#121526 = CARTESIAN_POINT('Ctrl Pts',(-22.0627069665889,12.7436129687706,
131.427847524928)) ;
#121527 = CARTESIAN_POINT('Ctrl Pts',(-22.1228015587848,12.9681022843807,
131.570102893173)) ;
#121528 = CARTESIAN_POINT('Ctrl Pts',(-22.1614820013196,13.2239471753799,
131.650012500945)) ;
#121529 = CARTESIAN_POINT('Ctrl Pts',(-22.1772375533801,13.4941633310118,
131.662924277638)) ;
#121530 = CARTESIAN_POINT('Ctrl Pts',(-22.1695983588983,13.7589186956337,
131.607544732681)) ;
#121531 = CARTESIAN_POINT('Ctrl Pts',(-22.1398896393099,13.9998349614895,
131.487676911223)) ;
#121532 = CARTESIAN_POINT('Ctrl Pts',(-22.0908619235723,14.1997646891006,
131.311332678912)) ;
#121533 = CARTESIAN_POINT('Ctrl Pts',(-22.0266945737524,14.344263749604,131.090721536142)) ;
#121534 = CARTESIAN_POINT('Ctrl Pts',(-21.952680793742,14.4224928496146,130.841310291008)) ;
#121535 = CARTESIAN_POINT('Ctrl Pts',(-21.8754606570184,14.4291711030004,
130.58274926124)) ;
#121536 = CARTESIAN_POINT('Ctrl Pts',(-21.8001571446588,14.3636108427049,
130.329504565342)) ;
#121537 = CARTESIAN_POINT('Ctrl Pts',(-21.7338905583542,14.2305640728087,
130.102800547914)) ;
#121538 = CARTESIAN_POINT('Ctrl Pts',(-21.6819125731549,14.0406274763076,
129.917954418755)) ;
#121539 = CARTESIAN_POINT('Ctrl Pts',(-21.6482766927022,13.8058698761943,
129.786568126659)) ;
#121540 = CARTESIAN_POINT('Ctrl Pts',(-21.6364270305114,13.5427807142404,
129.718722262125)) ;
#121541 = CARTESIAN_POINT('Ctrl Pts',(-21.6479525293074,13.2720604281958,
129.719284180321)) ;
#121542 = CARTESIAN_POINT('Ctrl Pts',(-21.6827354707971,13.0118428173477,
129.787740591491)) ;
#121543 = CARTESIAN_POINT('Ctrl Pts',(-21.7387645363647,12.7818787427455,
129.918382531202)) ;
#121544 = CARTESIAN_POINT('Ctrl Pts',(-21.8131751278323,12.5968716108038,
130.102584387991)) ;
#121545 = CARTESIAN_POINT('Ctrl Pts',(-21.9012978983489,12.4712516936664,
130.326815834056)) ;
#121546 = CARTESIAN_POINT('Ctrl Pts',(-21.9970924731431,12.4142247915804,
130.573571167119)) ;
#121547 = CARTESIAN_POINT('Ctrl Pts',(-22.0946249674174,12.4291610555867,
130.825434404428)) ;
#121548 = CARTESIAN_POINT('Ctrl Pts',(-22.1880538379132,12.5152749819563,
131.065210306025)) ;
#121549 = CARTESIAN_POINT('Ctrl Pts',(-22.2712353524733,12.6672522728085,
131.274961582696)) ;
#121550 = CARTESIAN_POINT('Ctrl Pts',(-22.3381448037188,12.8714563958125,
131.437501065827)) ;
#121551 = CARTESIAN_POINT('Ctrl Pts',(-22.3859106141911,13.1164156857726,
131.543882892038)) ;
#121552 = CARTESIAN_POINT('Ctrl Pts',(-22.4112282957359,13.3833143982509,
131.584711419103)) ;
#121553 = CARTESIAN_POINT('Ctrl Pts',(-22.4130217695324,13.6536761836367,
131.55673452737)) ;
#121554 = CARTESIAN_POINT('Ctrl Pts',(-22.3920167236971,13.9063303712051,
131.462322269529)) ;
#121555 = CARTESIAN_POINT('Ctrl Pts',(-22.3501194078207,14.1256565234766,
131.306665041968)) ;
#121556 = CARTESIAN_POINT('Ctrl Pts',(-22.2918172565239,14.2929703987116,
131.103406435929)) ;
#121557 = CARTESIAN_POINT('Ctrl Pts',(-22.2209556831958,14.3994043098715,
130.863140859753)) ;
#121558 = CARTESIAN_POINT('Ctrl Pts',(-22.1443006583547,14.4351253202518,
130.60615685561)) ;
#121559 = CARTESIAN_POINT('Ctrl Pts',(-22.0676126713909,14.3988243976867,
130.349047099311)) ;
#121560 = CARTESIAN_POINT('Ctrl Pts',(-21.9970015558164,14.2923293350233,
130.109611142122)) ;
#121561 = CARTESIAN_POINT('Ctrl Pts',(-21.9386211582789,14.1241731198379,
129.906023714666)) ;
#121562 = CARTESIAN_POINT('Ctrl Pts',(-21.8969564647824,13.9051613921294,
129.751139774253)) ;
#121563 = CARTESIAN_POINT('Ctrl Pts',(-21.8760425466096,13.6518311296983,
129.656921029517)) ;
#121564 = CARTESIAN_POINT('Ctrl Pts',(-21.8779576296647,13.382470855745,129.629430197668)) ;
#121565 = CARTESIAN_POINT('Ctrl Pts',(-21.903356370173,13.1154253093326,129.670468190117)) ;
#121566 = CARTESIAN_POINT('Ctrl Pts',(-21.9511796972224,12.870532627165,129.777021512631)) ;
#121567 = CARTESIAN_POINT('Ctrl Pts',(-22.018597334857,12.6655370623813,129.940858603322)) ;
#121568 = CARTESIAN_POINT('Ctrl Pts',(-22.1016149733205,12.5146112144562,
130.150247300748)) ;
#121569 = CARTESIAN_POINT('Ctrl Pts',(-22.1950646404757,12.4289101805898,
130.390085189532)) ;
#121570 = CARTESIAN_POINT('Ctrl Pts',(-22.2924700780955,12.414189675376,130.641628079446)) ;
#121571 = CARTESIAN_POINT('Ctrl Pts',(-22.3890144251563,12.4724108843215,
130.890294126128)) ;
#121572 = CARTESIAN_POINT('Ctrl Pts',(-22.4763336587939,12.5978142660017,
131.112435610646)) ;
#121573 = CARTESIAN_POINT('Ctrl Pts',(-22.5506291996143,12.7826552616513,
131.296338429027)) ;
#121574 = CARTESIAN_POINT('Ctrl Pts',(-22.6066949619686,13.0133815728599,
131.427008840756)) ;
#121575 = CARTESIAN_POINT('Ctrl Pts',(-22.6413737989187,13.2742169731993,
131.495103126571)) ;
#121576 = CARTESIAN_POINT('Ctrl Pts',(-22.652675011079,13.5450315924184,131.494998262817)) ;
#121577 = CARTESIAN_POINT('Ctrl Pts',(-22.6407386602464,13.8067212996898,
131.427059832861)) ;
#121578 = CARTESIAN_POINT('Ctrl Pts',(-22.6071088701475,14.041251387199,131.295715732246)) ;
#121579 = CARTESIAN_POINT('Ctrl Pts',(-22.5548293120912,14.2318697837458,
131.109842788739)) ;
#121580 = CARTESIAN_POINT('Ctrl Pts',(-22.4882219597125,14.3645253457052,
130.882041140552)) ;
#121581 = CARTESIAN_POINT('Ctrl Pts',(-22.4135301561278,14.4291513856489,
130.630867987503)) ;
#121582 = CARTESIAN_POINT('Ctrl Pts',(-22.3359383497484,14.4223448074479,
130.371059800614)) ;
#121583 = CARTESIAN_POINT('Ctrl Pts',(-22.2619633520101,14.3433927947591,
130.121750920733)) ;
#121584 = CARTESIAN_POINT('Ctrl Pts',(-22.1981313809753,14.1993296986607,
129.902268927259)) ;
#121585 = CARTESIAN_POINT('Ctrl Pts',(-22.1490456223981,13.9988089965648,
129.725677746774)) ;
#121586 = CARTESIAN_POINT('Ctrl Pts',(-22.1194205531409,13.7578101300497,
129.60606621788)) ;
#121587 = CARTESIAN_POINT('Ctrl Pts',(-22.1119250099299,13.4916490682303,
129.550940820402)) ;
#121588 = CARTESIAN_POINT('Ctrl Pts',(-22.1278069450151,13.2223242995655,
129.564332881806)) ;
#121589 = CARTESIAN_POINT('Ctrl Pts',(-22.166820729976,12.9657468504133,129.645089069852)) ;
#121590 = CARTESIAN_POINT('Ctrl Pts',(-22.2266899368361,12.7429296521264,
129.78689267835)) ;
#121591 = CARTESIAN_POINT('Ctrl Pts',(-22.3038746479134,12.5685157086448,
129.979270003299)) ;
#121592 = CARTESIAN_POINT('Ctrl Pts',(-22.3941718104836,12.4549912632195,
130.209772948028)) ;
#121593 = CARTESIAN_POINT('Ctrl Pts',(-22.4904254232344,12.4115665136302,
130.457995293597)) ;
#121594 = CARTESIAN_POINT('Ctrl Pts',(-22.5877870812419,12.4399153720153,
130.709299834689)) ;
#121595 = CARTESIAN_POINT('Ctrl Pts',(-22.6798460130406,12.5392662733084,
130.945012346427)) ;
#121596 = CARTESIAN_POINT('Ctrl Pts',(-22.7601047464817,12.7015765304021,
131.146380117816)) ;
#121597 = CARTESIAN_POINT('Ctrl Pts',(-22.8238896240796,12.9151235302472,
131.299658737214)) ;
#121598 = CARTESIAN_POINT('Ctrl Pts',(-22.8675764779866,13.1655123638567,
131.394148657853)) ;
#121599 = CARTESIAN_POINT('Ctrl Pts',(-22.8885227240857,13.4357073085102,
131.42204915288)) ;
#121600 = CARTESIAN_POINT('Ctrl Pts',(-22.8858619215617,13.7027427406616,
131.381268339562)) ;
#121601 = CARTESIAN_POINT('Ctrl Pts',(-22.8607916607201,13.9504288317899,
131.274952297113)) ;
#121602 = CARTESIAN_POINT('Ctrl Pts',(-22.815558311505,14.1608971109305,131.109650229729)) ;
#121603 = CARTESIAN_POINT('Ctrl Pts',(-22.7543026730754,14.3182076735822,
130.897587615978)) ;
#121604 = CARTESIAN_POINT('Ctrl Pts',(-22.6820714114506,14.4114239786406,
130.653451460202)) ;
#121605 = CARTESIAN_POINT('Ctrl Pts',(-22.6049103118654,14.4338711414245,
130.394968464032)) ;
#121606 = CARTESIAN_POINT('Ctrl Pts',(-22.5287473843446,14.3839736196214,
130.139317443058)) ;
#121607 = CARTESIAN_POINT('Ctrl Pts',(-22.459971667544,14.2649033535115,129.905232477421)) ;
#121608 = CARTESIAN_POINT('Ctrl Pts',(-22.4044402450173,14.0862372824977,
129.709967380025)) ;
#121609 = CARTESIAN_POINT('Ctrl Pts',(-22.3664456626379,13.8593709017047,
129.565802970245)) ;
#121610 = CARTESIAN_POINT('Ctrl Pts',(-22.3497272642463,13.6016401376878,
129.483857102706)) ;
#121611 = CARTESIAN_POINT('Ctrl Pts',(-22.3560994962859,13.3309240386314,
129.469335731797)) ;
#121612 = CARTESIAN_POINT('Ctrl Pts',(-22.3858506421703,13.0670232558749,
129.523137281469)) ;
#121613 = CARTESIAN_POINT('Ctrl Pts',(-22.4375345414781,12.828626100883,129.641014989765)) ;
#121614 = CARTESIAN_POINT('Ctrl Pts',(-22.5083363812964,12.6324568485675,
129.814684706642)) ;
#121615 = CARTESIAN_POINT('Ctrl Pts',(-22.5937839707588,12.4932133187338,
130.031160714492)) ;
#121616 = CARTESIAN_POINT('Ctrl Pts',(-22.6881953246157,12.4206918000049,
130.273922071333)) ;
#121617 = CARTESIAN_POINT('Ctrl Pts',(-22.7861951971573,12.4196226873693,
130.527040965204)) ;
#121618 = CARTESIAN_POINT('Ctrl Pts',(-22.8812583930361,12.491015534073,130.77152639582)) ;
#121619 = CARTESIAN_POINT('Ctrl Pts',(-22.9666341838661,12.6283740411058,
130.987922473245)) ;
#121620 = CARTESIAN_POINT('Ctrl Pts',(-23.0380241779246,12.8237070115403,
131.163235063303)) ;
#121621 = CARTESIAN_POINT('Ctrl Pts',(-23.0901672903314,13.061674988434,131.282420600478)) ;
#121622 = CARTESIAN_POINT('Ctrl Pts',(-23.1203227852946,13.32403831549,131.33754630017)) ;
#121623 = CARTESIAN_POINT('Ctrl Pts',(-23.1273409911795,13.5952494532198,
131.324861458868)) ;
#121624 = CARTESIAN_POINT('Ctrl Pts',(-23.1110257455182,13.8544595639362,
131.243964214945)) ;
#121625 = CARTESIAN_POINT('Ctrl Pts',(-23.0735006754812,14.0816540138682,
131.101239043931)) ;
#121626 = CARTESIAN_POINT('Ctrl Pts',(-23.0184218320253,14.2612880227879,
130.907347850486)) ;
#121627 = CARTESIAN_POINT('Ctrl Pts',(-22.9500143562106,14.3817634541805,
130.674390989242)) ;
#121628 = CARTESIAN_POINT('Ctrl Pts',(-22.8738736556778,14.4336477376616,
130.418767505991)) ;
#121629 = CARTESIAN_POINT('Ctrl Pts',(-22.7962947688756,14.4124733819028,
130.158897256619)) ;
#121630 = CARTESIAN_POINT('Ctrl Pts',(-22.7244222517359,14.3214777204803,
129.916058077239)) ;
#121631 = CARTESIAN_POINT('Ctrl Pts',(-22.6625658163423,14.1652192318908,
129.702115717874)) ;
#121632 = CARTESIAN_POINT('Ctrl Pts',(-22.616956336506,13.955565015999,129.535701263914)) ;
#121633 = CARTESIAN_POINT('Ctrl Pts',(-22.5914008763533,13.709559951643,129.428089151197)) ;
#121634 = CARTESIAN_POINT('Ctrl Pts',(-22.5882016234741,13.4405995053874,
129.385467312093)) ;
#121635 = CARTESIAN_POINT('Ctrl Pts',(-22.6086689737768,13.1715077449996,
129.412122430663)) ;
#121636 = CARTESIAN_POINT('Ctrl Pts',(-22.6515386816599,12.9214880577471,
129.504375180884)) ;
#121637 = CARTESIAN_POINT('Ctrl Pts',(-22.7152706299767,12.7055052948916,
129.657291190798)) ;
#121638 = CARTESIAN_POINT('Ctrl Pts',(-22.7950426841781,12.5425196624815,
129.857326438602)) ;
#121639 = CARTESIAN_POINT('Ctrl Pts',(-22.8865698066011,12.4416160232308,
130.091588674576)) ;
#121640 = CARTESIAN_POINT('Ctrl Pts',(-22.984492058789,12.4112449643292,130.344321485387)) ;
#121641 = CARTESIAN_POINT('Ctrl Pts',(-23.0811185429017,12.4537097251659,
130.593526328685)) ;
#121642 = CARTESIAN_POINT('Ctrl Pts',(-23.1710261323751,12.5652232898652,
130.823102119305)) ;
#121643 = CARTESIAN_POINT('Ctrl Pts',(-23.2485247769713,12.7379440423451,
131.01643444413)) ;
#121644 = CARTESIAN_POINT('Ctrl Pts',(-23.3089752450533,12.9603974854775,
131.159852173904)) ;
#121645 = CARTESIAN_POINT('Ctrl Pts',(-23.348408153789,13.2156635264027,131.241930685278)) ;
#121646 = CARTESIAN_POINT('Ctrl Pts',(-23.3649083403446,13.4857934304202,
131.257011973087)) ;
#121647 = CARTESIAN_POINT('Ctrl Pts',(-23.357909971757,13.7522947042676,131.203342265099)) ;
#121648 = CARTESIAN_POINT('Ctrl Pts',(-23.328617454617,13.9943545056691,131.084632132187)) ;
#121649 = CARTESIAN_POINT('Ctrl Pts',(-23.2803059324415,14.1947046686213,
130.910538675676)) ;
#121650 = CARTESIAN_POINT('Ctrl Pts',(-23.2162094085204,14.341452975733,130.689990853063)) ;
#121651 = CARTESIAN_POINT('Ctrl Pts',(-23.142748044954,14.4211243225131,130.442364505768)) ;
#121652 = CARTESIAN_POINT('Ctrl Pts',(-23.0653904655543,14.4300014254347,
130.183330074937)) ;
#121653 = CARTESIAN_POINT('Ctrl Pts',(-22.9900701305937,14.3664765373256,
129.930097446145)) ;
#121654 = CARTESIAN_POINT('Ctrl Pts',(-22.923513785988,14.2356051810154,129.702583954865)) ;
#121655 = CARTESIAN_POINT('Ctrl Pts',(-22.8708357577981,14.0463420011333,
129.515552886833)) ;
#121656 = CARTESIAN_POINT('Ctrl Pts',(-22.8367444403438,13.8127311118514,
129.382871206129)) ;
#121657 = CARTESIAN_POINT('Ctrl Pts',(-22.8242308008636,13.5514860506215,
129.313245492721)) ;
#121658 = CARTESIAN_POINT('Ctrl Pts',(-22.8350769331615,13.2797430818136,
129.311697539403)) ;
#121659 = CARTESIAN_POINT('Ctrl Pts',(-22.869098225033,13.0196140734991,129.378020218601)) ;
#121660 = CARTESIAN_POINT('Ctrl Pts',(-22.9247143370731,12.7876901355889,
129.507337456949)) ;
#121661 = CARTESIAN_POINT('Ctrl Pts',(-22.9985974383203,12.6015317076786,
129.69004468155)) ;
#121662 = CARTESIAN_POINT('Ctrl Pts',(-23.086121475707,12.474259722316,129.912620832564)) ;
#121663 = CARTESIAN_POINT('Ctrl Pts',(-23.1818805907226,12.41484596922,130.159228255654)) ;
#121664 = CARTESIAN_POINT('Ctrl Pts',(-23.2797131219869,12.4277168198839,
130.411880974866)) ;
#121665 = CARTESIAN_POINT('Ctrl Pts',(-23.3732545642975,12.511951186466,130.652010946363)) ;
#121666 = CARTESIAN_POINT('Ctrl Pts',(-23.4565110007243,12.6612551341691,
130.862127850995)) ;
#121667 = CARTESIAN_POINT('Ctrl Pts',(-23.5244261393507,12.8654798246469,
131.027369978243)) ;
#121668 = CARTESIAN_POINT('Ctrl Pts',(-23.5725829742774,13.1088716253824,
131.135002247458)) ;
#121669 = CARTESIAN_POINT('Ctrl Pts',(-23.5986019731753,13.3752799217244,
131.177886352702)) ;
#121670 = CARTESIAN_POINT('Ctrl Pts',(-23.6011015071733,13.6458120251598,
131.151980086065)) ;
#121671 = CARTESIAN_POINT('Ctrl Pts',(-23.5806843251492,13.8994658312756,
131.059242348324)) ;
#121672 = CARTESIAN_POINT('Ctrl Pts',(-23.5395648399883,14.1192749080617,
130.905996408547)) ;
#121673 = CARTESIAN_POINT('Ctrl Pts',(-23.4813848765133,14.2891803120814,
130.702911334462)) ;
#121674 = CARTESIAN_POINT('Ctrl Pts',(-23.4111139306529,14.3970324954729,
130.464529997136)) ;
#121675 = CARTESIAN_POINT('Ctrl Pts',(-23.3344012694939,14.4351164738745,
130.207301293697)) ;
#121676 = CARTESIAN_POINT('Ctrl Pts',(-23.2576890516809,14.4010787693592,
129.950158636102)) ;
#121677 = CARTESIAN_POINT('Ctrl Pts',(-23.1864140310954,14.2958209261601,
129.708587842653)) ;
#121678 = CARTESIAN_POINT('Ctrl Pts',(-23.1278795559311,14.1296521769512,
129.504668064509)) ;
#121679 = CARTESIAN_POINT('Ctrl Pts',(-23.0856754302554,13.9121761365587,
129.348238913807)) ;
#121680 = CARTESIAN_POINT('Ctrl Pts',(-23.0641329052405,13.6594303450515,
129.252162708667)) ;
#121681 = CARTESIAN_POINT('Ctrl Pts',(-23.0653052820305,13.3906473022496,
129.222550978665)) ;
#121682 = CARTESIAN_POINT('Ctrl Pts',(-23.090283304595,13.1215485534994,129.26213901249)) ;
#121683 = CARTESIAN_POINT('Ctrl Pts',(-23.1372175806603,12.8774994745799,
129.366325807078)) ;
#121684 = CARTESIAN_POINT('Ctrl Pts',(-23.204393997006,12.6702279287505,129.52931153654)) ;
#121685 = CARTESIAN_POINT('Ctrl Pts',(-23.2867150726529,12.5183910310168,
129.736808163785)) ;
#121686 = CARTESIAN_POINT('Ctrl Pts',(-23.3799501396602,12.4302683036152,
129.976005708702)) ;
#121687 = CARTESIAN_POINT('Ctrl Pts',(-23.4780194336623,12.4138255898749,
130.229248949606)) ;
#121688 = CARTESIAN_POINT('Ctrl Pts',(-23.5734967171244,12.4692849906945,
130.475218068993)) ;
#121689 = CARTESIAN_POINT('Ctrl Pts',(-23.6617647155434,12.593086865603,130.699920489542)) ;
#121690 = CARTESIAN_POINT('Ctrl Pts',(-23.7366528628754,12.7771359957172,
130.88546921267)) ;
#121691 = CARTESIAN_POINT('Ctrl Pts',(-23.7930824889268,13.0059650352549,
131.017318083727)) ;
#121692 = CARTESIAN_POINT('Ctrl Pts',(-23.8284573242334,13.2661472489738,
131.087445926367)) ;
#121693 = CARTESIAN_POINT('Ctrl Pts',(-23.8404774545327,13.5369907136561,
131.089436183749)) ;
#121694 = CARTESIAN_POINT('Ctrl Pts',(-23.829155718935,13.7997449792612,131.023219419023)) ;
#121695 = CARTESIAN_POINT('Ctrl Pts',(-23.7961622175003,14.0350784316614,
130.893776777003)) ;
#121696 = CARTESIAN_POINT('Ctrl Pts',(-23.7440972612148,14.2276701569779,
130.708399650426)) ;
#121697 = CARTESIAN_POINT('Ctrl Pts',(-23.6784579579534,14.3610391391533,
130.483737931397)) ;
#121698 = CARTESIAN_POINT('Ctrl Pts',(-23.6033254135512,14.4285213682471,
130.230995383092)) ;
#121699 = CARTESIAN_POINT('Ctrl Pts',(-23.5258829163053,14.4233691347863,
129.971694462302)) ;
#121700 = CARTESIAN_POINT('Ctrl Pts',(-23.4519103008065,14.3469900200021,
129.722496786167)) ;
#121701 = CARTESIAN_POINT('Ctrl Pts',(-23.3872758527117,14.2034039230656,
129.50041476823)) ;
#121702 = CARTESIAN_POINT('Ctrl Pts',(-23.3380843805541,14.0056847317555,
129.323768358841)) ;
#121703 = CARTESIAN_POINT('Ctrl Pts',(-23.3077174301833,13.7644934618712,
129.201819431847)) ;
#121704 = CARTESIAN_POINT('Ctrl Pts',(-23.2995656105439,13.5002463021735,
129.144972753961)) ;
#121705 = CARTESIAN_POINT('Ctrl Pts',(-23.31497764899,13.2284057614088,129.156686870194)) ;
#121706 = CARTESIAN_POINT('Ctrl Pts',(-23.3529809802264,12.9739037003026,
129.234851116751)) ;
#121707 = CARTESIAN_POINT('Ctrl Pts',(-23.4125409802653,12.7484703827135,
129.375556014686)) ;
#121708 = CARTESIAN_POINT('Ctrl Pts',(-23.489066219191,12.5731123065293,129.566119181298)) ;
#121709 = CARTESIAN_POINT('Ctrl Pts',(-23.5791220316779,12.4573590720307,
129.795883585505)) ;
#121710 = CARTESIAN_POINT('Ctrl Pts',(-23.6753629969101,12.4118025437708,
130.044038138499)) ;
#121711 = CARTESIAN_POINT('Ctrl Pts',(-23.7728143173082,12.4381298316287,
130.295594078623)) ;
#121712 = CARTESIAN_POINT('Ctrl Pts',(-23.8649582071419,12.5352056674708,
130.53162152315)) ;
#121713 = CARTESIAN_POINT('Ctrl Pts',(-23.9458556331746,12.6963006126537,
130.734754487128)) ;
#121714 = CARTESIAN_POINT('Ctrl Pts',(-24.0101297169403,12.9082756109017,
130.889506306032)) ;
#121715 = CARTESIAN_POINT('Ctrl Pts',(-24.0545841543703,13.1596325292673,
130.986017902497)) ;
#121716 = CARTESIAN_POINT('Ctrl Pts',(-24.0759302955051,13.4259468803236,
131.015538335644)) ;
#121717 = CARTESIAN_POINT('Ctrl Pts',(-24.0740919955481,13.6953761001562,
130.976901663814)) ;
#121718 = CARTESIAN_POINT('Ctrl Pts',(-24.0495884975813,13.943717027651,130.872263472699)) ;
#121719 = CARTESIAN_POINT('Ctrl Pts',(-24.0048388868655,14.1557110892649,
130.7083358927)) ;
#121720 = CARTESIAN_POINT('Ctrl Pts',(-23.9440791244033,14.3144000289701,
130.497783976676)) ;
#121721 = CARTESIAN_POINT('Ctrl Pts',(-23.8721181136908,14.4096307928531,
130.254444307952)) ;
#121722 = CARTESIAN_POINT('Ctrl Pts',(-23.7949917478579,14.4343455409311,
129.996055887983)) ;
#121723 = CARTESIAN_POINT('Ctrl Pts',(-23.7183945611364,14.3860725213322,
129.738990412357)) ;
#121724 = CARTESIAN_POINT('Ctrl Pts',(-23.6497155209254,14.269509697164,129.505378523881)) ;
#121725 = CARTESIAN_POINT('Ctrl Pts',(-23.5935085503092,14.0917907400684,
129.308007286199)) ;
#121726 = CARTESIAN_POINT('Ctrl Pts',(-23.5550865672651,13.8666926815631,
129.162696838379)) ;
#121727 = CARTESIAN_POINT('Ctrl Pts',(-23.5376687883105,13.6093228235484,
129.078662798644)) ;
#121728 = CARTESIAN_POINT('Ctrl Pts',(-23.5433650492229,13.3388431242067,
129.062185597359)) ;
#121729 = CARTESIAN_POINT('Ctrl Pts',(-23.5724839615649,13.0740473551912,
129.114088332955)) ;
#121730 = CARTESIAN_POINT('Ctrl Pts',(-23.6237334254588,12.834394570963,129.230640971734)) ;
#121731 = CARTESIAN_POINT('Ctrl Pts',(-23.6936925175192,12.6378258855697,
129.402017995682)) ;
#121732 = CARTESIAN_POINT('Ctrl Pts',(-23.7787793504876,12.4964629704439,
129.617422649139)) ;
#121733 = CARTESIAN_POINT('Ctrl Pts',(-23.8732647499766,12.4217253903026,
129.860312611565)) ;
#121734 = CARTESIAN_POINT('Ctrl Pts',(-23.9711567729886,12.4187226329277,
130.113148873488)) ;
#121735 = CARTESIAN_POINT('Ctrl Pts',(-24.0660810815152,12.4875916931866,
130.357347207621)) ;
#121736 = CARTESIAN_POINT('Ctrl Pts',(-24.1521509829385,12.6235712974209,
130.575641050135)) ;
#121737 = CARTESIAN_POINT('Ctrl Pts',(-24.2237599658154,12.8167008380917,
130.751719197744)) ;
#121738 = CARTESIAN_POINT('Ctrl Pts',(-24.2766320275245,13.053470182096,130.873029282451)) ;
#121739 = CARTESIAN_POINT('Ctrl Pts',(-24.3076017852851,13.3166530721009,
130.930371105452)) ;
#121740 = CARTESIAN_POINT('Ctrl Pts',(-24.3152190181606,13.5871782516177,
130.919526468752)) ;
#121741 = CARTESIAN_POINT('Ctrl Pts',(-24.2997261236397,13.8461111103248,
130.841158630787)) ;
#121742 = CARTESIAN_POINT('Ctrl Pts',(-24.2627363075861,14.0754123777246,
130.699882780774)) ;
#121743 = CARTESIAN_POINT('Ctrl Pts',(-24.2079729206968,14.2569965796042,
130.506838743706)) ;
#121744 = CARTESIAN_POINT('Ctrl Pts',(-24.1398686531416,14.3792169528627,
130.274773785101)) ;
#121745 = CARTESIAN_POINT('Ctrl Pts',(-24.0640873934345,14.4330645797171,
130.020296166721)) ;
#121746 = CARTESIAN_POINT('Ctrl Pts',(-23.9864701853882,14.4142942026361,
129.760321344143)) ;
#121747 = CARTESIAN_POINT('Ctrl Pts',(-23.9140656407132,14.3249818434921,
129.515797144389)) ;
#121748 = CARTESIAN_POINT('Ctrl Pts',(-23.8518321133868,14.1700409218133,
129.300722456645)) ;
#121749 = CARTESIAN_POINT('Ctrl Pts',(-23.8059089034799,13.9629928676694,
129.133578126005)) ;
#121750 = CARTESIAN_POINT('Ctrl Pts',(-23.7795827562579,13.7164972263621,
129.023526816175)) ;
#121751 = CARTESIAN_POINT('Ctrl Pts',(-23.7757564515604,13.4493823729498,
128.97926513916)) ;
#121752 = CARTESIAN_POINT('Ctrl Pts',(-23.7954419194189,13.1794660077169,
129.00356919432)) ;
#121753 = CARTESIAN_POINT('Ctrl Pts',(-23.8379907278059,12.9274139547086,
129.094708724123)) ;
#121754 = CARTESIAN_POINT('Ctrl Pts',(-23.9008430840631,12.7115777217288,
129.24525361468)) ;
#121755 = CARTESIAN_POINT('Ctrl Pts',(-23.9801928783826,12.5463884356972,
129.444024662867)) ;
#121756 = CARTESIAN_POINT('Ctrl Pts',(-24.0722443681962,12.443178693002,129.679554649046)) ;
#121757 = CARTESIAN_POINT('Ctrl Pts',(-24.1690180676137,12.4112124572602,
129.92930163527)) ;
#121758 = CARTESIAN_POINT('Ctrl Pts',(-24.2661327749485,12.4513454619086,
130.179802073149)) ;
#121759 = CARTESIAN_POINT('Ctrl Pts',(-24.3562959525543,12.5610016946322,
130.410134143463)) ;
#121760 = CARTESIAN_POINT('Ctrl Pts',(-24.4343250881083,12.732231543376,130.604978977865)) ;
#121761 = CARTESIAN_POINT('Ctrl Pts',(-24.4953391322898,12.9536822141676,
130.750023050811)) ;
#121762 = CARTESIAN_POINT('Ctrl Pts',(-24.5353305531141,13.2077095887355,
130.833800831059)) ;
#121763 = CARTESIAN_POINT('Ctrl Pts',(-24.5525587376172,13.4778390375596,
130.850989350465)) ;
#121764 = CARTESIAN_POINT('Ctrl Pts',(-24.5462019536801,13.7447250723396,
130.799190280117)) ;
#121765 = CARTESIAN_POINT('Ctrl Pts',(-24.5176953064597,13.9871379837623,
130.682880665988)) ;
#121766 = CARTESIAN_POINT('Ctrl Pts',(-24.4695538860457,14.1900737145365,
130.509067328973)) ;
#121767 = CARTESIAN_POINT('Ctrl Pts',(-24.4064340261719,14.3373318040479,
130.291685786572)) ;
#121768 = CARTESIAN_POINT('Ctrl Pts',(-24.3327321271544,14.419933546752,130.04313050484)) ;
#121769 = CARTESIAN_POINT('Ctrl Pts',(-24.2554111115595,14.4307823852778,
129.784218809138)) ;
#121770 = CARTESIAN_POINT('Ctrl Pts',(-24.1797499325286,14.3690285004678,
129.529899580821)) ;
#121771 = CARTESIAN_POINT('Ctrl Pts',(-24.1131557614582,14.2404409367686,
129.302414068984)) ;
#121772 = CARTESIAN_POINT('Ctrl Pts',(-24.0599615774343,14.0528075419849,
129.113868915362)) ;
#121773 = CARTESIAN_POINT('Ctrl Pts',(-24.0252316135323,13.8202654365076,
128.979314882882)) ;
#121774 = CARTESIAN_POINT('Ctrl Pts',(-24.0120333005036,13.5584443869878,
128.907549138537)) ;
#121775 = CARTESIAN_POINT('Ctrl Pts',(-24.0222813639588,13.2871049531719,
128.904304542644)) ;
#121776 = CARTESIAN_POINT('Ctrl Pts',(-24.0555382378822,13.0271135604128,
128.96848416764)) ;
#121777 = CARTESIAN_POINT('Ctrl Pts',(-24.1106071061266,12.7938647144907,
129.096170233129)) ;
#121778 = CARTESIAN_POINT('Ctrl Pts',(-24.1839223129408,12.6063347659711,
129.277257696409)) ;
#121779 = CARTESIAN_POINT('Ctrl Pts',(-24.2712622814274,12.4770287601625,
129.499241059545)) ;
#121780 = CARTESIAN_POINT('Ctrl Pts',(-24.366585154662,12.4155889088205,129.744672790457)) ;
#121781 = CARTESIAN_POINT('Ctrl Pts',(-24.4648941553705,12.4264045930434,
129.998562059193)) ;
#121782 = CARTESIAN_POINT('Ctrl Pts',(-24.5583069638422,12.5084013028489,
130.238438570714)) ;
#121783 = CARTESIAN_POINT('Ctrl Pts',(-24.6421105256963,12.6562046151244,
130.450082237767)) ;
#121784 = CARTESIAN_POINT('Ctrl Pts',(-24.7103360959245,12.8582528702238,
130.616348720843)) ;
#121785 = CARTESIAN_POINT('Ctrl Pts',(-24.7594534193122,13.10224809555,130.726572672664)) ;
#121786 = CARTESIAN_POINT('Ctrl Pts',(-24.7859819902892,13.3685511856617,
130.770923579385)) ;
#121787 = CARTESIAN_POINT('Ctrl Pts',(-24.7891497215362,13.6374690862059,
130.747188210183)) ;
#121788 = CARTESIAN_POINT('Ctrl Pts',(-24.7693680180505,13.8926337693761,
130.656209398717)) ;
#121789 = CARTESIAN_POINT('Ctrl Pts',(-24.728815676264,14.1134974060216,130.50464468711)) ;
#121790 = CARTESIAN_POINT('Ctrl Pts',(-24.670909042521,14.2854804589728,130.302270913447)) ;
#121791 = CARTESIAN_POINT('Ctrl Pts',(-24.60088451724,14.394916969494,130.064614299334)) ;
#121792 = CARTESIAN_POINT('Ctrl Pts',(-24.5245965657273,14.435095047054,129.808769177446)) ;
#121793 = CARTESIAN_POINT('Ctrl Pts',(-24.4473637068243,14.4027523560096,
129.549904857935)) ;
#121794 = CARTESIAN_POINT('Ctrl Pts',(-24.3764277230312,14.3004224301193,
129.309619108113)) ;
#121795 = CARTESIAN_POINT('Ctrl Pts',(-24.3169230241164,14.1345848207203,
129.102566773987)) ;
#121796 = CARTESIAN_POINT('Ctrl Pts',(-24.2744113644466,13.9188292654447,
128.945352262584)) ;
#121797 = CARTESIAN_POINT('Ctrl Pts',(-24.2522045947965,13.6668968226668,
128.847333371272)) ;
#121798 = CARTESIAN_POINT('Ctrl Pts',(-24.2527678420555,13.3982258049414,
128.815930108952)) ;
#121799 = CARTESIAN_POINT('Ctrl Pts',(-24.276897987138,13.1299459818543,128.853191114343)) ;
#121800 = CARTESIAN_POINT('Ctrl Pts',(-24.3234245762368,12.8837060048702,
128.956014438392)) ;
#121801 = CARTESIAN_POINT('Ctrl Pts',(-24.3900144260355,12.6755091037675,
129.117341319656)) ;
#121802 = CARTESIAN_POINT('Ctrl Pts',(-24.4721077500629,12.5215778341602,
129.324106647647)) ;
#121803 = CARTESIAN_POINT('Ctrl Pts',(-24.565308269843,12.4317802078497,129.563149664211)) ;
#121804 = CARTESIAN_POINT('Ctrl Pts',(-24.6624846240227,12.4131805145463,
129.814074666226)) ;
#121805 = CARTESIAN_POINT('Ctrl Pts',(-24.7588780185162,12.4668842843224,
130.062448733751)) ;
#121806 = CARTESIAN_POINT('Ctrl Pts',(-24.8470359043657,12.5884450791791,
130.286983079046)) ;
#121807 = CARTESIAN_POINT('Ctrl Pts',(-24.9226051504243,12.7713421564293,
130.474427343393)) ;
#121808 = CARTESIAN_POINT('Ctrl Pts',(-24.9795413821956,12.9988618767288,
130.607794145805)) ;
#121809 = CARTESIAN_POINT('Ctrl Pts',(-25.0156442703355,13.259491403766,130.679917395231)) ;
#121810 = CARTESIAN_POINT('Ctrl Pts',(-25.0282091631295,13.5289134128762,
130.683668585279)) ;
#121811 = CARTESIAN_POINT('Ctrl Pts',(-25.0176337181152,13.792044854945,130.619653232571)) ;
#121812 = CARTESIAN_POINT('Ctrl Pts',(-24.9852005413018,14.0286824176204,
130.491809147473)) ;
#121813 = CARTESIAN_POINT('Ctrl Pts',(-24.9337121650507,14.2226477736602,
130.308157090339)) ;
#121814 = CARTESIAN_POINT('Ctrl Pts',(-24.8682137054445,14.3581280459106,
130.083808960179)) ;
#121815 = CARTESIAN_POINT('Ctrl Pts',(-24.7936202112881,14.4275172368953,
129.832803504155)) ;
#121816 = CARTESIAN_POINT('Ctrl Pts',(-24.7155627562385,14.4244373227483,
129.57144348336)) ;
#121817 = CARTESIAN_POINT('Ctrl Pts',(-24.6418264545641,14.3501367823951,
129.323115479504)) ;
#121818 = CARTESIAN_POINT('Ctrl Pts',(-24.5769236801836,14.2089997399679,
129.100323776134)) ;
#121819 = CARTESIAN_POINT('Ctrl Pts',(-24.5270385018368,14.0121250451069,
128.921539786194)) ;
#121820 = CARTESIAN_POINT('Ctrl Pts',(-24.4960631962097,13.7718246711113,
128.797806971439)) ;
#121821 = CARTESIAN_POINT('Ctrl Pts',(-24.4872948571739,13.5078186231509,
128.739133036855)) ;
#121822 = CARTESIAN_POINT('Ctrl Pts',(-24.5018717870073,13.2372789127591,
128.748585611505)) ;
#121823 = CARTESIAN_POINT('Ctrl Pts',(-24.5394131760315,12.980432676453,128.82518927761)) ;
#121824 = CARTESIAN_POINT('Ctrl Pts',(-24.5984747883142,12.7540238473754,
128.964448209837)) ;
#121825 = CARTESIAN_POINT('Ctrl Pts',(-24.6744370598604,12.5774627214212,
129.153422120935)) ;
#121826 = CARTESIAN_POINT('Ctrl Pts',(-24.7639922634429,12.4598742845048,
129.381793089141)) ;
#121827 = CARTESIAN_POINT('Ctrl Pts',(-24.8605500897258,12.4120040771025,
129.630724349691)) ;
#121828 = CARTESIAN_POINT('Ctrl Pts',(-24.958005807099,12.4365719363613,129.882309681314)) ;
#121829 = CARTESIAN_POINT('Ctrl Pts',(-25.050014463376,12.5311793730478,130.118080286586)) ;
#121830 = CARTESIAN_POINT('Ctrl Pts',(-25.1316226244339,12.6910252991536,
130.323175898126)) ;
#121831 = CARTESIAN_POINT('Ctrl Pts',(-25.1962471146522,12.9015546057863,
130.478998345646)) ;
#121832 = CARTESIAN_POINT('Ctrl Pts',(-25.241234670559,13.1503193802668,130.577277708208)) ;
#121833 = CARTESIAN_POINT('Ctrl Pts',(-25.2634976452827,13.4198238149612,
130.609042385242)) ;
#121834 = CARTESIAN_POINT('Ctrl Pts',(-25.2622779519396,13.6867201832379,
130.572566966855)) ;
#121835 = CARTESIAN_POINT('Ctrl Pts',(-25.2383200577923,13.9376559863072,
130.469290386923)) ;
#121836 = CARTESIAN_POINT('Ctrl Pts',(-25.1941474736539,14.1502428615257,
130.307142874577)) ;
#121837 = CARTESIAN_POINT('Ctrl Pts',(-25.1337264695222,14.3108380697217,
130.097535620536)) ;
#121838 = CARTESIAN_POINT('Ctrl Pts',(-25.0620137026065,14.4079445348436,
129.854934695128)) ;
#121839 = CARTESIAN_POINT('Ctrl Pts',(-24.9848714963236,14.4345276706247,
129.596461986952)) ;
#121840 = CARTESIAN_POINT('Ctrl Pts',(-24.9086676865302,14.3888298731307,
129.340776078196)) ;
#121841 = CARTESIAN_POINT('Ctrl Pts',(-24.8393136852622,14.273828468375,129.105021772797)) ;
#121842 = CARTESIAN_POINT('Ctrl Pts',(-24.7827347158713,14.0978368302853,
128.906604072011)) ;
#121843 = CARTESIAN_POINT('Ctrl Pts',(-24.7436676855994,13.8735407233332,
128.759347918809)) ;
#121844 = CARTESIAN_POINT('Ctrl Pts',(-24.7256369859318,13.6168750178338,
128.673534453122)) ;
#121845 = CARTESIAN_POINT('Ctrl Pts',(-24.7306702277621,13.346506361492,128.655118284453)) ;
#121846 = CARTESIAN_POINT('Ctrl Pts',(-24.7590932103143,13.0815407666398,
128.705024346918)) ;
#121847 = CARTESIAN_POINT('Ctrl Pts',(-24.8097282840083,12.8409646602013,
128.819785475391)) ;
#121848 = CARTESIAN_POINT('Ctrl Pts',(-24.8791063732593,12.6428639918128,
128.989483254521)) ;
#121849 = CARTESIAN_POINT('Ctrl Pts',(-24.9645394688412,12.4989646430065,
129.205645392299)) ;
#121850 = CARTESIAN_POINT('Ctrl Pts',(-25.0579878899541,12.4231076853541,
129.445814572811)) ;
#121851 = CARTESIAN_POINT('Ctrl Pts',(-25.1562511213808,12.4177381591252,
129.699599598718)) ;
#121852 = CARTESIAN_POINT('Ctrl Pts',(-25.2512788586479,12.4847095466627,
129.944123699546)) ;
#121853 = CARTESIAN_POINT('Ctrl Pts',(-25.3377821946392,12.6190668251906,
130.163642451019)) ;
#121854 = CARTESIAN_POINT('Ctrl Pts',(-25.4097944339434,12.8107471895688,
130.340916677767)) ;
#121855 = CARTESIAN_POINT('Ctrl Pts',(-25.4631706931729,13.0461049078406,
130.463753164619)) ;
#121856 = CARTESIAN_POINT('Ctrl Pts',(-25.4948238815669,13.3089104890012,
130.523073615046)) ;
#121857 = CARTESIAN_POINT('Ctrl Pts',(-25.5031265241636,13.5795918474296,
130.514220263891)) ;
#121858 = CARTESIAN_POINT('Ctrl Pts',(-25.4881933952742,13.8398549511919,
130.437390626082)) ;
#121859 = CARTESIAN_POINT('Ctrl Pts',(-25.4517218808051,14.0698649783882,
130.297660885074)) ;
#121860 = CARTESIAN_POINT('Ctrl Pts',(-25.3975893597401,14.2524396498396,
130.106562738251)) ;
#121861 = CARTESIAN_POINT('Ctrl Pts',(-25.329628163741,14.3767943288433,129.874835912649)) ;
#121862 = CARTESIAN_POINT('Ctrl Pts',(-25.2541712601105,14.4324209617662,
129.621391122632)) ;
#121863 = CARTESIAN_POINT('Ctrl Pts',(-25.1765759645738,14.4159981078524,
129.361510885237)) ;
#121864 = CARTESIAN_POINT('Ctrl Pts',(-25.1037149073964,14.3283155075796,
129.115542900356)) ;
#121865 = CARTESIAN_POINT('Ctrl Pts',(-25.0413114335729,14.1755658927935,
128.900081780878)) ;
#121866 = CARTESIAN_POINT('Ctrl Pts',(-24.9947967152274,13.9699067943466,
128.731193187408)) ;
#121867 = CARTESIAN_POINT('Ctrl Pts',(-24.9678237957013,13.7239839863066,
128.619211007753)) ;
#121868 = CARTESIAN_POINT('Ctrl Pts',(-24.9632948194165,13.4571372735282,
128.57289064357)) ;
#121869 = CARTESIAN_POINT('Ctrl Pts',(-24.9824896393098,13.1860385080971,
128.595632297208)) ;
#121870 = CARTESIAN_POINT('Ctrl Pts',(-25.0240453693991,12.9351633372793,
128.684136780175)) ;
#121871 = CARTESIAN_POINT('Ctrl Pts',(-25.0868468687025,12.7162804283108,
128.834258486375)) ;
#121872 = CARTESIAN_POINT('Ctrl Pts',(-25.1654757864791,12.5504602978257,
129.03108391557)) ;
#121873 = CARTESIAN_POINT('Ctrl Pts',(-25.257301839938,12.4451571789981,129.265930804602)) ;
#121874 = CARTESIAN_POINT('Ctrl Pts',(-25.3538628354389,12.4110818133835,
129.515105703089)) ;
#121875 = CARTESIAN_POINT('Ctrl Pts',(-25.4513699463354,12.4493848627309,
129.766644069087)) ;
#121876 = CARTESIAN_POINT('Ctrl Pts',(-25.5413331144309,12.5564279149636,
129.996576060182)) ;
#121877 = CARTESIAN_POINT('Ctrl Pts',(-25.62031355426,12.7270948796437,130.19397859587)) ;
#121878 = CARTESIAN_POINT('Ctrl Pts',(-25.6816176160566,12.9467013560163,
130.339987705186)) ;
#121879 = CARTESIAN_POINT('Ctrl Pts',(-25.7223434773691,13.2005745815833,
130.425833032778)) ;
#121880 = CARTESIAN_POINT('Ctrl Pts',(-25.7401264335062,13.4697556430519,
130.444737141503)) ;
#121881 = CARTESIAN_POINT('Ctrl Pts',(-25.7345998226882,13.736255276326,130.395473264133)) ;
#121882 = CARTESIAN_POINT('Ctrl Pts',(-25.7064542497978,13.9814042376555,
130.279958796847)) ;
#121883 = CARTESIAN_POINT('Ctrl Pts',(-25.6591900336752,14.1841667225104,
130.108970524327)) ;
#121884 = CARTESIAN_POINT('Ctrl Pts',(-25.5960522185544,14.3343212234818,
129.891306413167)) ;
#121885 = CARTESIAN_POINT('Ctrl Pts',(-25.5227733731923,14.4184551255459,
129.644101823257)) ;
#121886 = CARTESIAN_POINT('Ctrl Pts',(-25.4454407026881,14.4314519910157,
129.385130431416)) ;
#121887 = CARTESIAN_POINT('Ctrl Pts',(-25.3699325639496,14.3721434966701,
129.13139873682)) ;
#121888 = CARTESIAN_POINT('Ctrl Pts',(-25.3027559014807,14.245373795937,128.90211376727)) ;
#121889 = CARTESIAN_POINT('Ctrl Pts',(-25.2488792802276,14.0581566175582,
128.711411678173)) ;
#121890 = CARTESIAN_POINT('Ctrl Pts',(-25.2137932802583,13.8276967157625,
128.575975328907)) ;
#121891 = CARTESIAN_POINT('Ctrl Pts',(-25.199880050692,13.5670202701056,128.502182318622)) ;
#121892 = CARTESIAN_POINT('Ctrl Pts',(-25.2093925008277,13.2953785672156,
128.496751191105)) ;
#121893 = CARTESIAN_POINT('Ctrl Pts',(-25.242028626857,13.0342213948757,128.559046958988)) ;
#121894 = CARTESIAN_POINT('Ctrl Pts',(-25.2967851107302,12.799235193231,128.685702810719)) ;
#121895 = CARTESIAN_POINT('Ctrl Pts',(-25.3692327223565,12.6113832489784,
128.864447663773)) ;
#121896 = CARTESIAN_POINT('Ctrl Pts',(-25.4562878134917,12.4798503572911,
129.085564966862)) ;
#121897 = CARTESIAN_POINT('Ctrl Pts',(-25.5516448147479,12.4163978542697,
129.33103303498)) ;
#121898 = CARTESIAN_POINT('Ctrl Pts',(-25.6496515407606,12.4249215089451,
129.584153609053)) ;
#121899 = CARTESIAN_POINT('Ctrl Pts',(-25.7437456969646,12.505375632336,129.82584674247)) ;
#121900 = CARTESIAN_POINT('Ctrl Pts',(-25.8274940922264,12.6507859579669,
130.037493290738)) ;
#121901 = CARTESIAN_POINT('Ctrl Pts',(-25.8964204891319,12.8517471604921,
130.205732105265)) ;
#121902 = CARTESIAN_POINT('Ctrl Pts',(-25.9460652372226,13.0945615121704,
130.317535454147)) ;
#121903 = CARTESIAN_POINT('Ctrl Pts',(-25.9733381607594,13.3602126938648,
130.364087679988)) ;
#121904 = CARTESIAN_POINT('Ctrl Pts',(-25.9771342123268,13.6310672418703,
130.341965603779)) ;
#121905 = CARTESIAN_POINT('Ctrl Pts',(-25.9580426264907,13.8852754196112,
130.253211878795)) ;
#121906 = CARTESIAN_POINT('Ctrl Pts',(-25.9180734791188,14.1076160961634,
130.103323578132)) ;
#121907 = CARTESIAN_POINT('Ctrl Pts',(-25.8607234852378,14.2808806775566,
129.902643243913)) ;
#121908 = CARTESIAN_POINT('Ctrl Pts',(-25.7910301799006,14.3926567140697,
129.665957266958)) ;
#121909 = CARTESIAN_POINT('Ctrl Pts',(-25.7142471691777,14.4348969487797,
129.408406813689)) ;
#121910 = CARTESIAN_POINT('Ctrl Pts',(-25.6376724285755,14.4049966938089,
129.151792715386)) ;
#121911 = CARTESIAN_POINT('Ctrl Pts',(-25.5658305442248,14.3037928879971,
128.908552136202)) ;
#121912 = CARTESIAN_POINT('Ctrl Pts',(-25.506358907673,14.1405203886364,128.701827306642)) ;
#121913 = CARTESIAN_POINT('Ctrl Pts',(-25.4631682807316,13.9258191090176,
128.542562680316)) ;
#121914 = CARTESIAN_POINT('Ctrl Pts',(-25.4403035221641,13.6747404934951,
128.442635874831)) ;
#121915 = CARTESIAN_POINT('Ctrl Pts',(-25.4402682048589,13.4052256661744,
128.409346773511)) ;
#121916 = CARTESIAN_POINT('Ctrl Pts',(-25.4635287824975,13.138469239792,128.444304954167)) ;
#121917 = CARTESIAN_POINT('Ctrl Pts',(-25.5097037479834,12.8897551396211,
128.545882952362)) ;
#121918 = CARTESIAN_POINT('Ctrl Pts',(-25.5754518262798,12.6813707794316,
128.704929877967)) ;
#121919 = CARTESIAN_POINT('Ctrl Pts',(-25.6572496262362,12.5252896254052,
128.910771575894)) ;
#121920 = CARTESIAN_POINT('Ctrl Pts',(-25.7500041562407,12.4335761990142,
129.148588024565)) ;
#121921 = CARTESIAN_POINT('Ctrl Pts',(-25.8474528188583,12.4126069682806,
129.400196063375)) ;
#121922 = CARTESIAN_POINT('Ctrl Pts',(-25.9442289971032,12.4645413943428,
129.649602932719)) ;
#121923 = CARTESIAN_POINT('Ctrl Pts',(-26.0326523326431,12.5845283028617,
129.87490638314)) ;
#121924 = CARTESIAN_POINT('Ctrl Pts',(-26.1084253037707,12.7652451622035,
130.063060396479)) ;
#121925 = CARTESIAN_POINT('Ctrl Pts',(-26.1660218667408,12.9922348070079,
130.198275358319)) ;
#121926 = CARTESIAN_POINT('Ctrl Pts',(-26.2025467695787,13.2501819432392,
130.271891359002)) ;
#121927 = CARTESIAN_POINT('Ctrl Pts',(-26.2160056211235,13.5208713939763,
130.278085368767)) ;
#121928 = CARTESIAN_POINT('Ctrl Pts',(-26.206009335873,13.7852949674506,130.21566252207)) ;
#121929 = CARTESIAN_POINT('Ctrl Pts',(-26.1740705858152,14.0230294711121,
130.089232482416)) ;
#121930 = CARTESIAN_POINT('Ctrl Pts',(-26.1231731249939,14.217815504055,129.907395112279)) ;
#121931 = CARTESIAN_POINT('Ctrl Pts',(-26.0580185278002,14.355293096106,129.684044299522)) ;
#121932 = CARTESIAN_POINT('Ctrl Pts',(-25.983262509313,14.4265292690715,129.43242362093)) ;
#121933 = CARTESIAN_POINT('Ctrl Pts',(-25.9060966194187,14.4257522115435,
129.174057322067)) ;
#121934 = CARTESIAN_POINT('Ctrl Pts',(-25.8315111612316,14.353191154613,128.922957605569)) ;
#121935 = CARTESIAN_POINT('Ctrl Pts',(-25.7664287352936,14.2139748477186,
128.699722439815)) ;
#121936 = CARTESIAN_POINT('Ctrl Pts',(-25.7159572141074,14.0181342342469,
128.519151627063)) ;
#121937 = CARTESIAN_POINT('Ctrl Pts',(-25.6844901245746,13.7796844257176,
128.394105513431)) ;
#121938 = CARTESIAN_POINT('Ctrl Pts',(-25.6750002228921,13.515523516605,128.333239510458)) ;
#121939 = CARTESIAN_POINT('Ctrl Pts',(-25.6888958759568,13.2452125858444,
128.340744783975)) ;
#121940 = CARTESIAN_POINT('Ctrl Pts',(-25.7257689266178,12.9877057714763,
128.415394038105)) ;
#121941 = CARTESIAN_POINT('Ctrl Pts',(-25.7841890846381,12.760206013501,128.55280276842)) ;
#121942 = CARTESIAN_POINT('Ctrl Pts',(-25.8598555926733,12.5817512352831,
128.740846836256)) ;
#121943 = CARTESIAN_POINT('Ctrl Pts',(-25.9488208517265,12.4625557335165,
128.967601700787)) ;
#121944 = CARTESIAN_POINT('Ctrl Pts',(-26.0453904919063,12.4124303702056,
129.216512455731)) ;
#121945 = CARTESIAN_POINT('Ctrl Pts',(-26.1427552661478,12.4345388206878,
129.467894999594)) ;
#121946 = CARTESIAN_POINT('Ctrl Pts',(-26.2357965592368,12.5283216628162,
129.706376449232)) ;
#121947 = CARTESIAN_POINT('Ctrl Pts',(-26.3169003500636,12.6848122547612,
129.910366034385)) ;
#121948 = CARTESIAN_POINT('Ctrl Pts',(-26.3826387576274,12.8954783028643,
130.069177959724)) ;
#121949 = CARTESIAN_POINT('Ctrl Pts',(-26.4280095043964,13.143031226721,130.168655675774)) ;
#121950 = CARTESIAN_POINT('Ctrl Pts',(-26.450935350615,13.4109716015929,130.202504343147)) ;
#121951 = CARTESIAN_POINT('Ctrl Pts',(-26.4504475400349,13.6794256952143,
130.168012298584)) ;
#121952 = CARTESIAN_POINT('Ctrl Pts',(-26.4270028495607,13.9314101071075,
130.066190753789)) ;
#121953 = CARTESIAN_POINT('Ctrl Pts',(-26.3834997753375,14.1445006476294,
129.906112198424)) ;
#121954 = CARTESIAN_POINT('Ctrl Pts',(-26.3235981297211,14.3067536446236,
129.698061730427)) ;
#121955 = CARTESIAN_POINT('Ctrl Pts',(-26.2520620230828,14.4060487060152,
129.455937008284)) ;
#121956 = CARTESIAN_POINT('Ctrl Pts',(-26.174928116071,14.4348548850669,129.197464917097)) ;
#121957 = CARTESIAN_POINT('Ctrl Pts',(-26.0984041323465,14.3909041577753,
128.94074554739)) ;
#121958 = CARTESIAN_POINT('Ctrl Pts',(-26.0290760972212,14.2783347271922,
128.705219923887)) ;
#121959 = CARTESIAN_POINT('Ctrl Pts',(-25.9717745366847,14.1031935059032,
128.504534965738)) ;
#121960 = CARTESIAN_POINT('Ctrl Pts',(-25.9322636718303,13.880010412854,128.356003427703)) ;
#121961 = CARTESIAN_POINT('Ctrl Pts',(-25.9136478323287,13.6249526911944,
128.268597684632)) ;
#121962 = CARTESIAN_POINT('Ctrl Pts',(-25.9179653984303,13.354798949211,128.248097370987)) ;
#121963 = CARTESIAN_POINT('Ctrl Pts',(-25.9455877308256,13.0897726213642,
128.295720076923)) ;
#121964 = CARTESIAN_POINT('Ctrl Pts',(-25.9958936161693,12.8467548703801,
128.409323070075)) ;
#121965 = CARTESIAN_POINT('Ctrl Pts',(-26.0647784470602,12.6478123647641,
128.57762440491)) ;
#121966 = CARTESIAN_POINT('Ctrl Pts',(-26.1492052203305,12.5027971632239,
128.791074301569)) ;
#121967 = CARTESIAN_POINT('Ctrl Pts',(-26.2432329578599,12.4240443471672,
129.032655898126)) ;
#121968 = CARTESIAN_POINT('Ctrl Pts',(-26.3415402813396,12.4170503727496,
129.286553901924)) ;
#121969 = CARTESIAN_POINT('Ctrl Pts',(-26.4363638435478,12.4817914292567,
129.530606090837)) ;
#121970 = CARTESIAN_POINT('Ctrl Pts',(-26.5232308323837,12.6142901362916,
129.751179335933)) ;
#121971 = CARTESIAN_POINT('Ctrl Pts',(-26.59563989411,12.8042104652996,129.929654314528)) ;
#121972 = CARTESIAN_POINT('Ctrl Pts',(-26.6497502115733,13.0388187683455,
130.054583398585)) ;
#121973 = CARTESIAN_POINT('Ctrl Pts',(-26.6820960427729,13.3023286417973,
130.115780574569)) ;
#121974 = CARTESIAN_POINT('Ctrl Pts',(-26.6909894034587,13.571341528554,130.108864472769)) ;
#121975 = CARTESIAN_POINT('Ctrl Pts',(-26.6767021676116,13.8329963549421,
130.0338176991)) ;
#121976 = CARTESIAN_POINT('Ctrl Pts',(-26.6408767843664,14.0635777479953,
129.896055870966)) ;
#121977 = CARTESIAN_POINT('Ctrl Pts',(-26.5871216615792,14.2479537659708,
129.706003217297)) ;
#121978 = CARTESIAN_POINT('Ctrl Pts',(-26.5197195012801,14.3739504814687,
129.476021464279)) ;
#121979 = CARTESIAN_POINT('Ctrl Pts',(-26.4437789239592,14.4320428256961,
129.220888386353)) ;
#121980 = CARTESIAN_POINT('Ctrl Pts',(-26.3663527850407,14.417227489115,128.961592061449)) ;
#121981 = CARTESIAN_POINT('Ctrl Pts',(-26.2935448158709,14.3318166696858,
128.715892691924)) ;
#121982 = CARTESIAN_POINT('Ctrl Pts',(-26.23079022742,14.1811817924182,128.499448823311)) ;
#121983 = CARTESIAN_POINT('Ctrl Pts',(-26.183588181247,13.9759967234678,128.328412475923)) ;
#121984 = CARTESIAN_POINT('Ctrl Pts',(-26.1560379678286,13.7313492030733,
128.214805352919)) ;
#121985 = CARTESIAN_POINT('Ctrl Pts',(-26.1509807959761,13.4634560829624,
128.166765320148)) ;
#121986 = CARTESIAN_POINT('Ctrl Pts',(-26.1691472957076,13.1958849143636,
128.186976695918)) ;
#121987 = CARTESIAN_POINT('Ctrl Pts',(-26.2104817509094,12.9412336892527,
128.274433943599)) ;
#121988 = CARTESIAN_POINT('Ctrl Pts',(-26.2721716135339,12.7230235102752,
128.421620019773)) ;
#121989 = CARTESIAN_POINT('Ctrl Pts',(-26.3510948457971,12.5539648148601,
128.618984638309)) ;
#121990 = CARTESIAN_POINT('Ctrl Pts',(-26.4416854984019,12.4477725883293,
128.850585921141)) ;
#121991 = CARTESIAN_POINT('Ctrl Pts',(-26.5388603867134,12.4110238127138,
129.101295822546)) ;
#121992 = CARTESIAN_POINT('Ctrl Pts',(-26.6359779446456,12.4468710240649,
129.351877582573)) ;
#121993 = CARTESIAN_POINT('Ctrl Pts',(-26.7271512360903,12.5531554013667,
129.584988732517)) ;
#121994 = CARTESIAN_POINT('Ctrl Pts',(-26.8058876475167,12.7211113727201,
129.781943258164)) ;
#121995 = CARTESIAN_POINT('Ctrl Pts',(-26.867958160108,12.9400020484962,129.930089354973)) ;
#121996 = CARTESIAN_POINT('Ctrl Pts',(-26.9091588040755,13.1921120918715,
130.017459671564)) ;
#121997 = CARTESIAN_POINT('Ctrl Pts',(-26.9277711979778,13.4620045892925,
130.038672040359)) ;
#121998 = CARTESIAN_POINT('Ctrl Pts',(-26.9228008675889,13.7292706883455,
129.990975910418)) ;
#121999 = CARTESIAN_POINT('Ctrl Pts',(-26.8955075945293,13.9738126531135,
129.878168064945)) ;
#122000 = CARTESIAN_POINT('Ctrl Pts',(-26.8485030327011,14.179494761427,129.707716653188)) ;
#122001 = CARTESIAN_POINT('Ctrl Pts',(-26.7855978873256,14.3311259562621,
129.490701648116)) ;
#122002 = CARTESIAN_POINT('Ctrl Pts',(-26.7129553496451,14.4169205750236,
129.24554392929)) ;
#122003 = CARTESIAN_POINT('Ctrl Pts',(-26.6352142982145,14.4320030262707,
128.98518159896)) ;
#122004 = CARTESIAN_POINT('Ctrl Pts',(-26.5599753455434,14.3751243416082,
128.732432725729)) ;
#122005 = CARTESIAN_POINT('Ctrl Pts',(-26.491906908084,14.2488767663409,128.500232903427)) ;
#122006 = CARTESIAN_POINT('Ctrl Pts',(-26.4381398546264,14.0648018016439,
128.310179587544)) ;
#122007 = CARTESIAN_POINT('Ctrl Pts',(-26.4022035176628,13.8343787612975,
128.17207828747)) ;
#122008 = CARTESIAN_POINT('Ctrl Pts',(-26.3877376570125,13.57360703546,128.096606127826)) ;
#122009 = CARTESIAN_POINT('Ctrl Pts',(-26.3966428099618,13.3025524242793,
128.089467724452)) ;
#122010 = CARTESIAN_POINT('Ctrl Pts',(-26.4285388264674,13.0417944958654,
128.149713107354)) ;
#122011 = CARTESIAN_POINT('Ctrl Pts',(-26.4824445567047,12.8063139825281,
128.273986576365)) ;
#122012 = CARTESIAN_POINT('Ctrl Pts',(-26.5547260838546,12.6158856325691,
128.452084531992)) ;
#122013 = CARTESIAN_POINT('Ctrl Pts',(-26.6416219728868,12.4825396581066,
128.672687777498)) ;
#122014 = CARTESIAN_POINT('Ctrl Pts',(-26.7365473365606,12.4173081126312,
128.916989601117)) ;
#122015 = CARTESIAN_POINT('Ctrl Pts',(-26.8344661154599,12.4236050164849,
129.169887633563)) ;
#122016 = CARTESIAN_POINT('Ctrl Pts',(-26.9287291207569,12.5018026361359,
129.4120930787)) ;
#122017 = CARTESIAN_POINT('Ctrl Pts',(-27.0131217845774,12.6458566369947,
129.625516102499)) ;
#122018 = CARTESIAN_POINT('Ctrl Pts',(-27.0824647965145,12.8453791511498,
129.794993955093)) ;
#122019 = CARTESIAN_POINT('Ctrl Pts',(-27.1326350432609,13.0865653368531,
129.908416385334)) ;
#122020 = CARTESIAN_POINT('Ctrl Pts',(-27.1606365627051,13.3521428238873,
129.957049192237)) ;
#122021 = CARTESIAN_POINT('Ctrl Pts',(-27.1651689294827,13.6222557770976,
129.93719049098)) ;
#122022 = CARTESIAN_POINT('Ctrl Pts',(-27.1467153752729,13.878388340665,129.850152045609)) ;
#122023 = CARTESIAN_POINT('Ctrl Pts',(-27.1071678329421,14.1022120909712,
129.701435023225)) ;
#122024 = CARTESIAN_POINT('Ctrl Pts',(-27.0504028748614,14.2765229673721,
129.502557758353)) ;
#122025 = CARTESIAN_POINT('Ctrl Pts',(-26.9810910649829,14.3902287028563,
129.267020257534)) ;
#122026 = CARTESIAN_POINT('Ctrl Pts',(-26.9043059277822,14.4347769425123,
129.009416197046)) ;
#122027 = CARTESIAN_POINT('Ctrl Pts',(-26.8275120953152,14.406672259026,128.752091523846)) ;
#122028 = CARTESIAN_POINT('Ctrl Pts',(-26.7558435515678,14.3082119103095,
128.509567117461)) ;
#122029 = CARTESIAN_POINT('Ctrl Pts',(-26.6956342816198,14.146035786889,128.300525349841)) ;
#122030 = CARTESIAN_POINT('Ctrl Pts',(-26.6519469354556,13.9328084599434,
128.139848548639)) ;
#122031 = CARTESIAN_POINT('Ctrl Pts',(-26.6284335363191,13.6817741285683,
128.037926381176)) ;
#122032 = CARTESIAN_POINT('Ctrl Pts',(-26.627674518559,13.4140262407359,128.002715819442)) ;
#122033 = CARTESIAN_POINT('Ctrl Pts',(-26.6504162861654,13.1453688481844,
128.035950834501)) ;
#122034 = CARTESIAN_POINT('Ctrl Pts',(-26.6955480888432,12.8977836730895,
128.134762681728)) ;
#122035 = CARTESIAN_POINT('Ctrl Pts',(-26.7612516854397,12.6861562581584,
128.293396651609)) ;
#122036 = CARTESIAN_POINT('Ctrl Pts',(-26.8425418015955,12.5289208542769,
128.497830773323)) ;
#122037 = CARTESIAN_POINT('Ctrl Pts',(-26.9351615000927,12.43515491016,128.735214369181)) ;
#122038 = CARTESIAN_POINT('Ctrl Pts',(-27.0323345672073,12.4122393521451,
128.986094141453)) ;
#122039 = CARTESIAN_POINT('Ctrl Pts',(-27.1292337281549,12.461921394401,129.235865336576)) ;
#122040 = CARTESIAN_POINT('Ctrl Pts',(-27.2181630496938,12.5803996881322,
129.462565138042)) ;
#122041 = CARTESIAN_POINT('Ctrl Pts',(-27.2941848507928,12.7591299511845,
129.651530481398)) ;
#122042 = CARTESIAN_POINT('Ctrl Pts',(-27.3524160962972,12.9850687744513,
129.788575819063)) ;
#122043 = CARTESIAN_POINT('Ctrl Pts',(-27.3895887844412,13.2423777832249,
129.864086182952)) ;
#122044 = CARTESIAN_POINT('Ctrl Pts',(-27.4037202433593,13.5129449874981,
129.872246514025)) ;
#122045 = CARTESIAN_POINT('Ctrl Pts',(-27.3944549137884,13.7774321466873,
129.812018614547)) ;
#122046 = CARTESIAN_POINT('Ctrl Pts',(-27.3630500859143,14.0166134840393,
129.687079327019)) ;
#122047 = CARTESIAN_POINT('Ctrl Pts',(-27.3129661381804,14.2120831170415,
129.507790243548)) ;
#122048 = CARTESIAN_POINT('Ctrl Pts',(-27.2477111859512,14.3524989582878,
129.283900035096)) ;
#122049 = CARTESIAN_POINT('Ctrl Pts',(-27.1733683419627,14.4253825851082,
129.033603144489)) ;
#122050 = CARTESIAN_POINT('Ctrl Pts',(-27.0960794174057,14.4267682802424,
128.774817103346)) ;
#122051 = CARTESIAN_POINT('Ctrl Pts',(-27.0214960019201,14.3564919766321,
128.523812290043)) ;
#122052 = CARTESIAN_POINT('Ctrl Pts',(-26.9558285638099,14.2186718710266,
128.298750545118)) ;
#122053 = CARTESIAN_POINT('Ctrl Pts',(-26.9049226632705,14.024316702861,128.116933923083)) ;
#122054 = CARTESIAN_POINT('Ctrl Pts',(-26.8728650693728,13.7866135128635,
127.990131547778)) ;
#122055 = CARTESIAN_POINT('Ctrl Pts',(-26.8627445051173,13.5238036073327,
127.927533017912)) ;
#122056 = CARTESIAN_POINT('Ctrl Pts',(-26.8759282572692,13.2527085149488,
127.932875171152)) ;
#122057 = CARTESIAN_POINT('Ctrl Pts',(-26.9124124688024,12.9936529878453,
128.006256802744)) ;
#122058 = CARTESIAN_POINT('Ctrl Pts',(-26.9700245887179,12.7662441294868,
128.141471141094)) ;
#122059 = CARTESIAN_POINT('Ctrl Pts',(-27.0453501773252,12.5858801023732,
128.328462165356)) ;
#122060 = CARTESIAN_POINT('Ctrl Pts',(-27.1340923349453,12.4648530530782,
128.554546945788)) ;
#122061 = CARTESIAN_POINT('Ctrl Pts',(-27.2306903180176,12.4128201852834,
128.803491256227)) ;
#122062 = CARTESIAN_POINT('Ctrl Pts',(-27.3277245909402,12.4330274205639,
129.054033267904)) ;
#122063 = CARTESIAN_POINT('Ctrl Pts',(-27.420587314234,12.5240123419654,129.292155039348)) ;
#122064 = CARTESIAN_POINT('Ctrl Pts',(-27.5026088157967,12.6795221471728,
129.4986303408)) ;
#122065 = CARTESIAN_POINT('Ctrl Pts',(-27.56880507535,12.8889214300487,129.658790927613)) ;
#122066 = CARTESIAN_POINT('Ctrl Pts',(-27.614815972317,13.1354947204779,129.760149867447)) ;
#122067 = CARTESIAN_POINT('Ctrl Pts',(-27.6384438856448,13.4042911484909,
129.795909071005)) ;
#122068 = CARTESIAN_POINT('Ctrl Pts',(-27.638531524892,13.6719452324486,129.763222402758)) ;
#122069 = CARTESIAN_POINT('Ctrl Pts',(-27.6158224189632,13.9242175313922,
129.663622850511)) ;
#122070 = CARTESIAN_POINT('Ctrl Pts',(-27.572798679322,14.1390288718251,129.504884677249)) ;
#122071 = CARTESIAN_POINT('Ctrl Pts',(-27.513252891317,14.3030286134432,129.297851793418)) ;
#122072 = CARTESIAN_POINT('Ctrl Pts',(-27.4419265027612,14.404195333154,129.056326335695)) ;
#122073 = CARTESIAN_POINT('Ctrl Pts',(-27.3651061813518,14.4349854783543,
128.79887103993)) ;
#122074 = CARTESIAN_POINT('Ctrl Pts',(-27.2884597326731,14.3934046860553,
128.541796190572)) ;
#122075 = CARTESIAN_POINT('Ctrl Pts',(-27.2186122844583,14.2822103029933,
128.304629732468)) ;
#122076 = CARTESIAN_POINT('Ctrl Pts',(-27.1612236221931,14.1097942178576,
128.103897060506)) ;
#122077 = CARTESIAN_POINT('Ctrl Pts',(-27.1209695384075,13.8877666791924,
127.953145883014)) ;
#122078 = CARTESIAN_POINT('Ctrl Pts',(-27.1016395309341,13.6324083997063,
127.863526650496)) ;
#122079 = CARTESIAN_POINT('Ctrl Pts',(-27.1052954562786,13.3624184985193,
127.841099006874)) ;
#122080 = CARTESIAN_POINT('Ctrl Pts',(-27.1323671349213,13.0965814202268,
127.887054838906)) ;
#122081 = CARTESIAN_POINT('Ctrl Pts',(-27.1817582727546,12.8540735599423,
127.99818617381)) ;
#122082 = CARTESIAN_POINT('Ctrl Pts',(-27.2501946458088,12.6529923851621,
128.165102805726)) ;
#122083 = CARTESIAN_POINT('Ctrl Pts',(-27.3347670251361,12.5055873938463,
128.378795585395)) ;
#122084 = CARTESIAN_POINT('Ctrl Pts',(-27.4281737202757,12.4255318492028,
128.618720146286)) ;
#122085 = CARTESIAN_POINT('Ctrl Pts',(-27.5260110615558,12.41606276029,128.871394756553)) ;
#122086 = CARTESIAN_POINT('Ctrl Pts',(-27.6214751824357,12.478829942444,129.117158137395)) ;
#122087 = CARTESIAN_POINT('Ctrl Pts',(-27.7087309583013,12.6096603386007,
129.338843492308)) ;
#122088 = CARTESIAN_POINT('Ctrl Pts',(-27.7817420501725,12.7985462969973,
129.519009420162)) ;
#122089 = CARTESIAN_POINT('Ctrl Pts',(-27.8362342975662,13.0317087125592,
129.645126399872)) ;
#122090 = CARTESIAN_POINT('Ctrl Pts',(-27.8691744514199,13.2930836864475,
129.708250616972)) ;
#122091 = CARTESIAN_POINT('Ctrl Pts',(-27.8788768367921,13.5641925745626,
129.70344323476)) ;
#122092 = CARTESIAN_POINT('Ctrl Pts',(-27.8651790612343,13.8256807565213,
129.630204378494)) ;
#122093 = CARTESIAN_POINT('Ctrl Pts',(-27.8301586837401,14.0565823950309,
129.494921896745)) ;
#122094 = CARTESIAN_POINT('Ctrl Pts',(-27.7767369569256,14.2434411721512,
129.305720870279)) ;
#122095 = CARTESIAN_POINT('Ctrl Pts',(-27.7093477667888,14.3714533932326,
129.075650866819)) ;
#122096 = CARTESIAN_POINT('Ctrl Pts',(-27.6341917569376,14.4311593781317,
128.823088377139)) ;
#122097 = CARTESIAN_POINT('Ctrl Pts',(-27.5565394264049,14.4188767221607,
128.563046725448)) ;
#122098 = CARTESIAN_POINT('Ctrl Pts',(-27.4833555543512,14.3353893492018,
128.316188475308)) ;
#122099 = CARTESIAN_POINT('Ctrl Pts',(-27.4200615928807,14.1858865785186,
128.098061220149)) ;
#122100 = CARTESIAN_POINT('Ctrl Pts',(-27.3725451189786,13.982932266947,127.926249851755)) ;
#122101 = CARTESIAN_POINT('Ctrl Pts',(-27.3443171583994,13.7386001468469,
127.81057521293)) ;
#122102 = CARTESIAN_POINT('Ctrl Pts',(-27.3385532435846,13.472491032427,127.760647208021)) ;
#122103 = CARTESIAN_POINT('Ctrl Pts',(-27.3561183196159,13.2027754330182,
127.778859895872)) ;
#122104 = CARTESIAN_POINT('Ctrl Pts',(-27.3969178375316,12.947572926699,127.864767200057)) ;
#122105 = CARTESIAN_POINT('Ctrl Pts',(-27.4579595443552,12.7286906750514,
128.010126305813)) ;
#122106 = CARTESIAN_POINT('Ctrl Pts',(-27.536242792453,12.5582194191414,128.205697792925)) ;
#122107 = CARTESIAN_POINT('Ctrl Pts',(-27.6270550381186,12.4495814743775,
128.437768406524)) ;
#122108 = CARTESIAN_POINT('Ctrl Pts',(-27.7239408227956,12.4111325032394,
128.687708168369)) ;
#122109 = CARTESIAN_POINT('Ctrl Pts',(-27.8209192941087,12.4448573223553,
128.937954006686)) ;
#122110 = CARTESIAN_POINT('Ctrl Pts',(-27.912140970553,12.5485736252265,129.171305648138)) ;
#122111 = CARTESIAN_POINT('Ctrl Pts',(-27.9918422589982,12.7160675406203,
129.370845077553)) ;
#122112 = CARTESIAN_POINT('Ctrl Pts',(-28.0541095191813,12.9327061663297,
129.519736214929)) ;
#122113 = CARTESIAN_POINT('Ctrl Pts',(-28.0961114867268,13.1846668461228,
129.609355795154)) ;
#122114 = CARTESIAN_POINT('Ctrl Pts',(-28.1153430533785,13.4544224662781,
129.632372704712)) ;
#122115 = CARTESIAN_POINT('Ctrl Pts',(-28.1110671408469,13.7215757501031,
129.586762859001)) ;
#122116 = CARTESIAN_POINT('Ctrl Pts',(-28.0843498664941,13.9674106040572,
129.475585032641)) ;
#122117 = CARTESIAN_POINT('Ctrl Pts',(-28.037929043125,14.1739595566239,129.306902469622)) ;
#122118 = CARTESIAN_POINT('Ctrl Pts',(-27.9756458993413,14.3272529144105,
129.091797948064)) ;
#122119 = CARTESIAN_POINT('Ctrl Pts',(-27.902736501693,14.4155298054197,128.845637413294)) ;
#122120 = CARTESIAN_POINT('Ctrl Pts',(-27.8255218107392,14.4326688880929,
128.587029784971)) ;
#122121 = CARTESIAN_POINT('Ctrl Pts',(-27.7496698410169,14.3775210612736,
128.332273988261)) ;
#122122 = CARTESIAN_POINT('Ctrl Pts',(-27.6817779587366,14.2540409039206,
128.10083691294)) ;
#122123 = CARTESIAN_POINT('Ctrl Pts',(-27.6272334434837,14.0709647731437,
127.908361698852)) ;
#122124 = CARTESIAN_POINT('Ctrl Pts',(-27.590771642816,13.8416199051522,127.768737814126)) ;
#122125 = CARTESIAN_POINT('Ctrl Pts',(-27.575654232938,13.5823884703292,127.691471326001)) ;
#122126 = CARTESIAN_POINT('Ctrl Pts',(-27.5837290890939,13.3112803473401,
127.681899023074)) ;
#122127 = CARTESIAN_POINT('Ctrl Pts',(-27.6151958140633,13.0483997002377,
127.740682725908)) ;
#122128 = CARTESIAN_POINT('Ctrl Pts',(-27.6682760357924,12.8130297532618,
127.862704973521)) ;
#122129 = CARTESIAN_POINT('Ctrl Pts',(-27.7402747174842,12.6204060162552,
128.039867549227)) ;
#122130 = CARTESIAN_POINT('Ctrl Pts',(-27.8268049555487,12.4854478919258,
128.259425965447)) ;
#122131 = CARTESIAN_POINT('Ctrl Pts',(-27.9215833060717,12.4181326606572,
128.503289393107)) ;
#122132 = CARTESIAN_POINT('Ctrl Pts',(-28.0197801582564,12.4224942646145,
128.756911867378)) ;
#122133 = CARTESIAN_POINT('Ctrl Pts',(-28.1141333474196,12.4989653492952,
128.99940414225)) ;
#122134 = CARTESIAN_POINT('Ctrl Pts',(-28.1985201718138,12.6405920086238,
129.212953820927)) ;
#122135 = CARTESIAN_POINT('Ctrl Pts',(-28.26860111647,12.8391594148647,129.384491828424)) ;
#122136 = CARTESIAN_POINT('Ctrl Pts',(-28.3194453499789,13.0802460396382,
129.499785089664)) ;
#122137 = CARTESIAN_POINT('Ctrl Pts',(-28.3479518760318,13.3449462912613,
129.549955580643)) ;
#122138 = CARTESIAN_POINT('Ctrl Pts',(-28.3531447899655,13.614299734848,129.532134045205)) ;
#122139 = CARTESIAN_POINT('Ctrl Pts',(-28.3353747732206,13.8710421702277,
129.447102522243)) ;
#122140 = CARTESIAN_POINT('Ctrl Pts',(-28.29643056891,14.0962488627573,129.300139789109)) ;
#122141 = CARTESIAN_POINT('Ctrl Pts',(-28.239735048489,14.272991429521,129.10127534637)) ;
#122142 = CARTESIAN_POINT('Ctrl Pts',(-28.171042991182,14.3876795568682,128.867727126792)) ;
#122143 = CARTESIAN_POINT('Ctrl Pts',(-28.0945098708047,14.4346057862448,
128.610910309842)) ;
#122144 = CARTESIAN_POINT('Ctrl Pts',(-28.0172199102355,14.4082599424993,
128.351948838014)) ;
#122145 = CARTESIAN_POINT('Ctrl Pts',(-27.945755360923,14.3122705822436,128.110224199333)) ;
#122146 = CARTESIAN_POINT('Ctrl Pts',(-27.8848607524878,14.1514361820495,
127.89905904971)) ;
#122147 = CARTESIAN_POINT('Ctrl Pts',(-27.8406503955374,13.9387188784373,
127.736773571724)) ;
#122148 = CARTESIAN_POINT('Ctrl Pts',(-27.8166293155747,13.6904434149952,
127.63362073482)) ;
#122149 = CARTESIAN_POINT('Ctrl Pts',(-27.8151767965197,13.4208420632377,
127.596115768567)) ;
#122150 = CARTESIAN_POINT('Ctrl Pts',(-27.8371800049029,13.1534853920285,
127.627393021463)) ;
#122151 = CARTESIAN_POINT('Ctrl Pts',(-27.8817255227419,12.9044050276542,
127.724409631791)) ;
#122152 = CARTESIAN_POINT('Ctrl Pts',(-27.9469701066089,12.691347593862,127.881682377476)) ;
#122153 = CARTESIAN_POINT('Ctrl Pts',(-28.027963628144,12.5324268950077,128.085219224786)) ;
#122154 = CARTESIAN_POINT('Ctrl Pts',(-28.1200287328796,12.4369854895294,
128.321097685028)) ;
#122155 = CARTESIAN_POINT('Ctrl Pts',(-28.2173464985682,12.4119049764517,
128.572326876044)) ;
#122156 = CARTESIAN_POINT('Ctrl Pts',(-28.3140197030252,12.4592885985088,
128.821560747272)) ;
#122157 = CARTESIAN_POINT('Ctrl Pts',(-28.4033508529203,12.575733706437,129.049405146958)) ;
#122158 = CARTESIAN_POINT('Ctrl Pts',(-28.4798796992957,12.7527803278304,
129.239845940824)) ;
#122159 = CARTESIAN_POINT('Ctrl Pts',(-28.5389784527639,12.9786618836061,
129.379263313413)) ;
#122160 = CARTESIAN_POINT('Ctrl Pts',(-28.5767125295995,13.2359089048801,
129.456355493055)) ;
#122161 = CARTESIAN_POINT('Ctrl Pts',(-28.5914322564073,13.5051027063819,
129.466392895388)) ;
#122162 = CARTESIAN_POINT('Ctrl Pts',(-28.5827452242765,13.771120969237,129.407710773932)) ;
#122163 = CARTESIAN_POINT('Ctrl Pts',(-28.5520458960196,14.0100004351276,
129.285003580461)) ;
#122164 = CARTESIAN_POINT('Ctrl Pts',(-28.5023750590468,14.2073725024461,
129.106849407342)) ;
#122165 = CARTESIAN_POINT('Ctrl Pts',(-28.4375690543573,14.3492226720416,
128.884331903099)) ;
#122166 = CARTESIAN_POINT('Ctrl Pts',(-28.3635165159496,14.4242520037555,
128.634920057826)) ;
#122167 = CARTESIAN_POINT('Ctrl Pts',(-28.2858996813637,14.4277364435235,
128.375036176081)) ;
#122168 = CARTESIAN_POINT('Ctrl Pts',(-28.2112539541308,14.3592419699784,
128.123884396452)) ;
#122169 = CARTESIAN_POINT('Ctrl Pts',(-28.1455253888997,14.2240686259208,
127.898803886575)) ;
#122170 = CARTESIAN_POINT('Ctrl Pts',(-28.0939162702605,14.0305584607837,
127.714807716224)) ;
#122171 = CARTESIAN_POINT('Ctrl Pts',(-28.061332463252,13.7945205251559,127.586559380918)) ;
#122172 = CARTESIAN_POINT('Ctrl Pts',(-28.0504816310014,13.5313066856814,
127.521709190659)) ;
#122173 = CARTESIAN_POINT('Ctrl Pts',(-28.0630246250275,13.2605191131678,
127.525225826364)) ;
#122174 = CARTESIAN_POINT('Ctrl Pts',(-28.0986987267832,13.0015410285169,
127.596334676114)) ;
#122175 = CARTESIAN_POINT('Ctrl Pts',(-28.1557429004217,12.7725523248786,
127.729845571357)) ;
#122176 = CARTESIAN_POINT('Ctrl Pts',(-28.2308151450779,12.5901313640957,
127.916009506223)) ;
#122177 = CARTESIAN_POINT('Ctrl Pts',(-28.3192039621127,12.4675131143056,
128.141087303876)) ;
#122178 = CARTESIAN_POINT('Ctrl Pts',(-28.4152292054608,12.4133289099041,
128.388505252399)) ;
#122179 = CARTESIAN_POINT('Ctrl Pts',(-28.51300012079,12.4315113584402,128.64096395705)) ;
#122180 = CARTESIAN_POINT('Ctrl Pts',(-28.6057703554483,12.5204618944922,
128.878923702572)) ;
#122181 = CARTESIAN_POINT('Ctrl Pts',(-28.6881745533434,12.6740885855686,
129.086523806388)) ;
#122182 = CARTESIAN_POINT('Ctrl Pts',(-28.7549081392456,12.8820605871686,
129.248262102328)) ;
#122183 = CARTESIAN_POINT('Ctrl Pts',(-28.8015673967949,13.1280849227168,
129.351472289244)) ;
#122184 = CARTESIAN_POINT('Ctrl Pts',(-28.8258432151059,13.3954305595711,
129.389263233344)) ;
#122185 = CARTESIAN_POINT('Ctrl Pts',(-28.8266274541713,13.664772130159,129.358428105594)) ;
#122186 = CARTESIAN_POINT('Ctrl Pts',(-28.8046464651445,13.916650368435,129.261114435001)) ;
#122187 = CARTESIAN_POINT('Ctrl Pts',(-28.7621302419893,14.1333087809813,
129.103782522449)) ;
#122188 = CARTESIAN_POINT('Ctrl Pts',(-28.7030824646286,14.2989356818664,
128.898242342101)) ;
#122189 = CARTESIAN_POINT('Ctrl Pts',(-28.6315878673714,14.4025578141661,
128.656030107433)) ;
#122190 = CARTESIAN_POINT('Ctrl Pts',(-28.5551034289532,14.4350103980761,
128.399673764832)) ;
#122191 = CARTESIAN_POINT('Ctrl Pts',(-28.4784248234603,14.3956728073431,
128.142535589966)) ;
#122192 = CARTESIAN_POINT('Ctrl Pts',(-28.4082689021954,14.2862787528374,
127.904446866476)) ;
#122193 = CARTESIAN_POINT('Ctrl Pts',(-28.3504831872354,14.1158603426533,
127.702603041365)) ;
#122194 = CARTESIAN_POINT('Ctrl Pts',(-28.3094811784105,13.8934485150928,
127.549446047251)) ;
#122195 = CARTESIAN_POINT('Ctrl Pts',(-28.2896953739857,13.6404741079279,
127.458725935806)) ;
#122196 = CARTESIAN_POINT('Ctrl Pts',(-28.2926725255243,13.3695006911583,
127.434168724953)) ;
#122197 = CARTESIAN_POINT('Ctrl Pts',(-28.3190303266563,13.1044456788723,
127.478181906027)) ;
#122198 = CARTESIAN_POINT('Ctrl Pts',(-28.3677161485524,12.8607039818763,
127.587239387159)) ;
#122199 = CARTESIAN_POINT('Ctrl Pts',(-28.436248601719,12.6571154322834,127.754197746226)) ;
#122200 = CARTESIAN_POINT('Ctrl Pts',(-28.519396273585,12.509808022699,127.964148826798)) ;
#122201 = CARTESIAN_POINT('Ctrl Pts',(-28.6131255277483,12.4266891378063,
128.204805011976)) ;
#122202 = CARTESIAN_POINT('Ctrl Pts',(-28.7112079392635,12.4154229833254,
128.458110282106)) ;
#122203 = CARTESIAN_POINT('Ctrl Pts',(-28.8064841551431,12.4759771003581,
128.703440260766)) ;
#122204 = CARTESIAN_POINT('Ctrl Pts',(-28.894082157132,12.6048252979973,128.92612571075)) ;
#122205 = CARTESIAN_POINT('Ctrl Pts',(-28.9676084232411,12.792164644416,129.10779157021)) ;
#122206 = CARTESIAN_POINT('Ctrl Pts',(-29.0227856027514,13.0247863190839,
129.235835629259)) ;
#122207 = CARTESIAN_POINT('Ctrl Pts',(-29.0563556978844,13.2853106439738,
129.300842762572)) ;
#122208 = CARTESIAN_POINT('Ctrl Pts',(-29.066673658485,13.5574332084958,129.297702546237)) ;
#122209 = CARTESIAN_POINT('Ctrl Pts',(-29.0537954995477,13.8171022396022,
129.22717000876)) ;
#122210 = CARTESIAN_POINT('Ctrl Pts',(-29.0191433426595,14.051173953077,129.092681320874)) ;
#122211 = CARTESIAN_POINT('Ctrl Pts',(-28.9661997934839,14.2388282531697,
128.904948271921)) ;
#122212 = CARTESIAN_POINT('Ctrl Pts',(-28.8993924137718,14.3685839592775,
128.676682134356)) ;
#122213 = CARTESIAN_POINT('Ctrl Pts',(-28.8238015023144,14.4305511556418,
128.422593404806)) ;
#122214 = CARTESIAN_POINT('Ctrl Pts',(-28.7466935435304,14.4203097239978,
128.164395594464)) ;
#122215 = CARTESIAN_POINT('Ctrl Pts',(-28.6729565347358,14.3384207836783,
127.915751318186)) ;
#122216 = CARTESIAN_POINT('Ctrl Pts',(-28.6096196405582,14.1915731436481,
127.697694520971)) ;
#122217 = CARTESIAN_POINT('Ctrl Pts',(-28.5612220772461,13.9880714714153,
127.523004005157)) ;
#122218 = CARTESIAN_POINT('Ctrl Pts',(-28.5327231257182,13.7471725052838,
127.406897590129)) ;
#122219 = CARTESIAN_POINT('Ctrl Pts',(-28.5261588350729,13.4800206037099,
127.354436040776)) ;
#122220 = CARTESIAN_POINT('Ctrl Pts',(-28.5430314034632,13.2110030429649,
127.370738064937)) ;
#122221 = CARTESIAN_POINT('Ctrl Pts',(-28.5831526985241,12.9547748927777,
127.454630608314)) ;
#122222 = CARTESIAN_POINT('Ctrl Pts',(-28.6436998125845,12.7344342247069,
127.598514032658)) ;
#122223 = CARTESIAN_POINT('Ctrl Pts',(-28.7215842030367,12.5623453660856,
127.792909823269)) ;
#122224 = CARTESIAN_POINT('Ctrl Pts',(-28.8119292432189,12.4518692088092,
128.023682354771)) ;
#122225 = CARTESIAN_POINT('Ctrl Pts',(-28.9089970305816,12.4112334911996,
128.274053197857)) ;
#122226 = CARTESIAN_POINT('Ctrl Pts',(-29.0059571272688,12.442749147776,128.524289458661)) ;
#122227 = CARTESIAN_POINT('Ctrl Pts',(-29.0979629404732,12.5456206773071,
128.759711132298)) ;
#122228 = CARTESIAN_POINT('Ctrl Pts',(-29.1770171698936,12.7091960236905,
128.957812071618)) ;
#122229 = CARTESIAN_POINT('Ctrl Pts',(-29.2404374453014,12.9259029773537,
129.109812864898)) ;
#122230 = CARTESIAN_POINT('Ctrl Pts',(-29.2829880269622,13.1770736237047,
129.201057279156)) ;
#122231 = CARTESIAN_POINT('Ctrl Pts',(-29.3029145413432,13.4468768400015,
129.226065673819)) ;
#122232 = CARTESIAN_POINT('Ctrl Pts',(-29.2992993295531,13.7138795897728,
129.182448022358)) ;
#122233 = CARTESIAN_POINT('Ctrl Pts',(-29.273233977091,13.9605431985016,129.073181644377)) ;
#122234 = CARTESIAN_POINT('Ctrl Pts',(-29.2273578624926,14.1686235654109,
128.906083428739)) ;
#122235 = CARTESIAN_POINT('Ctrl Pts',(-29.1651531009933,14.324111284162,128.691062013158)) ;
#122236 = CARTESIAN_POINT('Ctrl Pts',(-29.0928693974923,14.4138215880485,
128.446919954995)) ;
#122237 = CARTESIAN_POINT('Ctrl Pts',(-29.0154061666861,14.4331945050443,
128.187453589773)) ;
#122238 = CARTESIAN_POINT('Ctrl Pts',(-28.9396480617869,14.3801614626116,
127.933074508633)) ;
#122239 = CARTESIAN_POINT('Ctrl Pts',(-28.871348616006,14.2584942565519,127.70040173552)) ;
#122240 = CARTESIAN_POINT('Ctrl Pts',(-28.816378809689,14.0770491380578,127.506702993462)) ;
#122241 = CARTESIAN_POINT('Ctrl Pts',(-28.7792697685908,13.8484874642558,
127.365136455592)) ;
#122242 = CARTESIAN_POINT('Ctrl Pts',(-28.7635626541173,13.5893549989453,
127.286091315825)) ;
#122243 = CARTESIAN_POINT('Ctrl Pts',(-28.7709351586529,13.319692173746,127.274636454019)) ;
#122244 = CARTESIAN_POINT('Ctrl Pts',(-28.8016628955735,13.0561133199218,
127.331243888594)) ;
#122245 = CARTESIAN_POINT('Ctrl Pts',(-28.8542955948744,12.8190740737043,
127.451871104289)) ;
#122246 = CARTESIAN_POINT('Ctrl Pts',(-28.9257721083705,12.6252975626819,
127.627540714235)) ;
#122247 = CARTESIAN_POINT('Ctrl Pts',(-29.0116152850741,12.4887796662223,
127.845210673493)) ;
#122248 = CARTESIAN_POINT('Ctrl Pts',(-29.1065799591714,12.4190606373648,
128.089488486785)) ;
#122249 = CARTESIAN_POINT('Ctrl Pts',(-29.2044154397174,12.4213023433048,
128.342181133046)) ;
#122250 = CARTESIAN_POINT('Ctrl Pts',(-29.2990096465751,12.4953372710628,
128.585372578871)) ;
#122251 = CARTESIAN_POINT('Ctrl Pts',(-29.3841743519178,12.6358733450884,
128.801032099907)) ;
#122252 = CARTESIAN_POINT('Ctrl Pts',(-29.4545133975427,12.8325870207608,
128.973414377414)) ;
#122253 = CARTESIAN_POINT('Ctrl Pts',(-29.5058639057111,13.0715963225307,
129.090313702067)) ;
#122254 = CARTESIAN_POINT('Ctrl Pts',(-29.5352417115144,13.336692941588,129.142915133705)) ;
#122255 = CARTESIAN_POINT('Ctrl Pts',(-29.5411110857573,13.6067854476423,
129.126995341538)) ;
#122256 = CARTESIAN_POINT('Ctrl Pts',(-29.5239546110153,13.8640947363139,
129.043762287714)) ;
#122257 = CARTESIAN_POINT('Ctrl Pts',(-29.4857056732189,14.089839779911,128.898926454628)) ;
#122258 = CARTESIAN_POINT('Ctrl Pts',(-29.4295331965174,14.2683601910573,
128.701597333411)) ;
#122259 = CARTESIAN_POINT('Ctrl Pts',(-29.360862541889,14.385487730189,128.467980808694)) ;
#122260 = CARTESIAN_POINT('Ctrl Pts',(-29.2843675405681,14.4341894586694,
128.211244603888)) ;
#122261 = CARTESIAN_POINT('Ctrl Pts',(-29.2074361909077,14.4102459791679,
127.953517340241)) ;
#122262 = CARTESIAN_POINT('Ctrl Pts',(-29.1353314148325,14.3157190447574,
127.709734613321)) ;
#122263 = CARTESIAN_POINT('Ctrl Pts',(-29.0743992312775,14.1574302898824,
127.498651642287)) ;
#122264 = CARTESIAN_POINT('Ctrl Pts',(-29.0294533466867,13.9458829058386,
127.334150515467)) ;
#122265 = CARTESIAN_POINT('Ctrl Pts',(-29.0047556089691,13.6969896283466,
127.228845194687)) ;
#122266 = CARTESIAN_POINT('Ctrl Pts',(-29.002697162624,13.4292803806108,127.189768555857)) ;
#122267 = CARTESIAN_POINT('Ctrl Pts',(-29.0238997906195,13.1613091083809,
127.21867643542)) ;
#122268 = CARTESIAN_POINT('Ctrl Pts',(-29.0683112780447,12.9096301895175,
127.315037442774)) ;
#122269 = CARTESIAN_POINT('Ctrl Pts',(-29.1323454225498,12.6977069155964,
127.469143576858)) ;
#122270 = CARTESIAN_POINT('Ctrl Pts',(-29.2131615019566,12.536159176258,127.672031435155)) ;
#122271 = CARTESIAN_POINT('Ctrl Pts',(-29.3049808389405,12.4388403103588,
127.907201582671)) ;
#122272 = CARTESIAN_POINT('Ctrl Pts',(-29.4023352939487,12.4115721830993,
128.158500758783)) ;
#122273 = CARTESIAN_POINT('Ctrl Pts',(-29.4991788664738,12.457029419961,128.408212309088)) ;
#122274 = CARTESIAN_POINT('Ctrl Pts',(-29.5886148768168,12.5713337690677,
128.636430741871)) ;
#122275 = CARTESIAN_POINT('Ctrl Pts',(-29.6656598966229,12.7468028835324,
128.8283599722)) ;
#122276 = CARTESIAN_POINT('Ctrl Pts',(-29.72530058467,12.9715573467482,128.969356878356)) ;
#122277 = CARTESIAN_POINT('Ctrl Pts',(-29.7636615833883,13.2272671930713,
129.048385247754)) ;
#122278 = CARTESIAN_POINT('Ctrl Pts',(-29.7791134079089,13.4980619502807,
129.060344507591)) ;
#122279 = CARTESIAN_POINT('Ctrl Pts',(-29.7712053180438,13.7620975253013,
129.004251069011)) ;
#122280 = CARTESIAN_POINT('Ctrl Pts',(-29.7410277162991,14.0037249771829,
128.882841708814)) ;
#122281 = CARTESIAN_POINT('Ctrl Pts',(-29.6918330478677,14.202400093294,128.706094471898)) ;
#122282 = CARTESIAN_POINT('Ctrl Pts',(-29.6272000762833,14.3463073278919,
128.483991538536)) ;
#122283 = CARTESIAN_POINT('Ctrl Pts',(-29.5536316150379,14.4229407274136,
128.23613229049)) ;
#122284 = CARTESIAN_POINT('Ctrl Pts',(-29.4760239469434,14.4287087096985,
127.976268927856)) ;
#122285 = CARTESIAN_POINT('Ctrl Pts',(-29.4011723177642,14.3623691322231,
127.724508956974)) ;
#122286 = CARTESIAN_POINT('Ctrl Pts',(-29.3348404453428,14.2283779056864,
127.497526108696)) ;
#122287 = CARTESIAN_POINT('Ctrl Pts',(-29.2828965479532,14.0364255545022,
127.312602435389)) ;
#122288 = CARTESIAN_POINT('Ctrl Pts',(-29.2497959119098,13.8020943881553,
127.182934318226)) ;
#122289 = CARTESIAN_POINT('Ctrl Pts',(-29.2382576660052,13.5391612776222,
127.116043482078)) ;
#122290 = CARTESIAN_POINT('Ctrl Pts',(-29.2500815258749,13.268618582974,127.117498545445)) ;
#122291 = CARTESIAN_POINT('Ctrl Pts',(-29.2851644533423,13.0086418344895,
127.186825345389)) ;
#122292 = CARTESIAN_POINT('Ctrl Pts',(-29.3414272233796,12.7791079862287,
127.318152239982)) ;
#122293 = CARTESIAN_POINT('Ctrl Pts',(-29.4163793099061,12.5942976841109,
127.503809818284)) ;
#122294 = CARTESIAN_POINT('Ctrl Pts',(-29.5041535385455,12.4702970290912,
127.727214554869)) ;
#122295 = CARTESIAN_POINT('Ctrl Pts',(-29.6002280837878,12.4139049816003,
127.974704992316)) ;
#122296 = CARTESIAN_POINT('Ctrl Pts',(-29.6977091902929,12.4297924440583,
128.226434592627)) ;
#122297 = CARTESIAN_POINT('Ctrl Pts',(-29.7913157701915,12.5172147656158,
128.466623365714)) ;
#122298 = CARTESIAN_POINT('Ctrl Pts',(-29.874057974889,12.6696686051205,128.675189083843)) ;
#122299 = CARTESIAN_POINT('Ctrl Pts',(-29.9408743154327,12.8748936311913,
128.83738804483)) ;
#122300 = CARTESIAN_POINT('Ctrl Pts',(-29.9883376423857,13.1206629569548,
128.942849658263)) ;
#122301 = CARTESIAN_POINT('Ctrl Pts',(-30.0132537062615,13.3874987151297,
128.982535373887)) ;
#122302 = CARTESIAN_POINT('Ctrl Pts',(-30.0147150469051,13.6577700593923,
128.953591097854)) ;
#122303 = CARTESIAN_POINT('Ctrl Pts',(-29.9932705416419,13.9102263629719,
128.857849398636)) ;
#122304 = CARTESIAN_POINT('Ctrl Pts',(-29.9515223359549,14.127342135122,128.702904343381)) ;
#122305 = CARTESIAN_POINT('Ctrl Pts',(-29.8925096530416,14.2954362012379,
128.49726452035)) ;
#122306 = CARTESIAN_POINT('Ctrl Pts',(-29.8219114303992,14.400199046936,128.257970798247)) ;
#122307 = CARTESIAN_POINT('Ctrl Pts',(-29.7447976913517,14.4351706373417,
127.999457902045)) ;
#122308 = CARTESIAN_POINT('Ctrl Pts',(-29.6684583326803,14.3977719560938,
127.743498139774)) ;
#122309 = CARTESIAN_POINT('Ctrl Pts',(-29.5978717537841,14.2904204320916,
127.504095055123)) ;
#122310 = CARTESIAN_POINT('Ctrl Pts',(-29.5395109023276,14.1205426182846,
127.300429244723)) ;
#122311 = CARTESIAN_POINT('Ctrl Pts',(-29.4983530336309,13.9015880180689,
127.147150529684)) ;
#122312 = CARTESIAN_POINT('Ctrl Pts',(-29.4777158030966,13.6483197429669,
127.053786309688)) ;
#122313 = CARTESIAN_POINT('Ctrl Pts',(-29.4800308791957,13.3774459783215,
127.027292014993)) ;
#122314 = CARTESIAN_POINT('Ctrl Pts',(-29.5057826138513,13.1115163789139,
127.069470833923)) ;
#122315 = CARTESIAN_POINT('Ctrl Pts',(-29.553761607172,12.867627711837,127.176556695985)) ;
#122316 = CARTESIAN_POINT('Ctrl Pts',(-29.6214344601104,12.6630941323673,
127.341122773102)) ;
#122317 = CARTESIAN_POINT('Ctrl Pts',(-29.7047886913497,12.5128296370691,
127.551436680502)) ;
#122318 = CARTESIAN_POINT('Ctrl Pts',(-29.7983168331104,12.4280522080275,
127.791517147946)) ;
#122319 = CARTESIAN_POINT('Ctrl Pts',(-29.896197969887,12.4147676790035,128.044288782186)) ;
#122320 = CARTESIAN_POINT('Ctrl Pts',(-29.9916432988877,12.4732052495888,
128.290111005686)) ;
#122321 = CARTESIAN_POINT('Ctrl Pts',(-30.0798394969363,12.6008830846757,
128.514423176177)) ;
#122322 = CARTESIAN_POINT('Ctrl Pts',(-30.153418094144,12.7859101152191,128.69640859045)) ;
#122323 = CARTESIAN_POINT('Ctrl Pts',(-30.2092050348681,13.0171550939707,
128.826255988633)) ;
#122324 = CARTESIAN_POINT('Ctrl Pts',(-30.2434739775271,13.2774025189781,
128.893266135644)) ;
#122325 = CARTESIAN_POINT('Ctrl Pts',(-30.2545103544402,13.5492093049786,
128.892265384779)) ;
#122326 = CARTESIAN_POINT('Ctrl Pts',(-30.2422243054412,13.8101283643081,
128.823364688969)) ;
#122327 = CARTESIAN_POINT('Ctrl Pts',(-30.2083754507383,14.0442617204232,
128.691385046736)) ;
#122328 = CARTESIAN_POINT('Ctrl Pts',(-30.1554956679367,14.2348997538622,
128.503575628584)) ;
#122329 = CARTESIAN_POINT('Ctrl Pts',(-30.0893154304115,14.3654883224984,
128.277320876037)) ;
#122330 = CARTESIAN_POINT('Ctrl Pts',(-30.0140893274458,14.4297229265612,
128.02437201421)) ;
#122331 = CARTESIAN_POINT('Ctrl Pts',(-29.9366945426251,14.421668005349,127.765225227294)) ;
#122332 = CARTESIAN_POINT('Ctrl Pts',(-29.8627322861493,14.3417420843685,
127.515916221253)) ;
#122333 = CARTESIAN_POINT('Ctrl Pts',(-29.7990172516701,14.1964291100303,
127.296728535392)) ;
#122334 = CARTESIAN_POINT('Ctrl Pts',(-29.7503115001684,13.9955518397601,
127.121315751128)) ;
#122335 = CARTESIAN_POINT('Ctrl Pts',(-29.7209679395557,13.7541464168563,
127.002530885163)) ;
#122336 = CARTESIAN_POINT('Ctrl Pts',(-29.7138270012993,13.4873870374965,
126.948394752065)) ;
#122337 = CARTESIAN_POINT('Ctrl Pts',(-29.7300210673021,13.2187118678006,
126.962770014111)) ;
#122338 = CARTESIAN_POINT('Ctrl Pts',(-29.7693618809783,12.9622340205071,
127.04445153456)) ;
#122339 = CARTESIAN_POINT('Ctrl Pts',(-29.8296161918263,12.7396654906289,
127.187330698386)) ;
#122340 = CARTESIAN_POINT('Ctrl Pts',(-29.9070992084671,12.5663130117826,
127.380570436631)) ;
#122341 = CARTESIAN_POINT('Ctrl Pts',(-29.9967702563037,12.4542929765583,
127.609512573754)) ;
#122342 = CARTESIAN_POINT('Ctrl Pts',(-30.0940660663216,12.4113060992836,
127.860434811166)) ;
#122343 = CARTESIAN_POINT('Ctrl Pts',(-30.1909321832857,12.4409729765678,
128.110447724348)) ;
#122344 = CARTESIAN_POINT('Ctrl Pts',(-30.2827250654669,12.5408195809103,
128.345442109958)) ;
#122345 = CARTESIAN_POINT('Ctrl Pts',(-30.3631110575611,12.7045177174677,
128.54705780663)) ;
#122346 = CARTESIAN_POINT('Ctrl Pts',(-30.4266778642014,12.919412680773,128.69962285843)) ;
#122347 = CARTESIAN_POINT('Ctrl Pts',(-30.4698068753402,13.1689179430447,
128.792656682487)) ;
#122348 = CARTESIAN_POINT('Ctrl Pts',(-30.4904930950395,13.4397285825566,
128.819731723829)) ;
#122349 = CARTESIAN_POINT('Ctrl Pts',(-30.4874907257796,13.7064270622518,
128.777980012696)) ;
#122350 = CARTESIAN_POINT('Ctrl Pts',(-30.4620654317262,13.9538863073551,
128.670590863252)) ;
#122351 = CARTESIAN_POINT('Ctrl Pts',(-30.4167476705665,14.163192773507,128.505145630859)) ;
#122352 = CARTESIAN_POINT('Ctrl Pts',(-30.3548906755859,14.3205261321744,
128.291114365887)) ;
#122353 = CARTESIAN_POINT('Ctrl Pts',(-30.2829346299508,14.4121066537417,
128.047974510391)) ;
#122354 = CARTESIAN_POINT('Ctrl Pts',(-30.2054667933554,14.433704272446,127.788469415393)) ;
#122355 = CARTESIAN_POINT('Ctrl Pts',(-30.1294973360627,14.3826278008681,
127.533437022415)) ;
#122356 = CARTESIAN_POINT('Ctrl Pts',(-30.0609394463252,14.2628852203127,
127.300029416679)) ;
#122357 = CARTESIAN_POINT('Ctrl Pts',(-30.0055020233255,14.0829261229302,
127.104952049683)) ;
#122358 = CARTESIAN_POINT('Ctrl Pts',(-29.9678519682289,13.8556921301219,
126.961834528388)) ;
#122359 = CARTESIAN_POINT('Ctrl Pts',(-29.9515006435671,13.5972598207812,
126.880912604436)) ;
#122360 = CARTESIAN_POINT('Ctrl Pts',(-29.9581093878637,13.3277678231801,
126.867244122754)) ;
#122361 = CARTESIAN_POINT('Ctrl Pts',(-29.9885236753733,13.061810881333,126.92268198126)) ;
#122362 = CARTESIAN_POINT('Ctrl Pts',(-30.0401392420675,12.8260388711121,
127.040646354392)) ;
#122363 = CARTESIAN_POINT('Ctrl Pts',(-30.1113480471282,12.6298695868286,
127.215398293609)) ;
#122364 = CARTESIAN_POINT('Ctrl Pts',(-30.1968274118044,12.491768708706,127.432029083831)) ;
#122365 = CARTESIAN_POINT('Ctrl Pts',(-30.2917304339287,12.4199839155212,
127.676085528742)) ;
#122366 = CARTESIAN_POINT('Ctrl Pts',(-30.3895172732968,12.4203084391601,
127.928654142182)) ;
#122367 = CARTESIAN_POINT('Ctrl Pts',(-30.4841396004474,12.492208510643,128.171981243385)) ;
#122368 = CARTESIAN_POINT('Ctrl Pts',(-30.5697024940823,12.630997013847,128.388786123922)) ;
#122369 = CARTESIAN_POINT('Ctrl Pts',(-30.6405627396724,12.8263312491105,
128.562679987083)) ;
#122370 = CARTESIAN_POINT('Ctrl Pts',(-30.6926223743772,13.0651229525308,
128.681553834385)) ;
#122371 = CARTESIAN_POINT('Ctrl Pts',(-30.7225260149649,13.3295669294852,
128.735723381487)) ;
#122372 = CARTESIAN_POINT('Ctrl Pts',(-30.7290589510896,13.5989125314577,
128.72184499335)) ;
#122373 = CARTESIAN_POINT('Ctrl Pts',(-30.7124997713408,13.8574711990645,
128.640276978673)) ;
#122374 = CARTESIAN_POINT('Ctrl Pts',(-30.6748800157575,14.08370800358,128.497364451285)) ;
#122375 = CARTESIAN_POINT('Ctrl Pts',(-30.6192581352089,14.2638192585231,
128.301674339225)) ;
#122376 = CARTESIAN_POINT('Ctrl Pts',(-30.5506481335535,14.3831696043844,
128.068124805853)) ;
#122377 = CARTESIAN_POINT('Ctrl Pts',(-30.4745251971265,14.4337176712718,
127.812585526878)) ;
#122378 = CARTESIAN_POINT('Ctrl Pts',(-30.3974954804431,14.4120588565301,
127.554554597263)) ;
#122379 = CARTESIAN_POINT('Ctrl Pts',(-30.3250685590978,14.3193772826324,
127.309789317507)) ;
#122380 = CARTESIAN_POINT('Ctrl Pts',(-30.2637016994033,14.1628170776178,
127.097430559327)) ;
#122381 = CARTESIAN_POINT('Ctrl Pts',(-30.2181498014506,13.9515916120412,
126.931029962997)) ;
#122382 = CARTESIAN_POINT('Ctrl Pts',(-30.1929956511177,13.7055233139094,
126.824657543455)) ;
#122383 = CARTESIAN_POINT('Ctrl Pts',(-30.1902289107925,13.4359481903885,
126.783236403317)) ;
#122384 = CARTESIAN_POINT('Ctrl Pts',(-30.2107593001267,13.1690262561277,
126.810343623313)) ;
#122385 = CARTESIAN_POINT('Ctrl Pts',(-30.2545482372846,12.9162728254293,
126.904850728262)) ;
#122386 = CARTESIAN_POINT('Ctrl Pts',(-30.3178913728212,12.7036779683092,
127.057027568581)) ;
#122387 = CARTESIAN_POINT('Ctrl Pts',(-30.3981222067462,12.5403117617381,
127.258247374178)) ;
#122388 = CARTESIAN_POINT('Ctrl Pts',(-30.4903111236193,12.4404489557871,
127.494277250787)) ;
#122389 = CARTESIAN_POINT('Ctrl Pts',(-30.5871336885702,12.4114485631191,
127.744183561599)) ;
#122390 = CARTESIAN_POINT('Ctrl Pts',(-30.6840345143622,12.4544846447878,
127.994082811986)) ;
#122391 = CARTESIAN_POINT('Ctrl Pts',(-30.7741275020112,12.5672617831098,
128.224093354097)) ;
#122392 = CARTESIAN_POINT('Ctrl Pts',(-30.8516515642429,12.741774518216,128.417359705438)) ;
#122393 = CARTESIAN_POINT('Ctrl Pts',(-30.9114063327502,12.9633751206612,
128.558968956766)) ;
#122394 = CARTESIAN_POINT('Ctrl Pts',(-30.9507706166524,13.2203112306522,
128.64066766554)) ;
#122395 = CARTESIAN_POINT('Ctrl Pts',(-30.9667741641491,13.4905144393576,
128.654304855092)) ;
#122396 = CARTESIAN_POINT('Ctrl Pts',(-30.9595000465809,13.7550217254887,
128.60004785508)) ;
#122397 = CARTESIAN_POINT('Ctrl Pts',(-30.9300640821417,13.9967496932403,
128.480932627841)) ;
#122398 = CARTESIAN_POINT('Ctrl Pts',(-30.88124976571,14.1974243252069,128.305200960729)) ;
#122399 = CARTESIAN_POINT('Ctrl Pts',(-30.8173009837137,14.3425140414095,
128.0852559147)) ;
#122400 = CARTESIAN_POINT('Ctrl Pts',(-30.7437385247045,14.4218016114581,
127.837311335821)) ;
#122401 = CARTESIAN_POINT('Ctrl Pts',(-30.6657606026371,14.4294553389326,
127.576204351649)) ;
#122402 = CARTESIAN_POINT('Ctrl Pts',(-30.5911196828898,14.3652617891387,
127.325217316403)) ;
#122403 = CARTESIAN_POINT('Ctrl Pts',(-30.5245394207173,14.2335996006041,
127.097570146183)) ;
#122404 = CARTESIAN_POINT('Ctrl Pts',(-30.4720096954179,14.0430657817291,
126.910897477969)) ;
#122405 = CARTESIAN_POINT('Ctrl Pts',(-30.4382095748234,13.8093137336756,
126.779115500136)) ;
#122406 = CARTESIAN_POINT('Ctrl Pts',(-30.4260630552414,13.5459138184761,
126.710330077877)) ;
#122407 = CARTESIAN_POINT('Ctrl Pts',(-30.4371827081375,13.2769102523372,
126.709919831468)) ;
#122408 = CARTESIAN_POINT('Ctrl Pts',(-30.4715571173939,13.0160045287208,
126.777143004842)) ;
#122409 = CARTESIAN_POINT('Ctrl Pts',(-30.5273885697427,12.7850160477838,
126.907146547319)) ;
#122410 = CARTESIAN_POINT('Ctrl Pts',(-30.6015916024625,12.5991695463159,
127.09073027164)) ;
#122411 = CARTESIAN_POINT('Ctrl Pts',(-30.689509572293,12.4727066402134,127.314381139998)) ;
#122412 = CARTESIAN_POINT('Ctrl Pts',(-30.78498211656,12.414634000185,127.56027701158)) ;
#122413 = CARTESIAN_POINT('Ctrl Pts',(-30.8827162241977,12.4282724908794,
127.812670727123)) ;
#122414 = CARTESIAN_POINT('Ctrl Pts',(-30.9764215447378,12.5136822539145,
128.053186598358)) ;
#122415 = CARTESIAN_POINT('Ctrl Pts',(-31.0595380623793,12.6640314349918,
128.262872652563)) ;
#122416 = CARTESIAN_POINT('Ctrl Pts',(-31.1272621654378,12.8694014847424,
128.427501230652)) ;
#122417 = CARTESIAN_POINT('Ctrl Pts',(-31.1749753148501,13.11284739186,128.533901712675)) ;
#122418 = CARTESIAN_POINT('Ctrl Pts',(-31.2006444289191,13.3794714169119,
128.575760031987)) ;
#122419 = CARTESIAN_POINT('Ctrl Pts',(-31.2027867558287,13.649387589438,128.548872446442)) ;
#122420 = CARTESIAN_POINT('Ctrl Pts',(-31.182112101246,13.9027716993511,128.455382730857)) ;
#122421 = CARTESIAN_POINT('Ctrl Pts',(-31.1405097423725,14.1226004021729,
128.300604633976)) ;
#122422 = CARTESIAN_POINT('Ctrl Pts',(-31.0824924132861,14.2907614939367,
128.098200056456)) ;
#122423 = CARTESIAN_POINT('Ctrl Pts',(-31.0115394554541,14.3985142695992,
127.857562086865)) ;
#122424 = CARTESIAN_POINT('Ctrl Pts',(-30.9350167672811,14.4350393249369,
127.60100492444)) ;
#122425 = CARTESIAN_POINT('Ctrl Pts',(-30.8584423775873,14.4000355942845,
127.344298627008)) ;
#122426 = CARTESIAN_POINT('Ctrl Pts',(-30.7873589741607,14.294019259171,127.103326699404)) ;
#122427 = CARTESIAN_POINT('Ctrl Pts',(-30.7288526610613,14.1264036787102,
126.899375100568)) ;
#122428 = CARTESIAN_POINT('Ctrl Pts',(-30.687031834005,13.908713601209,126.744138494649)) ;
#122429 = CARTESIAN_POINT('Ctrl Pts',(-30.665740603527,13.6545233253026,126.648660834423)) ;
#122430 = CARTESIAN_POINT('Ctrl Pts',(-30.6674256184851,13.385850090519,126.620576704158)) ;
#122431 = CARTESIAN_POINT('Ctrl Pts',(-30.6924732658782,13.1190055030057,
126.660631420444)) ;
#122432 = CARTESIAN_POINT('Ctrl Pts',(-30.739931250503,12.8738785083339,126.766149985998)) ;
#122433 = CARTESIAN_POINT('Ctrl Pts',(-30.8072994517156,12.6676053408392,
126.929745605886)) ;
#122434 = CARTESIAN_POINT('Ctrl Pts',(-30.8902244330813,12.5160770794409,
127.138850466977)) ;
#122435 = CARTESIAN_POINT('Ctrl Pts',(-30.9830990181765,12.429744459131,127.377173832304)) ;
#122436 = CARTESIAN_POINT('Ctrl Pts',(-31.0808346305105,12.4139325867349,
127.629558482749)) ;
#122437 = CARTESIAN_POINT('Ctrl Pts',(-31.1769815706491,12.470818666654,127.877230342766)) ;
#122438 = CARTESIAN_POINT('Ctrl Pts',(-31.2647445655939,12.5954481980338,
128.100568864441)) ;
#122439 = CARTESIAN_POINT('Ctrl Pts',(-31.3392856003309,12.7795463836638,
128.285188591065)) ;
#122440 = CARTESIAN_POINT('Ctrl Pts',(-31.3957801377511,13.0105019678005,
128.417005984796)) ;
#122441 = CARTESIAN_POINT('Ctrl Pts',(-31.4306543783806,13.2704660588973,
128.485753447239)) ;
#122442 = CARTESIAN_POINT('Ctrl Pts',(-31.442287999366,13.5415026123175,128.48658603552)) ;
#122443 = CARTESIAN_POINT('Ctrl Pts',(-31.4307033779827,13.8030871080867,
128.419727155045)) ;
#122444 = CARTESIAN_POINT('Ctrl Pts',(-31.3971754129151,14.0389748553007,
128.288544481416)) ;
#122445 = CARTESIAN_POINT('Ctrl Pts',(-31.3454184265653,14.2290324993106,
128.104404269474)) ;
#122446 = CARTESIAN_POINT('Ctrl Pts',(-31.2790627226709,14.3629001779689,
127.877345831259)) ;
#122447 = CARTESIAN_POINT('Ctrl Pts',(-31.2041424100767,14.428830285179,127.625371610393)) ;
#122448 = CARTESIAN_POINT('Ctrl Pts',(-31.1265767826112,14.4228365042112,
127.365651786092)) ;
#122449 = CARTESIAN_POINT('Ctrl Pts',(-31.052679859191,14.3452101955046,127.116656966355)) ;
#122450 = CARTESIAN_POINT('Ctrl Pts',(-30.9884269255255,14.2014202619827,
126.895813741383)) ;
#122451 = CARTESIAN_POINT('Ctrl Pts',(-30.9392882282485,14.0021641250436,
126.719179096165)) ;
#122452 = CARTESIAN_POINT('Ctrl Pts',(-30.9093211350562,13.7617530552763,
126.598570707612)) ;
#122453 = CARTESIAN_POINT('Ctrl Pts',(-30.9014747573705,13.4956079562807,
126.542397455449)) ;
#122454 = CARTESIAN_POINT('Ctrl Pts',(-30.9170318360537,13.2262845260177,
126.55484606842)) ;
#122455 = CARTESIAN_POINT('Ctrl Pts',(-30.9555778404963,12.9698876491267,
126.634313026387)) ;
#122456 = CARTESIAN_POINT('Ctrl Pts',(-31.0153287793161,12.7457363777613,
126.77566667277)) ;
#122457 = CARTESIAN_POINT('Ctrl Pts',(-31.0921782746939,12.5708017324576,
126.967118677833)) ;
#122458 = CARTESIAN_POINT('Ctrl Pts',(-31.1824180985943,12.4561497047602,
127.197416346179)) ;
#122459 = CARTESIAN_POINT('Ctrl Pts',(-31.278554206561,12.4116404870753,127.445319108056)) ;
#122460 = CARTESIAN_POINT('Ctrl Pts',(-31.3762681488149,12.4391729366694,
127.697540638099)) ;
#122461 = CARTESIAN_POINT('Ctrl Pts',(-31.4680268263453,12.53717976609,127.932527251887)) ;
#122462 = CARTESIAN_POINT('Ctrl Pts',(-31.5485854179887,12.6985743476714,
128.13474547452)) ;
#122463 = CARTESIAN_POINT('Ctrl Pts',(-31.6127577477514,12.9117741339943,
128.289108577839)) ;
#122464 = CARTESIAN_POINT('Ctrl Pts',(-31.6567710961282,13.1624013119324,
128.384477088599)) ;
#122465 = CARTESIAN_POINT('Ctrl Pts',(-31.6779406587271,13.4305279124855,
128.413268749148)) ;
#122466 = CARTESIAN_POINT('Ctrl Pts',(-31.6757209320686,13.6988963529668,
128.373634329705)) ;
#122467 = CARTESIAN_POINT('Ctrl Pts',(-31.6508856851263,13.9472005440968,
128.267972545371)) ;
#122468 = CARTESIAN_POINT('Ctrl Pts',(-31.6060004910728,14.1580510718868,
128.103736864114)) ;
#122469 = CARTESIAN_POINT('Ctrl Pts',(-31.5448207362963,14.3165352463583,
127.891828892358)) ;
#122470 = CARTESIAN_POINT('Ctrl Pts',(-31.4727358243366,14.4105996736352,
127.648139770064)) ;
#122471 = CARTESIAN_POINT('Ctrl Pts',(-31.3955355088999,14.4340684642594,
127.389513002923)) ;
#122472 = CARTESIAN_POINT('Ctrl Pts',(-31.3193139953007,14.3850543763753,
127.133688710295)) ;
#122473 = CARTESIAN_POINT('Ctrl Pts',(-31.2504690412177,14.2669952008499,
126.899435868025)) ;
#122474 = CARTESIAN_POINT('Ctrl Pts',(-31.1947324047151,14.0891153904615,
126.703574539752)) ;
#122475 = CARTESIAN_POINT('Ctrl Pts',(-31.1564387248963,13.862922820575,126.558547490818)) ;
#122476 = CARTESIAN_POINT('Ctrl Pts',(-31.1394099641997,13.6044942948714,
126.47557023365)) ;
#122477 = CARTESIAN_POINT('Ctrl Pts',(-31.1454472203925,13.3352194719608,
126.460244590561)) ;
#122478 = CARTESIAN_POINT('Ctrl Pts',(-31.1748811284131,13.0705828677346,
126.513054618359)) ;
#122479 = CARTESIAN_POINT('Ctrl Pts',(-31.2262659374063,12.8316691546943,
126.630062656991)) ;
#122480 = CARTESIAN_POINT('Ctrl Pts',(-31.2971356400406,12.6342705619082,
126.803808781442)) ;
#122481 = CARTESIAN_POINT('Ctrl Pts',(-31.3819483703303,12.4949547618174,
127.018616528483)) ;
#122482 = CARTESIAN_POINT('Ctrl Pts',(-31.4766833238412,12.4210676007864,
127.262174213226)) ;
#122483 = CARTESIAN_POINT('Ctrl Pts',(-31.5743436337679,12.4192534953992,
127.514414718138)) ;
#122484 = CARTESIAN_POINT('Ctrl Pts',(-31.6693177267353,12.4890551433301,
127.758717643024)) ;
#122485 = CARTESIAN_POINT('Ctrl Pts',(-31.7555447049053,12.6269266116115,
127.977315822043)) ;
#122486 = CARTESIAN_POINT('Ctrl Pts',(-31.8264211692197,12.8196496525906,
128.15146867102)) ;
#122487 = CARTESIAN_POINT('Ctrl Pts',(-31.8792655119042,13.0580837190484,
128.272530897348)) ;
#122488 = CARTESIAN_POINT('Ctrl Pts',(-31.9097495081077,13.3214663424209,
128.328476209486)) ;
#122489 = CARTESIAN_POINT('Ctrl Pts',(-31.9169670179251,13.5912988654113,
128.316540654689)) ;
#122490 = CARTESIAN_POINT('Ctrl Pts',(-31.9011691067475,13.8497220068298,
128.237308488014)) ;
#122491 = CARTESIAN_POINT('Ctrl Pts',(-31.8637971767436,14.0789423187272,
128.0948445745)) ;
#122492 = CARTESIAN_POINT('Ctrl Pts',(-31.8086550954363,14.259760152893,127.900645843771)) ;
#122493 = CARTESIAN_POINT('Ctrl Pts',(-31.7405929166887,14.3805241864287,
127.668810176457)) ;
#122494 = CARTESIAN_POINT('Ctrl Pts',(-31.6647024826629,14.4333051091104,
127.413993047517)) ;
#122495 = CARTESIAN_POINT('Ctrl Pts',(-31.5873081578645,14.4135763051709,
127.154757112012)) ;
#122496 = CARTESIAN_POINT('Ctrl Pts',(-31.5147598783728,14.3230159686918,
126.909698801431)) ;
#122497 = CARTESIAN_POINT('Ctrl Pts',(-31.4527958504163,14.1669880508,126.695418871326)) ;
#122498 = CARTESIAN_POINT('Ctrl Pts',(-31.4072827436831,13.960185490464,126.529605369715)) ;
#122499 = CARTESIAN_POINT('Ctrl Pts',(-31.381143378296,13.7121979598798,126.419953822516)) ;
#122500 = CARTESIAN_POINT('Ctrl Pts',(-31.3777158961212,13.445325428157,126.376915063972)) ;
#122501 = CARTESIAN_POINT('Ctrl Pts',(-31.397745527697,13.1756579311624,126.402235763468)) ;
#122502 = CARTESIAN_POINT('Ctrl Pts',(-31.4404084183114,12.9248371147139,
126.493828264377)) ;
#122503 = CARTESIAN_POINT('Ctrl Pts',(-31.5036578664833,12.7087904234027,
126.645429976648)) ;
#122504 = CARTESIAN_POINT('Ctrl Pts',(-31.5834548863671,12.5441839986788,
126.845425287598)) ;
#122505 = CARTESIAN_POINT('Ctrl Pts',(-31.6753525848934,12.4422953627895,
127.08061008035)) ;
#122506 = CARTESIAN_POINT('Ctrl Pts',(-31.7723120116357,12.4112745918663,
127.330847845115)) ;
#122507 = CARTESIAN_POINT('Ctrl Pts',(-31.8691208728923,12.4523611263307,
127.580540139706)) ;
#122508 = CARTESIAN_POINT('Ctrl Pts',(-31.9592601337174,12.5627156351226,
127.810782853242)) ;
#122509 = CARTESIAN_POINT('Ctrl Pts',(-32.0375124865879,12.7362032520556,
128.006054251628)) ;
#122510 = CARTESIAN_POINT('Ctrl Pts',(-32.0976971478895,12.9562237292826,
128.148985066523)) ;
#122511 = CARTESIAN_POINT('Ctrl Pts',(-32.13773953768,13.2127632851082,128.232621281861)) ;
#122512 = CARTESIAN_POINT('Ctrl Pts',(-32.1543946447233,13.4814740425718,
128.248327464853)) ;
#122513 = CARTESIAN_POINT('Ctrl Pts',(-32.1478604320586,13.7476021325284,
128.196087364076)) ;
#122514 = CARTESIAN_POINT('Ctrl Pts',(-32.1188973813439,13.9907503270219,
128.078278588462)) ;
#122515 = CARTESIAN_POINT('Ctrl Pts',(-32.0707073756381,14.1921269255571,
127.904467261036)) ;
#122516 = CARTESIAN_POINT('Ctrl Pts',(-32.0072133952261,14.3392030791961,
127.685872025095)) ;
#122517 = CARTESIAN_POINT('Ctrl Pts',(-31.9332416636767,14.4207500388282,
127.436469066278)) ;
#122518 = CARTESIAN_POINT('Ctrl Pts',(-31.8560118722166,14.4302362494743,
127.177863683382)) ;
#122519 = CARTESIAN_POINT('Ctrl Pts',(-31.7807999346763,14.3680282355215,
126.925031033499)) ;
#122520 = CARTESIAN_POINT('Ctrl Pts',(-31.7138116605628,14.2375542878188,
126.69612628114)) ;
#122521 = CARTESIAN_POINT('Ctrl Pts',(-31.6609816023683,14.0487158820881,
126.50864330256)) ;
#122522 = CARTESIAN_POINT('Ctrl Pts',(-31.6267397291478,13.8167882878437,
126.375682453872)) ;
#122523 = CARTESIAN_POINT('Ctrl Pts',(-31.6138694456944,13.5548283790035,
126.304885636777)) ;
#122524 = CARTESIAN_POINT('Ctrl Pts',(-31.6242959406042,13.2844749263172,
126.302288767915)) ;
#122525 = CARTESIAN_POINT('Ctrl Pts',(-31.6581468262068,13.0226682928204,
126.367933605866)) ;
#122526 = CARTESIAN_POINT('Ctrl Pts',(-31.7132570926775,12.7913019037466,
126.495925056773)) ;
#122527 = CARTESIAN_POINT('Ctrl Pts',(-31.7868846932829,12.6040506886806,
126.677862167633)) ;
#122528 = CARTESIAN_POINT('Ctrl Pts',(-31.8744032872355,12.4756113608574,
126.900365413074)) ;
#122529 = CARTESIAN_POINT('Ctrl Pts',(-31.9700299165858,12.4152434806169,
127.14660580532)) ;
#122530 = CARTESIAN_POINT('Ctrl Pts',(-32.067726874144,12.4269403893897,127.398912991664)) ;
#122531 = CARTESIAN_POINT('Ctrl Pts',(-32.1614230211097,12.5099953392157,
127.639486026072)) ;
#122532 = CARTESIAN_POINT('Ctrl Pts',(-32.2450419055353,12.6587329493789,
127.850591786388)) ;
#122533 = CARTESIAN_POINT('Ctrl Pts',(-32.3131064085061,12.8618952615055,
128.016327167337)) ;
#122534 = CARTESIAN_POINT('Ctrl Pts',(-32.3617247556363,13.105407033224,128.125223389019)) ;
#122535 = CARTESIAN_POINT('Ctrl Pts',(-32.3880370855062,13.372198744835,128.168900378835)) ;
#122536 = CARTESIAN_POINT('Ctrl Pts',(-32.3908241094825,13.6415134475053,
128.143990115677)) ;
#122537 = CARTESIAN_POINT('Ctrl Pts',(-32.3708584046227,13.8954057522976,
128.052605580229)) ;
#122538 = CARTESIAN_POINT('Ctrl Pts',(-32.3297866697098,14.1169004817223,
127.899329717684)) ;
#122539 = CARTESIAN_POINT('Ctrl Pts',(-32.2720357073091,14.2868623314226,
127.697634443906)) ;
#122540 = CARTESIAN_POINT('Ctrl Pts',(-32.2018019882442,14.3960130363954,
127.45930091582)) ;
#122541 = CARTESIAN_POINT('Ctrl Pts',(-32.1250722199058,14.4351149221843,
127.202000748098)) ;
#122542 = CARTESIAN_POINT('Ctrl Pts',(-32.0482999804116,14.4019052033915,
126.944665606573)) ;
#122543 = CARTESIAN_POINT('Ctrl Pts',(-31.9771926809482,14.2983009205314,
126.70374147036)) ;
#122544 = CARTESIAN_POINT('Ctrl Pts',(-31.9180230665024,14.1317969233753,
126.497728005608)) ;
#122545 = CARTESIAN_POINT('Ctrl Pts',(-31.8757597160519,13.9153433735369,
126.341222269938)) ;
#122546 = CARTESIAN_POINT('Ctrl Pts',(-31.8538948818607,13.6633971657659,
126.244251306656)) ;
#122547 = CARTESIAN_POINT('Ctrl Pts',(-31.8547561893373,13.3943409356125,
126.213683501552)) ;
#122548 = CARTESIAN_POINT('Ctrl Pts',(-31.879305119298,13.125759479102,126.252108551624)) ;
#122549 = CARTESIAN_POINT('Ctrl Pts',(-31.9260462665466,12.8806964502858,
126.355648570145)) ;
#122550 = CARTESIAN_POINT('Ctrl Pts',(-31.992649963062,12.6734733504626,126.517098736783)) ;
#122551 = CARTESIAN_POINT('Ctrl Pts',(-32.0753331596735,12.5195857964099,
126.725421864695)) ;
#122552 = CARTESIAN_POINT('Ctrl Pts',(-32.1684606176005,12.431093262312,126.964324569044)) ;
#122553 = CARTESIAN_POINT('Ctrl Pts',(-32.2656426943434,12.4134132732782,
127.215267971027)) ;
#122554 = CARTESIAN_POINT('Ctrl Pts',(-32.3620515668434,12.4681188865971,
127.463663966544)) ;
#122555 = CARTESIAN_POINT('Ctrl Pts',(-32.4501306508827,12.5909169952097,
127.687925854587)) ;
#122556 = CARTESIAN_POINT('Ctrl Pts',(-32.5251176857849,12.7734489728906,
127.873850465839)) ;
#122557 = CARTESIAN_POINT('Ctrl Pts',(-32.5821383880763,13.0028155052197,
128.007264413582)) ;
#122558 = CARTESIAN_POINT('Ctrl Pts',(-32.6177275928939,13.2626813874081,
128.078031538423)) ;
#122559 = CARTESIAN_POINT('Ctrl Pts',(-32.6300773966959,13.5323092973528,
128.081128075608)) ;
#122560 = CARTESIAN_POINT('Ctrl Pts',(-32.6191171645962,13.7963544405994,
128.015846971038)) ;
#122561 = CARTESIAN_POINT('Ctrl Pts',(-32.5862481873824,14.0324258924939,
127.886706170116)) ;
#122562 = CARTESIAN_POINT('Ctrl Pts',(-32.5349051847159,14.2243212394665,
127.703714987948)) ;
#122563 = CARTESIAN_POINT('Ctrl Pts',(-32.4690664082192,14.3597397385498,
127.478255566514)) ;
#122564 = CARTESIAN_POINT('Ctrl Pts',(-32.3940630824478,14.4280132276383,
127.225921237608)) ;
#122565 = CARTESIAN_POINT('Ctrl Pts',(-32.3165287082417,14.4240026774031,
126.966315839368)) ;
#122566 = CARTESIAN_POINT('Ctrl Pts',(-32.2423883005505,14.3482148360276,
126.716578494938)) ;
#122567 = CARTESIAN_POINT('Ctrl Pts',(-32.1779893014855,14.2066838492508,
126.49541837889)) ;
#122568 = CARTESIAN_POINT('Ctrl Pts',(-32.1281752856826,14.0084843901798,
126.316727480174)) ;
#122569 = CARTESIAN_POINT('Ctrl Pts',(-32.0975903701439,13.7679162492584,
126.194182548856)) ;
#122570 = CARTESIAN_POINT('Ctrl Pts',(-32.0891787939898,13.5034892563332,
126.13652430323)) ;
#122571 = CARTESIAN_POINT('Ctrl Pts',(-32.1040626123099,13.2335993396584,
126.146949017154)) ;
#122572 = CARTESIAN_POINT('Ctrl Pts',(-32.1420329442231,12.9764075734903,
126.224715938811)) ;
#122573 = CARTESIAN_POINT('Ctrl Pts',(-32.2013713025453,12.7508791959946,
126.364815084693)) ;
#122574 = CARTESIAN_POINT('Ctrl Pts',(-32.2775403681359,12.5752390295055,
126.554404335388)) ;
#122575 = CARTESIAN_POINT('Ctrl Pts',(-32.3669984352675,12.4588914827239,
126.782580215258)) ;
#122576 = CARTESIAN_POINT('Ctrl Pts',(-32.4635757710145,12.4118138337187,
127.031576925067)) ;
#122577 = CARTESIAN_POINT('Ctrl Pts',(-32.5613228642034,12.4374481802068,
127.283905827195)) ;
#122578 = CARTESIAN_POINT('Ctrl Pts',(-32.6533055517079,12.5333386761198,
127.519560385033)) ;
#122579 = CARTESIAN_POINT('Ctrl Pts',(-32.7345801972341,12.6939673682458,
127.72372104471)) ;
#122580 = CARTESIAN_POINT('Ctrl Pts',(-32.7989235968999,12.905003236762,127.878741838257)) ;
#122581 = CARTESIAN_POINT('Ctrl Pts',(-32.8436689907595,13.1551454221065,
127.976196286225)) ;
#122582 = CARTESIAN_POINT('Ctrl Pts',(-32.8581698291871,13.3338159430811,
127.996517118284)) ;
#122583 = CARTESIAN_POINT('Ctrl Pts',(-32.8615556099148,13.423122164697,127.995387104394)) ;
#122584 = CARTESIAN_POINT('Ctrl Pts',(-11.4238141454945,13.1551399285885,
133.176569308009)) ;
#122585 = CARTESIAN_POINT('Ctrl Pts',(-11.4245530443044,13.1489709760559,
133.177996857566)) ;
#122586 = CARTESIAN_POINT('Ctrl Pts',(-11.4366069089063,13.0505875198745,
133.201526775898)) ;
#122587 = CARTESIAN_POINT('Ctrl Pts',(-11.4693539332526,12.8648901900081,
133.274214160344)) ;
#122588 = CARTESIAN_POINT('Ctrl Pts',(-11.5380924228032,12.637899642759,133.441994108163)) ;
#122589 = CARTESIAN_POINT('Ctrl Pts',(-11.6243468898402,12.4661938429578,
133.66085914641)) ;
#122590 = CARTESIAN_POINT('Ctrl Pts',(-11.723176143549,12.3629468652583,133.9162908092)) ;
#122591 = CARTESIAN_POINT('Ctrl Pts',(-11.8266263732223,12.3360866593215,
134.185565771878)) ;
#122592 = CARTESIAN_POINT('Ctrl Pts',(-11.9299575986037,12.3868468010151,
134.454196270192)) ;
#122593 = CARTESIAN_POINT('Ctrl Pts',(-12.0251860635232,12.5118616654237,
134.699290577349)) ;
#122594 = CARTESIAN_POINT('Ctrl Pts',(-12.1067707542268,12.7022377085439,
134.904476363702)) ;
#122595 = CARTESIAN_POINT('Ctrl Pts',(-12.1693898147792,12.9442212424904,
135.054278991416)) ;
#122596 = CARTESIAN_POINT('Ctrl Pts',(-12.2093211316432,13.2203923683254,
135.137814270087)) ;
#122597 = CARTESIAN_POINT('Ctrl Pts',(-12.2245264343576,13.5109002567873,
135.149142252338)) ;
#122598 = CARTESIAN_POINT('Ctrl Pts',(-12.2144214456397,13.7967279051741,
135.086333358288)) ;
#122599 = CARTESIAN_POINT('Ctrl Pts',(-12.1808130028206,14.053163616969,134.955192972495)) ;
#122600 = CARTESIAN_POINT('Ctrl Pts',(-12.1265747443939,14.2659162320927,
134.763620195857)) ;
#122601 = CARTESIAN_POINT('Ctrl Pts',(-12.0563659530723,14.4182156131257,
134.525407960618)) ;
#122602 = CARTESIAN_POINT('Ctrl Pts',(-11.9757170636332,14.4993926376335,
134.256600011119)) ;
#122603 = CARTESIAN_POINT('Ctrl Pts',(-11.8915786962281,14.5030673759949,
133.977690925007)) ;
#122604 = CARTESIAN_POINT('Ctrl Pts',(-11.8106152149464,14.4296657361334,
133.708106117249)) ;
#122605 = CARTESIAN_POINT('Ctrl Pts',(-11.7391300458456,14.2842404294125,
133.466176489072)) ;
#122606 = CARTESIAN_POINT('Ctrl Pts',(-11.6829581874867,14.0768884033213,
133.268933114529)) ;
#122607 = CARTESIAN_POINT('Ctrl Pts',(-11.646996920623,13.8219373708246,133.130656743182)) ;
#122608 = CARTESIAN_POINT('Ctrl Pts',(-11.6346497120723,13.5404395793698,
133.061608552357)) ;
#122609 = CARTESIAN_POINT('Ctrl Pts',(-11.6472238284623,13.2491901831122,
133.065198744336)) ;
#122610 = CARTESIAN_POINT('Ctrl Pts',(-11.6849339883728,12.969918720115,133.142151589187)) ;
#122611 = CARTESIAN_POINT('Ctrl Pts',(-11.7452470370939,12.7245501655325,
133.285329855241)) ;
#122612 = CARTESIAN_POINT('Ctrl Pts',(-11.8252651009664,12.5279693790049,
133.485884901424)) ;
#122613 = CARTESIAN_POINT('Ctrl Pts',(-11.9193252668049,12.3961376577074,
133.727590480155)) ;
#122614 = CARTESIAN_POINT('Ctrl Pts',(-12.0221825717366,12.3376103607184,
133.994834780915)) ;
#122615 = CARTESIAN_POINT('Ctrl Pts',(-12.1260592524752,12.3569098768634,
134.265282641821)) ;
#122616 = CARTESIAN_POINT('Ctrl Pts',(-12.2255494729972,12.4527690637887,
134.522706406723)) ;
#122617 = CARTESIAN_POINT('Ctrl Pts',(-12.3132365332066,12.6179594101214,
134.745773282964)) ;
#122618 = CARTESIAN_POINT('Ctrl Pts',(-12.3840649431859,12.8405880896203,
134.919582179066)) ;
#122619 = CARTESIAN_POINT('Ctrl Pts',(-12.4337419164154,13.1065246819692,
135.03142287103)) ;
#122620 = CARTESIAN_POINT('Ctrl Pts',(-12.4589118501879,13.3925179969382,
135.071991071504)) ;
#122621 = CARTESIAN_POINT('Ctrl Pts',(-12.4591401291713,13.6819916806813,
135.039543536461)) ;
#122622 = CARTESIAN_POINT('Ctrl Pts',(-12.4346814882847,13.953724245336,134.934877287873)) ;
#122623 = CARTESIAN_POINT('Ctrl Pts',(-12.388273358954,14.1863734270825,134.7662188792)) ;
#122624 = CARTESIAN_POINT('Ctrl Pts',(-12.3240143345099,14.3643807952629,
134.54544367418)) ;
#122625 = CARTESIAN_POINT('Ctrl Pts',(-12.2470026289218,14.4754559836596,
134.287355923251)) ;
#122626 = CARTESIAN_POINT('Ctrl Pts',(-12.1633433065906,14.5110246745496,
134.009759570375)) ;
#122627 = CARTESIAN_POINT('Ctrl Pts',(-12.0803955015974,14.468706357864,133.73440535818)) ;
#122628 = CARTESIAN_POINT('Ctrl Pts',(-12.0040990392821,14.3514018733064,
133.478353554825)) ;
#122629 = CARTESIAN_POINT('Ctrl Pts',(-11.9410368381369,14.1671964526519,
133.260957267519)) ;
#122630 = CARTESIAN_POINT('Ctrl Pts',(-11.8965833260819,13.9308607646815,
133.098080106287)) ;
#122631 = CARTESIAN_POINT('Ctrl Pts',(-11.8742320407181,13.6570089391064,
132.999605731374)) ;
#122632 = CARTESIAN_POINT('Ctrl Pts',(-11.8766523771408,13.3664658768335,
132.973516684588)) ;
#122633 = CARTESIAN_POINT('Ctrl Pts',(-11.9042552122956,13.0805680543038,
133.021054045171)) ;
#122634 = CARTESIAN_POINT('Ctrl Pts',(-11.9557279014714,12.8190538509803,
133.138321033065)) ;
#122635 = CARTESIAN_POINT('Ctrl Pts',(-12.0286271711589,12.599933753752,133.318014227644)) ;
#122636 = CARTESIAN_POINT('Ctrl Pts',(-12.1172930726756,12.4413956885076,
133.544067361959)) ;
#122637 = CARTESIAN_POINT('Ctrl Pts',(-12.2173395667587,12.3520377966892,
133.803159801022)) ;
#122638 = CARTESIAN_POINT('Ctrl Pts',(-12.3217048099071,12.3397344016033,
134.074918582379)) ;
#122639 = CARTESIAN_POINT('Ctrl Pts',(-12.4237285580169,12.4049383820741,
134.339842915822)) ;
#122640 = CARTESIAN_POINT('Ctrl Pts',(-12.5168448241173,12.5429636135127,
134.57875667178)) ;
#122641 = CARTESIAN_POINT('Ctrl Pts',(-12.5952694191645,12.744355559365,134.774694138797)) ;
#122642 = CARTESIAN_POINT('Ctrl Pts',(-12.6538589035849,12.99435234836,134.912710643206)) ;
#122643 = CARTESIAN_POINT('Ctrl Pts',(-12.6891834098298,13.2741649900779,
134.982863751975)) ;
#122644 = CARTESIAN_POINT('Ctrl Pts',(-12.6996678027026,13.5657204845938,
134.980326914716)) ;
#122645 = CARTESIAN_POINT('Ctrl Pts',(-12.6849427514785,13.8474317542271,
134.904091993754)) ;
#122646 = CARTESIAN_POINT('Ctrl Pts',(-12.6471924840568,14.0971651338937,
134.760804466809)) ;
#122647 = CARTESIAN_POINT('Ctrl Pts',(-12.5893357951143,14.300212406185,134.558553497018)) ;
#122648 = CARTESIAN_POINT('Ctrl Pts',(-12.5166162325577,14.439451037695,134.312982315221)) ;
#122649 = CARTESIAN_POINT('Ctrl Pts',(-12.4353628774632,14.5058688377535,
134.042653457514)) ;
#122650 = CARTESIAN_POINT('Ctrl Pts',(-12.35110971528,14.4952594512815,133.763340940985)) ;
#122651 = CARTESIAN_POINT('Ctrl Pts',(-12.2710628646113,14.4071576201155,
133.496266914171)) ;
#122652 = CARTESIAN_POINT('Ctrl Pts',(-12.2021338287001,14.2488069359853,
133.261802498077)) ;
#122653 = CARTESIAN_POINT('Ctrl Pts',(-12.1497382582167,14.0323324822322,
133.075749850883)) ;
#122654 = CARTESIAN_POINT('Ctrl Pts',(-12.1179861315855,13.7715184536488,
132.949872907299)) ;
#122655 = CARTESIAN_POINT('Ctrl Pts',(-12.1101419823041,13.4849967549257,
132.893761615134)) ;
#122656 = CARTESIAN_POINT('Ctrl Pts',(-12.1277484366407,13.1936953531143,
132.911952789586)) ;
#122657 = CARTESIAN_POINT('Ctrl Pts',(-12.1695498192332,12.9217410379526,
133.001184961085)) ;
#122658 = CARTESIAN_POINT('Ctrl Pts',(-12.2341785842338,12.6826992816898,
133.156739191655)) ;
#122659 = CARTESIAN_POINT('Ctrl Pts',(-12.3173687753878,12.4976839055064,
133.366582282212)) ;
#122660 = CARTESIAN_POINT('Ctrl Pts',(-12.4131346667197,12.37947113767,133.613382407111)) ;
#122661 = CARTESIAN_POINT('Ctrl Pts',(-12.5169846737337,12.3351744205894,
133.883477168164)) ;
#122662 = CARTESIAN_POINT('Ctrl Pts',(-12.620799301784,12.3695012767601,134.153620745015)) ;
#122663 = CARTESIAN_POINT('Ctrl Pts',(-12.718006444483,12.4786183713965,134.404573343174)) ;
#122664 = CARTESIAN_POINT('Ctrl Pts',(-12.8030921061426,12.6556201650726,
134.619996403116)) ;
#122665 = CARTESIAN_POINT('Ctrl Pts',(-12.8703633587299,12.8885376927875,
134.783284046582)) ;
#122666 = CARTESIAN_POINT('Ctrl Pts',(-12.9153284854686,13.1578672301346,
134.881649635031)) ;
#122667 = CARTESIAN_POINT('Ctrl Pts',(-12.9360932774699,13.4488181207259,
134.909004136217)) ;
#122668 = CARTESIAN_POINT('Ctrl Pts',(-12.9313786707726,13.7357351510131,
134.862180593803)) ;
#122669 = CARTESIAN_POINT('Ctrl Pts',(-12.902794866539,14.0000244491373,134.745686603675)) ;
#122670 = CARTESIAN_POINT('Ctrl Pts',(-12.8524484285654,14.2248064092014,
134.565353916144)) ;
#122671 = CARTESIAN_POINT('Ctrl Pts',(-12.7854240568806,14.3907221874245,
134.336542174488)) ;
#122672 = CARTESIAN_POINT('Ctrl Pts',(-12.706579030057,14.4880878252355,134.073042339653)) ;
#122673 = CARTESIAN_POINT('Ctrl Pts',(-12.6227960155401,14.5090844466389,
133.795223033695)) ;
#122674 = CARTESIAN_POINT('Ctrl Pts',(-12.539998525129,14.4517330875411,133.520035240251)) ;
#122675 = CARTESIAN_POINT('Ctrl Pts',(-12.4662105878813,14.3213872706393,
133.271495742536)) ;
#122676 = CARTESIAN_POINT('Ctrl Pts',(-12.4062689631647,14.1266125068475,
133.063268319006)) ;
#122677 = CARTESIAN_POINT('Ctrl Pts',(-12.3655117240341,13.8801112237431,
132.910943391806)) ;
#122678 = CARTESIAN_POINT('Ctrl Pts',(-12.3479181290299,13.6025838419119,
132.826510049742)) ;
#122679 = CARTESIAN_POINT('Ctrl Pts',(-12.3550115270232,13.3122087049322,
132.814182204973)) ;
#122680 = CARTESIAN_POINT('Ctrl Pts',(-12.3873488064402,13.0284663697123,
132.875444965799)) ;
#122681 = CARTESIAN_POINT('Ctrl Pts',(-12.4430942234961,12.7739763347418,
133.005207312266)) ;
#122682 = CARTESIAN_POINT('Ctrl Pts',(-12.5191788386626,12.5655227594086,
133.194325737859)) ;
#122683 = CARTESIAN_POINT('Ctrl Pts',(-12.6106767313811,12.4188417655465,
133.428523192485)) ;
#122684 = CARTESIAN_POINT('Ctrl Pts',(-12.7117766054599,12.343819791052,133.690792434329)) ;
#122685 = CARTESIAN_POINT('Ctrl Pts',(-12.816567838712,12.3461750188478,133.963682834605)) ;
#122686 = CARTESIAN_POINT('Ctrl Pts',(-12.9172505658003,12.4256200301873,
134.224741101302)) ;
#122687 = CARTESIAN_POINT('Ctrl Pts',(-13.0081288677706,12.5766361181176,
134.457068472408)) ;
#122688 = CARTESIAN_POINT('Ctrl Pts',(-13.0830551204936,12.7882866055861,
134.642823016933)) ;
#122689 = CARTESIAN_POINT('Ctrl Pts',(-13.1374659893816,13.0452021106171,
134.768666892341)) ;
#122690 = CARTESIAN_POINT('Ctrl Pts',(-13.1682549286523,13.3293878961544,
134.82547934159)) ;
#122691 = CARTESIAN_POINT('Ctrl Pts',(-13.173880051194,13.6204037391964,134.808769964606)) ;
#122692 = CARTESIAN_POINT('Ctrl Pts',(-13.1546580785961,13.8971497414612,
134.719488338554)) ;
#122693 = CARTESIAN_POINT('Ctrl Pts',(-13.1127775878744,14.1397539982186,
134.564047361394)) ;
#122694 = CARTESIAN_POINT('Ctrl Pts',(-13.0518026076723,14.3313465280224,
134.352767547066)) ;
#122695 = CARTESIAN_POINT('Ctrl Pts',(-12.9771687196265,14.4574458886048,
134.101695813006)) ;
#122696 = CARTESIAN_POINT('Ctrl Pts',(-12.8945575156937,14.509972396165,133.827242524673)) ;
#122697 = CARTESIAN_POINT('Ctrl Pts',(-12.810549262933,14.4843439557881,133.54862424111)) ;
#122698 = CARTESIAN_POINT('Ctrl Pts',(-12.7323948337942,14.3827749210334,
133.287220875815)) ;
#122699 = CARTESIAN_POINT('Ctrl Pts',(-12.6660452885251,14.2124739765949,
133.060271073219)) ;
#122700 = CARTESIAN_POINT('Ctrl Pts',(-12.617078134981,13.9855789270548,132.88409986354)) ;
#122701 = CARTESIAN_POINT('Ctrl Pts',(-12.5897214243873,13.7185805831256,
132.771079224658)) ;
#122702 = CARTESIAN_POINT('Ctrl Pts',(-12.5866426015232,13.4303185672317,
132.728965795836)) ;
#122703 = CARTESIAN_POINT('Ctrl Pts',(-12.6087424481062,13.1417758390937,
132.760436389614)) ;
#122704 = CARTESIAN_POINT('Ctrl Pts',(-12.6553781410414,12.8725286087569,
132.863473470132)) ;
#122705 = CARTESIAN_POINT('Ctrl Pts',(-12.7236698746677,12.6435096250976,
133.029870355786)) ;
#122706 = CARTESIAN_POINT('Ctrl Pts',(-12.8095900819889,12.470154617103,133.24774107517)) ;
#122707 = CARTESIAN_POINT('Ctrl Pts',(-12.9076323750732,12.3650501816311,
133.501043473753)) ;
#122708 = CARTESIAN_POINT('Ctrl Pts',(-13.0118238480069,12.3357586673989,
133.77222183819)) ;
#122709 = CARTESIAN_POINT('Ctrl Pts',(-13.1147537603917,12.3843195645159,
134.039849230825)) ;
#122710 = CARTESIAN_POINT('Ctrl Pts',(-13.2104578166392,12.5073667033233,
134.286277155853)) ;
#122711 = CARTESIAN_POINT('Ctrl Pts',(-13.2923817417662,12.695820098274,134.492504363806)) ;
#122712 = CARTESIAN_POINT('Ctrl Pts',(-13.3556189438732,12.9363650189031,
134.644124622663)) ;
#122713 = CARTESIAN_POINT('Ctrl Pts',(-13.3962896174136,13.2120463476192,
134.729791046471)) ;
#122714 = CARTESIAN_POINT('Ctrl Pts',(-13.4122210373586,13.5022482408363,
134.743260767323)) ;
#122715 = CARTESIAN_POINT('Ctrl Pts',(-13.4028633875802,13.788401757224,134.682652163882)) ;
#122716 = CARTESIAN_POINT('Ctrl Pts',(-13.3699700950396,14.0459452112238,
134.553608753382)) ;
#122717 = CARTESIAN_POINT('Ctrl Pts',(-13.3160081710471,14.261068186074,134.362699423646)) ;
#122718 = CARTESIAN_POINT('Ctrl Pts',(-13.2464308886998,14.4145624952327,
134.126463196777)) ;
#122719 = CARTESIAN_POINT('Ctrl Pts',(-13.1660070259215,14.4980852442795,
133.858308768603)) ;
#122720 = CARTESIAN_POINT('Ctrl Pts',(-13.0818602097117,14.5041312509629,
133.579371099685)) ;
#122721 = CARTESIAN_POINT('Ctrl Pts',(-13.0005482976357,14.4326961548768,
133.308694344568)) ;
#122722 = CARTESIAN_POINT('Ctrl Pts',(-12.9287700664934,14.2894246996344,
133.065951377945)) ;
#122723 = CARTESIAN_POINT('Ctrl Pts',(-12.8719513781794,14.0826506129639,
132.86668732997)) ;
#122724 = CARTESIAN_POINT('Ctrl Pts',(-12.8356455811312,13.8312289814619,
132.727716504135)) ;
#122725 = CARTESIAN_POINT('Ctrl Pts',(-12.8223908350727,13.5479803719868,
132.655735280563)) ;
#122726 = CARTESIAN_POINT('Ctrl Pts',(-12.8343672045851,13.257297898438,132.657650391912)) ;
#122727 = CARTESIAN_POINT('Ctrl Pts',(-12.8711497724761,12.9781390141801,
132.731997740918)) ;
#122728 = CARTESIAN_POINT('Ctrl Pts',(-12.9313756283262,12.7298469956755,
132.874665515828)) ;
#122729 = CARTESIAN_POINT('Ctrl Pts',(-13.0103407400145,12.5331717504731,
133.072398199913)) ;
#122730 = CARTESIAN_POINT('Ctrl Pts',(-13.104520422701,12.3987049958051,133.314282750599)) ;
#122731 = CARTESIAN_POINT('Ctrl Pts',(-13.206651695878,12.3381977038027,133.579601997238)) ;
#122732 = CARTESIAN_POINT('Ctrl Pts',(-13.3114979804847,12.3556286047268,
133.852577072708)) ;
#122733 = CARTESIAN_POINT('Ctrl Pts',(-13.410155841517,12.4484986932729,134.107929156)) ;
#122734 = CARTESIAN_POINT('Ctrl Pts',(-13.4988137139682,12.6124652381156,
134.333636594698)) ;
#122735 = CARTESIAN_POINT('Ctrl Pts',(-13.5699367109128,12.833019455732,134.508418387899)) ;
#122736 = CARTESIAN_POINT('Ctrl Pts',(-13.6204000704498,13.0981217097557,
134.622522835896)) ;
#122737 = CARTESIAN_POINT('Ctrl Pts',(-13.6463216515392,13.3840424084956,
134.665255919507)) ;
#122738 = CARTESIAN_POINT('Ctrl Pts',(-13.6472573616294,13.673804350161,134.63486456253)) ;
#122739 = CARTESIAN_POINT('Ctrl Pts',(-13.6235693400262,13.9458856599705,
134.532515817835)) ;
#122740 = CARTESIAN_POINT('Ctrl Pts',(-13.5776193745675,14.1805609779054,
134.365096818976)) ;
#122741 = CARTESIAN_POINT('Ctrl Pts',(-13.513877843915,14.3602096691543,134.145871518623)) ;
#122742 = CARTESIAN_POINT('Ctrl Pts',(-13.4366571499825,14.47371465445,133.886974753033)) ;
#122743 = CARTESIAN_POINT('Ctrl Pts',(-13.3536493203175,14.5109817362897,
133.611512807046)) ;
#122744 = CARTESIAN_POINT('Ctrl Pts',(-13.270489833554,14.4710234549687,133.335494570733)) ;
#122745 = CARTESIAN_POINT('Ctrl Pts',(-13.1939950003663,14.3558611737084,
133.078903250233)) ;
#122746 = CARTESIAN_POINT('Ctrl Pts',(-13.1304641501164,14.173605953239,132.860148687561)) ;
#122747 = CARTESIAN_POINT('Ctrl Pts',(-13.0853217322533,13.9381264570577,
132.695195172933)) ;
#122748 = CARTESIAN_POINT('Ctrl Pts',(-13.0623501902045,13.6651920565378,
132.594928970547)) ;
#122749 = CARTESIAN_POINT('Ctrl Pts',(-13.0639502382484,13.3755914390975,
132.566529475268)) ;
#122750 = CARTESIAN_POINT('Ctrl Pts',(-13.0910376757839,13.0874856739398,
132.612349617676)) ;
#122751 = CARTESIAN_POINT('Ctrl Pts',(-13.1416877816723,12.8264336867777,
132.72738070205)) ;
#122752 = CARTESIAN_POINT('Ctrl Pts',(-13.2137845958373,12.6060973636301,
132.904801873855)) ;
#122753 = CARTESIAN_POINT('Ctrl Pts',(-13.3022604878942,12.4450312815742,
133.130209138199)) ;
#122754 = CARTESIAN_POINT('Ctrl Pts',(-13.4023564676707,12.3534665915943,
133.389360301153)) ;
#122755 = CARTESIAN_POINT('Ctrl Pts',(-13.5063840325338,12.3390030026154,
133.660229603222)) ;
#122756 = CARTESIAN_POINT('Ctrl Pts',(-13.6088026539799,12.4020393022516,
133.926234642771)) ;
#122757 = CARTESIAN_POINT('Ctrl Pts',(-13.7023554945417,12.5385712255671,
134.166373386109)) ;
#122758 = CARTESIAN_POINT('Ctrl Pts',(-13.7808725717634,12.7373374755761,
134.362748710196)) ;
#122759 = CARTESIAN_POINT('Ctrl Pts',(-13.8402040940885,12.9861208763485,
134.502915815351)) ;
#122760 = CARTESIAN_POINT('Ctrl Pts',(-13.876327184752,13.2660912868939,134.575313990181)) ;
#122761 = CARTESIAN_POINT('Ctrl Pts',(-13.8874746844965,13.5573229974737,
134.57474671631)) ;
#122762 = CARTESIAN_POINT('Ctrl Pts',(-13.8735918642489,13.8386954173301,
134.501090795817)) ;
#122763 = CARTESIAN_POINT('Ctrl Pts',(-13.8363610091342,14.0906009261112,
134.359190696365)) ;
#122764 = CARTESIAN_POINT('Ctrl Pts',(-13.7792326201737,14.2945041038628,
134.159193115425)) ;
#122765 = CARTESIAN_POINT('Ctrl Pts',(-13.7069314087024,14.4361574942565,
133.914839142184)) ;
#122766 = CARTESIAN_POINT('Ctrl Pts',(-13.6254421725762,14.5051117773277,
133.643658661375)) ;
#122767 = CARTESIAN_POINT('Ctrl Pts',(-13.5413998090464,14.4965825882903,
133.36505223233)) ;
#122768 = CARTESIAN_POINT('Ctrl Pts',(-13.4614100970346,14.4113394048867,
133.098272224482)) ;
#122769 = CARTESIAN_POINT('Ctrl Pts',(-13.3917824494901,14.2546478359796,
132.861652683335)) ;
#122770 = CARTESIAN_POINT('Ctrl Pts',(-13.3387306382198,14.0391437504434,
132.673608609)) ;
#122771 = CARTESIAN_POINT('Ctrl Pts',(-13.3063690219606,13.7793415261531,
132.545957337206)) ;
#122772 = CARTESIAN_POINT('Ctrl Pts',(-13.2978117868869,13.4941094654563,
132.487858778329)) ;
#122773 = CARTESIAN_POINT('Ctrl Pts',(-13.3145790512622,13.2026873964626,
132.503605828306)) ;
#122774 = CARTESIAN_POINT('Ctrl Pts',(-13.3558347243656,12.9288332689777,
132.591113022334)) ;
#122775 = CARTESIAN_POINT('Ctrl Pts',(-13.42001442131,12.6885083227908,132.745324620566)) ;
#122776 = CARTESIAN_POINT('Ctrl Pts',(-13.502239679633,12.5026390523848,132.95253565952)) ;
#122777 = CARTESIAN_POINT('Ctrl Pts',(-13.5982356435554,12.3816810142256,
133.199819473708)) ;
#122778 = CARTESIAN_POINT('Ctrl Pts',(-13.7013793589073,12.3354826601101,
133.4680451402)) ;
#122779 = CARTESIAN_POINT('Ctrl Pts',(-13.80552054206,12.3671988695935,133.739067392066)) ;
#122780 = CARTESIAN_POINT('Ctrl Pts',(-13.9034200313392,12.4748749590594,
133.991897701478)) ;
#122781 = CARTESIAN_POINT('Ctrl Pts',(-13.9886532302031,12.6498955161038,
134.207834562929)) ;
#122782 = CARTESIAN_POINT('Ctrl Pts',(-14.0562984562977,12.8801431271714,
134.372370038988)) ;
#122783 = CARTESIAN_POINT('Ctrl Pts',(-14.1022223995616,13.1504415256103,
134.473311483202)) ;
#122784 = CARTESIAN_POINT('Ctrl Pts',(-14.123569864062,13.4387392039499,134.502646409052)) ;
#122785 = CARTESIAN_POINT('Ctrl Pts',(-14.1196852055216,13.7280473627643,
134.458016194927)) ;
#122786 = CARTESIAN_POINT('Ctrl Pts',(-14.0916226131084,13.9932362270437,
134.343028102369)) ;
#122787 = CARTESIAN_POINT('Ctrl Pts',(-14.0420866562791,14.2186784013421,
134.165196371218)) ;
#122788 = CARTESIAN_POINT('Ctrl Pts',(-13.9751431455741,14.3872014595801,
133.936454641031)) ;
#122789 = CARTESIAN_POINT('Ctrl Pts',(-13.8968885105808,14.4862165376707,
133.674833892658)) ;
#122790 = CARTESIAN_POINT('Ctrl Pts',(-13.8128617180063,14.5095010534955,
133.396175956052)) ;
#122791 = CARTESIAN_POINT('Ctrl Pts',(-13.7304497643329,14.4548476370639,
133.12233385827)) ;
#122792 = CARTESIAN_POINT('Ctrl Pts',(-13.6557838577664,14.3259645840264,
132.871005987492)) ;
#122793 = CARTESIAN_POINT('Ctrl Pts',(-13.5953724007658,14.132023950122,132.661341229371)) ;
#122794 = CARTESIAN_POINT('Ctrl Pts',(-13.5543327518314,13.8890686102105,
132.508494471355)) ;
#122795 = CARTESIAN_POINT('Ctrl Pts',(-13.5358381663009,13.6109286818878,
132.421258113055)) ;
#122796 = CARTESIAN_POINT('Ctrl Pts',(-13.542226996446,13.3205779167508,132.406873150315)) ;
#122797 = CARTESIAN_POINT('Ctrl Pts',(-13.5739794264152,13.0356408417454,
132.466340476707)) ;
#122798 = CARTESIAN_POINT('Ctrl Pts',(-13.6288864921363,12.7811566928917,
132.593791195391)) ;
#122799 = CARTESIAN_POINT('Ctrl Pts',(-13.7044062779157,12.5709849974497,
132.78125363208)) ;
#122800 = CARTESIAN_POINT('Ctrl Pts',(-13.7955344981284,12.4221765780121,
133.014364402187)) ;
#122801 = CARTESIAN_POINT('Ctrl Pts',(-13.8968781749281,12.3447406523641,
133.277205956951)) ;
#122802 = CARTESIAN_POINT('Ctrl Pts',(-14.0015137983245,12.3451621896592,
133.549692248237)) ;
#122803 = CARTESIAN_POINT('Ctrl Pts',(-14.1021214510041,12.4221618578868,
133.810621215989)) ;
#122804 = CARTESIAN_POINT('Ctrl Pts',(-14.1934712046152,12.5713294888185,
134.04429329116)) ;
#122805 = CARTESIAN_POINT('Ctrl Pts',(-14.2688631560375,12.781135912573,134.231447471873)) ;
#122806 = CARTESIAN_POINT('Ctrl Pts',(-14.3239990336241,13.0373855963871,
134.359354214164)) ;
#122807 = CARTESIAN_POINT('Ctrl Pts',(-14.3554632461864,13.3202249658799,
134.418237999123)) ;
#122808 = CARTESIAN_POINT('Ctrl Pts',(-14.3618511494396,13.6126651184226,
134.403601562198)) ;
#122809 = CARTESIAN_POINT('Ctrl Pts',(-14.3433707383352,13.8891096825995,
134.316608545591)) ;
#122810 = CARTESIAN_POINT('Ctrl Pts',(-14.3020343167185,14.1334577296797,
134.162685402609)) ;
#122811 = CARTESIAN_POINT('Ctrl Pts',(-14.2417808956239,14.3262011562841,
133.95363095538)) ;
#122812 = CARTESIAN_POINT('Ctrl Pts',(-14.1670021264005,14.4552702569289,
133.701921829577)) ;
#122813 = CARTESIAN_POINT('Ctrl Pts',(-14.0844340238259,14.5094659908496,
133.427572654941)) ;
#122814 = CARTESIAN_POINT('Ctrl Pts',(-14.0009203738356,14.4862792648155,
133.150618168943)) ;
#122815 = CARTESIAN_POINT('Ctrl Pts',(-13.9222696214615,14.3867194046613,
132.887667382131)) ;
#122816 = CARTESIAN_POINT('Ctrl Pts',(-13.8555447933731,14.2183273088974,
132.659645946051)) ;
#122817 = CARTESIAN_POINT('Ctrl Pts',(-13.8058821838959,13.992244078071,132.481355163551)) ;
#122818 = CARTESIAN_POINT('Ctrl Pts',(-13.7779670985824,13.7260908725509,
132.366711198007)) ;
#122819 = CARTESIAN_POINT('Ctrl Pts',(-13.7741339235042,13.4392990631296,
132.322525920907)) ;
#122820 = CARTESIAN_POINT('Ctrl Pts',(-13.7956345554261,13.1491383959326,
132.352086669861)) ;
#122821 = CARTESIAN_POINT('Ctrl Pts',(-13.8414238224562,12.8801381500525,
132.452791421209)) ;
#122822 = CARTESIAN_POINT('Ctrl Pts',(-13.9094358836924,12.64883120769,132.618229163413)) ;
#122823 = CARTESIAN_POINT('Ctrl Pts',(-13.9945003827061,12.4746173054018,
132.833772527183)) ;
#122824 = CARTESIAN_POINT('Ctrl Pts',(-14.092526137208,12.3669410554066,133.086930422302)) ;
#122825 = CARTESIAN_POINT('Ctrl Pts',(-14.1966145933381,12.3355244461353,
133.35782177204)) ;
#122826 = CARTESIAN_POINT('Ctrl Pts',(-14.2996113408853,12.3818824720289,
133.625656611254)) ;
#122827 = CARTESIAN_POINT('Ctrl Pts',(-14.3954499004576,12.5024424639559,
133.872548813345)) ;
#122828 = CARTESIAN_POINT('Ctrl Pts',(-14.4782507258047,12.6900860834509,
134.081174564054)) ;
#122829 = CARTESIAN_POINT('Ctrl Pts',(-14.5418899408693,12.9290694340201,
134.234032679536)) ;
#122830 = CARTESIAN_POINT('Ctrl Pts',(-14.5832089306858,13.2033803581446,
134.32166291928)) ;
#122831 = CARTESIAN_POINT('Ctrl Pts',(-14.5998913013211,13.4938855393019,
134.33727238423)) ;
#122832 = CARTESIAN_POINT('Ctrl Pts',(-14.5913281946562,13.7798209622441,
134.27907156831)) ;
#122833 = CARTESIAN_POINT('Ctrl Pts',(-14.5588933837246,14.0398148496058,
134.151181115851)) ;
#122834 = CARTESIAN_POINT('Ctrl Pts',(-14.5055772883064,14.2555982023478,
133.962265861814)) ;
#122835 = CARTESIAN_POINT('Ctrl Pts',(-14.4363858406778,14.4112165805385,
133.727140752466)) ;
#122836 = CARTESIAN_POINT('Ctrl Pts',(-14.3558616395475,14.4969136071728,
133.458576254405)) ;
#122837 = CARTESIAN_POINT('Ctrl Pts',(-14.2721531493714,14.5049696606859,
133.18108471151)) ;
#122838 = CARTESIAN_POINT('Ctrl Pts',(-14.1907040785466,14.4360248987559,
132.910029619532)) ;
#122839 = CARTESIAN_POINT('Ctrl Pts',(-14.1184830111954,14.2945753095186,
132.665954434727)) ;
#122840 = CARTESIAN_POINT('Ctrl Pts',(-14.0611734388472,14.0897547152948,
132.465297187422)) ;
#122841 = CARTESIAN_POINT('Ctrl Pts',(-14.0241626277862,13.8386999371902,
132.324168957696)) ;
#122842 = CARTESIAN_POINT('Ctrl Pts',(-14.0101940089266,13.557404245294,132.250264713925)) ;
#122843 = CARTESIAN_POINT('Ctrl Pts',(-14.0215298956694,13.2644127915957,
132.250046158682)) ;
#122844 = CARTESIAN_POINT('Ctrl Pts',(-14.0575338067527,12.9862193835362,
132.322298184115)) ;
#122845 = CARTESIAN_POINT('Ctrl Pts',(-14.11688454634,12.7371110279746,132.462483680312)) ;
#122846 = CARTESIAN_POINT('Ctrl Pts',(-14.1955901076799,12.5380202146654,
132.659347067288)) ;
#122847 = CARTESIAN_POINT('Ctrl Pts',(-14.28946201566,12.4015272035531,132.900325805036)) ;
#122848 = CARTESIAN_POINT('Ctrl Pts',(-14.3915176998432,12.3389469979449,
133.165397994997)) ;
#122849 = CARTESIAN_POINT('Ctrl Pts',(-14.495856941834,12.3537865285607,133.437069895814)) ;
#122850 = CARTESIAN_POINT('Ctrl Pts',(-14.5953958091729,12.4449099781865,
133.694784504948)) ;
#122851 = CARTESIAN_POINT('Ctrl Pts',(-14.6843904512869,12.6072328334928,
133.921485691051)) ;
#122852 = CARTESIAN_POINT('Ctrl Pts',(-14.7559156143078,12.8259752277409,
134.097497642623)) ;
#122853 = CARTESIAN_POINT('Ctrl Pts',(-14.8069969604636,13.0894865992637,
134.213476347008)) ;
#122854 = CARTESIAN_POINT('Ctrl Pts',(-14.8337697603498,13.3763086885043,
134.258547210058)) ;
#122855 = CARTESIAN_POINT('Ctrl Pts',(-14.8353123618202,13.6661024734113,
134.229945019376)) ;
#122856 = CARTESIAN_POINT('Ctrl Pts',(-14.8124440803992,13.9378774690874,
134.130130172042)) ;
#122857 = CARTESIAN_POINT('Ctrl Pts',(-14.7669543359677,14.1747933111433,
133.963938244878)) ;
#122858 = CARTESIAN_POINT('Ctrl Pts',(-14.7037362321117,14.3556679919274,
133.746303038478)) ;
#122859 = CARTESIAN_POINT('Ctrl Pts',(-14.6272249106364,14.4711053285872,
133.489636572354)) ;
#122860 = CARTESIAN_POINT('Ctrl Pts',(-14.5437193293295,14.5111709794694,
133.21248187099)) ;
#122861 = CARTESIAN_POINT('Ctrl Pts',(-14.4603753611253,14.4729025358904,
132.935881904141)) ;
#122862 = CARTESIAN_POINT('Ctrl Pts',(-14.3839774531889,14.3605014207988,
132.679746155635)) ;
#122863 = CARTESIAN_POINT('Ctrl Pts',(-14.3196308997706,14.1789799465746,
132.458418098484)) ;
#122864 = CARTESIAN_POINT('Ctrl Pts',(-14.2741191671532,13.9453130634453,
132.292485354684)) ;
#122865 = CARTESIAN_POINT('Ctrl Pts',(-14.2504732824165,13.6736132719233,
132.190294327821)) ;
#122866 = CARTESIAN_POINT('Ctrl Pts',(-14.2513173292015,13.3843416076431,
132.159699879319)) ;
#122867 = CARTESIAN_POINT('Ctrl Pts',(-14.2776743807249,13.0956424209517,
132.20336504898)) ;
#122868 = CARTESIAN_POINT('Ctrl Pts',(-14.3276746731947,12.8335786861196,
132.31649173796)) ;
#122869 = CARTESIAN_POINT('Ctrl Pts',(-14.3992226458396,12.611652190356,132.492301020647)) ;
#122870 = CARTESIAN_POINT('Ctrl Pts',(-14.4874521229701,12.4486057551385,
132.716936908001)) ;
#122871 = CARTESIAN_POINT('Ctrl Pts',(-14.5869437822239,12.3551665725231,
132.974446240664)) ;
#122872 = CARTESIAN_POINT('Ctrl Pts',(-14.6912604023576,12.338311146402,133.246052457304)) ;
#122873 = CARTESIAN_POINT('Ctrl Pts',(-14.7936701073007,12.39913191908,133.512086338097)) ;
#122874 = CARTESIAN_POINT('Ctrl Pts',(-14.8875591251362,12.5336134533254,
133.753205453511)) ;
#122875 = CARTESIAN_POINT('Ctrl Pts',(-14.9666002083636,12.7304748931974,
133.951130887302)) ;
#122876 = CARTESIAN_POINT('Ctrl Pts',(-15.0268934696713,12.9801495362985,
134.093853087901)) ;
#122877 = CARTESIAN_POINT('Ctrl Pts',(-15.0633119226926,13.2569932871313,
134.1674226943)) ;
#122878 = CARTESIAN_POINT('Ctrl Pts',(-15.0753247260425,13.5493203158773,
134.169247540756)) ;
#122879 = CARTESIAN_POINT('Ctrl Pts',(-15.0620951374536,13.8310611217576,
134.097523512761)) ;
#122880 = CARTESIAN_POINT('Ctrl Pts',(-15.0254414043506,14.0843639820839,
133.957268069224)) ;
#122881 = CARTESIAN_POINT('Ctrl Pts',(-14.9688116918277,14.2896245798539,
133.758745314845)) ;
#122882 = CARTESIAN_POINT('Ctrl Pts',(-14.8969851728588,14.433006390985,133.515831551673)) ;
#122883 = CARTESIAN_POINT('Ctrl Pts',(-14.8156323832822,14.5042107644556,
133.245031813908)) ;
#122884 = CARTESIAN_POINT('Ctrl Pts',(-14.7315386625411,14.4979449677576,
132.96626438036)) ;
#122885 = CARTESIAN_POINT('Ctrl Pts',(-14.6511153589677,14.4144600975177,
132.698120714996)) ;
#122886 = CARTESIAN_POINT('Ctrl Pts',(-14.5812309184614,14.259520873967,132.46078302777)) ;
#122887 = CARTESIAN_POINT('Ctrl Pts',(-14.5278024226519,14.0462147796788,
132.271741524007)) ;
#122888 = CARTESIAN_POINT('Ctrl Pts',(-14.4947222340059,13.7868051984224,
132.141911296577)) ;
#122889 = CARTESIAN_POINT('Ctrl Pts',(-14.4855193570548,13.5027355977882,
132.082011946942)) ;
#122890 = CARTESIAN_POINT('Ctrl Pts',(-14.5014599681923,13.2114163358095,
132.095374697993)) ;
#122891 = CARTESIAN_POINT('Ctrl Pts',(-14.5421822561904,12.9359342039492,
132.181213543049)) ;
#122892 = CARTESIAN_POINT('Ctrl Pts',(-14.6055653322678,12.6951561372944,
132.33320802425)) ;
#122893 = CARTESIAN_POINT('Ctrl Pts',(-14.6873122286846,12.5073060889563,
132.539005348311)) ;
#122894 = CARTESIAN_POINT('Ctrl Pts',(-14.7831217899283,12.3841592537523,
132.785703089486)) ;
#122895 = CARTESIAN_POINT('Ctrl Pts',(-14.8861739591066,12.3356200242118,
133.053655565713)) ;
#122896 = CARTESIAN_POINT('Ctrl Pts',(-14.9907676880009,12.3655842342963,
133.325869841831)) ;
#122897 = CARTESIAN_POINT('Ctrl Pts',(-15.0881721710896,12.4702048662911,
133.57752343002)) ;
#122898 = CARTESIAN_POINT('Ctrl Pts',(-15.1745656232195,12.6448837990351,
133.796562666015)) ;
#122899 = CARTESIAN_POINT('Ctrl Pts',(-15.2423252658601,12.8725084203653,
133.96163895876)) ;
#122900 = CARTESIAN_POINT('Ctrl Pts',(-15.2891967482421,13.1434988264021,
134.065150989214)) ;
#122901 = CARTESIAN_POINT('Ctrl Pts',(-15.3110173033622,13.4301737730148,
134.096029449475)) ;
#122902 = CARTESIAN_POINT('Ctrl Pts',(-15.3080372177454,13.718779591721,134.054168270157)) ;
#122903 = CARTESIAN_POINT('Ctrl Pts',(-15.2804060867555,13.9870154535706,
133.940172267824)) ;
#122904 = CARTESIAN_POINT('Ctrl Pts',(-15.2316377774267,14.2124398495338,
133.764769336654)) ;
#122905 = CARTESIAN_POINT('Ctrl Pts',(-15.165220452902,14.3830654639858,133.537573308493)) ;
#122906 = CARTESIAN_POINT('Ctrl Pts',(-15.086831973333,14.4846609671348,133.275405165143)) ;
#122907 = CARTESIAN_POINT('Ctrl Pts',(-15.0028388335443,14.5097913596576,
132.99683728162)) ;
#122908 = CARTESIAN_POINT('Ctrl Pts',(-14.9206500675865,14.4576092834796,
132.723792129969)) ;
#122909 = CARTESIAN_POINT('Ctrl Pts',(-14.8454721612017,14.3304830753539,
132.470882970049)) ;
#122910 = CARTESIAN_POINT('Ctrl Pts',(-14.7847088609425,14.1386182913456,
132.260264003398)) ;
#122911 = CARTESIAN_POINT('Ctrl Pts',(-14.743001227268,13.8965845637284,132.105417644869)) ;
#122912 = CARTESIAN_POINT('Ctrl Pts',(-14.7238223056134,13.6198364139058,
132.016265937607)) ;
#122913 = CARTESIAN_POINT('Ctrl Pts',(-14.7294887108316,13.3288843077371,
131.999686789623)) ;
#122914 = CARTESIAN_POINT('Ctrl Pts',(-14.7603420714365,13.0447398144614,
132.056683740009)) ;
#122915 = CARTESIAN_POINT('Ctrl Pts',(-14.8146479427189,12.7881834818384,
132.182276189974)) ;
#122916 = CARTESIAN_POINT('Ctrl Pts',(-14.8900730017905,12.5755908845443,
132.369299666731)) ;
#122917 = CARTESIAN_POINT('Ctrl Pts',(-14.9804283663031,12.4257573634701,
132.600310180538)) ;
#122918 = CARTESIAN_POINT('Ctrl Pts',(-15.081355257857,12.3460112100503,132.861995469573)) ;
#122919 = CARTESIAN_POINT('Ctrl Pts',(-15.1861080584628,12.3439532777376,
133.134786433152)) ;
#122920 = CARTESIAN_POINT('Ctrl Pts',(-15.2871434627303,12.4188219737117,
133.396894492333)) ;
#122921 = CARTESIAN_POINT('Ctrl Pts',(-15.3791342092762,12.5668342389243,
133.632321418082)) ;
#122922 = CARTESIAN_POINT('Ctrl Pts',(-15.4545799026391,12.7739567012615,
133.819824457066)) ;
#122923 = CARTESIAN_POINT('Ctrl Pts',(-15.5105014700374,13.0292277214245,
133.949992547475)) ;
#122924 = CARTESIAN_POINT('Ctrl Pts',(-15.54268567825,13.3121169680532,134.010916269422)) ;
#122925 = CARTESIAN_POINT('Ctrl Pts',(-15.5498365649966,13.603671342882,133.998623037179)) ;
#122926 = CARTESIAN_POINT('Ctrl Pts',(-15.531946047433,13.8822011658837,133.913179480728)) ;
#122927 = CARTESIAN_POINT('Ctrl Pts',(-15.491392435008,14.1265341471654,133.76170716662)) ;
#122928 = CARTESIAN_POINT('Ctrl Pts',(-15.431540081892,14.3215277974717,133.553749376831)) ;
#122929 = CARTESIAN_POINT('Ctrl Pts',(-15.3571603450366,14.4523872873454,
133.303244580285)) ;
#122930 = CARTESIAN_POINT('Ctrl Pts',(-15.2748106437101,14.509081275177,133.029560282638)) ;
#122931 = CARTESIAN_POINT('Ctrl Pts',(-15.1906905864766,14.4877530377578,
132.750612125616)) ;
#122932 = CARTESIAN_POINT('Ctrl Pts',(-15.1123084559039,14.3906972119634,
132.488655125181)) ;
#122933 = CARTESIAN_POINT('Ctrl Pts',(-15.0450774786089,14.2242126836462,
132.259127840119)) ;
#122934 = CARTESIAN_POINT('Ctrl Pts',(-14.9949477568096,14.0000453573048,
132.079539850124)) ;
#122935 = CARTESIAN_POINT('Ctrl Pts',(-14.9662169923433,13.7349940893193,
131.962516118515)) ;
#122936 = CARTESIAN_POINT('Ctrl Pts',(-14.9617452970706,13.4462937932098,
131.916206457482)) ;
#122937 = CARTESIAN_POINT('Ctrl Pts',(-14.9822951077096,13.1586523998495,
131.943317162503)) ;
#122938 = CARTESIAN_POINT('Ctrl Pts',(-15.0277849352445,12.8863235955885,
132.042839199694)) ;
#122939 = CARTESIAN_POINT('Ctrl Pts',(-15.0948411666316,12.6553854618845,
132.205713830206)) ;
#122940 = CARTESIAN_POINT('Ctrl Pts',(-15.1795278177596,12.4787538622729,
132.420093453233)) ;
#122941 = CARTESIAN_POINT('Ctrl Pts',(-15.2776667934257,12.3688114819393,
132.673464609376)) ;
#122942 = CARTESIAN_POINT('Ctrl Pts',(-15.3812344932646,12.3354319131045,
132.942973836331)) ;
#122943 = CARTESIAN_POINT('Ctrl Pts',(-15.4844363162764,12.3792576345139,
133.211386539826)) ;
#122944 = CARTESIAN_POINT('Ctrl Pts',(-15.5811089769105,12.4988399158766,
133.460512436159)) ;
#122945 = CARTESIAN_POINT('Ctrl Pts',(-15.6637127965401,12.6835118837374,
133.668813420161)) ;
#122946 = CARTESIAN_POINT('Ctrl Pts',(-15.728149203225,12.9214924452222,133.823933063528)) ;
#122947 = CARTESIAN_POINT('Ctrl Pts',(-15.7701936666408,13.1954917190088,
133.913637309434)) ;
#122948 = CARTESIAN_POINT('Ctrl Pts',(-15.7875791085066,13.4865486647074,
133.931220140978)) ;
#122949 = CARTESIAN_POINT('Ctrl Pts',(-15.7796291542385,13.7724716992733,
133.874855409992)) ;
#122950 = CARTESIAN_POINT('Ctrl Pts',(-15.7479919520967,14.0322260172615,
133.749447091464)) ;
#122951 = CARTESIAN_POINT('Ctrl Pts',(-15.695387454676,14.249618629869,133.56264873374)) ;
#122952 = CARTESIAN_POINT('Ctrl Pts',(-15.6261515803863,14.4079187286369,
133.327193888207)) ;
#122953 = CARTESIAN_POINT('Ctrl Pts',(-15.5465490261103,14.4951289707047,
133.061613614476)) ;
#122954 = CARTESIAN_POINT('Ctrl Pts',(-15.4624323059552,14.5060206612055,
132.782752303538)) ;
#122955 = CARTESIAN_POINT('Ctrl Pts',(-15.3805684268842,14.4388851270518,
132.51038836699)) ;
#122956 = CARTESIAN_POINT('Ctrl Pts',(-15.3079732071055,14.2990478381217,
132.265189265335)) ;
#122957 = CARTESIAN_POINT('Ctrl Pts',(-15.2503508442927,14.0962769263581,
132.063706906888)) ;
#122958 = CARTESIAN_POINT('Ctrl Pts',(-15.2126467032428,13.8463550292072,
131.920546038618)) ;
#122959 = CARTESIAN_POINT('Ctrl Pts',(-15.1980783490908,13.5643760642883,
131.844749375842)) ;
#122960 = CARTESIAN_POINT('Ctrl Pts',(-15.208492795854,13.2747378724678,131.842228274416)) ;
#122961 = CARTESIAN_POINT('Ctrl Pts',(-15.2439809385834,12.9934295019574,
131.912682502554)) ;
#122962 = CARTESIAN_POINT('Ctrl Pts',(-15.3026382333439,12.7438066422354,
132.050923610819)) ;
#122963 = CARTESIAN_POINT('Ctrl Pts',(-15.3810068220172,12.542694227186,132.246728650902)) ;
#122964 = CARTESIAN_POINT('Ctrl Pts',(-15.4741969738666,12.4046935574579,
132.485839130881)) ;
#122965 = CARTESIAN_POINT('Ctrl Pts',(-15.5763327366627,12.3396331607935,
132.751061057437)) ;
#122966 = CARTESIAN_POINT('Ctrl Pts',(-15.680579517544,12.3522551180279,133.022505742555)) ;
#122967 = CARTESIAN_POINT('Ctrl Pts',(-15.7803492810426,12.4411586824075,
133.280892840196)) ;
#122968 = CARTESIAN_POINT('Ctrl Pts',(-15.8697167426766,12.6013770610415,
133.508706785249)) ;
#122969 = CARTESIAN_POINT('Ctrl Pts',(-15.9419214668062,12.819071741669,133.686638072034)) ;
#122970 = CARTESIAN_POINT('Ctrl Pts',(-15.9935297236979,13.0807347129293,
133.804263305628)) ;
#122971 = CARTESIAN_POINT('Ctrl Pts',(-16.0211044801934,13.3675409458687,
133.851621859569)) ;
#122972 = CARTESIAN_POINT('Ctrl Pts',(-16.0234843448819,13.6570979950049,
133.825528484065)) ;
#122973 = CARTESIAN_POINT('Ctrl Pts',(-16.000995765069,13.9319894333905,133.726516831796)) ;
#122974 = CARTESIAN_POINT('Ctrl Pts',(-15.9565643522182,14.1676085516927,
133.563784888754)) ;
#122975 = CARTESIAN_POINT('Ctrl Pts',(-15.8933708369746,14.3519029701599,
133.345953408387)) ;
#122976 = CARTESIAN_POINT('Ctrl Pts',(-15.8172885156954,14.4687263887883,
133.09063231366)) ;
#122977 = CARTESIAN_POINT('Ctrl Pts',(-15.7341653709837,14.5110206737837,
132.814693127497)) ;
#122978 = CARTESIAN_POINT('Ctrl Pts',(-15.6507620381886,14.475483911121,132.537948900306)) ;
#122979 = CARTESIAN_POINT('Ctrl Pts',(-15.5735490936641,14.3641243915887,
132.279183520569)) ;
#122980 = CARTESIAN_POINT('Ctrl Pts',(-15.5093304300685,14.185998118253,132.058533710743)) ;
#122981 = CARTESIAN_POINT('Ctrl Pts',(-15.462903310711,13.9527739610766,131.889757868276)) ;
#122982 = CARTESIAN_POINT('Ctrl Pts',(-15.4385984833737,13.6818171752754,
131.785645579049)) ;
#122983 = CARTESIAN_POINT('Ctrl Pts',(-15.4387626916475,13.392345635537,131.753011052265)) ;
#122984 = CARTESIAN_POINT('Ctrl Pts',(-15.464243148025,13.1044624962765,131.794260353384)) ;
#122985 = CARTESIAN_POINT('Ctrl Pts',(-15.5138238528878,12.8400819723837,
131.905988502202)) ;
#122986 = CARTESIAN_POINT('Ctrl Pts',(-15.5846558690521,12.6174282729713,
132.079803115879)) ;
#122987 = CARTESIAN_POINT('Ctrl Pts',(-15.6725999837267,12.452181454216,132.303549807549)) ;
#122988 = CARTESIAN_POINT('Ctrl Pts',(-15.7718997242251,12.3567834927398,
132.560491848969)) ;
#122989 = CARTESIAN_POINT('Ctrl Pts',(-15.875884107787,12.3377092342152,132.831217635272)) ;
#122990 = CARTESIAN_POINT('Ctrl Pts',(-15.9785433015848,12.396207648245,133.097951008103)) ;
#122991 = CARTESIAN_POINT('Ctrl Pts',(-16.0729880468236,12.5290433262916,
133.340617185065)) ;
#122992 = CARTESIAN_POINT('Ctrl Pts',(-16.1524039006371,12.7244086521529,
133.539649727989)) ;
#122993 = CARTESIAN_POINT('Ctrl Pts',(-16.2129909856311,12.970950220754,133.683466380543)) ;
#122994 = CARTESIAN_POINT('Ctrl Pts',(-16.2505098060545,13.24944047257,133.759968218975)) ;
#122995 = CARTESIAN_POINT('Ctrl Pts',(-16.263091069111,13.5418969111079,133.763438478373)) ;
#122996 = CARTESIAN_POINT('Ctrl Pts',(-16.250600258302,13.8230885860474,133.693996985821)) ;
#122997 = CARTESIAN_POINT('Ctrl Pts',(-16.2145955295992,14.0775912623992,
133.555629667295)) ;
#122998 = CARTESIAN_POINT('Ctrl Pts',(-16.1585655383278,14.2842120208938,
133.358900373682)) ;
#122999 = CARTESIAN_POINT('Ctrl Pts',(-16.0870153349153,14.4299776255762,
133.11674202411)) ;
#123000 = CARTESIAN_POINT('Ctrl Pts',(-16.0054619777215,14.5033310573158,
132.845209708425)) ;
#123001 = CARTESIAN_POINT('Ctrl Pts',(-15.9218838426601,14.4992417521952,
132.568160042897)) ;
#123002 = CARTESIAN_POINT('Ctrl Pts',(-15.8410076302058,14.4177938992537,
132.298589352133)) ;
#123003 = CARTESIAN_POINT('Ctrl Pts',(-15.7708993179965,14.2650804914184,
132.060678070363)) ;
#123004 = CARTESIAN_POINT('Ctrl Pts',(-15.7168610518159,14.0529680000281,
131.86979828044)) ;
#123005 = CARTESIAN_POINT('Ctrl Pts',(-15.6831746324261,13.7955268691578,
131.738309075754)) ;
#123006 = CARTESIAN_POINT('Ctrl Pts',(-15.6731981033107,13.5095707979293,
131.675874334833)) ;
#123007 = CARTESIAN_POINT('Ctrl Pts',(-15.6885514732525,13.2189035142274,
131.687611361385)) ;
#123008 = CARTESIAN_POINT('Ctrl Pts',(-15.7284480149979,12.9437119836813,
131.771151515632)) ;
#123009 = CARTESIAN_POINT('Ctrl Pts',(-15.7910818229785,12.7018112503585,
131.921000136973)) ;
#123010 = CARTESIAN_POINT('Ctrl Pts',(-15.8727068944032,12.5115374305282,
132.126301688539)) ;
#123011 = CARTESIAN_POINT('Ctrl Pts',(-15.9680538025931,12.3865362301687,
132.371709386679)) ;
#123012 = CARTESIAN_POINT('Ctrl Pts',(-16.0715247163839,12.3360647675439,
132.640708439766)) ;
#123013 = CARTESIAN_POINT('Ctrl Pts',(-16.174745238061,12.3630945112241,132.909384991678)) ;
#123014 = CARTESIAN_POINT('Ctrl Pts',(-16.2735878679855,12.466576968382,133.164838729843)) ;
#123015 = CARTESIAN_POINT('Ctrl Pts',(-16.3596505741579,12.6378737412179,
133.38322435223)) ;
#123016 = CARTESIAN_POINT('Ctrl Pts',(-16.4286413429061,12.8661806777279,
133.551573412885)) ;
#123017 = CARTESIAN_POINT('Ctrl Pts',(-16.4756920792434,13.133327748888,133.655983965445)) ;
#123018 = CARTESIAN_POINT('Ctrl Pts',(-16.4985958888438,13.4221934769942,
133.689725454439)) ;
#123019 = CARTESIAN_POINT('Ctrl Pts',(-16.4962280317727,13.7107571262916,
133.649695546072)) ;
#123020 = CARTESIAN_POINT('Ctrl Pts',(-16.4693138102463,13.9798563789946,
133.537799466451)) ;
#123021 = CARTESIAN_POINT('Ctrl Pts',(-16.420975161463,14.2070905645433,133.363583331429)) ;
#123022 = CARTESIAN_POINT('Ctrl Pts',(-16.3550739984878,14.3790287585347,
133.137956843767)) ;
#123023 = CARTESIAN_POINT('Ctrl Pts',(-16.2771937418169,14.4826462603949,
132.877370348531)) ;
#123024 = CARTESIAN_POINT('Ctrl Pts',(-16.1929644857992,14.5101765741511,
132.597990225894)) ;
#123025 = CARTESIAN_POINT('Ctrl Pts',(-16.1108016882086,14.4602520915312,
132.325086668321)) ;
#123026 = CARTESIAN_POINT('Ctrl Pts',(-16.0352286482908,14.3349862853441,
132.070979800291)) ;
#123027 = CARTESIAN_POINT('Ctrl Pts',(-15.9742472099228,14.1459035788167,
131.859889211481)) ;
#123028 = CARTESIAN_POINT('Ctrl Pts',(-15.9316559559395,13.9042673527481,
131.702317007935)) ;
#123029 = CARTESIAN_POINT('Ctrl Pts',(-15.9118084366381,13.6274932797063,
131.611137097283)) ;
#123030 = CARTESIAN_POINT('Ctrl Pts',(-15.9167751273571,13.3375399739688,
131.592610463019)) ;
#123031 = CARTESIAN_POINT('Ctrl Pts',(-15.9467825641615,13.0529654851711,
131.647157462469)) ;
#123032 = CARTESIAN_POINT('Ctrl Pts',(-16.0009860132793,12.7935418575334,
131.77218792311)) ;
#123033 = CARTESIAN_POINT('Ctrl Pts',(-16.0752207882529,12.5815360245405,
131.956050381901)) ;
#123034 = CARTESIAN_POINT('Ctrl Pts',(-16.165618131101,12.4287257654979,132.187006003975)) ;
#123035 = CARTESIAN_POINT('Ctrl Pts',(-16.2665986908856,12.3470719681604,
132.448782400074)) ;
#123036 = CARTESIAN_POINT('Ctrl Pts',(-16.371126927041,12.3430683476044,132.720984392827)) ;
#123037 = CARTESIAN_POINT('Ctrl Pts',(-16.4719895721837,12.4155936903918,
132.982699381913)) ;
#123038 = CARTESIAN_POINT('Ctrl Pts',(-16.5641213124433,12.5608877107137,
133.218641097177)) ;
#123039 = CARTESIAN_POINT('Ctrl Pts',(-16.64051349192,12.76729595803,133.408747345421)) ;
#123040 = CARTESIAN_POINT('Ctrl Pts',(-16.6970812746958,13.021989825902,133.540754215802)) ;
#123041 = CARTESIAN_POINT('Ctrl Pts',(-16.7298559652697,13.303543839919,133.603497574117)) ;
#123042 = CARTESIAN_POINT('Ctrl Pts',(-16.7377714864704,13.5948424473805,
133.593472415343)) ;
#123043 = CARTESIAN_POINT('Ctrl Pts',(-16.7206605383398,13.8739531403396,
133.510325245329)) ;
#123044 = CARTESIAN_POINT('Ctrl Pts',(-16.6806111118358,14.1203175585331,
133.360220188526)) ;
#123045 = CARTESIAN_POINT('Ctrl Pts',(-16.6212526466619,14.3167169570115,
133.15372717127)) ;
#123046 = CARTESIAN_POINT('Ctrl Pts',(-16.5474137428711,14.4494067343281,
132.904886251952)) ;
#123047 = CARTESIAN_POINT('Ctrl Pts',(-16.4651040331395,14.5084702765568,
132.631270940826)) ;
#123048 = CARTESIAN_POINT('Ctrl Pts',(-16.381207376955,14.4897007225782,132.353087802305)) ;
#123049 = CARTESIAN_POINT('Ctrl Pts',(-16.3022005550565,14.3946105615284,
132.089157332748)) ;
#123050 = CARTESIAN_POINT('Ctrl Pts',(-16.2344715297939,14.2294634797175,
131.858114788284)) ;
#123051 = CARTESIAN_POINT('Ctrl Pts',(-16.1839485347065,14.0073333338193,
131.677471929649)) ;
#123052 = CARTESIAN_POINT('Ctrl Pts',(-16.1545348340837,13.743582797636,131.558487337903)) ;
#123053 = CARTESIAN_POINT('Ctrl Pts',(-16.1492756367797,13.4548247152231,
131.509829227)) ;
#123054 = CARTESIAN_POINT('Ctrl Pts',(-16.1692158859155,13.1663898310179,
131.53509076053)) ;
#123055 = CARTESIAN_POINT('Ctrl Pts',(-16.2137083792206,12.8948251828515,
131.63190140386)) ;
#123056 = CARTESIAN_POINT('Ctrl Pts',(-16.2803486569312,12.661361440579,131.79342760969)) ;
#123057 = CARTESIAN_POINT('Ctrl Pts',(-16.3648242376105,12.4827884895572,
132.007122021634)) ;
#123058 = CARTESIAN_POINT('Ctrl Pts',(-16.4621290434118,12.3713199015498,
132.258240175335)) ;
#123059 = CARTESIAN_POINT('Ctrl Pts',(-16.5656958305595,12.3351536533699,
132.527714564387)) ;
#123060 = CARTESIAN_POINT('Ctrl Pts',(-16.6694929915143,12.3771106009455,
132.79770710281)) ;
#123061 = CARTESIAN_POINT('Ctrl Pts',(-16.7657977656074,12.4937460494275,
133.04598965838)) ;
#123062 = CARTESIAN_POINT('Ctrl Pts',(-16.8492058389657,12.6767291591256,
133.256549538761)) ;
#123063 = CARTESIAN_POINT('Ctrl Pts',(-16.9145312067199,12.9147363341255,
133.414096808471)) ;
#123064 = CARTESIAN_POINT('Ctrl Pts',(-16.9570460781137,13.1870897744472,
133.505289820544)) ;
#123065 = CARTESIAN_POINT('Ctrl Pts',(-16.9751986910918,13.4771403047647,
133.525201879438)) ;
#123066 = CARTESIAN_POINT('Ctrl Pts',(-16.968053826777,13.7642377896945,133.47111354397)) ;
#123067 = CARTESIAN_POINT('Ctrl Pts',(-16.9368413071542,14.0261140993903,
133.34678648386)) ;
#123068 = CARTESIAN_POINT('Ctrl Pts',(-16.8850225105273,14.2437566933168,
133.16245913461)) ;
#123069 = CARTESIAN_POINT('Ctrl Pts',(-16.8161456299396,14.4043005148666,
132.928011967567)) ;
#123070 = CARTESIAN_POINT('Ctrl Pts',(-16.7367529131212,14.4936452056158,
132.66304467086)) ;
#123071 = CARTESIAN_POINT('Ctrl Pts',(-16.6526808835843,14.5067755080675,
132.384315913876)) ;
#123072 = CARTESIAN_POINT('Ctrl Pts',(-16.5707753130581,14.4421250993153,
132.111889673594)) ;
#123073 = CARTESIAN_POINT('Ctrl Pts',(-16.4976974816868,14.3039890578845,
131.865211800435)) ;
#123074 = CARTESIAN_POINT('Ctrl Pts',(-16.4397839505893,14.1040920585568,
131.663050653327)) ;
#123075 = CARTESIAN_POINT('Ctrl Pts',(-16.4011325865525,13.8535850410252,
131.516876468062)) ;
#123076 = CARTESIAN_POINT('Ctrl Pts',(-16.385954724659,13.573095030684,131.439416068659)) ;
#123077 = CARTESIAN_POINT('Ctrl Pts',(-16.395634910027,13.2829859633842,131.434689671062)) ;
#123078 = CARTESIAN_POINT('Ctrl Pts',(-16.4303004889498,13.0017735288795,
131.502829909788)) ;
#123079 = CARTESIAN_POINT('Ctrl Pts',(-16.4885081607421,12.7500889121872,
131.639639946355)) ;
#123080 = CARTESIAN_POINT('Ctrl Pts',(-16.5663528174175,12.5475576765503,
131.833937570297)) ;
#123081 = CARTESIAN_POINT('Ctrl Pts',(-16.6592929614882,12.4075651763914,
132.072286468684)) ;
#123082 = CARTESIAN_POINT('Ctrl Pts',(-16.7609250951473,12.3405227195362,
132.336146966397)) ;
#123083 = CARTESIAN_POINT('Ctrl Pts',(-16.8654707864991,12.3506976033877,
132.608381377182)) ;
#123084 = CARTESIAN_POINT('Ctrl Pts',(-16.9658202329978,12.4381775614935,
132.868330160183)) ;
#123085 = CARTESIAN_POINT('Ctrl Pts',(-17.0551055310643,12.5958828969702,
133.096070183763)) ;
#123086 = CARTESIAN_POINT('Ctrl Pts',(-17.1279925803926,12.8123888981795,
133.275937593456)) ;
#123087 = CARTESIAN_POINT('Ctrl Pts',(-17.1802441869066,13.0732935402693,
133.395423875302)) ;
#123088 = CARTESIAN_POINT('Ctrl Pts',(-17.2084980990116,13.3601445566741,
133.444717176536)) ;
#123089 = CARTESIAN_POINT('Ctrl Pts',(-17.2115018031446,13.6487325565986,
133.420571161755)) ;
#123090 = CARTESIAN_POINT('Ctrl Pts',(-17.1899377747894,13.9231969676619,
133.324422291905)) ;
#123091 = CARTESIAN_POINT('Ctrl Pts',(-17.1459076362519,14.161664923211,133.162667592942)) ;
#123092 = CARTESIAN_POINT('Ctrl Pts',(-17.0831501699344,14.3474885312589,
132.946120430805)) ;
#123093 = CARTESIAN_POINT('Ctrl Pts',(-17.0074107794741,14.4664584642889,
132.691814732617)) ;
#123094 = CARTESIAN_POINT('Ctrl Pts',(-16.9240118897558,14.5109046596075,
132.414920572147)) ;
#123095 = CARTESIAN_POINT('Ctrl Pts',(-16.8409250151227,14.4775384051983,
132.139258966291)) ;
#123096 = CARTESIAN_POINT('Ctrl Pts',(-16.7633048308355,14.3681997153804,
131.879250841701)) ;
#123097 = CARTESIAN_POINT('Ctrl Pts',(-16.698669890579,14.1916180826176,131.657376441869)) ;
#123098 = CARTESIAN_POINT('Ctrl Pts',(-16.6517651552372,13.9603525000671,
131.487287164895)) ;
#123099 = CARTESIAN_POINT('Ctrl Pts',(-16.6267138914172,13.6895220896488,
131.380907935397)) ;
#123100 = CARTESIAN_POINT('Ctrl Pts',(-16.6262261903022,13.4007319535163,
131.346419955467)) ;
#123101 = CARTESIAN_POINT('Ctrl Pts',(-16.6508307815869,13.1132078069033,
131.385200211347)) ;
#123102 = CARTESIAN_POINT('Ctrl Pts',(-16.7000127575053,12.846606824237,131.495596242918)) ;
#123103 = CARTESIAN_POINT('Ctrl Pts',(-16.7699340004991,12.623698437481,131.6669249854)) ;
#123104 = CARTESIAN_POINT('Ctrl Pts',(-16.8575811531176,12.4561011636242,
131.889737975163)) ;
#123105 = CARTESIAN_POINT('Ctrl Pts',(-16.9565025908863,12.3585967931485,
132.145620482729)) ;
#123106 = CARTESIAN_POINT('Ctrl Pts',(-17.0607608295923,12.3371246783343,
132.417041652335)) ;
#123107 = CARTESIAN_POINT('Ctrl Pts',(-17.1634369259646,12.3935413864574,
132.683861422773)) ;
#123108 = CARTESIAN_POINT('Ctrl Pts',(-17.2579099625892,12.5236724613545,
132.926727411168)) ;
#123109 = CARTESIAN_POINT('Ctrl Pts',(-17.3381899050013,12.7179305396398,
133.128155534346)) ;
#123110 = CARTESIAN_POINT('Ctrl Pts',(-17.3995267077133,12.9643002141067,
133.27404690597)) ;
#123111 = CARTESIAN_POINT('Ctrl Pts',(-17.4374881845313,13.2410163015689,
133.351981082144)) ;
#123112 = CARTESIAN_POINT('Ctrl Pts',(-17.4508755384222,13.5320328266363,
133.357960508206)) ;
#123113 = CARTESIAN_POINT('Ctrl Pts',(-17.4391231761998,13.8151978209727,
133.29051487951)) ;
#123114 = CARTESIAN_POINT('Ctrl Pts',(-17.4037054751815,14.0709652782984,
133.153839129592)) ;
#123115 = CARTESIAN_POINT('Ctrl Pts',(-17.3480561457166,14.2795163173677,
132.958154017432)) ;
#123116 = CARTESIAN_POINT('Ctrl Pts',(-17.2769868362532,14.4266234403896,
132.717472688248)) ;
#123117 = CARTESIAN_POINT('Ctrl Pts',(-17.1961177738273,14.5021445242865,
132.448130239206)) ;
#123118 = CARTESIAN_POINT('Ctrl Pts',(-17.1118876681302,14.5004798974739,
132.16892134338)) ;
#123119 = CARTESIAN_POINT('Ctrl Pts',(-17.0310427991464,14.4210757518903,
131.899528163471)) ;
#123120 = CARTESIAN_POINT('Ctrl Pts',(-16.9607834264823,14.2711636067417,
131.661303307297)) ;
#123121 = CARTESIAN_POINT('Ctrl Pts',(-16.9059182551002,14.0600318658462,
131.467885599582)) ;
#123122 = CARTESIAN_POINT('Ctrl Pts',(-16.8715689169995,13.8025044724255,
131.334333695269)) ;
#123123 = CARTESIAN_POINT('Ctrl Pts',(-16.8609448001921,13.5194348559979,
131.270285840575)) ;
#123124 = CARTESIAN_POINT('Ctrl Pts',(-16.8754425519544,13.2279296915562,
131.279438819765)) ;
#123125 = CARTESIAN_POINT('Ctrl Pts',(-16.9146883120641,12.9514278673655,
131.361017100262)) ;
#123126 = CARTESIAN_POINT('Ctrl Pts',(-16.9769612891766,12.7076269304905,
131.509703903638)) ;
#123127 = CARTESIAN_POINT('Ctrl Pts',(-17.0577658489045,12.5164543303433,
131.712752029851)) ;
#123128 = CARTESIAN_POINT('Ctrl Pts',(-17.1530301116951,12.3891143614251,
131.957830660672)) ;
#123129 = CARTESIAN_POINT('Ctrl Pts',(-17.255826018226,12.3364756135891,132.22503445106)) ;
#123130 = CARTESIAN_POINT('Ctrl Pts',(-17.3598675535299,12.3612642379946,
132.495867624495)) ;
#123131 = CARTESIAN_POINT('Ctrl Pts',(-17.4588984356061,12.4629839046161,
132.751884061504)) ;
#123132 = CARTESIAN_POINT('Ctrl Pts',(-17.5451750061563,12.6321971909499,
132.97096084242)) ;
#123133 = CARTESIAN_POINT('Ctrl Pts',(-17.6146347409835,12.8584558944589,
133.140756526335)) ;
#123134 = CARTESIAN_POINT('Ctrl Pts',(-17.6625907018637,13.126164869302,133.247632658704)) ;
#123135 = CARTESIAN_POINT('Ctrl Pts',(-17.686067276807,13.4141234527586,133.283124808462)) ;
#123136 = CARTESIAN_POINT('Ctrl Pts',(-17.6844047923767,13.7023852281616,
133.24521446728)) ;
#123137 = CARTESIAN_POINT('Ctrl Pts',(-17.6584006494406,13.9714211958417,
133.136118653712)) ;
#123138 = CARTESIAN_POINT('Ctrl Pts',(-17.6102464362103,14.2020200814189,
132.962158529894)) ;
#123139 = CARTESIAN_POINT('Ctrl Pts',(-17.5449058959592,14.3750071777218,
132.73827371451)) ;
#123140 = CARTESIAN_POINT('Ctrl Pts',(-17.4673010855026,14.4806351397631,
132.478490433168)) ;
#123141 = CARTESIAN_POINT('Ctrl Pts',(-17.3835397579498,14.5105855300703,
132.200638006031)) ;
#123142 = CARTESIAN_POINT('Ctrl Pts',(-17.30068437579,14.4625550533332,131.925476858829)) ;
#123143 = CARTESIAN_POINT('Ctrl Pts',(-17.2252675417554,14.3400369090667,
131.67203480792)) ;
#123144 = CARTESIAN_POINT('Ctrl Pts',(-17.1635231504772,14.1521956958397,
131.458588071982)) ;
#123145 = CARTESIAN_POINT('Ctrl Pts',(-17.1203550453216,13.9116488292757,
131.299323606361)) ;
#123146 = CARTESIAN_POINT('Ctrl Pts',(-17.0998333313807,13.6358543135724,
131.206201276277)) ;
#123147 = CARTESIAN_POINT('Ctrl Pts',(-17.1040414218408,13.3459426369887,
131.18545101084)) ;
#123148 = CARTESIAN_POINT('Ctrl Pts',(-17.1334554147273,13.0604648346963,
131.238204781291)) ;
#123149 = CARTESIAN_POINT('Ctrl Pts',(-17.186635109894,12.8015142493302,131.360449631812)) ;
#123150 = CARTESIAN_POINT('Ctrl Pts',(-17.2605647433702,12.5868713096869,
131.543281201559)) ;
#123151 = CARTESIAN_POINT('Ctrl Pts',(-17.3505844000603,12.432303139715,131.773142925006)) ;
#123152 = CARTESIAN_POINT('Ctrl Pts',(-17.450995478009,12.3486039806668,132.033365539858)) ;
#123153 = CARTESIAN_POINT('Ctrl Pts',(-17.5555454936255,12.3418345477554,
132.305622555726)) ;
#123154 = CARTESIAN_POINT('Ctrl Pts',(-17.6572109198033,12.4127258480294,
132.569475130721)) ;
#123155 = CARTESIAN_POINT('Ctrl Pts',(-17.74925550764,12.5554431662894,132.805322541401)) ;
#123156 = CARTESIAN_POINT('Ctrl Pts',(-17.8264454858064,12.7608030962308,
132.99765025968)) ;
#123157 = CARTESIAN_POINT('Ctrl Pts',(-17.8835674879356,13.0143081230203,
133.131299482817)) ;
#123158 = CARTESIAN_POINT('Ctrl Pts',(-17.9170703055575,13.29536631424,133.196160960181)) ;
#123159 = CARTESIAN_POINT('Ctrl Pts',(-17.9256862762086,13.5874993963847,
133.18809411502)) ;
#123160 = CARTESIAN_POINT('Ctrl Pts',(-17.9091691179215,13.8669340437894,
133.106704940277)) ;
#123161 = CARTESIAN_POINT('Ctrl Pts',(-17.8699206134807,14.1134264974216,
132.959083300844)) ;
#123162 = CARTESIAN_POINT('Ctrl Pts',(-17.8109235413731,14.312178191849,132.753550467114)) ;
#123163 = CARTESIAN_POINT('Ctrl Pts',(-17.7371490293014,14.447005080599,132.504799591305)) ;
#123164 = CARTESIAN_POINT('Ctrl Pts',(-17.6551253369284,14.50780864275,132.23208223908)) ;
#123165 = CARTESIAN_POINT('Ctrl Pts',(-17.5714598174354,14.4913412466958,
131.954681845237)) ;
#123166 = CARTESIAN_POINT('Ctrl Pts',(-17.4922372650921,14.3985298499944,
131.690131300663)) ;
#123167 = CARTESIAN_POINT('Ctrl Pts',(-17.4240290431123,14.23537642446,131.457680674098)) ;
#123168 = CARTESIAN_POINT('Ctrl Pts',(-17.372717665545,14.0132823702427,131.27454472913)) ;
#123169 = CARTESIAN_POINT('Ctrl Pts',(-17.3429068898243,13.7517705184138,
131.154578961015)) ;
#123170 = CARTESIAN_POINT('Ctrl Pts',(-17.3368035221446,13.4639004109061,
131.103505978631)) ;
#123171 = CARTESIAN_POINT('Ctrl Pts',(-17.3561906073303,13.1736259239267,
131.126963588793)) ;
#123172 = CARTESIAN_POINT('Ctrl Pts',(-17.399754261981,12.9029494163379,131.221266592512)) ;
#123173 = CARTESIAN_POINT('Ctrl Pts',(-17.4659861489072,12.6670694779248,
131.381471376982)) ;
#123174 = CARTESIAN_POINT('Ctrl Pts',(-17.5502293174444,12.4867414541686,
131.594432437116)) ;
#123175 = CARTESIAN_POINT('Ctrl Pts',(-17.6467937329341,12.3736046966953,
131.843541552857)) ;
#123176 = CARTESIAN_POINT('Ctrl Pts',(-17.7508568587286,12.3351061358333,
132.114275541439)) ;
#123177 = CARTESIAN_POINT('Ctrl Pts',(-17.8540445547543,12.3747297398712,
132.382714038541)) ;
#123178 = CARTESIAN_POINT('Ctrl Pts',(-17.9508908372742,12.4890530278271,
132.632514940323)) ;
#123179 = CARTESIAN_POINT('Ctrl Pts',(-18.0352482217783,12.671847392328,132.845621204235)) ;
#123180 = CARTESIAN_POINT('Ctrl Pts',(-18.1006691599388,12.9071471276995,
133.003666438983)) ;
#123181 = CARTESIAN_POINT('Ctrl Pts',(-18.1439831889663,13.1791584028572,
133.097130182838)) ;
#123182 = CARTESIAN_POINT('Ctrl Pts',(-18.1627954327558,13.4685703859445,
133.119024093136)) ;
#123183 = CARTESIAN_POINT('Ctrl Pts',(-18.1564134876139,13.7556866314948,
133.067206763249)) ;
#123184 = CARTESIAN_POINT('Ctrl Pts',(-18.12597352168,14.0184521546514,132.945168227283)) ;
#123185 = CARTESIAN_POINT('Ctrl Pts',(-18.0744435558841,14.2386836272176,
132.761515544376)) ;
#123186 = CARTESIAN_POINT('Ctrl Pts',(-18.005953850359,14.4009245820624,132.528213465536)) ;
#123187 = CARTESIAN_POINT('Ctrl Pts',(-17.9265298697312,14.4923209355322,
132.263056140391)) ;
#123188 = CARTESIAN_POINT('Ctrl Pts',(-17.8429057727029,14.5074993707076,
131.985805363542)) ;
#123189 = CARTESIAN_POINT('Ctrl Pts',(-17.7605057976756,14.4446390736038,
131.711788345313)) ;
#123190 = CARTESIAN_POINT('Ctrl Pts',(-17.6874814954345,14.3090137807522,
131.465438769024)) ;
#123191 = CARTESIAN_POINT('Ctrl Pts',(-17.6289271492235,14.1104147854154,
131.261333528496)) ;
#123192 = CARTESIAN_POINT('Ctrl Pts',(-17.5897575642381,13.8614586698981,
131.113706749861)) ;
#123193 = CARTESIAN_POINT('Ctrl Pts',(-17.5738212671254,13.5819684927305,
131.034067733009)) ;
#123194 = CARTESIAN_POINT('Ctrl Pts',(-17.5828139968281,13.2906276884224,
131.027193171422)) ;
#123195 = CARTESIAN_POINT('Ctrl Pts',(-17.616848627643,13.0092431055299,131.093525306334)) ;
#123196 = CARTESIAN_POINT('Ctrl Pts',(-17.6740860340513,12.7575166399562,
131.227660746191)) ;
#123197 = CARTESIAN_POINT('Ctrl Pts',(-17.7516753463476,12.5525238857448,
131.421087178671)) ;
#123198 = CARTESIAN_POINT('Ctrl Pts',(-17.8440081329895,12.4108769573351,
131.657753073151)) ;
#123199 = CARTESIAN_POINT('Ctrl Pts',(-17.9458175434282,12.3412908932615,
131.922013087473)) ;
#123200 = CARTESIAN_POINT('Ctrl Pts',(-18.0502423166348,12.3493862056845,
132.193940570029)) ;
#123201 = CARTESIAN_POINT('Ctrl Pts',(-18.1505364662407,12.434272868394,132.453821578147)) ;
#123202 = CARTESIAN_POINT('Ctrl Pts',(-18.240385583011,12.5900490117304,132.683164341833)) ;
#123203 = CARTESIAN_POINT('Ctrl Pts',(-18.3140154660262,12.8056267290578,
132.865114759058)) ;
#123204 = CARTESIAN_POINT('Ctrl Pts',(-18.366813447899,13.065385008078,132.986222365065)) ;
#123205 = CARTESIAN_POINT('Ctrl Pts',(-18.3957716324573,13.3504852311182,
133.03771979281)) ;
#123206 = CARTESIAN_POINT('Ctrl Pts',(-18.3995519707308,13.6412799194347,
133.015607297531)) ;
#123207 = CARTESIAN_POINT('Ctrl Pts',(-18.3786631552861,13.9155482376954,
132.921539059482)) ;
#123208 = CARTESIAN_POINT('Ctrl Pts',(-18.3352864113963,14.1552942576475,
132.761699945438)) ;
#123209 = CARTESIAN_POINT('Ctrl Pts',(-18.2730232374163,14.3429102218091,
132.546604772936)) ;
#123210 = CARTESIAN_POINT('Ctrl Pts',(-18.1974878680021,14.4639893151741,
132.292852310958)) ;
#123211 = CARTESIAN_POINT('Ctrl Pts',(-18.1145512503383,14.5107279947802,
132.017447527145)) ;
#123212 = CARTESIAN_POINT('Ctrl Pts',(-18.0309330183496,14.4794893711203,
131.74005057923)) ;
#123213 = CARTESIAN_POINT('Ctrl Pts',(-17.9533998997489,14.3727211556821,
131.480454525081)) ;
#123214 = CARTESIAN_POINT('Ctrl Pts',(-17.8881494032496,14.1977799605459,
131.256709819831)) ;
#123215 = CARTESIAN_POINT('Ctrl Pts',(-17.84064942172,13.9680803092071,131.08490378882)) ;
#123216 = CARTESIAN_POINT('Ctrl Pts',(-17.8148397147958,13.6967826979273,
130.976149136345)) ;
#123217 = CARTESIAN_POINT('Ctrl Pts',(-17.8136790517629,13.4094043760134,
130.939833355752)) ;
#123218 = CARTESIAN_POINT('Ctrl Pts',(-17.8375788446251,13.1212039235338,
130.976511139861)) ;
#123219 = CARTESIAN_POINT('Ctrl Pts',(-17.8858674033282,12.8546896055266,
131.084429899433)) ;
#123220 = CARTESIAN_POINT('Ctrl Pts',(-17.955361853148,12.6293810119528,131.254404916973)) ;
#123221 = CARTESIAN_POINT('Ctrl Pts',(-18.0430537668622,12.4594635136683,
131.477196723744)) ;
#123222 = CARTESIAN_POINT('Ctrl Pts',(-18.1412332588082,12.3604529147884,
131.731084274018)) ;
#123223 = CARTESIAN_POINT('Ctrl Pts',(-18.2457684052727,12.3366695110087,
132.003204681306)) ;
#123224 = CARTESIAN_POINT('Ctrl Pts',(-18.3481468441055,12.3907630911244,
132.269294142436)) ;
#123225 = CARTESIAN_POINT('Ctrl Pts',(-18.4431476781956,12.5187718172597,
132.513649957328)) ;
#123226 = CARTESIAN_POINT('Ctrl Pts',(-18.5241808191143,12.7125554078675,
132.717126113492)) ;
#123227 = CARTESIAN_POINT('Ctrl Pts',(-18.5855196122855,12.9551209833767,
132.863367722393)) ;
#123228 = CARTESIAN_POINT('Ctrl Pts',(-18.6245679674523,13.2325621685243,
132.944286617486)) ;
#123229 = CARTESIAN_POINT('Ctrl Pts',(-18.6386186599524,13.5243421587289,
132.952113131439)) ;
#123230 = CARTESIAN_POINT('Ctrl Pts',(-18.6275981947546,13.8069928303566,
132.886922542916)) ;
#123231 = CARTESIAN_POINT('Ctrl Pts',(-18.5928710094331,14.0639001821586,
132.752263942652)) ;
#123232 = CARTESIAN_POINT('Ctrl Pts',(-18.5377610477976,14.274156022816,132.558149542648)) ;
#123233 = CARTESIAN_POINT('Ctrl Pts',(-18.4669022465602,14.4234616465823,
132.318009347732)) ;
#123234 = CARTESIAN_POINT('Ctrl Pts',(-18.3863158160937,14.5011170980349,
132.049535240517)) ;
#123235 = CARTESIAN_POINT('Ctrl Pts',(-18.3017727099702,14.501361448933,131.769280894779)) ;
#123236 = CARTESIAN_POINT('Ctrl Pts',(-18.2214649543661,14.4249955787507,
131.501768767885)) ;
#123237 = CARTESIAN_POINT('Ctrl Pts',(-18.1501883393521,14.2760170248169,
131.260290403675)) ;
#123238 = CARTESIAN_POINT('Ctrl Pts',(-18.0950241994089,14.0665440737742,
131.066070425009)) ;
#123239 = CARTESIAN_POINT('Ctrl Pts',(-18.0600356895942,13.8110526556412,
130.930755576535)) ;
#123240 = CARTESIAN_POINT('Ctrl Pts',(-18.0487031148571,13.5262784611541,
130.864382352007)) ;
#123241 = CARTESIAN_POINT('Ctrl Pts',(-18.062412239786,13.2368368163846,130.871485132988)) ;
#123242 = CARTESIAN_POINT('Ctrl Pts',(-18.1011540315473,12.9583254451164,
130.951421021167)) ;
#123243 = CARTESIAN_POINT('Ctrl Pts',(-18.162442619362,12.7145798984787,131.097428040088)) ;
#123244 = CARTESIAN_POINT('Ctrl Pts',(-18.2435317670333,12.5201729680917,
131.301002269112)) ;
#123245 = CARTESIAN_POINT('Ctrl Pts',(-18.3374905555791,12.3922976801848,
131.542627125827)) ;
#123246 = CARTESIAN_POINT('Ctrl Pts',(-18.4407097729528,12.3368042006491,
131.810872082474)) ;
#123247 = CARTESIAN_POINT('Ctrl Pts',(-18.5444741358057,12.3594079761625,
132.081007895545)) ;
#123248 = CARTESIAN_POINT('Ctrl Pts',(-18.6438726401263,12.458842653819,132.338064760412)) ;
#123249 = CARTESIAN_POINT('Ctrl Pts',(-18.730666683213,12.6263833262832,132.5586223689)) ;
#123250 = CARTESIAN_POINT('Ctrl Pts',(-18.8006930563816,12.8513078347283,
132.730062824088)) ;
#123251 = CARTESIAN_POINT('Ctrl Pts',(-18.8492688728646,13.1175342113745,
132.838816465767)) ;
#123252 = CARTESIAN_POINT('Ctrl Pts',(-18.8735376930888,13.4059955031651,
132.876522375954)) ;
#123253 = CARTESIAN_POINT('Ctrl Pts',(-18.8726310881695,13.6942419631863,
132.840864257295)) ;
#123254 = CARTESIAN_POINT('Ctrl Pts',(-18.846988455619,13.9656571301542,132.732603873144)) ;
#123255 = CARTESIAN_POINT('Ctrl Pts',(-18.800060785329,14.1945698171883,132.562678543483)) ;
#123256 = CARTESIAN_POINT('Ctrl Pts',(-18.7347749337685,14.3711224521538,
132.338694883308)) ;
#123257 = CARTESIAN_POINT('Ctrl Pts',(-18.657438019017,14.4785950112144,132.079716383706)) ;
#123258 = CARTESIAN_POINT('Ctrl Pts',(-18.5736714267936,14.5108133119048,
131.801809937082)) ;
#123259 = CARTESIAN_POINT('Ctrl Pts',(-18.4908489270132,14.465039412922,131.52680696157)) ;
#123260 = CARTESIAN_POINT('Ctrl Pts',(-18.4151408888549,14.3446919180205,
131.272521239877)) ;
#123261 = CARTESIAN_POINT('Ctrl Pts',(-18.3528650039776,14.1586507475217,
131.057514981106)) ;
#123262 = CARTESIAN_POINT('Ctrl Pts',(-18.3089775079518,13.9182141888542,
130.896003116198)) ;
#123263 = CARTESIAN_POINT('Ctrl Pts',(-18.287897911152,13.6446893381856,130.801441722976)) ;
#123264 = CARTESIAN_POINT('Ctrl Pts',(-18.29136911731,13.3538162430507,130.778406138012)) ;
#123265 = CARTESIAN_POINT('Ctrl Pts',(-18.320015418867,13.0687528103835,130.829019791888)) ;
#123266 = CARTESIAN_POINT('Ctrl Pts',(-18.3725780715655,12.808402450481,130.949417001428)) ;
#123267 = CARTESIAN_POINT('Ctrl Pts',(-18.4459344258757,12.5923661463697,
131.130592731019)) ;
#123268 = CARTESIAN_POINT('Ctrl Pts',(-18.5356977693632,12.4355966192842,
131.359653802566)) ;
#123269 = CARTESIAN_POINT('Ctrl Pts',(-18.6360919268662,12.3498833858894,
131.619771018926)) ;
#123270 = CARTESIAN_POINT('Ctrl Pts',(-18.7400873983312,12.3409543002999,
131.890577260411)) ;
#123271 = CARTESIAN_POINT('Ctrl Pts',(-18.8420016780614,12.4093757985287,
132.155139312292)) ;
#123272 = CARTESIAN_POINT('Ctrl Pts',(-18.9346544889553,12.5505197572112,
132.392675801306)) ;
#123273 = CARTESIAN_POINT('Ctrl Pts',(-19.0122360971197,12.7541804700571,
132.586179998705)) ;
#123274 = CARTESIAN_POINT('Ctrl Pts',(-19.0698650565518,13.0055269427028,
132.721428807461)) ;
#123275 = CARTESIAN_POINT('Ctrl Pts',(-19.1042443289156,13.2870727031463,
132.788720725117)) ;
#123276 = CARTESIAN_POINT('Ctrl Pts',(-19.1135598388478,13.5781356431356,
132.782823251789)) ;
#123277 = CARTESIAN_POINT('Ctrl Pts',(-19.0978920623825,13.8583664416102,
132.70391043962)) ;
#123278 = CARTESIAN_POINT('Ctrl Pts',(-19.0590725975324,14.1072756620479,
132.557379585171)) ;
#123279 = CARTESIAN_POINT('Ctrl Pts',(-19.0006930075818,14.3069767003197,
132.35374086841)) ;
#123280 = CARTESIAN_POINT('Ctrl Pts',(-18.9276024226959,14.4436141295833,
132.107115025737)) ;
#123281 = CARTESIAN_POINT('Ctrl Pts',(-18.845475368495,14.5071928211091,131.833981429736)) ;
#123282 = CARTESIAN_POINT('Ctrl Pts',(-18.7615750440561,14.4928944928021,
131.555820733646)) ;
#123283 = CARTESIAN_POINT('Ctrl Pts',(-18.6821529870225,14.4021254320443,
131.290693534934)) ;
#123284 = CARTESIAN_POINT('Ctrl Pts',(-18.6137276419482,14.2413769659717,
131.057704478338)) ;
#123285 = CARTESIAN_POINT('Ctrl Pts',(-18.5617948270631,14.0210257728375,
130.872760524719)) ;
#123286 = CARTESIAN_POINT('Ctrl Pts',(-18.5311748689287,13.7594507578406,
130.75030009395)) ;
#123287 = CARTESIAN_POINT('Ctrl Pts',(-18.524462743248,13.4716752359127,130.697418025673)) ;
#123288 = CARTESIAN_POINT('Ctrl Pts',(-18.5429559165933,13.1827800209618,
130.718450895566)) ;
#123289 = CARTESIAN_POINT('Ctrl Pts',(-18.5860682542042,12.9097866027274,
130.811247666085)) ;
#123290 = CARTESIAN_POINT('Ctrl Pts',(-18.6513547850338,12.6739760958484,
130.968882762111)) ;
#123291 = CARTESIAN_POINT('Ctrl Pts',(-18.7352113453907,12.4911376309814,
131.180647458982)) ;
#123292 = CARTESIAN_POINT('Ctrl Pts',(-18.8320450972457,12.375575879239,131.430367588562)) ;
#123293 = CARTESIAN_POINT('Ctrl Pts',(-18.9353885585262,12.3352662333604,
131.699197648249)) ;
#123294 = CARTESIAN_POINT('Ctrl Pts',(-19.0388002165836,12.3722006124299,
131.968259729985)) ;
#123295 = CARTESIAN_POINT('Ctrl Pts',(-19.13663271086,12.4858118700224,132.220677550879)) ;
#123296 = CARTESIAN_POINT('Ctrl Pts',(-19.2204826471649,12.6649628036957,
132.432670825365)) ;
#123297 = CARTESIAN_POINT('Ctrl Pts',(-19.2868586701222,12.8995424395387,
132.593375480178)) ;
#123298 = CARTESIAN_POINT('Ctrl Pts',(-19.3308236821031,13.1707490219764,
132.688750556029)) ;
#123299 = CARTESIAN_POINT('Ctrl Pts',(-19.3504090557961,13.4602465795,132.7128657881)) ;
#123300 = CARTESIAN_POINT('Ctrl Pts',(-19.3447038706074,13.7479094630808,
132.663005441202)) ;
#123301 = CARTESIAN_POINT('Ctrl Pts',(-19.3149883980574,14.0110934234083,
132.543151049153)) ;
#123302 = CARTESIAN_POINT('Ctrl Pts',(-19.2640132574358,14.233019589697,132.361099714617)) ;
#123303 = CARTESIAN_POINT('Ctrl Pts',(-19.1959166618581,14.3970564643661,
132.128942413442)) ;
#123304 = CARTESIAN_POINT('Ctrl Pts',(-19.1169952616353,14.4906411189315,
131.865358043899)) ;
#123305 = CARTESIAN_POINT('Ctrl Pts',(-19.0328798147139,14.5080280038905,
131.586455112218)) ;
#123306 = CARTESIAN_POINT('Ctrl Pts',(-18.9510735202354,14.4480724922228,
131.314485578695)) ;
#123307 = CARTESIAN_POINT('Ctrl Pts',(-18.8771616284183,14.3139469642534,
131.065316852607)) ;
#123308 = CARTESIAN_POINT('Ctrl Pts',(-18.8181485060677,14.1169436134283,
130.859887328916)) ;
#123309 = CARTESIAN_POINT('Ctrl Pts',(-18.7782906077968,13.8684680278967,
130.710158901743)) ;
#123310 = CARTESIAN_POINT('Ctrl Pts',(-18.7617532070724,13.5907241662415,
130.628902383612)) ;
#123311 = CARTESIAN_POINT('Ctrl Pts',(-18.7699529682382,13.2994060447749,
130.619705093688)) ;
#123312 = CARTESIAN_POINT('Ctrl Pts',(-18.8032396782026,13.0173300828137,
130.683845657523)) ;
#123313 = CARTESIAN_POINT('Ctrl Pts',(-18.8601088458043,12.7634585275692,
130.816765455538)) ;
#123314 = CARTESIAN_POINT('Ctrl Pts',(-18.9371406149224,12.5574052301983,
131.008613631546)) ;
#123315 = CARTESIAN_POINT('Ctrl Pts',(-19.0288519820687,12.4141337315889,
131.243554207896)) ;
#123316 = CARTESIAN_POINT('Ctrl Pts',(-19.13057401488,12.3422331852162,131.507526439382)) ;
#123317 = CARTESIAN_POINT('Ctrl Pts',(-19.2349019043779,12.3479816705834,
131.779210106818)) ;
#123318 = CARTESIAN_POINT('Ctrl Pts',(-19.3355608700303,12.4308509408022,
132.04010176436)) ;
#123319 = CARTESIAN_POINT('Ctrl Pts',(-19.4255699007721,12.5841343909331,
132.27001036361)) ;
#123320 = CARTESIAN_POINT('Ctrl Pts',(-19.5000791880127,12.7991565720161,
132.454374408853)) ;
#123321 = CARTESIAN_POINT('Ctrl Pts',(-19.5533212332608,13.0570001115815,
132.576901554063)) ;
#123322 = CARTESIAN_POINT('Ctrl Pts',(-19.5830699103574,13.3421922466227,
132.63063668358)) ;
#123323 = CARTESIAN_POINT('Ctrl Pts',(-19.5876133607077,13.6321455836602,
132.610870942847)) ;
#123324 = CARTESIAN_POINT('Ctrl Pts',(-19.5673218035565,13.9089726379876,
132.518333296573)) ;
#123325 = CARTESIAN_POINT('Ctrl Pts',(-19.5243599298239,14.1498189010042,
132.359684334784)) ;
#123326 = CARTESIAN_POINT('Ctrl Pts',(-19.4629860879287,14.3379335627546,
132.147406052705)) ;
#123327 = CARTESIAN_POINT('Ctrl Pts',(-19.3875690527456,14.4615825928275,
131.893901802472)) ;
#123328 = CARTESIAN_POINT('Ctrl Pts',(-19.3048022308788,14.5104718340286,
131.619017490043)) ;
#123329 = CARTESIAN_POINT('Ctrl Pts',(-19.2208867293053,14.4813917007992,
131.340664971881)) ;
#123330 = CARTESIAN_POINT('Ctrl Pts',(-19.1431505631515,14.376410140061,131.080480626318)) ;
#123331 = CARTESIAN_POINT('Ctrl Pts',(-19.0776968905506,14.2041612959408,
130.856285283201)) ;
#123332 = CARTESIAN_POINT('Ctrl Pts',(-19.0293984514368,13.974383981629,130.68194601526)) ;
#123333 = CARTESIAN_POINT('Ctrl Pts',(-19.0031038029563,13.7063210465707,
130.572069348957)) ;
#123334 = CARTESIAN_POINT('Ctrl Pts',(-19.001145721614,13.4167011729611,130.533125822564)) ;
#123335 = CARTESIAN_POINT('Ctrl Pts',(-19.0243797093888,13.1291677764475,
130.5679716419)) ;
#123336 = CARTESIAN_POINT('Ctrl Pts',(-19.0719631831347,12.8617102719658,
130.673828410007)) ;
#123337 = CARTESIAN_POINT('Ctrl Pts',(-19.1409679175638,12.6350478347594,
130.842360735363)) ;
#123338 = CARTESIAN_POINT('Ctrl Pts',(-19.2278027464721,12.4638699496821,
131.062798616732)) ;
#123339 = CARTESIAN_POINT('Ctrl Pts',(-19.3262245567786,12.3621126749229,
131.317221532993)) ;
#123340 = CARTESIAN_POINT('Ctrl Pts',(-19.430537761891,12.336288295009,131.58874825821)) ;
#123341 = CARTESIAN_POINT('Ctrl Pts',(-19.5332636656819,12.3882079371413,
131.855786779012)) ;
#123342 = CARTESIAN_POINT('Ctrl Pts',(-19.6286546086938,12.5148240574062,
132.101228597858)) ;
#123343 = CARTESIAN_POINT('Ctrl Pts',(-19.7095188083265,12.7050813508199,
132.304501505355)) ;
#123344 = CARTESIAN_POINT('Ctrl Pts',(-19.7720060707541,12.9482678416441,
132.453826841834)) ;
#123345 = CARTESIAN_POINT('Ctrl Pts',(-19.8115111558353,13.2238579668187,
132.536233557694)) ;
#123346 = CARTESIAN_POINT('Ctrl Pts',(-19.8263700093836,13.5162934097049,
132.546326795299)) ;
#123347 = CARTESIAN_POINT('Ctrl Pts',(-19.8160540554796,13.7991654054394,
132.483232272363)) ;
#123348 = CARTESIAN_POINT('Ctrl Pts',(-19.7817797053596,14.0580269319691,
132.349765095749)) ;
#123349 = CARTESIAN_POINT('Ctrl Pts',(-19.7274211509896,14.2686029381806,
132.158015292144)) ;
#123350 = CARTESIAN_POINT('Ctrl Pts',(-19.6570350610866,14.419961933364,131.919277312271)) ;
#123351 = CARTESIAN_POINT('Ctrl Pts',(-19.5765562400787,14.49989585267,131.651079261874)) ;
#123352 = CARTESIAN_POINT('Ctrl Pts',(-19.4921101780105,14.5025664525356,
131.371149134813)) ;
#123353 = CARTESIAN_POINT('Ctrl Pts',(-19.4113969608343,14.4280651994865,
131.102354695495)) ;
#123354 = CARTESIAN_POINT('Ctrl Pts',(-19.3400486586853,14.2819176182956,
130.860829298988)) ;
#123355 = CARTESIAN_POINT('Ctrl Pts',(-19.2839264131876,14.0723875526179,
130.663547795459)) ;
#123356 = CARTESIAN_POINT('Ctrl Pts',(-19.2485926616992,13.8191593341655,
130.527403742645)) ;
#123357 = CARTESIAN_POINT('Ctrl Pts',(-19.2364478765941,13.5356700868247,
130.458732004174)) ;
#123358 = CARTESIAN_POINT('Ctrl Pts',(-19.2494300922433,13.2451624741664,
130.463600209638)) ;
#123359 = CARTESIAN_POINT('Ctrl Pts',(-19.2874907120602,12.9658957798679,
130.541539493339)) ;
#123360 = CARTESIAN_POINT('Ctrl Pts',(-19.3482532948302,12.7208678253265,
130.685983671784)) ;
#123361 = CARTESIAN_POINT('Ctrl Pts',(-19.4283743567801,12.5256177762791,
130.886907898066)) ;
#123362 = CARTESIAN_POINT('Ctrl Pts',(-19.5225746037128,12.3947248965929,
131.129026992541)) ;
#123363 = CARTESIAN_POINT('Ctrl Pts',(-19.6256543536979,12.3373274071284,
131.396874484283)) ;
#123364 = CARTESIAN_POINT('Ctrl Pts',(-19.7292828586896,12.3577351595859,
131.666668741082)) ;
#123365 = CARTESIAN_POINT('Ctrl Pts',(-19.828747484538,12.4546492902735,131.923987738611)) ;
#123366 = CARTESIAN_POINT('Ctrl Pts',(-19.9163629094891,12.6210677035252,
132.146795892703)) ;
#123367 = CARTESIAN_POINT('Ctrl Pts',(-19.9868245592564,12.8446767267699,
132.319524452122)) ;
#123368 = CARTESIAN_POINT('Ctrl Pts',(-20.0358951637964,13.1088081967542,
132.429861713404)) ;
#123369 = CARTESIAN_POINT('Ctrl Pts',(-20.0610202092485,13.3979062800969,
132.469955286352)) ;
#123370 = CARTESIAN_POINT('Ctrl Pts',(-20.0607325832847,13.6859097693729,
132.436152367253)) ;
#123371 = CARTESIAN_POINT('Ctrl Pts',(-20.0361182928156,13.9567565274245,
132.331106427657)) ;
#123372 = CARTESIAN_POINT('Ctrl Pts',(-19.989134080272,14.1899349081331,132.160581855048)) ;
#123373 = CARTESIAN_POINT('Ctrl Pts',(-19.9249163191982,14.3662692594446,
131.940072508991)) ;
#123374 = CARTESIAN_POINT('Ctrl Pts',(-19.8473720747076,14.4768289977238,
131.680256103619)) ;
#123375 = CARTESIAN_POINT('Ctrl Pts',(-19.7638911381145,14.5109207097569,
131.403278553501)) ;
#123376 = CARTESIAN_POINT('Ctrl Pts',(-19.6808599303053,14.4673589922836,
131.127620946744)) ;
#123377 = CARTESIAN_POINT('Ctrl Pts',(-19.6048776341735,14.3490297985362,
130.87254760327)) ;
#123378 = CARTESIAN_POINT('Ctrl Pts',(-19.5421323663737,14.1643442277036,
130.65613213943)) ;
#123379 = CARTESIAN_POINT('Ctrl Pts',(-19.4978928252363,13.9269540267458,
130.493822267582)) ;
#123380 = CARTESIAN_POINT('Ctrl Pts',(-19.4759282474524,13.6529086343547,
130.396504933955)) ;
#123381 = CARTESIAN_POINT('Ctrl Pts',(-19.4786884736238,13.3625039506586,
130.371432632605)) ;
#123382 = CARTESIAN_POINT('Ctrl Pts',(-19.5066515881235,13.0764916582392,
130.419989164608)) ;
#123383 = CARTESIAN_POINT('Ctrl Pts',(-19.5585742647346,12.8152456791565,
130.538527912325)) ;
#123384 = CARTESIAN_POINT('Ctrl Pts',(-19.6313995735152,12.5977359905825,
130.718150203984)) ;
#123385 = CARTESIAN_POINT('Ctrl Pts',(-19.7206731960293,12.439230107941,130.945816992587)) ;
#123386 = CARTESIAN_POINT('Ctrl Pts',(-19.8208275253365,12.3513755687183,
131.205236892769)) ;
#123387 = CARTESIAN_POINT('Ctrl Pts',(-19.9247572807901,12.339931649505,131.475869177705)) ;
#123388 = CARTESIAN_POINT('Ctrl Pts',(-20.0275777885888,12.4070555048895,
131.742824520254)) ;
#123389 = CARTESIAN_POINT('Ctrl Pts',(-20.1196954087276,12.5451371061637,
131.979106081002)) ;
#123390 = CARTESIAN_POINT('Ctrl Pts',(-20.1981516956985,12.7477728516222,
132.175029811803)) ;
#123391 = CARTESIAN_POINT('Ctrl Pts',(-20.256324633919,12.9979369346779,132.311891349811)) ;
#123392 = CARTESIAN_POINT('Ctrl Pts',(-20.2914356628922,13.2792373127526,
132.38127965356)) ;
#123393 = CARTESIAN_POINT('Ctrl Pts',(-20.3014130100161,13.570158269964,132.377333641783)) ;
#123394 = CARTESIAN_POINT('Ctrl Pts',(-20.286471936004,13.850537969179,132.300597227172)) ;
#123395 = CARTESIAN_POINT('Ctrl Pts',(-20.2482660446986,14.1007514006134,
132.155840929195)) ;
#123396 = CARTESIAN_POINT('Ctrl Pts',(-20.1903697230178,14.302171677131,131.953602989605)) ;
#123397 = CARTESIAN_POINT('Ctrl Pts',(-20.1173842617992,14.4410638896651,
131.707187218307)) ;
#123398 = CARTESIAN_POINT('Ctrl Pts',(-20.0354743272129,14.5064205925433,
131.434719899531)) ;
#123399 = CARTESIAN_POINT('Ctrl Pts',(-19.9518021159349,14.4944296430568,
131.157328547181)) ;
#123400 = CARTESIAN_POINT('Ctrl Pts',(-19.871969321922,14.405561123776,130.89092166106)) ;
#123401 = CARTESIAN_POINT('Ctrl Pts',(-19.8033463280559,14.2469874685197,
130.657440519266)) ;
#123402 = CARTESIAN_POINT('Ctrl Pts',(-19.7508500620726,14.0284941679127,
130.470881149737)) ;
#123403 = CARTESIAN_POINT('Ctrl Pts',(-19.719490022158,13.7670073728255,130.346148553405)) ;
#123404 = CARTESIAN_POINT('Ctrl Pts',(-19.7121011487977,13.480578033378,130.291399553805)) ;
#123405 = CARTESIAN_POINT('Ctrl Pts',(-19.7298039128491,13.1913387346796,
130.310107119157)) ;
#123406 = CARTESIAN_POINT('Ctrl Pts',(-19.7722865639601,12.9172330452571,
130.401022931997)) ;
#123407 = CARTESIAN_POINT('Ctrl Pts',(-19.8369732676592,12.6799728424888,
130.556899776584)) ;
#123408 = CARTESIAN_POINT('Ctrl Pts',(-19.920757365482,12.4949910313751,130.768323701621)) ;
#123409 = CARTESIAN_POINT('Ctrl Pts',(-20.0165266255756,12.3781840419528,
131.015200166848)) ;
#123410 = CARTESIAN_POINT('Ctrl Pts',(-20.1206017423873,12.3352411031327,
131.28589296705)) ;
#123411 = CARTESIAN_POINT('Ctrl Pts',(-20.2236087179121,12.3701183951614,
131.553933115692)) ;
#123412 = CARTESIAN_POINT('Ctrl Pts',(-20.3217871748641,12.4815908336551,
131.807337046377)) ;
#123413 = CARTESIAN_POINT('Ctrl Pts',(-20.4059913540354,12.6586744423265,
132.020414433851)) ;
#123414 = CARTESIAN_POINT('Ctrl Pts',(-20.4731244336742,12.8927064520039,
132.183222264498)) ;
#123415 = CARTESIAN_POINT('Ctrl Pts',(-20.5175674054042,13.161589606751,132.280177787723)) ;
#123416 = CARTESIAN_POINT('Ctrl Pts',(-20.5380308810597,13.452733819126,132.306636877863)) ;
#123417 = CARTESIAN_POINT('Ctrl Pts',(-20.5329915826682,13.7397606616034,
132.258839580122)) ;
#123418 = CARTESIAN_POINT('Ctrl Pts',(-20.5038780440695,14.0044957325971,
132.140665648964)) ;
#123419 = CARTESIAN_POINT('Ctrl Pts',(-20.4535510699206,14.2270717509881,
131.960602734661)) ;
#123420 = CARTESIAN_POINT('Ctrl Pts',(-20.3861724322445,14.3928428929851,
131.730652816318)) ;
#123421 = CARTESIAN_POINT('Ctrl Pts',(-20.3068708809211,14.4891680120794,
131.465698279101)) ;
#123422 = CARTESIAN_POINT('Ctrl Pts',(-20.2234454311449,14.5086708871169,
131.18907353064)) ;
#123423 = CARTESIAN_POINT('Ctrl Pts',(-20.1409292956804,14.4507090768999,
130.914800248059)) ;
#123424 = CARTESIAN_POINT('Ctrl Pts',(-20.0669532543017,14.3188233795464,
130.665558965042)) ;
#123425 = CARTESIAN_POINT('Ctrl Pts',(-20.0074043450587,14.1234066158898,
130.458538617797)) ;
#123426 = CARTESIAN_POINT('Ctrl Pts',(-19.9670504311719,13.8772494948289,
130.307501661299)) ;
#123427 = CARTESIAN_POINT('Ctrl Pts',(-19.9496300589494,13.5994496671663,
130.223567904008)) ;
#123428 = CARTESIAN_POINT('Ctrl Pts',(-19.9572207572621,13.306728753329,130.212428024428)) ;
#123429 = CARTESIAN_POINT('Ctrl Pts',(-19.9897127587384,13.0255130150403,
130.274404793934)) ;
#123430 = CARTESIAN_POINT('Ctrl Pts',(-20.0457523916351,12.7708775179562,
130.404962496167)) ;
#123431 = CARTESIAN_POINT('Ctrl Pts',(-20.122302311935,12.5628411654916,130.595365453384)) ;
#123432 = CARTESIAN_POINT('Ctrl Pts',(-20.213834085187,12.4171763297159,130.829710899479)) ;
#123433 = CARTESIAN_POINT('Ctrl Pts',(-20.3157550169223,12.3431378103405,
131.094146510188)) ;
#123434 = CARTESIAN_POINT('Ctrl Pts',(-20.4194887113378,12.346743528454,131.364286240996)) ;
#123435 = CARTESIAN_POINT('Ctrl Pts',(-20.520481797598,12.4272275492429,131.626120094335)) ;
#123436 = CARTESIAN_POINT('Ctrl Pts',(-20.611016823755,12.5790159402385,131.857501904824)) ;
#123437 = CARTESIAN_POINT('Ctrl Pts',(-20.6858521505329,12.7916689357573,
132.042932726522)) ;
#123438 = CARTESIAN_POINT('Ctrl Pts',(-20.7400044978734,13.0498140627792,
132.167945329551)) ;
#123439 = CARTESIAN_POINT('Ctrl Pts',(-20.7702882549419,13.3331758335929,
132.223407605724)) ;
#123440 = CARTESIAN_POINT('Ctrl Pts',(-20.7756374687898,13.6238936791233,
132.205920744498)) ;
#123441 = CARTESIAN_POINT('Ctrl Pts',(-20.7560346724831,13.9010886430072,
132.115433800579)) ;
#123442 = CARTESIAN_POINT('Ctrl Pts',(-20.7137971359534,14.1432055625841,
131.958927687778)) ;
#123443 = CARTESIAN_POINT('Ctrl Pts',(-20.6524404739172,14.334107077719,131.746477396685)) ;
#123444 = CARTESIAN_POINT('Ctrl Pts',(-20.5777682256743,14.4587992015315,
131.495357936276)) ;
#123445 = CARTESIAN_POINT('Ctrl Pts',(-20.4950831691612,14.5101605092006,
131.220685228617)) ;
#123446 = CARTESIAN_POINT('Ctrl Pts',(-20.4112704543339,14.4834097462587,
130.942700325563)) ;
#123447 = CARTESIAN_POINT('Ctrl Pts',(-20.3332099228401,14.3809866888584,
130.681571480112)) ;
#123448 = CARTESIAN_POINT('Ctrl Pts',(-20.2668912037514,14.2089571493578,
130.454589975505)) ;
#123449 = CARTESIAN_POINT('Ctrl Pts',(-20.218467666732,13.9828180389134,130.280212948204)) ;
#123450 = CARTESIAN_POINT('Ctrl Pts',(-20.1912296262005,13.7132629238328,
130.167271930086)) ;
#123451 = CARTESIAN_POINT('Ctrl Pts',(-20.1886479569655,13.4258376467274,
130.126737660166)) ;
#123452 = CARTESIAN_POINT('Ctrl Pts',(-20.2111109241553,13.1374631126408,
130.159264452679)) ;
#123453 = CARTESIAN_POINT('Ctrl Pts',(-20.2579828619858,12.8691197020598,
130.263056881787)) ;
#123454 = CARTESIAN_POINT('Ctrl Pts',(-20.3267504711329,12.6403113391648,
130.430759227376)) ;
#123455 = CARTESIAN_POINT('Ctrl Pts',(-20.4125317522278,12.4684206936737,
130.648356829009)) ;
#123456 = CARTESIAN_POINT('Ctrl Pts',(-20.511311636761,12.3638000131135,130.90360763348)) ;
#123457 = CARTESIAN_POINT('Ctrl Pts',(-20.6150180548314,12.3359859149595,
131.173540854503)) ;
#123458 = CARTESIAN_POINT('Ctrl Pts',(-20.7180532017287,12.3855342860159,
131.441422429249)) ;
#123459 = CARTESIAN_POINT('Ctrl Pts',(-20.8135713176557,12.5097023553619,
131.687312039212)) ;
#123460 = CARTESIAN_POINT('Ctrl Pts',(-20.8952342042776,12.6987170593864,
131.892805673695)) ;
#123461 = CARTESIAN_POINT('Ctrl Pts',(-20.958454326468,12.9413959891016,132.04418647609)) ;
#123462 = CARTESIAN_POINT('Ctrl Pts',(-20.998549110379,13.2164085190981,132.128309514099)) ;
#123463 = CARTESIAN_POINT('Ctrl Pts',(-21.0140910885354,13.5077477594262,
132.140512952863)) ;
#123464 = CARTESIAN_POINT('Ctrl Pts',(-21.0044134115614,13.7917086517815,
132.07920216301)) ;
#123465 = CARTESIAN_POINT('Ctrl Pts',(-20.9711009482148,14.0497091065288,
131.948804846017)) ;
#123466 = CARTESIAN_POINT('Ctrl Pts',(-20.9171221574838,14.2632251224131,
131.757995762905)) ;
#123467 = CARTESIAN_POINT('Ctrl Pts',(-20.8468654201181,14.4168538521645,
131.51953628378)) ;
#123468 = CARTESIAN_POINT('Ctrl Pts',(-20.76649453193,14.498759930122,131.251623228353)) ;
#123469 = CARTESIAN_POINT('Ctrl Pts',(-20.6822889980889,14.5035045472666,
130.97248421508)) ;
#123470 = CARTESIAN_POINT('Ctrl Pts',(-20.6013459781706,14.4313229189066,
130.703011266321)) ;
#123471 = CARTESIAN_POINT('Ctrl Pts',(-20.5294298629852,14.2860965422893,
130.459686692304)) ;
#123472 = CARTESIAN_POINT('Ctrl Pts',(-20.4733896837884,14.0806886832094,
130.263034151577)) ;
#123473 = CARTESIAN_POINT('Ctrl Pts',(-20.437003865906,13.8265803466444,130.123525632971)) ;
#123474 = CARTESIAN_POINT('Ctrl Pts',(-20.4242437811455,13.5441877343299,
130.053137789397)) ;
#123475 = CARTESIAN_POINT('Ctrl Pts',(-20.4365312961632,13.2530368711715,
130.055902630421)) ;
#123476 = CARTESIAN_POINT('Ctrl Pts',(-20.4737535574682,12.9741112441056,
130.131516179616)) ;
#123477 = CARTESIAN_POINT('Ctrl Pts',(-20.5340120502757,12.727211784615,130.274403584584)) ;
#123478 = CARTESIAN_POINT('Ctrl Pts',(-20.6135558274094,12.5305676715835,
130.47368429756)) ;
#123479 = CARTESIAN_POINT('Ctrl Pts',(-20.7074108358281,12.3976028269524,
130.7147928397)) ;
#123480 = CARTESIAN_POINT('Ctrl Pts',(-20.8102697894059,12.3378877483635,
130.982018981764)) ;
#123481 = CARTESIAN_POINT('Ctrl Pts',(-20.9141444616179,12.3561146706411,
131.252466517533)) ;
#123482 = CARTESIAN_POINT('Ctrl Pts',(-21.013548346515,12.4504996571453,131.509715354224)) ;
#123483 = CARTESIAN_POINT('Ctrl Pts',(-21.1017319257438,12.6151918757671,
131.734128219321)) ;
#123484 = CARTESIAN_POINT('Ctrl Pts',(-21.1727252896726,12.8367628546182,
131.908472936722)) ;
#123485 = CARTESIAN_POINT('Ctrl Pts',(-21.2228063284793,13.1024713310692,
132.02145618296)) ;
#123486 = CARTESIAN_POINT('Ctrl Pts',(-21.2483471373565,13.3880985112024,
132.063131681932)) ;
#123487 = CARTESIAN_POINT('Ctrl Pts',(-21.2488921318712,13.6786302833929,
132.03149649857)) ;
#123488 = CARTESIAN_POINT('Ctrl Pts',(-21.2248618457064,13.9495118102634,
131.928235541362)) ;
#123489 = CARTESIAN_POINT('Ctrl Pts',(-21.1787560649986,14.1831630718956,
131.760424667583)) ;
#123490 = CARTESIAN_POINT('Ctrl Pts',(-21.1147226870487,14.3622887223182,
131.540299304929)) ;
#123491 = CARTESIAN_POINT('Ctrl Pts',(-21.0373135712912,14.4748192512671,
131.28083347839)) ;
#123492 = CARTESIAN_POINT('Ctrl Pts',(-20.9542091849475,14.5109473635331,
131.005069073046)) ;
#123493 = CARTESIAN_POINT('Ctrl Pts',(-20.8711615353629,14.4698938664046,
130.729403038778)) ;
#123494 = CARTESIAN_POINT('Ctrl Pts',(-20.7947773885022,14.3536144682459,
130.473115915764)) ;
#123495 = CARTESIAN_POINT('Ctrl Pts',(-20.7314926566507,14.1706211200802,
130.255100908174)) ;
#123496 = CARTESIAN_POINT('Ctrl Pts',(-20.6865866876849,13.9337365390504,
130.090746076654)) ;
#123497 = CARTESIAN_POINT('Ctrl Pts',(-20.6640317813757,13.6617103922721,
129.991857066117)) ;
#123498 = CARTESIAN_POINT('Ctrl Pts',(-20.6660448486166,13.3701431433412,
129.964445738418)) ;
#123499 = CARTESIAN_POINT('Ctrl Pts',(-20.6933950437576,13.0839500606497,
130.011232944482)) ;
#123500 = CARTESIAN_POINT('Ctrl Pts',(-20.7444685293644,12.8226368169183,
130.127408051906)) ;
#123501 = CARTESIAN_POINT('Ctrl Pts',(-20.8166965559811,12.603615233857,130.305292057328)) ;
#123502 = CARTESIAN_POINT('Ctrl Pts',(-20.9053725966928,12.443223881209,130.531268705482)) ;
#123503 = CARTESIAN_POINT('Ctrl Pts',(-21.0058923229845,12.3525997217998,
130.791559536771)) ;
#123504 = CARTESIAN_POINT('Ctrl Pts',(-21.109651199822,12.339390379435,131.061737133445)) ;
#123505 = CARTESIAN_POINT('Ctrl Pts',(-21.2119649378887,12.4034681613504,
131.327439559372)) ;
#123506 = CARTESIAN_POINT('Ctrl Pts',(-21.3052562726005,12.5405073209883,
131.56686992949)) ;
#123507 = CARTESIAN_POINT('Ctrl Pts',(-21.3841471163856,12.742000710491,131.764047288441)) ;
#123508 = CARTESIAN_POINT('Ctrl Pts',(-21.4427047415853,12.9900803066021,
131.902157135438)) ;
#123509 = CARTESIAN_POINT('Ctrl Pts',(-21.4785501947781,13.2708160842573,
131.973683053502)) ;
#123510 = CARTESIAN_POINT('Ctrl Pts',(-21.4892592807922,13.5613606280666,
131.971916172654)) ;
#123511 = CARTESIAN_POINT('Ctrl Pts',(-21.4750643268527,13.8428562082264,
131.897307591027)) ;
#123512 = CARTESIAN_POINT('Ctrl Pts',(-21.4372222388411,14.0951248182504,
131.753467391875)) ;
#123513 = CARTESIAN_POINT('Ctrl Pts',(-21.3801699783513,14.2968155376203,
131.553906783451)) ;
#123514 = CARTESIAN_POINT('Ctrl Pts',(-21.3073404665403,14.4382063534547,
131.307842622038)) ;
#123515 = CARTESIAN_POINT('Ctrl Pts',(-21.2257750525136,14.5055714123115,
131.036462132016)) ;
#123516 = CARTESIAN_POINT('Ctrl Pts',(-21.1419504646032,14.4957941615493,
130.758568660941)) ;
#123517 = CARTESIAN_POINT('Ctrl Pts',(-21.062130144461,14.4095661599452,130.492310196492)) ;
#123518 = CARTESIAN_POINT('Ctrl Pts',(-20.9925528707413,14.2515334104405,
130.255766002423)) ;
#123519 = CARTESIAN_POINT('Ctrl Pts',(-20.9397828713012,14.0347235705321,
130.068496746948)) ;
#123520 = CARTESIAN_POINT('Ctrl Pts',(-20.9078955950986,13.7751698912538,
129.94233748602)) ;
#123521 = CARTESIAN_POINT('Ctrl Pts',(-20.8997160785567,13.489554992756,129.885321758747)) ;
#123522 = CARTESIAN_POINT('Ctrl Pts',(-20.9167899789178,13.1989623651925,
129.902052359333)) ;
#123523 = CARTESIAN_POINT('Ctrl Pts',(-20.9585152633915,12.9245155111551,
129.990817188961)) ;
#123524 = CARTESIAN_POINT('Ctrl Pts',(-21.0230710384516,12.6850931696754,
130.1461348862)) ;
#123525 = CARTESIAN_POINT('Ctrl Pts',(-21.1051698936851,12.5007200280461,
130.353109490092)) ;
#123526 = CARTESIAN_POINT('Ctrl Pts',(-21.2017300839304,12.3802347954754,
130.601895637296)) ;
#123527 = CARTESIAN_POINT('Ctrl Pts',(-21.3047713404402,12.3354177836866,
130.86988001272)) ;
#123528 = CARTESIAN_POINT('Ctrl Pts',(-21.4088230503547,12.3682931667049,
131.140651524699)) ;
#123529 = CARTESIAN_POINT('Ctrl Pts',(-21.5062542759513,12.4764500212594,
131.392235920731)) ;
#123530 = CARTESIAN_POINT('Ctrl Pts',(-21.5916025918959,12.6527561710341,
131.608397293271)) ;
#123531 = CARTESIAN_POINT('Ctrl Pts',(-21.6590311393467,12.8841372623909,
131.77224964389)) ;
#123532 = CARTESIAN_POINT('Ctrl Pts',(-21.7046072134825,13.1550291138396,
131.87215932753)) ;
#123533 = CARTESIAN_POINT('Ctrl Pts',(-21.7255333174223,13.4437302446049,
131.900234737756)) ;
#123534 = CARTESIAN_POINT('Ctrl Pts',(-21.7212604449213,13.7319393210826,
131.854574354767)) ;
#123535 = CARTESIAN_POINT('Ctrl Pts',(-21.6929317986939,13.996548190544,131.738831324701)) ;
#123536 = CARTESIAN_POINT('Ctrl Pts',(-21.6430685171198,14.2215298509627,
131.56000823255)) ;
#123537 = CARTESIAN_POINT('Ctrl Pts',(-21.5759281474204,14.38914835891,131.330697063604)) ;
#123538 = CARTESIAN_POINT('Ctrl Pts',(-21.4974078326725,14.4871687209254,
131.068241553781)) ;
#123539 = CARTESIAN_POINT('Ctrl Pts',(-21.4134771466602,14.5093408038881,
130.789919219591)) ;
#123540 = CARTESIAN_POINT('Ctrl Pts',(-21.3307764849043,14.4530254210031,
130.515076303721)) ;
#123541 = CARTESIAN_POINT('Ctrl Pts',(-21.2568613332395,14.3240304850431,
130.266200944563)) ;
#123542 = CARTESIAN_POINT('Ctrl Pts',(-21.1965031358292,14.1290978573837,
130.056618503273)) ;
#123543 = CARTESIAN_POINT('Ctrl Pts',(-21.1557411885856,13.8855602682148,
129.904586032072)) ;
#123544 = CARTESIAN_POINT('Ctrl Pts',(-21.1375373161458,13.605841493294,129.818053721067)) ;
#123545 = CARTESIAN_POINT('Ctrl Pts',(-21.1444136266794,13.3160019490386,
129.805155623741)) ;
#123546 = CARTESIAN_POINT('Ctrl Pts',(-21.1762636439198,13.0326884812318,
129.865076095617)) ;
#123547 = CARTESIAN_POINT('Ctrl Pts',(-21.2319115326232,12.7766370515925,
129.994424641396)) ;
#123548 = CARTESIAN_POINT('Ctrl Pts',(-21.3078505230511,12.5676696843858,
130.183109710706)) ;
#123549 = CARTESIAN_POINT('Ctrl Pts',(-21.3987133740418,12.4206516952527,
130.415612728524)) ;
#123550 = CARTESIAN_POINT('Ctrl Pts',(-21.5001018874593,12.34431502245,130.678595897684)) ;
#123551 = CARTESIAN_POINT('Ctrl Pts',(-21.604355434881,12.345456773331,130.950092534873)) ;
#123552 = CARTESIAN_POINT('Ctrl Pts',(-21.7056774142942,12.4241540990105,
131.212838185246)) ;
#123553 = CARTESIAN_POINT('Ctrl Pts',(-21.7963153488062,12.5736455946733,
131.444615300507)) ;
#123554 = CARTESIAN_POINT('Ctrl Pts',(-21.8716294111361,12.7844245874558,
131.631479009685)) ;
#123555 = CARTESIAN_POINT('Ctrl Pts',(-21.926464113242,13.0412646550238,131.758504009558)) ;
#123556 = CARTESIAN_POINT('Ctrl Pts',(-21.9575791398446,13.3250315602578,
131.816289040301)) ;
#123557 = CARTESIAN_POINT('Ctrl Pts',(-21.9635975249706,13.615649410723,131.800779000358)) ;
#123558 = CARTESIAN_POINT('Ctrl Pts',(-21.9447887810927,13.8929004143671,
131.712695653985)) ;
#123559 = CARTESIAN_POINT('Ctrl Pts',(-21.9031267111208,14.1366367418866,
131.557822791133)) ;
#123560 = CARTESIAN_POINT('Ctrl Pts',(-21.8425040812558,14.3287834464846,
131.347629205609)) ;
#123561 = CARTESIAN_POINT('Ctrl Pts',(-21.7678540280259,14.4563288635319,
131.096426004095)) ;
#123562 = CARTESIAN_POINT('Ctrl Pts',(-21.6851288303161,14.5097636487804,
130.821575692504)) ;
#123563 = CARTESIAN_POINT('Ctrl Pts',(-21.6014964088301,14.4852491667338,
130.544211499597)) ;
#123564 = CARTESIAN_POINT('Ctrl Pts',(-21.523248358388,14.3852131560936,130.282568889525)) ;
#123565 = CARTESIAN_POINT('Ctrl Pts',(-21.4563633176233,14.2148994142931,
130.053885615142)) ;
#123566 = CARTESIAN_POINT('Ctrl Pts',(-21.4073363060667,13.9895604970269,
129.877675130071)) ;
#123567 = CARTESIAN_POINT('Ctrl Pts',(-21.3795391128537,13.722649621575,129.763310479199)) ;
#123568 = CARTESIAN_POINT('Ctrl Pts',(-21.3761385230511,13.4342098870415,
129.720221810057)) ;
#123569 = CARTESIAN_POINT('Ctrl Pts',(-21.3978578853594,13.145818281647,129.750615209782)) ;
#123570 = CARTESIAN_POINT('Ctrl Pts',(-21.4442331193328,12.8759127187507,
129.852856124059)) ;
#123571 = CARTESIAN_POINT('Ctrl Pts',(-21.512001278979,12.646886857505,130.017831473784)) ;
#123572 = CARTESIAN_POINT('Ctrl Pts',(-21.5978716016616,12.4721832267463,
130.23548160431)) ;
#123573 = CARTESIAN_POINT('Ctrl Pts',(-21.6955599071442,12.3661739230268,
130.487824821297)) ;
#123574 = CARTESIAN_POINT('Ctrl Pts',(-21.8000520177911,12.3355863381279,
130.759770244015)) ;
#123575 = CARTESIAN_POINT('Ctrl Pts',(-21.9029799864568,12.383119877217,131.027414224694)) ;
#123576 = CARTESIAN_POINT('Ctrl Pts',(-21.9989039448222,12.5053833335783,
131.274450432666)) ;
#123577 = CARTESIAN_POINT('Ctrl Pts',(-22.0808309670336,12.6923271245218,
131.480792497128)) ;
#123578 = CARTESIAN_POINT('Ctrl Pts',(-22.1446987970862,12.933586655108,131.634070485524)) ;
#123579 = CARTESIAN_POINT('Ctrl Pts',(-22.1855556015519,13.2085815637178,
131.720337818846)) ;
#123580 = CARTESIAN_POINT('Ctrl Pts',(-22.2017695623135,13.499055887524,131.734588727789)) ;
#123581 = CARTESIAN_POINT('Ctrl Pts',(-22.1928346734152,13.7836908824952,
131.67542411847)) ;
#123582 = CARTESIAN_POINT('Ctrl Pts',(-22.1601714423331,14.0427282723312,
131.546925391615)) ;
#123583 = CARTESIAN_POINT('Ctrl Pts',(-22.1067337756389,14.2577310864089,
131.357698532383)) ;
#123584 = CARTESIAN_POINT('Ctrl Pts',(-22.0370124630534,14.4131665395365,
131.120862803271)) ;
#123585 = CARTESIAN_POINT('Ctrl Pts',(-21.9566962255491,14.4973756020118,
130.853040421815)) ;
#123586 = CARTESIAN_POINT('Ctrl Pts',(-21.8729279876658,14.5046723914937,
130.575350665997)) ;
#123587 = CARTESIAN_POINT('Ctrl Pts',(-21.7912035400918,14.4343110972272,
130.303348729222)) ;
#123588 = CARTESIAN_POINT('Ctrl Pts',(-21.7191872942723,14.2913902739099,
130.059848443852)) ;
#123589 = CARTESIAN_POINT('Ctrl Pts',(-21.6625256909842,14.0872938687907,
129.861320234201)) ;
#123590 = CARTESIAN_POINT('Ctrl Pts',(-21.6255724955298,13.8349905737135,
129.720243192355)) ;
#123591 = CARTESIAN_POINT('Ctrl Pts',(-21.6120328126858,13.5522016078203,
129.647460332955)) ;
#123592 = CARTESIAN_POINT('Ctrl Pts',(-21.623622872742,13.261176925901,129.64821085162)) ;
#123593 = CARTESIAN_POINT('Ctrl Pts',(-21.6602148810404,12.9814105366867,
129.721952022886)) ;
#123594 = CARTESIAN_POINT('Ctrl Pts',(-21.7196534333109,12.7341368123324,
129.862553970206)) ;
#123595 = CARTESIAN_POINT('Ctrl Pts',(-21.7988553081735,12.5351661127334,
130.060752426259)) ;
#123596 = CARTESIAN_POINT('Ctrl Pts',(-21.8928056856465,12.4000170335594,
130.30200784534)) ;
#123597 = CARTESIAN_POINT('Ctrl Pts',(-21.9950158650803,12.3385940998212,
130.567504847325)) ;
#123598 = CARTESIAN_POINT('Ctrl Pts',(-22.0991055754472,12.3545286959988,
130.838523437866)) ;
#123599 = CARTESIAN_POINT('Ctrl Pts',(-22.198792064463,12.4469846985816,131.096579489399)) ;
#123600 = CARTESIAN_POINT('Ctrl Pts',(-22.2874703472673,12.6102580102747,
131.322388272232)) ;
#123601 = CARTESIAN_POINT('Ctrl Pts',(-22.3586713429203,12.8296978065605,
131.4974644856)) ;
#123602 = CARTESIAN_POINT('Ctrl Pts',(-22.4092935566175,13.0929764235486,
131.612190617179)) ;
#123603 = CARTESIAN_POINT('Ctrl Pts',(-22.4357877911489,13.3798715648176,
131.656456165167)) ;
#123604 = CARTESIAN_POINT('Ctrl Pts',(-22.4369919562027,13.6705227890218,
131.626757747734)) ;
#123605 = CARTESIAN_POINT('Ctrl Pts',(-22.4136887889266,13.9421700624616,
131.525632072754)) ;
#123606 = CARTESIAN_POINT('Ctrl Pts',(-22.3679163610009,14.1780191075409,
131.358654623663)) ;
#123607 = CARTESIAN_POINT('Ctrl Pts',(-22.3045084630622,14.3579768131381,
131.140480788667)) ;
#123608 = CARTESIAN_POINT('Ctrl Pts',(-22.2275826101986,14.4725057536027,
130.882499856807)) ;
#123609 = CARTESIAN_POINT('Ctrl Pts',(-22.1444232291687,14.5110248787741,
130.60651491726)) ;
#123610 = CARTESIAN_POINT('Ctrl Pts',(-22.0612174095962,14.4721191985818,
130.33036485736)) ;
#123611 = CARTESIAN_POINT('Ctrl Pts',(-21.984532639996,14.3577454334386,130.073186159009)) ;
#123612 = CARTESIAN_POINT('Ctrl Pts',(-21.9209902476645,14.1770688600788,
129.854519186806)) ;
#123613 = CARTESIAN_POINT('Ctrl Pts',(-21.8754073396789,13.9416997135302,
129.688189111058)) ;
#123614 = CARTESIAN_POINT('Ctrl Pts',(-21.8521280328219,13.6694103999149,
129.587060443625)) ;
#123615 = CARTESIAN_POINT('Ctrl Pts',(-21.8533886977509,13.3798585419127,
129.557657884149)) ;
#123616 = CARTESIAN_POINT('Ctrl Pts',(-21.8798930282876,13.0927639720694,
129.601925595743)) ;
#123617 = CARTESIAN_POINT('Ctrl Pts',(-21.9305070655624,12.8294541996799,
129.716631316769)) ;
#123618 = CARTESIAN_POINT('Ctrl Pts',(-22.0021915119571,12.6090079342562,
129.892932878091)) ;
#123619 = CARTESIAN_POINT('Ctrl Pts',(-22.0906529644775,12.4466659033485,
130.118224388233)) ;
#123620 = CARTESIAN_POINT('Ctrl Pts',(-22.1903372657479,12.3544265083851,
130.376275283153)) ;
#123621 = CARTESIAN_POINT('Ctrl Pts',(-22.2942873445746,12.338485561048,130.646936791498)) ;
#123622 = CARTESIAN_POINT('Ctrl Pts',(-22.3973135054693,12.4009576642386,
130.914537921283)) ;
#123623 = CARTESIAN_POINT('Ctrl Pts',(-22.4904420137874,12.5356623711056,
131.153649825202)) ;
#123624 = CARTESIAN_POINT('Ctrl Pts',(-22.5695739948327,12.7342794409358,
131.351681157617)) ;
#123625 = CARTESIAN_POINT('Ctrl Pts',(-22.6291160828329,12.9822472239535,
131.492506830932)) ;
#123626 = CARTESIAN_POINT('Ctrl Pts',(-22.6656693979879,13.2626106306711,
131.566076960599)) ;
#123627 = CARTESIAN_POINT('Ctrl Pts',(-22.6770955873921,13.5537332478673,
131.566337188206)) ;
#123628 = CARTESIAN_POINT('Ctrl Pts',(-22.6635414721597,13.835078244523,131.493672842858)) ;
#123629 = CARTESIAN_POINT('Ctrl Pts',(-22.6266625017424,14.0872564093589,
131.352837031821)) ;
#123630 = CARTESIAN_POINT('Ctrl Pts',(-22.5697278634071,14.2922554026262,
131.153365374301)) ;
#123631 = CARTESIAN_POINT('Ctrl Pts',(-22.4973810272917,14.4349646687422,
130.908797184374)) ;
#123632 = CARTESIAN_POINT('Ctrl Pts',(-22.4163391881196,14.50455407939,130.639073907025)) ;
#123633 = CARTESIAN_POINT('Ctrl Pts',(-22.3321658591823,14.4973581073499,
130.360039361529)) ;
#123634 = CARTESIAN_POINT('Ctrl Pts',(-22.2518685737339,14.4126016063702,
130.092261416254)) ;
#123635 = CARTESIAN_POINT('Ctrl Pts',(-22.1824698979615,14.2578369760295,
129.856517613998)) ;
#123636 = CARTESIAN_POINT('Ctrl Pts',(-22.128910794309,14.0423605049128,129.666858615955)) ;
#123637 = CARTESIAN_POINT('Ctrl Pts',(-22.0962688121286,13.7833429469769,
129.538433890932)) ;
#123638 = CARTESIAN_POINT('Ctrl Pts',(-22.087408581468,13.4972453189194,129.479321882593)) ;
#123639 = CARTESIAN_POINT('Ctrl Pts',(-22.1036837457702,13.2077136867894,
129.493862670111)) ;
#123640 = CARTESIAN_POINT('Ctrl Pts',(-22.1448226422972,12.9318530296234,
129.580826868233)) ;
#123641 = CARTESIAN_POINT('Ctrl Pts',(-22.2083889117373,12.6922551548189,
129.733430569201)) ;
#123642 = CARTESIAN_POINT('Ctrl Pts',(-22.2905762804596,12.5046664561304,
129.940421973245)) ;
#123643 = CARTESIAN_POINT('Ctrl Pts',(-22.3868645087998,12.3825157092279,
130.188426397229)) ;
#123644 = CARTESIAN_POINT('Ctrl Pts',(-22.4895735286878,12.3357140446238,
130.455506685267)) ;
#123645 = CARTESIAN_POINT('Ctrl Pts',(-22.593480759488,12.36606795923,130.725932566438)) ;
#123646 = CARTESIAN_POINT('Ctrl Pts',(-22.6916956961957,12.4727573842292,
130.979628387978)) ;
#123647 = CARTESIAN_POINT('Ctrl Pts',(-22.7772373371253,12.6471452972706,
131.196428921888)) ;
#123648 = CARTESIAN_POINT('Ctrl Pts',(-22.8450776069585,12.8766362128536,
131.361554408823)) ;
#123649 = CARTESIAN_POINT('Ctrl Pts',(-22.8913157755796,13.1457609498557,
131.463497390875)) ;
#123650 = CARTESIAN_POINT('Ctrl Pts',(-22.9131064687665,13.4362085163513,
131.493864737926)) ;
#123651 = CARTESIAN_POINT('Ctrl Pts',(-22.9095252366571,13.7232902090159,
131.4503951076)) ;
#123652 = CARTESIAN_POINT('Ctrl Pts',(-22.8818492535102,13.9896012437994,
131.336467064761)) ;
#123653 = CARTESIAN_POINT('Ctrl Pts',(-22.8324906093414,14.215929645434,131.15911392552)) ;
#123654 = CARTESIAN_POINT('Ctrl Pts',(-22.7659015545217,14.3851342373848,
130.931470999385)) ;
#123655 = CARTESIAN_POINT('Ctrl Pts',(-22.6875045184051,14.4854517125692,
130.669322994244)) ;
#123656 = CARTESIAN_POINT('Ctrl Pts',(-22.603799348601,14.5096986582257,130.391723047381)) ;
#123657 = CARTESIAN_POINT('Ctrl Pts',(-22.5211552560533,14.4561737442075,
130.117138838309)) ;
#123658 = CARTESIAN_POINT('Ctrl Pts',(-22.4464425125738,14.3282784828902,
129.865710255824)) ;
#123659 = CARTESIAN_POINT('Ctrl Pts',(-22.3859620483162,14.1363002885468,
129.655987705534)) ;
#123660 = CARTESIAN_POINT('Ctrl Pts',(-22.3443239578635,13.8924838529507,
129.501179650082)) ;
#123661 = CARTESIAN_POINT('Ctrl Pts',(-22.3255548355993,13.6154600840217,
129.413243078531)) ;
#123662 = CARTESIAN_POINT('Ctrl Pts',(-22.3316054927386,13.3244464776438,
129.397782302623)) ;
#123663 = CARTESIAN_POINT('Ctrl Pts',(-22.362789865854,13.0407280398606,129.455770685946)) ;
#123664 = CARTESIAN_POINT('Ctrl Pts',(-22.4175554506853,12.7843964023836,
129.582650808215)) ;
#123665 = CARTESIAN_POINT('Ctrl Pts',(-22.4928772666945,12.5734337589229,
129.769524564463)) ;
#123666 = CARTESIAN_POINT('Ctrl Pts',(-22.5839516709931,12.4236458719393,
130.002437978547)) ;
#123667 = CARTESIAN_POINT('Ctrl Pts',(-22.6846738463837,12.3455712337427,
130.263634905139)) ;
#123668 = CARTESIAN_POINT('Ctrl Pts',(-22.789260868032,12.3443023954149,130.535996594304)) ;
#123669 = CARTESIAN_POINT('Ctrl Pts',(-22.89070007856,12.4209332624995,130.799108040952)) ;
#123670 = CARTESIAN_POINT('Ctrl Pts',(-22.9817398361439,12.5684898191716,
131.032050055215)) ;
#123671 = CARTESIAN_POINT('Ctrl Pts',(-23.0577480467898,12.7783873972307,
131.220853670815)) ;
#123672 = CARTESIAN_POINT('Ctrl Pts',(-23.1130745475148,13.0341437387016,
131.349338722741)) ;
#123673 = CARTESIAN_POINT('Ctrl Pts',(-23.1447720687108,13.3161554584295,
131.408969086763)) ;
#123674 = CARTESIAN_POINT('Ctrl Pts',(-23.1515934109415,13.6077103928711,
131.395709155052)) ;
#123675 = CARTESIAN_POINT('Ctrl Pts',(-23.1333286351704,13.8863968339185,
131.309116820984)) ;
#123676 = CARTESIAN_POINT('Ctrl Pts',(-23.092261773277,14.1306964208414,131.156045144409)) ;
#123677 = CARTESIAN_POINT('Ctrl Pts',(-23.0323203050515,14.3238933798465,
130.947948945004)) ;
#123678 = CARTESIAN_POINT('Ctrl Pts',(-22.9580389719213,14.4535138148578,
130.697833001555)) ;
#123679 = CARTESIAN_POINT('Ctrl Pts',(-22.8754326033728,14.5094099207336,
130.423321601385)) ;
#123680 = CARTESIAN_POINT('Ctrl Pts',(-22.7912683304849,14.4867701490887,
130.144213707131)) ;
#123681 = CARTESIAN_POINT('Ctrl Pts',(-22.7132364319315,14.3890643501402,
129.883381354507)) ;
#123682 = CARTESIAN_POINT('Ctrl Pts',(-22.6459538319007,14.2211868758739,
129.65358774104)) ;
#123683 = CARTESIAN_POINT('Ctrl Pts',(-22.5961304153725,13.9958857732727,
129.474863269661)) ;
#123684 = CARTESIAN_POINT('Ctrl Pts',(-22.5678649144097,13.731479333369,129.359334414953)) ;
#123685 = CARTESIAN_POINT('Ctrl Pts',(-22.5636217990249,13.44236393195,129.313663179006)) ;
#123686 = CARTESIAN_POINT('Ctrl Pts',(-22.5848238291133,13.1530743208287,
129.342464490565)) ;
#123687 = CARTESIAN_POINT('Ctrl Pts',(-22.6301149482752,12.884256615766,129.441790820135)) ;
#123688 = CARTESIAN_POINT('Ctrl Pts',(-22.6978320294382,12.6519995409111,
129.606348451409)) ;
#123689 = CARTESIAN_POINT('Ctrl Pts',(-22.7828059113389,12.4766942451725,
129.821579606252)) ;
#123690 = CARTESIAN_POINT('Ctrl Pts',(-22.8804228762943,12.3681120664589,
130.073631874159)) ;
#123691 = CARTESIAN_POINT('Ctrl Pts',(-22.9849198201405,12.3353450088633,
130.345571088682)) ;
#123692 = CARTESIAN_POINT('Ctrl Pts',(-23.0880396701076,12.380878936013,130.613744761632)) ;
#123693 = CARTESIAN_POINT('Ctrl Pts',(-23.1839462416439,12.5006496945069,
130.860845156785)) ;
#123694 = CARTESIAN_POINT('Ctrl Pts',(-23.266521775703,12.6862349323656,131.06900841109)) ;
#123695 = CARTESIAN_POINT('Ctrl Pts',(-23.3307747879631,12.9253055935091,
131.223534372518)) ;
#123696 = CARTESIAN_POINT('Ctrl Pts',(-23.3724397745999,13.1996775352275,
131.31213337044)) ;
#123697 = CARTESIAN_POINT('Ctrl Pts',(-23.3894540507773,13.4900584277301,
131.32871644911)) ;
#123698 = CARTESIAN_POINT('Ctrl Pts',(-23.3812045124378,13.7765695978382,
131.27139174498)) ;
#123699 = CARTESIAN_POINT('Ctrl Pts',(-23.3489874615433,14.036835781509,131.144138279515)) ;
#123700 = CARTESIAN_POINT('Ctrl Pts',(-23.2963232747133,14.2522895995138,
130.957329544454)) ;
#123701 = CARTESIAN_POINT('Ctrl Pts',(-23.226675069615,14.410142724822,130.720563800581)) ;
#123702 = CARTESIAN_POINT('Ctrl Pts',(-23.1469566767061,14.4959011671627,
130.45465902455)) ;
#123703 = CARTESIAN_POINT('Ctrl Pts',(-23.0630393438504,14.5055615409164,
130.176461828221)) ;
#123704 = CARTESIAN_POINT('Ctrl Pts',(-22.9812984775672,14.4373878436055,
129.904473138408)) ;
#123705 = CARTESIAN_POINT('Ctrl Pts',(-22.9089719408676,14.2968054840673,
129.660103398097)) ;
#123706 = CARTESIAN_POINT('Ctrl Pts',(-22.8515548229148,14.0934338457394,
129.459228202194)) ;
#123707 = CARTESIAN_POINT('Ctrl Pts',(-22.8141130964861,13.8423636115969,
129.316759095522)) ;
#123708 = CARTESIAN_POINT('Ctrl Pts',(-22.7998637079465,13.5615575056706,
129.242062802515)) ;
#123709 = CARTESIAN_POINT('Ctrl Pts',(-22.8107205774882,13.2694346825445,
129.240546215534)) ;
#123710 = CARTESIAN_POINT('Ctrl Pts',(-22.8464960658209,12.9897645897098,
129.311993364082)) ;
#123711 = CARTESIAN_POINT('Ctrl Pts',(-22.9054877650127,12.7403850896867,
129.451171580521)) ;
#123712 = CARTESIAN_POINT('Ctrl Pts',(-22.9841235537869,12.5401777346667,
129.647762655678)) ;
#123713 = CARTESIAN_POINT('Ctrl Pts',(-23.0774322582716,12.403253810304,129.887237341054)) ;
#123714 = CARTESIAN_POINT('Ctrl Pts',(-23.1796029037189,12.3392654629647,
130.152574531222)) ;
#123715 = CARTESIAN_POINT('Ctrl Pts',(-23.2840127627671,12.3529796001613,
130.424441355207)) ;
#123716 = CARTESIAN_POINT('Ctrl Pts',(-23.3838205000932,12.4434150313968,
130.682876822953)) ;
#123717 = CARTESIAN_POINT('Ctrl Pts',(-23.4725822238479,12.6038143238447,
130.909076120196)) ;
#123718 = CARTESIAN_POINT('Ctrl Pts',(-23.5448588483883,12.8232747601352,
131.087059295261)) ;
#123719 = CARTESIAN_POINT('Ctrl Pts',(-23.5959036411586,13.0848674968843,
131.203128049166)) ;
#123720 = CARTESIAN_POINT('Ctrl Pts',(-23.6231518851354,13.3712341167296,
131.2496031028)) ;
#123721 = CARTESIAN_POINT('Ctrl Pts',(-23.6251153546057,13.662067069188,131.222130850832)) ;
#123722 = CARTESIAN_POINT('Ctrl Pts',(-23.602443415498,13.9347879566426,131.122806374667)) ;
#123723 = CARTESIAN_POINT('Ctrl Pts',(-23.5575106719909,14.1711547211457,
130.958420904302)) ;
#123724 = CARTESIAN_POINT('Ctrl Pts',(-23.4942303983001,14.3538986016763,
130.740436482537)) ;
#123725 = CARTESIAN_POINT('Ctrl Pts',(-23.4179436544872,14.4699515412555,
130.484481417006)) ;
#123726 = CARTESIAN_POINT('Ctrl Pts',(-23.3347210664795,14.5110117292323,
130.208235504847)) ;
#123727 = CARTESIAN_POINT('Ctrl Pts',(-23.2514904333782,14.4745400439387,
129.932050841537)) ;
#123728 = CARTESIAN_POINT('Ctrl Pts',(-23.1740871767367,14.3614975022745,
129.672577858496)) ;
#123729 = CARTESIAN_POINT('Ctrl Pts',(-23.1103820389956,14.1829580281289,
129.453553214764)) ;
#123730 = CARTESIAN_POINT('Ctrl Pts',(-23.0642199301642,13.94924048582,129.285561754027)) ;
#123731 = CARTESIAN_POINT('Ctrl Pts',(-23.0402642951649,13.6775800783231,
129.182436219737)) ;
#123732 = CARTESIAN_POINT('Ctrl Pts',(-23.0407276337131,13.3886494305686,
129.150753202406)) ;
#123733 = CARTESIAN_POINT('Ctrl Pts',(-23.0667742903849,13.0993477502972,
129.193462997382)) ;
#123734 = CARTESIAN_POINT('Ctrl Pts',(-23.1164380145016,12.8369457747394,
129.305623227605)) ;
#123735 = CARTESIAN_POINT('Ctrl Pts',(-23.1878595146298,12.6140529182667,
129.481009963298)) ;
#123736 = CARTESIAN_POINT('Ctrl Pts',(-23.2755753916716,12.4507322880218,
129.704266224405)) ;
#123737 = CARTESIAN_POINT('Ctrl Pts',(-23.3750284522621,12.3558899058093,
129.961628164076)) ;
#123738 = CARTESIAN_POINT('Ctrl Pts',(-23.479686446813,12.3380969168945,130.23411873229)) ;
#123739 = CARTESIAN_POINT('Ctrl Pts',(-23.5815749533041,12.3976017184894,
130.498816720526)) ;
#123740 = CARTESIAN_POINT('Ctrl Pts',(-23.6757182527375,12.5305839180843,
130.740682440716)) ;
#123741 = CARTESIAN_POINT('Ctrl Pts',(-23.7554851540154,12.7283491883042,
130.94048328736)) ;
#123742 = CARTESIAN_POINT('Ctrl Pts',(-23.8154207293665,12.97427729496,131.082573958484)) ;
#123743 = CARTESIAN_POINT('Ctrl Pts',(-23.8527220355737,13.2539378203869,
131.158329529293)) ;
#123744 = CARTESIAN_POINT('Ctrl Pts',(-23.8649208036644,13.5450905398915,
131.160841634587)) ;
#123745 = CARTESIAN_POINT('Ctrl Pts',(-23.8520257273945,13.8275789493197,
131.090028727836)) ;
#123746 = CARTESIAN_POINT('Ctrl Pts',(-23.8158317196429,14.0806196920483,
130.951236564935)) ;
#123747 = CARTESIAN_POINT('Ctrl Pts',(-23.7591250103948,14.2877393448121,
130.75229965692)) ;
#123748 = CARTESIAN_POINT('Ctrl Pts',(-23.6878258800452,14.4312139219373,
130.511104094141)) ;
#123749 = CARTESIAN_POINT('Ctrl Pts',(-23.6063043055212,14.5038738405656,
130.239697508234)) ;
#123750 = CARTESIAN_POINT('Ctrl Pts',(-23.5222933412203,14.4984557258389,
129.961208367374)) ;
#123751 = CARTESIAN_POINT('Ctrl Pts',(-23.4420014140057,14.4164646007505,
129.693550319471)) ;
#123752 = CARTESIAN_POINT('Ctrl Pts',(-23.3717344521323,14.262213927018,129.455014247246)) ;
#123753 = CARTESIAN_POINT('Ctrl Pts',(-23.3180679682701,14.0497488038025,
129.265295151587)) ;
#123754 = CARTESIAN_POINT('Ctrl Pts',(-23.28462466296,13.7905256830516,129.134359382709)) ;
#123755 = CARTESIAN_POINT('Ctrl Pts',(-23.2750637821878,13.5064863468517,
129.073396466717)) ;
#123756 = CARTESIAN_POINT('Ctrl Pts',(-23.2908264747081,13.2142514411646,
129.08613493592)) ;
#123757 = CARTESIAN_POINT('Ctrl Pts',(-23.3308877115697,12.9406231812218,
129.170310866248)) ;
#123758 = CARTESIAN_POINT('Ctrl Pts',(-23.3941166605255,12.6982138034392,
129.321733729284)) ;
#123759 = CARTESIAN_POINT('Ctrl Pts',(-23.4755974532675,12.5096111619529,
129.5267733723)) ;
#123760 = CARTESIAN_POINT('Ctrl Pts',(-23.5716249889959,12.3850648455084,
129.773982751165)) ;
#123761 = CARTESIAN_POINT('Ctrl Pts',(-23.6743192939801,12.3359713262841,
130.040989207269)) ;
#123762 = CARTESIAN_POINT('Ctrl Pts',(-23.7783222708398,12.3641515786215,
130.311684259488)) ;
#123763 = CARTESIAN_POINT('Ctrl Pts',(-23.8766296215748,12.4683944870956,
130.565716794751)) ;
#123764 = CARTESIAN_POINT('Ctrl Pts',(-23.9628554188596,12.6414744959111,
130.784415332904)) ;
#123765 = CARTESIAN_POINT('Ctrl Pts',(-24.0312224543575,12.8692739699043,
130.951123740549)) ;
#123766 = CARTESIAN_POINT('Ctrl Pts',(-24.0782810666364,13.1394382776975,
131.05524281683)) ;
#123767 = CARTESIAN_POINT('Ctrl Pts',(-24.1005117267227,13.4257125359272,
131.08734716251)) ;
#123768 = CARTESIAN_POINT('Ctrl Pts',(-24.0978093052541,13.7153678906251,
131.046186164397)) ;
#123769 = CARTESIAN_POINT('Ctrl Pts',(-24.0707432978629,13.9823826139753,
130.934062209111)) ;
#123770 = CARTESIAN_POINT('Ctrl Pts',(-24.0219040196936,14.2103512804348,
130.758187634576)) ;
#123771 = CARTESIAN_POINT('Ctrl Pts',(-23.955849643307,14.3810373660196,130.532168758405)) ;
#123772 = CARTESIAN_POINT('Ctrl Pts',(-23.8777434923671,14.4835203984391,
130.270877518445)) ;
#123773 = CARTESIAN_POINT('Ctrl Pts',(-23.7940757142471,14.5102051461734,
129.993379912309)) ;
#123774 = CARTESIAN_POINT('Ctrl Pts',(-23.710961553393,14.4584272237243,129.717276640743)) ;
#123775 = CARTESIAN_POINT('Ctrl Pts',(-23.6363573990903,14.3332271033523,
129.466355935255)) ;
#123776 = CARTESIAN_POINT('Ctrl Pts',(-23.5751477681758,14.1422678192608,
129.25437061071)) ;
#123777 = CARTESIAN_POINT('Ctrl Pts',(-23.5330528209132,13.9003525396715,
129.09833046808)) ;
#123778 = CARTESIAN_POINT('Ctrl Pts',(-23.5135309290713,13.6237174619485,
129.008149760957)) ;
#123779 = CARTESIAN_POINT('Ctrl Pts',(-23.5188554697474,13.3329586763548,
128.990586666945)) ;
#123780 = CARTESIAN_POINT('Ctrl Pts',(-23.5493589827656,13.0482789829305,
129.04653418521)) ;
#123781 = CARTESIAN_POINT('Ctrl Pts',(-23.6036561801052,12.7905982685052,
129.171990054986)) ;
#123782 = CARTESIAN_POINT('Ctrl Pts',(-23.6780760446673,12.5792073074467,
129.356398168754)) ;
#123783 = CARTESIAN_POINT('Ctrl Pts',(-23.7687620320097,12.4271419499118,
129.588159424932)) ;
#123784 = CARTESIAN_POINT('Ctrl Pts',(-23.8695614818099,12.3466854310429,
129.849494389191)) ;
#123785 = CARTESIAN_POINT('Ctrl Pts',(-23.9740330662146,12.3433384713207,
130.121551280678)) ;
#123786 = CARTESIAN_POINT('Ctrl Pts',(-24.0753253630592,12.4172569566232,
130.384352183791)) ;
#123787 = CARTESIAN_POINT('Ctrl Pts',(-24.1671079597041,12.5633305895845,
130.619334311793)) ;
#123788 = CARTESIAN_POINT('Ctrl Pts',(-24.2433540945366,12.7708595617965,
130.808958800106)) ;
#123789 = CARTESIAN_POINT('Ctrl Pts',(-24.2994637691932,13.025326544213,130.939726803943)) ;
#123790 = CARTESIAN_POINT('Ctrl Pts',(-24.3320328505517,13.3082180027096,
131.001740671946)) ;
#123791 = CARTESIAN_POINT('Ctrl Pts',(-24.3395000117594,13.5990346851552,
130.990457636508)) ;
#123792 = CARTESIAN_POINT('Ctrl Pts',(-24.3221220233207,13.8774217687766,
130.906582943428)) ;
#123793 = CARTESIAN_POINT('Ctrl Pts',(-24.2816282044918,14.1239850259666,
130.755070979699)) ;
#123794 = CARTESIAN_POINT('Ctrl Pts',(-24.2220244331506,14.3192777030772,
130.547886906491)) ;
#123795 = CARTESIAN_POINT('Ctrl Pts',(-24.1480694747946,14.450773280104,130.298730541153)) ;
#123796 = CARTESIAN_POINT('Ctrl Pts',(-24.0658520531097,14.5087792742394,
130.025451200729)) ;
#123797 = CARTESIAN_POINT('Ctrl Pts',(-23.9816472191313,14.4887238114624,
129.746232190085)) ;
#123798 = CARTESIAN_POINT('Ctrl Pts',(-23.9030406933561,14.3928284673273,
129.483590372223)) ;
#123799 = CARTESIAN_POINT('Ctrl Pts',(-23.8353522715895,14.2263681576049,
129.252580503077)) ;
#123800 = CARTESIAN_POINT('Ctrl Pts',(-23.7851963074406,14.0038696004935,
129.073071183983)) ;
#123801 = CARTESIAN_POINT('Ctrl Pts',(-23.7560978597235,13.7389371650263,
128.954921255289)) ;
#123802 = CARTESIAN_POINT('Ctrl Pts',(-23.7511852521391,13.4518073481161,
128.907486201909)) ;
#123803 = CARTESIAN_POINT('Ctrl Pts',(-23.7715448720785,13.1616327343089,
128.933759632755)) ;
#123804 = CARTESIAN_POINT('Ctrl Pts',(-23.8164865399758,12.8906304369754,
129.031889334722)) ;
#123805 = CARTESIAN_POINT('Ctrl Pts',(-23.8832622051985,12.6585325356575,
129.193895242853)) ;
#123806 = CARTESIAN_POINT('Ctrl Pts',(-23.9677809880381,12.4808578781887,
129.407766266249)) ;
#123807 = CARTESIAN_POINT('Ctrl Pts',(-24.0659555708553,12.3697949694261,
129.661183417758)) ;
#123808 = CARTESIAN_POINT('Ctrl Pts',(-24.1692259037943,12.3353140236409,
129.929908779407)) ;
#123809 = CARTESIAN_POINT('Ctrl Pts',(-24.2728675346327,12.3783402030792,
130.199476077674)) ;
#123810 = CARTESIAN_POINT('Ctrl Pts',(-24.3690489704881,12.4961138022352,
130.447389063353)) ;
#123811 = CARTESIAN_POINT('Ctrl Pts',(-24.4521938819029,12.680095634731,130.657178424642)) ;
#123812 = CARTESIAN_POINT('Ctrl Pts',(-24.5170522529408,12.9180877630852,
130.813452787442)) ;
#123813 = CARTESIAN_POINT('Ctrl Pts',(-24.5593190809153,13.1911275854678,
130.903877630391)) ;
#123814 = CARTESIAN_POINT('Ctrl Pts',(-24.5771155225395,13.4815073291889,
130.92272617817)) ;
#123815 = CARTESIAN_POINT('Ctrl Pts',(-24.5695556225141,13.7684315330807,
130.867412489067)) ;
#123816 = CARTESIAN_POINT('Ctrl Pts',(-24.538185743673,14.0290764110969,130.742738622054)) ;
#123817 = CARTESIAN_POINT('Ctrl Pts',(-24.4856997530283,14.247309485019,130.556233652384)) ;
#123818 = CARTESIAN_POINT('Ctrl Pts',(-24.4171085411696,14.4057092189414,
130.322868851461)) ;
#123819 = CARTESIAN_POINT('Ctrl Pts',(-24.3371267720653,14.4946179014392,
130.055968417117)) ;
#123820 = CARTESIAN_POINT('Ctrl Pts',(-24.2532493451519,14.5063975048984,
129.777903719166)) ;
#123821 = CARTESIAN_POINT('Ctrl Pts',(-24.1711402608767,14.4401277902918,
129.504748463371)) ;
#123822 = CARTESIAN_POINT('Ctrl Pts',(-24.0987765462439,14.3020000140496,
129.26040859703)) ;
#123823 = CARTESIAN_POINT('Ctrl Pts',(-24.0408047371062,14.1003807123236,
129.057906743614)) ;
#123824 = CARTESIAN_POINT('Ctrl Pts',(-24.0026765942932,13.8504600276244,
128.91342573659)) ;
#123825 = CARTESIAN_POINT('Ctrl Pts',(-23.9876880401048,13.5690358349625,
128.836430226861)) ;
#123826 = CARTESIAN_POINT('Ctrl Pts',(-23.9979033292696,13.2773475296497,
128.833089888645)) ;
#123827 = CARTESIAN_POINT('Ctrl Pts',(-24.0328593108588,12.9978263790817,
128.902233054104)) ;
#123828 = CARTESIAN_POINT('Ctrl Pts',(-24.0912618908182,12.7470236955785,
129.039657768494)) ;
#123829 = CARTESIAN_POINT('Ctrl Pts',(-24.1692879855488,12.545343046617,129.234506974647)) ;
#123830 = CARTESIAN_POINT('Ctrl Pts',(-24.2623972637648,12.4062332571894,
129.473344009218)) ;
#123831 = CARTESIAN_POINT('Ctrl Pts',(-24.3641009492219,12.3400677783264,
129.737415771207)) ;
#123832 = CARTESIAN_POINT('Ctrl Pts',(-24.469019024179,12.3515723275397,130.010611884495)) ;
#123833 = CARTESIAN_POINT('Ctrl Pts',(-24.5686909269355,12.4396026158797,
130.268772857004)) ;
#123834 = CARTESIAN_POINT('Ctrl Pts',(-24.658038837005,12.5983880408564,130.496613023796)) ;
#123835 = CARTESIAN_POINT('Ctrl Pts',(-24.7306514855706,12.8155082856179,
130.675695316862)) ;
#123836 = CARTESIAN_POINT('Ctrl Pts',(-24.7827238953065,13.0777481932152,
130.79455185343)) ;
#123837 = CARTESIAN_POINT('Ctrl Pts',(-24.810519400862,13.364000804506,130.842603809486)) ;
#123838 = CARTESIAN_POINT('Ctrl Pts',(-24.8132060187631,13.6530970935561,
130.817462981774)) ;
#123839 = CARTESIAN_POINT('Ctrl Pts',(-24.7912152875116,13.9274411059631,
130.720031019279)) ;
#123840 = CARTESIAN_POINT('Ctrl Pts',(-24.7468930831162,14.1649405749744,
130.557453547458)) ;
#123841 = CARTESIAN_POINT('Ctrl Pts',(-24.6839050837765,14.3499177041157,
130.340235768366)) ;
#123842 = CARTESIAN_POINT('Ctrl Pts',(-24.6078837456822,14.4676736772021,
130.085060886655)) ;
#123843 = CARTESIAN_POINT('Ctrl Pts',(-24.5251215807483,14.5109849191037,
129.810302884381)) ;
#123844 = CARTESIAN_POINT('Ctrl Pts',(-24.4413268590606,14.4763368013962,
129.532269637636)) ;
#123845 = CARTESIAN_POINT('Ctrl Pts',(-24.364295503168,14.3664425306899,129.274177702535)) ;
#123846 = CARTESIAN_POINT('Ctrl Pts',(-24.2995399933717,14.188260258707,129.051786368571)) ;
#123847 = CARTESIAN_POINT('Ctrl Pts',(-24.253049988188,13.9563928722856,128.882950063364)) ;
#123848 = CARTESIAN_POINT('Ctrl Pts',(-24.2283801196271,13.6856074997971,
128.77773581213)) ;
#123849 = CARTESIAN_POINT('Ctrl Pts',(-24.2281882394076,13.3967977975017,
128.744126623715)) ;
#123850 = CARTESIAN_POINT('Ctrl Pts',(-24.2533268914288,13.1083771825577,
128.784333743028)) ;
#123851 = CARTESIAN_POINT('Ctrl Pts',(-24.3025480715288,12.8436200801875,
128.895028676077)) ;
#123852 = CARTESIAN_POINT('Ctrl Pts',(-24.373340176417,12.6197329194616,129.068631449711)) ;
#123853 = CARTESIAN_POINT('Ctrl Pts',(-24.4608094763246,12.4541609796659,
129.291101417274)) ;
#123854 = CARTESIAN_POINT('Ctrl Pts',(-24.5602240039795,12.357518085621,129.548297185279)) ;
#123855 = CARTESIAN_POINT('Ctrl Pts',(-24.6639285825146,12.3374075405641,
129.818292847781)) ;
#123856 = CARTESIAN_POINT('Ctrl Pts',(-24.7667954318842,12.3950240901617,
130.085577579692)) ;
#123857 = CARTESIAN_POINT('Ctrl Pts',(-24.8608236287849,12.5255975503683,
130.327260647649)) ;
#123858 = CARTESIAN_POINT('Ctrl Pts',(-24.9413203502761,12.7221237769604,
130.529099363759)) ;
#123859 = CARTESIAN_POINT('Ctrl Pts',(-25.0018011512601,12.9666439794892,
130.672820785154)) ;
#123860 = CARTESIAN_POINT('Ctrl Pts',(-25.0398820518506,13.2467844847395,
130.750722329137)) ;
#123861 = CARTESIAN_POINT('Ctrl Pts',(-25.0526700185416,13.5364086840901,
130.75512517665)) ;
#123862 = CARTESIAN_POINT('Ctrl Pts',(-25.0405775899547,13.8193015445878,
130.686678315808)) ;
#123863 = CARTESIAN_POINT('Ctrl Pts',(-25.0049851130658,14.0737432295645,
130.549605084074)) ;
#123864 = CARTESIAN_POINT('Ctrl Pts',(-24.9488992260672,14.28233845815,130.352522488622)) ;
#123865 = CARTESIAN_POINT('Ctrl Pts',(-24.8777495315051,14.428082061538,130.111665614575)) ;
#123866 = CARTESIAN_POINT('Ctrl Pts',(-24.7968113224133,14.5027907453993,
129.842125577233)) ;
#123867 = CARTESIAN_POINT('Ctrl Pts',(-24.712133705096,14.4996008871204,129.561426321041)) ;
#123868 = CARTESIAN_POINT('Ctrl Pts',(-24.6321001925199,14.419843429899,129.29470250768)) ;
#123869 = CARTESIAN_POINT('Ctrl Pts',(-24.561546919159,14.2682254316152,129.055404210481)) ;
#123870 = CARTESIAN_POINT('Ctrl Pts',(-24.5071324236837,14.0566690769085,
128.863388893838)) ;
#123871 = CARTESIAN_POINT('Ctrl Pts',(-24.4730352300617,13.7984045254372,
128.730536223149)) ;
#123872 = CARTESIAN_POINT('Ctrl Pts',(-24.462811119128,13.5146253545805,128.667609596018)) ;
#123873 = CARTESIAN_POINT('Ctrl Pts',(-24.4776804248282,13.223790028339,128.677916277619)) ;
#123874 = CARTESIAN_POINT('Ctrl Pts',(-24.5172399081723,12.9476428894619,
128.760415328231)) ;
#123875 = CARTESIAN_POINT('Ctrl Pts',(-24.5799331508047,12.7041857857084,
128.9102832082)) ;
#123876 = CARTESIAN_POINT('Ctrl Pts',(-24.6608098075135,12.5142907834555,
129.113613331222)) ;
#123877 = CARTESIAN_POINT('Ctrl Pts',(-24.7563003807409,12.3877724095918,
129.359323075658)) ;
#123878 = CARTESIAN_POINT('Ctrl Pts',(-24.8593314709221,12.336191203021,129.627164443025)) ;
#123879 = CARTESIAN_POINT('Ctrl Pts',(-24.9633392047127,12.3624798343251,
129.897889938277)) ;
#123880 = CARTESIAN_POINT('Ctrl Pts',(-25.0615038639838,12.4640688198504,
130.151643847771)) ;
#123881 = CARTESIAN_POINT('Ctrl Pts',(-25.1484909257269,12.6358046378966,
130.372452643299)) ;
#123882 = CARTESIAN_POINT('Ctrl Pts',(-25.2172355488953,12.8620488663086,
130.54031108306)) ;
#123883 = CARTESIAN_POINT('Ctrl Pts',(-25.264871833393,13.1294243702491,130.646328078678)) ;
#123884 = CARTESIAN_POINT('Ctrl Pts',(-25.2880788707182,13.4191275485285,
130.68085061096)) ;
#123885 = CARTESIAN_POINT('Ctrl Pts',(-25.2860495181123,13.7060585191979,
130.642009964889)) ;
#123886 = CARTESIAN_POINT('Ctrl Pts',(-25.259565164561,13.9758635048128,130.531352932413)) ;
#123887 = CARTESIAN_POINT('Ctrl Pts',(-25.2113485262632,14.2044690848735,
130.357391673997)) ;
#123888 = CARTESIAN_POINT('Ctrl Pts',(-25.145657524814,14.3772046545246,130.132389371412)) ;
#123889 = CARTESIAN_POINT('Ctrl Pts',(-25.0678187426741,14.4817041714967,
129.871892743955)) ;
#123890 = CARTESIAN_POINT('Ctrl Pts',(-24.9841332217802,14.5103977603672,
129.594305292428)) ;
#123891 = CARTESIAN_POINT('Ctrl Pts',(-24.9014475126332,14.4613877005576,
129.319684050441)) ;
#123892 = CARTESIAN_POINT('Ctrl Pts',(-24.8261139461188,14.3378670133984,
129.066461861856)) ;
#123893 = CARTESIAN_POINT('Ctrl Pts',(-24.7645055171052,14.1487648805611,
128.853351786338)) ;
#123894 = CARTESIAN_POINT('Ctrl Pts',(-24.7217158233187,13.9077123498208,
128.695220753593)) ;
#123895 = CARTESIAN_POINT('Ctrl Pts',(-24.70153541607,13.6318347847728,128.603127426418)) ;
#123896 = CARTESIAN_POINT('Ctrl Pts',(-24.7061472404895,13.3411960486728,
128.583480186491)) ;
#123897 = CARTESIAN_POINT('Ctrl Pts',(-24.7359035401613,13.0563345512955,
128.637281218857)) ;
#123898 = CARTESIAN_POINT('Ctrl Pts',(-24.7895403296563,12.7976620834808,
128.760811148666)) ;
#123899 = CARTESIAN_POINT('Ctrl Pts',(-24.8633359396006,12.5846251876044,
128.94341366769)) ;
#123900 = CARTESIAN_POINT('Ctrl Pts',(-24.9543879402352,12.429833205716,129.17599010507)) ;
#123901 = CARTESIAN_POINT('Ctrl Pts',(-25.0540797760828,12.3481748441672,
129.434397942324)) ;
#123902 = CARTESIAN_POINT('Ctrl Pts',(-25.1589469114049,12.3422836443017,
129.707474708614)) ;
#123903 = CARTESIAN_POINT('Ctrl Pts',(-25.2603506516879,12.4141623973689,
129.970624791442)) ;
#123904 = CARTESIAN_POINT('Ctrl Pts',(-25.3525979224572,12.5584918127645,
130.206923087342)) ;
#123905 = CARTESIAN_POINT('Ctrl Pts',(-25.4292776741146,12.7644626666543,
130.39783234548)) ;
#123906 = CARTESIAN_POINT('Ctrl Pts',(-25.4859302720378,13.0174117066364,
130.530239879527)) ;
#123907 = CARTESIAN_POINT('Ctrl Pts',(-25.5192334320429,13.2998966428893,
130.594380331104)) ;
#123908 = CARTESIAN_POINT('Ctrl Pts',(-25.52743704701,13.5908801629709,130.585237694254)) ;
#123909 = CARTESIAN_POINT('Ctrl Pts',(-25.5106586822041,13.8706961833489,
130.503017637028)) ;
#123910 = CARTESIAN_POINT('Ctrl Pts',(-25.4707228131626,14.1180204039502,
130.353167605114)) ;
#123911 = CARTESIAN_POINT('Ctrl Pts',(-25.4117996734716,14.3143766861394,
130.14807480119)) ;
#123912 = CARTESIAN_POINT('Ctrl Pts',(-25.33799703275,14.4481661316014,129.899283579083)) ;
#123913 = CARTESIAN_POINT('Ctrl Pts',(-25.256130538496,14.508083869743,129.627114688912)) ;
#123914 = CARTESIAN_POINT('Ctrl Pts',(-25.171950397789,14.490551827571,129.347998386774)) ;
#123915 = CARTESIAN_POINT('Ctrl Pts',(-25.0928509136473,14.3964091806781,
129.083806315848)) ;
#123916 = CARTESIAN_POINT('Ctrl Pts',(-25.0249827301023,14.2323049271919,
128.852381341929)) ;
#123917 = CARTESIAN_POINT('Ctrl Pts',(-24.9741907545614,14.0113006230555,
128.67099775518)) ;
#123918 = CARTESIAN_POINT('Ctrl Pts',(-24.9443961472462,13.7469852751569,
128.550772683403)) ;
#123919 = CARTESIAN_POINT('Ctrl Pts',(-24.9387279867118,13.4601450927403,
128.5011244625)) ;
#123920 = CARTESIAN_POINT('Ctrl Pts',(-24.9585569147683,13.1687002988962,
128.525718513046)) ;
#123921 = CARTESIAN_POINT('Ctrl Pts',(-25.0024370229123,12.8989650808956,
128.621013115827)) ;
#123922 = CARTESIAN_POINT('Ctrl Pts',(-25.0691511475481,12.6635916502146,
128.782564629959)) ;
#123923 = CARTESIAN_POINT('Ctrl Pts',(-25.1528982004687,12.4852398029377,
128.994341478292)) ;
#123924 = CARTESIAN_POINT('Ctrl Pts',(-25.2508294675198,12.371925952002,129.247023302253)) ;
#123925 = CARTESIAN_POINT('Ctrl Pts',(-25.3538720853292,12.3351771027553,
129.515132724498)) ;
#123926 = CARTESIAN_POINT('Ctrl Pts',(-25.4579330532035,12.3762351051066,
129.785816630675)) ;
#123927 = CARTESIAN_POINT('Ctrl Pts',(-25.5539034139904,12.4911992471527,
130.033297211774)) ;
#123928 = CARTESIAN_POINT('Ctrl Pts',(-25.6380661056327,12.6745749417996,
130.245838468086)) ;
#123929 = CARTESIAN_POINT('Ctrl Pts',(-25.7032387958614,12.9105841492293,
130.403148858585)) ;
#123930 = CARTESIAN_POINT('Ctrl Pts',(-25.7462934438778,13.1834575977754,
130.495797184592)) ;
#123931 = CARTESIAN_POINT('Ctrl Pts',(-25.7646883536981,13.472817267858,130.516488970866)) ;
#123932 = CARTESIAN_POINT('Ctrl Pts',(-25.7580233507089,13.7593252919433,
130.463899550352)) ;
#123933 = CARTESIAN_POINT('Ctrl Pts',(-25.7270360041595,14.0229112267302,
130.34008351448)) ;
#123934 = CARTESIAN_POINT('Ctrl Pts',(-25.675498907428,14.2409569319606,130.156613033591)) ;
#123935 = CARTESIAN_POINT('Ctrl Pts',(-25.6068834624728,14.4024703207306,
129.922947324608)) ;
#123936 = CARTESIAN_POINT('Ctrl Pts',(-25.5273592175764,14.4930253207348,
129.657498279644)) ;
#123937 = CARTESIAN_POINT('Ctrl Pts',(-25.4434689272461,14.5071137946879,
129.379370355167)) ;
#123938 = CARTESIAN_POINT('Ctrl Pts',(-25.3615278491778,14.4434721690138,
129.106846352464)) ;
#123939 = CARTESIAN_POINT('Ctrl Pts',(-25.2885360407668,14.3072990407348,
128.86057381183)) ;
#123940 = CARTESIAN_POINT('Ctrl Pts',(-25.2298270357142,14.1061280190249,
128.655755058378)) ;
#123941 = CARTESIAN_POINT('Ctrl Pts',(-25.1913201297001,13.8584456467317,
128.510325342625)) ;
#123942 = CARTESIAN_POINT('Ctrl Pts',(-25.1755647513378,13.5782525507237,
128.431150931071)) ;
#123943 = CARTESIAN_POINT('Ctrl Pts',(-25.1849885107696,13.2862403685174,
128.425460714649)) ;
#123944 = CARTESIAN_POINT('Ctrl Pts',(-25.2192755405819,13.0054671404376,
128.492579206751)) ;
#123945 = CARTESIAN_POINT('Ctrl Pts',(-25.2773394240981,12.7527976757228,
128.628896842881)) ;
#123946 = CARTESIAN_POINT('Ctrl Pts',(-25.3544373750974,12.5507720823643,
128.821226560556)) ;
#123947 = CARTESIAN_POINT('Ctrl Pts',(-25.4472393440595,12.4092692851511,
129.059132005569)) ;
#123948 = CARTESIAN_POINT('Ctrl Pts',(-25.5489779403507,12.3409405879061,
129.323242391553)) ;
#123949 = CARTESIAN_POINT('Ctrl Pts',(-25.6535733607532,12.3499819514293,
129.595610275213)) ;
#123950 = CARTESIAN_POINT('Ctrl Pts',(-25.7539733542539,12.4363532900494,
129.855724418261)) ;
#123951 = CARTESIAN_POINT('Ctrl Pts',(-25.8432653409665,12.592566468637,130.083565255521)) ;
#123952 = CARTESIAN_POINT('Ctrl Pts',(-25.9166293802248,12.808517161013,130.264767590827)) ;
#123953 = CARTESIAN_POINT('Ctrl Pts',(-25.9692694104626,13.0694867381501,
130.385320946943)) ;
#123954 = CARTESIAN_POINT('Ctrl Pts',(-25.9978655735776,13.3550372325075,
130.435738703826)) ;
#123955 = CARTESIAN_POINT('Ctrl Pts',(-26.0012228110646,13.6462143914832,
130.41233473643)) ;
#123956 = CARTESIAN_POINT('Ctrl Pts',(-25.9799786820042,13.9195288326514,
130.317292866585)) ;
#123957 = CARTESIAN_POINT('Ctrl Pts',(-25.9362831066957,14.1586151342569,
130.156518689827)) ;
#123958 = CARTESIAN_POINT('Ctrl Pts',(-25.873895400124,14.3449690064031,129.941121871803)) ;
#123959 = CARTESIAN_POINT('Ctrl Pts',(-25.798230728825,14.4652397459023,129.686991964219)) ;
#123960 = CARTESIAN_POINT('Ctrl Pts',(-25.7149306992069,14.5107689860091,
129.410403584569)) ;
#123961 = CARTESIAN_POINT('Ctrl Pts',(-25.6318516915594,14.4787461953136,
129.134788811335)) ;
#123962 = CARTESIAN_POINT('Ctrl Pts',(-25.5538394007471,14.3700644333909,
128.873522851825)) ;
#123963 = CARTESIAN_POINT('Ctrl Pts',(-25.4891252246343,14.1946408209154,
128.651483185167)) ;
#123964 = CARTESIAN_POINT('Ctrl Pts',(-25.4419035532708,13.9639077381356,
128.480442817708)) ;
#123965 = CARTESIAN_POINT('Ctrl Pts',(-25.416526533386,13.6940409342519,128.373177036019)) ;
#123966 = CARTESIAN_POINT('Ctrl Pts',(-25.4156877261185,13.4043243870117,
128.337540729079)) ;
#123967 = CARTESIAN_POINT('Ctrl Pts',(-25.4398971208575,13.1175424203496,
128.375270653993)) ;
#123968 = CARTESIAN_POINT('Ctrl Pts',(-25.4887349254359,12.8501253800453,
128.484627505498)) ;
#123969 = CARTESIAN_POINT('Ctrl Pts',(-25.5586262014652,12.6260375072132,
128.655777801442)) ;
#123970 = CARTESIAN_POINT('Ctrl Pts',(-25.6457761900823,12.4581544955602,
128.877254650212)) ;
#123971 = CARTESIAN_POINT('Ctrl Pts',(-25.7447128579694,12.3594525317711,
129.13313074971)) ;
#123972 = CARTESIAN_POINT('Ctrl Pts',(-25.8487073343646,12.3367944106136,
129.403860832314)) ;
#123973 = CARTESIAN_POINT('Ctrl Pts',(-25.9519835342391,12.3925085766977,
129.672255974499)) ;
#123974 = CARTESIAN_POINT('Ctrl Pts',(-26.0462967491219,12.5213899475148,
129.914765311702)) ;
#123975 = CARTESIAN_POINT('Ctrl Pts',(-26.1270148304609,12.715572513745,130.117365292637)) ;
#123976 = CARTESIAN_POINT('Ctrl Pts',(-26.1882034971608,12.9595222132268,
130.263073734265)) ;
#123977 = CARTESIAN_POINT('Ctrl Pts',(-26.2267435953605,13.2367790657483,
130.342576650586)) ;
#123978 = CARTESIAN_POINT('Ctrl Pts',(-26.2404887282104,13.5277645483974,
130.34960696324)) ;
#123979 = CARTESIAN_POINT('Ctrl Pts',(-26.2290166843068,13.8120455612361,
130.282873037212)) ;
#123980 = CARTESIAN_POINT('Ctrl Pts',(-26.1939550681954,14.0676656402339,
130.147320284264)) ;
#123981 = CARTESIAN_POINT('Ctrl Pts',(-26.1385064231525,14.2771421243593,
129.952187707759)) ;
#123982 = CARTESIAN_POINT('Ctrl Pts',(-26.0677264199933,14.4250319650245,
129.712403604366)) ;
#123983 = CARTESIAN_POINT('Ctrl Pts',(-25.9866105764485,14.5017260343279,
129.442204203795)) ;
#123984 = CARTESIAN_POINT('Ctrl Pts',(-25.9029004553032,14.5010098763796,
129.164720483973)) ;
#123985 = CARTESIAN_POINT('Ctrl Pts',(-25.8219478737643,14.4231232861786,
128.895020725302)) ;
#123986 = CARTESIAN_POINT('Ctrl Pts',(-25.7512036699718,14.2735699420865,
128.655246017135)) ;
#123987 = CARTESIAN_POINT('Ctrl Pts',(-25.6961574433566,14.0631259217895,
128.461311286501)) ;
#123988 = CARTESIAN_POINT('Ctrl Pts',(-25.6615347817568,13.8068511447586,
128.327046916864)) ;
#123989 = CARTESIAN_POINT('Ctrl Pts',(-25.6505331648762,13.5229066982492,
128.261764796241)) ;
#123990 = CARTESIAN_POINT('Ctrl Pts',(-25.6646712038547,13.2323183656793,
128.269978142886)) ;
#123991 = CARTESIAN_POINT('Ctrl Pts',(-25.7035121417102,12.9554622848227,
128.35037611329)) ;
#123992 = CARTESIAN_POINT('Ctrl Pts',(-25.7655162081559,12.7108336294588,
128.498254383038)) ;
#123993 = CARTESIAN_POINT('Ctrl Pts',(-25.846073101608,12.5189036240624,128.700584553235)) ;
#123994 = CARTESIAN_POINT('Ctrl Pts',(-25.9409316376887,12.390658589764,128.944555230365)) ;
#123995 = CARTESIAN_POINT('Ctrl Pts',(-26.0439737290693,12.3366531307129,
129.212373718036)) ;
#123996 = CARTESIAN_POINT('Ctrl Pts',(-26.1478846663642,12.3602977893096,
129.482879326308)) ;
#123997 = CARTESIAN_POINT('Ctrl Pts',(-26.2471522651563,12.4609988755096,
129.739549452939)) ;
#123998 = CARTESIAN_POINT('Ctrl Pts',(-26.3336049302479,12.6291274896935,
129.959164506964)) ;
#123999 = CARTESIAN_POINT('Ctrl Pts',(-26.403541070526,12.8555169939373,130.130239113931)) ;
#124000 = CARTESIAN_POINT('Ctrl Pts',(-26.4515909872396,13.1215885619852,
130.237543390251)) ;
#124001 = CARTESIAN_POINT('Ctrl Pts',(-26.4755139644934,13.4096083947618,
130.274304939758)) ;
#124002 = CARTESIAN_POINT('Ctrl Pts',(-26.4742683561914,13.6982129377788,
130.237599168761)) ;
#124003 = CARTESIAN_POINT('Ctrl Pts',(-26.4483350169052,13.969145223664,130.128507626156)) ;
#124004 = CARTESIAN_POINT('Ctrl Pts',(-26.4008409219027,14.1982918384811,
129.956770249216)) ;
#124005 = CARTESIAN_POINT('Ctrl Pts',(-26.3357094157164,14.3728095638234,
129.733441982711)) ;
#124006 = CARTESIAN_POINT('Ctrl Pts',(-26.2580598390402,14.4796622896265,
129.47345820633)) ;
#124007 = CARTESIAN_POINT('Ctrl Pts',(-26.1743828769687,14.5107460885462,
129.195872130029)) ;
#124008 = CARTESIAN_POINT('Ctrl Pts',(-26.091350817327,14.4636147877097,128.920140958459)) ;
#124009 = CARTESIAN_POINT('Ctrl Pts',(-26.0160489320887,14.3427084446703,
128.667164147215)) ;
#124010 = CARTESIAN_POINT('Ctrl Pts',(-25.9536601172443,14.1545213571348,
128.451617980833)) ;
#124011 = CARTESIAN_POINT('Ctrl Pts',(-25.9103939029223,13.9146657038493,
128.292116078991)) ;
#124012 = CARTESIAN_POINT('Ctrl Pts',(-25.8895873786261,13.6405171669677,
128.198310769231)) ;
#124013 = CARTESIAN_POINT('Ctrl Pts',(-25.8934300722509,13.3501101589506,
128.176423228012)) ;
#124014 = CARTESIAN_POINT('Ctrl Pts',(-25.9223270326843,13.0651841999784,
128.227769457602)) ;
#124015 = CARTESIAN_POINT('Ctrl Pts',(-25.9756051647074,12.8038875928186,
128.350055164985)) ;
#124016 = CARTESIAN_POINT('Ctrl Pts',(-26.0488715170654,12.5899464176031,
128.531156076502)) ;
#124017 = CARTESIAN_POINT('Ctrl Pts',(-26.1388470008162,12.4339562439877,
128.760815215957)) ;
#124018 = CARTESIAN_POINT('Ctrl Pts',(-26.2391546987785,12.3491846670138,
129.020742228805)) ;
#124019 = CARTESIAN_POINT('Ctrl Pts',(-26.3440686577084,12.3415474496416,
129.293939952554)) ;
#124020 = CARTESIAN_POINT('Ctrl Pts',(-26.4452555059315,12.4110292965116,
129.556580973751)) ;
#124021 = CARTESIAN_POINT('Ctrl Pts',(-26.5378931940764,12.5533606733183,
129.794011949483)) ;
#124022 = CARTESIAN_POINT('Ctrl Pts',(-26.615000146917,12.7574393223527,129.986210703798)) ;
#124023 = CARTESIAN_POINT('Ctrl Pts',(-26.6724404028421,13.009581913367,130.120867414048)) ;
#124024 = CARTESIAN_POINT('Ctrl Pts',(-26.7064847425196,13.2928228925075,
130.187026380122)) ;
#124025 = CARTESIAN_POINT('Ctrl Pts',(-26.7153278695728,13.582012204951,130.179963532695)) ;
#124026 = CARTESIAN_POINT('Ctrl Pts',(-26.699241537175,13.8633231100431,130.099661124816)) ;
#124027 = CARTESIAN_POINT('Ctrl Pts',(-26.6600020906481,14.1112604273849,
129.951925919837)) ;
#124028 = CARTESIAN_POINT('Ctrl Pts',(-26.60148356948,14.3095522815314,129.747958126555)) ;
#124029 = CARTESIAN_POINT('Ctrl Pts',(-26.5282846692839,14.44510578155,129.501042571553)) ;
#124030 = CARTESIAN_POINT('Ctrl Pts',(-26.4458923835004,14.5076745879146,
129.227062356217)) ;
#124031 = CARTESIAN_POINT('Ctrl Pts',(-26.3618964181972,14.4918702238892,
128.94857384037)) ;
#124032 = CARTESIAN_POINT('Ctrl Pts',(-26.2828570043338,14.4001695332023,
128.68467078182)) ;
#124033 = CARTESIAN_POINT('Ctrl Pts',(-26.2146127566021,14.2383391968108,
128.452190174529)) ;
#124034 = CARTESIAN_POINT('Ctrl Pts',(-26.1630788147266,14.0178456765348,
128.268499220438)) ;
#124035 = CARTESIAN_POINT('Ctrl Pts',(-26.132665228877,13.7549023993413,128.146527433501)) ;
#124036 = CARTESIAN_POINT('Ctrl Pts',(-26.1264250234098,13.4669383110673,
128.095031448519)) ;
#124037 = CARTESIAN_POINT('Ctrl Pts',(-26.1451597576439,13.179287796842,128.116902786845)) ;
#124038 = CARTESIAN_POINT('Ctrl Pts',(-26.1887921440493,12.9054935054356,
128.21107289621)) ;
#124039 = CARTESIAN_POINT('Ctrl Pts',(-26.2543181709187,12.6708451736549,
128.369465417359)) ;
#124040 = CARTESIAN_POINT('Ctrl Pts',(-26.3383737496348,12.489010935019,128.581822970063)) ;
#124041 = CARTESIAN_POINT('Ctrl Pts',(-26.4349845939226,12.3747427452421,
128.831010816488)) ;
#124042 = CARTESIAN_POINT('Ctrl Pts',(-26.5386809419236,12.3351181280502,
129.100771617171)) ;
#124043 = CARTESIAN_POINT('Ctrl Pts',(-26.6423270739193,12.3735357239234,
129.370425059392)) ;
#124044 = CARTESIAN_POINT('Ctrl Pts',(-26.739590487989,12.4876827047378,129.621327059493)) ;
#124045 = CARTESIAN_POINT('Ctrl Pts',(-26.8234966069003,12.6681438766094,
129.833383660537)) ;
#124046 = CARTESIAN_POINT('Ctrl Pts',(-26.8894910230064,12.9033828008646,
129.992992511596)) ;
#124047 = CARTESIAN_POINT('Ctrl Pts',(-26.9330590975584,13.1743601977476,
130.087278715581)) ;
#124048 = CARTESIAN_POINT('Ctrl Pts',(-26.95234321523,13.4644840524054,130.110453366062)) ;
#124049 = CARTESIAN_POINT('Ctrl Pts',(-26.9462750235192,13.7518156372007,
130.059550094245)) ;
#124050 = CARTESIAN_POINT('Ctrl Pts',(-26.9162087617747,14.0147481121993,
129.938641619233)) ;
#124051 = CARTESIAN_POINT('Ctrl Pts',(-26.8649460510337,14.2359323146828,
129.755751034222)) ;
#124052 = CARTESIAN_POINT('Ctrl Pts',(-26.7965801586489,14.3990328961567,
129.52278375049)) ;
#124053 = CARTESIAN_POINT('Ctrl Pts',(-26.7177443738962,14.4913721477539,
129.259533927694)) ;
#124054 = CARTESIAN_POINT('Ctrl Pts',(-26.6334108075472,14.5077030506771,
128.979913126939)) ;
#124055 = CARTESIAN_POINT('Ctrl Pts',(-26.5517638677785,14.4466726392651,
128.70844483765)) ;
#124056 = CARTESIAN_POINT('Ctrl Pts',(-26.4778064684304,14.3110619945875,
128.459041808409)) ;
#124057 = CARTESIAN_POINT('Ctrl Pts',(-26.4192231879076,14.1132679223134,
128.25491902626)) ;
#124058 = CARTESIAN_POINT('Ctrl Pts',(-26.3797981720978,13.8656263142686,
128.106626377481)) ;
#124059 = CARTESIAN_POINT('Ctrl Pts',(-26.3634473247229,13.5853315264496,
128.025647675686)) ;
#124060 = CARTESIAN_POINT('Ctrl Pts',(-26.3722199816823,13.2939510978671,
128.018122216624)) ;
#124061 = CARTESIAN_POINT('Ctrl Pts',(-26.405714171083,13.0136079092844,128.083036282935)) ;
#124062 = CARTESIAN_POINT('Ctrl Pts',(-26.4628659654867,12.7604082845335,
128.216792359251)) ;
#124063 = CARTESIAN_POINT('Ctrl Pts',(-26.5397813309025,12.5556139237626,
128.408426975407)) ;
#124064 = CARTESIAN_POINT('Ctrl Pts',(-26.6324107937376,12.4121627059908,
128.645779498262)) ;
#124065 = CARTESIAN_POINT('Ctrl Pts',(-26.7336873599695,12.3419224610127,
128.908634855302)) ;
#124066 = CARTESIAN_POINT('Ctrl Pts',(-26.8381886857235,12.3485705952627,
129.180762238741)) ;
#124067 = CARTESIAN_POINT('Ctrl Pts',(-26.9387702278677,12.4325162963297,
129.441425792212)) ;
#124068 = CARTESIAN_POINT('Ctrl Pts',(-27.0287520463112,12.5872707160174,
129.671176207014)) ;
#124069 = CARTESIAN_POINT('Ctrl Pts',(-27.1025641524698,12.8016743120911,
129.853709459553)) ;
#124070 = CARTESIAN_POINT('Ctrl Pts',(-27.1557706951775,13.0608928169866,
129.97600170914)) ;
#124071 = CARTESIAN_POINT('Ctrl Pts',(-27.1851489147898,13.3463628711479,
130.02865621953)) ;
#124072 = CARTESIAN_POINT('Ctrl Pts',(-27.189300141959,13.6367414871714,130.007684109365)) ;
#124073 = CARTESIAN_POINT('Ctrl Pts',(-27.1687387851865,13.9121235287477,
129.914488218401)) ;
#124074 = CARTESIAN_POINT('Ctrl Pts',(-27.1254953280649,14.1528033818472,
129.754974456862)) ;
#124075 = CARTESIAN_POINT('Ctrl Pts',(-27.0637389687625,14.3402810469184,
129.541515996158)) ;
#124076 = CARTESIAN_POINT('Ctrl Pts',(-26.9884856177373,14.4626257228514,
129.288621690848)) ;
#124077 = CARTESIAN_POINT('Ctrl Pts',(-26.9051827015451,14.5106364095724,
129.011977483569)) ;
#124078 = CARTESIAN_POINT('Ctrl Pts',(-26.8218668490788,14.4805445911802,
128.735600274415)) ;
#124079 = CARTESIAN_POINT('Ctrl Pts',(-26.7440463514374,14.3748126734896,
128.475104392524)) ;
#124080 = CARTESIAN_POINT('Ctrl Pts',(-26.6785355196267,14.2005693780012,
128.250575368186)) ;
#124081 = CARTESIAN_POINT('Ctrl Pts',(-26.630780882824,13.9714225005758,128.078016941159)) ;
#124082 = CARTESIAN_POINT('Ctrl Pts',(-26.6047039211808,13.7016038518799,
127.968605933267)) ;
#124083 = CARTESIAN_POINT('Ctrl Pts',(-26.6030915854038,13.4137877751622,
127.930902605108)) ;
#124084 = CARTESIAN_POINT('Ctrl Pts',(-26.6267380627707,13.1249621012608,
127.966780515293)) ;
#124085 = CARTESIAN_POINT('Ctrl Pts',(-26.6744609448017,12.8587597894488,
128.07316158682)) ;
#124086 = CARTESIAN_POINT('Ctrl Pts',(-26.7442975058962,12.6311848852698,
128.243869033046)) ;
#124087 = CARTESIAN_POINT('Ctrl Pts',(-26.830903329108,12.462061420416,128.463831733263)) ;
#124088 = CARTESIAN_POINT('Ctrl Pts',(-26.9296939602677,12.3611529098997,
128.719242246554)) ;
#124089 = CARTESIAN_POINT('Ctrl Pts',(-27.0333937390888,12.3364027391132,
128.989188260464)) ;
#124090 = CARTESIAN_POINT('Ctrl Pts',(-27.1368020606483,12.3896955050154,
129.2579744258)) ;
#124091 = CARTESIAN_POINT('Ctrl Pts',(-27.2316571620167,12.5169546340526,
129.501984988792)) ;
#124092 = CARTESIAN_POINT('Ctrl Pts',(-27.3126444315144,12.709001546384,129.705455771372)) ;
#124093 = CARTESIAN_POINT('Ctrl Pts',(-27.3745146596021,12.9518210421532,
129.853131534273)) ;
#124094 = CARTESIAN_POINT('Ctrl Pts',(-27.4137510170451,13.2283912816006,
129.934670418908)) ;
#124095 = CARTESIAN_POINT('Ctrl Pts',(-27.4282191216373,13.5192446194064,
129.943814180425)) ;
#124096 = CARTESIAN_POINT('Ctrl Pts',(-27.4175340945595,13.8035931145738,
129.879438970957)) ;
#124097 = CARTESIAN_POINT('Ctrl Pts',(-27.383044952722,14.0607676757129,129.745489590902)) ;
#124098 = CARTESIAN_POINT('Ctrl Pts',(-27.3284746860088,14.2709777793726,
129.553094789489)) ;
#124099 = CARTESIAN_POINT('Ctrl Pts',(-27.2575815807168,14.4220258992613,
129.312734052738)) ;
#124100 = CARTESIAN_POINT('Ctrl Pts',(-27.1769127132677,14.5004900232679,
129.043957183488)) ;
#124101 = CARTESIAN_POINT('Ctrl Pts',(-27.0930692805598,14.5020985489184,
128.766023699838)) ;
#124102 = CARTESIAN_POINT('Ctrl Pts',(-27.0121212643559,14.4266675394507,
128.49642621361)) ;
#124103 = CARTESIAN_POINT('Ctrl Pts',(-26.9407458153866,14.2786156866751,
128.254689867483)) ;
#124104 = CARTESIAN_POINT('Ctrl Pts',(-26.8852334771517,14.0697688504795,
128.059416629246)) ;
#124105 = CARTESIAN_POINT('Ctrl Pts',(-26.849975543147,13.8142974441725,127.923265218697)) ;
#124106 = CARTESIAN_POINT('Ctrl Pts',(-26.8382987967745,13.5318060155786,
127.856120671583)) ;
#124107 = CARTESIAN_POINT('Ctrl Pts',(-26.8516696284158,13.2403760089107,
127.862009333327)) ;
#124108 = CARTESIAN_POINT('Ctrl Pts',(-26.890089361851,12.9618560085294,127.941045133668)) ;
#124109 = CARTESIAN_POINT('Ctrl Pts',(-26.9512286696893,12.7173262571543,
128.086563315903)) ;
#124110 = CARTESIAN_POINT('Ctrl Pts',(-27.0314174703486,12.5233446116289,
128.28776106198)) ;
#124111 = CARTESIAN_POINT('Ctrl Pts',(-27.1260354307218,12.3931311939353,
128.531010608056)) ;
#124112 = CARTESIAN_POINT('Ctrl Pts',(-27.2291064958659,12.3370752417009,
128.79886449417)) ;
#124113 = CARTESIAN_POINT('Ctrl Pts',(-27.3326646670925,12.35867646463,129.068464529043)) ;
#124114 = CARTESIAN_POINT('Ctrl Pts',(-27.4317434817778,12.4563696655718,
129.324745138766)) ;
#124115 = CARTESIAN_POINT('Ctrl Pts',(-27.5191780495442,12.6234424548744,
129.547033430675)) ;
#124116 = CARTESIAN_POINT('Ctrl Pts',(-27.5896064413482,12.8484690633149,
129.719557189226)) ;
#124117 = CARTESIAN_POINT('Ctrl Pts',(-27.6383447085001,13.1134860837276,
129.828883494931)) ;
#124118 = CARTESIAN_POINT('Ctrl Pts',(-27.6630194526296,13.4024250602232,
129.867700766758)) ;
#124119 = CARTESIAN_POINT('Ctrl Pts',(-27.6623953842175,13.6901681965896,
129.832935013288)) ;
#124120 = CARTESIAN_POINT('Ctrl Pts',(-27.6372548988728,13.9614083334907,
129.726232762252)) ;
#124121 = CARTESIAN_POINT('Ctrl Pts',(-27.5902751351061,14.1924050626967,
129.55593800189)) ;
#124122 = CARTESIAN_POINT('Ctrl Pts',(-27.5255259120584,14.3688010138631,
129.333704515503)) ;
#124123 = CARTESIAN_POINT('Ctrl Pts',(-27.4481016761685,14.4776662108143,
129.074365641602)) ;
#124124 = CARTESIAN_POINT('Ctrl Pts',(-27.3647643666235,14.5108828487548,
128.797872509103)) ;
#124125 = CARTESIAN_POINT('Ctrl Pts',(-27.28160086979,14.4662997659133,128.521759647642)) ;
#124126 = CARTESIAN_POINT('Ctrl Pts',(-27.2057377958646,14.3468724175,128.26701996428)) ;
#124127 = CARTESIAN_POINT('Ctrl Pts',(-27.1432603861286,14.1616148952727,
128.051421722211)) ;
#124128 = CARTESIAN_POINT('Ctrl Pts',(-27.0991941479983,13.9230022148217,
127.889534238923)) ;
#124129 = CARTESIAN_POINT('Ctrl Pts',(-27.0776168898842,13.6485313215457,
127.793350195976)) ;
#124130 = CARTESIAN_POINT('Ctrl Pts',(-27.0807484826604,13.3583010704495,
127.76939083884)) ;
#124131 = CARTESIAN_POINT('Ctrl Pts',(-27.1090520806657,13.0725041550786,
127.818945431234)) ;
#124132 = CARTESIAN_POINT('Ctrl Pts',(-27.1613516583747,12.8117565584391,
127.938573083935)) ;
#124133 = CARTESIAN_POINT('Ctrl Pts',(-27.234133998536,12.5955170585835,128.118185428868)) ;
#124134 = CARTESIAN_POINT('Ctrl Pts',(-27.3242615124707,12.4369579838143,
128.348106217854)) ;
#124135 = CARTESIAN_POINT('Ctrl Pts',(-27.4239051442321,12.3507869319176,
128.606250511175)) ;
#124136 = CARTESIAN_POINT('Ctrl Pts',(-27.5283170847605,12.3404899824772,
128.878131255211)) ;
#124137 = CARTESIAN_POINT('Ctrl Pts',(-27.6301884886677,12.4078495192289,
129.142611995147)) ;
#124138 = CARTESIAN_POINT('Ctrl Pts',(-27.7232432838034,12.548387321603,129.381237810726)) ;
#124139 = CARTESIAN_POINT('Ctrl Pts',(-27.8009955997897,12.7513534766359,
129.575254101371)) ;
#124140 = CARTESIAN_POINT('Ctrl Pts',(-27.8588477984997,13.0019415175825,
129.711186382699)) ;
#124141 = CARTESIAN_POINT('Ctrl Pts',(-27.8935349743183,13.2828870424453,
129.779414110512)) ;
#124142 = CARTESIAN_POINT('Ctrl Pts',(-27.9032420933332,13.5743280761341,
129.774620556531)) ;
#124143 = CARTESIAN_POINT('Ctrl Pts',(-27.8877912603147,13.8554589732171,
129.696260558318)) ;
#124144 = CARTESIAN_POINT('Ctrl Pts',(-27.8494200240865,14.1037392604584,
129.551189336801)) ;
#124145 = CARTESIAN_POINT('Ctrl Pts',(-27.7912574236898,14.3046991320609,
129.348138971575)) ;
#124146 = CARTESIAN_POINT('Ctrl Pts',(-27.7180698943492,14.4424189349425,
129.101130494134)) ;
#124147 = CARTESIAN_POINT('Ctrl Pts',(-27.6365275795886,14.5067209378496,
128.829911927971)) ;
#124148 = CARTESIAN_POINT('Ctrl Pts',(-27.5522869891486,14.4936392386325,
128.550624236163)) ;
#124149 = CARTESIAN_POINT('Ctrl Pts',(-27.472842461916,14.4040066761143,128.285476965489)) ;
#124150 = CARTESIAN_POINT('Ctrl Pts',(-27.4040161809218,14.2433941808528,
128.051188349872)) ;
#124151 = CARTESIAN_POINT('Ctrl Pts',(-27.3521479099506,14.0252992108477,
127.866664237617)) ;
#124152 = CARTESIAN_POINT('Ctrl Pts',(-27.321003828356,13.7626962224851,127.742470842385)) ;
#124153 = CARTESIAN_POINT('Ctrl Pts',(-27.3140081793116,13.4766512855246,
127.688944617931)) ;
#124154 = CARTESIAN_POINT('Ctrl Pts',(-27.3320904586992,13.186696570853,127.708668192988)) ;
#124155 = CARTESIAN_POINT('Ctrl Pts',(-27.3751478872209,12.9123106604455,
127.801171448176)) ;
#124156 = CARTESIAN_POINT('Ctrl Pts',(-27.4399784096183,12.676940859845,127.957598680988)) ;
#124157 = CARTESIAN_POINT('Ctrl Pts',(-27.5233472974592,12.4935889461196,
128.168026659701)) ;
#124158 = CARTESIAN_POINT('Ctrl Pts',(-27.6201918302586,12.3766908564608,
128.417719170936)) ;
#124159 = CARTESIAN_POINT('Ctrl Pts',(-27.7235786308746,12.3352383867213,
128.686650110514)) ;
#124160 = CARTESIAN_POINT('Ctrl Pts',(-27.8270763638829,12.3713735993149,
128.955940427189)) ;
#124161 = CARTESIAN_POINT('Ctrl Pts',(-27.9243939471655,12.482759025907,129.207099816065)) ;
#124162 = CARTESIAN_POINT('Ctrl Pts',(-28.0093322756141,12.6627224299211,
129.421938016894)) ;
#124163 = CARTESIAN_POINT('Ctrl Pts',(-28.0755419239468,12.8955397907263,
129.582345907045)) ;
#124164 = CARTESIAN_POINT('Ctrl Pts',(-28.119969509644,13.1663559129077,129.679051355865)) ;
#124165 = CARTESIAN_POINT('Ctrl Pts',(-28.139919232561,13.4563321375684,129.70416618866)) ;
#124166 = CARTESIAN_POINT('Ctrl Pts',(-28.1345989094075,13.7435418421396,
129.655505344651)) ;
#124167 = CARTESIAN_POINT('Ctrl Pts',(-28.1051508122028,14.0078637990346,
129.536350066241)) ;
#124168 = CARTESIAN_POINT('Ctrl Pts',(-28.0545171617177,14.2299792933114,
129.355360726874)) ;
#124169 = CARTESIAN_POINT('Ctrl Pts',(-27.9868221963933,14.3948659933446,
129.124446850834)) ;
#124170 = CARTESIAN_POINT('Ctrl Pts',(-27.9076947051592,14.489874104301,128.860121628846)) ;
#124171 = CARTESIAN_POINT('Ctrl Pts',(-27.8239321297246,14.5084149170405,
128.582385907377)) ;
#124172 = CARTESIAN_POINT('Ctrl Pts',(-27.7416214849835,14.4492458860129,
128.308762621808)) ;
#124173 = CARTESIAN_POINT('Ctrl Pts',(-27.6678598600451,14.3166093969371,
128.060178483998)) ;
#124174 = CARTESIAN_POINT('Ctrl Pts',(-27.6084375739192,14.1198899210566,
127.853454017954)) ;
#124175 = CARTESIAN_POINT('Ctrl Pts',(-27.5684481950325,13.8734077643859,
127.703525149204)) ;
#124176 = CARTESIAN_POINT('Ctrl Pts',(-27.551399761937,13.5947692208086,127.62061763421)) ;
#124177 = CARTESIAN_POINT('Ctrl Pts',(-27.5592798183032,13.3033323132003,
127.610476269779)) ;
#124178 = CARTESIAN_POINT('Ctrl Pts',(-27.5923075525496,13.0207082772212,
127.673820091286)) ;
#124179 = CARTESIAN_POINT('Ctrl Pts',(-27.6485757964368,12.7676285186634,
127.805155390212)) ;
#124180 = CARTESIAN_POINT('Ctrl Pts',(-27.7251843515254,12.5604750217273,
127.995784618736)) ;
#124181 = CARTESIAN_POINT('Ctrl Pts',(-27.8174211146232,12.4152915919243,
128.232013295708)) ;
#124182 = CARTESIAN_POINT('Ctrl Pts',(-27.9185391559007,12.3428120384338,
128.494396627763)) ;
#124183 = CARTESIAN_POINT('Ctrl Pts',(-28.023337038121,12.3473797731266,128.767302447243)) ;
#124184 = CARTESIAN_POINT('Ctrl Pts',(-28.1240157714969,12.4294696184163,
129.028273300787)) ;
#124185 = CARTESIAN_POINT('Ctrl Pts',(-28.2139942287922,12.5816149593444,
129.258157610135)) ;
#124186 = CARTESIAN_POINT('Ctrl Pts',(-28.2885971304493,12.7949908749712,
129.442905443656)) ;
#124187 = CARTESIAN_POINT('Ctrl Pts',(-28.3425258290396,13.0541013315914,
129.567209238913)) ;
#124188 = CARTESIAN_POINT('Ctrl Pts',(-28.3724481699799,13.3386275615382,
129.621515697744)) ;
#124189 = CARTESIAN_POINT('Ctrl Pts',(-28.3773117940733,13.6281886067776,
129.602732220181)) ;
#124190 = CARTESIAN_POINT('Ctrl Pts',(-28.3574855498393,13.9042250282851,
129.511693915976)) ;
#124191 = CARTESIAN_POINT('Ctrl Pts',(-28.3148907454231,14.1463904196779,
129.354066819802)) ;
#124192 = CARTESIAN_POINT('Ctrl Pts',(-28.253205086578,14.3364820143999,129.140624870235)) ;
#124193 = CARTESIAN_POINT('Ctrl Pts',(-28.1786223292026,14.4598817897301,
128.889868366299)) ;
#124194 = CARTESIAN_POINT('Ctrl Pts',(-28.095592031095,14.5104486172097,128.61407158427)) ;
#124195 = CARTESIAN_POINT('Ctrl Pts',(-28.0117388077113,14.4822486282368,
128.33593709542)) ;
#124196 = CARTESIAN_POINT('Ctrl Pts',(-27.9341428136596,14.3791732925603,
128.076300893861)) ;
#124197 = CARTESIAN_POINT('Ctrl Pts',(-27.867892600365,14.2063740239316,127.849490613762)) ;
#124198 = CARTESIAN_POINT('Ctrl Pts',(-27.8195738401177,13.977776586442,127.675203409093)) ;
#124199 = CARTESIAN_POINT('Ctrl Pts',(-27.7929572214305,13.7109259547803,
127.564468320854)) ;
#124200 = CARTESIAN_POINT('Ctrl Pts',(-27.7905925854493,13.4211174219504,
127.524298821139)) ;
#124201 = CARTESIAN_POINT('Ctrl Pts',(-27.8134496811496,13.1336909374666,
127.558070503479)) ;
#124202 = CARTESIAN_POINT('Ctrl Pts',(-27.8605400703067,12.8658812614538,
127.662521352308)) ;
#124203 = CARTESIAN_POINT('Ctrl Pts',(-27.9298825210266,12.6367690077997,
127.831765044912)) ;
#124204 = CARTESIAN_POINT('Ctrl Pts',(-28.0161685887183,12.4658337758404,
128.050762811657)) ;
#124205 = CARTESIAN_POINT('Ctrl Pts',(-28.1143654830391,12.363124510772,128.30455384214)) ;
#124206 = CARTESIAN_POINT('Ctrl Pts',(-28.2182189316931,12.3360466249849,
128.574875482197)) ;
#124207 = CARTESIAN_POINT('Ctrl Pts',(-28.3213869556432,12.3868688211213,
128.843082429485)) ;
#124208 = CARTESIAN_POINT('Ctrl Pts',(-28.4166731561539,12.5119418808478,
129.088323098358)) ;
#124209 = CARTESIAN_POINT('Ctrl Pts',(-28.4982051798402,12.7021784508198,
129.293379489094)) ;
#124210 = CARTESIAN_POINT('Ctrl Pts',(-28.5610042308682,12.9449354906641,
129.443606404056)) ;
#124211 = CARTESIAN_POINT('Ctrl Pts',(-28.6008426985914,13.2214385193801,
129.526846062899)) ;
#124212 = CARTESIAN_POINT('Ctrl Pts',(-28.6159465633725,13.5108149265418,
129.538005633189)) ;
#124213 = CARTESIAN_POINT('Ctrl Pts',(-28.6058800353516,13.7968085806489,
129.475293641202)) ;
#124214 = CARTESIAN_POINT('Ctrl Pts',(-28.5721530465612,14.0536577586376,
129.343741854781)) ;
#124215 = CARTESIAN_POINT('Ctrl Pts',(-28.5180253984698,14.2659121796834,
129.152568163917)) ;
#124216 = CARTESIAN_POINT('Ctrl Pts',(-28.4476164033553,14.4185013343906,
128.913682850671)) ;
#124217 = CARTESIAN_POINT('Ctrl Pts',(-28.3672606870272,14.4992712533562,
128.645857764565)) ;
#124218 = CARTESIAN_POINT('Ctrl Pts',(-28.2830619034491,14.5031359858994,
128.366746278371)) ;
#124219 = CARTESIAN_POINT('Ctrl Pts',(-28.2020479697154,14.42962012524,128.096991292358)) ;
#124220 = CARTESIAN_POINT('Ctrl Pts',(-28.1306108659269,14.2844129921914,
127.855234639704)) ;
#124221 = CARTESIAN_POINT('Ctrl Pts',(-28.0743399793536,14.07647539704,127.657620218949)) ;
#124222 = CARTESIAN_POINT('Ctrl Pts',(-28.038518814024,13.8227945386488,127.519914708429)) ;
#124223 = CARTESIAN_POINT('Ctrl Pts',(-28.0260544093946,13.5398700971536,
127.450350848859)) ;
#124224 = CARTESIAN_POINT('Ctrl Pts',(-28.0387376470672,13.2487715870731,
127.454277173227)) ;
#124225 = CARTESIAN_POINT('Ctrl Pts',(-28.0762887916964,12.9703360488667,
127.530869359068)) ;
#124226 = CARTESIAN_POINT('Ctrl Pts',(-28.1368163621099,12.724109148074,127.674556172722)) ;
#124227 = CARTESIAN_POINT('Ctrl Pts',(-28.2167305097807,12.5279170556122,
127.874864580102)) ;
#124228 = CARTESIAN_POINT('Ctrl Pts',(-28.3109689538554,12.3959938215062,
128.117030677241)) ;
#124229 = CARTESIAN_POINT('Ctrl Pts',(-28.4134273221919,12.3376260911869,
128.383241476252)) ;
#124230 = CARTESIAN_POINT('Ctrl Pts',(-28.5177715853634,12.3570498023057,
128.65490265925)) ;
#124231 = CARTESIAN_POINT('Ctrl Pts',(-28.616753088127,12.4525560159372,128.911007152944)) ;
#124232 = CARTESIAN_POINT('Ctrl Pts',(-28.7045988631486,12.6176036615847,
129.134503535126)) ;
#124233 = CARTESIAN_POINT('Ctrl Pts',(-28.7756048272567,12.841094749517,129.308722571836)) ;
#124234 = CARTESIAN_POINT('Ctrl Pts',(-28.8250390574099,13.1055203905307,
129.420039183832)) ;
#124235 = CARTESIAN_POINT('Ctrl Pts',(-28.8504133952678,13.3928980582864,
129.461039192628)) ;
#124236 = CARTESIAN_POINT('Ctrl Pts',(-28.8505343656059,13.682454377304,129.428266482564)) ;
#124237 = CARTESIAN_POINT('Ctrl Pts',(-28.826180486495,13.953269278216,129.324020975927)) ;
#124238 = CARTESIAN_POINT('Ctrl Pts',(-28.779745106423,14.1862511207232,129.155240175136)) ;
#124239 = CARTESIAN_POINT('Ctrl Pts',(-28.7155326099511,14.3643962047435,
128.934612491699)) ;
#124240 = CARTESIAN_POINT('Ctrl Pts',(-28.6379231259812,14.4759024798905,
128.674537064384)) ;
#124241 = CARTESIAN_POINT('Ctrl Pts',(-28.5549498566636,14.5109062470025,
128.399225139776)) ;
#124242 = CARTESIAN_POINT('Ctrl Pts',(-28.4717526539607,14.4687351613561,
128.123044427645)) ;
#124243 = CARTESIAN_POINT('Ctrl Pts',(-28.395557559578,14.3512437869113,127.867313690745)) ;
#124244 = CARTESIAN_POINT('Ctrl Pts',(-28.3326545693278,14.1681343320696,
127.650520958287)) ;
#124245 = CARTESIAN_POINT('Ctrl Pts',(-28.2877790237795,13.9291093087556,
127.486048344275)) ;
#124246 = CARTESIAN_POINT('Ctrl Pts',(-28.265717377919,13.6572014758575,127.388679901215)) ;
#124247 = CARTESIAN_POINT('Ctrl Pts',(-28.2681157526834,13.3659145810937,
127.362431930975)) ;
#124248 = CARTESIAN_POINT('Ctrl Pts',(-28.2956553555426,13.0809590498869,
127.40989746564)) ;
#124249 = CARTESIAN_POINT('Ctrl Pts',(-28.3471963188551,12.8188858312814,
127.527295565738)) ;
#124250 = CARTESIAN_POINT('Ctrl Pts',(-28.4200761323168,12.5999509531083,
127.706953707642)) ;
#124251 = CARTESIAN_POINT('Ctrl Pts',(-28.5086819650502,12.441498416931,127.932849511783)) ;
#124252 = CARTESIAN_POINT('Ctrl Pts',(-28.6086670984304,12.3520342804443,
128.191780765644)) ;
#124253 = CARTESIAN_POINT('Ctrl Pts',(-28.7133402836128,12.339805477818,128.464339419248)) ;
#124254 = CARTESIAN_POINT('Ctrl Pts',(-28.8150120925492,12.404786593097,128.72835260752)) ;
#124255 = CARTESIAN_POINT('Ctrl Pts',(-28.9084344751011,12.543193504082,128.968052605152)) ;
#124256 = CARTESIAN_POINT('Ctrl Pts',(-28.9867401792367,12.7444967223723,
129.163680460267)) ;
#124257 = CARTESIAN_POINT('Ctrl Pts',(-29.0453267744929,12.9945027181083,
129.301684319518)) ;
#124258 = CARTESIAN_POINT('Ctrl Pts',(-29.0806918598349,13.2745331235142,
129.371935091382)) ;
#124259 = CARTESIAN_POINT('Ctrl Pts',(-29.0910577293678,13.5670628518901,
129.368934829634)) ;
#124260 = CARTESIAN_POINT('Ctrl Pts',(-29.076494701345,13.8462372757585,129.293480346358)) ;
#124261 = CARTESIAN_POINT('Ctrl Pts',(-29.0385132292895,14.0979242906841,
129.14926585312)) ;
#124262 = CARTESIAN_POINT('Ctrl Pts',(-28.9808663325831,14.299738463193,128.947793088852)) ;
#124263 = CARTESIAN_POINT('Ctrl Pts',(-28.9083068168729,14.4393312892027,
128.702723448988)) ;
#124264 = CARTESIAN_POINT('Ctrl Pts',(-28.8262915558581,14.5060643737482,
128.429867504545)) ;
#124265 = CARTESIAN_POINT('Ctrl Pts',(-28.7426422363419,14.4951758470579,
128.152560658863)) ;
#124266 = CARTESIAN_POINT('Ctrl Pts',(-28.6625995451793,14.4072622582047,
127.885495825799)) ;
#124267 = CARTESIAN_POINT('Ctrl Pts',(-28.5937320513035,14.2495038720977,
127.651282692144)) ;
#124268 = CARTESIAN_POINT('Ctrl Pts',(-28.5409096402226,14.0308220187667,
127.463666032205)) ;
#124269 = CARTESIAN_POINT('Ctrl Pts',(-28.5094830415525,13.7719099555025,
127.339007189851)) ;
#124270 = CARTESIAN_POINT('Ctrl Pts',(-28.5016223810496,13.4847455489294,
127.282758603318)) ;
#124271 = CARTESIAN_POINT('Ctrl Pts',(-28.5189628663482,13.1955424238471,
127.300427535986)) ;
#124272 = CARTESIAN_POINT('Ctrl Pts',(-28.5612901890702,12.9200552439899,
127.390764466653)) ;
#124273 = CARTESIAN_POINT('Ctrl Pts',(-28.6255879815174,12.6831184051196,
127.545604609315)) ;
#124274 = CARTESIAN_POINT('Ctrl Pts',(-28.7085274648009,12.4980281051702,
127.754767655982)) ;
#124275 = CARTESIAN_POINT('Ctrl Pts',(-28.8048707795907,12.3791543391629,
128.003062725603)) ;
#124276 = CARTESIAN_POINT('Ctrl Pts',(-28.9084505011422,12.3353503724763,
128.272456641543)) ;
#124277 = CARTESIAN_POINT('Ctrl Pts',(-29.0119290399947,12.3691099624238,
128.541734986675)) ;
#124278 = CARTESIAN_POINT('Ctrl Pts',(-29.1100844988828,12.4795856754925,
128.795121393085)) ;
#124279 = CARTESIAN_POINT('Ctrl Pts',(-29.1943370244015,12.655336096254,129.008407922735)) ;
#124280 = CARTESIAN_POINT('Ctrl Pts',(-29.2617806972532,12.8882259195335,
129.172162118277)) ;
#124281 = CARTESIAN_POINT('Ctrl Pts',(-29.3067986316922,13.1581921439883,
129.27061431898)) ;
#124282 = CARTESIAN_POINT('Ctrl Pts',(-29.3274947127435,13.4482190553547,
129.297870820219)) ;
#124283 = CARTESIAN_POINT('Ctrl Pts',(-29.3228861406397,13.7352663481711,
129.251351301865)) ;
#124284 = CARTESIAN_POINT('Ctrl Pts',(-29.2941391682194,14.0004787801146,
129.134251206445)) ;
#124285 = CARTESIAN_POINT('Ctrl Pts',(-29.2440911045041,14.224240187898,128.954965629854)) ;
#124286 = CARTESIAN_POINT('Ctrl Pts',(-29.1764772767869,14.391486040761,128.724142908791)) ;
#124287 = CARTESIAN_POINT('Ctrl Pts',(-29.0980269041192,14.4880342043903,
128.4619863877)) ;
#124288 = CARTESIAN_POINT('Ctrl Pts',(-29.0139943422698,14.508976716731,128.183329278251)) ;
#124289 = CARTESIAN_POINT('Ctrl Pts',(-28.9317871778469,14.4520806960152,
127.910110797654)) ;
#124290 = CARTESIAN_POINT('Ctrl Pts',(-28.8575866214198,14.3213934161067,
127.660199327887)) ;
#124291 = CARTESIAN_POINT('Ctrl Pts',(-28.7977078233166,14.1264275067293,
127.452160129362)) ;
#124292 = CARTESIAN_POINT('Ctrl Pts',(-28.7570216525618,13.8807879238241,
127.300143854661)) ;
#124293 = CARTESIAN_POINT('Ctrl Pts',(-28.7393381079918,13.6022564662603,
127.215325042563)) ;
#124294 = CARTESIAN_POINT('Ctrl Pts',(-28.7464673511228,13.3123737627951,
127.203159550126)) ;
#124295 = CARTESIAN_POINT('Ctrl Pts',(-28.7787003276841,13.0290002093282,
127.264164185569)) ;
#124296 = CARTESIAN_POINT('Ctrl Pts',(-28.8344853392707,12.7741269018416,
127.394000134619)) ;
#124297 = CARTESIAN_POINT('Ctrl Pts',(-28.9105332614011,12.5657350925596,
127.583024031671)) ;
#124298 = CARTESIAN_POINT('Ctrl Pts',(-29.0020340800631,12.4188761283997,
127.817221451334)) ;
#124299 = CARTESIAN_POINT('Ctrl Pts',(-29.1033490521045,12.3438128182006,
128.08005015539)) ;
#124300 = CARTESIAN_POINT('Ctrl Pts',(-29.2077611012054,12.346102551177,128.351954688411)) ;
#124301 = CARTESIAN_POINT('Ctrl Pts',(-29.3086983900599,12.4255736713201,
128.613675945362)) ;
#124302 = CARTESIAN_POINT('Ctrl Pts',(-29.3995090119233,12.5765458005785,
128.845828673796)) ;
#124303 = CARTESIAN_POINT('Ctrl Pts',(-29.4743911046107,12.7879288159169,
129.031482386916)) ;
#124304 = CARTESIAN_POINT('Ctrl Pts',(-29.528866555057,13.0448055751977,129.157510490086)) ;
#124305 = CARTESIAN_POINT('Ctrl Pts',(-29.5597228216667,13.3297564879043,
129.214430894783)) ;
#124306 = CARTESIAN_POINT('Ctrl Pts',(-29.5653119671571,13.6201108686768,
129.197692480837)) ;
#124307 = CARTESIAN_POINT('Ctrl Pts',(-29.5461454694217,13.8967555620889,
129.108587621245)) ;
#124308 = CARTESIAN_POINT('Ctrl Pts',(-29.5043003614803,14.1394984275279,
128.953246429327)) ;
#124309 = CARTESIAN_POINT('Ctrl Pts',(-29.4431774798725,14.3315002121409,
128.741455873336)) ;
#124310 = CARTESIAN_POINT('Ctrl Pts',(-29.368615149488,14.4575223198637,128.490628214048)) ;
#124311 = CARTESIAN_POINT('Ctrl Pts',(-29.2856254843638,14.5099977953481,
128.214919388015)) ;
#124312 = CARTESIAN_POINT('Ctrl Pts',(-29.2021625668279,14.4843800737971,
127.938111696582)) ;
#124313 = CARTESIAN_POINT('Ctrl Pts',(-29.1238742274253,14.3828781274989,
127.676265154723)) ;
#124314 = CARTESIAN_POINT('Ctrl Pts',(-29.0575885175731,14.2128161512202,
127.449543125235)) ;
#124315 = CARTESIAN_POINT('Ctrl Pts',(-29.0084776120694,13.9854781588929,
127.272874876826)) ;
#124316 = CARTESIAN_POINT('Ctrl Pts',(-28.9811292783656,13.7179644901035,
127.159826468009)) ;
#124317 = CARTESIAN_POINT('Ctrl Pts',(-28.9781179163729,13.4301920421151,
127.117966111952)) ;
#124318 = CARTESIAN_POINT('Ctrl Pts',(-29.0001132553344,13.1421055702502,
127.149189708795)) ;
#124319 = CARTESIAN_POINT('Ctrl Pts',(-29.047053104884,12.871501287512,127.252936726976)) ;
#124320 = CARTESIAN_POINT('Ctrl Pts',(-29.1151027479743,12.6436097972574,
127.418773188666)) ;
#124321 = CARTESIAN_POINT('Ctrl Pts',(-29.2011947687253,12.469849836909,127.637073459389)) ;
#124322 = CARTESIAN_POINT('Ctrl Pts',(-29.2991274824965,12.3651221790713,
127.890102388539)) ;
#124323 = CARTESIAN_POINT('Ctrl Pts',(-29.4030193284557,12.3356922244687,
128.160499003177)) ;
#124324 = CARTESIAN_POINT('Ctrl Pts',(-29.5063698934818,12.3844432220599,
128.429219190107)) ;
#124325 = CARTESIAN_POINT('Ctrl Pts',(-29.6017701668784,12.5072148267233,
128.674860804049)) ;
#124326 = CARTESIAN_POINT('Ctrl Pts',(-29.6838564893298,12.695755079112,128.881517005376)) ;
#124327 = CARTESIAN_POINT('Ctrl Pts',(-29.7472379158472,12.9373000432248,
129.033441592439)) ;
#124328 = CARTESIAN_POINT('Ctrl Pts',(-29.7877524940672,13.2121500744088,
129.118761133929)) ;
#124329 = CARTESIAN_POINT('Ctrl Pts',(-29.8036385546026,13.503246650252,129.131988911234)) ;
#124330 = CARTESIAN_POINT('Ctrl Pts',(-29.7944161810133,13.7871081777778,
129.072056104051)) ;
#124331 = CARTESIAN_POINT('Ctrl Pts',(-29.7612451453642,14.04691061429,128.941902135837)) ;
#124332 = CARTESIAN_POINT('Ctrl Pts',(-29.7076298212576,14.260565028937,128.752241000725)) ;
#124333 = CARTESIAN_POINT('Ctrl Pts',(-29.6374049797901,14.4153650292754,
128.513802744357)) ;
#124334 = CARTESIAN_POINT('Ctrl Pts',(-29.5575729299202,14.4978583100618,
128.247645906219)) ;
#124335 = CARTESIAN_POINT('Ctrl Pts',(-29.4733841555509,14.5041773759635,
127.968557400909)) ;
#124336 = CARTESIAN_POINT('Ctrl Pts',(-29.3921490619895,14.4329778405108,
127.698149651333)) ;
#124337 = CARTESIAN_POINT('Ctrl Pts',(-29.3200604919066,14.2890421003468,
127.454349974841)) ;
#124338 = CARTESIAN_POINT('Ctrl Pts',(-29.2634311723797,14.0827792612075,
127.255738950957)) ;
#124339 = CARTESIAN_POINT('Ctrl Pts',(-29.2270568377556,13.830933510425,127.116507499098)) ;
#124340 = CARTESIAN_POINT('Ctrl Pts',(-29.2138529064416,13.5483118095736,
127.044750757746)) ;
#124341 = CARTESIAN_POINT('Ctrl Pts',(-29.2257641491017,13.2574775512287,
127.046461089286)) ;
#124342 = CARTESIAN_POINT('Ctrl Pts',(-29.2626784751596,12.9779695749568,
127.121137886348)) ;
#124343 = CARTESIAN_POINT('Ctrl Pts',(-29.3223683269202,12.7311578821155,
127.262476188241)) ;
#124344 = CARTESIAN_POINT('Ctrl Pts',(-29.4021493735836,12.5323979618,127.46224042951)) ;
#124345 = CARTESIAN_POINT('Ctrl Pts',(-29.4957297661686,12.3989896763175,
127.702606498418)) ;
#124346 = CARTESIAN_POINT('Ctrl Pts',(-29.5982391003597,12.3382487508946,
127.96889464722)) ;
#124347 = CARTESIAN_POINT('Ctrl Pts',(-29.7022741235999,12.3552058345121,
128.239769962473)) ;
#124348 = CARTESIAN_POINT('Ctrl Pts',(-29.8021494393376,12.449068120654,128.498271362135)) ;
#124349 = CARTESIAN_POINT('Ctrl Pts',(-29.890357842438,12.6128543666523,128.722805283861)) ;
#124350 = CARTESIAN_POINT('Ctrl Pts',(-29.9614573415197,12.8333918946772,
128.897516477767)) ;
#124351 = CARTESIAN_POINT('Ctrl Pts',(-30.0117536796374,13.0975419716129,
129.01125406221)) ;
#124352 = CARTESIAN_POINT('Ctrl Pts',(-30.0378168368427,13.38437019925,129.054290739338)) ;
#124353 = CARTESIAN_POINT('Ctrl Pts',(-30.0386639542191,13.6749248877936,
129.023552155716)) ;
#124354 = CARTESIAN_POINT('Ctrl Pts',(-30.0148871543085,13.9463602698171,
128.920997210423)) ;
#124355 = CARTESIAN_POINT('Ctrl Pts',(-29.969281069923,14.179832441143,128.754782276744)) ;
#124356 = CARTESIAN_POINT('Ctrl Pts',(-29.9051021306394,14.3606302747574,
128.534050459932)) ;
#124357 = CARTESIAN_POINT('Ctrl Pts',(-29.8284637932964,14.4733618846649,
128.277111973948)) ;
#124358 = CARTESIAN_POINT('Ctrl Pts',(-29.744806599407,14.5110756603655,127.999483924866)) ;
#124359 = CARTESIAN_POINT('Ctrl Pts',(-29.6619786972772,14.4709889018576,
127.724569420284)) ;
#124360 = CARTESIAN_POINT('Ctrl Pts',(-29.5853193662016,14.3556941953622,
127.467426228982)) ;
#124361 = CARTESIAN_POINT('Ctrl Pts',(-29.5217947117476,14.1731666349653,
127.24867559156)) ;
#124362 = CARTESIAN_POINT('Ctrl Pts',(-29.4767596890819,13.9378583888153,
127.084070689769)) ;
#124363 = CARTESIAN_POINT('Ctrl Pts',(-29.4537789685261,13.665635486159,126.983860518829)) ;
#124364 = CARTESIAN_POINT('Ctrl Pts',(-29.4554655103503,13.3744562424158,
126.955530110006)) ;
#124365 = CARTESIAN_POINT('Ctrl Pts',(-29.482352001784,13.0885611024712,127.001023851845)) ;
#124366 = CARTESIAN_POINT('Ctrl Pts',(-29.5331352905586,12.8263305673749,
127.116301798459)) ;
#124367 = CARTESIAN_POINT('Ctrl Pts',(-29.6050937436806,12.6063806997543,
127.293387240896)) ;
#124368 = CARTESIAN_POINT('Ctrl Pts',(-29.6939157301013,12.4447492337382,
127.519673899328)) ;
#124369 = CARTESIAN_POINT('Ctrl Pts',(-29.793684780295,12.353502559508,127.777985701848)) ;
#124370 = CARTESIAN_POINT('Ctrl Pts',(-29.8981426431129,12.3391045182876,
128.049969682744)) ;
#124371 = CARTESIAN_POINT('Ctrl Pts',(-29.999995923788,12.4018104838522,128.314511218612)) ;
#124372 = CARTESIAN_POINT('Ctrl Pts',(-30.0940583651971,12.5389587593729,
128.555960228962)) ;
#124373 = CARTESIAN_POINT('Ctrl Pts',(-30.1724238258053,12.7377765995817,
128.751929330358)) ;
#124374 = CARTESIAN_POINT('Ctrl Pts',(-30.231666115958,12.9863021610025,128.891870713091)) ;
#124375 = CARTESIAN_POINT('Ctrl Pts',(-30.2677813975979,13.26603407284,128.9642745019)) ;
#124376 = CARTESIAN_POINT('Ctrl Pts',(-30.278920299464,13.5582234410802,128.963573253356)) ;
#124377 = CARTESIAN_POINT('Ctrl Pts',(-30.26499159685,13.8387406073518,128.889873934224)) ;
#124378 = CARTESIAN_POINT('Ctrl Pts',(-30.2278772365566,14.0904926888755,
128.748354891165)) ;
#124379 = CARTESIAN_POINT('Ctrl Pts',(-30.1702932972715,14.2955137272415,
128.546803394523)) ;
#124380 = CARTESIAN_POINT('Ctrl Pts',(-30.0984120784379,14.4360007562524,
128.303894575953)) ;
#124381 = CARTESIAN_POINT('Ctrl Pts',(-30.0167909849871,14.5051703131075,
128.032264264772)) ;
#124382 = CARTESIAN_POINT('Ctrl Pts',(-29.9328311834785,14.4966323444729,
127.753939337243)) ;
#124383 = CARTESIAN_POINT('Ctrl Pts',(-29.8525465680788,14.4108290646986,
127.48616105779)) ;
#124384 = CARTESIAN_POINT('Ctrl Pts',(-29.7832722853812,14.2547208432748,
127.250733345617)) ;
#124385 = CARTESIAN_POINT('Ctrl Pts',(-29.7301231215459,14.0388604849956,
127.062340185207)) ;
#124386 = CARTESIAN_POINT('Ctrl Pts',(-29.6977837486614,13.7794054501878,
126.934803763672)) ;
#124387 = CARTESIAN_POINT('Ctrl Pts',(-29.6893035192315,13.4926640432345,
126.876755208931)) ;
#124388 = CARTESIAN_POINT('Ctrl Pts',(-29.7059159424158,13.2038301120676,
126.892352602474)) ;
#124389 = CARTESIAN_POINT('Ctrl Pts',(-29.7474057347377,12.9280759212708,
126.980311855023)) ;
#124390 = CARTESIAN_POINT('Ctrl Pts',(-29.8113849358203,12.6887447030163,
127.134072403226)) ;
#124391 = CARTESIAN_POINT('Ctrl Pts',(-29.8938930194494,12.5022966098147,
127.341991684149)) ;
#124392 = CARTESIAN_POINT('Ctrl Pts',(-29.9895145374687,12.3817639702232,
127.588316710086)) ;
#124393 = CARTESIAN_POINT('Ctrl Pts',(-30.0933362893935,12.3354318122153,
127.858302940627)) ;
#124394 = CARTESIAN_POINT('Ctrl Pts',(-30.1967145851462,12.3672035542546,
128.127339641179)) ;
#124395 = CARTESIAN_POINT('Ctrl Pts',(-30.2946449394812,12.4744264817991,
128.380263197516)) ;
#124396 = CARTESIAN_POINT('Ctrl Pts',(-30.3803208267645,12.6503068789,128.59733206961)) ;
#124397 = CARTESIAN_POINT('Ctrl Pts',(-30.447925069988,12.88124813694,128.761691535732)) ;
#124398 = CARTESIAN_POINT('Ctrl Pts',(-30.4935671315089,13.1494231043328,
128.862066641)) ;
#124399 = CARTESIAN_POINT('Ctrl Pts',(-30.5150767542471,13.4405328336443,
128.891547059133)) ;
#124400 = CARTESIAN_POINT('Ctrl Pts',(-30.5111288053941,13.7272524235385,
128.847033061191)) ;
#124401 = CARTESIAN_POINT('Ctrl Pts',(-30.4830702446878,13.9933198018618,
128.731951447052)) ;
#124402 = CARTESIAN_POINT('Ctrl Pts',(-30.4336230875361,14.2183989347204,
128.554443162596)) ;
#124403 = CARTESIAN_POINT('Ctrl Pts',(-30.3663826934686,14.3876287809154,
128.32468557259)) ;
#124404 = CARTESIAN_POINT('Ctrl Pts',(-30.2882857864212,14.4861871139801,
128.063606645417)) ;
#124405 = CARTESIAN_POINT('Ctrl Pts',(-30.2042479014223,14.5095212263095,
127.784908710589)) ;
#124406 = CARTESIAN_POINT('Ctrl Pts',(-30.121812915052,14.4547286941079,127.510988806245)) ;
#124407 = CARTESIAN_POINT('Ctrl Pts',(-30.047335214886,14.3261104850367,127.260287876867)) ;
#124408 = CARTESIAN_POINT('Ctrl Pts',(-29.9869536457719,14.1327423956962,
127.05076735835)) ;
#124409 = CARTESIAN_POINT('Ctrl Pts',(-29.9456867841733,13.8885304573601,
126.897084193712)) ;
#124410 = CARTESIAN_POINT('Ctrl Pts',(-29.9273110105387,13.6107522710193,
126.810248321643)) ;
#124411 = CARTESIAN_POINT('Ctrl Pts',(-29.933619766616,13.3210540758006,126.795703495367)) ;
#124412 = CARTESIAN_POINT('Ctrl Pts',(-29.9655096904855,13.0351249391052,
126.855452075723)) ;
#124413 = CARTESIAN_POINT('Ctrl Pts',(-30.0202087483359,12.7816148571452,
126.982424137597)) ;
#124414 = CARTESIAN_POINT('Ctrl Pts',(-30.0959655060956,12.5706516748794,
127.170461842928)) ;
#124415 = CARTESIAN_POINT('Ctrl Pts',(-30.187075628918,12.4220918167394,127.403541558847)) ;
#124416 = CARTESIAN_POINT('Ctrl Pts',(-30.2883231009899,12.3448083545055,
127.666131810962)) ;
#124417 = CARTESIAN_POINT('Ctrl Pts',(-30.3926830064791,12.3450375900235,
127.93790207961)) ;
#124418 = CARTESIAN_POINT('Ctrl Pts',(-30.4936514271429,12.4222141215766,
128.199767789345)) ;
#124419 = CARTESIAN_POINT('Ctrl Pts',(-30.5848893407942,12.5713074000372,
128.433150896225)) ;
#124420 = CARTESIAN_POINT('Ctrl Pts',(-30.6603311521981,12.7812070105723,
128.620428718384)) ;
#124421 = CARTESIAN_POINT('Ctrl Pts',(-30.7155665117066,13.0378488607775,
128.748579693311)) ;
#124422 = CARTESIAN_POINT('Ctrl Pts',(-30.7469885961688,13.3220974223082,
128.807185014511)) ;
#124423 = CARTESIAN_POINT('Ctrl Pts',(-30.7532932333332,13.611647883706,128.792639705149)) ;
#124424 = CARTESIAN_POINT('Ctrl Pts',(-30.7347671239028,13.8896345343945,
128.705325771604)) ;
#124425 = CARTESIAN_POINT('Ctrl Pts',(-30.693600390576,14.1329049356831,128.552051589304)) ;
#124426 = CARTESIAN_POINT('Ctrl Pts',(-30.633070371467,14.3266158098986,128.342023513571)) ;
#124427 = CARTESIAN_POINT('Ctrl Pts',(-30.5585711021984,14.4550272244897,
128.091269880465)) ;
#124428 = CARTESIAN_POINT('Ctrl Pts',(-30.4759843115532,14.5094869188899,
127.816847983147)) ;
#124429 = CARTESIAN_POINT('Ctrl Pts',(-30.3924156986506,14.4863254941317,
127.539715217734)) ;
#124430 = CARTESIAN_POINT('Ctrl Pts',(-30.3137804479421,14.3868080621077,
127.276813774952)) ;
#124431 = CARTESIAN_POINT('Ctrl Pts',(-30.2470276101846,14.2186053489218,
127.04872115819)) ;
#124432 = CARTESIAN_POINT('Ctrl Pts',(-30.1972622816575,13.9916146636668,
126.870012022956)) ;
#124433 = CARTESIAN_POINT('Ctrl Pts',(-30.1694297843685,13.7271394613145,
126.755815447488)) ;
#124434 = CARTESIAN_POINT('Ctrl Pts',(-30.1656502016795,13.4373621630931,
126.711435528483)) ;
#124435 = CARTESIAN_POINT('Ctrl Pts',(-30.1869265241885,13.1504054567353,
126.740721815544)) ;
#124436 = CARTESIAN_POINT('Ctrl Pts',(-30.2331958971664,12.8786465082132,
126.842474926041)) ;
#124437 = CARTESIAN_POINT('Ctrl Pts',(-30.3005045160255,12.6500332847712,
127.006235986259)) ;
#124438 = CARTESIAN_POINT('Ctrl Pts',(-30.3859680592901,12.4743183889617,
127.222741912272)) ;
#124439 = CARTESIAN_POINT('Ctrl Pts',(-30.484292867573,12.3668547885935,127.476696341652)) ;
#124440 = CARTESIAN_POINT('Ctrl Pts',(-30.587616388384,12.3355629410877,127.745593654544)) ;
#124441 = CARTESIAN_POINT('Ctrl Pts',(-30.6910287858327,12.3817108160481,
128.014514918498)) ;
#124442 = CARTESIAN_POINT('Ctrl Pts',(-30.7871323371635,12.5028398511796,
128.262083898072)) ;
#124443 = CARTESIAN_POINT('Ctrl Pts',(-30.8697321583824,12.6903514923922,
128.470177876443)) ;
#124444 = CARTESIAN_POINT('Ctrl Pts',(-30.9332422444198,12.9285060131068,
128.622757398001)) ;
#124445 = CARTESIAN_POINT('Ctrl Pts',(-30.9748295562401,13.2046732930674,
128.710950155907)) ;
#124446 = CARTESIAN_POINT('Ctrl Pts',(-30.9913101196902,13.4951334329262,
128.725980834387)) ;
#124447 = CARTESIAN_POINT('Ctrl Pts',(-30.9827689117977,13.7795013395347,
128.668022330097)) ;
#124448 = CARTESIAN_POINT('Ctrl Pts',(-30.9503979576926,14.0394109591315,
128.540333225843)) ;
#124449 = CARTESIAN_POINT('Ctrl Pts',(-30.8971895152289,14.2552142278511,
128.351765160571)) ;
#124450 = CARTESIAN_POINT('Ctrl Pts',(-30.827703837052,14.4112842986504,128.115645384182)) ;
#124451 = CARTESIAN_POINT('Ctrl Pts',(-30.7478762186822,14.4966304081093,
127.849398626646)) ;
#124452 = CARTESIAN_POINT('Ctrl Pts',(-30.6632860167029,14.5049768575903,
127.568975433367)) ;
#124453 = CARTESIAN_POINT('Ctrl Pts',(-30.5822812878458,14.4360834976797,
127.299398037642)) ;
#124454 = CARTESIAN_POINT('Ctrl Pts',(-30.5099274709679,14.2946512650185,
127.054884795324)) ;
#124455 = CARTESIAN_POINT('Ctrl Pts',(-30.4526678489903,14.0899138392311,
126.854394854671)) ;
#124456 = CARTESIAN_POINT('Ctrl Pts',(-30.4155401891835,13.8386915040984,
126.712892259472)) ;
#124457 = CARTESIAN_POINT('Ctrl Pts',(-30.4016797337328,13.5555689993548,
126.639099979704)) ;
#124458 = CARTESIAN_POINT('Ctrl Pts',(-30.4128387173659,13.2663899085958,
126.638804628752)) ;
#124459 = CARTESIAN_POINT('Ctrl Pts',(-30.4489906096477,12.9858845454111,
126.711220297671)) ;
#124460 = CARTESIAN_POINT('Ctrl Pts',(-30.5082151997129,12.737510093137,126.851136088065)) ;
#124461 = CARTESIAN_POINT('Ctrl Pts',(-30.5871935739308,12.5376375211986,
127.048669841167)) ;
#124462 = CARTESIAN_POINT('Ctrl Pts',(-30.6809240837796,12.4015826391132,
127.289300668043)) ;
#124463 = CARTESIAN_POINT('Ctrl Pts',(-30.7827898108076,12.3390360778661,
127.553872708322)) ;
#124464 = CARTESIAN_POINT('Ctrl Pts',(-30.8870946705224,12.3535754317009,
127.825461319271)) ;
#124465 = CARTESIAN_POINT('Ctrl Pts',(-30.9870766402844,12.4452741320202,
128.084312934138)) ;
#124466 = CARTESIAN_POINT('Ctrl Pts',(-31.0756876477193,12.6067972439988,
128.310049838523)) ;
#124467 = CARTESIAN_POINT('Ctrl Pts',(-31.1477578491021,12.8274893323333,
128.487374513247)) ;
#124468 = CARTESIAN_POINT('Ctrl Pts',(-31.1983271909888,13.0891409681253,
128.602118684947)) ;
#124469 = CARTESIAN_POINT('Ctrl Pts',(-31.2251992522325,13.3757401842095,
128.647491129551)) ;
#124470 = CARTESIAN_POINT('Ctrl Pts',(-31.2267800238666,13.6659116467556,
128.618963093478)) ;
#124471 = CARTESIAN_POINT('Ctrl Pts',(-31.2038312103077,13.9383430933064,
128.518829961431)) ;
#124472 = CARTESIAN_POINT('Ctrl Pts',(-31.1583764244852,14.1747318891546,
128.352797912173)) ;
#124473 = CARTESIAN_POINT('Ctrl Pts',(-31.0952754500218,14.3556000253484,
128.135542669314)) ;
#124474 = CARTESIAN_POINT('Ctrl Pts',(-31.0182491364109,14.4715471838241,
127.877162829971)) ;
#124475 = CARTESIAN_POINT('Ctrl Pts',(-30.9352331910558,14.5109306883494,
127.601637155271)) ;
#124476 = CARTESIAN_POINT('Ctrl Pts',(-30.8521513235924,14.4734197529204,
127.325920803467)) ;
#124477 = CARTESIAN_POINT('Ctrl Pts',(-30.7749550777624,14.3595613324345,
127.067091655152)) ;
#124478 = CARTESIAN_POINT('Ctrl Pts',(-30.7112774432419,14.1794661673076,
126.848033266043)) ;
#124479 = CARTESIAN_POINT('Ctrl Pts',(-30.6655292058414,13.945518104717,126.681323661303)) ;
#124480 = CARTESIAN_POINT('Ctrl Pts',(-30.6418404807834,13.6723045433651,
126.578842288596)) ;
#124481 = CARTESIAN_POINT('Ctrl Pts',(-30.6428557130489,13.3834915419228,
126.548801546779)) ;
#124482 = CARTESIAN_POINT('Ctrl Pts',(-30.6689836005855,13.096613347718,126.59201192854)) ;
#124483 = CARTESIAN_POINT('Ctrl Pts',(-30.7192056164411,12.8330520382444,
126.705604956252)) ;
#124484 = CARTESIAN_POINT('Ctrl Pts',(-30.790834532404,12.611232367513,126.881647244547)) ;
#124485 = CARTESIAN_POINT('Ctrl Pts',(-30.8791960095022,12.4482428501487,
127.1066335396)) ;
#124486 = CARTESIAN_POINT('Ctrl Pts',(-30.9782658750989,12.3553252132509,
127.363054948833)) ;
#124487 = CARTESIAN_POINT('Ctrl Pts',(-31.0825679140159,12.3382107203878,
127.634621858498)) ;
#124488 = CARTESIAN_POINT('Ctrl Pts',(-31.1851705795097,12.3992481995866,
127.901152590329)) ;
#124489 = CARTESIAN_POINT('Ctrl Pts',(-31.2787737046393,12.533120575299,128.141551668428)) ;
#124490 = CARTESIAN_POINT('Ctrl Pts',(-31.3581694597885,12.7309389352082,
128.340353310314)) ;
#124491 = CARTESIAN_POINT('Ctrl Pts',(-31.4181700324155,12.9791526214122,
128.482412755056)) ;
#124492 = CARTESIAN_POINT('Ctrl Pts',(-31.4549351457382,13.2585792633392,
128.556683953962)) ;
#124493 = CARTESIAN_POINT('Ctrl Pts',(-31.4667178812962,13.5499400001449,
128.557952145081)) ;
#124494 = CARTESIAN_POINT('Ctrl Pts',(-31.4535429896863,13.831171440361,128.486447666919)) ;
#124495 = CARTESIAN_POINT('Ctrl Pts',(-31.4167705477339,14.0848087373092,
128.345787022824)) ;
#124496 = CARTESIAN_POINT('Ctrl Pts',(-31.3604022147667,14.2892042753313,
128.148175854391)) ;
#124497 = CARTESIAN_POINT('Ctrl Pts',(-31.2883262191337,14.4332159857665,
127.904406939294)) ;
#124498 = CARTESIAN_POINT('Ctrl Pts',(-31.2070359185829,14.5042074008981,
127.63382430801)) ;
#124499 = CARTESIAN_POINT('Ctrl Pts',(-31.1228911241346,14.4978850234615,
127.35488500635)) ;
#124500 = CARTESIAN_POINT('Ctrl Pts',(-31.0426799297735,14.4145533230364,
127.087444540291)) ;
#124501 = CARTESIAN_POINT('Ctrl Pts',(-30.9728258224195,14.2600829811303,
126.850238813674)) ;
#124502 = CARTESIAN_POINT('Ctrl Pts',(-30.9192125542816,14.0459658246631,
126.660532770035)) ;
#124503 = CARTESIAN_POINT('Ctrl Pts',(-30.8862030827133,13.7875806302573,
126.53103679406)) ;
#124504 = CARTESIAN_POINT('Ctrl Pts',(-30.8769652131714,13.5015007624486,
126.470798628312)) ;
#124505 = CARTESIAN_POINT('Ctrl Pts',(-30.8928913009424,13.2119710918027,
126.484325214026)) ;
#124506 = CARTESIAN_POINT('Ctrl Pts',(-30.9335291322578,12.9363052863804,
126.569902948706)) ;
#124507 = CARTESIAN_POINT('Ctrl Pts',(-30.9969656458465,12.6952735982691,
126.722023128662)) ;
#124508 = CARTESIAN_POINT('Ctrl Pts',(-31.0787937782132,12.5071256429724,
126.928019042158)) ;
#124509 = CARTESIAN_POINT('Ctrl Pts',(-31.1750192801707,12.383762838378,127.175802450844)) ;
#124510 = CARTESIAN_POINT('Ctrl Pts',(-31.2776023117639,12.3357954087545,
127.442538372625)) ;
#124511 = CARTESIAN_POINT('Ctrl Pts',(-31.3818855655355,12.3652711313032,
127.713950589831)) ;
#124512 = CARTESIAN_POINT('Ctrl Pts',(-31.4797808939481,12.4705156862028,
127.966863975208)) ;
#124513 = CARTESIAN_POINT('Ctrl Pts',(-31.5656441790736,12.6439184984734,
128.184578603)) ;
#124514 = CARTESIAN_POINT('Ctrl Pts',(-31.6338998959943,12.8730354014428,
128.350870354409)) ;
#124515 = CARTESIAN_POINT('Ctrl Pts',(-31.6804874469165,13.1424159380097,
128.453758787972)) ;
#124516 = CARTESIAN_POINT('Ctrl Pts',(-31.7025235008913,13.4306391713404,
128.485081697739)) ;
#124517 = CARTESIAN_POINT('Ctrl Pts',(-31.6994134419099,13.7191539467883,
128.442846383316)) ;
#124518 = CARTESIAN_POINT('Ctrl Pts',(-31.6719894670492,13.9861294006722,
128.329622243672)) ;
#124519 = CARTESIAN_POINT('Ctrl Pts',(-31.6230063053965,14.2128684177951,
128.153415320966)) ;
#124520 = CARTESIAN_POINT('Ctrl Pts',(-31.5564974117218,14.3833348165239,
127.925939532501)) ;
#124521 = CARTESIAN_POINT('Ctrl Pts',(-31.4782582440777,14.4845639234701,
127.664272210316)) ;
#124522 = CARTESIAN_POINT('Ctrl Pts',(-31.3945103482704,14.5099092452808,
127.386518238402)) ;
#124523 = CARTESIAN_POINT('Ctrl Pts',(-31.3118033167592,14.4573340950599,
127.111748041755)) ;
#124524 = CARTESIAN_POINT('Ctrl Pts',(-31.2370170461689,14.3305257687139,
126.860139050925)) ;
#124525 = CARTESIAN_POINT('Ctrl Pts',(-31.1763161492696,14.1393929887669,
126.649775812031)) ;
#124526 = CARTESIAN_POINT('Ctrl Pts',(-31.1343568830856,13.8963011605845,
126.494040620924)) ;
#124527 = CARTESIAN_POINT('Ctrl Pts',(-31.1152511809763,13.6185277978384,
126.404996071388)) ;
#124528 = CARTESIAN_POINT('Ctrl Pts',(-31.1209459798989,13.3290636880528,
126.388670020425)) ;
#124529 = CARTESIAN_POINT('Ctrl Pts',(-31.1517877758926,13.0445547365035,
126.44559285922)) ;
#124530 = CARTESIAN_POINT('Ctrl Pts',(-31.2062319103761,12.7876682378207,
126.571537992278)) ;
#124531 = CARTESIAN_POINT('Ctrl Pts',(-31.2816236951061,12.5753841966509,
126.758494307984)) ;
#124532 = CARTESIAN_POINT('Ctrl Pts',(-31.3720200163798,12.4255193729721,
126.989613193023)) ;
#124533 = CARTESIAN_POINT('Ctrl Pts',(-31.4730863859192,12.3459765323798,
127.251666609436)) ;
#124534 = CARTESIAN_POINT('Ctrl Pts',(-31.5773109497355,12.3439073605975,
127.523083026688)) ;
#124535 = CARTESIAN_POINT('Ctrl Pts',(-31.6786559521164,12.4188280799993,
127.785997053854)) ;
#124536 = CARTESIAN_POINT('Ctrl Pts',(-31.7706041117922,12.5669348779127,
128.021308309052)) ;
#124537 = CARTESIAN_POINT('Ctrl Pts',(-31.8460678201719,12.7740278443755,
128.208861704662)) ;
#124538 = CARTESIAN_POINT('Ctrl Pts',(-31.9021441339329,13.0302841857639,
128.339365368756)) ;
#124539 = CARTESIAN_POINT('Ctrl Pts',(-31.9341916798789,13.313391034623,128.39987822107)) ;
#124540 = CARTESIAN_POINT('Ctrl Pts',(-31.9412308825654,13.603463825877,128.387421784324)) ;
#124541 = CARTESIAN_POINT('Ctrl Pts',(-31.9235255942991,13.881303539034,128.302617667535)) ;
#124542 = CARTESIAN_POINT('Ctrl Pts',(-31.8826193869947,14.1277804532013,
128.149829200477)) ;
#124543 = CARTESIAN_POINT('Ctrl Pts',(-31.8226073128335,14.3222500271651,
127.941403939693)) ;
#124544 = CARTESIAN_POINT('Ctrl Pts',(-31.7486997913269,14.4521801534422,
127.692492488672)) ;
#124545 = CARTESIAN_POINT('Ctrl Pts',(-31.6663643399628,14.5090397064551,
127.418847768858)) ;
#124546 = CARTESIAN_POINT('Ctrl Pts',(-31.5824009229194,14.4879536180509,
127.140421787047)) ;
#124547 = CARTESIAN_POINT('Ctrl Pts',(-31.5036370266105,14.3907168838663,
126.877206024863)) ;
#124548 = CARTESIAN_POINT('Ctrl Pts',(-31.436238274105,14.2230874548014,126.647049834908)) ;
#124549 = CARTESIAN_POINT('Ctrl Pts',(-31.386526275312,14.0008520915057,126.468970265157)) ;
#124550 = CARTESIAN_POINT('Ctrl Pts',(-31.3576250453209,13.7343152411408,
126.351250585093)) ;
#124551 = CARTESIAN_POINT('Ctrl Pts',(-31.3531426090254,13.4474451384185,
126.305130028153)) ;
#124552 = CARTESIAN_POINT('Ctrl Pts',(-31.3738726128369,13.1575373566889,
126.332496699286)) ;
#124553 = CARTESIAN_POINT('Ctrl Pts',(-31.4189399340047,12.8878586213282,
126.431113174391)) ;
#124554 = CARTESIAN_POINT('Ctrl Pts',(-31.486140272065,12.6555337208909,126.594256475355)) ;
#124555 = CARTESIAN_POINT('Ctrl Pts',(-31.5711382567036,12.4784852889698,
126.809445172476)) ;
#124556 = CARTESIAN_POINT('Ctrl Pts',(-31.6691499143102,12.3688435118071,
127.062490447939)) ;
#124557 = CARTESIAN_POINT('Ctrl Pts',(-31.7726188430086,12.3353790498827,
127.331744180192)) ;
#124558 = CARTESIAN_POINT('Ctrl Pts',(-31.8759336246217,12.3794309096132,
127.600441979446)) ;
#124559 = CARTESIAN_POINT('Ctrl Pts',(-31.9720889415792,12.4979553163596,
127.848259175371)) ;
#124560 = CARTESIAN_POINT('Ctrl Pts',(-32.0554688914873,12.6843641883006,
128.05850963336)) ;
#124561 = CARTESIAN_POINT('Ctrl Pts',(-32.1194424670517,12.9208195747622,
128.212508863396)) ;
#124562 = CARTESIAN_POINT('Ctrl Pts',(-32.161757747067,13.1965599985602,128.302784788776)) ;
#124563 = CARTESIAN_POINT('Ctrl Pts',(-32.1789423174569,13.4854151022566,
128.320037673356)) ;
#124564 = CARTESIAN_POINT('Ctrl Pts',(-32.1711933637879,13.7715246215189,
128.264248994403)) ;
#124565 = CARTESIAN_POINT('Ctrl Pts',(-32.1393291975497,14.0329604460064,
128.137965297033)) ;
#124566 = CARTESIAN_POINT('Ctrl Pts',(-32.0867940958276,14.2495175049027,
127.951460801025)) ;
#124567 = CARTESIAN_POINT('Ctrl Pts',(-32.0177979789177,14.4077222066367,
127.716792376886)) ;
#124568 = CARTESIAN_POINT('Ctrl Pts',(-31.9375247117624,14.4954975109272,
127.44898097478)) ;
#124569 = CARTESIAN_POINT('Ctrl Pts',(-31.8537460867362,14.5058124049383,
127.171244726261)) ;
#124570 = CARTESIAN_POINT('Ctrl Pts',(-31.772123804296,14.4390539454557,126.899685772576)) ;
#124571 = CARTESIAN_POINT('Ctrl Pts',(-31.6993301037076,14.2988993787837,
126.653821842272)) ;
#124572 = CARTESIAN_POINT('Ctrl Pts',(-31.6417494548733,14.0959845150152,
126.452461138729)) ;
#124573 = CARTESIAN_POINT('Ctrl Pts',(-31.6041498202792,13.8467236092075,
126.309691385775)) ;
#124574 = CARTESIAN_POINT('Ctrl Pts',(-31.5895140395483,13.5651497445093,
126.233737086702)) ;
#124575 = CARTESIAN_POINT('Ctrl Pts',(-31.5999241287719,13.2745208567972,
126.231092292525)) ;
#124576 = CARTESIAN_POINT('Ctrl Pts',(-31.6355120865293,12.9930479903862,
126.301811575219)) ;
#124577 = CARTESIAN_POINT('Ctrl Pts',(-31.6939636509035,12.744268366307,126.439563836285)) ;
#124578 = CARTESIAN_POINT('Ctrl Pts',(-31.7723241051701,12.5428868462353,
126.635326857753)) ;
#124579 = CARTESIAN_POINT('Ctrl Pts',(-31.8656254635545,12.4047082626809,
126.874723079366)) ;
#124580 = CARTESIAN_POINT('Ctrl Pts',(-31.9676540092607,12.3396945376806,
127.139665153436)) ;
#124581 = CARTESIAN_POINT('Ctrl Pts',(-32.0719191102728,12.3521469878651,
127.411159614694)) ;
#124582 = CARTESIAN_POINT('Ctrl Pts',(-32.1718927341903,12.4413144196275,
127.670070810723)) ;
#124583 = CARTESIAN_POINT('Ctrl Pts',(-32.2610423474875,12.6011044167591,
127.8973332851)) ;
#124584 = CARTESIAN_POINT('Ctrl Pts',(-32.3334806640345,12.8194225372239,
128.075845726197)) ;
#124585 = CARTESIAN_POINT('Ctrl Pts',(-32.3850196376036,13.0811435285209,
128.193273866145)) ;
#124586 = CARTESIAN_POINT('Ctrl Pts',(-32.4125817943959,13.3679218651448,
128.240601929342)) ;
#124587 = CARTESIAN_POINT('Ctrl Pts',(-32.4148577451004,13.6574454628282,
128.214198686858)) ;
#124588 = CARTESIAN_POINT('Ctrl Pts',(-32.3926720296224,13.9304219315962,
128.116328916553)) ;
#124589 = CARTESIAN_POINT('Ctrl Pts',(-32.3477869876259,14.1686008809453,
127.951913381079)) ;
#124590 = CARTESIAN_POINT('Ctrl Pts',(-32.284971158177,14.3514046906987,127.735422298426)) ;
#124591 = CARTESIAN_POINT('Ctrl Pts',(-32.2087232804531,14.4688537021457,
127.479519830962)) ;
#124592 = CARTESIAN_POINT('Ctrl Pts',(-32.1254819939557,14.5110084059665,
127.203197805899)) ;
#124593 = CARTESIAN_POINT('Ctrl Pts',(-32.042186619966,14.4754271671864,126.926806872625)) ;
#124594 = CARTESIAN_POINT('Ctrl Pts',(-31.9649675676906,14.3641624837098,
126.668028698741)) ;
#124595 = CARTESIAN_POINT('Ctrl Pts',(-31.9005738315734,14.1852632714168,
126.446754200325)) ;
#124596 = CARTESIAN_POINT('Ctrl Pts',(-31.8543504110818,13.9526451363771,
126.278680058295)) ;
#124597 = CARTESIAN_POINT('Ctrl Pts',(-31.8300493968808,13.6818446977071,
126.174592372268)) ;
#124598 = CARTESIAN_POINT('Ctrl Pts',(-31.8301771516343,13.3926206183681,
126.141881666587)) ;
#124599 = CARTESIAN_POINT('Ctrl Pts',(-31.8557646547221,13.1038754492096,
126.183340661804)) ;
#124600 = CARTESIAN_POINT('Ctrl Pts',(-31.9052187214914,12.840383579606,126.294805831761)) ;
#124601 = CARTESIAN_POINT('Ctrl Pts',(-31.97602772857,12.6175434058043,126.468540816622)) ;
#124602 = CARTESIAN_POINT('Ctrl Pts',(-32.0641273166764,12.452017834643,126.692686648714)) ;
#124603 = CARTESIAN_POINT('Ctrl Pts',(-32.1634651082686,12.3567780373273,
126.949731371185)) ;
#124604 = CARTESIAN_POINT('Ctrl Pts',(-32.2671759723703,12.3376561181457,
127.219747078339)) ;
#124605 = CARTESIAN_POINT('Ctrl Pts',(-32.3700590194861,12.3963495269004,
127.487055840793)) ;
#124606 = CARTESIAN_POINT('Ctrl Pts',(-32.4640016861435,12.5282530119487,
127.728446795974)) ;
#124607 = CARTESIAN_POINT('Ctrl Pts',(-32.5438766891884,12.7243874356401,
127.928650447838)) ;
#124608 = CARTESIAN_POINT('Ctrl Pts',(-32.6044439637128,12.9708925599776,
128.072424865895)) ;
#124609 = CARTESIAN_POINT('Ctrl Pts',(-32.6419759471104,13.2502128136118,
128.148867357921)) ;
#124610 = CARTESIAN_POINT('Ctrl Pts',(-32.6545321724612,13.5400585853171,
128.152566906686)) ;
#124611 = CARTESIAN_POINT('Ctrl Pts',(-32.6420230728552,13.8239340251458,
128.082761152627)) ;
#124612 = CARTESIAN_POINT('Ctrl Pts',(-32.6059615988536,14.0777678447128,
127.944294228757)) ;
#124613 = CARTESIAN_POINT('Ctrl Pts',(-32.5500370870999,14.2841379825029,
127.74791925335)) ;
#124614 = CARTESIAN_POINT('Ctrl Pts',(-32.4785189411542,14.4298157397374,
127.50586889978)) ;
#124615 = CARTESIAN_POINT('Ctrl Pts',(-32.3971370747449,14.5033259419055,
127.234901175803)) ;
#124616 = CARTESIAN_POINT('Ctrl Pts',(-32.3130267071577,14.499135083616,126.956085571107)) ;
#124617 = CARTESIAN_POINT('Ctrl Pts',(-32.2325533904374,14.4177797503692,
126.687848133579)) ;
#124618 = CARTESIAN_POINT('Ctrl Pts',(-32.1625451627168,14.2657375874764,
126.450301985178)) ;
#124619 = CARTESIAN_POINT('Ctrl Pts',(-32.1082043097961,14.0527572687347,
126.258387004546)) ;
#124620 = CARTESIAN_POINT('Ctrl Pts',(-32.0745277451477,13.7942042748117,
126.126810553039)) ;
#124621 = CARTESIAN_POINT('Ctrl Pts',(-32.0646864224014,13.5099720674089,
126.064975641642)) ;
#124622 = CARTESIAN_POINT('Ctrl Pts',(-32.0798874202907,13.2198346279653,
126.076326920652)) ;
#124623 = CARTESIAN_POINT('Ctrl Pts',(-32.1199058770128,12.943315390008,126.160076953794)) ;
#124624 = CARTESIAN_POINT('Ctrl Pts',(-32.1828974962533,12.7008041601945,
126.310848236002)) ;
#124625 = CARTESIAN_POINT('Ctrl Pts',(-32.2639968728833,12.5118987867612,
126.514840222286)) ;
#124626 = CARTESIAN_POINT('Ctrl Pts',(-32.3593853092676,12.3867144274878,
126.760340270936)) ;
#124627 = CARTESIAN_POINT('Ctrl Pts',(-32.4624376893913,12.3359851179155,
127.028252288718)) ;
#124628 = CARTESIAN_POINT('Ctrl Pts',(-32.5667565587772,12.3634203975105,
127.299779078233)) ;
#124629 = CARTESIAN_POINT('Ctrl Pts',(-32.6648922781871,12.4663876776292,
127.553408260374)) ;
#124630 = CARTESIAN_POINT('Ctrl Pts',(-32.7515226393346,12.638970046877,127.773214375674)) ;
#124631 = CARTESIAN_POINT('Ctrl Pts',(-32.8199640950515,12.8657476347374,
127.940206666324)) ;
#124632 = CARTESIAN_POINT('Ctrl Pts',(-32.8673394624009,13.1346340040003,
128.045343963703)) ;
#124633 = CARTESIAN_POINT('Ctrl Pts',(-32.8824457910606,13.3266515427633,
128.067433585776)) ;
#124634 = CARTESIAN_POINT('Ctrl Pts',(-32.8858452579044,13.4226803244344,
128.066343554261)) ;
#124635 = CARTESIAN_POINT('Ctrl Pts',(-11.4002577710971,13.1368456608817,
133.107754941818)) ;
#124636 = CARTESIAN_POINT('Ctrl Pts',(-11.4010320218078,13.130243425216,133.109285763722)) ;
#124637 = CARTESIAN_POINT('Ctrl Pts',(-11.4136660872789,13.0249708380281,
133.134510598115)) ;
#124638 = CARTESIAN_POINT('Ctrl Pts',(-11.4481829779826,12.8263019600079,
133.212368232307)) ;
#124639 = CARTESIAN_POINT('Ctrl Pts',(-11.5209841688121,12.5833994930382,
133.392016397403)) ;
#124640 = CARTESIAN_POINT('Ctrl Pts',(-11.6125279315863,12.399626766211,133.62633286024)) ;
#124641 = CARTESIAN_POINT('Ctrl Pts',(-11.717528730411,12.2890731618772,133.899793229475)) ;
#124642 = CARTESIAN_POINT('Ctrl Pts',(-11.827489308955,12.2602312948732,134.188086633698)) ;
#124643 = CARTESIAN_POINT('Ctrl Pts',(-11.9373256353546,12.3144254522227,
134.475720243095)) ;
#124644 = CARTESIAN_POINT('Ctrl Pts',(-12.0385056054605,12.4480642946114,
134.738200462315)) ;
#124645 = CARTESIAN_POINT('Ctrl Pts',(-12.1250966539337,12.6516399899179,
134.958011136489)) ;
#124646 = CARTESIAN_POINT('Ctrl Pts',(-12.1914055409655,12.9104453038702,
135.118592717814)) ;
#124647 = CARTESIAN_POINT('Ctrl Pts',(-12.2334481989971,13.2058492691314,
135.208295779282)) ;
#124648 = CARTESIAN_POINT('Ctrl Pts',(-12.2490421032075,13.5166185684314,
135.22075896859)) ;
#124649 = CARTESIAN_POINT('Ctrl Pts',(-12.237555231611,13.8224101024019,135.153913230989)) ;
#124650 = CARTESIAN_POINT('Ctrl Pts',(-12.2009286992494,14.0967865746008,
135.013956211633)) ;
#124651 = CARTESIAN_POINT('Ctrl Pts',(-12.1422243505478,14.3244563595429,
134.80933681038)) ;
#124652 = CARTESIAN_POINT('Ctrl Pts',(-12.0664283308639,14.4874742407207,
134.554802811274)) ;
#124653 = CARTESIAN_POINT('Ctrl Pts',(-11.9794532032229,14.5744205093284,
134.267514255778)) ;
#124654 = CARTESIAN_POINT('Ctrl Pts',(-11.8887376179606,14.5784621609188,
133.969391386105)) ;
#124655 = CARTESIAN_POINT('Ctrl Pts',(-11.8014099454108,14.5000469368875,
133.68121510151)) ;
#124656 = CARTESIAN_POINT('Ctrl Pts',(-11.7242121847904,14.344572658684,133.422597490784)) ;
#124657 = CARTESIAN_POINT('Ctrl Pts',(-11.6633872837288,14.1228337492368,
133.211761354524)) ;
#124658 = CARTESIAN_POINT('Ctrl Pts',(-11.6241753304534,13.8501516005036,
133.063988873109)) ;
#124659 = CARTESIAN_POINT('Ctrl Pts',(-11.6102266012163,13.5490422759736,
132.990262219122)) ;
#124660 = CARTESIAN_POINT('Ctrl Pts',(-11.6229330001199,13.2374716075454,
132.994238843195)) ;
#124661 = CARTESIAN_POINT('Ctrl Pts',(-11.6625289722949,12.9386843836575,
133.076700641843)) ;
#124662 = CARTESIAN_POINT('Ctrl Pts',(-11.7263131186438,12.6761376580761,
133.230018897246)) ;
#124663 = CARTESIAN_POINT('Ctrl Pts',(-11.8111790631952,12.4657586342273,
133.444735878277)) ;
#124664 = CARTESIAN_POINT('Ctrl Pts',(-11.911077725081,12.3246285440834,133.703497239924)) ;
#124665 = CARTESIAN_POINT('Ctrl Pts',(-12.0203931142099,12.2619062203987,
133.989607303608)) ;
#124666 = CARTESIAN_POINT('Ctrl Pts',(-12.1308137714884,12.282438847825,134.27917184153)) ;
#124667 = CARTESIAN_POINT('Ctrl Pts',(-12.2365472028457,12.3848777791117,
134.554833667752)) ;
#124668 = CARTESIAN_POINT('Ctrl Pts',(-12.3296655117059,12.5614992054213,
134.79376665016)) ;
#124669 = CARTESIAN_POINT('Ctrl Pts',(-12.4047561054307,12.7995868451149,
134.980026506312)) ;
#124670 = CARTESIAN_POINT('Ctrl Pts',(-12.4572212407894,13.0840300183346,
135.100012153463)) ;
#124671 = CARTESIAN_POINT('Ctrl Pts',(-12.4834787916185,13.3899587420559,
135.143757569566)) ;
#124672 = CARTESIAN_POINT('Ctrl Pts',(-12.4830515741286,13.6996411471026,
135.109395157013)) ;
#124673 = CARTESIAN_POINT('Ctrl Pts',(-12.4562104047493,13.9903747367888,
134.997768916073)) ;
#124674 = CARTESIAN_POINT('Ctrl Pts',(-12.4058859416825,14.2393240379775,
134.817669866416)) ;
#124675 = CARTESIAN_POINT('Ctrl Pts',(-12.3364587321995,14.4298400275378,
134.581797033424)) ;
#124676 = CARTESIAN_POINT('Ctrl Pts',(-12.2533791769935,14.5487685200995,
134.305983497596)) ;
#124677 = CARTESIAN_POINT('Ctrl Pts',(-12.1631769591534,14.5869290465038,
134.009273625762)) ;
#124678 = CARTESIAN_POINT('Ctrl Pts',(-12.0737300908341,14.5417666874379,
133.714933939927)) ;
#124679 = CARTESIAN_POINT('Ctrl Pts',(-11.9913868019149,14.4163781165351,
133.441217765322)) ;
#124680 = CARTESIAN_POINT('Ctrl Pts',(-11.9231930742505,14.2194053123055,
133.20883093906)) ;
#124681 = CARTESIAN_POINT('Ctrl Pts',(-11.8749035853691,13.966643682879,133.034747880334)) ;
#124682 = CARTESIAN_POINT('Ctrl Pts',(-11.8502504010927,13.6737230006816,
132.929549053018)) ;
#124683 = CARTESIAN_POINT('Ctrl Pts',(-11.8520956128137,13.3629182756251,
132.901779915529)) ;
#124684 = CARTESIAN_POINT('Ctrl Pts',(-11.8808821309348,13.0570540996615,
132.952775125275)) ;
#124685 = CARTESIAN_POINT('Ctrl Pts',(-11.935206739513,12.7772473921445,133.078373319798)) ;
#124686 = CARTESIAN_POINT('Ctrl Pts',(-12.0124542548402,12.5427680100154,
133.270768883532)) ;
#124687 = CARTESIAN_POINT('Ctrl Pts',(-12.1065821193436,12.3730788139632,
133.512777848402)) ;
#124688 = CARTESIAN_POINT('Ctrl Pts',(-12.2128884056889,12.2773830368376,
133.790156787178)) ;
#124689 = CARTESIAN_POINT('Ctrl Pts',(-12.3238251084816,12.2641121803462,
134.081112530677)) ;
#124690 = CARTESIAN_POINT('Ctrl Pts',(-12.4322664877904,12.3337583656513,
134.364784452925)) ;
#124691 = CARTESIAN_POINT('Ctrl Pts',(-12.5311880770591,12.4813161327732,
134.620657084876)) ;
#124692 = CARTESIAN_POINT('Ctrl Pts',(-12.6143995811317,12.6966780658121,
134.830578372292)) ;
#124693 = CARTESIAN_POINT('Ctrl Pts',(-12.6763987510127,12.9640585789761,
134.978555464806)) ;
#124694 = CARTESIAN_POINT('Ctrl Pts',(-12.7135158186447,13.263362217281,135.053945116895)) ;
#124695 = CARTESIAN_POINT('Ctrl Pts',(-12.7240587194064,13.5752569117425,
135.051579196554)) ;
#124696 = CARTESIAN_POINT('Ctrl Pts',(-12.7076312662777,13.8766503644376,
134.970371111819)) ;
#124697 = CARTESIAN_POINT('Ctrl Pts',(-12.6665728722074,14.1438627014427,
134.817419676745)) ;
#124698 = CARTESIAN_POINT('Ctrl Pts',(-12.6039948511626,14.3611558948339,
134.601376453978)) ;
#124699 = CARTESIAN_POINT('Ctrl Pts',(-12.525511231779,14.5102071341288,134.338966946009)) ;
#124700 = CARTESIAN_POINT('Ctrl Pts',(-12.437892956187,14.5813677967462,134.050044481287)) ;
#124701 = CARTESIAN_POINT('Ctrl Pts',(-12.3470512850699,14.5701314848988,
133.751485197144)) ;
#124702 = CARTESIAN_POINT('Ctrl Pts',(-12.2606985128047,14.4759918680502,
133.465989914691)) ;
#124703 = CARTESIAN_POINT('Ctrl Pts',(-12.1862330004605,14.3066892261713,
133.21535199468)) ;
#124704 = CARTESIAN_POINT('Ctrl Pts',(-12.1294493909379,14.0751878259722,
133.016480731285)) ;
#124705 = CARTESIAN_POINT('Ctrl Pts',(-12.0947410023423,13.7962286301239,
132.881967768999)) ;
#124706 = CARTESIAN_POINT('Ctrl Pts',(-12.0856036163849,13.489739255107,132.822078592483)) ;
#124707 = CARTESIAN_POINT('Ctrl Pts',(-12.1036908448989,13.1781056591445,
132.841674234956)) ;
#124708 = CARTESIAN_POINT('Ctrl Pts',(-12.1476711989599,12.8871394405402,
132.93727175541)) ;
#124709 = CARTESIAN_POINT('Ctrl Pts',(-12.2160680563488,12.6313542948275,
133.103833575226)) ;
#124710 = CARTESIAN_POINT('Ctrl Pts',(-12.304329738268,12.4333423799844,133.328491824527)) ;
#124711 = CARTESIAN_POINT('Ctrl Pts',(-12.4060576918611,12.3067788244502,
133.592708701729)) ;
#124712 = CARTESIAN_POINT('Ctrl Pts',(-12.5164365286364,12.2592790120272,
133.88187589207)) ;
#124713 = CARTESIAN_POINT('Ctrl Pts',(-12.6267907100765,12.2958890745914,
134.171123224698)) ;
#124714 = CARTESIAN_POINT('Ctrl Pts',(-12.7300880676908,12.412515961838,134.439866942717)) ;
#124715 = CARTESIAN_POINT('Ctrl Pts',(-12.8204242204879,12.6017795181092,
134.670628068448)) ;
#124716 = CARTESIAN_POINT('Ctrl Pts',(-12.8917076442904,12.8508820386888,
134.845636319413)) ;
#124717 = CARTESIAN_POINT('Ctrl Pts',(-12.9391378423724,13.1389626270395,
134.951203029648)) ;
#124718 = CARTESIAN_POINT('Ctrl Pts',(-12.9606749539296,13.4502019217322,
134.980813679307)) ;
#124719 = CARTESIAN_POINT('Ctrl Pts',(-12.9549597016316,13.7571545307035,
134.931066987763)) ;
#124720 = CARTESIAN_POINT('Ctrl Pts',(-12.9237083445955,14.0399279839555,
134.806780374082)) ;
#124721 = CARTESIAN_POINT('Ctrl Pts',(-12.8691654878234,14.2804627639154,
134.614188843193)) ;
#124722 = CARTESIAN_POINT('Ctrl Pts',(-12.796779207288,14.4580430592262,134.369713555185)) ;
#124723 = CARTESIAN_POINT('Ctrl Pts',(-12.7117359750767,14.5623041916472,
134.08810713179)) ;
#124724 = CARTESIAN_POINT('Ctrl Pts',(-12.6214033477903,14.5848738279965,
133.791154683889)) ;
#124725 = CARTESIAN_POINT('Ctrl Pts',(-12.5321103413004,14.5236285085623,
133.496991779123)) ;
#124726 = CARTESIAN_POINT('Ctrl Pts',(-12.4524536540473,14.3842858340258,
133.231308118728)) ;
#124727 = CARTESIAN_POINT('Ctrl Pts',(-12.3875985781014,14.1760036072079,
133.008727211519)) ;
#124728 = CARTESIAN_POINT('Ctrl Pts',(-12.343257008202,13.9123644757914,132.845931511127)) ;
#124729 = CARTESIAN_POINT('Ctrl Pts',(-12.3236960043334,13.6155078278093,
132.755750850139)) ;
#124730 = CARTESIAN_POINT('Ctrl Pts',(-12.3305423757926,13.3048785674805,
132.742701375793)) ;
#124731 = CARTESIAN_POINT('Ctrl Pts',(-12.364391139041,13.0013157661824,132.808379578404)) ;
#124732 = CARTESIAN_POINT('Ctrl Pts',(-12.4232870796455,12.7290184016179,
132.947345432854)) ;
#124733 = CARTESIAN_POINT('Ctrl Pts',(-12.5039453987805,12.5059452399051,
133.149824850825)) ;
#124734 = CARTESIAN_POINT('Ctrl Pts',(-12.601100948694,12.3489356287849,133.400549810363)) ;
#124735 = CARTESIAN_POINT('Ctrl Pts',(-12.7085376350216,12.2685725543234,
133.681330547702)) ;
#124736 = CARTESIAN_POINT('Ctrl Pts',(-12.81992922974,12.2709800429639,133.973502340089)) ;
#124737 = CARTESIAN_POINT('Ctrl Pts',(-12.9269390332323,12.3558597729099,
134.253043661359)) ;
#124738 = CARTESIAN_POINT('Ctrl Pts',(-13.0234674587026,12.5173149603475,
134.501876529553)) ;
#124739 = CARTESIAN_POINT('Ctrl Pts',(-13.1029392456179,12.7436533990505,
134.700909775251)) ;
#124740 = CARTESIAN_POINT('Ctrl Pts',(-13.1604706398527,13.0184391558732,
134.835869526156)) ;
#124741 = CARTESIAN_POINT('Ctrl Pts',(-13.1927351300675,13.3224259864685,
134.896992447974)) ;
#124742 = CARTESIAN_POINT('Ctrl Pts',(-13.1980809728987,13.6337497242247,
134.879467221621)) ;
#124743 = CARTESIAN_POINT('Ctrl Pts',(-13.1768448022821,13.9298382282655,
134.784301593456)) ;
#124744 = CARTESIAN_POINT('Ctrl Pts',(-13.1313657290487,14.189430649662,134.618348210303)) ;
#124745 = CARTESIAN_POINT('Ctrl Pts',(-13.0654522975526,14.394475769408,134.392641880832)) ;
#124746 = CARTESIAN_POINT('Ctrl Pts',(-12.9849210113024,14.5294751555696,
134.124342295431)) ;
#124747 = CARTESIAN_POINT('Ctrl Pts',(-12.8958448031638,14.5857784692471,
133.831003029331)) ;
#124748 = CARTESIAN_POINT('Ctrl Pts',(-12.8052622704107,14.5584757915825,
133.533179544693)) ;
#124749 = CARTESIAN_POINT('Ctrl Pts',(-12.7209347423681,14.4499269428434,
133.253742933785)) ;
#124750 = CARTESIAN_POINT('Ctrl Pts',(-12.6492262981972,14.2678362353556,
133.011138377953)) ;
#124751 = CARTESIAN_POINT('Ctrl Pts',(-12.5961058796925,14.025181457992,132.822834388908)) ;
#124752 = CARTESIAN_POINT('Ctrl Pts',(-12.566099157907,13.7395989373351,132.70207237033)) ;
#124753 = CARTESIAN_POINT('Ctrl Pts',(-12.5620613966533,13.4312396323536,
132.657157630282)) ;
#124754 = CARTESIAN_POINT('Ctrl Pts',(-12.5849599127162,13.1225497358479,
132.690961347731)) ;
#124755 = CARTESIAN_POINT('Ctrl Pts',(-12.6341066221525,12.8344723691042,
132.801333767966)) ;
#124756 = CARTESIAN_POINT('Ctrl Pts',(-12.7064275143261,12.5894057797878,
132.97950088557)) ;
#124757 = CARTESIAN_POINT('Ctrl Pts',(-12.7976132379566,12.403866954954,133.212753563123)) ;
#124758 = CARTESIAN_POINT('Ctrl Pts',(-12.9017755510911,12.2913271395126,
133.483934150059)) ;
#124759 = CARTESIAN_POINT('Ctrl Pts',(-13.0125233870004,12.2598830910024,
133.774265375283)) ;
#124760 = CARTESIAN_POINT('Ctrl Pts',(-13.1219338101741,12.3117248800856,
134.060824044522)) ;
#124761 = CARTESIAN_POINT('Ctrl Pts',(-13.2236212395332,12.4432581969561,
134.3247309762)) ;
#124762 = CARTESIAN_POINT('Ctrl Pts',(-13.3105761021659,12.6447768479475,
134.545654875861)) ;
#124763 = CARTESIAN_POINT('Ctrl Pts',(-13.3775463734392,12.9020427023331,
134.708180411592)) ;
#124764 = CARTESIAN_POINT('Ctrl Pts',(-13.4203792864058,13.1969220955149,
134.800163305388)) ;
#124765 = CARTESIAN_POINT('Ctrl Pts',(-13.4367503191474,13.5073634201221,
134.814917250719)) ;
#124766 = CARTESIAN_POINT('Ctrl Pts',(-13.4260632417067,13.8135028677167,
134.750425039199)) ;
#124767 = CARTESIAN_POINT('Ctrl Pts',(-13.3902019475775,14.0890635163078,
134.612711315212)) ;
#124768 = CARTESIAN_POINT('Ctrl Pts',(-13.3317903671586,14.3192685446141,
134.408803368418)) ;
#124769 = CARTESIAN_POINT('Ctrl Pts',(-13.2566727359362,14.4835637983032,
134.156382324995)) ;
#124770 = CARTESIAN_POINT('Ctrl Pts',(-13.169938469823,14.5730188285823,133.869793548611)) ;
#124771 = CARTESIAN_POINT('Ctrl Pts',(-13.0792140349077,14.5795967764284,
133.571640925124)) ;
#124772 = CARTESIAN_POINT('Ctrl Pts',(-12.9915123363953,14.5032853646564,
133.282297922924)) ;
#124773 = CARTESIAN_POINT('Ctrl Pts',(-12.9140022949989,14.3501151249434,
133.022810830752)) ;
#124774 = CARTESIAN_POINT('Ctrl Pts',(-12.8524828347806,14.1289951799062,
132.809814591485)) ;
#124775 = CARTESIAN_POINT('Ctrl Pts',(-12.812909471201,13.8600883343583,132.661298344278)) ;
#124776 = CARTESIAN_POINT('Ctrl Pts',(-12.7979838300487,13.5571075891159,
132.584435996641)) ;
#124777 = CARTESIAN_POINT('Ctrl Pts',(-12.8100524681606,13.246144038551,132.586620648894)) ;
#124778 = CARTESIAN_POINT('Ctrl Pts',(-12.8486585081772,12.9474784018938,
132.666294839717)) ;
#124779 = CARTESIAN_POINT('Ctrl Pts',(-12.9123435540383,12.6818049804595,
132.819067818709)) ;
#124780 = CARTESIAN_POINT('Ctrl Pts',(-12.9960885885724,12.4713261551404,
133.030763914884)) ;
#124781 = CARTESIAN_POINT('Ctrl Pts',(-13.0961110849497,12.3273775060339,
133.28971686147)) ;
#124782 = CARTESIAN_POINT('Ctrl Pts',(-13.2046537208031,12.2625380401702,
133.573765385136)) ;
#124783 = CARTESIAN_POINT('Ctrl Pts',(-13.3161047474788,12.2810707697993,
133.866034649765)) ;
#124784 = CARTESIAN_POINT('Ctrl Pts',(-13.4209550321827,12.3803129449242,
134.139476431641)) ;
#124785 = CARTESIAN_POINT('Ctrl Pts',(-13.5151074581699,12.5556239471542,
134.381234906763)) ;
#124786 = CARTESIAN_POINT('Ctrl Pts',(-13.5905152917745,12.7914917481058,
134.56853383512)) ;
#124787 = CARTESIAN_POINT('Ctrl Pts',(-13.6438208480912,13.0750410185669,
134.690941087749)) ;
#124788 = CARTESIAN_POINT('Ctrl Pts',(-13.6708818850032,13.3808908825506,
134.737002821677)) ;
#124789 = CARTESIAN_POINT('Ctrl Pts',(-13.6712113749413,13.6908805105498,
134.704840536306)) ;
#124790 = CARTESIAN_POINT('Ctrl Pts',(-13.6451962539586,13.9819858860809,
134.595693722298)) ;
#124791 = CARTESIAN_POINT('Ctrl Pts',(-13.5953602405429,14.2331023170552,
134.416922555225)) ;
#124792 = CARTESIAN_POINT('Ctrl Pts',(-13.5264879005436,14.425373738482,134.18270881116)) ;
#124793 = CARTESIAN_POINT('Ctrl Pts',(-13.4431809018768,14.5469025467051,
133.906032348469)) ;
#124794 = CARTESIAN_POINT('Ctrl Pts',(-13.3536808661597,14.5868798002751,
133.611604960804)) ;
#124795 = CARTESIAN_POINT('Ctrl Pts',(-13.2640066674077,14.544243012127,133.316555537026)) ;
#124796 = CARTESIAN_POINT('Ctrl Pts',(-13.1814521156651,14.4211466682183,
133.042262184532)) ;
#124797 = CARTESIAN_POINT('Ctrl Pts',(-13.1127573154354,14.2262607668007,
132.808422365474)) ;
#124798 = CARTESIAN_POINT('Ctrl Pts',(-13.0637294316636,13.9744157440355,
132.632118382732)) ;
#124799 = CARTESIAN_POINT('Ctrl Pts',(-13.0384131550304,13.6824769956245,
132.525002593695)) ;
#124800 = CARTESIAN_POINT('Ctrl Pts',(-13.0393827410548,13.3726811075526,
132.494761352875)) ;
#124801 = CARTESIAN_POINT('Ctrl Pts',(-13.0676131106458,13.0644552653701,
132.54392030028)) ;
#124802 = CARTESIAN_POINT('Ctrl Pts',(-13.121061409599,12.7851437456734,132.667125642549)) ;
#124803 = CARTESIAN_POINT('Ctrl Pts',(-13.1974519715877,12.5493640024945,
132.85708998106)) ;
#124804 = CARTESIAN_POINT('Ctrl Pts',(-13.2913743910714,12.376970726474,133.098407984603)) ;
#124805 = CARTESIAN_POINT('Ctrl Pts',(-13.3977315690652,12.2789142943649,
133.375849754409)) ;
#124806 = CARTESIAN_POINT('Ctrl Pts',(-13.5083089279773,12.2633331335236,
133.665852727719)) ;
#124807 = CARTESIAN_POINT('Ctrl Pts',(-13.6171709080123,12.3306602868788,
133.950680512518)) ;
#124808 = CARTESIAN_POINT('Ctrl Pts',(-13.716558237696,12.4766203405944,134.20786333325)) ;
#124809 = CARTESIAN_POINT('Ctrl Pts',(-13.7998719371381,12.6891737116268,
134.418250852531)) ;
#124810 = CARTESIAN_POINT('Ctrl Pts',(-13.8626642883641,12.9552556025245,
134.568527949207)) ;
#124811 = CARTESIAN_POINT('Ctrl Pts',(-13.9006336626054,13.2547271279824,
134.646319603981)) ;
#124812 = CARTESIAN_POINT('Ctrl Pts',(-13.9118864628166,13.5662747472623,
134.646059940436)) ;
#124813 = CARTESIAN_POINT('Ctrl Pts',(-13.8963623296496,13.8673047437589,
134.567609313136)) ;
#124814 = CARTESIAN_POINT('Ctrl Pts',(-13.8558569907757,14.1368397654386,
134.416143585266)) ;
#124815 = CARTESIAN_POINT('Ctrl Pts',(-13.7940607472378,14.3550474854522,
134.202509973235)) ;
#124816 = CARTESIAN_POINT('Ctrl Pts',(-13.7160248113303,14.5066809969925,
133.941403361426)) ;
#124817 = CARTESIAN_POINT('Ctrl Pts',(-13.6281511120074,14.5805550021418,
133.651572184232)) ;
#124818 = CARTESIAN_POINT('Ctrl Pts',(-13.5375371319342,14.5715434154247,
133.353768334661)) ;
#124819 = CARTESIAN_POINT('Ctrl Pts',(-13.45124859715,14.4804614253832,133.068587808668)) ;
#124820 = CARTESIAN_POINT('Ctrl Pts',(-13.37603363823,14.3129344322758,132.815646261363)) ;
#124821 = CARTESIAN_POINT('Ctrl Pts',(-13.3185466362034,14.0824719348205,
132.61464582826)) ;
#124822 = CARTESIAN_POINT('Ctrl Pts',(-13.2831865687033,13.8045959520742,
132.478235291779)) ;
#124823 = CARTESIAN_POINT('Ctrl Pts',(-13.2732886080672,13.4994871825109,
132.416220120997)) ;
#124824 = CARTESIAN_POINT('Ctrl Pts',(-13.2904782460621,13.1877258357311,
132.4332010356)) ;
#124825 = CARTESIAN_POINT('Ctrl Pts',(-13.3338717484347,12.8947281462995,
132.526953391422)) ;
#124826 = CARTESIAN_POINT('Ctrl Pts',(-13.4017873141061,12.6375710279023,
132.692078445121)) ;
#124827 = CARTESIAN_POINT('Ctrl Pts',(-13.4890204567564,12.4386468610117,
132.91391883166)) ;
#124828 = CARTESIAN_POINT('Ctrl Pts',(-13.5909900935397,12.3091460957756,
133.178653315814)) ;
#124829 = CARTESIAN_POINT('Ctrl Pts',(-13.7006170362624,12.2596124823544,
133.465818195012)) ;
#124830 = CARTESIAN_POINT('Ctrl Pts',(-13.8113185228843,12.2934287608505,
133.756004819139)) ;
#124831 = CARTESIAN_POINT('Ctrl Pts',(-13.915353328685,12.4085128327331,134.026758002108)) ;
#124832 = CARTESIAN_POINT('Ctrl Pts',(-14.0058487547682,12.5956557289105,
134.25806721356)) ;
#124833 = CARTESIAN_POINT('Ctrl Pts',(-14.0775354249195,12.8419007225992,
134.434408810845)) ;
#124834 = CARTESIAN_POINT('Ctrl Pts',(-14.1259869919832,13.1310174961036,
134.542734109053)) ;
#124835 = CARTESIAN_POINT('Ctrl Pts',(-14.1481532280157,13.4394174357417,
134.574460881878)) ;
#124836 = CARTESIAN_POINT('Ctrl Pts',(-14.1433213153389,13.7489280911395,
134.52706348914)) ;
#124837 = CARTESIAN_POINT('Ctrl Pts',(-14.1126273341243,14.0326636377924,
134.4043884176)) ;
#124838 = CARTESIAN_POINT('Ctrl Pts',(-14.0589544553989,14.2739040852335,
134.214471649233)) ;
#124839 = CARTESIAN_POINT('Ctrl Pts',(-13.9866513654702,14.4542739196418,
133.970073178127)) ;
#124840 = CARTESIAN_POINT('Ctrl Pts',(-13.9022431575821,14.5602989728585,
133.69047622448)) ;
#124841 = CARTESIAN_POINT('Ctrl Pts',(-13.8116472296482,14.5853165149043,
133.392628115289)) ;
#124842 = CARTESIAN_POINT('Ctrl Pts',(-13.7227715761924,14.5269566975762,
133.099903849994)) ;
#124843 = CARTESIAN_POINT('Ctrl Pts',(-13.6421710441629,14.3891797557674,
132.831239376946)) ;
#124844 = CARTESIAN_POINT('Ctrl Pts',(-13.5768120757702,14.1817902541555,
132.607121636432)) ;
#124845 = CARTESIAN_POINT('Ctrl Pts',(-13.5321752968255,13.9219441435514,
132.443766715308)) ;
#124846 = CARTESIAN_POINT('Ctrl Pts',(-13.5116468125809,13.6244332360091,
132.350588803698)) ;
#124847 = CARTESIAN_POINT('Ctrl Pts',(-13.5177395880814,13.3138307533241,
132.335338987358)) ;
#124848 = CARTESIAN_POINT('Ctrl Pts',(-13.550960796519,13.0089906490168,132.399097001905)) ;
#124849 = CARTESIAN_POINT('Ctrl Pts',(-13.6089629814311,12.7367004546504,
132.535589377863)) ;
#124850 = CARTESIAN_POINT('Ctrl Pts',(-13.6890168410449,12.5117902226442,
132.736297036857)) ;
#124851 = CARTESIAN_POINT('Ctrl Pts',(-13.7857765994093,12.3525055718321,
132.985859011256)) ;
#124852 = CARTESIAN_POINT('Ctrl Pts',(-13.8934707756066,12.2695603422194,
133.26725204525)) ;
#124853 = CARTESIAN_POINT('Ctrl Pts',(-14.0046967664786,12.2698997587057,
133.55899053355)) ;
#124854 = CARTESIAN_POINT('Ctrl Pts',(-14.1116278789902,12.3521640390818,
133.838391990892)) ;
#124855 = CARTESIAN_POINT('Ctrl Pts',(-14.2086596235602,12.5116415634716,
134.088662656359)) ;
#124856 = CARTESIAN_POINT('Ctrl Pts',(-14.2886301094502,12.7360069700772,
134.289191940705)) ;
#124857 = CARTESIAN_POINT('Ctrl Pts',(-14.3469357043129,13.0100796293743,
134.426358261043)) ;
#124858 = CARTESIAN_POINT('Ctrl Pts',(-14.3799244113915,13.3126253374921,
134.489695495591)) ;
#124859 = CARTESIAN_POINT('Ctrl Pts',(-14.3860830172785,13.6254715524663,
134.474389220875)) ;
#124860 = CARTESIAN_POINT('Ctrl Pts',(-14.3656426582198,13.9212365418522,
134.381670680832)) ;
#124861 = CARTESIAN_POINT('Ctrl Pts',(-14.3207442896342,14.1826934673073,
134.217342153918)) ;
#124862 = CARTESIAN_POINT('Ctrl Pts',(-14.2556054285751,14.3889686584202,
133.994016051553)) ;
#124863 = CARTESIAN_POINT('Ctrl Pts',(-14.1749150301037,14.5271450156122,
133.725037501823)) ;
#124864 = CARTESIAN_POINT('Ctrl Pts',(-14.0858847391717,14.5852339348323,
133.431810575258)) ;
#124865 = CARTESIAN_POINT('Ctrl Pts',(-13.995836417164,14.5605427661762,133.135766593463)) ;
#124866 = CARTESIAN_POINT('Ctrl Pts',(-13.9109761751291,14.4541441537073,
132.854676254093)) ;
#124867 = CARTESIAN_POINT('Ctrl Pts',(-13.8388670781715,14.2740963281162,
132.610925952439)) ;
#124868 = CARTESIAN_POINT('Ctrl Pts',(-13.7850008698074,14.0323112919108,
132.420355351968)) ;
#124869 = CARTESIAN_POINT('Ctrl Pts',(-13.75439702107,13.747634010638,132.297856801284)) ;
#124870 = CARTESIAN_POINT('Ctrl Pts',(-13.7495551212371,13.4408490944308,
132.250724773907)) ;
#124871 = CARTESIAN_POINT('Ctrl Pts',(-13.7718087995071,13.1304291630284,
132.282485369413)) ;
#124872 = CARTESIAN_POINT('Ctrl Pts',(-13.8200527246112,12.8426172833002,
132.390360822731)) ;
#124873 = CARTESIAN_POINT('Ctrl Pts',(-13.8920711083226,12.5951022439345,
132.567502086748)) ;
#124874 = CARTESIAN_POINT('Ctrl Pts',(-13.9823448757499,12.4086451367459,
132.798263093832)) ;
#124875 = CARTESIAN_POINT('Ctrl Pts',(-14.0864872492279,12.2933533526165,
133.069289241896)) ;
#124876 = CARTESIAN_POINT('Ctrl Pts',(-14.1971250254784,12.2596356642452,
133.359312878413)) ;
#124877 = CARTESIAN_POINT('Ctrl Pts',(-14.3066070487481,12.3091205579985,
133.646092913872)) ;
#124878 = CARTESIAN_POINT('Ctrl Pts',(-14.4084397056733,12.4379929419073,
133.910495450968)) ;
#124879 = CARTESIAN_POINT('Ctrl Pts',(-14.4963291891085,12.6386445208212,
134.133986510367)) ;
#124880 = CARTESIAN_POINT('Ctrl Pts',(-14.5637307355296,12.8942395319149,
134.297835385292)) ;
#124881 = CARTESIAN_POINT('Ctrl Pts',(-14.6072585432434,13.1876524015431,
134.391918163003)) ;
#124882 = CARTESIAN_POINT('Ctrl Pts',(-14.6244317780042,13.4984175352415,
134.408961571031)) ;
#124883 = CARTESIAN_POINT('Ctrl Pts',(-14.6145964259596,13.804322978022,134.347044191526)) ;
#124884 = CARTESIAN_POINT('Ctrl Pts',(-14.5792218548473,14.0825044690989,
134.210565926119)) ;
#124885 = CARTESIAN_POINT('Ctrl Pts',(-14.5215034218389,14.3134151939565,
134.008790285794)) ;
#124886 = CARTESIAN_POINT('Ctrl Pts',(-14.4467983753446,14.4799820430956,
133.757558503687)) ;
#124887 = CARTESIAN_POINT('Ctrl Pts',(-14.3599545208039,14.5717629111611,
133.470532635478)) ;
#124888 = CARTESIAN_POINT('Ctrl Pts',(-14.2697026757989,14.5804902345133,
133.173926231809)) ;
#124889 = CARTESIAN_POINT('Ctrl Pts',(-14.1818550312755,14.5068426017295,
132.884179222822)) ;
#124890 = CARTESIAN_POINT('Ctrl Pts',(-14.1038707278137,14.3556215142155,
132.62326810925)) ;
#124891 = CARTESIAN_POINT('Ctrl Pts',(-14.0418273324944,14.1365915328991,
132.408782119764)) ;
#124892 = CARTESIAN_POINT('Ctrl Pts',(-14.0014978593324,13.8680779330351,
132.25795920505)) ;
#124893 = CARTESIAN_POINT('Ctrl Pts',(-13.9858123788647,13.567186800724,132.1790395569)) ;
#124894 = CARTESIAN_POINT('Ctrl Pts',(-13.9971900795798,13.2537545062593,
132.178943151311)) ;
#124895 = CARTESIAN_POINT('Ctrl Pts',(-14.0349672123987,12.9561224404112,
132.256375223925)) ;
#124896 = CARTESIAN_POINT('Ctrl Pts',(-14.0977176900152,12.6895769772328,
132.406492249292)) ;
#124897 = CARTESIAN_POINT('Ctrl Pts',(-14.1811824094918,12.4765148457442,
132.617258389176)) ;
#124898 = CARTESIAN_POINT('Ctrl Pts',(-14.2808752566479,12.3303992852147,
132.875241621594)) ;
#124899 = CARTESIAN_POINT('Ctrl Pts',(-14.3893361764667,12.2633426599666,
133.159025189874)) ;
#124900 = CARTESIAN_POINT('Ctrl Pts',(-14.5002482335499,12.279103982185,133.44989801271)) ;
#124901 = CARTESIAN_POINT('Ctrl Pts',(-14.606036142801,12.3764767576561,133.725867717232)) ;
#124902 = CARTESIAN_POINT('Ctrl Pts',(-14.7005487610914,12.5500289101503,
133.968688363446)) ;
#124903 = CARTESIAN_POINT('Ctrl Pts',(-14.7763877253057,12.7839578561676,
134.157302063182)) ;
#124904 = CARTESIAN_POINT('Ctrl Pts',(-14.8303556214475,13.0658041228342,
134.281713139573)) ;
#124905 = CARTESIAN_POINT('Ctrl Pts',(-14.8583242280902,13.3726170647806,
134.330277268878)) ;
#124906 = CARTESIAN_POINT('Ctrl Pts',(-14.8593033695257,13.6826397531364,
134.300029063359)) ;
#124907 = CARTESIAN_POINT('Ctrl Pts',(-14.8341682762792,13.9734160289762,
134.193592262512)) ;
#124908 = CARTESIAN_POINT('Ctrl Pts',(-14.7848225301107,14.2269288377743,
134.01613594009)) ;
#124909 = CARTESIAN_POINT('Ctrl Pts',(-14.7165117945592,14.4205112274409,
133.783623816956)) ;
#124910 = CARTESIAN_POINT('Ctrl Pts',(-14.6339676590262,14.5441065971854,
133.509333914104)) ;
#124911 = CARTESIAN_POINT('Ctrl Pts',(-14.543930379516,14.5870792664814,133.213098404156)) ;
#124912 = CARTESIAN_POINT('Ctrl Pts',(-14.4540579265701,14.5462510463569,
132.917427016041)) ;
#124913 = CARTESIAN_POINT('Ctrl Pts',(-14.371611013546,14.426108976537,132.643620532443)) ;
#124914 = CARTESIAN_POINT('Ctrl Pts',(-14.3020392766499,14.2320089292168,
132.40702833977)) ;
#124915 = CARTESIAN_POINT('Ctrl Pts',(-14.2526185482894,13.9821034896837,
132.229676391051)) ;
#124916 = CARTESIAN_POINT('Ctrl Pts',(-14.2265818489062,13.6914860951574,
132.120501165582)) ;
#124917 = CARTESIAN_POINT('Ctrl Pts',(-14.2267429244149,13.3820426901867,
132.087911578203)) ;
#124918 = CARTESIAN_POINT('Ctrl Pts',(-14.254191395465,13.0731824495073,132.134765071221)) ;
#124919 = CARTESIAN_POINT('Ctrl Pts',(-14.3069443025686,12.7927891220342,
132.255932871511)) ;
#124920 = CARTESIAN_POINT('Ctrl Pts',(-14.3827474169739,12.5553086793863,
132.444172542437)) ;
#124921 = CARTESIAN_POINT('Ctrl Pts',(-14.4764049521844,12.3807971317929,
132.684665215156)) ;
#124922 = CARTESIAN_POINT('Ctrl Pts',(-14.5821181703053,12.2807361314401,
132.960349357715)) ;
#124923 = CARTESIAN_POINT('Ctrl Pts',(-14.6930022007284,12.2625961547027,
133.25114070724)) ;
#124924 = CARTESIAN_POINT('Ctrl Pts',(-14.8018555982343,12.3275534841213,
133.535998308902)) ;
#124925 = CARTESIAN_POINT('Ctrl Pts',(-14.9016022738294,12.4713200428819,
133.794229183378)) ;
#124926 = CARTESIAN_POINT('Ctrl Pts',(-14.9854766671218,12.6818354528321,
134.006273987192)) ;
#124927 = CARTESIAN_POINT('Ctrl Pts',(-15.0492924045249,12.9488696704077,
134.159286266937)) ;
#124928 = CARTESIAN_POINT('Ctrl Pts',(-15.0875838966062,13.2449965342222,
134.238327513091)) ;
#124929 = CARTESIAN_POINT('Ctrl Pts',(-15.0997594597476,13.5577147943103,
134.240627823641)) ;
#124930 = CARTESIAN_POINT('Ctrl Pts',(-15.084934557853,13.85913805832,134.164243465792)) ;
#124931 = CARTESIAN_POINT('Ctrl Pts',(-15.045045788871,14.1301670031634,134.014537631445)) ;
#124932 = CARTESIAN_POINT('Ctrl Pts',(-14.9837834759939,14.3498259886228,
133.802481832815)) ;
#124933 = CARTESIAN_POINT('Ctrl Pts',(-14.9062566288333,14.5033075932482,
133.542915911526)) ;
#124934 = CARTESIAN_POINT('Ctrl Pts',(-14.8185287898435,14.5795881010438,
133.253492977493)) ;
#124935 = CARTESIAN_POINT('Ctrl Pts',(-14.7278599526965,14.5729975043218,
132.95551789938)) ;
#124936 = CARTESIAN_POINT('Ctrl Pts',(-14.6411058259546,14.4837968036715,
132.668880234287)) ;
#124937 = CARTESIAN_POINT('Ctrl Pts',(-14.5656171298555,14.3181445279312,
132.415171042367)) ;
#124938 = CARTESIAN_POINT('Ctrl Pts',(-14.5077297104301,14.0900336140832,
132.213103849881)) ;
#124939 = CARTESIAN_POINT('Ctrl Pts',(-14.4715993847153,13.812578673719,132.074363369864)) ;
#124940 = CARTESIAN_POINT('Ctrl Pts',(-14.4610127677944,13.5087142835403,
132.010421751901)) ;
#124941 = CARTESIAN_POINT('Ctrl Pts',(-14.4773187825163,13.1970641651478,
132.024851943105)) ;
#124942 = CARTESIAN_POINT('Ctrl Pts',(-14.5201391181318,12.9023258221912,
132.116819737304)) ;
#124943 = CARTESIAN_POINT('Ctrl Pts',(-14.5872047154943,12.644685125118,132.279571832042)) ;
#124944 = CARTESIAN_POINT('Ctrl Pts',(-14.6739254344846,12.4436426605292,
132.499899000355)) ;
#124945 = CARTESIAN_POINT('Ctrl Pts',(-14.7756943865195,12.3118006025232,
132.76400568983)) ;
#124946 = CARTESIAN_POINT('Ctrl Pts',(-14.8852228559566,12.2597626712743,
133.050877142863)) ;
#124947 = CARTESIAN_POINT('Ctrl Pts',(-14.996405412822,12.291703918078,133.342339118856)) ;
#124948 = CARTESIAN_POINT('Ctrl Pts',(-15.0999158484911,12.4035190278675,
133.611829800801)) ;
#124949 = CARTESIAN_POINT('Ctrl Pts',(-15.1916464629765,12.5902948833878,
133.846460292102)) ;
#124950 = CARTESIAN_POINT('Ctrl Pts',(-15.263459595405,12.8337324563932,134.023377894843)) ;
#124951 = CARTESIAN_POINT('Ctrl Pts',(-15.3129209886316,13.1235886445067,
134.134455736189)) ;
#124952 = CARTESIAN_POINT('Ctrl Pts',(-15.3355967699743,13.4302519414742,
134.167832537199)) ;
#124953 = CARTESIAN_POINT('Ctrl Pts',(-15.3317353809439,13.7390104772614,
134.123396838734)) ;
#124954 = CARTESIAN_POINT('Ctrl Pts',(-15.3014976225916,14.0260062302898,
134.001786192092)) ;
#124955 = CARTESIAN_POINT('Ctrl Pts',(-15.2486500083372,14.267226902407,133.814466538076)) ;
#124956 = CARTESIAN_POINT('Ctrl Pts',(-15.1769102109966,14.4498458952908,
133.571722166596)) ;
#124957 = CARTESIAN_POINT('Ctrl Pts',(-15.092355680759,14.5586319352592,133.291541367095)) ;
#124958 = CARTESIAN_POINT('Ctrl Pts',(-15.0017957168739,14.5856242088894,
132.993790062797)) ;
#124959 = CARTESIAN_POINT('Ctrl Pts',(-14.913162148146,14.5299078181027,132.701917946807)) ;
#124960 = CARTESIAN_POINT('Ctrl Pts',(-14.8320122022859,14.3940107606991,
132.431562888425)) ;
#124961 = CARTESIAN_POINT('Ctrl Pts',(-14.766278636578,14.1888420463645,132.206424468802)) ;
#124962 = CARTESIAN_POINT('Ctrl Pts',(-14.7209263709597,13.9299824320437,
132.040931181505)) ;
#124963 = CARTESIAN_POINT('Ctrl Pts',(-14.6996678155027,13.6339608398866,
131.94570431671)) ;
#124964 = CARTESIAN_POINT('Ctrl Pts',(-14.7049859859979,13.3227158538243,
131.928107883363)) ;
#124965 = CARTESIAN_POINT('Ctrl Pts',(-14.737248964863,13.018724359071,131.989222699374)) ;
#124966 = CARTESIAN_POINT('Ctrl Pts',(-14.794605691487,12.7442183705068,132.123727500233)) ;
#124967 = CARTESIAN_POINT('Ctrl Pts',(-14.8745544931001,12.5167188464288,
132.323966018835)) ;
#124968 = CARTESIAN_POINT('Ctrl Pts',(-14.9704908580808,12.3563385813199,
132.571280103058)) ;
#124969 = CARTESIAN_POINT('Ctrl Pts',(-15.0777402856303,12.2709228201269,
132.851435182846)) ;
#124970 = CARTESIAN_POINT('Ctrl Pts',(-15.1890905041819,12.2686101214329,
133.143498939687)) ;
#124971 = CARTESIAN_POINT('Ctrl Pts',(-15.296477362581,12.3485946759632,133.42416126715)) ;
#124972 = CARTESIAN_POINT('Ctrl Pts',(-15.3941920414611,12.5068357117029,
133.676309304964)) ;
#124973 = CARTESIAN_POINT('Ctrl Pts',(-15.4742237583938,12.7283302241023,
133.877209325191)) ;
#124974 = CARTESIAN_POINT('Ctrl Pts',(-15.5333688655842,13.0013551128606,
134.016794223351)) ;
#124975 = CARTESIAN_POINT('Ctrl Pts',(-15.5671263312359,13.3039532563625,
134.082313844199)) ;
#124976 = CARTESIAN_POINT('Ctrl Pts',(-15.5741033716375,13.6158509275634,
134.069512761149)) ;
#124977 = CARTESIAN_POINT('Ctrl Pts',(-15.554290548579,13.9138456123568,133.978453644798)) ;
#124978 = CARTESIAN_POINT('Ctrl Pts',(-15.510233046302,14.1752853033959,133.816745546828)) ;
#124979 = CARTESIAN_POINT('Ctrl Pts',(-15.4455219248175,14.3839669210711,
133.594594016653)) ;
#124980 = CARTESIAN_POINT('Ctrl Pts',(-15.3652594931835,14.5240578631267,
133.326904321361)) ;
#124981 = CARTESIAN_POINT('Ctrl Pts',(-15.2764638116133,14.584818935146,133.034389619939)) ;
#124982 = CARTESIAN_POINT('Ctrl Pts',(-15.1857623337452,14.5621167265827,
132.736215402154)) ;
#124983 = CARTESIAN_POINT('Ctrl Pts',(-15.1011943241471,14.4583966229727,
132.456187822001)) ;
#124984 = CARTESIAN_POINT('Ctrl Pts',(-15.0285434791858,14.2803903749363,
132.210827677929)) ;
#124985 = CARTESIAN_POINT('Ctrl Pts',(-14.9741792799019,14.0406559377366,
132.018869665459)) ;
#124986 = CARTESIAN_POINT('Ctrl Pts',(-14.9427029763615,13.7571590105316,
131.893825492125)) ;
#124987 = CARTESIAN_POINT('Ctrl Pts',(-14.9371721138493,13.4483332581187,
131.844421725102)) ;
#124988 = CARTESIAN_POINT('Ctrl Pts',(-14.9584157245602,13.140610392606,131.873559202715)) ;
#124989 = CARTESIAN_POINT('Ctrl Pts',(-15.006332152192,12.8492377200964,131.980169977206)) ;
#124990 = CARTESIAN_POINT('Ctrl Pts',(-15.0773325730432,12.6021186062381,
132.154566622699)) ;
#124991 = CARTESIAN_POINT('Ctrl Pts',(-15.1672005368303,12.4130744443633,
132.384082222969)) ;
#124992 = CARTESIAN_POINT('Ctrl Pts',(-15.2714613998002,12.2953575363629,
132.655337022259)) ;
#124993 = CARTESIAN_POINT('Ctrl Pts',(-15.3815448297722,12.259540004683,132.943880410845)) ;
#124994 = CARTESIAN_POINT('Ctrl Pts',(-15.4912456386987,12.3063152851138,
133.231278361687)) ;
#124995 = CARTESIAN_POINT('Ctrl Pts',(-15.5939663384943,12.4341408318063,
133.498072171221)) ;
#124996 = CARTESIAN_POINT('Ctrl Pts',(-15.6816501279818,12.6316134862806,
133.721213083362)) ;
#124997 = CARTESIAN_POINT('Ctrl Pts',(-15.7499030351048,12.8861350461837,
133.887481728305)) ;
#124998 = CARTESIAN_POINT('Ctrl Pts',(-15.7942059688853,13.179213941093,133.98378356009)) ;
#124999 = CARTESIAN_POINT('Ctrl Pts',(-15.8121296747286,13.4905687882747,
134.002938802132)) ;
#125000 = CARTESIAN_POINT('Ctrl Pts',(-15.8029511716908,13.7964604527636,
133.942985156857)) ;
#125001 = CARTESIAN_POINT('Ctrl Pts',(-15.7684329938962,14.0743848720617,
133.809160750471)) ;
#125002 = CARTESIAN_POINT('Ctrl Pts',(-15.7114766984834,14.3070163090694,
133.609649645911)) ;
#125003 = CARTESIAN_POINT('Ctrl Pts',(-15.6367201521411,14.4764518819419,
133.358067464935)) ;
#125004 = CARTESIAN_POINT('Ctrl Pts',(-15.550868483393,14.5698501931718,133.074231883872)) ;
#125005 = CARTESIAN_POINT('Ctrl Pts',(-15.4601765122184,14.5816111155488,
132.776162534956)) ;
#125006 = CARTESIAN_POINT('Ctrl Pts',(-15.3718833098534,14.5098991366122,
132.48501685371)) ;
#125007 = CARTESIAN_POINT('Ctrl Pts',(-15.2934983361019,14.3604029768198,
132.222904357616)) ;
#125008 = CARTESIAN_POINT('Ctrl Pts',(-15.2311225152342,14.1435656071336,
132.007535897725)) ;
#125009 = CARTESIAN_POINT('Ctrl Pts',(-15.1900514509045,13.8762645151226,
131.854539360844)) ;
#125010 = CARTESIAN_POINT('Ctrl Pts',(-15.173721426937,13.5746433207973,131.77359639711)) ;
#125011 = CARTESIAN_POINT('Ctrl Pts',(-15.1841222852425,13.2647985797715,
131.771035600231)) ;
#125012 = CARTESIAN_POINT('Ctrl Pts',(-15.2213411645311,12.9638355607027,
131.846545765161)) ;
#125013 = CARTESIAN_POINT('Ctrl Pts',(-15.2833515972968,12.6967406329269,
131.994582271641)) ;
#125014 = CARTESIAN_POINT('Ctrl Pts',(-15.3664540430693,12.4815166817384,
132.204216153634)) ;
#125015 = CARTESIAN_POINT('Ctrl Pts',(-15.465420080429,12.3337893264045,132.460199514638)) ;
#125016 = CARTESIAN_POINT('Ctrl Pts',(-15.5739645042299,12.2640797848313,
132.744142825912)) ;
#125017 = CARTESIAN_POINT('Ctrl Pts',(-15.6847782481481,12.2774691635847,
133.034771337634)) ;
#125018 = CARTESIAN_POINT('Ctrl Pts',(-15.7908127641154,12.3724670755757,
133.311459425319)) ;
#125019 = CARTESIAN_POINT('Ctrl Pts',(-15.8857243578106,12.5437674769879,
133.555469238688)) ;
#125020 = CARTESIAN_POINT('Ctrl Pts',(-15.9622886843345,12.7765747381498,
133.746136071001)) ;
#125021 = CARTESIAN_POINT('Ctrl Pts',(-16.0168222647185,13.056442748956,133.872306944188)) ;
#125022 = CARTESIAN_POINT('Ctrl Pts',(-16.0456475901748,13.3632374806636,
133.923318739201)) ;
#125023 = CARTESIAN_POINT('Ctrl Pts',(-16.0475237873609,13.6730055446753,
133.895754018573)) ;
#125024 = CARTESIAN_POINT('Ctrl Pts',(-16.0227887843929,13.9671153512335,
133.790179973524)) ;
#125025 = CARTESIAN_POINT('Ctrl Pts',(-15.9745831485738,14.2192391234479,
133.616422532478)) ;
#125026 = CARTESIAN_POINT('Ctrl Pts',(-15.9062934997798,14.4164802375927,
133.3837039056)) ;
#125027 = CARTESIAN_POINT('Ctrl Pts',(-15.8242106414318,14.5415580398573,
133.110853663732)) ;
#125028 = CARTESIAN_POINT('Ctrl Pts',(-15.7345851181313,14.5869148378636,
132.815919319322)) ;
#125029 = CARTESIAN_POINT('Ctrl Pts',(-15.6446503042506,14.549009953407,132.520094917807)) ;
#125030 = CARTESIAN_POINT('Ctrl Pts',(-15.5613259222977,14.4299835709606,
132.243476421726)) ;
#125031 = CARTESIAN_POINT('Ctrl Pts',(-15.4918978635437,14.2395160277486,
132.007608598271)) ;
#125032 = CARTESIAN_POINT('Ctrl Pts',(-15.441493990576,13.9900850952094,131.827215612351)) ;
#125033 = CARTESIAN_POINT('Ctrl Pts',(-15.4147523737952,13.7002631098511,
131.715984820068)) ;
#125034 = CARTESIAN_POINT('Ctrl Pts',(-15.4141848692343,13.3906063370585,
131.681212767504)) ;
#125035 = CARTESIAN_POINT('Ctrl Pts',(-15.4406987166013,13.0826197342829,
131.725480875401)) ;
#125036 = CARTESIAN_POINT('Ctrl Pts',(-15.4929987863392,12.7997480934514,
131.845153004214)) ;
#125037 = CARTESIAN_POINT('Ctrl Pts',(-15.5680380099016,12.5614902723847,
132.031257977271)) ;
#125038 = CARTESIAN_POINT('Ctrl Pts',(-15.6613888907222,12.3846250062646,
132.270799254956)) ;
#125039 = CARTESIAN_POINT('Ctrl Pts',(-15.7668964947916,12.2824687795427,
132.545876098705)) ;
#125040 = CARTESIAN_POINT('Ctrl Pts',(-15.8774268513273,12.2619556367439,
132.835724393864)) ;
#125041 = CARTESIAN_POINT('Ctrl Pts',(-15.9865462840208,12.3244285368361,
133.121329823739)) ;
#125042 = CARTESIAN_POINT('Ctrl Pts',(-16.0868856191326,12.4664340564494,
133.381215648153)) ;
#125043 = CARTESIAN_POINT('Ctrl Pts',(-16.1711609881106,12.6753487848156,
133.594444113081)) ;
#125044 = CARTESIAN_POINT('Ctrl Pts',(-16.2352956880658,12.9390315175275,
133.748624282027)) ;
#125045 = CARTESIAN_POINT('Ctrl Pts',(-16.274758335238,13.2369183961831,133.830804549625)) ;
#125046 = CARTESIAN_POINT('Ctrl Pts',(-16.2875416134419,13.5497744886041,
133.834864948315)) ;
#125047 = CARTESIAN_POINT('Ctrl Pts',(-16.27350948019,13.8506095454533,133.76092084741)) ;
#125048 = CARTESIAN_POINT('Ctrl Pts',(-16.2343148511589,14.1229210683533,
133.613234990865)) ;
#125049 = CARTESIAN_POINT('Ctrl Pts',(-16.1736950386534,14.3440341407498,
133.403097622042)) ;
#125050 = CARTESIAN_POINT('Ctrl Pts',(-16.0964629275866,14.5000650906738,
133.144340925564)) ;
#125051 = CARTESIAN_POINT('Ctrl Pts',(-16.0085177153032,14.5786444747034,
132.854136319792)) ;
#125052 = CARTESIAN_POINT('Ctrl Pts',(-15.9184051398423,14.5743811476286,
132.557997834982)) ;
#125053 = CARTESIAN_POINT('Ctrl Pts',(-15.8311646501359,14.4873598311618,
132.269835416294)) ;
#125054 = CARTESIAN_POINT('Ctrl Pts',(-15.7554385199139,14.3240886154077,
132.015513010405)) ;
#125055 = CARTESIAN_POINT('Ctrl Pts',(-15.6968978333521,14.0972552260208,
131.811480466257)) ;
#125056 = CARTESIAN_POINT('Ctrl Pts',(-15.660121717312,13.8219066558181,131.670965445006)) ;
#125057 = CARTESIAN_POINT('Ctrl Pts',(-15.6487014566343,13.516025574875,131.604313184565)) ;
#125058 = CARTESIAN_POINT('Ctrl Pts',(-15.6643812999087,13.2050736952722,
131.617003925741)) ;
#125059 = CARTESIAN_POINT('Ctrl Pts',(-15.7063207684821,12.9106473531297,
131.706512006777)) ;
#125060 = CARTESIAN_POINT('Ctrl Pts',(-15.7725855680298,12.6518068036689,
131.866967709783)) ;
#125061 = CARTESIAN_POINT('Ctrl Pts',(-15.8591726098178,12.4481718276841,
132.086764482203)) ;
#125062 = CARTESIAN_POINT('Ctrl Pts',(-15.9604476025779,12.3143466020562,
132.349489674931)) ;
#125063 = CARTESIAN_POINT('Ctrl Pts',(-16.0704199585515,12.2602411283263,
132.637481151036)) ;
#125064 = CARTESIAN_POINT('Ctrl Pts',(-16.180142994227,12.289044221804,132.925153256942)) ;
#125065 = CARTESIAN_POINT('Ctrl Pts',(-16.2851832841205,12.3996399121577,
133.19871199035)) ;
#125066 = CARTESIAN_POINT('Ctrl Pts',(-16.3765661818685,12.5827969137066,
133.432639291923)) ;
#125067 = CARTESIAN_POINT('Ctrl Pts',(-16.4496897001009,12.8269629913892,
133.613061201054)) ;
#125068 = CARTESIAN_POINT('Ctrl Pts',(-16.4993504127323,13.1127056194501,
133.725096180988)) ;
#125069 = CARTESIAN_POINT('Ctrl Pts',(-16.5231792047334,13.4217118754633,
133.761539786929)) ;
#125070 = CARTESIAN_POINT('Ctrl Pts',(-16.5199738631592,13.7304251092952,
133.719063366019)) ;
#125071 = CARTESIAN_POINT('Ctrl Pts',(-16.490503384238,14.0183443121755,133.599699786057)) ;
#125072 = CARTESIAN_POINT('Ctrl Pts',(-16.4381141934094,14.2615012050008,
133.413650952144)) ;
#125073 = CARTESIAN_POINT('Ctrl Pts',(-16.3669280545773,14.4455241702922,
133.172585659673)) ;
#125074 = CARTESIAN_POINT('Ctrl Pts',(-16.2829194787264,14.5564730573808,
132.894096731923)) ;
#125075 = CARTESIAN_POINT('Ctrl Pts',(-16.1921044498383,14.5860332568258,
132.59547783415)) ;
#125076 = CARTESIAN_POINT('Ctrl Pts',(-16.103500275386,14.5327319791753,132.303757320234)) ;
#125077 = CARTESIAN_POINT('Ctrl Pts',(-16.0219268181338,14.3988254927601,
132.032121654547)) ;
#125078 = CARTESIAN_POINT('Ctrl Pts',(-15.9559637229476,14.1966329256883,
131.806478335606)) ;
#125079 = CARTESIAN_POINT('Ctrl Pts',(-15.9096631410881,13.9381994026002,
131.638070209423)) ;
#125080 = CARTESIAN_POINT('Ctrl Pts',(-15.8876877659076,13.6421506980583,
131.540674271844)) ;
#125081 = CARTESIAN_POINT('Ctrl Pts',(-15.892259652353,13.3319747136995,131.520994310315)) ;
#125082 = CARTESIAN_POINT('Ctrl Pts',(-15.9236182041974,13.0275240722509,
131.579488272079)) ;
#125083 = CARTESIAN_POINT('Ctrl Pts',(-15.9808594345229,12.7499512402199,
131.71339289058)) ;
#125084 = CARTESIAN_POINT('Ctrl Pts',(-16.0595419330876,12.5230805349149,
131.910248319882)) ;
#125085 = CARTESIAN_POINT('Ctrl Pts',(-16.1555190707494,12.3595163071095,
132.1575039903)) ;
#125086 = CARTESIAN_POINT('Ctrl Pts',(-16.2628242846162,12.2720600916224,
132.437756364617)) ;
#125087 = CARTESIAN_POINT('Ctrl Pts',(-16.3739355148782,12.2676665525214,
132.729189014784)) ;
#125088 = CARTESIAN_POINT('Ctrl Pts',(-16.4811396900132,12.3451448696153,
133.009429281113)) ;
#125089 = CARTESIAN_POINT('Ctrl Pts',(-16.5790070302067,12.5004783202174,
133.26212619254)) ;
#125090 = CARTESIAN_POINT('Ctrl Pts',(-16.6600475484308,12.7212078449696,
133.465811461035)) ;
#125091 = CARTESIAN_POINT('Ctrl Pts',(-16.7198827149784,12.9936146304865,
133.607363218945)) ;
#125092 = CARTESIAN_POINT('Ctrl Pts',(-16.754273605641,13.2947838231295,133.67482792291)) ;
#125093 = CARTESIAN_POINT('Ctrl Pts',(-16.7620692032191,13.6064069014527,
133.664452435759)) ;
#125094 = CARTESIAN_POINT('Ctrl Pts',(-16.7430907146308,13.9050218268895,
133.575849688899)) ;
#125095 = CARTESIAN_POINT('Ctrl Pts',(-16.6995705306357,14.1686337353897,
133.415605636576)) ;
#125096 = CARTESIAN_POINT('Ctrl Pts',(-16.6353883774132,14.3788183161701,
133.195021357759)) ;
#125097 = CARTESIAN_POINT('Ctrl Pts',(-16.5557065457281,14.520866298431,132.929111709198)) ;
#125098 = CARTESIAN_POINT('Ctrl Pts',(-16.4669529903276,14.5841620003351,
132.636672229951)) ;
#125099 = CARTESIAN_POINT('Ctrl Pts',(-16.3764933029576,14.5641966090762,
132.339316751059)) ;
#125100 = CARTESIAN_POINT('Ctrl Pts',(-16.2912541780602,14.4625801801971,
132.057180085173)) ;
#125101 = CARTESIAN_POINT('Ctrl Pts',(-16.2180694744256,14.2860054922745,
131.810200069221)) ;
#125102 = CARTESIAN_POINT('Ctrl Pts',(-16.1632868666625,14.0484511491475,
131.617113761597)) ;
#125103 = CARTESIAN_POINT('Ctrl Pts',(-16.1310808580205,13.7663469405247,
131.48997210374)) ;
#125104 = CARTESIAN_POINT('Ctrl Pts',(-16.1247064234406,13.4574607709576,
131.438056091553)) ;
#125105 = CARTESIAN_POINT('Ctrl Pts',(-16.1452962590473,13.1488899250601,
131.465215238141)) ;
#125106 = CARTESIAN_POINT('Ctrl Pts',(-16.1921499049796,12.8583365008137,
131.568923429512)) ;
#125107 = CARTESIAN_POINT('Ctrl Pts',(-16.2627019723822,12.6085157648157,
131.741877002118)) ;
#125108 = CARTESIAN_POINT('Ctrl Pts',(-16.3523422100756,12.4173946912655,
131.970658735821)) ;
#125109 = CARTESIAN_POINT('Ctrl Pts',(-16.4557143149458,12.2980452527152,
132.239501066131)) ;
#125110 = CARTESIAN_POINT('Ctrl Pts',(-16.5657958992365,12.2592457777712,
132.528006891345)) ;
#125111 = CARTESIAN_POINT('Ctrl Pts',(-16.6761302057644,12.3040208605449,
132.817096151529)) ;
#125112 = CARTESIAN_POINT('Ctrl Pts',(-16.7784620002637,12.4286939369855,
133.082985219044)) ;
#125113 = CARTESIAN_POINT('Ctrl Pts',(-16.8670042340399,12.6243590090332,
133.308543332453)) ;
#125114 = CARTESIAN_POINT('Ctrl Pts',(-16.9362046600572,12.8789083522399,
133.477410666535)) ;
#125115 = CARTESIAN_POINT('Ctrl Pts',(-16.981013129791,13.1702261318585,133.575303882571)) ;
#125116 = CARTESIAN_POINT('Ctrl Pts',(-16.9997593267908,13.4805037318096,
133.596949956385)) ;
#125117 = CARTESIAN_POINT('Ctrl Pts',(-16.9914405859225,13.7876511812746,
133.539432418538)) ;
#125118 = CARTESIAN_POINT('Ctrl Pts',(-16.9573735315458,14.0678452982214,
133.406766511356)) ;
#125119 = CARTESIAN_POINT('Ctrl Pts',(-16.9012614485024,14.3007432991358,
133.209897343)) ;
#125120 = CARTESIAN_POINT('Ctrl Pts',(-16.8268882457025,14.472578666663,132.959393972783)) ;
#125121 = CARTESIAN_POINT('Ctrl Pts',(-16.7412612448846,14.5682598997855,
132.676214692444)) ;
#125122 = CARTESIAN_POINT('Ctrl Pts',(-16.6506173444698,14.5824152858443,
132.378287771747)) ;
#125123 = CARTESIAN_POINT('Ctrl Pts',(-16.5622810767315,14.5133614382036,
132.087075773177)) ;
#125124 = CARTESIAN_POINT('Ctrl Pts',(-16.4833786073322,14.3656854854221,
131.823382600048)) ;
#125125 = CARTESIAN_POINT('Ctrl Pts',(-16.4206953534256,14.1519222579812,
131.60728783786)) ;
#125126 = CARTESIAN_POINT('Ctrl Pts',(-16.378605818651,13.8839964820202,131.451069851381)) ;
#125127 = CARTESIAN_POINT('Ctrl Pts',(-16.3616265485276,13.5839684953717,
131.368347064637)) ;
#125128 = CARTESIAN_POINT('Ctrl Pts',(-16.3712407110028,13.2736209953703,
131.363427796788)) ;
#125129 = CARTESIAN_POINT('Ctrl Pts',(-16.4075816986682,12.9727615411734,
131.436462345173)) ;
#125130 = CARTESIAN_POINT('Ctrl Pts',(-16.4691084518117,12.7034620049653,
131.582968291489)) ;
#125131 = CARTESIAN_POINT('Ctrl Pts',(-16.5516508067842,12.4867211493109,
131.790989127946)) ;
#125132 = CARTESIAN_POINT('Ctrl Pts',(-16.6503484981561,12.3368636809282,
132.046157336608)) ;
#125133 = CARTESIAN_POINT('Ctrl Pts',(-16.7583562953978,12.2650346838616,
132.328642824857)) ;
#125134 = CARTESIAN_POINT('Ctrl Pts',(-16.8694876280613,12.2758062745913,
132.620115626391)) ;
#125135 = CARTESIAN_POINT('Ctrl Pts',(-16.9761391690963,12.3692807546481,
132.898474485446)) ;
#125136 = CARTESIAN_POINT('Ctrl Pts',(-17.0709660600708,12.5378929706017,
133.142402959768)) ;
#125137 = CARTESIAN_POINT('Ctrl Pts',(-17.1482588531112,12.7694277831183,
133.335140705917)) ;
#125138 = CARTESIAN_POINT('Ctrl Pts',(-17.203480116346,13.0484836383152,133.463302136376)) ;
#125139 = CARTESIAN_POINT('Ctrl Pts',(-17.2330309055993,13.3553252345684,
133.516383957086)) ;
#125140 = CARTESIAN_POINT('Ctrl Pts',(-17.2355770259433,13.6640556396721,
133.490901219807)) ;
#125141 = CARTESIAN_POINT('Ctrl Pts',(-17.2118345762843,13.9577070644724,
133.38838860845)) ;
#125142 = CARTESIAN_POINT('Ctrl Pts',(-17.1640544883737,14.2128779960594,
133.215679321086)) ;
#125143 = CARTESIAN_POINT('Ctrl Pts',(-17.0962318726985,14.4117544272494,
132.984335525429)) ;
#125144 = CARTESIAN_POINT('Ctrl Pts',(-17.0145165993263,14.5391283033453,
132.712572701399)) ;
#125145 = CARTESIAN_POINT('Ctrl Pts',(-16.9245932202189,14.5867879380275,
132.416618791262)) ;
#125146 = CARTESIAN_POINT('Ctrl Pts',(-16.8350007935137,14.5512051546367,
132.121952756565)) ;
#125147 = CARTESIAN_POINT('Ctrl Pts',(-16.7512399326396,14.4343419889086,
131.844006100408)) ;
#125148 = CARTESIAN_POINT('Ctrl Pts',(-16.6813663736858,14.2455278937518,
131.606828317341)) ;
#125149 = CARTESIAN_POINT('Ctrl Pts',(-16.6304533077385,13.9981929158514,
131.425029652249)) ;
#125150 = CARTESIAN_POINT('Ctrl Pts',(-16.6029110965595,13.7085066698523,
131.311373710203)) ;
#125151 = CARTESIAN_POINT('Ctrl Pts',(-16.6016472246784,13.3995793870564,
131.274618331211)) ;
#125152 = CARTESIAN_POINT('Ctrl Pts',(-16.6272259405872,13.0919774585784,
131.316244261262)) ;
#125153 = CARTESIAN_POINT('Ctrl Pts',(-16.6790956075483,12.8067303604848,
131.434491745221)) ;
#125154 = CARTESIAN_POINT('Ctrl Pts',(-16.7531642097008,12.5682008646981,
131.617936014673)) ;
#125155 = CARTESIAN_POINT('Ctrl Pts',(-16.846195785703,12.3888212047449,131.85647832136)) ;
#125156 = CARTESIAN_POINT('Ctrl Pts',(-16.9512994964481,12.2844119375082,
132.130420874405)) ;
#125157 = CARTESIAN_POINT('Ctrl Pts',(-17.0621203595401,12.2613333969067,
132.421013195999)) ;
#125158 = CARTESIAN_POINT('Ctrl Pts',(-17.1712584780037,12.3215794743214,
132.706710232666)) ;
#125159 = CARTESIAN_POINT('Ctrl Pts',(-17.2716303151699,12.4606919481936,
132.966808168993)) ;
#125160 = CARTESIAN_POINT('Ctrl Pts',(-17.3568271309369,12.6684214506416,
133.182599772503)) ;
#125161 = CARTESIAN_POINT('Ctrl Pts',(-17.4217613046076,12.9319196123432,
133.339000010842)) ;
#125162 = CARTESIAN_POINT('Ctrl Pts',(-17.4617001910976,13.2279083302756,
133.42271072074)) ;
#125163 = CARTESIAN_POINT('Ctrl Pts',(-17.4753487897358,13.5392234184095,
133.429453311327)) ;
#125164 = CARTESIAN_POINT('Ctrl Pts',(-17.462103295986,13.8421684111979,133.357645852584)) ;
#125165 = CARTESIAN_POINT('Ctrl Pts',(-17.4235361943751,14.1158321070144,
133.211769875002)) ;
#125166 = CARTESIAN_POINT('Ctrl Pts',(-17.363322316069,14.339009376798,133.002750514916)) ;
#125167 = CARTESIAN_POINT('Ctrl Pts',(-17.2866062600397,14.4964746049257,
132.745573553595)) ;
#125168 = CARTESIAN_POINT('Ctrl Pts',(-17.199397296313,14.5773715889881,132.457710585118)) ;
#125169 = CARTESIAN_POINT('Ctrl Pts',(-17.1085822658646,14.5757025147149,
132.159265391924)) ;
#125170 = CARTESIAN_POINT('Ctrl Pts',(-17.0213774045602,14.490867072331,131.871293001474)) ;
#125171 = CARTESIAN_POINT('Ctrl Pts',(-16.9454927949128,14.330592253299,131.616635348384)) ;
#125172 = CARTESIAN_POINT('Ctrl Pts',(-16.8860651829023,14.1048089901007,
131.409889551505)) ;
#125173 = CARTESIAN_POINT('Ctrl Pts',(-16.84857731132,13.8293690778141,131.267169165395)) ;
#125174 = CARTESIAN_POINT('Ctrl Pts',(-16.8364706813943,13.526576284789,131.198790499997)) ;
#125175 = CARTESIAN_POINT('Ctrl Pts',(-16.8512333940757,13.2147294294983,
131.208717499866)) ;
#125176 = CARTESIAN_POINT('Ctrl Pts',(-16.8924752507082,12.9189024654219,
131.296126903513)) ;
#125177 = CARTESIAN_POINT('Ctrl Pts',(-16.9583514927503,12.6580299108607,
131.455339791763)) ;
#125178 = CARTESIAN_POINT('Ctrl Pts',(-17.044063698862,12.4534345481142,131.672724444165)) ;
#125179 = CARTESIAN_POINT('Ctrl Pts',(-17.1452480350567,12.3171076600088,
131.935097166867)) ;
#125180 = CARTESIAN_POINT('Ctrl Pts',(-17.2545016602799,12.2606844017973,
132.221165652428)) ;
#125181 = CARTESIAN_POINT('Ctrl Pts',(-17.3650975011876,12.2870889602567,
132.511145676812)) ;
#125182 = CARTESIAN_POINT('Ctrl Pts',(-17.4703391463682,12.3957983185939,
132.785305386783)) ;
#125183 = CARTESIAN_POINT('Ctrl Pts',(-17.5619519450176,12.576725714127,133.019970693794)) ;
#125184 = CARTESIAN_POINT('Ctrl Pts',(-17.6355785374756,12.8186993235838,
133.201938865071)) ;
#125185 = CARTESIAN_POINT('Ctrl Pts',(-17.686204034739,13.1050418168408,133.316613415552)) ;
#125186 = CARTESIAN_POINT('Ctrl Pts',(-17.7106472500127,13.4130762749516,
133.354929376056)) ;
#125187 = CARTESIAN_POINT('Ctrl Pts',(-17.708198005418,13.7214651862128,133.314720701507)) ;
#125188 = CARTESIAN_POINT('Ctrl Pts',(-17.6797043677166,14.0093161749257,
133.198352418862)) ;
#125189 = CARTESIAN_POINT('Ctrl Pts',(-17.6275067830574,14.2560736746896,
133.012580543426)) ;
#125190 = CARTESIAN_POINT('Ctrl Pts',(-17.5569227810102,14.4412184365536,
132.773378196759)) ;
#125191 = CARTESIAN_POINT('Ctrl Pts',(-17.47320903247,14.5543182537731,132.495749100207)) ;
#125192 = CARTESIAN_POINT('Ctrl Pts',(-17.3828982361184,14.5864671229327,
132.198763951724)) ;
#125193 = CARTESIAN_POINT('Ctrl Pts',(-17.2935482114435,14.5351930359694,
131.904630245163)) ;
#125194 = CARTESIAN_POINT('Ctrl Pts',(-17.212146566953,14.4042256510203,131.633704988442)) ;
#125195 = CARTESIAN_POINT('Ctrl Pts',(-17.1453646293854,14.2033619799806,
131.405542254505)) ;
#125196 = CARTESIAN_POINT('Ctrl Pts',(-17.0984468920315,13.9460942692561,
131.235324126716)) ;
#125197 = CARTESIAN_POINT('Ctrl Pts',(-17.0757509849467,13.6510939576202,
131.135850406364)) ;
#125198 = CARTESIAN_POINT('Ctrl Pts',(-17.0795112397246,13.3409631929891,
131.113791894958)) ;
#125199 = CARTESIAN_POINT('Ctrl Pts',(-17.1102336251651,13.0355468372364,
131.170367824082)) ;
#125200 = CARTESIAN_POINT('Ctrl Pts',(-17.1663842613516,12.7584809477333,
131.301291574706)) ;
#125201 = CARTESIAN_POINT('Ctrl Pts',(-17.2447371033767,12.5287898024968,
131.497044500039)) ;
#125202 = CARTESIAN_POINT('Ctrl Pts',(-17.3403102773083,12.3633456659364,
131.743129508113)) ;
#125203 = CARTESIAN_POINT('Ctrl Pts',(-17.4470084964624,12.2737023197767,
132.021718516189)) ;
#125204 = CARTESIAN_POINT('Ctrl Pts',(-17.5581425262806,12.2663504667095,
132.31320916941)) ;
#125205 = CARTESIAN_POINT('Ctrl Pts',(-17.6662007298593,12.34208017502,132.595736728779)) ;
#125206 = CARTESIAN_POINT('Ctrl Pts',(-17.7639779601898,12.4946576903152,
132.848330696143)) ;
#125207 = CARTESIAN_POINT('Ctrl Pts',(-17.845869332575,12.7142650578431,133.054392423635)) ;
#125208 = CARTESIAN_POINT('Ctrl Pts',(-17.9062976280735,12.9853995961956,
133.197700199445)) ;
#125209 = CARTESIAN_POINT('Ctrl Pts',(-17.9414670577148,13.2860375673385,
133.267430288951)) ;
#125210 = CARTESIAN_POINT('Ctrl Pts',(-17.9500100804759,13.5985523264733,
133.259150343869)) ;
#125211 = CARTESIAN_POINT('Ctrl Pts',(-17.9316672579666,13.8975129640997,
133.17242792376)) ;
#125212 = CARTESIAN_POINT('Ctrl Pts',(-17.8890068524942,14.1612607305214,
133.014839223972)) ;
#125213 = CARTESIAN_POINT('Ctrl Pts',(-17.8252095466582,14.3739608986485,
132.795283644914)) ;
#125214 = CARTESIAN_POINT('Ctrl Pts',(-17.745594810308,14.5182947311408,132.529471937836)) ;
#125215 = CARTESIAN_POINT('Ctrl Pts',(-17.6571488015363,14.5834512891337,
132.23799331013)) ;
#125216 = CARTESIAN_POINT('Ctrl Pts',(-17.5669390064096,14.5659482056826,
131.94147536579)) ;
#125217 = CARTESIAN_POINT('Ctrl Pts',(-17.4814696878511,14.4667697468738,
131.65867637402)) ;
#125218 = CARTESIAN_POINT('Ctrl Pts',(-17.4077725179851,14.2923285358451,
131.410191086964)) ;
#125219 = CARTESIAN_POINT('Ctrl Pts',(-17.3521425033157,14.0548140143778,
131.21443926717)) ;
#125220 = CARTESIAN_POINT('Ctrl Pts',(-17.3195158312481,13.7751053966171,
131.086247525205)) ;
#125221 = CARTESIAN_POINT('Ctrl Pts',(-17.312239483779,13.4671706685235,131.031747960473)) ;
#125222 = CARTESIAN_POINT('Ctrl Pts',(-17.3322332196275,13.1566326629542,
131.056977756949)) ;
#125223 = CARTESIAN_POINT('Ctrl Pts',(-17.3780975395808,12.8670308580196,
131.158001609314)) ;
#125224 = CARTESIAN_POINT('Ctrl Pts',(-17.4482094790245,12.614625742012,131.329541047974)) ;
#125225 = CARTESIAN_POINT('Ctrl Pts',(-17.5375995577901,12.4216271710516,
131.557537586871)) ;
#125226 = CARTESIAN_POINT('Ctrl Pts',(-17.6401822990097,12.3004936351809,
131.824227815252)) ;
#125227 = CARTESIAN_POINT('Ctrl Pts',(-17.7507907280733,12.2591976942699,
132.114082356459)) ;
#125228 = CARTESIAN_POINT('Ctrl Pts',(-17.8604775826945,12.3014766458867,
132.401506605415)) ;
#125229 = CARTESIAN_POINT('Ctrl Pts',(-17.9633872935851,12.4236752425343,
132.669020376417)) ;
#125230 = CARTESIAN_POINT('Ctrl Pts',(-18.0529404696377,12.6191375618547,
132.897304914097)) ;
#125231 = CARTESIAN_POINT('Ctrl Pts',(-18.1222475619153,12.8707902517674,
133.066702627176)) ;
#125232 = CARTESIAN_POINT('Ctrl Pts',(-18.1679096652003,13.1617413465553,
133.167025713482)) ;
#125233 = CARTESIAN_POINT('Ctrl Pts',(-18.1873626654556,13.4713353015044,
133.190791441837)) ;
#125234 = CARTESIAN_POINT('Ctrl Pts',(-18.1798609889004,13.7785022490456,
133.135703081782)) ;
#125235 = CARTESIAN_POINT('Ctrl Pts',(-18.1466211271099,14.0596469751513,
133.005485313342)) ;
#125236 = CARTESIAN_POINT('Ctrl Pts',(-18.0908146756498,14.2953142931135,
132.80933989071)) ;
#125237 = CARTESIAN_POINT('Ctrl Pts',(-18.0168560810249,14.468964761841,132.560061748028)) ;
#125238 = CARTESIAN_POINT('Ctrl Pts',(-17.9311937335186,14.566840747798,132.276680512061)) ;
#125239 = CARTESIAN_POINT('Ctrl Pts',(-17.8410327874371,14.5831863557758,
131.980333879477)) ;
#125240 = CARTESIAN_POINT('Ctrl Pts',(-17.7521647268769,14.5160478882273,
131.687421881803)) ;
#125241 = CARTESIAN_POINT('Ctrl Pts',(-17.6733234585166,14.3710572999732,
131.424079417212)) ;
#125242 = CARTESIAN_POINT('Ctrl Pts',(-17.6099533809622,14.1586831437498,
131.205906158547)) ;
#125243 = CARTESIAN_POINT('Ctrl Pts',(-17.567311041449,13.8924167167611,131.04813455033)) ;
#125244 = CARTESIAN_POINT('Ctrl Pts',(-17.5495214646108,13.5934589593166,
130.963081615833)) ;
#125245 = CARTESIAN_POINT('Ctrl Pts',(-17.5583972008256,13.2817948443867,
130.95586528545)) ;
#125246 = CARTESIAN_POINT('Ctrl Pts',(-17.5940640660166,12.9807519837477,
131.02696560632)) ;
#125247 = CARTESIAN_POINT('Ctrl Pts',(-17.6545564421108,12.7114087835464,
131.170609668857)) ;
#125248 = CARTESIAN_POINT('Ctrl Pts',(-17.7368226999729,12.4920355070178,
131.377698689643)) ;
#125249 = CARTESIAN_POINT('Ctrl Pts',(-17.8348724901337,12.340409192469,131.631065455317)) ;
#125250 = CARTESIAN_POINT('Ctrl Pts',(-17.9430670356921,12.2658594126602,
131.913978129015)) ;
#125251 = CARTESIAN_POINT('Ctrl Pts',(-18.054069728851,12.2744067953506,132.205121446175)) ;
#125252 = CARTESIAN_POINT('Ctrl Pts',(-18.1606637543709,12.3651074088565,
132.483406049134)) ;
#125253 = CARTESIAN_POINT('Ctrl Pts',(-18.2560924961007,12.5316553295761,
132.729048365178)) ;
#125254 = CARTESIAN_POINT('Ctrl Pts',(-18.3341778607555,12.7621962066438,
132.924014416432)) ;
#125255 = CARTESIAN_POINT('Ctrl Pts',(-18.3899839397294,13.0400249877383,
133.0539094655)) ;
#125256 = CARTESIAN_POINT('Ctrl Pts',(-18.4202910006776,13.3449925663018,
133.109347316149)) ;
#125257 = CARTESIAN_POINT('Ctrl Pts',(-18.4236631714754,13.6560824874518,
133.086042456464)) ;
#125258 = CARTESIAN_POINT('Ctrl Pts',(-18.4006453620218,13.949523069505,132.98575486702)) ;
#125259 = CARTESIAN_POINT('Ctrl Pts',(-18.3535646409171,14.2060602321428,
132.815095461345)) ;
#125260 = CARTESIAN_POINT('Ctrl Pts',(-18.2862713344444,14.4068533843326,
132.585305948808)) ;
#125261 = CARTESIAN_POINT('Ctrl Pts',(-18.2047737795013,14.5364834537221,
132.314136374667)) ;
#125262 = CARTESIAN_POINT('Ctrl Pts',(-18.115348409199,14.5865952294226,132.019776237642)) ;
#125263 = CARTESIAN_POINT('Ctrl Pts',(-18.0251839000944,14.5532896916384,
131.723255892366)) ;
#125264 = CARTESIAN_POINT('Ctrl Pts',(-17.9415200376328,14.4391769961996,
131.445750322776)) ;
#125265 = CARTESIAN_POINT('Ctrl Pts',(-17.8709865879843,14.2521193934998,
131.206572721742)) ;
#125266 = CARTESIAN_POINT('Ctrl Pts',(-17.8194372166682,14.0064610043906,
131.02293735799)) ;
#125267 = CARTESIAN_POINT('Ctrl Pts',(-17.7910798255988,13.7162751862111,
130.906740249931)) ;
#125268 = CARTESIAN_POINT('Ctrl Pts',(-17.789099001038,13.4088590372399,130.868028561726)) ;
#125269 = CARTESIAN_POINT('Ctrl Pts',(-17.8139225822361,13.10053389726,130.907404974492)) ;
#125270 = CARTESIAN_POINT('Ctrl Pts',(-17.8648392613618,12.8153801351655,
131.023001165044)) ;
#125271 = CARTESIAN_POINT('Ctrl Pts',(-17.9384487251623,12.5742829301141,
131.20499722078)) ;
#125272 = CARTESIAN_POINT('Ctrl Pts',(-18.031524743861,12.3924207645517,131.443517414331)) ;
#125273 = CARTESIAN_POINT('Ctrl Pts',(-18.1358382897965,12.2864008460228,
131.715324149777)) ;
#125274 = CARTESIAN_POINT('Ctrl Pts',(-18.2469528531772,12.2608494094795,
132.006664764433)) ;
#125275 = CARTESIAN_POINT('Ctrl Pts',(-18.3557753142692,12.318610673207,132.291578909571)) ;
#125276 = CARTESIAN_POINT('Ctrl Pts',(-18.4567104546273,12.4554523498405,
132.553270393945)) ;
#125277 = CARTESIAN_POINT('Ctrl Pts',(-18.5427096959362,12.6626735869421,
132.771253835525)) ;
#125278 = CARTESIAN_POINT('Ctrl Pts',(-18.6076529154857,12.9221026671482,
132.928024921922)) ;
#125279 = CARTESIAN_POINT('Ctrl Pts',(-18.648750425879,13.2188659560216,133.014929938329)) ;
#125280 = CARTESIAN_POINT('Ctrl Pts',(-18.6631067095924,13.5309970504502,
133.023649164472)) ;
#125281 = CARTESIAN_POINT('Ctrl Pts',(-18.6506464875791,13.833391117926,132.954252667471)) ;
#125282 = CARTESIAN_POINT('Ctrl Pts',(-18.612818085529,14.1082733327472,132.810534597262)) ;
#125283 = CARTESIAN_POINT('Ctrl Pts',(-18.5531811994103,14.333273457915,132.603195859953)) ;
#125284 = CARTESIAN_POINT('Ctrl Pts',(-18.4766889860136,14.493089968581,132.346598986185)) ;
#125285 = CARTESIAN_POINT('Ctrl Pts',(-18.3897834881845,14.5762694878071,
132.059665220926)) ;
#125286 = CARTESIAN_POINT('Ctrl Pts',(-18.2986311211206,14.5766426332955,
131.760103485388)) ;
#125287 = CARTESIAN_POINT('Ctrl Pts',(-18.212007783448,14.4950561386841,131.474141881949)) ;
#125288 = CARTESIAN_POINT('Ctrl Pts',(-18.1350292671629,14.3357812086937,
131.216006764261)) ;
#125289 = CARTESIAN_POINT('Ctrl Pts',(-18.075283615151,14.1117725486506,131.008402983714)) ;
#125290 = CARTESIAN_POINT('Ctrl Pts',(-18.0371145753747,13.8385111509001,
130.863796970643)) ;
#125291 = CARTESIAN_POINT('Ctrl Pts',(-18.0242445077644,13.5338961508562,
130.792932325099)) ;
#125292 = CARTESIAN_POINT('Ctrl Pts',(-18.038169338582,13.224257482388,130.800665239807)) ;
#125293 = CARTESIAN_POINT('Ctrl Pts',(-18.0788682297641,12.9262818286679,
130.886318330355)) ;
#125294 = CARTESIAN_POINT('Ctrl Pts',(-18.1436956382508,12.6654697880194,
131.042663175476)) ;
#125295 = CARTESIAN_POINT('Ctrl Pts',(-18.2297053008849,12.4574145749278,
131.260611523241)) ;
#125296 = CARTESIAN_POINT('Ctrl Pts',(-18.3295006899858,12.3205165370977,
131.519286625616)) ;
#125297 = CARTESIAN_POINT('Ctrl Pts',(-18.4392025215922,12.2610390449612,
131.806469003895)) ;
#125298 = CARTESIAN_POINT('Ctrl Pts',(-18.5495038928619,12.2851065235111,
132.095701138264)) ;
#125299 = CARTESIAN_POINT('Ctrl Pts',(-18.6551377015888,12.3913707658575,
132.370972967707)) ;
#125300 = CARTESIAN_POINT('Ctrl Pts',(-18.7473031876051,12.5705078939367,
132.607221974091)) ;
#125301 = CARTESIAN_POINT('Ctrl Pts',(-18.8215355648859,12.8110531024917,
132.79094927383)) ;
#125302 = CARTESIAN_POINT('Ctrl Pts',(-18.8728254696963,13.0958081066442,
132.907631481588)) ;
#125303 = CARTESIAN_POINT('Ctrl Pts',(-18.8981142773173,13.4043791396556,
132.948317043376)) ;
#125304 = CARTESIAN_POINT('Ctrl Pts',(-18.8964748240015,13.7127503611852,
132.91051808184)) ;
#125305 = CARTESIAN_POINT('Ctrl Pts',(-18.8683636782998,14.0031465384866,
132.795046521471)) ;
#125306 = CARTESIAN_POINT('Ctrl Pts',(-18.8174880240775,14.2480984869967,
132.613588092215)) ;
#125307 = CARTESIAN_POINT('Ctrl Pts',(-18.7469572957245,14.4370589144751,
132.37428276721)) ;
#125308 = CARTESIAN_POINT('Ctrl Pts',(-18.6635307918454,14.5521322480481,
132.097514975815)) ;
#125309 = CARTESIAN_POINT('Ctrl Pts',(-18.5732136816833,14.5867077636068,
131.800472743053)) ;
#125310 = CARTESIAN_POINT('Ctrl Pts',(-18.4839003383178,14.5378478925882,
131.506508305884)) ;
#125311 = CARTESIAN_POINT('Ctrl Pts',(-18.402187454381,14.409203021957,131.234680849945)) ;
#125312 = CARTESIAN_POINT('Ctrl Pts',(-18.334836902335,14.2102655044933,131.004850153329)) ;
#125313 = CARTESIAN_POINT('Ctrl Pts',(-18.2871464008144,13.9531164546974,
130.83222870879)) ;
#125314 = CARTESIAN_POINT('Ctrl Pts',(-18.2638580254884,13.6605444903127,
130.731214892336)) ;
#125315 = CARTESIAN_POINT('Ctrl Pts',(-18.2668270499817,13.3493859295917,
130.706712302463)) ;
#125316 = CARTESIAN_POINT('Ctrl Pts',(-18.2967304908482,13.0444134847032,
130.760998390813)) ;
#125317 = CARTESIAN_POINT('Ctrl Pts',(-18.3522199844922,12.7658508385772,
130.889945672519)) ;
#125318 = CARTESIAN_POINT('Ctrl Pts',(-18.4299598853039,12.5346698137633,
131.083926894411)) ;
#125319 = CARTESIAN_POINT('Ctrl Pts',(-18.5252575613863,12.3668712653983,
131.32915520716)) ;
#125320 = CARTESIAN_POINT('Ctrl Pts',(-18.6319362740028,12.2750736353354,
131.607631262067)) ;
#125321 = CARTESIAN_POINT('Ctrl Pts',(-18.7424805338833,12.2654123935104,
131.897568237114)) ;
#125322 = CARTESIAN_POINT('Ctrl Pts',(-18.8508042611965,12.3385001490515,
132.180853971329)) ;
#125323 = CARTESIAN_POINT('Ctrl Pts',(-18.9492299885013,12.4893941605664,
132.435254667707)) ;
#125324 = CARTESIAN_POINT('Ctrl Pts',(-19.0315407300344,12.7071836242874,
132.642573907651)) ;
#125325 = CARTESIAN_POINT('Ctrl Pts',(-19.0925135202913,12.976008781698,132.787590925835)) ;
#125326 = CARTESIAN_POINT('Ctrl Pts',(-19.1286176776364,13.2771672423765,
132.859921686262)) ;
#125327 = CARTESIAN_POINT('Ctrl Pts',(-19.1379114672632,13.5885364783272,
132.853960762233)) ;
#125328 = CARTESIAN_POINT('Ctrl Pts',(-19.1204771380458,13.8883475892356,
132.769887384823)) ;
#125329 = CARTESIAN_POINT('Ctrl Pts',(-19.0782724812617,14.1546798103871,
132.613467494316)) ;
#125330 = CARTESIAN_POINT('Ctrl Pts',(-19.0151377103599,14.3683945721778,
132.395937643212)) ;
#125331 = CARTESIAN_POINT('Ctrl Pts',(-18.9362575078144,14.5146640723976,
132.132398804477)) ;
#125332 = CARTESIAN_POINT('Ctrl Pts',(-18.8476989080688,14.5827891637854,
131.840476972232)) ;
#125333 = CARTESIAN_POINT('Ctrl Pts',(-18.7572366847191,14.5676065821518,
131.543147243417)) ;
#125334 = CARTESIAN_POINT('Ctrl Pts',(-18.6715544040139,14.4706130851543,
131.259732284729)) ;
#125335 = CARTESIAN_POINT('Ctrl Pts',(-18.5976273893705,14.2987448591994,
131.010671404235)) ;
#125336 = CARTESIAN_POINT('Ctrl Pts',(-18.5413330377305,14.063095759129,130.812986254615)) ;
#125337 = CARTESIAN_POINT('Ctrl Pts',(-18.5078379421256,13.7833207941159,
130.682126791118)) ;
#125338 = CARTESIAN_POINT('Ctrl Pts',(-18.4999097117007,13.4754882889809,
130.625692161167)) ;
#125339 = CARTESIAN_POINT('Ctrl Pts',(-18.5189512412166,13.1664272505894,
130.648326923808)) ;
#125340 = CARTESIAN_POINT('Ctrl Pts',(-18.5643283555043,12.8743475054809,
130.747739702902)) ;
#125341 = CARTESIAN_POINT('Ctrl Pts',(-18.6334328686697,12.6220180592587,
130.916528129785)) ;
#125342 = CARTESIAN_POINT('Ctrl Pts',(-18.7224073978982,12.4263341461984,
131.143243760147)) ;
#125343 = CARTESIAN_POINT('Ctrl Pts',(-18.8252741733722,12.3026056592769,
131.410587938808)) ;
#125344 = CARTESIAN_POINT('Ctrl Pts',(-18.9351163454627,12.2593725249827,
131.698402442325)) ;
#125345 = CARTESIAN_POINT('Ctrl Pts',(-19.0450419186209,12.2987734012192,
131.986493383599)) ;
#125346 = CARTESIAN_POINT('Ctrl Pts',(-19.1490013516762,12.4202091762236,
132.256809604344)) ;
#125347 = CARTESIAN_POINT('Ctrl Pts',(-19.2380191086713,12.611773656706,132.483899442427)) ;
#125348 = CARTESIAN_POINT('Ctrl Pts',(-19.3083453259853,12.8626551620978,
132.656143653974)) ;
#125349 = CARTESIAN_POINT('Ctrl Pts',(-19.3547040728807,13.1527448434828,
132.758511459085)) ;
#125350 = CARTESIAN_POINT('Ctrl Pts',(-19.3749834629373,13.4624298007765,
132.784654095395)) ;
#125351 = CARTESIAN_POINT('Ctrl Pts',(-19.36820543525,13.7701811084813,132.731659693189)) ;
#125352 = CARTESIAN_POINT('Ctrl Pts',(-19.3357421024822,14.0517728674994,
132.603778078472)) ;
#125353 = CARTESIAN_POINT('Ctrl Pts',(-19.2805289193557,14.2892527094167,
132.40934630679)) ;
#125354 = CARTESIAN_POINT('Ctrl Pts',(-19.2069909200465,14.4648240462418,
132.161293233759)) ;
#125355 = CARTESIAN_POINT('Ctrl Pts',(-19.1218686179884,14.5650403206084,
131.879594398651)) ;
#125356 = CARTESIAN_POINT('Ctrl Pts',(-19.031177665857,14.583748953291,131.581482686387)) ;
#125357 = CARTESIAN_POINT('Ctrl Pts',(-18.9429516230396,14.5197167656378,
131.290759379113)) ;
#125358 = CARTESIAN_POINT('Ctrl Pts',(-18.8631562519392,14.3763314306489,
131.024403462222)) ;
#125359 = CARTESIAN_POINT('Ctrl Pts',(-18.7992959670841,14.1656644644825,
130.804814101691)) ;
#125360 = CARTESIAN_POINT('Ctrl Pts',(-18.7559154993296,13.8999127599495,
130.644795322315)) ;
#125361 = CARTESIAN_POINT('Ctrl Pts',(-18.7374861463171,13.6028234452547,
130.558011913804)) ;
#125362 = CARTESIAN_POINT('Ctrl Pts',(-18.7455135996191,13.291184455058,130.548311267216)) ;
#125363 = CARTESIAN_POINT('Ctrl Pts',(-18.78038027663,12.9894029525186,130.617067330366)) ;
#125364 = CARTESIAN_POINT('Ctrl Pts',(-18.8404755456934,12.717765879006,130.759411419359)) ;
#125365 = CARTESIAN_POINT('Ctrl Pts',(-18.9221464088355,12.4972589130398,
130.964811609339)) ;
#125366 = CARTESIAN_POINT('Ctrl Pts',(-19.0195332489729,12.3438957008414,
131.216331735262)) ;
#125367 = CARTESIAN_POINT('Ctrl Pts',(-19.1276333368959,12.2668705096983,
131.498935943536)) ;
#125368 = CARTESIAN_POINT('Ctrl Pts',(-19.2385329213481,12.2729078297229,
131.789817260693)) ;
#125369 = CARTESIAN_POINT('Ctrl Pts',(-19.3455156987851,12.3614501849398,
132.069182436036)) ;
#125370 = CARTESIAN_POINT('Ctrl Pts',(-19.4411172478051,12.5253315667214,
132.315428252389)) ;
#125371 = CARTESIAN_POINT('Ctrl Pts',(-19.5201398347916,12.7552771114224,
132.512976833561)) ;
#125372 = CARTESIAN_POINT('Ctrl Pts',(-19.5764232616451,13.0310570491295,
132.644388654594)) ;
#125373 = CARTESIAN_POINT('Ctrl Pts',(-19.6075743657055,13.3361218325012,
132.702220642329)) ;
#125374 = CARTESIAN_POINT('Ctrl Pts',(-19.6117652558764,13.6463105662156,
132.681424980702)) ;
#125375 = CARTESIAN_POINT('Ctrl Pts',(-19.5893821264966,13.9424874348681,
132.582777301933)) ;
#125376 = CARTESIAN_POINT('Ctrl Pts',(-19.5427449303092,14.2002009461362,
132.413391756609)) ;
#125377 = CARTESIAN_POINT('Ctrl Pts',(-19.4764078517587,14.4015262761072,
132.186614554798)) ;
#125378 = CARTESIAN_POINT('Ctrl Pts',(-19.3950352335705,14.5339055048123,
131.915712480138)) ;
#125379 = CARTESIAN_POINT('Ctrl Pts',(-19.3057924258839,14.5863178640293,
131.621910109743)) ;
#125380 = CARTESIAN_POINT('Ctrl Pts',(-19.2153083863566,14.55532217226,131.324369164492)) ;
#125381 = CARTESIAN_POINT('Ctrl Pts',(-19.1314276970006,14.4431215003341,
131.046235050427)) ;
#125382 = CARTESIAN_POINT('Ctrl Pts',(-19.0606803517198,14.2589451908106,
130.806575496976)) ;
#125383 = CARTESIAN_POINT('Ctrl Pts',(-19.0082723613581,14.0132050933504,
130.620231148887)) ;
#125384 = CARTESIAN_POINT('Ctrl Pts',(-18.9794027695462,13.7264814781089,
130.502832395796)) ;
#125385 = CARTESIAN_POINT('Ctrl Pts',(-18.976561908527,13.4166671262314,130.461310037739)) ;
#125386 = CARTESIAN_POINT('Ctrl Pts',(-19.0006755833375,13.1090562119369,
130.498725654268)) ;
#125387 = CARTESIAN_POINT('Ctrl Pts',(-19.0508377132365,12.8228936687179,
130.612115355244)) ;
#125388 = CARTESIAN_POINT('Ctrl Pts',(-19.123922843109,12.5803482500096,130.792567588959)) ;
#125389 = CARTESIAN_POINT('Ctrl Pts',(-19.2160850433945,12.3971382780487,
131.028568123365)) ;
#125390 = CARTESIAN_POINT('Ctrl Pts',(-19.3206538990753,12.2881794710329,
131.300948176029)) ;
#125391 = CARTESIAN_POINT('Ctrl Pts',(-19.431532048178,12.260444774343,131.591652829408)) ;
#125392 = CARTESIAN_POINT('Ctrl Pts',(-19.5407246258012,12.3158800590199,
131.877582205411)) ;
#125393 = CARTESIAN_POINT('Ctrl Pts',(-19.6420758380499,12.4512316435153,
132.140435538389)) ;
#125394 = CARTESIAN_POINT('Ctrl Pts',(-19.7279001857045,12.6546809911043,
132.358198342916)) ;
#125395 = CARTESIAN_POINT('Ctrl Pts',(-19.7940662440651,12.9147731891358,
132.518270409866)) ;
#125396 = CARTESIAN_POINT('Ctrl Pts',(-19.8356553710753,13.2095560207855,
132.606765160291)) ;
#125397 = CARTESIAN_POINT('Ctrl Pts',(-19.8508741819814,13.5223875094378,
132.617909927863)) ;
#125398 = CARTESIAN_POINT('Ctrl Pts',(-19.8391683542652,13.8250175828272,
132.550755217814)) ;
#125399 = CARTESIAN_POINT('Ctrl Pts',(-19.8018217312818,14.1019896446971,
132.408313123862)) ;
#125400 = CARTESIAN_POINT('Ctrl Pts',(-19.7429921890077,14.3273313285593,
132.203502388414)) ;
#125401 = CARTESIAN_POINT('Ctrl Pts',(-19.6670062696929,14.4893435909273,
131.948405833705)) ;
#125402 = CARTESIAN_POINT('Ctrl Pts',(-19.5802153190921,14.5749600250314,
131.661768392291)) ;
#125403 = CARTESIAN_POINT('Ctrl Pts',(-19.4891679081042,14.5779281119493,
131.362553988494)) ;
#125404 = CARTESIAN_POINT('Ctrl Pts',(-19.4021090416363,14.4983364866609,
131.075222238346)) ;
#125405 = CARTESIAN_POINT('Ctrl Pts',(-19.3250576696382,14.3420895520869,
130.817036674605)) ;
#125406 = CARTESIAN_POINT('Ctrl Pts',(-19.2642816474385,14.1180210697834,
130.60616026518)) ;
#125407 = CARTESIAN_POINT('Ctrl Pts',(-19.2257474518653,13.8471807636704,
130.460666873348)) ;
#125408 = CARTESIAN_POINT('Ctrl Pts',(-19.2120103918454,13.5439412036153,
130.387343681072)) ;
#125409 = CARTESIAN_POINT('Ctrl Pts',(-19.225155205879,13.2331633714353,130.39268687927)) ;
#125410 = CARTESIAN_POINT('Ctrl Pts',(-19.2651252384059,12.9343807646982,
130.476204059893)) ;
#125411 = CARTESIAN_POINT('Ctrl Pts',(-19.3293892623455,12.6721977503837,
130.630876869171)) ;
#125412 = CARTESIAN_POINT('Ctrl Pts',(-19.414367024647,12.4632419123552,130.845988794884)) ;
#125413 = CARTESIAN_POINT('Ctrl Pts',(-19.5144157619604,12.3231158449139,
131.105192868357)) ;
#125414 = CARTESIAN_POINT('Ctrl Pts',(-19.6239682958549,12.2616017868531,
131.391949064764)) ;
#125415 = CARTESIAN_POINT('Ctrl Pts',(-19.7341251748847,12.2833201930426,
131.680814419557)) ;
#125416 = CARTESIAN_POINT('Ctrl Pts',(-19.8398307670297,12.3868877539332,
131.956364921524)) ;
#125417 = CARTESIAN_POINT('Ctrl Pts',(-19.9328715849158,12.5648231593225,
132.195022075704)) ;
#125418 = CARTESIAN_POINT('Ctrl Pts',(-20.0075697806433,12.8039602386114,
132.380126700454)) ;
#125419 = CARTESIAN_POINT('Ctrl Pts',(-20.0593917089716,13.0864729218444,
132.498501302387)) ;
#125420 = CARTESIAN_POINT('Ctrl Pts',(-20.0855942601537,13.3957238551008,
132.541742553164)) ;
#125421 = CARTESIAN_POINT('Ctrl Pts',(-20.0846180974026,13.7038340489926,
132.505928237067)) ;
#125422 = CARTESIAN_POINT('Ctrl Pts',(-20.0576118412634,13.9936201437027,
132.39389473662)) ;
#125423 = CARTESIAN_POINT('Ctrl Pts',(-20.0066670074455,14.2431366533872,
132.211800147466)) ;
#125424 = CARTESIAN_POINT('Ctrl Pts',(-19.9372867453542,14.4318623911142,
131.976209777932)) ;
#125425 = CARTESIAN_POINT('Ctrl Pts',(-19.8536336247197,14.5502397440411,
131.698547738352)) ;
#125426 = CARTESIAN_POINT('Ctrl Pts',(-19.763624304503,14.5868194748713,131.402499062289)) ;
#125427 = CARTESIAN_POINT('Ctrl Pts',(-19.6740868384927,14.5403267777303,
131.107834963745)) ;
#125428 = CARTESIAN_POINT('Ctrl Pts',(-19.5920809579075,14.4138414860088,
130.835165145447)) ;
#125429 = CARTESIAN_POINT('Ctrl Pts',(-19.5242274982525,14.2163546818928,
130.60382730934)) ;
#125430 = CARTESIAN_POINT('Ctrl Pts',(-19.4761656045147,13.9624647587777,
130.430351339929)) ;
#125431 = CARTESIAN_POINT('Ctrl Pts',(-19.4519267245949,13.6693367218364,
130.326390171342)) ;
#125432 = CARTESIAN_POINT('Ctrl Pts',(-19.4541360813185,13.3586797958361,
130.299708635269)) ;
#125433 = CARTESIAN_POINT('Ctrl Pts',(-19.4833072792466,13.0526929008547,
130.351794296597)) ;
#125434 = CARTESIAN_POINT('Ctrl Pts',(-19.5381123459215,12.7731727546938,
130.478753263755)) ;
#125435 = CARTESIAN_POINT('Ctrl Pts',(-19.6152840129382,12.5404161552581,
130.671072410998)) ;
#125436 = CARTESIAN_POINT('Ctrl Pts',(-19.7100584664821,12.370760764573,130.914808573912)) ;
#125437 = CARTESIAN_POINT('Ctrl Pts',(-19.8164805054715,12.2766729448487,
131.192538102687)) ;
#125438 = CARTESIAN_POINT('Ctrl Pts',(-19.9269545882548,12.2643218542415,
131.482288089165)) ;
#125439 = CARTESIAN_POINT('Ctrl Pts',(-20.0362420787139,12.336020687125,131.768135189097)) ;
#125440 = CARTESIAN_POINT('Ctrl Pts',(-20.1341015859013,12.4836397645111,
132.021190312288)) ;
#125441 = CARTESIAN_POINT('Ctrl Pts',(-20.2173448724865,12.7003320009064,
132.231098128125)) ;
#125442 = CARTESIAN_POINT('Ctrl Pts',(-20.2788998542731,12.9678918714247,
132.377839505011)) ;
#125443 = CARTESIAN_POINT('Ctrl Pts',(-20.3157857749859,13.2687870375049,
132.452412734401)) ;
#125444 = CARTESIAN_POINT('Ctrl Pts',(-20.3257878201776,13.5800036106842,
132.44853887218)) ;
#125445 = CARTESIAN_POINT('Ctrl Pts',(-20.3091319227027,13.8799730706512,
132.366793007165)) ;
#125446 = CARTESIAN_POINT('Ctrl Pts',(-20.2675833294922,14.1476994881547,
132.212271797659)) ;
#125447 = CARTESIAN_POINT('Ctrl Pts',(-20.2049654614363,14.3632525192321,
131.996240979151)) ;
#125448 = CARTESIAN_POINT('Ctrl Pts',(-20.1261959413298,14.5119336191473,
131.732928450416)) ;
#125449 = CARTESIAN_POINT('Ctrl Pts',(-20.0378705228692,14.5819602234039,
131.44171981574)) ;
#125450 = CARTESIAN_POINT('Ctrl Pts',(-19.9476548293995,14.5692454166129,
131.145213230718)) ;
#125451 = CARTESIAN_POINT('Ctrl Pts',(-19.8615317882014,14.4742854326631,
130.860430878038)) ;
#125452 = CARTESIAN_POINT('Ctrl Pts',(-19.7873954923186,14.3047438743695,
130.610843930884)) ;
#125453 = CARTESIAN_POINT('Ctrl Pts',(-19.7304993539858,14.0710830609088,
130.411431376984)) ;
#125454 = CARTESIAN_POINT('Ctrl Pts',(-19.6962102503808,13.7914035953126,
130.278142215268)) ;
#125455 = CARTESIAN_POINT('Ctrl Pts',(-19.6875605883208,13.48501227345,130.219710120386)) ;
#125456 = CARTESIAN_POINT('Ctrl Pts',(-19.7057561296348,13.1755843630713,
130.239857217883)) ;
#125457 = CARTESIAN_POINT('Ctrl Pts',(-19.7504585123233,12.8823157457974,
130.337257450733)) ;
#125458 = CARTESIAN_POINT('Ctrl Pts',(-19.8189208985259,12.6284362839445,
130.504164057257)) ;
#125459 = CARTESIAN_POINT('Ctrl Pts',(-19.9078147749595,12.4304595143626,
130.730514989918)) ;
#125460 = CARTESIAN_POINT('Ctrl Pts',(-20.0095479920409,12.3053999518157,
130.994813742423)) ;
#125461 = CARTESIAN_POINT('Ctrl Pts',(-20.1201667027676,12.2593484399968,
131.284622101872)) ;
#125462 = CARTESIAN_POINT('Ctrl Pts',(-20.2296622699611,12.2965483921961,
131.571617133664)) ;
#125463 = CARTESIAN_POINT('Ctrl Pts',(-20.3339911299089,12.4156949295869,
131.842988009414)) ;
#125464 = CARTESIAN_POINT('Ctrl Pts',(-20.4233888978307,12.6050470782002,
132.071237235801)) ;
#125465 = CARTESIAN_POINT('Ctrl Pts',(-20.4945228765996,12.85534209768,132.245732745191)) ;
#125466 = CARTESIAN_POINT('Ctrl Pts',(-20.5413967325497,13.1429454569684,
132.349789520615)) ;
#125467 = CARTESIAN_POINT('Ctrl Pts',(-20.562611118273,13.4543917047447,132.378442216463)) ;
#125468 = CARTESIAN_POINT('Ctrl Pts',(-20.5565479376348,13.7614620059086,
132.327653889222)) ;
#125469 = CARTESIAN_POINT('Ctrl Pts',(-20.5247270670738,14.0447128346805,
132.201571129089)) ;
#125470 = CARTESIAN_POINT('Ctrl Pts',(-20.4702093585612,14.2828873109444,
132.009265977188)) ;
#125471 = CARTESIAN_POINT('Ctrl Pts',(-20.3974418851067,14.4603132478387,
131.763573851832)) ;
#125472 = CARTESIAN_POINT('Ctrl Pts',(-20.3119076274948,14.5634617520393,
131.480411939824)) ;
#125473 = CARTESIAN_POINT('Ctrl Pts',(-20.221960576711,14.5844329879889,131.184735879175)) ;
#125474 = CARTESIAN_POINT('Ctrl Pts',(-20.1329704818831,14.5225343310152,
130.891550458131)) ;
#125475 = CARTESIAN_POINT('Ctrl Pts',(-20.0531091686615,14.381544806336,130.625116747778)) ;
#125476 = CARTESIAN_POINT('Ctrl Pts',(-19.9886753908938,14.1725754677665,
130.403826414472)) ;
#125477 = CARTESIAN_POINT('Ctrl Pts',(-19.9447676258649,13.9093040451571,
130.242407723814)) ;
#125478 = CARTESIAN_POINT('Ctrl Pts',(-19.9253917310527,13.6121558294026,
130.152761370539)) ;
#125479 = CARTESIAN_POINT('Ctrl Pts',(-19.9327640731267,13.2990170967779,
130.140983614842)) ;
#125480 = CARTESIAN_POINT('Ctrl Pts',(-19.966784211622,12.9981565078101,130.207424474512)) ;
#125481 = CARTESIAN_POINT('Ctrl Pts',(-20.0259934420432,12.7257032392755,
130.347241404834)) ;
#125482 = CARTESIAN_POINT('Ctrl Pts',(-20.1071478867376,12.50307580565,130.551095389013)) ;
#125483 = CARTESIAN_POINT('Ctrl Pts',(-20.2043408359347,12.3471529691752,
130.801978619226)) ;
#125484 = CARTESIAN_POINT('Ctrl Pts',(-20.3126508795515,12.2678408556735,
131.085078506438)) ;
#125485 = CARTESIAN_POINT('Ctrl Pts',(-20.4229187326262,12.2715869300384,
131.374306233546)) ;
#125486 = CARTESIAN_POINT('Ctrl Pts',(-20.5302578375964,12.3575776259723,
131.654678476933)) ;
#125487 = CARTESIAN_POINT('Ctrl Pts',(-20.6264204325903,12.5198592417277,
131.902499896415)) ;
#125488 = CARTESIAN_POINT('Ctrl Pts',(-20.7057938697997,12.7472701152985,
132.101187732545)) ;
#125489 = CARTESIAN_POINT('Ctrl Pts',(-20.7630472962772,13.0233715005783,
132.235259403599)) ;
#125490 = CARTESIAN_POINT('Ctrl Pts',(-20.7947740167793,13.3264775703159,
132.294936955644)) ;
#125491 = CARTESIAN_POINT('Ctrl Pts',(-20.7998253098923,13.6374829528976,
132.276579789714)) ;
#125492 = CARTESIAN_POINT('Ctrl Pts',(-20.7781798467671,13.9340523066843,
132.180125678852)) ;
#125493 = CARTESIAN_POINT('Ctrl Pts',(-20.7323182863517,14.1931239778517,
132.013032839121)) ;
#125494 = CARTESIAN_POINT('Ctrl Pts',(-20.6659952400125,14.3974304902421,
131.78607443323)) ;
#125495 = CARTESIAN_POINT('Ctrl Pts',(-20.5854240712101,14.5309245532204,
131.517722674269)) ;
#125496 = CARTESIAN_POINT('Ctrl Pts',(-20.4962685721323,14.5859814539265,
131.224148101963)) ;
#125497 = CARTESIAN_POINT('Ctrl Pts',(-20.4058963569354,14.5574777806989,
130.927001172984)) ;
#125498 = CARTESIAN_POINT('Ctrl Pts',(-20.3216691370053,14.4480150523887,
130.647857808576)) ;
#125499 = CARTESIAN_POINT('Ctrl Pts',(-20.2499907856577,14.2640746902433,
130.405219408407)) ;
#125500 = CARTESIAN_POINT('Ctrl Pts',(-20.1974565013379,14.0222278683344,
130.218833806972)) ;
#125501 = CARTESIAN_POINT('Ctrl Pts',(-20.1675706919809,13.7339092296597,
130.098157959704)) ;
#125502 = CARTESIAN_POINT('Ctrl Pts',(-20.1640677436926,13.4264443376891,
130.054932391349)) ;
#125503 = CARTESIAN_POINT('Ctrl Pts',(-20.1873548159157,13.1179337351116,
130.089866611451)) ;
#125504 = CARTESIAN_POINT('Ctrl Pts',(-20.2367558298266,12.8308236558004,
130.201047137032)) ;
#125505 = CARTESIAN_POINT('Ctrl Pts',(-20.3095840954364,12.5859821192932,
130.380611728237)) ;
#125506 = CARTESIAN_POINT('Ctrl Pts',(-20.4006241545898,12.4020104607834,
130.613571603836)) ;
#125507 = CARTESIAN_POINT('Ctrl Pts',(-20.5055712162227,12.2899875616105,
130.886838354764)) ;
#125508 = CARTESIAN_POINT('Ctrl Pts',(-20.6158038744858,12.260124778228,131.175836440016)) ;
#125509 = CARTESIAN_POINT('Ctrl Pts',(-20.725325813667,12.3130229090721,131.46266764125)) ;
#125510 = CARTESIAN_POINT('Ctrl Pts',(-20.8268144993231,12.445755568189,131.72599885581)) ;
#125511 = CARTESIAN_POINT('Ctrl Pts',(-20.9134907572975,12.6478749143986,
131.94613786665)) ;
#125512 = CARTESIAN_POINT('Ctrl Pts',(-20.9804389337324,12.9074235529971,
132.108409295979)) ;
#125513 = CARTESIAN_POINT('Ctrl Pts',(-21.0226586722023,13.201587990353,132.198739885101)) ;
#125514 = CARTESIAN_POINT('Ctrl Pts',(-21.0386105188704,13.5132462797945,
132.212140657446)) ;
#125515 = CARTESIAN_POINT('Ctrl Pts',(-21.0275858269164,13.8170405083281,
132.14689488238)) ;
#125516 = CARTESIAN_POINT('Ctrl Pts',(-20.9912734830522,14.0930904717493,
132.007734125149)) ;
#125517 = CARTESIAN_POINT('Ctrl Pts',(-20.9328468771947,14.3215765569393,
131.803931803933)) ;
#125518 = CARTESIAN_POINT('Ctrl Pts',(-20.8569974472105,14.4860164684736,
131.549134598391)) ;
#125519 = CARTESIAN_POINT('Ctrl Pts',(-20.7703215178779,14.5737422146348,
131.262802859148)) ;
#125520 = CARTESIAN_POINT('Ctrl Pts',(-20.6795334980067,14.5789283273619,
130.964434672584)) ;
#125521 = CARTESIAN_POINT('Ctrl Pts',(-20.5922289646685,14.5018179973275,
130.676378069679)) ;
#125522 = CARTESIAN_POINT('Ctrl Pts',(-20.5145673896872,14.3465570817491,
130.416269496224)) ;
#125523 = CARTESIAN_POINT('Ctrl Pts',(-20.4538879568746,14.1268974135735,
130.206064475321)) ;
#125524 = CARTESIAN_POINT('Ctrl Pts',(-20.4142221803974,13.8551171351805,
130.056974334884)) ;
#125525 = CARTESIAN_POINT('Ctrl Pts',(-20.3998288749854,13.5530512913373,
129.981815424211)) ;
#125526 = CARTESIAN_POINT('Ctrl Pts',(-20.4122289800202,13.2415863722887,
129.98490917036)) ;
#125527 = CARTESIAN_POINT('Ctrl Pts',(-20.451304951926,12.9431696446184,130.06593789593)) ;
#125528 = CARTESIAN_POINT('Ctrl Pts',(-20.5150277326967,12.6789855652346,
130.218945397434)) ;
#125529 = CARTESIAN_POINT('Ctrl Pts',(-20.59938870539,12.4685393411929,130.432298405932)) ;
#125530 = CARTESIAN_POINT('Ctrl Pts',(-20.6990677999997,12.3261974567536,
130.690420636)) ;
#125531 = CARTESIAN_POINT('Ctrl Pts',(-20.8083842807917,12.2622045863294,
130.976510913894)) ;
#125532 = CARTESIAN_POINT('Ctrl Pts',(-20.9188027504055,12.2815898353466,
131.266074603366)) ;
#125533 = CARTESIAN_POINT('Ctrl Pts',(-21.0244452528796,12.3824517800912,
131.541548083244)) ;
#125534 = CARTESIAN_POINT('Ctrl Pts',(-21.118092393428,12.5585397023802,131.781921448334)) ;
#125535 = CARTESIAN_POINT('Ctrl Pts',(-21.1933604529092,12.7954955062998,
131.968753676057)) ;
#125536 = CARTESIAN_POINT('Ctrl Pts',(-21.2462570078652,13.0796940190917,
132.089961785782)) ;
#125537 = CARTESIAN_POINT('Ctrl Pts',(-21.2729118079994,13.3852304458179,
132.134891546362)) ;
#125538 = CARTESIAN_POINT('Ctrl Pts',(-21.2728211559508,13.69604445911,132.101399472322)) ;
#125539 = CARTESIAN_POINT('Ctrl Pts',(-21.2464415175453,13.985866733445,131.991275439313)) ;
#125540 = CARTESIAN_POINT('Ctrl Pts',(-21.1964399533081,14.2358877356182,
131.812083957128)) ;
#125541 = CARTESIAN_POINT('Ctrl Pts',(-21.1272541863527,14.4275999337175,
131.57690711089)) ;
#125542 = CARTESIAN_POINT('Ctrl Pts',(-21.0437448885435,14.5480862858471,
131.299621047924)) ;
#125543 = CARTESIAN_POINT('Ctrl Pts',(-20.9541410393014,14.5868446718797,
131.004870001721)) ;
#125544 = CARTESIAN_POINT('Ctrl Pts',(-20.8645870046891,14.5430357670067,
130.71019710521)) ;
#125545 = CARTESIAN_POINT('Ctrl Pts',(-20.7821504245794,14.41874401797,130.436229232474)) ;
#125546 = CARTESIAN_POINT('Ctrl Pts',(-20.7137193836823,14.2230681528207,
130.203180502296)) ;
#125547 = CARTESIAN_POINT('Ctrl Pts',(-20.6649423891261,13.9697197453762,
130.027517386602)) ;
#125548 = CARTESIAN_POINT('Ctrl Pts',(-20.6400754360656,13.6787523324498,
129.921874279192)) ;
#125549 = CARTESIAN_POINT('Ctrl Pts',(-20.6414819785661,13.3668522755562,
129.892691132996)) ;
#125550 = CARTESIAN_POINT('Ctrl Pts',(-20.6699979410068,13.060672465625,129.942883851846)) ;
#125551 = CARTESIAN_POINT('Ctrl Pts',(-20.7238971217684,12.7810810976344,
130.067313557987)) ;
#125552 = CARTESIAN_POINT('Ctrl Pts',(-20.8004298736072,12.5467077229853,
130.257772798001)) ;
#125553 = CARTESIAN_POINT('Ctrl Pts',(-20.8945661196432,12.375036029875,130.499700142091)) ;
#125554 = CARTESIAN_POINT('Ctrl Pts',(-21.0013745401089,12.2779852364334,
130.778361903145)) ;
#125555 = CARTESIAN_POINT('Ctrl Pts',(-21.1116666074204,12.263745955446,131.067624667673)) ;
#125556 = CARTESIAN_POINT('Ctrl Pts',(-21.2204165815676,12.3321871906188,
131.352129032139)) ;
#125557 = CARTESIAN_POINT('Ctrl Pts',(-21.3195254329621,12.4786900321498,
131.608553898707)) ;
#125558 = CARTESIAN_POINT('Ctrl Pts',(-21.4032330604707,12.6941599570478,
131.81980234989)) ;
#125559 = CARTESIAN_POINT('Ctrl Pts',(-21.4652019062618,12.9594898311094,
131.967877269519)) ;
#125560 = CARTESIAN_POINT('Ctrl Pts',(-21.5028731218885,13.2597802878034,
132.044736719879)) ;
#125561 = CARTESIAN_POINT('Ctrl Pts',(-21.5136586591111,13.5705933911082,
132.043193173102)) ;
#125562 = CARTESIAN_POINT('Ctrl Pts',(-21.4977998320591,13.8717555022921,
131.963723980422)) ;
#125563 = CARTESIAN_POINT('Ctrl Pts',(-21.4566374898941,14.1416796956212,
131.810184445512)) ;
#125564 = CARTESIAN_POINT('Ctrl Pts',(-21.3949269775792,14.3575208853318,
131.597015858169)) ;
#125565 = CARTESIAN_POINT('Ctrl Pts',(-21.3163223809269,14.5088742851846,
131.334081154852)) ;
#125566 = CARTESIAN_POINT('Ctrl Pts',(-21.2283674664414,14.5810485932283,
131.044035253294)) ;
#125567 = CARTESIAN_POINT('Ctrl Pts',(-21.1379878817008,14.5707018107426,
130.74699291225)) ;
#125568 = CARTESIAN_POINT('Ctrl Pts',(-21.0518809543132,14.4785662345022,
130.46236961443)) ;
#125569 = CARTESIAN_POINT('Ctrl Pts',(-20.976718142438,14.3096045878152,130.209508594268)) ;
#125570 = CARTESIAN_POINT('Ctrl Pts',(-20.9195313547551,14.0777449679159,
130.009336738625)) ;
#125571 = CARTESIAN_POINT('Ctrl Pts',(-20.8846809598118,13.8001341455209,
129.874521428525)) ;
#125572 = CARTESIAN_POINT('Ctrl Pts',(-20.8751865502058,13.4946152703642,
129.813664552878)) ;
#125573 = CARTESIAN_POINT('Ctrl Pts',(-20.8927061896601,13.1837406589244,
129.831697274769)) ;
#125574 = CARTESIAN_POINT('Ctrl Pts',(-20.9365995694632,12.8901082273082,
129.926795681337)) ;
#125575 = CARTESIAN_POINT('Ctrl Pts',(-21.0049177915536,12.6339160706406,
130.093104476252)) ;
#125576 = CARTESIAN_POINT('Ctrl Pts',(-21.0920187661593,12.4365925645623,
130.314691586752)) ;
#125577 = CARTESIAN_POINT('Ctrl Pts',(-21.1945890656971,12.3075969590058,
130.581034844336)) ;
#125578 = CARTESIAN_POINT('Ctrl Pts',(-21.3041078767494,12.2595413699531,
130.867941860621)) ;
#125579 = CARTESIAN_POINT('Ctrl Pts',(-21.414714087137,12.2945981250866,131.157860792763)) ;
#125580 = CARTESIAN_POINT('Ctrl Pts',(-21.5182505698646,12.4101972577176,
131.42728025094)) ;
#125581 = CARTESIAN_POINT('Ctrl Pts',(-21.6088669941318,12.598715944425,131.658831153717)) ;
#125582 = CARTESIAN_POINT('Ctrl Pts',(-21.6803208590174,12.8461743706132,
131.834442515426)) ;
#125583 = CARTESIAN_POINT('Ctrl Pts',(-21.7283998303603,13.1359262374288,
131.941663820147)) ;
#125584 = CARTESIAN_POINT('Ctrl Pts',(-21.7501146102558,13.4447581529336,
131.97204316023)) ;
#125585 = CARTESIAN_POINT('Ctrl Pts',(-21.7448694054129,13.7530929209566,
131.923542338584)) ;
#125586 = CARTESIAN_POINT('Ctrl Pts',(-21.7138911823186,14.0362080508941,
131.800059197407)) ;
#125587 = CARTESIAN_POINT('Ctrl Pts',(-21.6598673248284,14.2769560090218,
131.609081968409)) ;
#125588 = CARTESIAN_POINT('Ctrl Pts',(-21.5873536841721,14.4563581984587,
131.364074061383)) ;
#125589 = CARTESIAN_POINT('Ctrl Pts',(-21.5026599241299,14.5613193565883,
131.083584293766)) ;
#125590 = CARTESIAN_POINT('Ctrl Pts',(-21.4121679015584,14.5851466740993,
130.786094569346)) ;
#125591 = CARTESIAN_POINT('Ctrl Pts',(-21.3229798957179,14.5250094201889,
130.492300414709)) ;
#125592 = CARTESIAN_POINT('Ctrl Pts',(-21.2431880284182,14.3871118872338,
130.226257623174)) ;
#125593 = CARTESIAN_POINT('Ctrl Pts',(-21.1778843641689,14.1786613146333,
130.002228172161)) ;
#125594 = CARTESIAN_POINT('Ctrl Pts',(-21.1335446386563,13.9181921404444,
129.839744069384)) ;
#125595 = CARTESIAN_POINT('Ctrl Pts',(-21.1133238256431,13.6189922621126,
129.747319744249)) ;
#125596 = CARTESIAN_POINT('Ctrl Pts',(-21.1199394173291,13.3089360963624,
129.733660018502)) ;
#125597 = CARTESIAN_POINT('Ctrl Pts',(-21.15326877726,13.0058324971489,129.797902039434)) ;
#125598 = CARTESIAN_POINT('Ctrl Pts',(-21.2120574557122,12.7318651916952,
129.936425658188)) ;
#125599 = CARTESIAN_POINT('Ctrl Pts',(-21.2925597772729,12.5082426234418,
130.138441418088)) ;
#125600 = CARTESIAN_POINT('Ctrl Pts',(-21.3890394795578,12.3508732167538,
130.387352736043)) ;
#125601 = CARTESIAN_POINT('Ctrl Pts',(-21.496781967904,12.2691036353101,130.668897537391)) ;
#125602 = CARTESIAN_POINT('Ctrl Pts',(-21.6076020846144,12.2702137418504,
130.959576850838)) ;
#125603 = CARTESIAN_POINT('Ctrl Pts',(-21.7152916878763,12.3542930287051,
131.240924005532)) ;
#125604 = CARTESIAN_POINT('Ctrl Pts',(-21.8115660696969,12.5141177100409,
131.489166666111)) ;
#125605 = CARTESIAN_POINT('Ctrl Pts',(-21.8914520404614,12.7395234896818,
131.689386122552)) ;
#125606 = CARTESIAN_POINT('Ctrl Pts',(-21.949435548747,13.0142280160873,131.825609613672)) ;
#125607 = CARTESIAN_POINT('Ctrl Pts',(-21.9820492110329,13.3177663479764,
131.887772553571)) ;
#125608 = CARTESIAN_POINT('Ctrl Pts',(-21.9878167428512,13.6286638171374,
131.871529705244)) ;
#125609 = CARTESIAN_POINT('Ctrl Pts',(-21.9670224795337,13.925291931835,131.777646134426)) ;
#125610 = CARTESIAN_POINT('Ctrl Pts',(-21.9217757158089,14.1860950196788,
131.61230143831)) ;
#125611 = CARTESIAN_POINT('Ctrl Pts',(-21.8562405122822,14.3917324528471,
131.387756932998)) ;
#125612 = CARTESIAN_POINT('Ctrl Pts',(-21.7756903472869,14.5282787585867,
131.119317953133)) ;
#125613 = CARTESIAN_POINT('Ctrl Pts',(-21.6864909606961,14.585553871015,130.825554832936)) ;
#125614 = CARTESIAN_POINT('Ctrl Pts',(-21.5963140146045,14.5594424124574,
130.529072362239)) ;
#125615 = CARTESIAN_POINT('Ctrl Pts',(-21.5118873080126,14.452533822029,130.249380272377)) ;
#125616 = CARTESIAN_POINT('Ctrl Pts',(-21.4396023594563,14.2704301815678,
130.004922447039)) ;
#125617 = CARTESIAN_POINT('Ctrl Pts',(-21.3864210307148,14.0294404722423,
129.816576108765)) ;
#125618 = CARTESIAN_POINT('Ctrl Pts',(-21.3559418238359,13.7439522492757,
129.694376590572)) ;
#125619 = CARTESIAN_POINT('Ctrl Pts',(-21.3515590072131,13.4354033023599,
129.648418578587)) ;
#125620 = CARTESIAN_POINT('Ctrl Pts',(-21.3740511377046,13.1268757917154,
129.681069437497)) ;
#125621 = CARTESIAN_POINT('Ctrl Pts',(-21.4229183024262,12.8380942366352,
129.790589937005)) ;
#125622 = CARTESIAN_POINT('Ctrl Pts',(-21.4946813071599,12.5930207366324,
129.967235280058)) ;
#125623 = CARTESIAN_POINT('Ctrl Pts',(-21.5858119382305,12.406038861412,130.200252155053)) ;
#125624 = CARTESIAN_POINT('Ctrl Pts',(-21.68959704384,12.292531234905,130.470405728911)) ;
#125625 = CARTESIAN_POINT('Ctrl Pts',(-21.8006640611008,12.259700175239,130.761558183255)) ;
#125626 = CARTESIAN_POINT('Ctrl Pts',(-21.9100727883452,12.3104428593725,
131.048134164405)) ;
#125627 = CARTESIAN_POINT('Ctrl Pts',(-22.0119946874219,12.4411375655696,
131.312691934815)) ;
#125628 = CARTESIAN_POINT('Ctrl Pts',(-22.0989549674782,12.6410412802729,
131.533737469327)) ;
#125629 = CARTESIAN_POINT('Ctrl Pts',(-22.1665960353877,12.8990710258353,
131.698038077876)) ;
#125630 = CARTESIAN_POINT('Ctrl Pts',(-22.2096292017843,13.1932159520557,
131.790663136746)) ;
#125631 = CARTESIAN_POINT('Ctrl Pts',(-22.2263015712469,13.5039484440362,
131.80625317794)) ;
#125632 = CARTESIAN_POINT('Ctrl Pts',(-22.2160709879322,13.8084630693567,
131.743303504259)) ;
#125633 = CARTESIAN_POINT('Ctrl Pts',(-22.1804532453563,14.0856215831729,
131.606173872007)) ;
#125634 = CARTESIAN_POINT('Ctrl Pts',(-22.1226056277055,14.3156974837171,
131.404064385855)) ;
#125635 = CARTESIAN_POINT('Ctrl Pts',(-22.0473303523545,14.482069329469,131.1510040704)) ;
#125636 = CARTESIAN_POINT('Ctrl Pts',(-21.9607116573561,14.5722583544091,
130.864770552622)) ;
#125637 = CARTESIAN_POINT('Ctrl Pts',(-21.8703953183131,14.5801736799871,
130.567952070754)) ;
#125638 = CARTESIAN_POINT('Ctrl Pts',(-21.7822499355248,14.5050113517495,
130.277192893103)) ;
#125639 = CARTESIAN_POINT('Ctrl Pts',(-21.7044840301903,14.3522164750112,
130.01689633979)) ;
#125640 = CARTESIAN_POINT('Ctrl Pts',(-21.6431388088135,14.1339602612738,
129.804686049646)) ;
#125641 = CARTESIAN_POINT('Ctrl Pts',(-21.6028682983574,13.8641112712326,
129.65391825805)) ;
#125642 = CARTESIAN_POINT('Ctrl Pts',(-21.5876385948603,13.5616225014003,
129.576198403786)) ;
#125643 = CARTESIAN_POINT('Ctrl Pts',(-21.5992932161767,13.2502934236062,
129.577137522919)) ;
#125644 = CARTESIAN_POINT('Ctrl Pts',(-21.6376942912837,12.9509782560257,
129.656163454282)) ;
#125645 = CARTESIAN_POINT('Ctrl Pts',(-21.7005423302571,12.6863948819192,
129.806725409211)) ;
#125646 = CARTESIAN_POINT('Ctrl Pts',(-21.7845354885147,12.4734606146631,
130.018920464526)) ;
#125647 = CARTESIAN_POINT('Ctrl Pts',(-21.8843134729441,12.3287823734524,
130.277199856625)) ;
#125648 = CARTESIAN_POINT('Ctrl Pts',(-21.9929392570174,12.262963408062,130.561438527531)) ;
#125649 = CARTESIAN_POINT('Ctrl Pts',(-22.1035861834769,12.2798963364109,
130.851612471303)) ;
#125650 = CARTESIAN_POINT('Ctrl Pts',(-22.2095302910128,12.3786944152069,
131.127948672773)) ;
#125651 = CARTESIAN_POINT('Ctrl Pts',(-22.3037053420613,12.5532637477409,
131.369814961767)) ;
#125652 = CARTESIAN_POINT('Ctrl Pts',(-22.3791978821218,12.7879392173085,
131.557427905372)) ;
#125653 = CARTESIAN_POINT('Ctrl Pts',(-22.432676499044,13.0695371613245,131.68049834232)) ;
#125654 = CARTESIAN_POINT('Ctrl Pts',(-22.460347286562,13.3764287313842,131.728200911231)) ;
#125655 = CARTESIAN_POINT('Ctrl Pts',(-22.460962142873,13.6873693944069,131.696780968098)) ;
#125656 = CARTESIAN_POINT('Ctrl Pts',(-22.4353608541561,13.9780097537181,
131.58894187598)) ;
#125657 = CARTESIAN_POINT('Ctrl Pts',(-22.385713314181,14.2303816916052,131.410644205357)) ;
#125658 = CARTESIAN_POINT('Ctrl Pts',(-22.3171996696004,14.4229832275646,
131.177555141404)) ;
#125659 = CARTESIAN_POINT('Ctrl Pts',(-22.2342095372013,14.545607197334,130.901858853861)) ;
#125660 = CARTESIAN_POINT('Ctrl Pts',(-22.1445457999827,14.5869244372964,
130.606872978911)) ;
#125661 = CARTESIAN_POINT('Ctrl Pts',(-22.0548221478016,14.545413999477,130.311682615408)) ;
#125662 = CARTESIAN_POINT('Ctrl Pts',(-21.9720637241757,14.4231615318539,
130.036761175897)) ;
#125663 = CARTESIAN_POINT('Ctrl Pts',(-21.9033593370502,14.2299646003197,
129.803014658946)) ;
#125664 = CARTESIAN_POINT('Ctrl Pts',(-21.8538582145753,13.9782380349311,
129.625238447864)) ;
#125665 = CARTESIAN_POINT('Ctrl Pts',(-21.8282135190343,13.6869896701315,
129.517199857734)) ;
#125666 = CARTESIAN_POINT('Ctrl Pts',(-21.8288197658371,13.3772462280803,
129.48588557063)) ;
#125667 = CARTESIAN_POINT('Ctrl Pts',(-21.8564296864021,13.0701026348063,
129.533383001369)) ;
#125668 = CARTESIAN_POINT('Ctrl Pts',(-21.9098344339023,12.7883757721948,
129.656241120906)) ;
#125669 = CARTESIAN_POINT('Ctrl Pts',(-21.9857856890572,12.5524788061311,
129.84500715286)) ;
#125670 = CARTESIAN_POINT('Ctrl Pts',(-22.0796909556344,12.3787205922408,
130.086201475717)) ;
#125671 = CARTESIAN_POINT('Ctrl Pts',(-22.1856098910202,12.2799428361804,
130.362465376775)) ;
#125672 = CARTESIAN_POINT('Ctrl Pts',(-22.2961046110537,12.26278144672,130.652245503551)) ;
#125673 = CARTESIAN_POINT('Ctrl Pts',(-22.4056125857822,12.3295044441556,
130.938781716438)) ;
#125674 = CARTESIAN_POINT('Ctrl Pts',(-22.5045503687808,12.4735104762095,
131.194864039758)) ;
#125675 = CARTESIAN_POINT('Ctrl Pts',(-22.5885187900511,12.6859036202202,
131.407023886207)) ;
#125676 = CARTESIAN_POINT('Ctrl Pts',(-22.6515372036972,12.9511128750471,
131.558004821108)) ;
#125677 = CARTESIAN_POINT('Ctrl Pts',(-22.689964997057,13.2510042881428,131.637050794627)) ;
#125678 = CARTESIAN_POINT('Ctrl Pts',(-22.7015161637052,13.5624349033162,
131.637676113596)) ;
#125679 = CARTESIAN_POINT('Ctrl Pts',(-22.686344284073,13.8634351893562,131.560285852855)) ;
#125680 = CARTESIAN_POINT('Ctrl Pts',(-22.6462161333374,14.1332614315187,
131.409958331396)) ;
#125681 = CARTESIAN_POINT('Ctrl Pts',(-22.5846264147229,14.3526410215066,
131.196887959862)) ;
#125682 = CARTESIAN_POINT('Ctrl Pts',(-22.506540094871,14.5054039917793,130.935553228196)) ;
#125683 = CARTESIAN_POINT('Ctrl Pts',(-22.4191482201114,14.5799567731311,
130.647279826546)) ;
#125684 = CARTESIAN_POINT('Ctrl Pts',(-22.3283933686161,14.572371407252,130.349018922444)) ;
#125685 = CARTESIAN_POINT('Ctrl Pts',(-22.2417737954577,14.4818104179813,
130.062771911775)) ;
#125686 = CARTESIAN_POINT('Ctrl Pts',(-22.1668084149478,14.3163442533983,
129.810766300736)) ;
#125687 = CARTESIAN_POINT('Ctrl Pts',(-22.1087759662198,14.0859120132609,
129.608039485136)) ;
#125688 = CARTESIAN_POINT('Ctrl Pts',(-22.0731170711164,13.8088757639041,
129.470801563983)) ;
#125689 = CARTESIAN_POINT('Ctrl Pts',(-22.0628921530061,13.5028415696086,
129.407702944784)) ;
#125690 = CARTESIAN_POINT('Ctrl Pts',(-22.0795605465254,13.1931030740132,
129.423392458417)) ;
#125691 = CARTESIAN_POINT('Ctrl Pts',(-22.1228245546184,12.8979592088334,
129.516564666613)) ;
#125692 = CARTESIAN_POINT('Ctrl Pts',(-22.1900878866385,12.6415806575113,
129.679968460052)) ;
#125693 = CARTESIAN_POINT('Ctrl Pts',(-22.2772779130057,12.4408172036161,
129.901573943192)) ;
#125694 = CARTESIAN_POINT('Ctrl Pts',(-22.379557207116,12.3100401552364,130.167079846431)) ;
#125695 = CARTESIAN_POINT('Ctrl Pts',(-22.4887216341412,12.2598615756175,
130.453018076937)) ;
#125696 = CARTESIAN_POINT('Ctrl Pts',(-22.5991744377342,12.2922205464447,
130.742565298188)) ;
#125697 = CARTESIAN_POINT('Ctrl Pts',(-22.7035453793508,12.40624849515,131.014244429529)) ;
#125698 = CARTESIAN_POINT('Ctrl Pts',(-22.7943699277688,12.5927140641391,
131.246477725961)) ;
#125699 = CARTESIAN_POINT('Ctrl Pts',(-22.8662655898373,12.8381488954601,
131.423450080432)) ;
#125700 = CARTESIAN_POINT('Ctrl Pts',(-22.9150550731725,13.1260095358548,
131.532846123897)) ;
#125701 = CARTESIAN_POINT('Ctrl Pts',(-22.9376902134472,13.4367097241923,
131.565680322971)) ;
#125702 = CARTESIAN_POINT('Ctrl Pts',(-22.9331885517525,13.7438376773702,
131.519521875637)) ;
#125703 = CARTESIAN_POINT('Ctrl Pts',(-22.9029068463003,14.0287736558089,
131.397981832409)) ;
#125704 = CARTESIAN_POINT('Ctrl Pts',(-22.8494229071779,14.2709621799374,
131.20857762131)) ;
#125705 = CARTESIAN_POINT('Ctrl Pts',(-22.7775004359681,14.4520608011874,
130.965354382792)) ;
#125706 = CARTESIAN_POINT('Ctrl Pts',(-22.6929376253596,14.5594794464979,
130.685194528285)) ;
#125707 = CARTESIAN_POINT('Ctrl Pts',(-22.6026883853366,14.5855261750269,
130.38847763073)) ;
#125708 = CARTESIAN_POINT('Ctrl Pts',(-22.5135631277621,14.5283738687936,
130.094960233559)) ;
#125709 = CARTESIAN_POINT('Ctrl Pts',(-22.4329133576036,14.3916536122689,
129.826188034227)) ;
#125710 = CARTESIAN_POINT('Ctrl Pts',(-22.367483851615,14.1863632945959,129.602008031043)) ;
#125711 = CARTESIAN_POINT('Ctrl Pts',(-22.3222022530891,13.9255968041967,
129.43655632992)) ;
#125712 = CARTESIAN_POINT('Ctrl Pts',(-22.3013824069524,13.6292800303555,
129.342629054356)) ;
#125713 = CARTESIAN_POINT('Ctrl Pts',(-22.3071114891914,13.3179689166563,
129.326228873449)) ;
#125714 = CARTESIAN_POINT('Ctrl Pts',(-22.3397290895377,13.0144328238462,
129.388404090424)) ;
#125715 = CARTESIAN_POINT('Ctrl Pts',(-22.3975763598925,12.7401667038842,
129.524286626664)) ;
#125716 = CARTESIAN_POINT('Ctrl Pts',(-22.4774181520926,12.5144106692782,
129.724364422283)) ;
#125717 = CARTESIAN_POINT('Ctrl Pts',(-22.5741193712273,12.3540784251448,
129.973715242602)) ;
#125718 = CARTESIAN_POINT('Ctrl Pts',(-22.6811523681517,12.2704506674806,
130.253347738944)) ;
#125719 = CARTESIAN_POINT('Ctrl Pts',(-22.7923265389067,12.2689821034606,
130.544952223405)) ;
#125720 = CARTESIAN_POINT('Ctrl Pts',(-22.9001417640839,12.350850990926,130.826689686085)) ;
#125721 = CARTESIAN_POINT('Ctrl Pts',(-22.9968454884217,12.5086055972373,
131.076177637184)) ;
#125722 = CARTESIAN_POINT('Ctrl Pts',(-23.0774719156549,12.7330677829212,
131.278472278326)) ;
#125723 = CARTESIAN_POINT('Ctrl Pts',(-23.1359818046982,13.0066124889692,
131.416256845004)) ;
#125724 = CARTESIAN_POINT('Ctrl Pts',(-23.1692213521271,13.308272601369,131.480391873357)) ;
#125725 = CARTESIAN_POINT('Ctrl Pts',(-23.1758458307034,13.6201713325224,
131.466556851235)) ;
#125726 = CARTESIAN_POINT('Ctrl Pts',(-23.1556315248226,13.9183341039009,
131.374269427024)) ;
#125727 = CARTESIAN_POINT('Ctrl Pts',(-23.1110228710728,14.1797388278147,
131.210851244888)) ;
#125728 = CARTESIAN_POINT('Ctrl Pts',(-23.0462187780778,14.3864987369051,
130.988550039522)) ;
#125729 = CARTESIAN_POINT('Ctrl Pts',(-22.966063587632,14.5252641755352,130.721275013867)) ;
#125730 = CARTESIAN_POINT('Ctrl Pts',(-22.8769915510678,14.5851721038055,
130.42787569678)) ;
#125731 = CARTESIAN_POINT('Ctrl Pts',(-22.7862418920941,14.5610669162746,
130.129530157643)) ;
#125732 = CARTESIAN_POINT('Ctrl Pts',(-22.7020506121271,14.4566509798001,
129.850704631775)) ;
#125733 = CARTESIAN_POINT('Ctrl Pts',(-22.6293418474591,14.2771545198569,
129.605059764206)) ;
#125734 = CARTESIAN_POINT('Ctrl Pts',(-22.5753044942391,14.0362065305465,
129.414025275407)) ;
#125735 = CARTESIAN_POINT('Ctrl Pts',(-22.5443289524662,13.753398715095,129.290579678709)) ;
#125736 = CARTESIAN_POINT('Ctrl Pts',(-22.5390419745757,13.4441283585126,
129.241859045919)) ;
#125737 = CARTESIAN_POINT('Ctrl Pts',(-22.5609786844499,13.1346408966579,
129.272806550467)) ;
#125738 = CARTESIAN_POINT('Ctrl Pts',(-22.6086912148905,12.8470251737848,
129.379206459385)) ;
#125739 = CARTESIAN_POINT('Ctrl Pts',(-22.6803934288997,12.5984937869307,
129.555405712019)) ;
#125740 = CARTESIAN_POINT('Ctrl Pts',(-22.7705691384996,12.4108688278635,
129.785832773901)) ;
#125741 = CARTESIAN_POINT('Ctrl Pts',(-22.8742759459874,12.2946081096869,
130.055675073743)) ;
#125742 = CARTESIAN_POINT('Ctrl Pts',(-22.9853475814919,12.2594450533974,
130.346820691978)) ;
#125743 = CARTESIAN_POINT('Ctrl Pts',(-23.0949607973134,12.30804814686,130.633963194578)) ;
#125744 = CARTESIAN_POINT('Ctrl Pts',(-23.1968663509126,12.4360760991486,
130.898588194265)) ;
#125745 = CARTESIAN_POINT('Ctrl Pts',(-23.2845187744347,12.634525822386,131.12158237805)) ;
#125746 = CARTESIAN_POINT('Ctrl Pts',(-23.352574330873,12.8902137015407,131.287216571131)) ;
#125747 = CARTESIAN_POINT('Ctrl Pts',(-23.3964713954108,13.1836915440523,
131.382336055602)) ;
#125748 = CARTESIAN_POINT('Ctrl Pts',(-23.4139997612099,13.4943234250401,
131.400420925134)) ;
#125749 = CARTESIAN_POINT('Ctrl Pts',(-23.4044990531187,13.8008444914087,
131.339441224861)) ;
#125750 = CARTESIAN_POINT('Ctrl Pts',(-23.3693574684695,14.0793170573489,
131.203644426842)) ;
#125751 = CARTESIAN_POINT('Ctrl Pts',(-23.3123406169852,14.3098745304063,
131.004120413233)) ;
#125752 = CARTESIAN_POINT('Ctrl Pts',(-23.2371407307095,14.4788324739109,
130.751136748099)) ;
#125753 = CARTESIAN_POINT('Ctrl Pts',(-23.1511653084581,14.5706780118123,
130.466953543331)) ;
#125754 = CARTESIAN_POINT('Ctrl Pts',(-23.0606882221465,14.5811216563982,
130.169593581504)) ;
#125755 = CARTESIAN_POINT('Ctrl Pts',(-22.9725268245407,14.5082991498853,
129.878848830671)) ;
#125756 = CARTESIAN_POINT('Ctrl Pts',(-22.8944300957472,14.3580057871193,
129.61762284133)) ;
#125757 = CARTESIAN_POINT('Ctrl Pts',(-22.8322738880316,14.1405256903455,
129.402903517555)) ;
#125758 = CARTESIAN_POINT('Ctrl Pts',(-22.7914817526284,13.8719961113424,
129.250646984915)) ;
#125759 = CARTESIAN_POINT('Ctrl Pts',(-22.7754966150293,13.5716289607196,
129.170880112309)) ;
#125760 = CARTESIAN_POINT('Ctrl Pts',(-22.7863642218149,13.2591262832754,
129.169394891665)) ;
#125761 = CARTESIAN_POINT('Ctrl Pts',(-22.8238939066087,12.9599151059205,
129.245966509562)) ;
#125762 = CARTESIAN_POINT('Ctrl Pts',(-22.8862611929524,12.6930800437845,
129.395005704093)) ;
#125763 = CARTESIAN_POINT('Ctrl Pts',(-22.9696496692536,12.4788237616548,
129.605480629806)) ;
#125764 = CARTESIAN_POINT('Ctrl Pts',(-23.0687430408362,12.332247898292,129.861853849545)) ;
#125765 = CARTESIAN_POINT('Ctrl Pts',(-23.1773252167152,12.2636849567094,
130.14592080679)) ;
#125766 = CARTESIAN_POINT('Ctrl Pts',(-23.2883124035474,12.2782423804387,
130.437001735549)) ;
#125767 = CARTESIAN_POINT('Ctrl Pts',(-23.3943864358888,12.3748788763276,
130.713742699543)) ;
#125768 = CARTESIAN_POINT('Ctrl Pts',(-23.4886534469715,12.5463735135204,
130.956024389397)) ;
#125769 = CARTESIAN_POINT('Ctrl Pts',(-23.5652915574259,12.7810696956234,
131.146748612279)) ;
#125770 = CARTESIAN_POINT('Ctrl Pts',(-23.6192243080399,13.0608633683861,
131.271253850874)) ;
#125771 = CARTESIAN_POINT('Ctrl Pts',(-23.6477017970955,13.3671883117348,
131.321319852897)) ;
#125772 = CARTESIAN_POINT('Ctrl Pts',(-23.6491292020382,13.6783221132163,
131.292281615599)) ;
#125773 = CARTESIAN_POINT('Ctrl Pts',(-23.6242025058468,13.9701100820096,
131.18637040101)) ;
#125774 = CARTESIAN_POINT('Ctrl Pts',(-23.5754565039934,14.2230345342298,
131.010845400058)) ;
#125775 = CARTESIAN_POINT('Ctrl Pts',(-23.5070759200868,14.4186168912711,
130.777961630613)) ;
#125776 = CARTESIAN_POINT('Ctrl Pts',(-23.4247733783215,14.5428705870382,
130.504432836877)) ;
#125777 = CARTESIAN_POINT('Ctrl Pts',(-23.335040863465,14.5869069845901,130.209169715997)) ;
#125778 = CARTESIAN_POINT('Ctrl Pts',(-23.2452918150756,14.5480013185182,
129.913943046972)) ;
#125779 = CARTESIAN_POINT('Ctrl Pts',(-23.1617603223781,14.4271740783889,
129.63656787434)) ;
#125780 = CARTESIAN_POINT('Ctrl Pts',(-23.09288452206,14.2362638793065,129.402438365019)) ;
#125781 = CARTESIAN_POINT('Ctrl Pts',(-23.0427644300731,13.9863048350813,
129.222884594247)) ;
#125782 = CARTESIAN_POINT('Ctrl Pts',(-23.0163956850893,13.6957298115947,
129.112709730807)) ;
#125783 = CARTESIAN_POINT('Ctrl Pts',(-23.0161499853956,13.3866515588876,
129.078955426148)) ;
#125784 = CARTESIAN_POINT('Ctrl Pts',(-23.0432652761747,13.0771469470951,
129.124786982275)) ;
#125785 = CARTESIAN_POINT('Ctrl Pts',(-23.0956584483429,12.7963920748989,
129.244920648132)) ;
#125786 = CARTESIAN_POINT('Ctrl Pts',(-23.1713250322537,12.5578779077828,
129.432708390056)) ;
#125787 = CARTESIAN_POINT('Ctrl Pts',(-23.2644357106903,12.3830735450268,
129.671724285025)) ;
#125788 = CARTESIAN_POINT('Ctrl Pts',(-23.3701067648639,12.2815115080033,
129.947250619451)) ;
#125789 = CARTESIAN_POINT('Ctrl Pts',(-23.4813534599636,12.262368243914,130.238988514974)) ;
#125790 = CARTESIAN_POINT('Ctrl Pts',(-23.5896531894837,12.3259184462842,
130.522415372058)) ;
#125791 = CARTESIAN_POINT('Ctrl Pts',(-23.6896717899316,12.4680809705656,
130.78144439189)) ;
#125792 = CARTESIAN_POINT('Ctrl Pts',(-23.7743174451553,12.6795623808911,
130.995497362049)) ;
#125793 = CARTESIAN_POINT('Ctrl Pts',(-23.8377589698062,12.9425895546652,
131.147829833242)) ;
#125794 = CARTESIAN_POINT('Ctrl Pts',(-23.8769867469141,13.2417283918,131.229213132218)) ;
#125795 = CARTESIAN_POINT('Ctrl Pts',(-23.8893641527961,13.5531903661268,
131.232247085425)) ;
#125796 = CARTESIAN_POINT('Ctrl Pts',(-23.8748957358541,13.8554129193782,
131.156838036651)) ;
#125797 = CARTESIAN_POINT('Ctrl Pts',(-23.8355012217854,14.1261609524352,
131.008696352866)) ;
#125798 = CARTESIAN_POINT('Ctrl Pts',(-23.7741527595749,14.3478085326463,
130.796199663414)) ;
#125799 = CARTESIAN_POINT('Ctrl Pts',(-23.6971938021371,14.5013887047212,
130.538470256886)) ;
#125800 = CARTESIAN_POINT('Ctrl Pts',(-23.6092831974912,14.5792263128841,
130.248399633376)) ;
#125801 = CARTESIAN_POINT('Ctrl Pts',(-23.5187037661353,14.5735423168914,
129.950722272445)) ;
#125802 = CARTESIAN_POINT('Ctrl Pts',(-23.4320925272048,14.4859391814988,
129.664603852775)) ;
#125803 = CARTESIAN_POINT('Ctrl Pts',(-23.3561930515529,14.3210239309704,
129.409613726262)) ;
#125804 = CARTESIAN_POINT('Ctrl Pts',(-23.2980515559861,14.0938128758495,
129.206821944333)) ;
#125805 = CARTESIAN_POINT('Ctrl Pts',(-23.2615318957367,13.8165579042321,
129.066899333572)) ;
#125806 = CARTESIAN_POINT('Ctrl Pts',(-23.2505619538317,13.5127263915299,
129.001820179472)) ;
#125807 = CARTESIAN_POINT('Ctrl Pts',(-23.2666753004263,13.2000971209204,
129.015583001645)) ;
#125808 = CARTESIAN_POINT('Ctrl Pts',(-23.3087944429129,12.907342662141,129.105770615746)) ;
#125809 = CARTESIAN_POINT('Ctrl Pts',(-23.3756923407858,12.6479572241649,
129.267911443883)) ;
#125810 = CARTESIAN_POINT('Ctrl Pts',(-23.4621286873441,12.4461100173765,
129.487427563302)) ;
#125811 = CARTESIAN_POINT('Ctrl Pts',(-23.564127946314,12.3127706189861,129.752081916825)) ;
#125812 = CARTESIAN_POINT('Ctrl Pts',(-23.6732755910501,12.2601401087974,
130.037940276038)) ;
#125813 = CARTESIAN_POINT('Ctrl Pts',(-23.7838302243714,12.2901733256143,
130.327774440353)) ;
#125814 = CARTESIAN_POINT('Ctrl Pts',(-23.8883010360076,12.4015833067204,
130.599812066351)) ;
#125815 = CARTESIAN_POINT('Ctrl Pts',(-23.9798552045445,12.5866483791686,
130.834076178681)) ;
#125816 = CARTESIAN_POINT('Ctrl Pts',(-24.0523151917746,12.8302723289068,
131.012741175065)) ;
#125817 = CARTESIAN_POINT('Ctrl Pts',(-24.1019779789025,13.1192440261277,
131.124467731164)) ;
#125818 = CARTESIAN_POINT('Ctrl Pts',(-24.1250931579403,13.4254781915307,
131.159155989376)) ;
#125819 = CARTESIAN_POINT('Ctrl Pts',(-24.1215266149602,13.7353596810941,
131.11547066498)) ;
#125820 = CARTESIAN_POINT('Ctrl Pts',(-24.0918980981446,14.0210482002996,
130.995860945524)) ;
#125821 = CARTESIAN_POINT('Ctrl Pts',(-24.0389691525216,14.2649914716046,
130.808039376452)) ;
#125822 = CARTESIAN_POINT('Ctrl Pts',(-23.9676201622106,14.4476747030691,
130.566553540134)) ;
#125823 = CARTESIAN_POINT('Ctrl Pts',(-23.8833688710434,14.5574100040251,
130.287310728939)) ;
#125824 = CARTESIAN_POINT('Ctrl Pts',(-23.7931596806364,14.5860647514156,
129.990703936635)) ;
#125825 = CARTESIAN_POINT('Ctrl Pts',(-23.7035285456496,14.5307819261163,
129.695562869129)) ;
#125826 = CARTESIAN_POINT('Ctrl Pts',(-23.6229992772553,14.3969445095406,
129.42733334663)) ;
#125827 = CARTESIAN_POINT('Ctrl Pts',(-23.5567869860424,14.1927448984532,
129.200733935221)) ;
#125828 = CARTESIAN_POINT('Ctrl Pts',(-23.5110190745614,13.93401239778,129.033964097782)) ;
#125829 = CARTESIAN_POINT('Ctrl Pts',(-23.4893930698321,13.6381121003486,
128.93763672327)) ;
#125830 = CARTESIAN_POINT('Ctrl Pts',(-23.494345890272,13.3270742285028,128.918987736531)) ;
#125831 = CARTESIAN_POINT('Ctrl Pts',(-23.5262340039663,13.0225106106699,
128.978980037465)) ;
#125832 = CARTESIAN_POINT('Ctrl Pts',(-23.5835789347515,12.7468019660475,
129.113339138239)) ;
#125833 = CARTESIAN_POINT('Ctrl Pts',(-23.6624595718155,12.5205887293237,
129.310778341826)) ;
#125834 = CARTESIAN_POINT('Ctrl Pts',(-23.7587447135317,12.3578209293796,
129.558896200725)) ;
#125835 = CARTESIAN_POINT('Ctrl Pts',(-23.8658582136432,12.2716454717833,
129.838676166816)) ;
#125836 = CARTESIAN_POINT('Ctrl Pts',(-23.9769093594406,12.2679543097138,
130.129953687869)) ;
#125837 = CARTESIAN_POINT('Ctrl Pts',(-24.0845696446032,12.3469222200597,
130.411357159961)) ;
#125838 = CARTESIAN_POINT('Ctrl Pts',(-24.1820649364697,12.503089881748,130.663027573452)) ;
#125839 = CARTESIAN_POINT('Ctrl Pts',(-24.2629482232578,12.7250182855012,
130.866198402469)) ;
#125840 = CARTESIAN_POINT('Ctrl Pts',(-24.3222955108618,12.9971829063299,
131.006424325435)) ;
#125841 = CARTESIAN_POINT('Ctrl Pts',(-24.3564639158183,13.2997829333183,
131.07311023844)) ;
#125842 = CARTESIAN_POINT('Ctrl Pts',(-24.3637810053582,13.6108911186927,
131.061388804265)) ;
#125843 = CARTESIAN_POINT('Ctrl Pts',(-24.3445179230017,13.9087324272285,
130.972007256068)) ;
#125844 = CARTESIAN_POINT('Ctrl Pts',(-24.3005201013976,14.1725576742086,
130.810259178625)) ;
#125845 = CARTESIAN_POINT('Ctrl Pts',(-24.2360759456044,14.3815588265502,
130.588935069275)) ;
#125846 = CARTESIAN_POINT('Ctrl Pts',(-24.1562702964475,14.5223296073452,
130.322687297205)) ;
#125847 = CARTESIAN_POINT('Ctrl Pts',(-24.0676167127849,14.5844939687617,
130.030606234737)) ;
#125848 = CARTESIAN_POINT('Ctrl Pts',(-23.9768242528743,14.5631534202887,
129.732143036026)) ;
#125849 = CARTESIAN_POINT('Ctrl Pts',(-23.892015745999,14.4606750911625,129.451383600056)) ;
#125850 = CARTESIAN_POINT('Ctrl Pts',(-23.8188724297923,14.2826953933965,
129.204438549508)) ;
#125851 = CARTESIAN_POINT('Ctrl Pts',(-23.7644837114012,14.0447463333177,
129.01256424196)) ;
#125852 = CARTESIAN_POINT('Ctrl Pts',(-23.7326129631891,13.7613771036905,
128.886315694404)) ;
#125853 = CARTESIAN_POINT('Ctrl Pts',(-23.7266140527177,13.4542323232824,
128.835707264658)) ;
#125854 = CARTESIAN_POINT('Ctrl Pts',(-23.7476478247381,13.143799460901,128.86395007119)) ;
#125855 = CARTESIAN_POINT('Ctrl Pts',(-23.7949823521457,12.8538469192422,
128.969069945321)) ;
#125856 = CARTESIAN_POINT('Ctrl Pts',(-23.8656813263339,12.6054873495862,
129.142536871026)) ;
#125857 = CARTESIAN_POINT('Ctrl Pts',(-23.9553690976935,12.4153273206803,
129.37150786963)) ;
#125858 = CARTESIAN_POINT('Ctrl Pts',(-24.0596667735144,12.2964112458501,
129.642812186469)) ;
#125859 = CARTESIAN_POINT('Ctrl Pts',(-24.169433739975,12.2594155900217,129.930515923544)) ;
#125860 = CARTESIAN_POINT('Ctrl Pts',(-24.279602294317,12.3053349442499,130.2191500822)) ;
#125861 = CARTESIAN_POINT('Ctrl Pts',(-24.3818019884218,12.4312259098382,
130.484643983243)) ;
#125862 = CARTESIAN_POINT('Ctrl Pts',(-24.4700626756975,12.6279597260861,
130.709377871418)) ;
#125863 = CARTESIAN_POINT('Ctrl Pts',(-24.5387653735917,12.8824933120028,
130.876882524073)) ;
#125864 = CARTESIAN_POINT('Ctrl Pts',(-24.5833076087164,13.1745455822002,
130.973954429722)) ;
#125865 = CARTESIAN_POINT('Ctrl Pts',(-24.6016723074617,13.485175620818,130.994463005875)) ;
#125866 = CARTESIAN_POINT('Ctrl Pts',(-24.5929092913481,13.7921379938219,
130.935634698017)) ;
#125867 = CARTESIAN_POINT('Ctrl Pts',(-24.5586761808863,14.0710148384314,
130.802596578121)) ;
#125868 = CARTESIAN_POINT('Ctrl Pts',(-24.501845620011,14.3045452555015,130.603399975795)) ;
#125869 = CARTESIAN_POINT('Ctrl Pts',(-24.4277830561673,14.4740866338348,
130.35405191635)) ;
#125870 = CARTESIAN_POINT('Ctrl Pts',(-24.3415214169763,14.5693022561264,
130.068806329395)) ;
#125871 = CARTESIAN_POINT('Ctrl Pts',(-24.2510875787444,14.582012624519,129.771588629195)) ;
#125872 = CARTESIAN_POINT('Ctrl Pts',(-24.1625305892248,14.5112270801159,
129.47959734592)) ;
#125873 = CARTESIAN_POINT('Ctrl Pts',(-24.0843973310296,14.3635590913307,
129.218403125075)) ;
#125874 = CARTESIAN_POINT('Ctrl Pts',(-24.021647896778,14.1479538826623,129.001944571865)) ;
#125875 = CARTESIAN_POINT('Ctrl Pts',(-23.9801215750542,13.8806546187411,
128.847536590297)) ;
#125876 = CARTESIAN_POINT('Ctrl Pts',(-23.963342779706,13.5796272829373,128.765311315185)) ;
#125877 = CARTESIAN_POINT('Ctrl Pts',(-23.9735252945803,13.2675901061276,
128.761875234646)) ;
#125878 = CARTESIAN_POINT('Ctrl Pts',(-24.0101803838354,12.9685391977506,
128.835981940567)) ;
#125879 = CARTESIAN_POINT('Ctrl Pts',(-24.0719166755097,12.7001826766663,
128.98314530386)) ;
#125880 = CARTESIAN_POINT('Ctrl Pts',(-24.1546536581567,12.4843513272629,
129.191756252885)) ;
#125881 = CARTESIAN_POINT('Ctrl Pts',(-24.2535322461022,12.3354377542164,
129.447446958892)) ;
#125882 = CARTESIAN_POINT('Ctrl Pts',(-24.3616167437817,12.2645466478322,
129.730158751956)) ;
#125883 = CARTESIAN_POINT('Ctrl Pts',(-24.4731438929875,12.276740062036,130.022661709796)) ;
#125884 = CARTESIAN_POINT('Ctrl Pts',(-24.5790748900288,12.3708039289104,
130.299107143294)) ;
#125885 = CARTESIAN_POINT('Ctrl Pts',(-24.6739671483137,12.5405714665883,
130.543143809825)) ;
#125886 = CARTESIAN_POINT('Ctrl Pts',(-24.7509668752168,12.7727637010119,
130.735041912881)) ;
#125887 = CARTESIAN_POINT('Ctrl Pts',(-24.8059943713008,13.0532482908803,
130.862531034195)) ;
#125888 = CARTESIAN_POINT('Ctrl Pts',(-24.8350568114348,13.3594504233503,
130.914284039588)) ;
#125889 = CARTESIAN_POINT('Ctrl Pts',(-24.8372623159899,13.6687251009062,
130.887737753365)) ;
#125890 = CARTESIAN_POINT('Ctrl Pts',(-24.8130625569726,13.9622484425501,
130.78385263984)) ;
#125891 = CARTESIAN_POINT('Ctrl Pts',(-24.7649704899683,14.2163837439272,
130.610262407807)) ;
#125892 = CARTESIAN_POINT('Ctrl Pts',(-24.696901125032,14.4143549492585,130.378200623285)) ;
#125893 = CARTESIAN_POINT('Ctrl Pts',(-24.6148829741244,14.5404303849103,
130.105507473975)) ;
#125894 = CARTESIAN_POINT('Ctrl Pts',(-24.5256465957694,14.5868747911533,
129.811836591317)) ;
#125895 = CARTESIAN_POINT('Ctrl Pts',(-24.4352900112969,14.5499212467829,
129.514634417336)) ;
#125896 = CARTESIAN_POINT('Ctrl Pts',(-24.3521632833049,14.4324626312606,
129.238736296956)) ;
#125897 = CARTESIAN_POINT('Ctrl Pts',(-24.282156962627,14.2419356966938,129.001005963156)) ;
#125898 = CARTESIAN_POINT('Ctrl Pts',(-24.2316886119294,13.9939564791264,
128.820547864145)) ;
#125899 = CARTESIAN_POINT('Ctrl Pts',(-24.2045556444576,13.7043181769273,
128.708138252988)) ;
#125900 = CARTESIAN_POINT('Ctrl Pts',(-24.2036086367596,13.395369790062,128.672323138478)) ;
#125901 = CARTESIAN_POINT('Ctrl Pts',(-24.2297557957195,13.086808383261,128.715476371712)) ;
#125902 = CARTESIAN_POINT('Ctrl Pts',(-24.2816715668208,12.8035341555048,
128.834042913763)) ;
#125903 = CARTESIAN_POINT('Ctrl Pts',(-24.3566659267985,12.5639567351557,
129.019921579767)) ;
#125904 = CARTESIAN_POINT('Ctrl Pts',(-24.4495112025863,12.3867441251715,
129.258096186901)) ;
#125905 = CARTESIAN_POINT('Ctrl Pts',(-24.555139738116,12.2832559633923,129.533444706346)) ;
#125906 = CARTESIAN_POINT('Ctrl Pts',(-24.6653725410066,12.2616345665819,
129.822511029336)) ;
#125907 = CARTESIAN_POINT('Ctrl Pts',(-24.7747128452521,12.3231638960011,
130.108706425634)) ;
#125908 = CARTESIAN_POINT('Ctrl Pts',(-24.8746113532042,12.4627500215576,
130.367538216252)) ;
#125909 = CARTESIAN_POINT('Ctrl Pts',(-24.9600355501279,12.6729053974916,
130.583771384125)) ;
#125910 = CARTESIAN_POINT('Ctrl Pts',(-25.0240609203247,12.9344260822497,
130.737847424504)) ;
#125911 = CARTESIAN_POINT('Ctrl Pts',(-25.0641198333657,13.234077565713,130.821527263044)) ;
#125912 = CARTESIAN_POINT('Ctrl Pts',(-25.0771308739537,13.5439039553039,
130.826581768022)) ;
#125913 = CARTESIAN_POINT('Ctrl Pts',(-25.0635214617943,13.8465582342306,
130.753703399045)) ;
#125914 = CARTESIAN_POINT('Ctrl Pts',(-25.0247696848298,14.1188040415087,
130.607401020676)) ;
#125915 = CARTESIAN_POINT('Ctrl Pts',(-24.9640862870837,14.3420291426398,
130.396887886905)) ;
#125916 = CARTESIAN_POINT('Ctrl Pts',(-24.8872853575658,14.4980360771653,
130.13952226897)) ;
#125917 = CARTESIAN_POINT('Ctrl Pts',(-24.8000024335385,14.5780642539032,
129.85144765031)) ;
#125918 = CARTESIAN_POINT('Ctrl Pts',(-24.7087046539535,14.5747644514925,
129.551409158721)) ;
#125919 = CARTESIAN_POINT('Ctrl Pts',(-24.6223739304756,14.489550077403,129.266289535855)) ;
#125920 = CARTESIAN_POINT('Ctrl Pts',(-24.5461701581343,14.3274511232625,
129.010484644828)) ;
#125921 = CARTESIAN_POINT('Ctrl Pts',(-24.4872263455305,14.10121310871,128.805238001483)) ;
#125922 = CARTESIAN_POINT('Ctrl Pts',(-24.4500072639137,13.8249843797631,
128.663265474858)) ;
#125923 = CARTESIAN_POINT('Ctrl Pts',(-24.438327381082,13.5214320860101,128.59608615518)) ;
#125924 = CARTESIAN_POINT('Ctrl Pts',(-24.4534890626492,13.2103011439188,
128.607246943733)) ;
#125925 = CARTESIAN_POINT('Ctrl Pts',(-24.495066640313,12.9148531024708,128.695641378851)) ;
#125926 = CARTESIAN_POINT('Ctrl Pts',(-24.5613915132952,12.6543477240414,
128.856118206563)) ;
#125927 = CARTESIAN_POINT('Ctrl Pts',(-24.6471825551665,12.4511188454898,
129.073804541509)) ;
#125928 = CARTESIAN_POINT('Ctrl Pts',(-24.7486084980389,12.3156705346788,
129.336853062175)) ;
#125929 = CARTESIAN_POINT('Ctrl Pts',(-24.8581128521185,12.2603783289395,
129.62360453636)) ;
#125930 = CARTESIAN_POINT('Ctrl Pts',(-24.9686726023263,12.2883877322888,
129.913470195239)) ;
#125931 = CARTESIAN_POINT('Ctrl Pts',(-25.0729932645916,12.396958266653,130.185207408956)) ;
#125932 = CARTESIAN_POINT('Ctrl Pts',(-25.1653592270199,12.5805839766397,
130.421729388471)) ;
#125933 = CARTESIAN_POINT('Ctrl Pts',(-25.2382239831384,12.8225431268309,
130.601623820474)) ;
#125934 = CARTESIAN_POINT('Ctrl Pts',(-25.2885089962269,13.1085293602313,
130.715378449147)) ;
#125935 = CARTESIAN_POINT('Ctrl Pts',(-25.3126600961537,13.4184312820959,
130.752658836677)) ;
#125936 = CARTESIAN_POINT('Ctrl Pts',(-25.3098210842849,13.725396855158,130.711452962924)) ;
#125937 = CARTESIAN_POINT('Ctrl Pts',(-25.2808102713298,14.0140710233184,
130.593415477902)) ;
#125938 = CARTESIAN_POINT('Ctrl Pts',(-25.2285495788724,14.2586953082214,
130.407640473417)) ;
#125939 = CARTESIAN_POINT('Ctrl Pts',(-25.1575885801058,14.4435712393275,
130.167243122289)) ;
#125940 = CARTESIAN_POINT('Ctrl Pts',(-25.0736237827417,14.5554638081498,
129.888850792781)) ;
#125941 = CARTESIAN_POINT('Ctrl Pts',(-24.9833949472367,14.5862678501096,
129.592148597905)) ;
#125942 = CARTESIAN_POINT('Ctrl Pts',(-24.8942273387361,14.5339455279845,
129.298592022686)) ;
#125943 = CARTESIAN_POINT('Ctrl Pts',(-24.8129142069753,14.4019055584218,
129.027901950915)) ;
#125944 = CARTESIAN_POINT('Ctrl Pts',(-24.746276318339,14.1996929308369,128.800099500665)) ;
#125945 = CARTESIAN_POINT('Ctrl Pts',(-24.699763961038,13.9418839763085,128.631093588378)) ;
#125946 = CARTESIAN_POINT('Ctrl Pts',(-24.6774338462082,13.6467945517117,
128.532720399714)) ;
#125947 = CARTESIAN_POINT('Ctrl Pts',(-24.6816242532169,13.3358857358536,
128.511842088529)) ;
#125948 = CARTESIAN_POINT('Ctrl Pts',(-24.7127138700083,13.0311283359512,
128.569538090796)) ;
#125949 = CARTESIAN_POINT('Ctrl Pts',(-24.7693523753043,12.7543595067604,
128.70183682194)) ;
#125950 = CARTESIAN_POINT('Ctrl Pts',(-24.8475655059419,12.5263863833961,
128.897344080859)) ;
#125951 = CARTESIAN_POINT('Ctrl Pts',(-24.9442364116292,12.3607017684255,
129.146334817841)) ;
#125952 = CARTESIAN_POINT('Ctrl Pts',(-25.0501716622116,12.2732420029804,
129.422981311838)) ;
#125953 = CARTESIAN_POINT('Ctrl Pts',(-25.161642701429,12.2668291294782,129.715349818511)) ;
#125954 = CARTESIAN_POINT('Ctrl Pts',(-25.2694224447278,12.3436152480751,
129.997125883339)) ;
#125955 = CARTESIAN_POINT('Ctrl Pts',(-25.3674136502751,12.4979168003383,
130.250203723664)) ;
#125956 = CARTESIAN_POINT('Ctrl Pts',(-25.4487609142858,12.7181781437397,
130.454748013193)) ;
#125957 = CARTESIAN_POINT('Ctrl Pts',(-25.5086898509027,12.9887185054322,
130.596726594436)) ;
#125958 = CARTESIAN_POINT('Ctrl Pts',(-25.5436429825189,13.2908827967775,
130.665687047163)) ;
#125959 = CARTESIAN_POINT('Ctrl Pts',(-25.5517475698564,13.6021684785122,
130.656255124618)) ;
#125960 = CARTESIAN_POINT('Ctrl Pts',(-25.5331239691341,13.901537415506,130.568644647974)) ;
#125961 = CARTESIAN_POINT('Ctrl Pts',(-25.48972374552,14.1661758295122,130.408674325154)) ;
#125962 = CARTESIAN_POINT('Ctrl Pts',(-25.4260099872032,14.3763137224392,
130.189586864129)) ;
#125963 = CARTESIAN_POINT('Ctrl Pts',(-25.3463659017589,14.5195379343594,
129.923731245516)) ;
#125964 = CARTESIAN_POINT('Ctrl Pts',(-25.2580898168815,14.5837467777198,
129.632838255193)) ;
#125965 = CARTESIAN_POINT('Ctrl Pts',(-25.1673248310042,14.5651055472896,
129.334485888311)) ;
#125966 = CARTESIAN_POINT('Ctrl Pts',(-25.0819869198981,14.4645028537766,
129.052069731339)) ;
#125967 = CARTESIAN_POINT('Ctrl Pts',(-25.0086540266316,14.2890439615902,
128.80468090298)) ;
#125968 = CARTESIAN_POINT('Ctrl Pts',(-24.9535847938953,14.0526944517644,
128.610802322953)) ;
#125969 = CARTESIAN_POINT('Ctrl Pts',(-24.9209684987911,13.7699865640071,
128.482334359054)) ;
#125970 = CARTESIAN_POINT('Ctrl Pts',(-24.914161154007,13.4631529119525,128.429358281431)) ;
#125971 = CARTESIAN_POINT('Ctrl Pts',(-24.9346241902268,13.1513620896954,
128.455804728885)) ;
#125972 = CARTESIAN_POINT('Ctrl Pts',(-24.9808286764254,12.8627668245119,
128.557889451478)) ;
#125973 = CARTESIAN_POINT('Ctrl Pts',(-25.0514554263938,12.6109028721184,
128.730870773543)) ;
#125974 = CARTESIAN_POINT('Ctrl Pts',(-25.1403206144582,12.4200193080497,
128.957599041015)) ;
#125975 = CARTESIAN_POINT('Ctrl Pts',(-25.2443570951015,12.298694725006,129.228115799905)) ;
#125976 = CARTESIAN_POINT('Ctrl Pts',(-25.3538813352196,12.2592723921271,
129.515159745908)) ;
#125977 = CARTESIAN_POINT('Ctrl Pts',(-25.4644961600716,12.3030853474822,
129.804989192264)) ;
#125978 = CARTESIAN_POINT('Ctrl Pts',(-25.5664737135498,12.4259705793417,
130.070018363366)) ;
#125979 = CARTESIAN_POINT('Ctrl Pts',(-25.6558186570055,12.6220550039555,
130.297698340302)) ;
#125980 = CARTESIAN_POINT('Ctrl Pts',(-25.7248599756662,12.8744669424422,
130.466310011983)) ;
#125981 = CARTESIAN_POINT('Ctrl Pts',(-25.7702434103864,13.1663406139675,
130.565761336406)) ;
#125982 = CARTESIAN_POINT('Ctrl Pts',(-25.78925027389,13.475878892664,130.588240800229)) ;
#125983 = CARTESIAN_POINT('Ctrl Pts',(-25.7814468787295,13.7823953075606,
130.532325836571)) ;
#125984 = CARTESIAN_POINT('Ctrl Pts',(-25.7476177585212,14.064418215805,130.400208232113)) ;
#125985 = CARTESIAN_POINT('Ctrl Pts',(-25.6918077811808,14.2977471414108,
130.204255542855)) ;
#125986 = CARTESIAN_POINT('Ctrl Pts',(-25.6177147063912,14.4706194179794,
129.95458823605)) ;
#125987 = CARTESIAN_POINT('Ctrl Pts',(-25.5319450619605,14.5675955159237,
129.670894736031)) ;
#125988 = CARTESIAN_POINT('Ctrl Pts',(-25.4414971518042,14.5827755983601,
129.373610278919)) ;
#125989 = CARTESIAN_POINT('Ctrl Pts',(-25.3531231344059,14.5148008413574,
129.082293968107)) ;
#125990 = CARTESIAN_POINT('Ctrl Pts',(-25.2743161800529,14.3692242855325,
128.81903385639)) ;
#125991 = CARTESIAN_POINT('Ctrl Pts',(-25.2107747912008,14.1540994204916,
128.600098438583)) ;
#125992 = CARTESIAN_POINT('Ctrl Pts',(-25.168846979142,13.889194577701,128.444675356342)) ;
#125993 = CARTESIAN_POINT('Ctrl Pts',(-25.1512494519835,13.5894848313417,
128.36011954352)) ;
#125994 = CARTESIAN_POINT('Ctrl Pts',(-25.1605845207115,13.2771021698192,
128.354170238193)) ;
#125995 = CARTESIAN_POINT('Ctrl Pts',(-25.1965224543068,12.9767128859996,
128.426111454514)) ;
#125996 = CARTESIAN_POINT('Ctrl Pts',(-25.2578937374659,12.7063601582146,
128.572090875043)) ;
#125997 = CARTESIAN_POINT('Ctrl Pts',(-25.3396420278382,12.4901609157503,
128.778005457338)) ;
#125998 = CARTESIAN_POINT('Ctrl Pts',(-25.4381908746274,12.338688213011,129.032699044275)) ;
#125999 = CARTESIAN_POINT('Ctrl Pts',(-25.5463110659534,12.2654833215425,
129.315451748126)) ;
#126000 = CARTESIAN_POINT('Ctrl Pts',(-25.6574951807458,12.2750423939134,
129.607066941372)) ;
#126001 = CARTESIAN_POINT('Ctrl Pts',(-25.7642010115431,12.3673309477628,
129.885602094051)) ;
#126002 = CARTESIAN_POINT('Ctrl Pts',(-25.8590365897066,12.5343469793072,
130.129637220304)) ;
#126003 = CARTESIAN_POINT('Ctrl Pts',(-25.9368382713176,12.7652871615339,
130.32380307639)) ;
#126004 = CARTESIAN_POINT('Ctrl Pts',(-25.9924735837026,13.0444119641298,
130.453106439739)) ;
#126005 = CARTESIAN_POINT('Ctrl Pts',(-26.0223929863957,13.3498617711502,
130.507389727664)) ;
#126006 = CARTESIAN_POINT('Ctrl Pts',(-26.0253114098023,13.6613615410962,
130.482703869082)) ;
#126007 = CARTESIAN_POINT('Ctrl Pts',(-26.0019147375177,13.9537822456917,
130.381373854376)) ;
#126008 = CARTESIAN_POINT('Ctrl Pts',(-25.9544927342726,14.2096141723503,
130.209713801522)) ;
#126009 = CARTESIAN_POINT('Ctrl Pts',(-25.8870673150101,14.4090573352496,
129.979600499692)) ;
#126010 = CARTESIAN_POINT('Ctrl Pts',(-25.8054312777494,14.5378227777349,
129.70802666148)) ;
#126011 = CARTESIAN_POINT('Ctrl Pts',(-25.7156142292361,14.5866410232384,
129.41240035545)) ;
#126012 = CARTESIAN_POINT('Ctrl Pts',(-25.6260309545434,14.5524956968184,
129.117784907284)) ;
#126013 = CARTESIAN_POINT('Ctrl Pts',(-25.5418482572694,14.4363359787846,
128.838493567448)) ;
#126014 = CARTESIAN_POINT('Ctrl Pts',(-25.4718915415956,14.2487612531945,
128.601139063692)) ;
#126015 = CARTESIAN_POINT('Ctrl Pts',(-25.42063882581,14.0019963672536,128.4183229551)) ;
#126016 = CARTESIAN_POINT('Ctrl Pts',(-25.392749544608,13.7133413750086,128.303718197207)) ;
#126017 = CARTESIAN_POINT('Ctrl Pts',(-25.391107247378,13.4034231078491,128.265734684646)) ;
#126018 = CARTESIAN_POINT('Ctrl Pts',(-25.4162654592174,13.0966156009071,
128.306236353819)) ;
#126019 = CARTESIAN_POINT('Ctrl Pts',(-25.4677661028884,12.8104956204696,
128.423372058635)) ;
#126020 = CARTESIAN_POINT('Ctrl Pts',(-25.5418005766506,12.5707042349948,
128.606625724916)) ;
#126021 = CARTESIAN_POINT('Ctrl Pts',(-25.6343027539285,12.3910193657153,
128.84373772453)) ;
#126022 = CARTESIAN_POINT('Ctrl Pts',(-25.7394215596981,12.285328864528,129.117673474855)) ;
#126023 = CARTESIAN_POINT('Ctrl Pts',(-25.8499618498709,12.2609818529467,
129.407525601254)) ;
#126024 = CARTESIAN_POINT('Ctrl Pts',(-25.9597380713748,12.3204757590526,
129.694909016279)) ;
#126025 = CARTESIAN_POINT('Ctrl Pts',(-26.0599411656007,12.4582515921679,
129.954624240264)) ;
#126026 = CARTESIAN_POINT('Ctrl Pts',(-26.145604357151,12.6658998652864,130.171670188794)) ;
#126027 = CARTESIAN_POINT('Ctrl Pts',(-26.2103851275808,12.9268096194457,
130.32787211021)) ;
#126028 = CARTESIAN_POINT('Ctrl Pts',(-26.2509404211424,13.2233761882574,
130.413261942169)) ;
#126029 = CARTESIAN_POINT('Ctrl Pts',(-26.2649718352972,13.5346577028184,
130.421128557714)) ;
#126030 = CARTESIAN_POINT('Ctrl Pts',(-26.2520240327405,13.8387961550216,
130.350083552355)) ;
#126031 = CARTESIAN_POINT('Ctrl Pts',(-26.2138395505756,14.1123018093557,
130.205408086112)) ;
#126032 = CARTESIAN_POINT('Ctrl Pts',(-26.153839721311,14.3364687446635,129.996980303238)) ;
#126033 = CARTESIAN_POINT('Ctrl Pts',(-26.0774343121864,14.494770833943,129.74076290921)) ;
#126034 = CARTESIAN_POINT('Ctrl Pts',(-25.9899586435841,14.5769227995843,
129.45198478666)) ;
#126035 = CARTESIAN_POINT('Ctrl Pts',(-25.8997042911877,14.5762675412157,
129.155383645879)) ;
#126036 = CARTESIAN_POINT('Ctrl Pts',(-25.812384586297,14.4930554177443,128.867083845034)) ;
#126037 = CARTESIAN_POINT('Ctrl Pts',(-25.73597860465,14.3331650364545,128.610769594454)) ;
#126038 = CARTESIAN_POINT('Ctrl Pts',(-25.6763576726058,14.1081176093321,
128.403470945939)) ;
#126039 = CARTESIAN_POINT('Ctrl Pts',(-25.6385794389391,13.8340178637995,
128.259988320297)) ;
#126040 = CARTESIAN_POINT('Ctrl Pts',(-25.6260661068604,13.5302898798933,
128.190290082024)) ;
#126041 = CARTESIAN_POINT('Ctrl Pts',(-25.6404465317525,13.2194241455141,
128.199211501796)) ;
#126042 = CARTESIAN_POINT('Ctrl Pts',(-25.6812553568026,12.9232187981691,
128.285358188475)) ;
#126043 = CARTESIAN_POINT('Ctrl Pts',(-25.7468433316738,12.6614612454166,
128.443705997656)) ;
#126044 = CARTESIAN_POINT('Ctrl Pts',(-25.8322906105427,12.4560560128417,
128.660322270214)) ;
#126045 = CARTESIAN_POINT('Ctrl Pts',(-25.9330424236509,12.3187614460116,
128.921508759944)) ;
#126046 = CARTESIAN_POINT('Ctrl Pts',(-26.0425569662323,12.2608758912203,
129.208234980341)) ;
#126047 = CARTESIAN_POINT('Ctrl Pts',(-26.1530140665807,12.2860567579314,
129.497863653022)) ;
#126048 = CARTESIAN_POINT('Ctrl Pts',(-26.2585079710758,12.3936760882031,
129.772722456645)) ;
#126049 = CARTESIAN_POINT('Ctrl Pts',(-26.3503095104322,12.5734427246259,
130.007962979543)) ;
#126050 = CARTESIAN_POINT('Ctrl Pts',(-26.4244433834245,12.8155556850103,
130.191300268138)) ;
#126051 = CARTESIAN_POINT('Ctrl Pts',(-26.4751724700827,13.1001458972495,
130.306431104727)) ;
#126052 = CARTESIAN_POINT('Ctrl Pts',(-26.5000925783719,13.4082451879306,
130.346105536368)) ;
#126053 = CARTESIAN_POINT('Ctrl Pts',(-26.4980891723479,13.7170001803432,
130.307186038938)) ;
#126054 = CARTESIAN_POINT('Ctrl Pts',(-26.4696671842496,14.0068803402206,
130.190824498522)) ;
#126055 = CARTESIAN_POINT('Ctrl Pts',(-26.4181820684679,14.2520830293328,
130.007428300008)) ;
#126056 = CARTESIAN_POINT('Ctrl Pts',(-26.3478207017117,14.4388654830233,
129.768822234995)) ;
#126057 = CARTESIAN_POINT('Ctrl Pts',(-26.2640576549974,14.5532758732377,
129.490979404376)) ;
#126058 = CARTESIAN_POINT('Ctrl Pts',(-26.1738376378664,14.5866372920254,
129.194279342961)) ;
#126059 = CARTESIAN_POINT('Ctrl Pts',(-26.0842975023075,14.5363254176441,
128.899536369528)) ;
#126060 = CARTESIAN_POINT('Ctrl Pts',(-26.0030217669562,14.4070821621483,
128.629108370544)) ;
#126061 = CARTESIAN_POINT('Ctrl Pts',(-25.9355456978039,14.2058492083664,
128.398700995927)) ;
#126062 = CARTESIAN_POINT('Ctrl Pts',(-25.8885241340143,13.9493209948446,
128.22822873028)) ;
#126063 = CARTESIAN_POINT('Ctrl Pts',(-25.8655269249234,13.6560816427411,
128.12802385383)) ;
#126064 = CARTESIAN_POINT('Ctrl Pts',(-25.8688947460715,13.3454213686902,
128.104749085037)) ;
#126065 = CARTESIAN_POINT('Ctrl Pts',(-25.8990663345431,13.0405957785926,
128.159818838281)) ;
#126066 = CARTESIAN_POINT('Ctrl Pts',(-25.9553167132455,12.761020315257,128.290787259896)) ;
#126067 = CARTESIAN_POINT('Ctrl Pts',(-26.0329645870705,12.5320804704421,
128.484687748095)) ;
#126068 = CARTESIAN_POINT('Ctrl Pts',(-26.1284887813019,12.3651153247515,
128.730556130345)) ;
#126069 = CARTESIAN_POINT('Ctrl Pts',(-26.2350764396969,12.2743249868604,
129.008828559484)) ;
#126070 = CARTESIAN_POINT('Ctrl Pts',(-26.3465970340771,12.2660445265336,
129.301326003185)) ;
#126071 = CARTESIAN_POINT('Ctrl Pts',(-26.4541471683152,12.3402671637665,
129.582555856666)) ;
#126072 = CARTESIAN_POINT('Ctrl Pts',(-26.552555555769,12.492431210345,129.836844563032)) ;
#126073 = CARTESIAN_POINT('Ctrl Pts',(-26.634360399724,12.7106681794057,130.042767093069)) ;
#126074 = CARTESIAN_POINT('Ctrl Pts',(-26.6951305941108,12.9803450583886,
130.187151429511)) ;
#126075 = CARTESIAN_POINT('Ctrl Pts',(-26.7308734422664,13.2833171432177,
130.258272185674)) ;
#126076 = CARTESIAN_POINT('Ctrl Pts',(-26.7396663356869,13.5926828813481,
130.251062592622)) ;
#126077 = CARTESIAN_POINT('Ctrl Pts',(-26.7217809067384,13.8936498651441,
130.165504550532)) ;
#126078 = CARTESIAN_POINT('Ctrl Pts',(-26.6791273969298,14.1589431067745,
130.007795968708)) ;
#126079 = CARTESIAN_POINT('Ctrl Pts',(-26.6158454773809,14.3711507970921,
129.789913035813)) ;
#126080 = CARTESIAN_POINT('Ctrl Pts',(-26.5368498372877,14.5162610816314,
129.526063678826)) ;
#126081 = CARTESIAN_POINT('Ctrl Pts',(-26.4480058430415,14.583306350133,129.233236326082)) ;
#126082 = CARTESIAN_POINT('Ctrl Pts',(-26.3574400513536,14.5665129586633,
128.93555561929)) ;
#126083 = CARTESIAN_POINT('Ctrl Pts',(-26.2721691927967,14.4685223967189,
128.653448871717)) ;
#126084 = CARTESIAN_POINT('Ctrl Pts',(-26.1984352857841,14.2954966012034,
128.404931525748)) ;
#126085 = CARTESIAN_POINT('Ctrl Pts',(-26.1425694482062,14.0596946296019,
128.208585964953)) ;
#126086 = CARTESIAN_POINT('Ctrl Pts',(-26.1092924899254,13.7784555956093,
128.078249514083)) ;
#126087 = CARTESIAN_POINT('Ctrl Pts',(-26.1018692508435,13.4704205391721,
128.02329757689)) ;
#126088 = CARTESIAN_POINT('Ctrl Pts',(-26.1211722195802,13.1626906793203,
128.046828877772)) ;
#126089 = CARTESIAN_POINT('Ctrl Pts',(-26.1671025371893,12.8697533216184,
128.147711848821)) ;
#126090 = CARTESIAN_POINT('Ctrl Pts',(-26.2364647283035,12.6186668370347,
128.317310814944)) ;
#126091 = CARTESIAN_POINT('Ctrl Pts',(-26.3256526534725,12.4240570551779,
128.544661301817)) ;
#126092 = CARTESIAN_POINT('Ctrl Pts',(-26.4282836894432,12.301712902155,128.811435711836)) ;
#126093 = CARTESIAN_POINT('Ctrl Pts',(-26.5385014971337,12.2592124433866,
129.100247411797)) ;
#126094 = CARTESIAN_POINT('Ctrl Pts',(-26.648676203193,12.3002004237818,129.388972536211)) ;
#126095 = CARTESIAN_POINT('Ctrl Pts',(-26.7520297398877,12.4222100081088,
129.657665386469)) ;
#126096 = CARTESIAN_POINT('Ctrl Pts',(-26.8411055662838,12.6151763804986,
129.88482406291)) ;
#126097 = CARTESIAN_POINT('Ctrl Pts',(-26.9110238859048,12.866763553233,130.055895668219)) ;
#126098 = CARTESIAN_POINT('Ctrl Pts',(-26.9569593910413,13.1566083036236,
130.157097759597)) ;
#126099 = CARTESIAN_POINT('Ctrl Pts',(-26.9769152324821,13.4669635155183,
130.182234691764)) ;
#126100 = CARTESIAN_POINT('Ctrl Pts',(-26.9697491794495,13.7743605860558,
130.128124278071)) ;
#126101 = CARTESIAN_POINT('Ctrl Pts',(-26.9369099290201,14.0556835712851,
129.999115173521)) ;
#126102 = CARTESIAN_POINT('Ctrl Pts',(-26.8813890693662,14.2923698679386,
129.803785415256)) ;
#126103 = CARTESIAN_POINT('Ctrl Pts',(-26.8075624299722,14.4669398360514,
129.554865852864)) ;
#126104 = CARTESIAN_POINT('Ctrl Pts',(-26.7225333981472,14.5658237204842,
129.273523926098)) ;
#126105 = CARTESIAN_POINT('Ctrl Pts',(-26.6316073168798,14.5834030750835,
128.974644654919)) ;
#126106 = CARTESIAN_POINT('Ctrl Pts',(-26.5435523900135,14.5182209369221,
128.68445694957)) ;
#126107 = CARTESIAN_POINT('Ctrl Pts',(-26.4637060287768,14.3732472228341,
128.41785071339)) ;
#126108 = CARTESIAN_POINT('Ctrl Pts',(-26.4003065211889,14.161734042983,128.199658464977)) ;
#126109 = CARTESIAN_POINT('Ctrl Pts',(-26.3573928265329,13.8968738672396,
128.041174467491)) ;
#126110 = CARTESIAN_POINT('Ctrl Pts',(-26.3391569924333,13.5970560174392,
127.954689223546)) ;
#126111 = CARTESIAN_POINT('Ctrl Pts',(-26.3477971534029,13.285349771455,127.946776708797)) ;
#126112 = CARTESIAN_POINT('Ctrl Pts',(-26.3828895156986,12.9854213227035,
128.016359458515)) ;
#126113 = CARTESIAN_POINT('Ctrl Pts',(-26.4432873742687,12.7145025865389,
128.159598142136)) ;
#126114 = CARTESIAN_POINT('Ctrl Pts',(-26.5248365779504,12.4953422149561,
128.364769418823)) ;
#126115 = CARTESIAN_POINT('Ctrl Pts',(-26.6231996145882,12.3417857538749,
128.618871219026)) ;
#126116 = CARTESIAN_POINT('Ctrl Pts',(-26.7308273833783,12.2665368093941,
128.900280109487)) ;
#126117 = CARTESIAN_POINT('Ctrl Pts',(-26.8419112559872,12.2735361740405,
129.191636843919)) ;
#126118 = CARTESIAN_POINT('Ctrl Pts',(-26.9488113349784,12.3632299565235,
129.470758505725)) ;
#126119 = CARTESIAN_POINT('Ctrl Pts',(-27.044382308045,12.5286847950401,129.716836311528)) ;
#126120 = CARTESIAN_POINT('Ctrl Pts',(-27.122663508425,12.7579694730324,129.912424964013)) ;
#126121 = CARTESIAN_POINT('Ctrl Pts',(-27.1789063470941,13.0352202971202,
130.043587032945)) ;
#126122 = CARTESIAN_POINT('Ctrl Pts',(-27.2096612668745,13.3405829184085,
130.100263246823)) ;
#126123 = CARTESIAN_POINT('Ctrl Pts',(-27.2134313544353,13.6512271972451,
130.078177727749)) ;
#126124 = CARTESIAN_POINT('Ctrl Pts',(-27.1907621951,13.9458587168303,129.978824391193)) ;
#126125 = CARTESIAN_POINT('Ctrl Pts',(-27.1438228231877,14.2033946727232,
129.808513890498)) ;
#126126 = CARTESIAN_POINT('Ctrl Pts',(-27.0770750626635,14.4040391264647,
129.580474233963)) ;
#126127 = CARTESIAN_POINT('Ctrl Pts',(-26.9958801704917,14.5350227428464,
129.310223124161)) ;
#126128 = CARTESIAN_POINT('Ctrl Pts',(-26.906059475308,14.5864958766325,129.014538770092)) ;
#126129 = CARTESIAN_POINT('Ctrl Pts',(-26.8162216028424,14.5544169233344,
128.719109024983)) ;
#126130 = CARTESIAN_POINT('Ctrl Pts',(-26.732249151307,14.4414134366696,128.440641667586)) ;
#126131 = CARTESIAN_POINT('Ctrl Pts',(-26.6614367576336,14.2551029691134,
128.200625386532)) ;
#126132 = CARTESIAN_POINT('Ctrl Pts',(-26.6096148301924,14.0100365412081,
128.016185333679)) ;
#126133 = CARTESIAN_POINT('Ctrl Pts',(-26.5809743060425,13.7214335751914,
127.899285485358)) ;
#126134 = CARTESIAN_POINT('Ctrl Pts',(-26.5785086522485,13.4135493095884,
127.859089390774)) ;
#126135 = CARTESIAN_POINT('Ctrl Pts',(-26.6030598393761,13.1045553543373,
127.897610196084)) ;
#126136 = CARTESIAN_POINT('Ctrl Pts',(-26.6533738007603,12.819735905808,128.011560491911)) ;
#126137 = CARTESIAN_POINT('Ctrl Pts',(-26.7273433263528,12.5762135123813,
128.194341414483)) ;
#126138 = CARTESIAN_POINT('Ctrl Pts',(-26.8192648566206,12.3952019865551,
128.429832693203)) ;
#126139 = CARTESIAN_POINT('Ctrl Pts',(-26.9242264204427,12.2871509096393,
128.703270123928)) ;
#126140 = CARTESIAN_POINT('Ctrl Pts',(-27.0344529109704,12.2605661260812,
128.992282379476)) ;
#126141 = CARTESIAN_POINT('Ctrl Pts',(-27.1443703931417,12.3174696156297,
129.280083515023)) ;
#126142 = CARTESIAN_POINT('Ctrl Pts',(-27.2451512743396,12.4535095799729,
129.541404839542)) ;
#126143 = CARTESIAN_POINT('Ctrl Pts',(-27.331104012236,12.6588731415835,129.759381061345)) ;
#126144 = CARTESIAN_POINT('Ctrl Pts',(-27.3966132229069,12.9185733098552,
129.917687249482)) ;
#126145 = CARTESIAN_POINT('Ctrl Pts',(-27.437913249649,13.2144047799764,130.005254654864)) ;
#126146 = CARTESIAN_POINT('Ctrl Pts',(-27.4527179999152,13.5255442513147,
130.015381846826)) ;
#126147 = CARTESIAN_POINT('Ctrl Pts',(-27.4406132753305,13.8297540824603,
129.946859327367)) ;
#126148 = CARTESIAN_POINT('Ctrl Pts',(-27.4030398195296,14.1049218673864,
129.803899854786)) ;
#126149 = CARTESIAN_POINT('Ctrl Pts',(-27.3439832338372,14.3298724417038,
129.59839933543)) ;
#126150 = CARTESIAN_POINT('Ctrl Pts',(-27.2674519754825,14.4915528402348,
129.34156807038)) ;
#126151 = CARTESIAN_POINT('Ctrl Pts',(-27.1804570845726,14.5755974614276,
129.054311222488)) ;
#126152 = CARTESIAN_POINT('Ctrl Pts',(-27.0900591437139,14.5774288175943,
128.75723029633)) ;
#126153 = CARTESIAN_POINT('Ctrl Pts',(-27.0027465267917,14.4968431022692,
128.469040137176)) ;
#126154 = CARTESIAN_POINT('Ctrl Pts',(-26.9256630669634,14.3385595023236,
128.210629189847)) ;
#126155 = CARTESIAN_POINT('Ctrl Pts',(-26.8655442910329,14.1152209980979,
128.00189933541)) ;
#126156 = CARTESIAN_POINT('Ctrl Pts',(-26.8270860169213,13.8419813754815,
127.856398889617)) ;
#126157 = CARTESIAN_POINT('Ctrl Pts',(-26.8138530884316,13.5398084238246,
127.784708325254)) ;
#126158 = CARTESIAN_POINT('Ctrl Pts',(-26.8274109995624,13.2280435028726,
127.791143495503)) ;
#126159 = CARTESIAN_POINT('Ctrl Pts',(-26.8677662548996,12.9300590292135,
127.875833464593)) ;
#126160 = CARTESIAN_POINT('Ctrl Pts',(-26.9324327506608,12.6684083848218,
128.031655490712)) ;
#126161 = CARTESIAN_POINT('Ctrl Pts',(-27.0174847633721,12.4608091208846,
128.247059958605)) ;
#126162 = CARTESIAN_POINT('Ctrl Pts',(-27.1179785264983,12.3214093347923,
128.507474270325)) ;
#126163 = CARTESIAN_POINT('Ctrl Pts',(-27.2275226737143,12.2613302981185,
128.794237732112)) ;
#126164 = CARTESIAN_POINT('Ctrl Pts',(-27.3376047432448,12.2843255086961,
129.082895790181)) ;
#126165 = CARTESIAN_POINT('Ctrl Pts',(-27.4428996493216,12.3887269891781,
129.357335238183)) ;
#126166 = CARTESIAN_POINT('Ctrl Pts',(-27.5357472832916,12.567362762576,129.595436520551)) ;
#126167 = CARTESIAN_POINT('Ctrl Pts',(-27.6104078073465,12.8080166965812,
129.780323450839)) ;
#126168 = CARTESIAN_POINT('Ctrl Pts',(-27.6618734446833,13.0914774469774,
129.897617122415)) ;
#126169 = CARTESIAN_POINT('Ctrl Pts',(-27.6875950196144,13.4005589719555,
129.939492462511)) ;
#126170 = CARTESIAN_POINT('Ctrl Pts',(-27.6862592435431,13.7083911607305,
129.902647623818)) ;
#126171 = CARTESIAN_POINT('Ctrl Pts',(-27.6586873787824,13.9985991355892,
129.788842673993)) ;
#126172 = CARTESIAN_POINT('Ctrl Pts',(-27.6077515908902,14.2457812535683,
129.606991326531)) ;
#126173 = CARTESIAN_POINT('Ctrl Pts',(-27.5377989327998,14.434573414283,129.369557237588)) ;
#126174 = CARTESIAN_POINT('Ctrl Pts',(-27.4542768495757,14.5511370884747,
129.092404947508)) ;
#126175 = CARTESIAN_POINT('Ctrl Pts',(-27.3644225518952,14.5867802191552,
128.796873978276)) ;
#126176 = CARTESIAN_POINT('Ctrl Pts',(-27.2747420069069,14.5391948457713,
128.501723104712)) ;
#126177 = CARTESIAN_POINT('Ctrl Pts',(-27.1928633072709,14.4115345320068,
128.229410196093)) ;
#126178 = CARTESIAN_POINT('Ctrl Pts',(-27.125297150064,14.2134355726879,127.998946383917)) ;
#126179 = CARTESIAN_POINT('Ctrl Pts',(-27.0774187575892,13.958237750451,127.825922594833)) ;
#126180 = CARTESIAN_POINT('Ctrl Pts',(-27.0535942488343,13.6646542433851,
127.723173741456)) ;
#126181 = CARTESIAN_POINT('Ctrl Pts',(-27.0562015090421,13.3541836423797,
127.697682670805)) ;
#126182 = CARTESIAN_POINT('Ctrl Pts',(-27.0857370264101,13.0484268899304,
127.750836023562)) ;
#126183 = CARTESIAN_POINT('Ctrl Pts',(-27.1409450439948,12.769439556936,127.87895999406)) ;
#126184 = CARTESIAN_POINT('Ctrl Pts',(-27.2180733512631,12.538041732005,128.071268052011)) ;
#126185 = CARTESIAN_POINT('Ctrl Pts',(-27.3137559998053,12.3683285737822,
128.317416850313)) ;
#126186 = CARTESIAN_POINT('Ctrl Pts',(-27.4196365681885,12.2760420146323,
128.593780876063)) ;
#126187 = CARTESIAN_POINT('Ctrl Pts',(-27.5306231079652,12.2649172046645,
128.884867753868)) ;
#126188 = CARTESIAN_POINT('Ctrl Pts',(-27.6389017948996,12.3368690960139,
129.1680658529)) ;
#126189 = CARTESIAN_POINT('Ctrl Pts',(-27.7377556093054,12.4871143046054,
129.423632129144)) ;
#126190 = CARTESIAN_POINT('Ctrl Pts',(-27.8202491494068,12.7041606562746,
129.631498782579)) ;
#126191 = CARTESIAN_POINT('Ctrl Pts',(-27.8814612994333,12.9721743226057,
129.777246365525)) ;
#126192 = CARTESIAN_POINT('Ctrl Pts',(-27.9178954972168,13.2726903984431,
129.850577604052)) ;
#126193 = CARTESIAN_POINT('Ctrl Pts',(-27.9276073498743,13.5844635777056,
129.845797878301)) ;
#126194 = CARTESIAN_POINT('Ctrl Pts',(-27.9104034593952,13.8852371899129,
129.762316738143)) ;
#126195 = CARTESIAN_POINT('Ctrl Pts',(-27.8686813644329,14.1508961258859,
129.607456776857)) ;
#126196 = CARTESIAN_POINT('Ctrl Pts',(-27.805777890454,14.3659570919706,129.390557072871)) ;
#126197 = CARTESIAN_POINT('Ctrl Pts',(-27.7267920219095,14.5133844766524,
129.126610121449)) ;
#126198 = CARTESIAN_POINT('Ctrl Pts',(-27.6388634022396,14.5822824975676,
128.836735478804)) ;
#126199 = CARTESIAN_POINT('Ctrl Pts',(-27.5480345518923,14.5684017551043,
128.538201746879)) ;
#126200 = CARTESIAN_POINT('Ctrl Pts',(-27.4623293694807,14.4726240030268,
128.254765455669)) ;
#126201 = CARTESIAN_POINT('Ctrl Pts',(-27.3879707689627,14.3009017831871,
128.004315479595)) ;
#126202 = CARTESIAN_POINT('Ctrl Pts',(-27.3317507009227,14.0676661547484,
127.807078623479)) ;
#126203 = CARTESIAN_POINT('Ctrl Pts',(-27.2976904983125,13.7867922981234,
127.67436647184)) ;
#126204 = CARTESIAN_POINT('Ctrl Pts',(-27.2894631150385,13.4808115386222,
127.61724202784)) ;
#126205 = CARTESIAN_POINT('Ctrl Pts',(-27.3080625977825,13.1706177086878,
127.638476490103)) ;
#126206 = CARTESIAN_POINT('Ctrl Pts',(-27.3533779369102,12.877048394192,127.737575696294)) ;
#126207 = CARTESIAN_POINT('Ctrl Pts',(-27.4219972748813,12.6251910446387,
127.905071056163)) ;
#126208 = CARTESIAN_POINT('Ctrl Pts',(-27.5104518024654,12.4289584730978,
128.130355526478)) ;
#126209 = CARTESIAN_POINT('Ctrl Pts',(-27.6133286223986,12.3038002385442,
128.397669935348)) ;
#126210 = CARTESIAN_POINT('Ctrl Pts',(-27.7232164389536,12.2593442702032,
128.68559205266)) ;
#126211 = CARTESIAN_POINT('Ctrl Pts',(-27.8332334336571,12.2978898762746,
128.973926847691)) ;
#126212 = CARTESIAN_POINT('Ctrl Pts',(-27.9366469237781,12.4169444265874,
129.242893983991)) ;
#126213 = CARTESIAN_POINT('Ctrl Pts',(-28.0268222922301,12.6093773192219,
129.473030956235)) ;
#126214 = CARTESIAN_POINT('Ctrl Pts',(-28.0969743287122,12.8583734151229,
129.644955599161)) ;
#126215 = CARTESIAN_POINT('Ctrl Pts',(-28.1438275325612,13.1480449796925,
129.748746916576)) ;
#126216 = CARTESIAN_POINT('Ctrl Pts',(-28.1644954117435,13.4582418088587,
129.775959672609)) ;
#126217 = CARTESIAN_POINT('Ctrl Pts',(-28.1581306779681,13.7655079341762,
129.724247830302)) ;
#126218 = CARTESIAN_POINT('Ctrl Pts',(-28.1259517579114,14.048316994012,129.59711509984)) ;
#126219 = CARTESIAN_POINT('Ctrl Pts',(-28.0711052803105,14.2859990299988,
129.403818984126)) ;
#126220 = CARTESIAN_POINT('Ctrl Pts',(-27.9979984934453,14.4624790722787,
129.157095753605)) ;
#126221 = CARTESIAN_POINT('Ctrl Pts',(-27.9126529086255,14.5642184031824,
128.874605844398)) ;
#126222 = CARTESIAN_POINT('Ctrl Pts',(-27.82234244871,14.584160945988,128.577742029782)) ;
#126223 = CARTESIAN_POINT('Ctrl Pts',(-27.7335731289501,14.5209707107522,
128.285251255355)) ;
#126224 = CARTESIAN_POINT('Ctrl Pts',(-27.6539417613536,14.3791778899535,
128.019520055056)) ;
#126225 = CARTESIAN_POINT('Ctrl Pts',(-27.5896417043547,14.1688150689694,
127.798546337055)) ;
#126226 = CARTESIAN_POINT('Ctrl Pts',(-27.5461247472488,13.9051956236196,
127.638312484282)) ;
#126227 = CARTESIAN_POINT('Ctrl Pts',(-27.5271452909361,13.6071499712881,
127.54976394242)) ;
#126228 = CARTESIAN_POINT('Ctrl Pts',(-27.5348305475125,13.2953842790605,
127.539053516484)) ;
#126229 = CARTESIAN_POINT('Ctrl Pts',(-27.5694192910359,12.9930168542047,
127.606957456664)) ;
#126230 = CARTESIAN_POINT('Ctrl Pts',(-27.6288755570811,12.722227284065,127.747605806903)) ;
#126231 = CARTESIAN_POINT('Ctrl Pts',(-27.7100939855666,12.5005440271994,
127.951701688244)) ;
#126232 = CARTESIAN_POINT('Ctrl Pts',(-27.8080372736976,12.3451352919228,
128.204600625969)) ;
#126233 = CARTESIAN_POINT('Ctrl Pts',(-27.9154950057297,12.2674914162103,
128.485503862418)) ;
#126234 = CARTESIAN_POINT('Ctrl Pts',(-28.0268939179855,12.2722652816386,
128.777693027108)) ;
#126235 = CARTESIAN_POINT('Ctrl Pts',(-28.1338981955741,12.3599738875374,
129.057142459325)) ;
#126236 = CARTESIAN_POINT('Ctrl Pts',(-28.2294682857705,12.522637910065,129.303361399343)) ;
#126237 = CARTESIAN_POINT('Ctrl Pts',(-28.3085931444286,12.7508223350777,
129.501319058887)) ;
#126238 = CARTESIAN_POINT('Ctrl Pts',(-28.3656063081004,13.0279566235447,
129.634633388162)) ;
#126239 = CARTESIAN_POINT('Ctrl Pts',(-28.3969444639279,13.3323088318152,
129.693075814844)) ;
#126240 = CARTESIAN_POINT('Ctrl Pts',(-28.4014787981811,13.6420774787073,
129.673330395157)) ;
#126241 = CARTESIAN_POINT('Ctrl Pts',(-28.3795963264581,13.9374078863426,
129.576285309709)) ;
#126242 = CARTESIAN_POINT('Ctrl Pts',(-28.3333509219362,14.1965319765984,
129.407993850494)) ;
#126243 = CARTESIAN_POINT('Ctrl Pts',(-28.266675124667,14.3999725992787,129.179974394099)) ;
#126244 = CARTESIAN_POINT('Ctrl Pts',(-28.1862016672231,14.5320840225921,
128.912009605806)) ;
#126245 = CARTESIAN_POINT('Ctrl Pts',(-28.0966741913854,14.5862914481746,
128.617232858697)) ;
#126246 = CARTESIAN_POINT('Ctrl Pts',(-28.0062577051871,14.5562373139742,
128.319925352826)) ;
#126247 = CARTESIAN_POINT('Ctrl Pts',(-27.9225302663962,14.446076002877,128.042377588389)) ;
#126248 = CARTESIAN_POINT('Ctrl Pts',(-27.8509244482422,14.2613118658137,
127.799922177814)) ;
#126249 = CARTESIAN_POINT('Ctrl Pts',(-27.798497284698,14.0168342944467,127.613633246462)) ;
#126250 = CARTESIAN_POINT('Ctrl Pts',(-27.7692851272863,13.7314084945653,
127.495315906887)) ;
#126251 = CARTESIAN_POINT('Ctrl Pts',(-27.7660083743788,13.4213927806631,
127.45248187371)) ;
#126252 = CARTESIAN_POINT('Ctrl Pts',(-27.7897193573963,13.1138964829047,
127.488747985494)) ;
#126253 = CARTESIAN_POINT('Ctrl Pts',(-27.8393546178715,12.8273574952535,
127.600633072825)) ;
#126254 = CARTESIAN_POINT('Ctrl Pts',(-27.9127949354444,12.5821904217373,
127.781847712348)) ;
#126255 = CARTESIAN_POINT('Ctrl Pts',(-28.0043735492926,12.3992406566731,
128.016306398527)) ;
#126256 = CARTESIAN_POINT('Ctrl Pts',(-28.1087022331987,12.2892635320147,
128.288009999253)) ;
#126257 = CARTESIAN_POINT('Ctrl Pts',(-28.2190913648179,12.2601882735182,
128.57742408835)) ;
#126258 = CARTESIAN_POINT('Ctrl Pts',(-28.3287542082612,12.3144490437337,
128.864604111698)) ;
#126259 = CARTESIAN_POINT('Ctrl Pts',(-28.4299954593875,12.4481500552587,
129.127241049758)) ;
#126260 = CARTESIAN_POINT('Ctrl Pts',(-28.5165306603846,12.6515765738091,
129.346913037363)) ;
#126261 = CARTESIAN_POINT('Ctrl Pts',(-28.5830300089725,12.911209097722,129.507949494699)) ;
#126262 = CARTESIAN_POINT('Ctrl Pts',(-28.6249728675832,13.2069681338802,
129.597336632742)) ;
#126263 = CARTESIAN_POINT('Ctrl Pts',(-28.6404608703377,13.5165271467016,
129.609618370989)) ;
#126264 = CARTESIAN_POINT('Ctrl Pts',(-28.6290148464267,13.8224961920609,
129.542876508472)) ;
#126265 = CARTESIAN_POINT('Ctrl Pts',(-28.5922601971028,14.0973150821475,
129.402480129101)) ;
#126266 = CARTESIAN_POINT('Ctrl Pts',(-28.5336757378928,14.3244518569206,
129.198286920491)) ;
#126267 = CARTESIAN_POINT('Ctrl Pts',(-28.4576637523532,14.4877799967397,
128.943033798244)) ;
#126268 = CARTESIAN_POINT('Ctrl Pts',(-28.3710048581047,14.5742905029568,
128.656795471305)) ;
#126269 = CARTESIAN_POINT('Ctrl Pts',(-28.2802241255344,14.5785355282753,
128.35845638066)) ;
#126270 = CARTESIAN_POINT('Ctrl Pts',(-28.1928419853,14.4999982805016,128.070098188264)) ;
#126271 = CARTESIAN_POINT('Ctrl Pts',(-28.1156963429542,14.344757358462,127.811665392834)) ;
#126272 = CARTESIAN_POINT('Ctrl Pts',(-28.0547636884467,14.1223923332962,
127.600432721674)) ;
#126273 = CARTESIAN_POINT('Ctrl Pts',(-28.0157051647959,13.8510685521418,
127.45327003594)) ;
#126274 = CARTESIAN_POINT('Ctrl Pts',(-28.0016271877878,13.5484335086258,
127.378992507059)) ;
#126275 = CARTESIAN_POINT('Ctrl Pts',(-28.014450669107,13.2370240609784,127.383328520091)) ;
#126276 = CARTESIAN_POINT('Ctrl Pts',(-28.0538788566097,12.9391310692164,
127.465404042021)) ;
#126277 = CARTESIAN_POINT('Ctrl Pts',(-28.1178898237982,12.6756659712694,
127.619266774088)) ;
#126278 = CARTESIAN_POINT('Ctrl Pts',(-28.2026458744836,12.4657027471288,
127.833719653981)) ;
#126279 = CARTESIAN_POINT('Ctrl Pts',(-28.3027339455981,12.3244745287068,
128.092974050606)) ;
#126280 = CARTESIAN_POINT('Ctrl Pts',(-28.4116254389229,12.2619232724697,
128.377977700105)) ;
#126281 = CARTESIAN_POINT('Ctrl Pts',(-28.5225430499368,12.2825882461712,
128.668841361449)) ;
#126282 = CARTESIAN_POINT('Ctrl Pts',(-28.6277358208058,12.3846501373822,
128.943090603315)) ;
#126283 = CARTESIAN_POINT('Ctrl Pts',(-28.7210231729538,12.5611187376007,
129.182483263865)) ;
#126284 = CARTESIAN_POINT('Ctrl Pts',(-28.7963015152677,12.8001289118654,
129.369183041344)) ;
#126285 = CARTESIAN_POINT('Ctrl Pts',(-28.848510718025,13.0829558583446,129.488606078419)) ;
#126286 = CARTESIAN_POINT('Ctrl Pts',(-28.8749835754297,13.3903655570018,
129.532815151912)) ;
#126287 = CARTESIAN_POINT('Ctrl Pts',(-28.8744412770404,13.7001366244489,
129.498104859533)) ;
#126288 = CARTESIAN_POINT('Ctrl Pts',(-28.8477145078455,13.9898881879969,
129.386927516853)) ;
#126289 = CARTESIAN_POINT('Ctrl Pts',(-28.7973599708568,14.2391934604651,
129.206697827823)) ;
#126290 = CARTESIAN_POINT('Ctrl Pts',(-28.7279827552736,14.4298567276207,
128.970982641298)) ;
#126291 = CARTESIAN_POINT('Ctrl Pts',(-28.644258384591,14.5492471456149,128.693044021335)) ;
#126292 = CARTESIAN_POINT('Ctrl Pts',(-28.554796284374,14.5868020959289,128.39877651472)) ;
#126293 = CARTESIAN_POINT('Ctrl Pts',(-28.4650804844611,14.5417975153692,
128.103553265323)) ;
#126294 = CARTESIAN_POINT('Ctrl Pts',(-28.3828462169605,14.4162088209851,
127.830180515014)) ;
#126295 = CARTESIAN_POINT('Ctrl Pts',(-28.3148259514202,14.2204083214859,
127.598438875209)) ;
#126296 = CARTESIAN_POINT('Ctrl Pts',(-28.2660768691486,13.9647701024183,
127.422650641298)) ;
#126297 = CARTESIAN_POINT('Ctrl Pts',(-28.2417393818523,13.6739288437871,
127.318633866623)) ;
#126298 = CARTESIAN_POINT('Ctrl Pts',(-28.2435589798425,13.362328471029,127.290695136997)) ;
#126299 = CARTESIAN_POINT('Ctrl Pts',(-28.272280384429,13.0574724209015,127.341613025253)) ;
#126300 = CARTESIAN_POINT('Ctrl Pts',(-28.3266764891578,12.7770676806865,
127.467351744318)) ;
#126301 = CARTESIAN_POINT('Ctrl Pts',(-28.4039036629146,12.5427864739332,
127.659709669059)) ;
#126302 = CARTESIAN_POINT('Ctrl Pts',(-28.4979676565153,12.3731888111629,
127.901550196768)) ;
#126303 = CARTESIAN_POINT('Ctrl Pts',(-28.6042086691124,12.2773794230824,
128.178756519312)) ;
#126304 = CARTESIAN_POINT('Ctrl Pts',(-28.715472627962,12.2641879723106,128.47056855639)) ;
#126305 = CARTESIAN_POINT('Ctrl Pts',(-28.8235400299554,12.3335960858358,
128.753264954274)) ;
#126306 = CARTESIAN_POINT('Ctrl Pts',(-28.9227867930702,12.4815617101667,
129.009979499555)) ;
#126307 = CARTESIAN_POINT('Ctrl Pts',(-29.0058719352323,12.6968288003286,
129.219569350323)) ;
#126308 = CARTESIAN_POINT('Ctrl Pts',(-29.0678679462344,12.9642191171328,
129.367533009777)) ;
#126309 = CARTESIAN_POINT('Ctrl Pts',(-29.1050280217852,13.2637556030546,
129.443027420191)) ;
#126310 = CARTESIAN_POINT('Ctrl Pts',(-29.1154418002506,13.5766924952844,
129.440167113031)) ;
#126311 = CARTESIAN_POINT('Ctrl Pts',(-29.0991939031422,13.8753723119149,
129.359790683957)) ;
#126312 = CARTESIAN_POINT('Ctrl Pts',(-29.0578831159195,14.1446746282912,
129.205850385365)) ;
#126313 = CARTESIAN_POINT('Ctrl Pts',(-28.9955328716822,14.3606486732163,
128.990637905782)) ;
#126314 = CARTESIAN_POINT('Ctrl Pts',(-28.9172212199739,14.510078619128,128.72876476362)) ;
#126315 = CARTESIAN_POINT('Ctrl Pts',(-28.8287816094018,14.5815775918547,
128.437141604284)) ;
#126316 = CARTESIAN_POINT('Ctrl Pts',(-28.7385909291533,14.5700419701179,
128.140725723263)) ;
#126317 = CARTESIAN_POINT('Ctrl Pts',(-28.6522425556229,14.4761037327312,
127.855240333411)) ;
#126318 = CARTESIAN_POINT('Ctrl Pts',(-28.5778444620489,14.3074346005472,
127.604870863317)) ;
#126319 = CARTESIAN_POINT('Ctrl Pts',(-28.5205972031991,14.073572566118,127.404328059254)) ;
#126320 = CARTESIAN_POINT('Ctrl Pts',(-28.4862429573869,13.7966474057212,
127.271116789574)) ;
#126321 = CARTESIAN_POINT('Ctrl Pts',(-28.4770859270264,13.4894704941488,
127.211081165859)) ;
#126322 = CARTESIAN_POINT('Ctrl Pts',(-28.4948943292332,13.1800818047294,
127.230117007035)) ;
#126323 = CARTESIAN_POINT('Ctrl Pts',(-28.5394276796164,12.8853355952022,
127.326898324992)) ;
#126324 = CARTESIAN_POINT('Ctrl Pts',(-28.6074761504503,12.6318025855322,
127.492695185973)) ;
#126325 = CARTESIAN_POINT('Ctrl Pts',(-28.695470726565,12.4337108442548,127.716625488695)) ;
#126326 = CARTESIAN_POINT('Ctrl Pts',(-28.7978123159624,12.3064394695167,
127.982443096435)) ;
#126327 = CARTESIAN_POINT('Ctrl Pts',(-28.9079039717027,12.259467253753,128.270860085229)) ;
#126328 = CARTESIAN_POINT('Ctrl Pts',(-29.0179009527206,12.2954707770716,
128.559180514689)) ;
#126329 = CARTESIAN_POINT('Ctrl Pts',(-29.1222060572925,12.4135506736779,
128.830531653871)) ;
#126330 = CARTESIAN_POINT('Ctrl Pts',(-29.2116568789094,12.6014761688176,
129.059003773852)) ;
#126331 = CARTESIAN_POINT('Ctrl Pts',(-29.2831239492051,12.8505488617132,
129.234511371657)) ;
#126332 = CARTESIAN_POINT('Ctrl Pts',(-29.3306092364222,13.1393106642719,
129.340171358804)) ;
#126333 = CARTESIAN_POINT('Ctrl Pts',(-29.3520748841438,13.4495612707078,
129.369675966618)) ;
#126334 = CARTESIAN_POINT('Ctrl Pts',(-29.3464729517262,13.7566531065693,
129.320254581372)) ;
#126335 = CARTESIAN_POINT('Ctrl Pts',(-29.3150443593479,14.0404143617275,
129.195320768512)) ;
#126336 = CARTESIAN_POINT('Ctrl Pts',(-29.2608243465156,14.2798568103851,
129.003847830969)) ;
#126337 = CARTESIAN_POINT('Ctrl Pts',(-29.1878014525805,14.4588607973601,
128.757223804424)) ;
#126338 = CARTESIAN_POINT('Ctrl Pts',(-29.1031844107461,14.5622468207321,
128.477052820405)) ;
#126339 = CARTESIAN_POINT('Ctrl Pts',(-29.0125825178535,14.5847589284177,
128.179204966729)) ;
#126340 = CARTESIAN_POINT('Ctrl Pts',(-28.9239262939069,14.5239999294188,
127.887147086676)) ;
#126341 = CARTESIAN_POINT('Ctrl Pts',(-28.8438246268334,14.3842925756614,
127.619996920254)) ;
#126342 = CARTESIAN_POINT('Ctrl Pts',(-28.7790368369442,14.1758058754008,
127.397617265261)) ;
#126343 = CARTESIAN_POINT('Ctrl Pts',(-28.7347735365329,13.9130883833925,
127.235151253729)) ;
#126344 = CARTESIAN_POINT('Ctrl Pts',(-28.7151135618664,13.6151579335754,
127.144558769301)) ;
#126345 = CARTESIAN_POINT('Ctrl Pts',(-28.7219995435927,13.3050553518441,
127.131682646232)) ;
#126346 = CARTESIAN_POINT('Ctrl Pts',(-28.7557377597948,13.0018870987347,
127.197084482543)) ;
#126347 = CARTESIAN_POINT('Ctrl Pts',(-28.814675083667,12.7291797299788,127.336129164948)) ;
#126348 = CARTESIAN_POINT('Ctrl Pts',(-28.8952944144317,12.5061726224373,
127.538507349107)) ;
#126349 = CARTESIAN_POINT('Ctrl Pts',(-28.992452875052,12.3489725905771,127.789232229175)) ;
#126350 = CARTESIAN_POINT('Ctrl Pts',(-29.1001181450375,12.2685649990364,
128.070611823995)) ;
#126351 = CARTESIAN_POINT('Ctrl Pts',(-29.2111067626934,12.2709027590492,
128.361728243776)) ;
#126352 = CARTESIAN_POINT('Ctrl Pts',(-29.3183871335447,12.3558100715775,
128.641979311852)) ;
#126353 = CARTESIAN_POINT('Ctrl Pts',(-29.4148436719289,12.5172182560686,
128.890625247685)) ;
#126354 = CARTESIAN_POINT('Ctrl Pts',(-29.4942688116787,12.743270611073,129.089550396418)) ;
#126355 = CARTESIAN_POINT('Ctrl Pts',(-29.551869204403,13.0180148278647,129.224707278106)) ;
#126356 = CARTESIAN_POINT('Ctrl Pts',(-29.5842039318189,13.3228200342207,
129.285946655861)) ;
#126357 = CARTESIAN_POINT('Ctrl Pts',(-29.5895128485569,13.6334362897112,
129.268389620136)) ;
#126358 = CARTESIAN_POINT('Ctrl Pts',(-29.5683363278282,13.929416387864,129.173412954777)) ;
#126359 = CARTESIAN_POINT('Ctrl Pts',(-29.5228950497417,14.1891570751448,
129.007566404027)) ;
#126360 = CARTESIAN_POINT('Ctrl Pts',(-29.4568217632275,14.3946402332245,
128.78131441326)) ;
#126361 = CARTESIAN_POINT('Ctrl Pts',(-29.3763677570869,14.5295569095383,
128.513275619402)) ;
#126362 = CARTESIAN_POINT('Ctrl Pts',(-29.2868834281595,14.5858061320267,
128.218594172143)) ;
#126363 = CARTESIAN_POINT('Ctrl Pts',(-29.1968889427481,14.5585141684262,
127.922706052922)) ;
#126364 = CARTESIAN_POINT('Ctrl Pts',(-29.1124170400181,14.4500372102403,
127.642795696124)) ;
#126365 = CARTESIAN_POINT('Ctrl Pts',(-29.0407778038687,14.268202012558,127.400434608182)) ;
#126366 = CARTESIAN_POINT('Ctrl Pts',(-28.9875018774522,14.0250734119471,
127.211599238186)) ;
#126367 = CARTESIAN_POINT('Ctrl Pts',(-28.9575029477622,13.7389393518604,
127.090807741331)) ;
#126368 = CARTESIAN_POINT('Ctrl Pts',(-28.9535386701218,13.4311037036194,
127.046163668047)) ;
#126369 = CARTESIAN_POINT('Ctrl Pts',(-28.9763267200494,13.1229020321195,
127.079702982171)) ;
#126370 = CARTESIAN_POINT('Ctrl Pts',(-29.0257949317233,12.8333723855065,
127.190836011178)) ;
#126371 = CARTESIAN_POINT('Ctrl Pts',(-29.0978600733987,12.5895126789185,
127.368402800474)) ;
#126372 = CARTESIAN_POINT('Ctrl Pts',(-29.1892280354939,12.4035404975601,
127.602115483622)) ;
#126373 = CARTESIAN_POINT('Ctrl Pts',(-29.2932741260525,12.2914040477839,
127.873003194407)) ;
#126374 = CARTESIAN_POINT('Ctrl Pts',(-29.4037033629628,12.259812265838,128.162497247571)) ;
#126375 = CARTESIAN_POINT('Ctrl Pts',(-29.5135609204899,12.3118570241587,
128.450226071125)) ;
#126376 = CARTESIAN_POINT('Ctrl Pts',(-29.6149254569401,12.4430958843788,
128.713290866227)) ;
#126377 = CARTESIAN_POINT('Ctrl Pts',(-29.7020530820368,12.6447072746916,
128.934674038552)) ;
#126378 = CARTESIAN_POINT('Ctrl Pts',(-29.7691752470244,12.9030427397014,
129.097526306521)) ;
#126379 = CARTESIAN_POINT('Ctrl Pts',(-29.8118434047462,13.1970329557463,
129.189137020104)) ;
#126380 = CARTESIAN_POINT('Ctrl Pts',(-29.8281637012964,13.5084313502234,
129.203633314877)) ;
#126381 = CARTESIAN_POINT('Ctrl Pts',(-29.8176270439828,13.8121188302543,
129.139861139091)) ;
#126382 = CARTESIAN_POINT('Ctrl Pts',(-29.7814625744293,14.0900962513971,
129.000962562861)) ;
#126383 = CARTESIAN_POINT('Ctrl Pts',(-29.7234265946476,14.31872996458,128.798387529551)) ;
#126384 = CARTESIAN_POINT('Ctrl Pts',(-29.6476098832969,14.484422730659,128.543613950177)) ;
#126385 = CARTESIAN_POINT('Ctrl Pts',(-29.5615142448024,14.5727758927101,
128.259159521948)) ;
#126386 = CARTESIAN_POINT('Ctrl Pts',(-29.4707443641585,14.5796460422286,
127.960845873962)) ;
#126387 = CARTESIAN_POINT('Ctrl Pts',(-29.3831258062148,14.5035865487986,
127.671790345692)) ;
#126388 = CARTESIAN_POINT('Ctrl Pts',(-29.3052805384703,14.3497062950072,
127.411173840987)) ;
#126389 = CARTESIAN_POINT('Ctrl Pts',(-29.2439657968061,14.1291329679128,
127.198875466525)) ;
#126390 = CARTESIAN_POINT('Ctrl Pts',(-29.2043177636014,13.8597726326946,
127.05008067997)) ;
#126391 = CARTESIAN_POINT('Ctrl Pts',(-29.1894481468779,13.557462341525,126.973458033413)) ;
#126392 = CARTESIAN_POINT('Ctrl Pts',(-29.2014467723286,13.2463365194833,
126.975423633126)) ;
#126393 = CARTESIAN_POINT('Ctrl Pts',(-29.240192496977,12.9472973154242,127.055450427306)) ;
#126394 = CARTESIAN_POINT('Ctrl Pts',(-29.3033094304608,12.6832077780023,
127.2068001365)) ;
#126395 = CARTESIAN_POINT('Ctrl Pts',(-29.3879194372612,12.4704982394892,
127.420671040737)) ;
#126396 = CARTESIAN_POINT('Ctrl Pts',(-29.4873059937918,12.3276823235439,
127.677998441968)) ;
#126397 = CARTESIAN_POINT('Ctrl Pts',(-29.5962501169316,12.2625925201889,
127.963084302124)) ;
#126398 = CARTESIAN_POINT('Ctrl Pts',(-29.7068390569069,12.280619224966,128.25310533232)) ;
#126399 = CARTESIAN_POINT('Ctrl Pts',(-29.8129831084837,12.3809214756921,
128.529919358557)) ;
#126400 = CARTESIAN_POINT('Ctrl Pts',(-29.906657709987,12.556040128184,128.770421483879)) ;
#126401 = CARTESIAN_POINT('Ctrl Pts',(-29.9820403676067,12.7918901581632,
128.957644910704)) ;
#126402 = CARTESIAN_POINT('Ctrl Pts',(-30.0351697168892,13.0744209862709,
129.079658466158)) ;
#126403 = CARTESIAN_POINT('Ctrl Pts',(-30.0623799674238,13.3812416833702,
129.126046104789)) ;
#126404 = CARTESIAN_POINT('Ctrl Pts',(-30.0626128615332,13.6920797161949,
129.093513213577)) ;
#126405 = CARTESIAN_POINT('Ctrl Pts',(-30.0365037669751,13.9824941766623,
128.984145022211)) ;
#126406 = CARTESIAN_POINT('Ctrl Pts',(-29.987039803891,14.2323227471641,128.806660210106)) ;
#126407 = CARTESIAN_POINT('Ctrl Pts',(-29.9176946082372,14.4258243482768,
128.570836399515)) ;
#126408 = CARTESIAN_POINT('Ctrl Pts',(-29.8350161561935,14.5465247223938,
128.29625314965)) ;
#126409 = CARTESIAN_POINT('Ctrl Pts',(-29.7448155074623,14.5869806833893,
127.999509947687)) ;
#126410 = CARTESIAN_POINT('Ctrl Pts',(-29.6554990618739,14.5442058476213,
127.705640700795)) ;
#126411 = CARTESIAN_POINT('Ctrl Pts',(-29.5727669786191,14.4209679586328,
127.430757402841)) ;
#126412 = CARTESIAN_POINT('Ctrl Pts',(-29.5040785211676,14.2257906516459,
127.196921938398)) ;
#126413 = CARTESIAN_POINT('Ctrl Pts',(-29.4551663445329,13.9741287595616,
127.020990849854)) ;
#126414 = CARTESIAN_POINT('Ctrl Pts',(-29.4298421339555,13.6829512293512,
126.91393472797)) ;
#126415 = CARTESIAN_POINT('Ctrl Pts',(-29.4309001415048,13.37146650651,126.88376820502)) ;
#126416 = CARTESIAN_POINT('Ctrl Pts',(-29.4589213897168,13.0656058260286,
126.932576869768)) ;
#126417 = CARTESIAN_POINT('Ctrl Pts',(-29.5125089739452,12.7850334229127,
127.056046900933)) ;
#126418 = CARTESIAN_POINT('Ctrl Pts',(-29.5887530272508,12.5496672671412,
127.24565170869)) ;
#126419 = CARTESIAN_POINT('Ctrl Pts',(-29.6830427688529,12.3766688304073,
127.487911118153)) ;
#126420 = CARTESIAN_POINT('Ctrl Pts',(-29.7890527274797,12.2789529109886,
127.76445425575)) ;
#126421 = CARTESIAN_POINT('Ctrl Pts',(-29.9000873163388,12.2634413575716,
128.055650583301)) ;
#126422 = CARTESIAN_POINT('Ctrl Pts',(-30.0083485486883,12.3304157181155,
128.338911431539)) ;
#126423 = CARTESIAN_POINT('Ctrl Pts',(-30.1082772334579,12.4770344340702,
128.597497281747)) ;
#126424 = CARTESIAN_POINT('Ctrl Pts',(-30.1914295574665,12.6896430839443,
128.807450070267)) ;
#126425 = CARTESIAN_POINT('Ctrl Pts',(-30.2541271970478,12.9554492280344,
128.957485437549)) ;
#126426 = CARTESIAN_POINT('Ctrl Pts',(-30.2920888176688,13.2546656267019,
129.035282868155)) ;
#126427 = CARTESIAN_POINT('Ctrl Pts',(-30.3033302444878,13.5672375771819,
129.034881121933)) ;
#126428 = CARTESIAN_POINT('Ctrl Pts',(-30.2877588882589,13.8673528503954,
128.956383179478)) ;
#126429 = CARTESIAN_POINT('Ctrl Pts',(-30.2473790223749,14.1367236573279,
128.805324735594)) ;
#126430 = CARTESIAN_POINT('Ctrl Pts',(-30.1850909266063,14.3561277006207,
128.590031160462)) ;
#126431 = CARTESIAN_POINT('Ctrl Pts',(-30.1075087264643,14.5065131900063,
128.33046827587)) ;
#126432 = CARTESIAN_POINT('Ctrl Pts',(-30.0194926425284,14.5806176996537,
128.040156515334)) ;
#126433 = CARTESIAN_POINT('Ctrl Pts',(-29.9289678243319,14.5715966835969,
127.742653447193)) ;
#126434 = CARTESIAN_POINT('Ctrl Pts',(-29.8423608500082,14.4799160450286,
127.456405894327)) ;
#126435 = CARTESIAN_POINT('Ctrl Pts',(-29.7675273190922,14.3130125765193,
127.204738155842)) ;
#126436 = CARTESIAN_POINT('Ctrl Pts',(-29.7099347429233,14.0821691302311,
127.003364619287)) ;
#126437 = CARTESIAN_POINT('Ctrl Pts',(-29.6745995577671,13.8046644835193,
126.86707664218)) ;
#126438 = CARTESIAN_POINT('Ctrl Pts',(-29.6647800371637,13.4979410489725,
126.805115665796)) ;
#126439 = CARTESIAN_POINT('Ctrl Pts',(-29.6818108175296,13.1889483563346,
126.821935190838)) ;
#126440 = CARTESIAN_POINT('Ctrl Pts',(-29.725449588497,12.8939178220345,126.916172175486)) ;
#126441 = CARTESIAN_POINT('Ctrl Pts',(-29.7931536798143,12.6378239154038,
127.080814108066)) ;
#126442 = CARTESIAN_POINT('Ctrl Pts',(-29.8806868304317,12.4382802078468,
127.303412931666)) ;
#126443 = CARTESIAN_POINT('Ctrl Pts',(-29.9822588186338,12.3092349638881,
127.567120846418)) ;
#126444 = CARTESIAN_POINT('Ctrl Pts',(-30.0926065124654,12.2595575251469,
127.856171070087)) ;
#126445 = CARTESIAN_POINT('Ctrl Pts',(-30.2024969870066,12.2934341319413,
128.14423155801)) ;
#126446 = CARTESIAN_POINT('Ctrl Pts',(-30.3065648134954,12.4080333826879,
128.415084285074)) ;
#126447 = CARTESIAN_POINT('Ctrl Pts',(-30.3975305959679,12.5960960403323,
128.647606332589)) ;
#126448 = CARTESIAN_POINT('Ctrl Pts',(-30.4691722757746,12.843083593107,128.823760213034)) ;
#126449 = CARTESIAN_POINT('Ctrl Pts',(-30.5173273876776,13.1299282656209,
128.931476599513)) ;
#126450 = CARTESIAN_POINT('Ctrl Pts',(-30.5396604134547,13.4413370847319,
128.963362394438)) ;
#126451 = CARTESIAN_POINT('Ctrl Pts',(-30.5347668850085,13.7480777848253,
128.916086109686)) ;
#126452 = CARTESIAN_POINT('Ctrl Pts',(-30.5040750576494,14.0327532963684,
128.793312030853)) ;
#126453 = CARTESIAN_POINT('Ctrl Pts',(-30.4504985045057,14.2736050959338,
128.603740694333)) ;
#126454 = CARTESIAN_POINT('Ctrl Pts',(-30.3778747113513,14.4547314296563,
128.358256779292)) ;
#126455 = CARTESIAN_POINT('Ctrl Pts',(-30.2936369428916,14.5602675742185,
128.079238780443)) ;
#126456 = CARTESIAN_POINT('Ctrl Pts',(-30.2030290094892,14.5853381801731,
127.781348005785)) ;
#126457 = CARTESIAN_POINT('Ctrl Pts',(-30.1141284940414,14.5268295873478,
127.488540590074)) ;
#126458 = CARTESIAN_POINT('Ctrl Pts',(-30.0337309834468,14.3893357497607,
127.220546337056)) ;
#126459 = CARTESIAN_POINT('Ctrl Pts',(-29.9684052682184,14.1825586684621,
126.996582667017)) ;
#126460 = CARTESIAN_POINT('Ctrl Pts',(-29.9235216001179,13.9213687845982,
126.832333859035)) ;
#126461 = CARTESIAN_POINT('Ctrl Pts',(-29.9031213775104,13.6242447212575,
126.739584038851)) ;
#126462 = CARTESIAN_POINT('Ctrl Pts',(-29.9091301453683,13.3143403284212,
126.724162867979)) ;
#126463 = CARTESIAN_POINT('Ctrl Pts',(-29.9424957055977,13.0084389968774,
126.788222170186)) ;
#126464 = CARTESIAN_POINT('Ctrl Pts',(-30.0002782546044,12.7371908431784,
126.924201920801)) ;
#126465 = CARTESIAN_POINT('Ctrl Pts',(-30.080582965063,12.5114337629303,127.125525392247)) ;
#126466 = CARTESIAN_POINT('Ctrl Pts',(-30.1773238460316,12.3524149247727,
127.375054033863)) ;
#126467 = CARTESIAN_POINT('Ctrl Pts',(-30.2849157680511,12.2696327934899,
127.656178093181)) ;
#126468 = CARTESIAN_POINT('Ctrl Pts',(-30.3958487396615,12.2697667408868,
127.947150017038)) ;
#126469 = CARTESIAN_POINT('Ctrl Pts',(-30.5031632538382,12.3522197325102,
128.227554335304)) ;
#126470 = CARTESIAN_POINT('Ctrl Pts',(-30.6000761875062,12.5116177862274,
128.477515668528)) ;
#126471 = CARTESIAN_POINT('Ctrl Pts',(-30.6800995647237,12.736082772034,128.678177449685)) ;
#126472 = CARTESIAN_POINT('Ctrl Pts',(-30.738510649036,13.0105747690242,128.815605552237)) ;
#126473 = CARTESIAN_POINT('Ctrl Pts',(-30.7714511773727,13.3146279151312,
128.878646647535)) ;
#126474 = CARTESIAN_POINT('Ctrl Pts',(-30.7775275155768,13.6243832359542,
128.863434416948)) ;
#126475 = CARTESIAN_POINT('Ctrl Pts',(-30.7570344764649,13.9217978697246,
128.770374564534)) ;
#126476 = CARTESIAN_POINT('Ctrl Pts',(-30.7123207653944,14.1821018677862,
128.606738727323)) ;
#126477 = CARTESIAN_POINT('Ctrl Pts',(-30.6468826077252,14.3894123612741,
128.382372687917)) ;
#126478 = CARTESIAN_POINT('Ctrl Pts',(-30.5664940708433,14.5268848445949,
128.114414955078)) ;
#126479 = CARTESIAN_POINT('Ctrl Pts',(-30.4774434259798,14.585256166508,127.821110439417)) ;
#126480 = CARTESIAN_POINT('Ctrl Pts',(-30.387335916858,14.5605921317333,127.524875838204)) ;
#126481 = CARTESIAN_POINT('Ctrl Pts',(-30.3024923367865,14.4542388415829,
127.243838232397)) ;
#126482 = CARTESIAN_POINT('Ctrl Pts',(-30.230353520966,14.2743936202259,127.000011757054)) ;
#126483 = CARTESIAN_POINT('Ctrl Pts',(-30.1763747618644,14.0316377152924,
126.808994082915)) ;
#126484 = CARTESIAN_POINT('Ctrl Pts',(-30.1458639176194,13.7487556087195,
126.686973351521)) ;
#126485 = CARTESIAN_POINT('Ctrl Pts',(-30.1410714925664,13.4387761357976,
126.639634653648)) ;
#126486 = CARTESIAN_POINT('Ctrl Pts',(-30.1630937482503,13.131784657343,126.671100007775)) ;
#126487 = CARTESIAN_POINT('Ctrl Pts',(-30.2118435570482,12.8410201909971,
126.78009912382)) ;
#126488 = CARTESIAN_POINT('Ctrl Pts',(-30.2831176592298,12.5963886012332,
126.955444403938)) ;
#126489 = CARTESIAN_POINT('Ctrl Pts',(-30.3738139118341,12.4083250161853,
127.187236450367)) ;
#126490 = CARTESIAN_POINT('Ctrl Pts',(-30.4782746115266,12.2932606214,127.459115432517)) ;
#126491 = CARTESIAN_POINT('Ctrl Pts',(-30.5880990881978,12.2596773190563,
127.747003747489)) ;
#126492 = CARTESIAN_POINT('Ctrl Pts',(-30.6980230573031,12.3089369873083,
128.03494702501)) ;
#126493 = CARTESIAN_POINT('Ctrl Pts',(-30.8001371723159,12.4384179192494,
128.300074442046)) ;
#126494 = CARTESIAN_POINT('Ctrl Pts',(-30.887812752522,12.6389284665683,128.522996047447)) ;
#126495 = CARTESIAN_POINT('Ctrl Pts',(-30.9550781560894,12.8936369055523,
128.686545839235)) ;
#126496 = CARTESIAN_POINT('Ctrl Pts',(-30.9988884958278,13.1890353554826,
128.781232646274)) ;
#126497 = CARTESIAN_POINT('Ctrl Pts',(-31.0158460752313,13.4997524264947,
128.797656813682)) ;
#126498 = CARTESIAN_POINT('Ctrl Pts',(-31.0060377770145,13.8039809535807,
128.735996805114)) ;
#126499 = CARTESIAN_POINT('Ctrl Pts',(-30.9707318332435,14.0820722250227,
128.599733823845)) ;
#126500 = CARTESIAN_POINT('Ctrl Pts',(-30.9131292647479,14.3130041304952,
128.398329360413)) ;
#126501 = CARTESIAN_POINT('Ctrl Pts',(-30.8381066903904,14.4800545558914,
128.146034853665)) ;
#126502 = CARTESIAN_POINT('Ctrl Pts',(-30.7520139126598,14.5714592047604,
127.861485917471)) ;
#126503 = CARTESIAN_POINT('Ctrl Pts',(-30.6608114307688,14.580498376248,127.561746515086)) ;
#126504 = CARTESIAN_POINT('Ctrl Pts',(-30.5734428928017,14.5069052062207,
127.273578758881)) ;
#126505 = CARTESIAN_POINT('Ctrl Pts',(-30.4953155212185,14.355702929433,127.012199444464)) ;
#126506 = CARTESIAN_POINT('Ctrl Pts',(-30.4333260025628,14.1367618967332,
126.797892231372)) ;
#126507 = CARTESIAN_POINT('Ctrl Pts',(-30.3928708035435,13.8680692745211,
126.646669018808)) ;
#126508 = CARTESIAN_POINT('Ctrl Pts',(-30.3772964122241,13.5652241802336,
126.567869881532)) ;
#126509 = CARTESIAN_POINT('Ctrl Pts',(-30.3884947265944,13.2558695648544,
126.567689426035)) ;
#126510 = CARTESIAN_POINT('Ctrl Pts',(-30.4264241019016,12.9557645621013,
126.645297590501)) ;
#126511 = CARTESIAN_POINT('Ctrl Pts',(-30.489041829683,12.6900041384903,126.795125628811)) ;
#126512 = CARTESIAN_POINT('Ctrl Pts',(-30.5727955453991,12.4761054960812,
127.006609410694)) ;
#126513 = CARTESIAN_POINT('Ctrl Pts',(-30.6723385952662,12.330458638013,127.264220196088)) ;
#126514 = CARTESIAN_POINT('Ctrl Pts',(-30.7805975050551,12.2634381555471,
127.547468405064)) ;
#126515 = CARTESIAN_POINT('Ctrl Pts',(-30.8914731168471,12.2788783725225,
127.838251911419)) ;
#126516 = CARTESIAN_POINT('Ctrl Pts',(-30.997731735831,12.3768660101259,128.115439269918)) ;
#126517 = CARTESIAN_POINT('Ctrl Pts',(-31.0918372330593,12.5495630530058,
128.357227024484)) ;
#126518 = CARTESIAN_POINT('Ctrl Pts',(-31.1682535327665,12.7855771799242,
128.547247795842)) ;
#126519 = CARTESIAN_POINT('Ctrl Pts',(-31.2216790671275,13.0654345443907,
128.67033565722)) ;
#126520 = CARTESIAN_POINT('Ctrl Pts',(-31.249754075546,13.3720089515071,128.719222227115)) ;
#126521 = CARTESIAN_POINT('Ctrl Pts',(-31.2507732919044,13.6824357040732,
128.689053740515)) ;
#126522 = CARTESIAN_POINT('Ctrl Pts',(-31.2255503193694,13.9739144872618,
128.582277192005)) ;
#126523 = CARTESIAN_POINT('Ctrl Pts',(-31.1762431065979,14.2268633761364,
128.404991190371)) ;
#126524 = CARTESIAN_POINT('Ctrl Pts',(-31.1080584867575,14.4204385567601,
128.172885282172)) ;
#126525 = CARTESIAN_POINT('Ctrl Pts',(-31.0249588173677,14.5445800980489,
127.896763573076)) ;
#126526 = CARTESIAN_POINT('Ctrl Pts',(-30.9354496148306,14.5868220517618,
127.602269386102)) ;
#126527 = CARTESIAN_POINT('Ctrl Pts',(-30.8458602695974,14.5468039115563,
127.307542979927)) ;
#126528 = CARTESIAN_POINT('Ctrl Pts',(-30.762551181364,14.4251034056979,127.030856610899)) ;
#126529 = CARTESIAN_POINT('Ctrl Pts',(-30.6937022254225,14.2325286559051,
126.796691431518)) ;
#126530 = CARTESIAN_POINT('Ctrl Pts',(-30.6440265776777,13.9823226082249,
126.618508827956)) ;
#126531 = CARTESIAN_POINT('Ctrl Pts',(-30.6179403580397,13.6900857614276,
126.509023742768)) ;
#126532 = CARTESIAN_POINT('Ctrl Pts',(-30.6182858076127,13.3811329933267,
126.4770263894)) ;
#126533 = CARTESIAN_POINT('Ctrl Pts',(-30.6454939352929,13.0742211924304,
126.523392436635)) ;
#126534 = CARTESIAN_POINT('Ctrl Pts',(-30.6984799823791,12.7922255681548,
126.645059926506)) ;
#126535 = CARTESIAN_POINT('Ctrl Pts',(-30.7743696130924,12.5548593941868,
126.833548883208)) ;
#126536 = CARTESIAN_POINT('Ctrl Pts',(-30.8681675859231,12.3804086208566,
127.074416612223)) ;
#126537 = CARTESIAN_POINT('Ctrl Pts',(-30.9734327320213,12.2809059673708,
127.348936065361)) ;
#126538 = CARTESIAN_POINT('Ctrl Pts',(-31.0843011975214,12.2624888540407,
127.639685234248)) ;
#126539 = CARTESIAN_POINT('Ctrl Pts',(-31.1933595883704,12.3276777325191,
127.925074837892)) ;
#126540 = CARTESIAN_POINT('Ctrl Pts',(-31.2928028436846,12.4707929525642,
128.182534472415)) ;
#126541 = CARTESIAN_POINT('Ctrl Pts',(-31.3770533192461,12.6823314867526,
128.395518029563)) ;
#126542 = CARTESIAN_POINT('Ctrl Pts',(-31.4405599270799,12.9478032750239,
128.547819525315)) ;
#126543 = CARTESIAN_POINT('Ctrl Pts',(-31.4792159130957,13.2466924677811,
128.627614460685)) ;
#126544 = CARTESIAN_POINT('Ctrl Pts',(-31.4911477632263,13.5583773879723,
128.629318254641)) ;
#126545 = CARTESIAN_POINT('Ctrl Pts',(-31.4763826013898,13.8592557726353,
128.553168178792)) ;
#126546 = CARTESIAN_POINT('Ctrl Pts',(-31.4363656825528,14.1306426193177,
128.403029564233)) ;
#126547 = CARTESIAN_POINT('Ctrl Pts',(-31.3753860029681,14.3493760513521,
128.191947439307)) ;
#126548 = CARTESIAN_POINT('Ctrl Pts',(-31.2975897155965,14.5035317935641,
127.93146804733)) ;
#126549 = CARTESIAN_POINT('Ctrl Pts',(-31.2099294270891,14.5795845166173,
127.642277005627)) ;
#126550 = CARTESIAN_POINT('Ctrl Pts',(-31.119205465658,14.5729335427119,127.344118226607)) ;
#126551 = CARTESIAN_POINT('Ctrl Pts',(-31.0326800003559,14.4838964505683,
127.058232114227)) ;
#126552 = CARTESIAN_POINT('Ctrl Pts',(-30.9572247193135,14.3187457002778,
126.804663885965)) ;
#126553 = CARTESIAN_POINT('Ctrl Pts',(-30.8991368803147,14.0897675242826,
126.601886443905)) ;
#126554 = CARTESIAN_POINT('Ctrl Pts',(-30.8630850303705,13.8134082052382,
126.463502880507)) ;
#126555 = CARTESIAN_POINT('Ctrl Pts',(-30.8524556689723,13.5073935686165,
126.399199801176)) ;
#126556 = CARTESIAN_POINT('Ctrl Pts',(-30.8687507658311,13.1976576575877,
126.413804359631)) ;
#126557 = CARTESIAN_POINT('Ctrl Pts',(-30.9114804240192,12.902722923634,126.505492871026)) ;
#126558 = CARTESIAN_POINT('Ctrl Pts',(-30.9786025123769,12.6448108187769,
126.668379584555)) ;
#126559 = CARTESIAN_POINT('Ctrl Pts',(-31.0654092817325,12.4434495534872,
126.888919406482)) ;
#126560 = CARTESIAN_POINT('Ctrl Pts',(-31.1676204617471,12.3113759719957,
127.154188555509)) ;
#126561 = CARTESIAN_POINT('Ctrl Pts',(-31.2766504169667,12.2599503304337,
127.439757637193)) ;
#126562 = CARTESIAN_POINT('Ctrl Pts',(-31.3875029822561,12.291369325937,127.730360541563)) ;
#126563 = CARTESIAN_POINT('Ctrl Pts',(-31.4915349615509,12.4038516063155,
128.00120069853)) ;
#126564 = CARTESIAN_POINT('Ctrl Pts',(-31.5827029401584,12.5892626492753,
128.23441173148)) ;
#126565 = CARTESIAN_POINT('Ctrl Pts',(-31.6550420442372,12.8342966688913,
128.412632130978)) ;
#126566 = CARTESIAN_POINT('Ctrl Pts',(-31.7042037977048,13.122430564087,128.523040487345)) ;
#126567 = CARTESIAN_POINT('Ctrl Pts',(-31.7271063430556,13.4307504301952,
128.55689464633)) ;
#126568 = CARTESIAN_POINT('Ctrl Pts',(-31.7231059517512,13.7394115406098,
128.512058436927)) ;
#126569 = CARTESIAN_POINT('Ctrl Pts',(-31.6930932489722,14.0250582572476,
128.391271941973)) ;
#126570 = CARTESIAN_POINT('Ctrl Pts',(-31.6400121197202,14.2676857637035,
128.203093777817)) ;
#126571 = CARTESIAN_POINT('Ctrl Pts',(-31.5681740871473,14.4501343866895,
127.960050172645)) ;
#126572 = CARTESIAN_POINT('Ctrl Pts',(-31.4837806638188,14.5585281733049,
127.680404650567)) ;
#126573 = CARTESIAN_POINT('Ctrl Pts',(-31.393485187641,14.5857500263022,127.383523473882)) ;
#126574 = CARTESIAN_POINT('Ctrl Pts',(-31.3042926382178,14.5296138137444,
127.089807373214)) ;
#126575 = CARTESIAN_POINT('Ctrl Pts',(-31.2235650511201,14.3940563365778,
126.820842233824)) ;
#126576 = CARTESIAN_POINT('Ctrl Pts',(-31.157899893824,14.1896705870724,126.595977084309)) ;
#126577 = CARTESIAN_POINT('Ctrl Pts',(-31.112275041275,13.929679500594,126.42953375103)) ;
#126578 = CARTESIAN_POINT('Ctrl Pts',(-31.0910923977529,13.6325613008054,
126.334421909125)) ;
#126579 = CARTESIAN_POINT('Ctrl Pts',(-31.0964447394053,13.3229079041448,
126.31709545029)) ;
#126580 = CARTESIAN_POINT('Ctrl Pts',(-31.1286944233721,13.0185266052724,
126.378131100081)) ;
#126581 = CARTESIAN_POINT('Ctrl Pts',(-31.1861978833459,12.7436673209471,
126.513013327565)) ;
#126582 = CARTESIAN_POINT('Ctrl Pts',(-31.2661117501715,12.5164978313935,
126.713179834526)) ;
#126583 = CARTESIAN_POINT('Ctrl Pts',(-31.3620916624292,12.3560839841268,
126.960609857562)) ;
#126584 = CARTESIAN_POINT('Ctrl Pts',(-31.4694894479972,12.2708854639731,
127.241159005647)) ;
#126585 = CARTESIAN_POINT('Ctrl Pts',(-31.5802782657031,12.2685612257957,
127.531751335238)) ;
#126586 = CARTESIAN_POINT('Ctrl Pts',(-31.6879941774975,12.3486010166685,
127.813276464684)) ;
#126587 = CARTESIAN_POINT('Ctrl Pts',(-31.7856635186791,12.5069431442139,
128.065300796062)) ;
#126588 = CARTESIAN_POINT('Ctrl Pts',(-31.8657144711242,12.7284060361604,
128.266254738305)) ;
#126589 = CARTESIAN_POINT('Ctrl Pts',(-31.9250227559616,13.0024846524795,
128.406199840165)) ;
#126590 = CARTESIAN_POINT('Ctrl Pts',(-31.95863385165,13.3053157268251,128.471280232653)) ;
#126591 = CARTESIAN_POINT('Ctrl Pts',(-31.9654947472056,13.6156287863426,
128.458302913958)) ;
#126592 = CARTESIAN_POINT('Ctrl Pts',(-31.9458820818508,13.9128850712382,
128.367926847057)) ;
#126593 = CARTESIAN_POINT('Ctrl Pts',(-31.9014415972457,14.1766185876755,
128.204813826453)) ;
#126594 = CARTESIAN_POINT('Ctrl Pts',(-31.8365595302308,14.3847399014371,
127.982162035615)) ;
#126595 = CARTESIAN_POINT('Ctrl Pts',(-31.7568066659652,14.5238361204557,
127.716174800887)) ;
#126596 = CARTESIAN_POINT('Ctrl Pts',(-31.6680261972628,14.5847743037998,
127.423702490199)) ;
#126597 = CARTESIAN_POINT('Ctrl Pts',(-31.5774936879742,14.562330930931,127.126086462082)) ;
#126598 = CARTESIAN_POINT('Ctrl Pts',(-31.4925141748482,14.4584177990408,
126.844713248296)) ;
#126599 = CARTESIAN_POINT('Ctrl Pts',(-31.4196806977938,14.2791868588028,
126.59868079849)) ;
#126600 = CARTESIAN_POINT('Ctrl Pts',(-31.365769806941,14.0415186925473,126.408335160599)) ;
#126601 = CARTESIAN_POINT('Ctrl Pts',(-31.3341067123459,13.7564325224017,
126.28254734767)) ;
#126602 = CARTESIAN_POINT('Ctrl Pts',(-31.3285693219295,13.4495648486799,
126.233344992335)) ;
#126603 = CARTESIAN_POINT('Ctrl Pts',(-31.3499996979768,13.1394167822153,
126.262757635103)) ;
#126604 = CARTESIAN_POINT('Ctrl Pts',(-31.3974714496979,12.8508801279426,
126.368398084406)) ;
#126605 = CARTESIAN_POINT('Ctrl Pts',(-31.4686226776466,12.6022770183791,
126.543082974062)) ;
#126606 = CARTESIAN_POINT('Ctrl Pts',(-31.5588216270401,12.4127865792607,
126.773465057354)) ;
#126607 = CARTESIAN_POINT('Ctrl Pts',(-31.662947243727,12.2953916608247,127.044370815528)) ;
#126608 = CARTESIAN_POINT('Ctrl Pts',(-31.7729256743816,12.2594835078991,
127.332640515269)) ;
#126609 = CARTESIAN_POINT('Ctrl Pts',(-31.8827463763512,12.3065006928956,
127.620343819185)) ;
#126610 = CARTESIAN_POINT('Ctrl Pts',(-31.984917749441,12.4331949975966,127.8857354975)) ;
#126611 = CARTESIAN_POINT('Ctrl Pts',(-32.0734252963866,12.6325251245457,
128.110965015092)) ;
#126612 = CARTESIAN_POINT('Ctrl Pts',(-32.1411877862138,12.8854154202419,
128.276032660269)) ;
#126613 = CARTESIAN_POINT('Ctrl Pts',(-32.185775956454,13.1803567120122,128.37294829569)) ;
#126614 = CARTESIAN_POINT('Ctrl Pts',(-32.2034899901905,13.4893561619414,
128.391747881859)) ;
#126615 = CARTESIAN_POINT('Ctrl Pts',(-32.1945262955173,13.7954471105094,
128.33241062473)) ;
#126616 = CARTESIAN_POINT('Ctrl Pts',(-32.1597610137556,14.0751705649909,
128.197652005603)) ;
#126617 = CARTESIAN_POINT('Ctrl Pts',(-32.102880816017,14.3069080842483,127.998454341013)) ;
#126618 = CARTESIAN_POINT('Ctrl Pts',(-32.0283825626093,14.4762413340772,
127.747712728677)) ;
#126619 = CARTESIAN_POINT('Ctrl Pts',(-31.9418077598481,14.5702449830263,
127.461492883282)) ;
#126620 = CARTESIAN_POINT('Ctrl Pts',(-31.8514803012559,14.5813885604022,
127.16462576914)) ;
#126621 = CARTESIAN_POINT('Ctrl Pts',(-31.7634476739157,14.5100796553899,
126.874340511653)) ;
#126622 = CARTESIAN_POINT('Ctrl Pts',(-31.6848485468524,14.3602444697485,
126.611517403404)) ;
#126623 = CARTESIAN_POINT('Ctrl Pts',(-31.6225173073783,14.1432531479422,
126.396278974897)) ;
#126624 = CARTESIAN_POINT('Ctrl Pts',(-31.5815599114105,13.8766589305714,
126.243700317679)) ;
#126625 = CARTESIAN_POINT('Ctrl Pts',(-31.5651586334022,13.575471110015,126.162588536627)) ;
#126626 = CARTESIAN_POINT('Ctrl Pts',(-31.5755523169396,13.2645667872771,
126.159895817134)) ;
#126627 = CARTESIAN_POINT('Ctrl Pts',(-31.6128773468518,12.9634276879521,
126.235689544571)) ;
#126628 = CARTESIAN_POINT('Ctrl Pts',(-31.6746702091294,12.6972348288673,
126.383202615797)) ;
#126629 = CARTESIAN_POINT('Ctrl Pts',(-31.7577635170574,12.4817230037899,
126.592791547872)) ;
#126630 = CARTESIAN_POINT('Ctrl Pts',(-31.8568476398735,12.3338051645045,
126.849080745658)) ;
#126631 = CARTESIAN_POINT('Ctrl Pts',(-31.9652781019356,12.2641455947444,
127.132724501552)) ;
#126632 = CARTESIAN_POINT('Ctrl Pts',(-32.0761113464017,12.2773535863406,
127.423406237724)) ;
#126633 = CARTESIAN_POINT('Ctrl Pts',(-32.1823624472709,12.3726335000392,
127.700655595375)) ;
#126634 = CARTESIAN_POINT('Ctrl Pts',(-32.2770427894398,12.5434758841393,
127.944074783812)) ;
#126635 = CARTESIAN_POINT('Ctrl Pts',(-32.3538549195629,12.7769498129424,
128.135364285058)) ;
#126636 = CARTESIAN_POINT('Ctrl Pts',(-32.4083145195709,13.0568800238177,
128.261324343271)) ;
#126637 = CARTESIAN_POINT('Ctrl Pts',(-32.4371265032857,13.3636449854545,
128.312303479849)) ;
#126638 = CARTESIAN_POINT('Ctrl Pts',(-32.4388913807184,13.6733774781512,
128.28440725804)) ;
#126639 = CARTESIAN_POINT('Ctrl Pts',(-32.4144856546222,13.9654381108949,
128.180052252876)) ;
#126640 = CARTESIAN_POINT('Ctrl Pts',(-32.3657873055419,14.2203012801684,
128.004497044474)) ;
#126641 = CARTESIAN_POINT('Ctrl Pts',(-32.2979066090449,14.4159470499748,
127.773210152946)) ;
#126642 = CARTESIAN_POINT('Ctrl Pts',(-32.2156445726619,14.541694367896,127.499738746105)) ;
#126643 = CARTESIAN_POINT('Ctrl Pts',(-32.1258917680055,14.5869018897487,
127.204394863701)) ;
#126644 = CARTESIAN_POINT('Ctrl Pts',(-32.0360732595204,14.5489491309812,
126.908948138677)) ;
#126645 = CARTESIAN_POINT('Ctrl Pts',(-31.9527424544331,14.4300240468882,
126.632315927122)) ;
#126646 = CARTESIAN_POINT('Ctrl Pts',(-31.8831245966444,14.2387296194583,
126.395780395041)) ;
#126647 = CARTESIAN_POINT('Ctrl Pts',(-31.8329411061117,13.9899468992174,
126.216137846651)) ;
#126648 = CARTESIAN_POINT('Ctrl Pts',(-31.8062039119009,13.7002922296482,
126.10493343788)) ;
#126649 = CARTESIAN_POINT('Ctrl Pts',(-31.8055981139312,13.3909003011237,
126.070079831623)) ;
#126650 = CARTESIAN_POINT('Ctrl Pts',(-31.8322241901464,13.0819914193172,
126.114572771983)) ;
#126651 = CARTESIAN_POINT('Ctrl Pts',(-31.8843911764362,12.8000707089261,
126.233963093376)) ;
#126652 = CARTESIAN_POINT('Ctrl Pts',(-31.959405494078,12.561613461146,126.419982896461)) ;
#126653 = CARTESIAN_POINT('Ctrl Pts',(-32.0529214736794,12.3844498728761,
126.659951432733)) ;
#126654 = CARTESIAN_POINT('Ctrl Pts',(-32.1584695989366,12.2824628123426,
126.935138173326)) ;
#126655 = CARTESIAN_POINT('Ctrl Pts',(-32.2687092503971,12.2618989630133,
127.224226185651)) ;
#126656 = CARTESIAN_POINT('Ctrl Pts',(-32.3780664721287,12.3245801672036,
127.510447715042)) ;
#126657 = CARTESIAN_POINT('Ctrl Pts',(-32.4778727214042,12.4655890286878,
127.768967737361)) ;
#126658 = CARTESIAN_POINT('Ctrl Pts',(-32.562635692592,12.6753258983896,127.983450429838)) ;
#126659 = CARTESIAN_POINT('Ctrl Pts',(-32.6267495393494,12.9389696147355,
128.137585318208)) ;
#126660 = CARTESIAN_POINT('Ctrl Pts',(-32.6662243013269,13.2377442398154,
128.219703177418)) ;
#126661 = CARTESIAN_POINT('Ctrl Pts',(-32.6789869482266,13.5478078732814,
128.224005737763)) ;
#126662 = CARTESIAN_POINT('Ctrl Pts',(-32.6649289811142,13.8515136096922,
128.149675334215)) ;
#126663 = CARTESIAN_POINT('Ctrl Pts',(-32.6256750103247,14.1231097969316,
128.001882287398)) ;
#126664 = CARTESIAN_POINT('Ctrl Pts',(-32.5651689894839,14.3439547255393,
127.792123518752)) ;
#126665 = CARTESIAN_POINT('Ctrl Pts',(-32.4879714740893,14.4998917409251,
127.533482233047)) ;
#126666 = CARTESIAN_POINT('Ctrl Pts',(-32.400211067042,14.5786386561727,127.243881113999)) ;
#126667 = CARTESIAN_POINT('Ctrl Pts',(-32.3095247060737,14.574267489829,126.945855302846)) ;
#126668 = CARTESIAN_POINT('Ctrl Pts',(-32.2227184803242,14.4873446647109,
126.65911777222)) ;
#126669 = CARTESIAN_POINT('Ctrl Pts',(-32.1471010239481,14.3247913257021,
126.405185591465)) ;
#126670 = CARTESIAN_POINT('Ctrl Pts',(-32.0882333339096,14.0970301472897,
126.200046528919)) ;
#126671 = CARTESIAN_POINT('Ctrl Pts',(-32.0514651201517,13.820492300365,126.059438557222)) ;
#126672 = CARTESIAN_POINT('Ctrl Pts',(-32.0401940508131,13.5164548784845,
125.993426980055)) ;
#126673 = CARTESIAN_POINT('Ctrl Pts',(-32.0557122282716,13.2060699162722,
126.00570482415)) ;
#126674 = CARTESIAN_POINT('Ctrl Pts',(-32.0977788098025,12.9102232065258,
126.095437968778)) ;
#126675 = CARTESIAN_POINT('Ctrl Pts',(-32.1644236899613,12.6507291243944,
126.25688138731)) ;
#126676 = CARTESIAN_POINT('Ctrl Pts',(-32.2504533776306,12.4485585440169,
126.475276109183)) ;
#126677 = CARTESIAN_POINT('Ctrl Pts',(-32.3517721832678,12.3145373722517,
126.738100326614)) ;
#126678 = CARTESIAN_POINT('Ctrl Pts',(-32.4612996077681,12.2601564021124,
127.024927652369)) ;
#126679 = CARTESIAN_POINT('Ctrl Pts',(-32.572190253351,12.2893926148143,127.315652329271)) ;
#126680 = CARTESIAN_POINT('Ctrl Pts',(-32.6764790046662,12.3994366791386,
127.587256135716)) ;
#126681 = CARTESIAN_POINT('Ctrl Pts',(-32.7684650814352,12.5839727255082,
127.822707706638)) ;
#126682 = CARTESIAN_POINT('Ctrl Pts',(-32.841004593203,12.8264920327129,128.001671494392)) ;
#126683 = CARTESIAN_POINT('Ctrl Pts',(-32.8910099340424,13.1141225858941,
128.11449164118)) ;
#126684 = CARTESIAN_POINT('Ctrl Pts',(-32.9067217529341,13.3194871424456,
128.138350053268)) ;
#126685 = CARTESIAN_POINT('Ctrl Pts',(-32.9101349058941,13.4222384841719,
128.137300004128)) ;
#126686 = CARTESIAN_POINT('Ctrl Pts',(-11.3289906305328,13.1368456608817,
133.132150944256)) ;
#126687 = CARTESIAN_POINT('Ctrl Pts',(-11.3297648820373,13.1302434176427,
133.133681768478)) ;
#126688 = CARTESIAN_POINT('Ctrl Pts',(-11.3423989273914,13.0249710001428,
133.158906544104)) ;
#126689 = CARTESIAN_POINT('Ctrl Pts',(-11.3769158459995,12.826301888656,133.236764259813)) ;
#126690 = CARTESIAN_POINT('Ctrl Pts',(-11.4497170247885,12.5833995163819,
133.416412389735)) ;
#126691 = CARTESIAN_POINT('Ctrl Pts',(-11.5412607886117,12.3996267668574,
133.650728855637)) ;
#126692 = CARTESIAN_POINT('Ctrl Pts',(-11.646261583587,12.289073168245,133.924189213627)) ;
#126693 = CARTESIAN_POINT('Ctrl Pts',(-11.756222160173,12.2602312941192,134.21248261213)) ;
#126694 = CARTESIAN_POINT('Ctrl Pts',(-11.8660584839532,12.3144254424815,
134.500116213875)) ;
#126695 = CARTESIAN_POINT('Ctrl Pts',(-11.9672384530468,12.4480642715863,
134.762596430137)) ;
#126696 = CARTESIAN_POINT('Ctrl Pts',(-12.0538295019936,12.6516399513856,
134.982407105695)) ;
#126697 = CARTESIAN_POINT('Ctrl Pts',(-12.1201383915298,12.9104452496318,
135.142988694336)) ;
#126698 = CARTESIAN_POINT('Ctrl Pts',(-12.1621810540703,13.2058492015505,
135.232691768976)) ;
#126699 = CARTESIAN_POINT('Ctrl Pts',(-12.1777749644098,13.5166184921212,
135.245154976188)) ;
#126700 = CARTESIAN_POINT('Ctrl Pts',(-12.1662881003302,13.8224100223415,
135.178309260546)) ;
#126701 = CARTESIAN_POINT('Ctrl Pts',(-12.1296615754862,14.0967865008827,
135.038352263151)) ;
#126702 = CARTESIAN_POINT('Ctrl Pts',(-12.0709572339323,14.3244562986112,
134.833732882778)) ;
#126703 = CARTESIAN_POINT('Ctrl Pts',(-11.9951612200146,14.4874741997871,
134.579198900516)) ;
#126704 = CARTESIAN_POINT('Ctrl Pts',(-11.9081860961099,14.5744204937736,
134.291910355936)) ;
#126705 = CARTESIAN_POINT('Ctrl Pts',(-11.8174705117483,14.5784621737365,
133.993787488894)) ;
#126706 = CARTESIAN_POINT('Ctrl Pts',(-11.7301428372465,14.5000469778991,
133.705611198596)) ;
#126707 = CARTESIAN_POINT('Ctrl Pts',(-11.6529450720055,14.3445727249932,
133.446993574372)) ;
#126708 = CARTESIAN_POINT('Ctrl Pts',(-11.5921201640469,14.122833835347,133.236157417965)) ;
#126709 = CARTESIAN_POINT('Ctrl Pts',(-11.5529082022929,13.8501516984393,
133.088384911782)) ;
#126710 = CARTESIAN_POINT('Ctrl Pts',(-11.5389594641307,13.5490423779197,
133.014658231721)) ;
#126711 = CARTESIAN_POINT('Ctrl Pts',(-11.5516658542996,13.2374717045801,
133.018634830279)) ;
#126712 = CARTESIAN_POINT('Ctrl Pts',(-11.5912618190877,12.9386844676289,
133.101096607348)) ;
#126713 = CARTESIAN_POINT('Ctrl Pts',(-11.6550459597695,12.6761377246457,
133.254414846195)) ;
#126714 = CARTESIAN_POINT('Ctrl Pts',(-11.739911901217,12.4657586790897,133.469131818159)) ;
#126715 = CARTESIAN_POINT('Ctrl Pts',(-11.8398105621753,12.3246285674056,
133.727893177096)) ;
#126716 = CARTESIAN_POINT('Ctrl Pts',(-11.9491259530435,12.2619062239342,
134.014003245861)) ;
#126717 = CARTESIAN_POINT('Ctrl Pts',(-12.0595466130642,12.282438835861,134.303567791795)) ;
#126718 = CARTESIAN_POINT('Ctrl Pts',(-12.1652800488837,12.3848777571664,
134.579229631052)) ;
#126719 = CARTESIAN_POINT('Ctrl Pts',(-12.2583983620761,12.5614991790326,
134.818162626115)) ;
#126720 = CARTESIAN_POINT('Ctrl Pts',(-12.3334889598739,12.7995868191894,
135.004422494166)) ;
#126721 = CARTESIAN_POINT('Ctrl Pts',(-12.3859540985011,13.084029998422,135.124408150865)) ;
#126722 = CARTESIAN_POINT('Ctrl Pts',(-12.4122116510868,13.3899587273314,
135.168153572099)) ;
#126723 = CARTESIAN_POINT('Ctrl Pts',(-12.4117844343827,13.6996411393276,
135.133791161841)) ;
#126724 = CARTESIAN_POINT('Ctrl Pts',(-12.3849432646615,13.9903747350237,
135.022164919903)) ;
#126725 = CARTESIAN_POINT('Ctrl Pts',(-12.3346188008902,14.2393240390192,
134.842065868188)) ;
#126726 = CARTESIAN_POINT('Ctrl Pts',(-12.2651915907767,14.429840029191,134.606193033354)) ;
#126727 = CARTESIAN_POINT('Ctrl Pts',(-12.1821120354275,14.5487685207819,
134.330379497108)) ;
#126728 = CARTESIAN_POINT('Ctrl Pts',(-12.0919098184049,14.5869290462078,
134.033669627662)) ;
#126729 = CARTESIAN_POINT('Ctrl Pts',(-12.0024629512785,14.5417666879112,
133.739329945311)) ;
#126730 = CARTESIAN_POINT('Ctrl Pts',(-11.920119663901,14.4163781206347,133.46561377521)) ;
#126731 = CARTESIAN_POINT('Ctrl Pts',(-11.8519259373826,14.2194053236093,
133.233226952296)) ;
#126732 = CARTESIAN_POINT('Ctrl Pts',(-11.8036364484147,13.9666437025949,
133.059143893317)) ;
#126733 = CARTESIAN_POINT('Ctrl Pts',(-11.7789832629656,13.6737230311142,
132.953945062575)) ;
#126734 = CARTESIAN_POINT('Ctrl Pts',(-11.7808284718151,13.3629183159293,
132.926175916698)) ;
#126735 = CARTESIAN_POINT('Ctrl Pts',(-11.8096149856141,13.0570541461369,
132.977171113818)) ;
#126736 = CARTESIAN_POINT('Ctrl Pts',(-11.8639395888902,12.7772474401736,
133.102769292852)) ;
#126737 = CARTESIAN_POINT('Ctrl Pts',(-11.9411870980062,12.542768054334,133.295164838442)) ;
#126738 = CARTESIAN_POINT('Ctrl Pts',(-12.0353149573993,12.3730788461159,
133.537173788383)) ;
#126739 = CARTESIAN_POINT('Ctrl Pts',(-12.1416212392354,12.2773830517675,
133.814552713987)) ;
#126740 = CARTESIAN_POINT('Ctrl Pts',(-12.2525579395139,12.2641121727855,
134.105508450141)) ;
#126741 = CARTESIAN_POINT('Ctrl Pts',(-12.3609993187246,12.3337583329821,
134.389180372102)) ;
#126742 = CARTESIAN_POINT('Ctrl Pts',(-12.4599209105406,12.4813160749921,
134.645053011495)) ;
#126743 = CARTESIAN_POINT('Ctrl Pts',(-12.5431324196802,12.6966779854676,
134.854974313712)) ;
#126744 = CARTESIAN_POINT('Ctrl Pts',(-12.60513159688,12.964058481658,135.002951427607)) ;
#126745 = CARTESIAN_POINT('Ctrl Pts',(-12.642248673285,13.2633621106785,135.078341105324)) ;
#126746 = CARTESIAN_POINT('Ctrl Pts',(-12.6527915834591,13.5752568041736,
135.075975212479)) ;
#126747 = CARTESIAN_POINT('Ctrl Pts',(-12.6363641393793,13.8766502651513,
134.994767154178)) ;
#126748 = CARTESIAN_POINT('Ctrl Pts',(-12.5953057530699,14.1438626179913,
134.841815741776)) ;
#126749 = CARTESIAN_POINT('Ctrl Pts',(-12.5327277376817,14.3611558339141,
134.625772535533)) ;
#126750 = CARTESIAN_POINT('Ctrl Pts',(-12.454244121328,14.5102070990302,134.363363036415)) ;
#126751 = CARTESIAN_POINT('Ctrl Pts',(-12.3666258464247,14.5813677878946,
134.074440573705)) ;
#126752 = CARTESIAN_POINT('Ctrl Pts',(-12.2757841730223,14.5701315008181,
133.775881282886)) ;
#126753 = CARTESIAN_POINT('Ctrl Pts',(-12.1894313961296,14.4759919036324,
133.490385986915)) ;
#126754 = CARTESIAN_POINT('Ctrl Pts',(-12.114965878112,14.3066892752371,133.239748050331)) ;
#126755 = CARTESIAN_POINT('Ctrl Pts',(-12.0581822625266,14.0751878826871,
133.040876769225)) ;
#126756 = CARTESIAN_POINT('Ctrl Pts',(-12.0234738677265,13.7962286869884,
132.906363788813)) ;
#126757 = CARTESIAN_POINT('Ctrl Pts',(-12.0143364764407,13.4897393053989,
132.846474596732)) ;
#126758 = CARTESIAN_POINT('Ctrl Pts',(-12.0324237013593,13.1781056984616,
132.866070228703)) ;
#126759 = CARTESIAN_POINT('Ctrl Pts',(-12.076404053086,12.8871394706553,132.961667742337)) ;
#126760 = CARTESIAN_POINT('Ctrl Pts',(-12.144800910124,12.6313543123433,133.128229561128)) ;
#126761 = CARTESIAN_POINT('Ctrl Pts',(-12.2330625930333,12.4333423882355,
133.352887813321)) ;
#126762 = CARTESIAN_POINT('Ctrl Pts',(-12.3347905478153,12.3067788270204,
133.617104693997)) ;
#126763 = CARTESIAN_POINT('Ctrl Pts',(-12.4451693867627,12.2592790115486,
133.906271890683)) ;
#126764 = CARTESIAN_POINT('Ctrl Pts',(-12.555523569585,12.2958890743791,134.195519227349)) ;
#126765 = CARTESIAN_POINT('Ctrl Pts',(-12.6588209278628,12.412515962942,134.464262947306)) ;
#126766 = CARTESIAN_POINT('Ctrl Pts',(-12.7491570807097,12.6017795206287,
134.695024073182)) ;
#126767 = CARTESIAN_POINT('Ctrl Pts',(-12.8204405039154,12.850882040149,134.870032322403)) ;
#126768 = CARTESIAN_POINT('Ctrl Pts',(-12.8678707015775,13.1389626258658,
134.975599031413)) ;
#126769 = CARTESIAN_POINT('Ctrl Pts',(-12.8894078132323,13.4502019142914,
135.005209681357)) ;
#126770 = CARTESIAN_POINT('Ctrl Pts',(-12.8836925621681,13.7571545177325,
134.955462993416)) ;
#126771 = CARTESIAN_POINT('Ctrl Pts',(-12.8524412071742,14.0399279671086,
134.831176385702)) ;
#126772 = CARTESIAN_POINT('Ctrl Pts',(-12.7978983539385,14.2804627439869,
134.638584865143)) ;
#126773 = CARTESIAN_POINT('Ctrl Pts',(-12.7255120770098,14.4580430421026,
134.394109587671)) ;
#126774 = CARTESIAN_POINT('Ctrl Pts',(-12.6404688487952,14.5623041816762,
134.112503175951)) ;
#126775 = CARTESIAN_POINT('Ctrl Pts',(-12.5501362245032,14.5848738304735,
133.815550736798)) ;
#126776 = CARTESIAN_POINT('Ctrl Pts',(-12.4608432203707,14.5236285286568,
133.521387838919)) ;
#126777 = CARTESIAN_POINT('Ctrl Pts',(-12.3811865324715,14.3842858734187,
133.255704176636)) ;
#126778 = CARTESIAN_POINT('Ctrl Pts',(-12.316331454127,14.176003666528,133.03312326242)) ;
#126779 = CARTESIAN_POINT('Ctrl Pts',(-12.2719898795752,13.9123645540699,
132.870327548437)) ;
#126780 = CARTESIAN_POINT('Ctrl Pts',(-12.2524288688057,13.6155079184588,
132.780146867289)) ;
#126781 = CARTESIAN_POINT('Ctrl Pts',(-12.25927523216,13.3048786639477,132.767097369268)) ;
#126782 = CARTESIAN_POINT('Ctrl Pts',(-12.2931239866176,13.0013158611206,
132.832775546198)) ;
#126783 = CARTESIAN_POINT('Ctrl Pts',(-12.3520199188583,12.7290184859203,
132.971741376215)) ;
#126784 = CARTESIAN_POINT('Ctrl Pts',(-12.4326782308627,12.5059453059748,
133.174220773356)) ;
#126785 = CARTESIAN_POINT('Ctrl Pts',(-12.5298337757618,12.3489356704195,
133.424945718245)) ;
#126786 = CARTESIAN_POINT('Ctrl Pts',(-12.6372704596358,12.2685725679141,
133.705726448417)) ;
#126787 = CARTESIAN_POINT('Ctrl Pts',(-12.7486620548609,12.2709800275436,
133.997898242284)) ;
#126788 = CARTESIAN_POINT('Ctrl Pts',(-12.8556718615591,12.3558597307768,
134.27743957292)) ;
#126789 = CARTESIAN_POINT('Ctrl Pts',(-12.9522002926599,12.5173148963124,
134.526272457561)) ;
#126790 = CARTESIAN_POINT('Ctrl Pts',(-13.0316720868523,12.7436533200346,
134.725305724518)) ;
#126791 = CARTESIAN_POINT('Ctrl Pts',(-13.0892034891378,13.018439069694,134.860265498941)) ;
#126792 = CARTESIAN_POINT('Ctrl Pts',(-13.1214679873254,13.3224259013371,
134.92138844405)) ;
#126793 = CARTESIAN_POINT('Ctrl Pts',(-13.1268138371495,13.6337496474671,
134.903863238124)) ;
#126794 = CARTESIAN_POINT('Ctrl Pts',(-13.1055776718622,13.9298381651934,
134.808697625528)) ;
#126795 = CARTESIAN_POINT('Ctrl Pts',(-13.0600986020032,14.1894306031692,
134.642744252233)) ;
#126796 = CARTESIAN_POINT('Ctrl Pts',(-12.9941851716164,14.3944757405405,
134.417037926002)) ;
#126797 = CARTESIAN_POINT('Ctrl Pts',(-12.913653884883,14.5294751420936,134.14873833919)) ;
#126798 = CARTESIAN_POINT('Ctrl Pts',(-12.8245776745816,14.5857784683659,
133.855399066771)) ;
#126799 = CARTESIAN_POINT('Ctrl Pts',(-12.7339951385361,14.5584757984426,
133.557575572516)) ;
#126800 = CARTESIAN_POINT('Ctrl Pts',(-12.6496676074224,14.4499269528594,
133.278138952637)) ;
#126801 = CARTESIAN_POINT('Ctrl Pts',(-12.5779591604913,14.2678362445854,
133.035534388741)) ;
#126802 = CARTESIAN_POINT('Ctrl Pts',(-12.524838740077,14.0251814638135,132.847230394118)) ;
#126803 = CARTESIAN_POINT('Ctrl Pts',(-12.4948320173684,13.7395989389894,
132.726468372843)) ;
#126804 = CARTESIAN_POINT('Ctrl Pts',(-12.4907942560101,13.4312396305714,
132.681553632489)) ;
#126805 = CARTESIAN_POINT('Ctrl Pts',(-12.5136927724239,13.122549732562,132.715357350964)) ;
#126806 = CARTESIAN_POINT('Ctrl Pts',(-12.5628394820659,12.8344723669187,
132.825729771799)) ;
#126807 = CARTESIAN_POINT('Ctrl Pts',(-12.6351603737995,12.5894057801397,
133.003896888117)) ;
#126808 = CARTESIAN_POINT('Ctrl Pts',(-12.7263460961529,12.403866957567,133.23714956194)) ;
#126809 = CARTESIAN_POINT('Ctrl Pts',(-12.8305084073274,12.2913271425025,
133.508330143151)) ;
#126810 = CARTESIAN_POINT('Ctrl Pts',(-12.9412562406573,12.2598830910493,
133.79866136084)) ;
#126811 = CARTESIAN_POINT('Ctrl Pts',(-13.0506666618133,12.3117248733074,
134.085220024184)) ;
#126812 = CARTESIAN_POINT('Ctrl Pts',(-13.1523540896968,12.443258179484,134.349126951551)) ;
#126813 = CARTESIAN_POINT('Ctrl Pts',(-13.2393089523663,12.6447768173015,
134.57005085132)) ;
#126814 = CARTESIAN_POINT('Ctrl Pts',(-13.3062792253377,12.9020426575426,
134.732576392011)) ;
#126815 = CARTESIAN_POINT('Ctrl Pts',(-13.3491121418991,13.1969220375029,
134.824559296309)) ;
#126816 = CARTESIAN_POINT('Ctrl Pts',(-13.3654831799169,13.5073633530841,
134.839313257053)) ;
#126817 = CARTESIAN_POINT('Ctrl Pts',(-13.3547961092594,13.8135027955519,
134.774821065349)) ;
#126818 = CARTESIAN_POINT('Ctrl Pts',(-13.3189348221119,14.0890634485619,
134.637107361757)) ;
#126819 = CARTESIAN_POINT('Ctrl Pts',(-13.2605232489219,14.3192684868255,
134.433199436081)) ;
#126820 = CARTESIAN_POINT('Ctrl Pts',(-13.1854056232735,14.4835637589644,
134.18077840894)) ;
#126821 = CARTESIAN_POINT('Ctrl Pts',(-13.0986713612669,14.5730188127273,
133.894189644553)) ;
#126822 = CARTESIAN_POINT('Ctrl Pts',(-13.0079469277613,14.57959678794,133.596037025184)) ;
#126823 = CARTESIAN_POINT('Ctrl Pts',(-12.9202452278553,14.5032854042053,
133.306694018913)) ;
#126824 = CARTESIAN_POINT('Ctrl Pts',(-12.8427351822991,14.3501151902807,
133.047206914589)) ;
#126825 = CARTESIAN_POINT('Ctrl Pts',(-12.7812157154848,14.1289952661381,
132.834210656053)) ;
#126826 = CARTESIAN_POINT('Ctrl Pts',(-12.7416423436877,13.8600884343622,
132.685694384841)) ;
#126827 = CARTESIAN_POINT('Ctrl Pts',(-12.7267166933267,13.5571076942101,
132.608832010303)) ;
#126828 = CARTESIAN_POINT('Ctrl Pts',(-12.7387853224196,13.2461441401465,
132.611016636209)) ;
#126829 = CARTESIAN_POINT('Ctrl Pts',(-12.7773913543468,12.9474784920459,
132.690690803401)) ;
#126830 = CARTESIAN_POINT('Ctrl Pts',(-12.8410763941597,12.6818050518092,
132.843463764725)) ;
#126831 = CARTESIAN_POINT('Ctrl Pts',(-12.9248214245163,12.4713262054323,
133.055159848696)) ;
#126832 = CARTESIAN_POINT('Ctrl Pts',(-13.0248439197258,12.3273775325765,
133.314112791871)) ;
#126833 = CARTESIAN_POINT('Ctrl Pts',(-13.1333865563481,12.2625380449618,
133.598161317782)) ;
#126834 = CARTESIAN_POINT('Ctrl Pts',(-13.2448375865862,12.2810707567545,
133.890430592819)) ;
#126835 = CARTESIAN_POINT('Ctrl Pts',(-13.349687874794,12.3803129183538,134.16387238493)) ;
#126836 = CARTESIAN_POINT('Ctrl Pts',(-13.4438403061782,12.5556239144648,
134.405630875818)) ;
#126837 = CARTESIAN_POINT('Ctrl Pts',(-13.5192481442775,12.7914917134663,
134.592929817305)) ;
#126838 = CARTESIAN_POINT('Ctrl Pts',(-13.5725537048544,13.0750409894439,
134.715337082379)) ;
#126839 = CARTESIAN_POINT('Ctrl Pts',(-13.5996147443617,13.3808908591526,
134.76139882389)) ;
#126840 = CARTESIAN_POINT('Ctrl Pts',(-13.5999442357729,13.6908804953288,
134.729236542822)) ;
#126841 = CARTESIAN_POINT('Ctrl Pts',(-13.5739291149334,13.9819858786258,
134.620089729232)) ;
#126842 = CARTESIAN_POINT('Ctrl Pts',(-13.5240931007593,14.2331023151693,
134.441318559943)) ;
#126843 = CARTESIAN_POINT('Ctrl Pts',(-13.4552207598495,14.4253737390559,
134.207104813219)) ;
#126844 = CARTESIAN_POINT('Ctrl Pts',(-13.3719137602938,14.5469025476726,
133.930428347931)) ;
#126845 = CARTESIAN_POINT('Ctrl Pts',(-13.2824137245965,14.5868798001592,
133.636000960324)) ;
#126846 = CARTESIAN_POINT('Ctrl Pts',(-13.1927395264543,14.5442430115436,
133.340951538328)) ;
#126847 = CARTESIAN_POINT('Ctrl Pts',(-13.1101849758616,14.4211466691175,
133.066658189192)) ;
#126848 = CARTESIAN_POINT('Ctrl Pts',(-13.0414901767957,14.2262607722871,
132.832818373534)) ;
#126849 = CARTESIAN_POINT('Ctrl Pts',(-12.9924622934676,13.9744157563079,
132.656514392088)) ;
#126850 = CARTESIAN_POINT('Ctrl Pts',(-12.9671460162565,13.6824770169396,
132.549398601363)) ;
#126851 = CARTESIAN_POINT('Ctrl Pts',(-12.9681156003432,13.3726811372132,
132.519157354883)) ;
#126852 = CARTESIAN_POINT('Ctrl Pts',(-12.9963459663067,13.0644553037201,
132.568316291691)) ;
#126853 = CARTESIAN_POINT('Ctrl Pts',(-13.0497942608992,12.7851437851833,
132.691521621221)) ;
#126854 = CARTESIAN_POINT('Ctrl Pts',(-13.1261848175249,12.5493640401518,
132.881485944065)) ;
#126855 = CARTESIAN_POINT('Ctrl Pts',(-13.2201072319773,12.3769707551736,
133.122803932911)) ;
#126856 = CARTESIAN_POINT('Ctrl Pts',(-13.3264644051921,12.2789143084507,
133.400245688756)) ;
#126857 = CARTESIAN_POINT('Ctrl Pts',(-13.4370417615997,12.2633331273902,
133.690248654749)) ;
#126858 = CARTESIAN_POINT('Ctrl Pts',(-13.5459037408289,12.3306602572705,
133.975076437194)) ;
#126859 = CARTESIAN_POINT('Ctrl Pts',(-13.6452910724307,12.476620286477,134.232259263529)) ;
#126860 = CARTESIAN_POINT('Ctrl Pts',(-13.7286047765094,12.6891736358698,
134.442646796355)) ;
#126861 = CARTESIAN_POINT('Ctrl Pts',(-13.791397134402,12.9552555089657,134.592923912506)) ;
#126862 = CARTESIAN_POINT('Ctrl Pts',(-13.8293665170543,13.2547270236638,
134.670715591851)) ;
#126863 = CARTESIAN_POINT('Ctrl Pts',(-13.840619326519,13.5662746405731,134.670455955337)) ;
#126864 = CARTESIAN_POINT('Ctrl Pts',(-13.8250952024996,13.8673046435887,
134.592005354761)) ;
#126865 = CARTESIAN_POINT('Ctrl Pts',(-13.7845898717327,14.1368396800883,
134.440539650573)) ;
#126866 = CARTESIAN_POINT('Ctrl Pts',(-13.7227936344222,14.3550474216671,
134.226906056734)) ;
#126867 = CARTESIAN_POINT('Ctrl Pts',(-13.6447577022458,14.5066809592571,
133.965799455824)) ;
#126868 = CARTESIAN_POINT('Ctrl Pts',(-13.5568840038658,14.5805549920085,
133.675968281385)) ;
#126869 = CARTESIAN_POINT('Ctrl Pts',(-13.466270022072,14.5715434315125,133.378164426788)) ;
#126870 = CARTESIAN_POINT('Ctrl Pts',(-13.3799814831956,14.480461463905,133.09298388884)) ;
#126871 = CARTESIAN_POINT('Ctrl Pts',(-13.3047665182075,14.3129344866538,
132.840042323809)) ;
#126872 = CARTESIAN_POINT('Ctrl Pts',(-13.2472795095458,14.0824719984918,
132.639041871323)) ;
#126873 = CARTESIAN_POINT('Ctrl Pts',(-13.2119194352514,13.8045960176135,
132.502631314994)) ;
#126874 = CARTESIAN_POINT('Ctrl Pts',(-13.2020214685182,13.4994872434927,
132.440616126401)) ;
#126875 = CARTESIAN_POINT('Ctrl Pts',(-13.2192111018863,13.1877258858405,
132.457597027487)) ;
#126876 = CARTESIAN_POINT('Ctrl Pts',(-13.2626046011989,12.8947281848912,
132.551349374371)) ;
#126877 = CARTESIAN_POINT('Ctrl Pts',(-13.3305201660103,12.6375710521211,
132.716474425557)) ;
#126878 = CARTESIAN_POINT('Ctrl Pts',(-13.417753308808,12.4386468746083,132.938314812527)) ;
#126879 = CARTESIAN_POINT('Ctrl Pts',(-13.5197229471736,12.3091461004709,
133.203049301303)) ;
#126880 = CARTESIAN_POINT('Ctrl Pts',(-13.6293498918982,12.259612482053,133.490214186349)) ;
#126881 = CARTESIAN_POINT('Ctrl Pts',(-13.7400513807603,12.2934287591009,
133.78040081702)) ;
#126882 = CARTESIAN_POINT('Ctrl Pts',(-13.8440861880681,12.4085128322788,
134.051154004392)) ;
#126883 = CARTESIAN_POINT('Ctrl Pts',(-13.9345816147693,12.5956557303843,
134.28246321765)) ;
#126884 = CARTESIAN_POINT('Ctrl Pts',(-14.0062682849132,12.8419007256208,
134.458804814913)) ;
#126885 = CARTESIAN_POINT('Ctrl Pts',(-14.0547198515339,13.1310174981793,
134.567130111826)) ;
#126886 = CARTESIAN_POINT('Ctrl Pts',(-14.0768860873263,13.4394174350743,
134.598856883951)) ;
#126887 = CARTESIAN_POINT('Ctrl Pts',(-14.0720541751936,13.7489280848763,
134.551459492802)) ;
#126888 = CARTESIAN_POINT('Ctrl Pts',(-14.0413601954176,14.0326636274873,
134.428784425465)) ;
#126889 = CARTESIAN_POINT('Ctrl Pts',(-13.9876873191308,14.2739040718616,
134.238867664221)) ;
#126890 = CARTESIAN_POINT('Ctrl Pts',(-13.9153842326398,14.4542739063911,
133.994469203157)) ;
#126891 = CARTESIAN_POINT('Ctrl Pts',(-13.8309760279277,14.5602989647872,
133.714872258789)) ;
#126892 = CARTESIAN_POINT('Ctrl Pts',(-13.7403801033257,14.5853165165248,
133.417024159331)) ;
#126893 = CARTESIAN_POINT('Ctrl Pts',(-13.65150445181,14.5269567135038,133.124299899704)) ;
#126894 = CARTESIAN_POINT('Ctrl Pts',(-13.5709039203925,14.3891797896351,
132.855635428443)) ;
#126895 = CARTESIAN_POINT('Ctrl Pts',(-13.5055449502742,14.1817903074031,
132.631517682888)) ;
#126896 = CARTESIAN_POINT('Ctrl Pts',(-13.460908167106,13.9219442128278,132.468162749426)) ;
#126897 = CARTESIAN_POINT('Ctrl Pts',(-13.4403796769414,13.6244333194243,
132.374984820522)) ;
#126898 = CARTESIAN_POINT('Ctrl Pts',(-13.4464724449161,13.3138308436316,
132.359734982198)) ;
#126899 = CARTESIAN_POINT('Ctrl Pts',(-13.4796936448716,13.0089907399567,
132.423492971966)) ;
#126900 = CARTESIAN_POINT('Ctrl Pts',(-13.5376958216924,12.7367005360714,
132.559985324287)) ;
#126901 = CARTESIAN_POINT('Ctrl Pts',(-13.6177496740489,12.5117902877451,
132.760692962081)) ;
#126902 = CARTESIAN_POINT('Ctrl Pts',(-13.7145094270354,12.3525056138097,
133.010254920769)) ;
#126903 = CARTESIAN_POINT('Ctrl Pts',(-13.8222036002752,12.2695603566645,
133.291647946124)) ;
#126904 = CARTESIAN_POINT('Ctrl Pts',(-13.9334295911699,12.2698997440141,
133.58338643449)) ;
#126905 = CARTESIAN_POINT('Ctrl Pts',(-14.0403607064271,12.352163996818,133.862787899853)) ;
#126906 = CARTESIAN_POINT('Ctrl Pts',(-14.1373924563583,12.5116414977634,
134.113058580981)) ;
#126907 = CARTESIAN_POINT('Ctrl Pts',(-14.2173629494588,12.7360068873482,
134.313587886391)) ;
#126908 = CARTESIAN_POINT('Ctrl Pts',(-14.2756685526493,13.0100795378332,
134.450754231057)) ;
#126909 = CARTESIAN_POINT('Ctrl Pts',(-14.3086572681643,13.3126252447019,
134.514091490249)) ;
#126910 = CARTESIAN_POINT('Ctrl Pts',(-14.3148158817546,13.6254714681501,
134.498785238037)) ;
#126911 = CARTESIAN_POINT('Ctrl Pts',(-14.2943755288969,13.921236470121,134.406066716109)) ;
#126912 = CARTESIAN_POINT('Ctrl Pts',(-14.2494771644102,14.1826934134292,
134.241738201168)) ;
#126913 = CARTESIAN_POINT('Ctrl Pts',(-14.1843383054734,14.3889686231296,
134.018412105004)) ;
#126914 = CARTESIAN_POINT('Ctrl Pts',(-14.1036479063904,14.5271449992224,
133.749433553487)) ;
#126915 = CARTESIAN_POINT('Ctrl Pts',(-14.0146176133587,14.5852339330884,
133.456206620789)) ;
#126916 = CARTESIAN_POINT('Ctrl Pts',(-13.9245692886674,14.5605427750385,
133.160162631154)) ;
#126917 = CARTESIAN_POINT('Ctrl Pts',(-13.8397090427971,14.4541441679249,
132.879072280579)) ;
#126918 = CARTESIAN_POINT('Ctrl Pts',(-13.7675999424785,14.2740963431477,
132.635321969107)) ;
#126919 = CARTESIAN_POINT('Ctrl Pts',(-13.7137337312793,14.0323113034301,
132.444751360353)) ;
#126920 = CARTESIAN_POINT('Ctrl Pts',(-13.6831298810078,13.7476340175603,
132.322252805189)) ;
#126921 = CARTESIAN_POINT('Ctrl Pts',(-13.6782879805551,13.4408490970619,
132.275120776001)) ;
#126922 = CARTESIAN_POINT('Ctrl Pts',(-13.7005416589842,13.1304291613817,
132.306881371971)) ;
#126923 = CARTESIAN_POINT('Ctrl Pts',(-13.7487855845768,12.8426172804035,
132.414756826716)) ;
#126924 = CARTESIAN_POINT('Ctrl Pts',(-13.8208039684073,12.5951022421241,
132.591898091082)) ;
#126925 = CARTESIAN_POINT('Ctrl Pts',(-13.9110777354065,12.4086451366849,
132.822659096915)) ;
#126926 = CARTESIAN_POINT('Ctrl Pts',(-14.0152201075138,12.2933533540089,
133.093685240975)) ;
#126927 = CARTESIAN_POINT('Ctrl Pts',(-14.1258578816827,12.259635664544,133.383708871411)) ;
#126928 = CARTESIAN_POINT('Ctrl Pts',(-14.2353399031304,12.3091205538474,
133.670488901547)) ;
#126929 = CARTESIAN_POINT('Ctrl Pts',(-14.3371725585979,12.4379929301553,
133.934891434385)) ;
#126930 = CARTESIAN_POINT('Ctrl Pts',(-14.4250620411893,12.6386444970783,
134.158382491319)) ;
#126931 = CARTESIAN_POINT('Ctrl Pts',(-14.4924635887895,12.8942394959608,
134.322231369689)) ;
#126932 = CARTESIAN_POINT('Ctrl Pts',(-14.5359913992517,13.1876523538433,
134.416314155428)) ;
#126933 = CARTESIAN_POINT('Ctrl Pts',(-14.5531646384012,13.4984174777635,
134.433357576276)) ;
#126934 = CARTESIAN_POINT('Ctrl Pts',(-14.5433292922397,13.804322914882,134.371440213958)) ;
#126935 = CARTESIAN_POINT('Ctrl Pts',(-14.5079547278182,14.0825044071424,
134.234961968097)) ;
#126936 = CARTESIAN_POINT('Ctrl Pts',(-14.4502363015794,14.3134151405244,
134.033186347547)) ;
#126937 = CARTESIAN_POINT('Ctrl Pts',(-14.3755312606289,14.4799820056889,
133.781954581635)) ;
#126938 = CARTESIAN_POINT('Ctrl Pts',(-14.2886874107007,14.5717628953294,
133.4949287269)) ;
#126939 = CARTESIAN_POINT('Ctrl Pts',(-14.1984355671894,14.5804902446719,
133.198322327595)) ;
#126940 = CARTESIAN_POINT('Ctrl Pts',(-14.1105879218463,14.5068426391239,
132.908575316213)) ;
#126941 = CARTESIAN_POINT('Ctrl Pts',(-14.0326036147844,14.3556215775595,
132.647664192124)) ;
#126942 = CARTESIAN_POINT('Ctrl Pts',(-13.9705602133679,14.1365916181852,
132.433178184827)) ;
#126943 = CARTESIAN_POINT('Ctrl Pts',(-13.9302307321672,13.8680780332019,
132.282355246629)) ;
#126944 = CARTESIAN_POINT('Ctrl Pts',(-13.9145452425664,13.5671869080058,
132.2034355718)) ;
#126945 = CARTESIAN_POINT('Ctrl Pts',(-13.9259229339394,13.2537546109161,
132.20333913892)) ;
#126946 = CARTESIAN_POINT('Ctrl Pts',(-13.9637000582678,12.9561225351469,
132.280771186731)) ;
#126947 = CARTESIAN_POINT('Ctrl Pts',(-14.0264505290295,12.6895770541959,
132.430888192073)) ;
#126948 = CARTESIAN_POINT('Ctrl Pts',(-14.1099152437945,12.4765149005577,
132.641654318194)) ;
#126949 = CARTESIAN_POINT('Ctrl Pts',(-14.2096080891455,12.3303993150384,
132.899637545338)) ;
#126950 = CARTESIAN_POINT('Ctrl Pts',(-14.3180690093773,12.2633426661684,
133.183421114825)) ;
#126951 = CARTESIAN_POINT('Ctrl Pts',(-14.4289810692293,12.2791039677748,
133.474293945749)) ;
#126952 = CARTESIAN_POINT('Ctrl Pts',(-14.5347689827399,12.3764767274057,
133.750263662714)) ;
#126953 = CARTESIAN_POINT('Ctrl Pts',(-14.6292816067322,12.5500288715812,
133.993084325586)) ;
#126954 = CARTESIAN_POINT('Ctrl Pts',(-14.7051205759119,12.78395781333,134.181698039827)) ;
#126955 = CARTESIAN_POINT('Ctrl Pts',(-14.7590884771075,13.0658040836913,
134.306109130981)) ;
#126956 = CARTESIAN_POINT('Ctrl Pts',(-14.7870570873247,13.3726170327576,
134.354673270728)) ;
#126957 = CARTESIAN_POINT('Ctrl Pts',(-14.7880362308985,13.6826397298667,
134.324425071455)) ;
#126958 = CARTESIAN_POINT('Ctrl Pts',(-14.7629011385649,13.9734160140871,
134.217988273275)) ;
#126959 = CARTESIAN_POINT('Ctrl Pts',(-14.7135553917032,14.2269288316592,
134.040531948829)) ;
#126960 = CARTESIAN_POINT('Ctrl Pts',(-14.6452446553135,14.4205112254327,
133.808019823246)) ;
#126961 = CARTESIAN_POINT('Ctrl Pts',(-14.5627005184461,14.5441065975964,
133.533729916496)) ;
#126962 = CARTESIAN_POINT('Ctrl Pts',(-14.4726632379768,14.5870792666042,
133.237494403746)) ;
#126963 = CARTESIAN_POINT('Ctrl Pts',(-14.3827907850209,14.5462510454972,
132.941823015601)) ;
#126964 = CARTESIAN_POINT('Ctrl Pts',(-14.3003438724804,14.4261089753038,
132.668016533417)) ;
#126965 = CARTESIAN_POINT('Ctrl Pts',(-14.2307721367749,14.2320089308133,
132.431424344221)) ;
#126966 = CARTESIAN_POINT('Ctrl Pts',(-14.1813514089669,13.9821034957132,
132.254072397116)) ;
#126967 = CARTESIAN_POINT('Ctrl Pts',(-14.155314709505,13.6914861079863,132.144897171417)) ;
#126968 = CARTESIAN_POINT('Ctrl Pts',(-14.1554757838754,13.3820427102498,
132.112307580713)) ;
#126969 = CARTESIAN_POINT('Ctrl Pts',(-14.1829242521949,13.0731824784138,
132.159161065755)) ;
#126970 = CARTESIAN_POINT('Ctrl Pts',(-14.2356771557397,12.7927891532511,
132.280328855648)) ;
#126971 = CARTESIAN_POINT('Ctrl Pts',(-14.3114802654347,12.555308710761,132.468568512814)) ;
#126972 = CARTESIAN_POINT('Ctrl Pts',(-14.405137795849,12.3807971567645,132.709061171522)) ;
#126973 = CARTESIAN_POINT('Ctrl Pts',(-14.5108510096583,12.2807361442519,
132.984745301486)) ;
#126974 = CARTESIAN_POINT('Ctrl Pts',(-14.6217350370507,12.2625961499198,
133.275536642157)) ;
#126975 = CARTESIAN_POINT('Ctrl Pts',(-14.7305884334379,12.3275534579407,
133.560394240551)) ;
#126976 = CARTESIAN_POINT('Ctrl Pts',(-14.8303351103071,12.4713199935408,
133.818625118749)) ;
#126977 = CARTESIAN_POINT('Ctrl Pts',(-14.9142095075345,12.6818353825156,
134.030669934059)) ;
#126978 = CARTESIAN_POINT('Ctrl Pts',(-14.9780252508446,12.9488695805188,
134.183682231059)) ;
#126979 = CARTESIAN_POINT('Ctrl Pts',(-15.0163167509657,13.2449964341876,
134.2627235007)) ;
#126980 = CARTESIAN_POINT('Ctrl Pts',(-15.0284923230541,13.5577146897345,
134.265023837386)) ;
#126981 = CARTESIAN_POINT('Ctrl Pts',(-15.0136674302917,13.8591379588549,
134.188639506214)) ;
#126982 = CARTESIAN_POINT('Ctrl Pts',(-14.9737786696409,14.1301669170847,
134.038933696206)) ;
#126983 = CARTESIAN_POINT('Ctrl Pts',(-14.9125163633659,14.3498259232659,
133.826877916861)) ;
#126984 = CARTESIAN_POINT('Ctrl Pts',(-14.8349895204821,14.5033075535996,
133.567312008067)) ;
#126985 = CARTESIAN_POINT('Ctrl Pts',(-14.7472616829707,14.5795880895815,
133.277889078353)) ;
#126986 = CARTESIAN_POINT('Ctrl Pts',(-14.6565928445212,14.5729975204269,
132.979913996434)) ;
#126987 = CARTESIAN_POINT('Ctrl Pts',(-14.5698387137469,14.4837968438998,
132.693276319562)) ;
#126988 = CARTESIAN_POINT('Ctrl Pts',(-14.4943500116682,14.3181445860539,
132.439567110174)) ;
#126989 = CARTESIAN_POINT('Ctrl Pts',(-14.4364625855008,14.0900336842333,
132.237499897993)) ;
#126990 = CARTESIAN_POINT('Ctrl Pts',(-14.4003322523361,13.8125787469842,
132.098759396213)) ;
#126991 = CARTESIAN_POINT('Ctrl Pts',(-14.3897456286772,13.5087143541534,
132.034817758566)) ;
#126992 = CARTESIAN_POINT('Ctrl Pts',(-14.4060516377967,13.1970642256003,
132.049247933405)) ;
#126993 = CARTESIAN_POINT('Ctrl Pts',(-14.4488719696154,12.9023258693894,
132.141215716512)) ;
#126994 = CARTESIAN_POINT('Ctrl Pts',(-14.5159375651983,12.6446851573858,
132.303967806051)) ;
#126995 = CARTESIAN_POINT('Ctrl Pts',(-14.6026582838117,12.4436426796563,
132.524294973263)) ;
#126996 = CARTESIAN_POINT('Ctrl Pts',(-14.704427237355,12.3118006099846,132.788401667145)) ;
#126997 = CARTESIAN_POINT('Ctrl Pts',(-14.8139557089677,12.259762671147,133.075273126533)) ;
#126998 = CARTESIAN_POINT('Ctrl Pts',(-14.9251382688252,12.2917039149137,
133.366735111266)) ;
#126999 = CARTESIAN_POINT('Ctrl Pts',(-15.0286487061425,12.4035190243102,
133.636225798027)) ;
#127000 = CARTESIAN_POINT('Ctrl Pts',(-15.1203793223657,12.5902948826821,
133.870856294404)) ;
#127001 = CARTESIAN_POINT('Ctrl Pts',(-15.1921924551787,12.8337324578526,
134.047773898269)) ;
#127002 = CARTESIAN_POINT('Ctrl Pts',(-15.2416538483721,13.1235886478701,
134.158851739517)) ;
#127003 = CARTESIAN_POINT('Ctrl Pts',(-15.2643296293558,13.4302519439914,
134.192228539478)) ;
#127004 = CARTESIAN_POINT('Ctrl Pts',(-15.2604682402602,13.7390104771059,
134.147792840823)) ;
#127005 = CARTESIAN_POINT('Ctrl Pts',(-15.2302304828528,14.0260062251914,
134.026182196942)) ;
#127006 = CARTESIAN_POINT('Ctrl Pts',(-15.1773828700923,14.267226894927,133.83886254729)) ;
#127007 = CARTESIAN_POINT('Ctrl Pts',(-15.1056430753497,14.4498458863908,
133.596118183399)) ;
#127008 = CARTESIAN_POINT('Ctrl Pts',(-15.021088548327,14.5586319287784,133.315937393289)) ;
#127009 = CARTESIAN_POINT('Ctrl Pts',(-14.9305285876603,14.5856242099091,
133.018186098394)) ;
#127010 = CARTESIAN_POINT('Ctrl Pts',(-14.8418950205614,14.5299078303726,
132.726313987162)) ;
#127011 = CARTESIAN_POINT('Ctrl Pts',(-14.7607450760407,14.3940107888909,
132.455958932693)) ;
#127012 = CARTESIAN_POINT('Ctrl Pts',(-14.6950115091372,14.1888420918384,
132.230820509577)) ;
#127013 = CARTESIAN_POINT('Ctrl Pts',(-14.6496592401671,13.9299824930108,
132.065327212489)) ;
#127014 = CARTESIAN_POINT('Ctrl Pts',(-14.6284006795938,13.6339609144374,
131.970100332748)) ;
#127015 = CARTESIAN_POINT('Ctrl Pts',(-14.6337188432872,13.3227159368467,
131.952503879531)) ;
#127016 = CARTESIAN_POINT('Ctrl Pts',(-14.6659818143214,13.0187244434426,
132.013618672665)) ;
#127017 = CARTESIAN_POINT('Ctrl Pts',(-14.7233385330698,12.7442184480219,
132.148123450518)) ;
#127018 = CARTESIAN_POINT('Ctrl Pts',(-14.8032873271645,12.516718909921,132.348361947156)) ;
#127019 = CARTESIAN_POINT('Ctrl Pts',(-14.8992236867721,12.3563386228632,
132.595676015683)) ;
#127020 = CARTESIAN_POINT('Ctrl Pts',(-15.00647311092,12.2709228353889,132.875831085534)) ;
#127021 = CARTESIAN_POINT('Ctrl Pts',(-15.1178233288828,12.2686101077704,
133.167894840655)) ;
#127022 = CARTESIAN_POINT('Ctrl Pts',(-15.2252101895966,12.3485946341444,
133.44855717488)) ;
#127023 = CARTESIAN_POINT('Ctrl Pts',(-15.3229248735586,12.5068356453483,
133.70070522754)) ;
#127024 = CARTESIAN_POINT('Ctrl Pts',(-15.4029565974295,12.728330138996,133.901605268035)) ;
#127025 = CARTESIAN_POINT('Ctrl Pts',(-15.4621017130809,13.0013550169445,
134.041190190912)) ;
#127026 = CARTESIAN_POINT('Ctrl Pts',(-15.4958591875495,13.303953158046,134.106709837516)) ;
#127027 = CARTESIAN_POINT('Ctrl Pts',(-15.5028362362812,13.6158508355622,
134.093908778801)) ;
#127028 = CARTESIAN_POINT('Ctrl Pts',(-15.4830234200552,13.9138455338492,
134.002849682409)) ;
#127029 = CARTESIAN_POINT('Ctrl Pts',(-15.4389659228457,14.1752852419692,
133.841141599243)) ;
#127030 = CARTESIAN_POINT('Ctrl Pts',(-15.3742548041053,14.3839668801463,
133.618990077083)) ;
#127031 = CARTESIAN_POINT('Ctrl Pts',(-15.2939923725203,14.5240578429112,
133.351300381935)) ;
#127032 = CARTESIAN_POINT('Ctrl Pts',(-15.2051966892418,14.584818932524,133.058785675523)) ;
#127033 = CARTESIAN_POINT('Ctrl Pts',(-15.1144952079084,14.5621167369362,
132.760611447614)) ;
#127034 = CARTESIAN_POINT('Ctrl Pts',(-15.0299271948312,14.4583966415937,
132.480583857298)) ;
#127035 = CARTESIAN_POINT('Ctrl Pts',(-14.9572763457915,14.2803903963779,
132.235223701312)) ;
#127036 = CARTESIAN_POINT('Ctrl Pts',(-14.9029121430072,14.0406559571458,
132.043265678617)) ;
#127037 = CARTESIAN_POINT('Ctrl Pts',(-14.8714358369862,13.7571590252373,
131.918221498036)) ;
#127038 = CARTESIAN_POINT('Ctrl Pts',(-14.8659049731751,13.4483332658606,
131.868817727218)) ;
#127039 = CARTESIAN_POINT('Ctrl Pts',(-14.8871485835861,13.1406103959238,
131.897955203955)) ;
#127040 = CARTESIAN_POINT('Ctrl Pts',(-14.9350650117889,12.849237718573,132.004565980115)) ;
#127041 = CARTESIAN_POINT('Ctrl Pts',(-15.0060654331534,12.6021186040621,
132.178962627107)) ;
#127042 = CARTESIAN_POINT('Ctrl Pts',(-15.0959333972116,12.4130744428075,
132.408478228169)) ;
#127043 = CARTESIAN_POINT('Ctrl Pts',(-15.2001942594425,12.295357536539,132.6797330253)) ;
#127044 = CARTESIAN_POINT('Ctrl Pts',(-15.3102776881432,12.2595400049776,
132.968276410172)) ;
#127045 = CARTESIAN_POINT('Ctrl Pts',(-15.4199784955262,12.3063152833776,
133.255674356506)) ;
#127046 = CARTESIAN_POINT('Ctrl Pts',(-15.522699193365,12.4341408238282,133.522468160323)) ;
#127047 = CARTESIAN_POINT('Ctrl Pts',(-15.6103829822627,12.6316134700122,
133.745609070741)) ;
#127048 = CARTESIAN_POINT('Ctrl Pts',(-15.6786358897342,12.8861350192124,
133.911877716703)) ;
#127049 = CARTESIAN_POINT('Ctrl Pts',(-15.7229388254079,13.1792139028364,
134.008179554018)) ;
#127050 = CARTESIAN_POINT('Ctrl Pts',(-15.7408625348171,13.490568739432,134.027334806477)) ;
#127051 = CARTESIAN_POINT('Ctrl Pts',(-15.7316840369272,13.7964603979055,
133.96738117624)) ;
#127052 = CARTESIAN_POINT('Ctrl Pts',(-15.6971658649045,14.0743848180785,
133.833556786715)) ;
#127053 = CARTESIAN_POINT('Ctrl Pts',(-15.640209575695,14.3070162611111,133.634045700277)) ;
#127054 = CARTESIAN_POINT('Ctrl Pts',(-15.5654530352524,14.476451846962,133.382463536536)) ;
#127055 = CARTESIAN_POINT('Ctrl Pts',(-15.4796013706087,14.569850177848,133.098627967463)) ;
#127056 = CARTESIAN_POINT('Ctrl Pts',(-15.3889094017471,14.5816111241078,
132.800558625303)) ;
#127057 = CARTESIAN_POINT('Ctrl Pts',(-15.300616199253,14.5098991717079,132.50941294368)) ;
#127058 = CARTESIAN_POINT('Ctrl Pts',(-15.2222312224412,14.360403037698,132.247300438646)) ;
#127059 = CARTESIAN_POINT('Ctrl Pts',(-15.1598553959439,14.143565690272,132.031931962309)) ;
#127060 = CARTESIAN_POINT('Ctrl Pts',(-15.1187843239202,13.8762646142661,
131.878935402952)) ;
#127061 = CARTESIAN_POINT('Ctrl Pts',(-15.1024542909266,13.5746434283165,
131.79799241285)) ;
#127062 = CARTESIAN_POINT('Ctrl Pts',(-15.1128551398615,13.2647986868619,
131.795431588597)) ;
#127063 = CARTESIAN_POINT('Ctrl Pts',(-15.1500740102669,12.9638356585252,
131.870941727578)) ;
#127064 = CARTESIAN_POINT('Ctrl Pts',(-15.2120844356372,12.696740713892,132.018978212453)) ;
#127065 = CARTESIAN_POINT('Ctrl Pts',(-15.2951868761685,12.4815167402667,
132.228612079136)) ;
#127066 = CARTESIAN_POINT('Ctrl Pts',(-15.3941529108664,12.3337893595149,
132.484595432364)) ;
#127067 = CARTESIAN_POINT('Ctrl Pts',(-15.5026973347409,12.2640797923872,
132.768538743853)) ;
#127068 = CARTESIAN_POINT('Ctrl Pts',(-15.6135110810389,12.2774691483239,
133.059167262527)) ;
#127069 = CARTESIAN_POINT('Ctrl Pts',(-15.7195456012451,12.3724670418659,
133.335855362595)) ;
#127070 = CARTESIAN_POINT('Ctrl Pts',(-15.8144572008724,12.543767432119,133.579865193293)) ;
#127071 = CARTESIAN_POINT('Ctrl Pts',(-15.8910215330709,12.7765746874498,
133.770532042184)) ;
#127072 = CARTESIAN_POINT('Ctrl Pts',(-15.9455551191463,13.056442699504,133.896702931996)) ;
#127073 = CARTESIAN_POINT('Ctrl Pts',(-15.9743804491519,13.3632374383365,
133.947714740299)) ;
#127074 = CARTESIAN_POINT('Ctrl Pts',(-15.9762566494674,13.6730055112077,
133.920150028813)) ;
#127075 = CARTESIAN_POINT('Ctrl Pts',(-15.9515216477166,13.9671153301203,
133.81457598732)) ;
#127076 = CARTESIAN_POINT('Ctrl Pts',(-15.9033160121956,14.2192391105439,
133.640818547145)) ;
#127077 = CARTESIAN_POINT('Ctrl Pts',(-15.835026362201,14.4164802327196,133.408099916759)) ;
#127078 = CARTESIAN_POINT('Ctrl Pts',(-15.7529435024503,14.5415580388922,
133.135249670794)) ;
#127079 = CARTESIAN_POINT('Ctrl Pts',(-15.6633179777156,14.5869148382087,
132.840315322194)) ;
#127080 = CARTESIAN_POINT('Ctrl Pts',(-15.5733831628916,14.5490099529441,
132.544490917924)) ;
#127081 = CARTESIAN_POINT('Ctrl Pts',(-15.490058780783,14.4299835692337,132.267872421387)) ;
#127082 = CARTESIAN_POINT('Ctrl Pts',(-15.4206307225619,14.2395160261302,
132.032004599489)) ;
#127083 = CARTESIAN_POINT('Ctrl Pts',(-15.3702268503173,13.9900850961344,
131.851611615681)) ;
#127084 = CARTESIAN_POINT('Ctrl Pts',(-15.3434852338531,13.7002631156838,
131.740380824323)) ;
#127085 = CARTESIAN_POINT('Ctrl Pts',(-15.34291772876,13.3906063492619,131.705608770205)) ;
#127086 = CARTESIAN_POINT('Ctrl Pts',(-15.3694315743629,13.0826197535591,
131.749876872948)) ;
#127087 = CARTESIAN_POINT('Ctrl Pts',(-15.4217316411397,12.7997481172877,
131.869548993111)) ;
#127088 = CARTESIAN_POINT('Ctrl Pts',(-15.4967708608653,12.5614902971475,
132.05565395496)) ;
#127089 = CARTESIAN_POINT('Ctrl Pts',(-15.5901217372407,12.3846250273346,
132.295195219659)) ;
#127090 = CARTESIAN_POINT('Ctrl Pts',(-15.695629337142,12.2824687909252,132.570272051232)) ;
#127091 = CARTESIAN_POINT('Ctrl Pts',(-15.8061596908325,12.2619556332192,
132.860120338079)) ;
#127092 = CARTESIAN_POINT('Ctrl Pts',(-15.9152791218839,12.3244285143439,
133.145725763157)) ;
#127093 = CARTESIAN_POINT('Ctrl Pts',(-16.0156184574548,12.4664340119557,
133.405611588913)) ;
#127094 = CARTESIAN_POINT('Ctrl Pts',(-16.0998938298251,12.675348720281,133.618840063751)) ;
#127095 = CARTESIAN_POINT('Ctrl Pts',(-16.1640285350581,12.9390314346698,
133.773020248114)) ;
#127096 = CARTESIAN_POINT('Ctrl Pts',(-16.2034911895346,13.2369183007794,
133.85520053705)) ;
#127097 = CARTESIAN_POINT('Ctrl Pts',(-16.2162744763826,13.549774387286,133.859260960991)) ;
#127098 = CARTESIAN_POINT('Ctrl Pts',(-16.2022423520224,13.850609448165,133.785316886062)) ;
#127099 = CARTESIAN_POINT('Ctrl Pts',(-16.1630477314313,14.1229209827014,
133.637631054172)) ;
#127100 = CARTESIAN_POINT('Ctrl Pts',(-16.1024279258205,14.3440340746158,
133.42749370549)) ;
#127101 = CARTESIAN_POINT('Ctrl Pts',(-16.0251958195372,14.5000650496519,
133.168737022986)) ;
#127102 = CARTESIAN_POINT('Ctrl Pts',(-15.9372506091348,14.578644462167,132.878532422709)) ;
#127103 = CARTESIAN_POINT('Ctrl Pts',(-15.8471380330024,14.5743811633841,
132.582393935937)) ;
#127104 = CARTESIAN_POINT('Ctrl Pts',(-15.7598975395241,14.4873598726622,
132.29423150623)) ;
#127105 = CARTESIAN_POINT('Ctrl Pts',(-15.6841714035355,14.3240886770746,
132.039909083496)) ;
#127106 = CARTESIAN_POINT('Ctrl Pts',(-15.625630709951,14.0972553014586,131.835876518833)) ;
#127107 = CARTESIAN_POINT('Ctrl Pts',(-15.5888545861176,13.8219067372358,
131.695361474815)) ;
#127108 = CARTESIAN_POINT('Ctrl Pts',(-15.5774343178227,13.5160256526642,
131.628709192123)) ;
#127109 = CARTESIAN_POINT('Ctrl Pts',(-15.5931141548672,13.2050737641674,
131.6413999151)) ;
#127110 = CARTESIAN_POINT('Ctrl Pts',(-15.6350536186872,12.9106474096039,
131.73090798225)) ;
#127111 = CARTESIAN_POINT('Ctrl Pts',(-15.7013184155062,12.6518068441283,
131.891363677284)) ;
#127112 = CARTESIAN_POINT('Ctrl Pts',(-15.7879054566775,12.4481718520534,
132.111160447903)) ;
#127113 = CARTESIAN_POINT('Ctrl Pts',(-15.8891804504899,12.3143466124611,
132.373885643705)) ;
#127114 = CARTESIAN_POINT('Ctrl Pts',(-15.9991528091625,12.2602411287431,
132.661877127695)) ;
#127115 = CARTESIAN_POINT('Ctrl Pts',(-16.1088758468445,12.289044216294,132.949549239462)) ;
#127116 = CARTESIAN_POINT('Ctrl Pts',(-16.2139161399805,12.3996399053781,
133.223107982342)) ;
#127117 = CARTESIAN_POINT('Ctrl Pts',(-16.3052990396997,12.5827969083002,
133.457035289673)) ;
#127118 = CARTESIAN_POINT('Ctrl Pts',(-16.3784225593528,12.826962989628,133.637457202955)) ;
#127119 = CARTESIAN_POINT('Ctrl Pts',(-16.4280832723587,13.1127056207623,
133.749492183983)) ;
#127120 = CARTESIAN_POINT('Ctrl Pts',(-16.4519120641996,13.421711878802,133.785935789456)) ;
#127121 = CARTESIAN_POINT('Ctrl Pts',(-16.4487067222851,13.7304251120726,
133.743459367552)) ;
#127122 = CARTESIAN_POINT('Ctrl Pts',(-16.4192362436366,14.018344311728,133.624095788386)) ;
#127123 = CARTESIAN_POINT('Ctrl Pts',(-16.3668470537399,14.2615012017521,
133.438046957195)) ;
#127124 = CARTESIAN_POINT('Ctrl Pts',(-16.2956609167277,14.4455241651706,
133.196981670041)) ;
#127125 = CARTESIAN_POINT('Ctrl Pts',(-16.2116523432265,14.5564730529287,
132.918492749156)) ;
#127126 = CARTESIAN_POINT('Ctrl Pts',(-16.1208373176366,14.58603325722,132.619873861017)) ;
#127127 = CARTESIAN_POINT('Ctrl Pts',(-16.0322331447019,14.5327319880778,
132.328153351535)) ;
#127128 = CARTESIAN_POINT('Ctrl Pts',(-15.9506596892589,14.3988255152791,
132.056517691132)) ;
#127129 = CARTESIAN_POINT('Ctrl Pts',(-15.8846965931716,14.1966329622431,
131.830874369559)) ;
#127130 = CARTESIAN_POINT('Ctrl Pts',(-15.8383960091304,13.9381994545952,
131.662466237002)) ;
#127131 = CARTESIAN_POINT('Ctrl Pts',(-15.8164206296693,13.6421507642692,
131.565070286919)) ;
#127132 = CARTESIAN_POINT('Ctrl Pts',(-15.8209925100705,13.3319747880892,
131.545390307733)) ;
#127133 = CARTESIAN_POINT('Ctrl Pts',(-15.8523510548153,13.0275241495644,
131.603884248757)) ;
#127134 = CARTESIAN_POINT('Ctrl Pts',(-15.90959227723,12.7499513139427,131.737788844149)) ;
#127135 = CARTESIAN_POINT('Ctrl Pts',(-15.9882747688464,12.5230805952481,
131.934644253153)) ;
#127136 = CARTESIAN_POINT('Ctrl Pts',(-16.0842519007302,12.3595163479197,
132.181899906692)) ;
#127137 = CARTESIAN_POINT('Ctrl Pts',(-16.1915571107785,12.2720601072795,
132.462152269854)) ;
#127138 = CARTESIAN_POINT('Ctrl Pts',(-16.3026683400584,12.2676665398888,
132.753584917152)) ;
#127139 = CARTESIAN_POINT('Ctrl Pts',(-16.4098725171092,12.3451448289758,
133.033825189078)) ;
#127140 = CARTESIAN_POINT('Ctrl Pts',(-16.5077398618101,12.5004782540512,
133.286522113672)) ;
#127141 = CARTESIAN_POINT('Ctrl Pts',(-16.5887803868399,12.7212077587515,
133.490207402048)) ;
#127142 = CARTESIAN_POINT('Ctrl Pts',(-16.6486155618414,12.9936145319541,
133.631759184654)) ;
#127143 = CARTESIAN_POINT('Ctrl Pts',(-16.6830064614964,13.2947837203187,
133.699223914889)) ;
#127144 = CARTESIAN_POINT('Ctrl Pts',(-16.690802067885,13.6064068032795,133.688848453476)) ;
#127145 = CARTESIAN_POINT('Ctrl Pts',(-16.6718235868781,13.9050217412781,
133.600245728763)) ;
#127146 = CARTESIAN_POINT('Ctrl Pts',(-16.6283034085852,14.1686336677941,
133.440001693097)) ;
#127147 = CARTESIAN_POINT('Ctrl Pts',(-16.5641212588145,14.3788182698461,
133.219417424364)) ;
#127148 = CARTESIAN_POINT('Ctrl Pts',(-16.4844394280471,14.5208662743525,
132.953507778483)) ;
#127149 = CARTESIAN_POINT('Ctrl Pts',(-16.3956858711808,14.5841619964858,
132.661068294954)) ;
#127150 = CARTESIAN_POINT('Ctrl Pts',(-16.3052261807868,14.5641966212731,
132.363712807229)) ;
#127151 = CARTESIAN_POINT('Ctrl Pts',(-16.219987051645,14.4625802031817,132.081576128943)) ;
#127152 = CARTESIAN_POINT('Ctrl Pts',(-16.1468023432749,14.286005519678,131.834596099158)) ;
#127153 = CARTESIAN_POINT('Ctrl Pts',(-16.092019731511,14.0484511766116,131.641509779847)) ;
#127154 = CARTESIAN_POINT('Ctrl Pts',(-16.0598137195397,13.7663469641466,
131.514368112264)) ;
#127155 = CARTESIAN_POINT('Ctrl Pts',(-16.0534392828027,13.4574607862846,
131.462452093776)) ;
#127156 = CARTESIAN_POINT('Ctrl Pts',(-16.0740291175869,13.1488899343714,
131.489611237961)) ;
#127157 = CARTESIAN_POINT('Ctrl Pts',(-16.1208827636923,12.8583365038161,
131.593319429838)) ;
#127158 = CARTESIAN_POINT('Ctrl Pts',(-16.1914348318743,12.6085157642258,
131.76627300472)) ;
#127159 = CARTESIAN_POINT('Ctrl Pts',(-16.2810750702995,12.417394689709,131.995054740562)) ;
#127160 = CARTESIAN_POINT('Ctrl Pts',(-16.3844471754088,12.2980452519264,
132.26389707157)) ;
#127161 = CARTESIAN_POINT('Ctrl Pts',(-16.4945287592018,12.2592457780577,
132.55240289533)) ;
#127162 = CARTESIAN_POINT('Ctrl Pts',(-16.6048630643841,12.304020860261,132.841492151583)) ;
#127163 = CARTESIAN_POINT('Ctrl Pts',(-16.7071948575937,12.4286939335528,
133.107381215331)) ;
#127164 = CARTESIAN_POINT('Ctrl Pts',(-16.7957370903251,12.6243589997422,
133.332939325687)) ;
#127165 = CARTESIAN_POINT('Ctrl Pts',(-16.8649375159105,12.878908332841,133.501806658507)) ;
#127166 = CARTESIAN_POINT('Ctrl Pts',(-16.9097459869717,13.1702261034011,
133.599699878422)) ;
#127167 = CARTESIAN_POINT('Ctrl Pts',(-16.9284921865684,13.4805036941569,
133.621345959822)) ;
#127168 = CARTESIAN_POINT('Ctrl Pts',(-16.9201734499076,13.7876511360062,
133.563828434265)) ;
#127169 = CARTESIAN_POINT('Ctrl Pts',(-16.8861064009168,14.0678452510403,
133.431162542818)) ;
#127170 = CARTESIAN_POINT('Ctrl Pts',(-16.8299943231887,14.3007432572347,
133.234293389989)) ;
#127171 = CARTESIAN_POINT('Ctrl Pts',(-16.7556211261533,14.4725786347777,
132.983790036611)) ;
#127172 = CARTESIAN_POINT('Ctrl Pts',(-16.669994129504,14.5682598851549,132.70061076845)) ;
#127173 = CARTESIAN_POINT('Ctrl Pts',(-16.5793502317154,14.5824152929646,
132.402683855424)) ;
#127174 = CARTESIAN_POINT('Ctrl Pts',(-16.4910139643223,14.5133614701989,
132.111471857863)) ;
#127175 = CARTESIAN_POINT('Ctrl Pts',(-16.412111492588,14.3656855427812,131.847778677913)) ;
#127176 = CARTESIAN_POINT('Ctrl Pts',(-16.3494282335617,14.1519223371762,
131.631683900769)) ;
#127177 = CARTESIAN_POINT('Ctrl Pts',(-16.3073386916834,13.8839965789022,
131.475465893538)) ;
#127178 = CARTESIAN_POINT('Ctrl Pts',(-16.2903594127806,13.5839686018203,
131.392743081148)) ;
#127179 = CARTESIAN_POINT('Ctrl Pts',(-16.2999735659199,13.2736211027787,
131.387823786026)) ;
#127180 = CARTESIAN_POINT('Ctrl Pts',(-16.3363145444872,12.9727616409807,
131.460858307833)) ;
#127181 = CARTESIAN_POINT('Ctrl Pts',(-16.3978412897984,12.7034620887289,
131.607364231269)) ;
#127182 = CARTESIAN_POINT('Ctrl Pts',(-16.4803836389756,12.4867212109574,
131.815385050795)) ;
#127183 = CARTESIAN_POINT('Ctrl Pts',(-16.5790813271514,12.3368637166341,
132.070553250121)) ;
#127184 = CARTESIAN_POINT('Ctrl Pts',(-16.6870891237373,12.265034692949,132.353038736455)) ;
#127185 = CARTESIAN_POINT('Ctrl Pts',(-16.7982204585899,12.2758062586622,
132.644511544384)) ;
#127186 = CARTESIAN_POINT('Ctrl Pts',(-16.9048720041156,12.3692807185403,
132.922870416557)) ;
#127187 = CARTESIAN_POINT('Ctrl Pts',(-16.9996989007579,12.5378929203228,
133.166798907436)) ;
#127188 = CARTESIAN_POINT('Ctrl Pts',(-17.0769917000868,12.7694277251572,
133.359536671956)) ;
#127189 = CARTESIAN_POINT('Ctrl Pts',(-17.1322129697081,13.0484835802669,
133.487698121072)) ;
#127190 = CARTESIAN_POINT('Ctrl Pts',(-17.1617637643126,13.3553251834758,
133.540779957413)) ;
#127191 = CARTESIAN_POINT('Ctrl Pts',(-17.1643098885835,13.664055596243,133.515297231606)) ;
#127192 = CARTESIAN_POINT('Ctrl Pts',(-17.1405674412535,13.9577070332473,
133.412784627053)) ;
#127193 = CARTESIAN_POINT('Ctrl Pts',(-17.0927873539426,14.2128779767414,
133.240075341441)) ;
#127194 = CARTESIAN_POINT('Ctrl Pts',(-17.0249647373013,14.4117544181439,
133.008731542962)) ;
#127195 = CARTESIAN_POINT('Ctrl Pts',(-16.9432494624858,14.539128300591,132.736968714715)) ;
#127196 = CARTESIAN_POINT('Ctrl Pts',(-16.8533260812375,14.5867879384206,
132.441014798324)) ;
#127197 = CARTESIAN_POINT('Ctrl Pts',(-16.7637336532915,14.5512051552351,
132.146348760003)) ;
#127198 = CARTESIAN_POINT('Ctrl Pts',(-16.6799727913344,14.4343419878625,
131.868402100681)) ;
#127199 = CARTESIAN_POINT('Ctrl Pts',(-16.6100992323604,14.2455278913779,
131.631224317555)) ;
#127200 = CARTESIAN_POINT('Ctrl Pts',(-16.5591861668346,13.9981929136205,
131.449425653695)) ;
#127201 = CARTESIAN_POINT('Ctrl Pts',(-16.5316439561812,13.7085066706188,
131.335769713184)) ;
#127202 = CARTESIAN_POINT('Ctrl Pts',(-16.5303800842125,13.3995793923712,
131.299014333936)) ;
#127203 = CARTESIAN_POINT('Ctrl Pts',(-16.5559587992191,13.0919774693214,
131.340640261352)) ;
#127204 = CARTESIAN_POINT('Ctrl Pts',(-16.6078284638175,12.8067303773131,
131.458887738409)) ;
#127205 = CARTESIAN_POINT('Ctrl Pts',(-16.6818970632097,12.5682008824759,
131.642331999797)) ;
#127206 = CARTESIAN_POINT('Ctrl Pts',(-16.774928635233,12.3888212214355,131.88087429486)) ;
#127207 = CARTESIAN_POINT('Ctrl Pts',(-16.8800323422373,12.2844119471438,
132.154816836978)) ;
#127208 = CARTESIAN_POINT('Ctrl Pts',(-16.9908532021063,12.2613333945147,
132.445409149157)) ;
#127209 = CARTESIAN_POINT('Ctrl Pts',(-17.0999913187427,12.3215794553672,
132.731106180485)) ;
#127210 = CARTESIAN_POINT('Ctrl Pts',(-17.2003631560383,12.4606919099578,
132.991204117191)) ;
#127211 = CARTESIAN_POINT('Ctrl Pts',(-17.2855599741373,12.6684213928488,
133.206995727513)) ;
#127212 = CARTESIAN_POINT('Ctrl Pts',(-17.3504941522615,12.9319195354802,
133.363395978862)) ;
#127213 = CARTESIAN_POINT('Ctrl Pts',(-17.3904330455179,13.2279082414743,
133.447106708526)) ;
#127214 = CARTESIAN_POINT('Ctrl Pts',(-17.4040816521376,13.5392233230321,
133.453849322429)) ;
#127215 = CARTESIAN_POINT('Ctrl Pts',(-17.390836167045,13.8421683173594,133.382041888976)) ;
#127216 = CARTESIAN_POINT('Ctrl Pts',(-17.3522690738895,14.1158320229517,
133.236165936095)) ;
#127217 = CARTESIAN_POINT('Ctrl Pts',(-17.2920552027206,14.3390093108208,
133.027146596858)) ;
#127218 = CARTESIAN_POINT('Ctrl Pts',(-17.2153391517714,14.4964745631391,
132.769969650378)) ;
#127219 = CARTESIAN_POINT('Ctrl Pts',(-17.128130190575,14.5773715751741,132.482106689292)) ;
#127220 = CARTESIAN_POINT('Ctrl Pts',(-17.0373151597888,14.5757025299613,
132.183661495111)) ;
#127221 = CARTESIAN_POINT('Ctrl Pts',(-16.9501102952013,14.4908671144554,
131.895689095071)) ;
#127222 = CARTESIAN_POINT('Ctrl Pts',(-16.8742256801646,14.3305923177535,
131.641031426237)) ;
#127223 = CARTESIAN_POINT('Ctrl Pts',(-16.8147980608555,14.1048090701634,
131.434285608037)) ;
#127224 = CARTESIAN_POINT('Ctrl Pts',(-16.7773101810593,13.8293691647795,
131.291565197932)) ;
#127225 = CARTESIAN_POINT('Ctrl Pts',(-16.7652035431411,13.5265763718341,
131.223186509187)) ;
#127226 = CARTESIAN_POINT('Ctrl Pts',(-16.7799662486554,13.2147295079812,
131.233113488118)) ;
#127227 = CARTESIAN_POINT('Ctrl Pts',(-16.8212080996971,12.9189025307067,
131.320522875433)) ;
#127228 = CARTESIAN_POINT('Ctrl Pts',(-16.887084338435,12.6580299583616,131.47973575403)) ;
#127229 = CARTESIAN_POINT('Ctrl Pts',(-16.9727965429337,12.4534345786707,
131.697120401721)) ;
#127230 = CARTESIAN_POINT('Ctrl Pts',(-17.0739808799952,12.3171076737635,
131.959493126955)) ;
#127231 = CARTESIAN_POINT('Ctrl Pts',(-17.1832345072622,12.2606844029487,
132.245561618487)) ;
#127232 = CARTESIAN_POINT('Ctrl Pts',(-17.2938303511549,12.2870889528383,
132.53554165159)) ;
#127233 = CARTESIAN_POINT('Ctrl Pts',(-17.399072000023,12.3957983082861,132.809701372333)) ;
#127234 = CARTESIAN_POINT('Ctrl Pts',(-17.4906848011028,12.5767257036487,
133.044366686444)) ;
#127235 = CARTESIAN_POINT('Ctrl Pts',(-17.5643113957083,12.818699316301,133.226334863995)) ;
#127236 = CARTESIAN_POINT('Ctrl Pts',(-17.6149368941073,13.105041814552,133.341009417793)) ;
#127237 = CARTESIAN_POINT('Ctrl Pts',(-17.6393801095251,13.4130762761878,
133.379325378718)) ;
#127238 = CARTESIAN_POINT('Ctrl Pts',(-17.636930864629,13.7214651892491,133.339116703289)) ;
#127239 = CARTESIAN_POINT('Ctrl Pts',(-17.6084372265889,14.0093161776234,
133.222748419654)) ;
#127240 = CARTESIAN_POINT('Ctrl Pts',(-17.5562396423716,14.2560736746046,
133.036976545508)) ;
#127241 = CARTESIAN_POINT('Ctrl Pts',(-17.4856556413898,14.4412184345139,
132.797774201954)) ;
#127242 = CARTESIAN_POINT('Ctrl Pts',(-17.4019418945911,14.5543182512014,
132.52014511049)) ;
#127243 = CARTESIAN_POINT('Ctrl Pts',(-17.3116311006331,14.5864671227743,
132.223159968999)) ;
#127244 = CARTESIAN_POINT('Ctrl Pts',(-17.2222810781303,14.5351930421584,
131.929026268783)) ;
#127245 = CARTESIAN_POINT('Ctrl Pts',(-17.1408794351008,14.4042256673591,
131.65810101633)) ;
#127246 = CARTESIAN_POINT('Ctrl Pts',(-17.0740974975755,14.2033620088234,
131.429938282516)) ;
#127247 = CARTESIAN_POINT('Ctrl Pts',(-17.0271797587778,13.9460943123355,
131.25972015051)) ;
#127248 = CARTESIAN_POINT('Ctrl Pts',(-17.0044838482656,13.651094014162,131.160246420146)) ;
#127249 = CARTESIAN_POINT('Ctrl Pts',(-17.0082440978773,13.340963258282,131.138187893648)) ;
#127250 = CARTESIAN_POINT('Ctrl Pts',(-17.0389664768321,13.0355469071403,
131.194763803826)) ;
#127251 = CARTESIAN_POINT('Ctrl Pts',(-17.0951171059167,12.7584810147084,
131.325687533703)) ;
#127252 = CARTESIAN_POINT('Ctrl Pts',(-17.1734699410036,12.5287898592304,
131.521440438767)) ;
#127253 = CARTESIAN_POINT('Ctrl Pts',(-17.2690431091153,12.3633457050948,
131.76752542984)) ;
#127254 = CARTESIAN_POINT('Ctrl Pts',(-17.3757413243156,12.2737023356338,
132.046114426366)) ;
#127255 = CARTESIAN_POINT('Ctrl Pts',(-17.4868753525456,12.2663504555484,
132.337605074947)) ;
#127256 = CARTESIAN_POINT('Ctrl Pts',(-17.594933557408,12.3420801358765,132.620132638066)) ;
#127257 = CARTESIAN_POINT('Ctrl Pts',(-17.6927107918119,12.4946576254463,
132.872726617329)) ;
#127258 = CARTESIAN_POINT('Ctrl Pts',(-17.7746021706281,12.7142649717312,
133.078788363608)) ;
#127259 = CARTESIAN_POINT('Ctrl Pts',(-17.8350304744198,12.9853994961716,
133.222096163646)) ;
#127260 = CARTESIAN_POINT('Ctrl Pts',(-17.8701999131744,13.2860374615536,
133.291826279773)) ;
#127261 = CARTESIAN_POINT('Ctrl Pts',(-17.8787429450958,13.5985522242575,
133.283546361451)) ;
#127262 = CARTESIAN_POINT('Ctrl Pts',(-17.860400130644,13.8975128735152,133.19682396488)) ;
#127263 = CARTESIAN_POINT('Ctrl Pts',(-17.817739731672,14.1612606569833,133.039235284081)) ;
#127264 = CARTESIAN_POINT('Ctrl Pts',(-17.7539424298962,14.3739608476098,
132.819679716885)) ;
#127265 = CARTESIAN_POINT('Ctrl Pts',(-17.6743276947805,14.518294704107,132.553868013413)) ;
#127266 = CARTESIAN_POINT('Ctrl Pts',(-17.5858816850883,14.5834512840226,
132.262389383018)) ;
#127267 = CARTESIAN_POINT('Ctrl Pts',(-17.495671887429,14.5659482192211,131.965871431279)) ;
#127268 = CARTESIAN_POINT('Ctrl Pts',(-17.4102025645197,14.4667697740707,
131.683072426799)) ;
#127269 = CARTESIAN_POINT('Ctrl Pts',(-17.3365053893818,14.2923285700355,
131.434587124343)) ;
#127270 = CARTESIAN_POINT('Ctrl Pts',(-17.2808753696568,14.0548140486651,
131.23883528978)) ;
#127271 = CARTESIAN_POINT('Ctrl Pts',(-17.2482486938309,13.7751054294997,
131.110643536837)) ;
#127272 = CARTESIAN_POINT('Ctrl Pts',(-17.2409723432271,13.4671706932676,
131.056143962947)) ;
#127273 = CARTESIAN_POINT('Ctrl Pts',(-17.2609660776528,13.1566326789877,
131.081373755266)) ;
#127274 = CARTESIAN_POINT('Ctrl Pts',(-17.3068303971445,12.8670308674408,
131.182397606284)) ;
#127275 = CARTESIAN_POINT('Ctrl Pts',(-17.3769423374258,12.6146257445343,
131.353937047391)) ;
#127276 = CARTESIAN_POINT('Ctrl Pts',(-17.4663324172258,12.4216271707414,
131.581933589309)) ;
#127277 = CARTESIAN_POINT('Ctrl Pts',(-17.5689151592292,12.3004936343569,
131.848623819979)) ;
#127278 = CARTESIAN_POINT('Ctrl Pts',(-17.6795235886028,12.2591976943178,
132.138478362093)) ;
#127279 = CARTESIAN_POINT('Ctrl Pts',(-17.7892104427003,12.3014766465694,
132.425902609519)) ;
#127280 = CARTESIAN_POINT('Ctrl Pts',(-17.8921201526179,12.4236752423031,
132.693416377678)) ;
#127281 = CARTESIAN_POINT('Ctrl Pts',(-17.9816733272528,12.6191375568078,
132.921700911216)) ;
#127282 = CARTESIAN_POINT('Ctrl Pts',(-18.0509804191005,12.8707902400354,
133.091098623039)) ;
#127283 = CARTESIAN_POINT('Ctrl Pts',(-18.0966425229612,13.1617413268143,
133.191421711028)) ;
#127284 = CARTESIAN_POINT('Ctrl Pts',(-18.1160955250332,13.4713352737269,
133.215187444689)) ;
#127285 = CARTESIAN_POINT('Ctrl Pts',(-18.1085938517289,13.7785022138413,
133.160099094131)) ;
#127286 = CARTESIAN_POINT('Ctrl Pts',(-18.0753539943821,14.0596469368124,
133.029881338672)) ;
#127287 = CARTESIAN_POINT('Ctrl Pts',(-18.0195475480246,14.2953142567661,
132.833735930946)) ;
#127288 = CARTESIAN_POINT('Ctrl Pts',(-17.9455889588625,14.4689647332084,
132.584457804222)) ;
#127289 = CARTESIAN_POINT('Ctrl Pts',(-17.8599266157843,14.5668407340065,
132.301076581191)) ;
#127290 = CARTESIAN_POINT('Ctrl Pts',(-17.7697656720865,14.5831863615057,
132.004729955571)) ;
#127291 = CARTESIAN_POINT('Ctrl Pts',(-17.6808976127122,14.5160479174659,
131.711817961361)) ;
#127292 = CARTESIAN_POINT('Ctrl Pts',(-17.6020563422739,14.3710573530436,
131.448475490699)) ;
#127293 = CARTESIAN_POINT('Ctrl Pts',(-17.5386862603335,14.1586832186318,
131.230302219222)) ;
#127294 = CARTESIAN_POINT('Ctrl Pts',(-17.4960439142544,13.8924168097658,
131.072530591824)) ;
#127295 = CARTESIAN_POINT('Ctrl Pts',(-17.4782543290687,13.5934590630732,
130.987477632941)) ;
#127296 = CARTESIAN_POINT('Ctrl Pts',(-17.4871300560662,13.2817949508325,
130.980261275632)) ;
#127297 = CARTESIAN_POINT('Ctrl Pts',(-17.5227969121146,12.9807520838768,
131.051361569795)) ;
#127298 = CARTESIAN_POINT('Ctrl Pts',(-17.5832892800494,12.7114088692144,
131.195005608496)) ;
#127299 = CARTESIAN_POINT('Ctrl Pts',(-17.6655555316227,12.4920355710748,
131.402094610911)) ;
#127300 = CARTESIAN_POINT('Ctrl Pts',(-17.763605317929,12.3404092306431,131.655461365325)) ;
#127301 = CARTESIAN_POINT('Ctrl Pts',(-17.8717998624488,12.2658594230555,
131.938374035989)) ;
#127302 = CARTESIAN_POINT('Ctrl Pts',(-17.9828025573186,12.2744067792623,
132.229517358147)) ;
#127303 = CARTESIAN_POINT('Ctrl Pts',(-18.0893965868874,12.3651073701196,
132.507801972934)) ;
#127304 = CARTESIAN_POINT('Ctrl Pts',(-18.1848253344922,12.5316552741645,
132.75344430614)) ;
#127305 = CARTESIAN_POINT('Ctrl Pts',(-18.262910706008,12.7621961418758,132.948410377436)) ;
#127306 = CARTESIAN_POINT('Ctrl Pts',(-18.3187167918841,13.0400249210017,
133.078305446668)) ;
#127307 = CARTESIAN_POINT('Ctrl Pts',(-18.3490238590159,13.3449925039121,
133.133743315381)) ;
#127308 = CARTESIAN_POINT('Ctrl Pts',(-18.3523960346358,13.6560824350963,
133.110438469782)) ;
#127309 = CARTESIAN_POINT('Ctrl Pts',(-18.3293782283672,13.9495230290834,
133.010150889642)) ;
#127310 = CARTESIAN_POINT('Ctrl Pts',(-18.2822975086196,14.2060602053469,
132.839491487932)) ;
#127311 = CARTESIAN_POINT('Ctrl Pts',(-18.2150042015936,14.4068533701998,
132.609701973779)) ;
#127312 = CARTESIAN_POINT('Ctrl Pts',(-18.1335066452029,14.5364834485285,
132.338532395409)) ;
#127313 = CARTESIAN_POINT('Ctrl Pts',(-18.0440812727696,14.5865952297017,
132.044172252159)) ;
#127314 = CARTESIAN_POINT('Ctrl Pts',(-17.9539167615346,14.553289693682,131.747651900659)) ;
#127315 = CARTESIAN_POINT('Ctrl Pts',(-17.8702528974652,14.4391769973074,
131.470146326373)) ;
#127316 = CARTESIAN_POINT('Ctrl Pts',(-17.7997194469578,14.2521193924325,
131.230968722829)) ;
#127317 = CARTESIAN_POINT('Ctrl Pts',(-17.7481700755364,14.0064610013992,
131.04733335877)) ;
#127318 = CARTESIAN_POINT('Ctrl Pts',(-17.719812684897,13.7162751839027,130.931136251967)) ;
#127319 = CARTESIAN_POINT('Ctrl Pts',(-17.7178318605647,13.4088590372776,
130.89242456443)) ;
#127320 = CARTESIAN_POINT('Ctrl Pts',(-17.7426554414359,13.1005339015723,
130.93180097624)) ;
#127321 = CARTESIAN_POINT('Ctrl Pts',(-17.7935721191777,12.8153801442626,
131.04739716275)) ;
#127322 = CARTESIAN_POINT('Ctrl Pts',(-17.8671815808783,12.5742829419459,
131.229393212351)) ;
#127323 = CARTESIAN_POINT('Ctrl Pts',(-17.9602575957707,12.3924207775489,
131.467913394784)) ;
#127324 = CARTESIAN_POINT('Ctrl Pts',(-18.0645711388433,12.2864008537638,
131.739720121866)) ;
#127325 = CARTESIAN_POINT('Ctrl Pts',(-18.1756856987231,12.2608494079679,
132.031060726295)) ;
#127326 = CARTESIAN_POINT('Ctrl Pts',(-18.2845081582116,12.3186106579848,
132.315974866748)) ;
#127327 = CARTESIAN_POINT('Ctrl Pts',(-18.385443297942,12.4554523175926,132.577666349289)) ;
#127328 = CARTESIAN_POINT('Ctrl Pts',(-18.4714425406617,12.6626735352652,
132.79564979499)) ;
#127329 = CARTESIAN_POINT('Ctrl Pts',(-18.5363857643237,12.9221025997255,
132.952420893401)) ;
#127330 = CARTESIAN_POINT('Ctrl Pts',(-18.577483280411,13.2188658748081,133.039325926442)) ;
#127331 = CARTESIAN_POINT('Ctrl Pts',(-18.5918395715828,13.5309969609299,
133.048045174373)) ;
#127332 = CARTESIAN_POINT('Ctrl Pts',(-18.579379357718,13.8333910291505,132.978648701175)) ;
#127333 = CARTESIAN_POINT('Ctrl Pts',(-18.5415509639557,14.1082732516314,
132.834930655177)) ;
#127334 = CARTESIAN_POINT('Ctrl Pts',(-18.4819140851022,14.3332733930533,
132.627591939092)) ;
#127335 = CARTESIAN_POINT('Ctrl Pts',(-18.4054218771447,14.4930899265818,
132.370995081213)) ;
#127336 = CARTESIAN_POINT('Ctrl Pts',(-18.318516382284,14.5762694731203,132.084061324625)) ;
#127337 = CARTESIAN_POINT('Ctrl Pts',(-18.2273640153455,14.5766426477847,
131.784499589454)) ;
#127338 = CARTESIAN_POINT('Ctrl Pts',(-18.1407406750204,14.4950561808568,
131.498537978266)) ;
#127339 = CARTESIAN_POINT('Ctrl Pts',(-18.0637621533931,14.3357812745788,
131.240402844972)) ;
#127340 = CARTESIAN_POINT('Ctrl Pts',(-18.0040164942051,14.1117726317635,
131.032799043462)) ;
#127341 = CARTESIAN_POINT('Ctrl Pts',(-17.9658474460896,13.8385112435954,
130.88819300603)) ;
#127342 = CARTESIAN_POINT('Ctrl Pts',(-17.9529773698967,13.5338962434735,
130.817328335414)) ;
#127343 = CARTESIAN_POINT('Ctrl Pts',(-17.966902192937,13.2242575692473,130.825061227403)) ;
#127344 = CARTESIAN_POINT('Ctrl Pts',(-18.0076010778523,12.9262819012927,
130.910714299643)) ;
#127345 = CARTESIAN_POINT('Ctrl Pts',(-18.0724284818989,12.6654698435916,
131.067059131794)) ;
#127346 = CARTESIAN_POINT('Ctrl Pts',(-18.1584381429643,12.4574146101121,
131.285007474977)) ;
#127347 = CARTESIAN_POINT('Ctrl Pts',(-18.2582335314427,12.3205165550688,
131.543682575533)) ;
#127348 = CARTESIAN_POINT('Ctrl Pts',(-18.3679353654617,12.2610390468186,
131.83086496086)) ;
#127349 = CARTESIAN_POINT('Ctrl Pts',(-18.4782367394613,12.2851065141721,
132.120097103203)) ;
#127350 = CARTESIAN_POINT('Ctrl Pts',(-18.5838705524631,12.3913707511119,
132.395368945134)) ;
#127351 = CARTESIAN_POINT('Ctrl Pts',(-18.6760360416254,12.5705078775683,
132.631617960708)) ;
#127352 = CARTESIAN_POINT('Ctrl Pts',(-18.7502684218209,12.8110530886845,
132.815345268963)) ;
#127353 = CARTESIAN_POINT('Ctrl Pts',(-18.8015583285115,13.0958080980136,
132.932027482214)) ;
#127354 = CARTESIAN_POINT('Ctrl Pts',(-18.8268471368734,13.4043791366155,
132.972713046166)) ;
#127355 = CARTESIAN_POINT('Ctrl Pts',(-18.8252076834743,13.7127503618814,
132.934914084386)) ;
#127356 = CARTESIAN_POINT('Ctrl Pts',(-18.7970965372467,14.0031465413693,
132.819442522481)) ;
#127357 = CARTESIAN_POINT('Ctrl Pts',(-18.7462208827452,14.2480984891944,
132.637984092409)) ;
#127358 = CARTESIAN_POINT('Ctrl Pts',(-18.6756901548005,14.4370589148149,
132.398678768597)) ;
#127359 = CARTESIAN_POINT('Ctrl Pts',(-18.5922636520362,14.5521322470153,
132.121910980458)) ;
#127360 = CARTESIAN_POINT('Ctrl Pts',(-18.5019465438144,14.5867077632741,
131.824868753365)) ;
#127361 = CARTESIAN_POINT('Ctrl Pts',(-18.412633202275,14.5378478961583,131.53090432153)) ;
#127362 = CARTESIAN_POINT('Ctrl Pts',(-18.330920319899,14.4092030329905,131.25907687015)) ;
#127363 = CARTESIAN_POINT('Ctrl Pts',(-18.263569768423,14.2102655256447,131.0292461752)) ;
#127364 = CARTESIAN_POINT('Ctrl Pts',(-18.2158792663467,13.953116489833,130.856624729037)) ;
#127365 = CARTESIAN_POINT('Ctrl Pts',(-18.1925908882483,13.6605445363077,
130.755610904485)) ;
#127366 = CARTESIAN_POINT('Ctrl Pts',(-18.1955599085021,13.3493859858442,
130.731108302227)) ;
#127367 = CARTESIAN_POINT('Ctrl Pts',(-18.225463343713,13.0444135456855,130.785394374056)) ;
#127368 = CARTESIAN_POINT('Ctrl Pts',(-18.2809528308207,12.7658508988887,
130.914341636667)) ;
#127369 = CARTESIAN_POINT('Ctrl Pts',(-18.3586927250528,12.5346698659633,
131.108322839338)) ;
#127370 = CARTESIAN_POINT('Ctrl Pts',(-18.4539903952345,12.3668713025773,
131.35355113485)) ;
#127371 = CARTESIAN_POINT('Ctrl Pts',(-18.5606691035786,12.2750736510529,
131.632027177276)) ;
#127372 = CARTESIAN_POINT('Ctrl Pts',(-18.6712133617814,12.2654123837922,
131.921964147422)) ;
#127373 = CARTESIAN_POINT('Ctrl Pts',(-18.7795370897269,12.3385001121927,
132.205249883484)) ;
#127374 = CARTESIAN_POINT('Ctrl Pts',(-18.8779628205114,12.4893940977294,
132.459650590027)) ;
#127375 = CARTESIAN_POINT('Ctrl Pts',(-18.9602735680414,12.7071835395625,
132.66696984749)) ;
#127376 = CARTESIAN_POINT('Ctrl Pts',(-19.0212463662573,12.9760086815988,
132.811986888924)) ;
#127377 = CARTESIAN_POINT('Ctrl Pts',(-19.0573505327277,13.2771671350434,
132.884317676009)) ;
#127378 = CARTESIAN_POINT('Ctrl Pts',(-19.0666443316968,13.5885363726329,
132.878356779271)) ;
#127379 = CARTESIAN_POINT('Ctrl Pts',(-19.0492100110848,13.8883474938027,
132.794283427)) ;
#127380 = CARTESIAN_POINT('Ctrl Pts',(-19.0070053612913,14.1546797324028,
132.637863556914)) ;
#127381 = CARTESIAN_POINT('Ctrl Pts',(-18.9438705951811,14.3683945164845,
132.420333719808)) ;
#127382 = CARTESIAN_POINT('Ctrl Pts',(-18.8649903948833,14.5146640414989,
132.156794887638)) ;
#127383 = CARTESIAN_POINT('Ctrl Pts',(-18.7764317944818,14.5827891573481,
131.864873053478)) ;
#127384 = CARTESIAN_POINT('Ctrl Pts',(-18.6859695685718,14.5676065967762,
131.567543317184)) ;
#127385 = CARTESIAN_POINT('Ctrl Pts',(-18.6002872834926,14.4706131159399,
131.284128345717)) ;
#127386 = CARTESIAN_POINT('Ctrl Pts',(-18.5263602634957,14.2987449000821,
131.035067449585)) ;
#127387 = CARTESIAN_POINT('Ctrl Pts',(-18.4700659060945,14.063095802434,130.837382283135)) ;
#127388 = CARTESIAN_POINT('Ctrl Pts',(-18.4365708056881,13.7833208359645,
130.706522805611)) ;
#127389 = CARTESIAN_POINT('Ctrl Pts',(-18.4286425713622,13.4754883225496,
130.650088164264)) ;
#127390 = CARTESIAN_POINT('Ctrl Pts',(-18.4476840985486,13.1664272763286,
130.6727229201)) ;
#127391 = CARTESIAN_POINT('Ctrl Pts',(-18.4930612119151,12.8743475214726,
130.772135696503)) ;
#127392 = CARTESIAN_POINT('Ctrl Pts',(-18.5621657253508,12.6220180673462,
130.940924124175)) ;
#127393 = CARTESIAN_POINT('Ctrl Pts',(-18.6511402558302,12.4263341483682,
131.167639758192)) ;
#127394 = CARTESIAN_POINT('Ctrl Pts',(-18.7540070326684,12.302605659073,131.434983940839)) ;
#127395 = CARTESIAN_POINT('Ctrl Pts',(-18.863849205629,12.2593725247806,131.722798446897)) ;
#127396 = CARTESIAN_POINT('Ctrl Pts',(-18.973774779168,12.2987734021689,132.010889389283)) ;
#127397 = CARTESIAN_POINT('Ctrl Pts',(-19.0777342115767,12.4202091773167,
132.281205608139)) ;
#127398 = CARTESIAN_POINT('Ctrl Pts',(-19.1667519677935,12.6117736562181,
132.508295443949)) ;
#127399 = CARTESIAN_POINT('Ctrl Pts',(-19.2370781843148,12.8626551569237,
132.68053965318)) ;
#127400 = CARTESIAN_POINT('Ctrl Pts',(-19.2834369312527,13.1527448320073,
132.782907458416)) ;
#127401 = CARTESIAN_POINT('Ctrl Pts',(-19.3037163223515,13.4624297819909,
132.809050097769)) ;
#127402 = CARTESIAN_POINT('Ctrl Pts',(-19.2969382971085,13.7701810821573,
132.756055702704)) ;
#127403 = CARTESIAN_POINT('Ctrl Pts',(-19.2644749678557,14.0517728376964,
132.628174098256)) ;
#127404 = CARTESIAN_POINT('Ctrl Pts',(-19.2092617891683,14.2892526795151,
132.433742339541)) ;
#127405 = CARTESIAN_POINT('Ctrl Pts',(-19.1357237949252,14.4648240216747,
132.18568928131)) ;
#127406 = CARTESIAN_POINT('Ctrl Pts',(-19.0506014968616,14.5650403080843,
131.903990457871)) ;
#127407 = CARTESIAN_POINT('Ctrl Pts',(-18.9599105479305,14.5837489578772,
131.605878754956)) ;
#127408 = CARTESIAN_POINT('Ctrl Pts',(-18.8716845059285,14.519716790758,131.315155450063)) ;
#127409 = CARTESIAN_POINT('Ctrl Pts',(-18.7918891339899,14.3763314788885,
131.048799530724)) ;
#127410 = CARTESIAN_POINT('Ctrl Pts',(-18.7280288453663,14.1656645339802,
130.829210159184)) ;
#127411 = CARTESIAN_POINT('Ctrl Pts',(-18.6846483717695,13.8999128484359,
130.669191362741)) ;
#127412 = CARTESIAN_POINT('Ctrl Pts',(-18.6662190108552,13.6028235446839,
130.582407931147)) ;
#127413 = CARTESIAN_POINT('Ctrl Pts',(-18.6742464552894,13.291184558806,130.572707258654)) ;
#127414 = CARTESIAN_POINT('Ctrl Pts',(-18.7091131232011,12.9894030516706,
130.641463295222)) ;
#127415 = CARTESIAN_POINT('Ctrl Pts',(-18.7692083838662,12.7177659651588,
130.783807359682)) ;
#127416 = CARTESIAN_POINT('Ctrl Pts',(-18.8508792403486,12.49725897855,130.989207530208)) ;
#127417 = CARTESIAN_POINT('Ctrl Pts',(-18.9482660761094,12.3438957408669,
131.240727643345)) ;
#127418 = CARTESIAN_POINT('Ctrl Pts',(-19.05636616245,12.2668705214432,131.523331846997)) ;
#127419 = CARTESIAN_POINT('Ctrl Pts',(-19.1672657480986,12.2729078136877,
131.814213167649)) ;
#127420 = CARTESIAN_POINT('Ctrl Pts',(-19.2742485294026,12.3614501444855,
132.093578354288)) ;
#127421 = CARTESIAN_POINT('Ctrl Pts',(-19.3698500840989,12.5253315069565,
132.339824187223)) ;
#127422 = CARTESIAN_POINT('Ctrl Pts',(-19.4488726784715,12.75527704082,132.537372789972)) ;
#127423 = CARTESIAN_POINT('Ctrl Pts',(-19.5051561125912,13.0310569738766,
132.668784632231)) ;
#127424 = CARTESIAN_POINT('Ctrl Pts',(-19.5363072236389,13.336121760913,132.726616640379)) ;
#127425 = CARTESIAN_POINT('Ctrl Pts',(-19.5404981195686,13.6463105031288,
132.705820995574)) ;
#127426 = CARTESIAN_POINT('Ctrl Pts',(-19.518114994087,13.942487386476,132.607173328192)) ;
#127427 = CARTESIAN_POINT('Ctrl Pts',(-19.4714777997713,14.2002009126819,
132.437787788337)) ;
#127428 = CARTESIAN_POINT('Ctrl Pts',(-19.4051407217541,14.4015262560108,
132.211010588083)) ;
#127429 = CARTESIAN_POINT('Ctrl Pts',(-19.3237681020821,14.5339054968789,
131.940108509089)) ;
#127430 = CARTESIAN_POINT('Ctrl Pts',(-19.2345252922065,14.5863178640126,
131.646306132299)) ;
#127431 = CARTESIAN_POINT('Ctrl Pts',(-19.1440412498707,14.5553221759541,
131.348765178843)) ;
#127432 = CARTESIAN_POINT('Ctrl Pts',(-19.0601605583772,14.4431215041297,
131.070631058535)) ;
#127433 = CARTESIAN_POINT('Ctrl Pts',(-18.9894132116751,14.2589451929284,
130.830971500932)) ;
#127434 = CARTESIAN_POINT('Ctrl Pts',(-18.937005220446,14.0132050920919,130.644627150308)) ;
#127435 = CARTESIAN_POINT('Ctrl Pts',(-18.9081356286921,13.7264814749198,
130.527228397387)) ;
#127436 = CARTESIAN_POINT('Ctrl Pts',(-18.9052947680092,13.4166671234753,
130.485706040313)) ;
#127437 = CARTESIAN_POINT('Ctrl Pts',(-18.929408442906,13.1090562116308,130.523121657094)) ;
#127438 = CARTESIAN_POINT('Ctrl Pts',(-18.9795705721345,12.82289367226,130.636511356112)) ;
#127439 = CARTESIAN_POINT('Ctrl Pts',(-19.0526557005628,12.5803482566307,
130.816963585608)) ;
#127440 = CARTESIAN_POINT('Ctrl Pts',(-19.1448178981947,12.3971382864686,
131.052964112262)) ;
#127441 = CARTESIAN_POINT('Ctrl Pts',(-19.2493867509754,12.2881794770673,
131.325344156453)) ;
#127442 = CARTESIAN_POINT('Ctrl Pts',(-19.3602648969248,12.2604447735571,
131.616048800621)) ;
#127443 = CARTESIAN_POINT('Ctrl Pts',(-19.4694574725562,12.3158800471475,
131.901978170805)) ;
#127444 = CARTESIAN_POINT('Ctrl Pts',(-19.5708086836812,12.4512316162553,
132.164831500501)) ;
#127445 = CARTESIAN_POINT('Ctrl Pts',(-19.6566330326797,12.6546809483565,
132.382594308953)) ;
#127446 = CARTESIAN_POINT('Ctrl Pts',(-19.7227990938615,12.9147731293523,
132.542666384145)) ;
#127447 = CARTESIAN_POINT('Ctrl Pts',(-19.7643882259244,13.2095559485039,
132.63116114933)) ;
#127448 = CARTESIAN_POINT('Ctrl Pts',(-19.7796070435146,13.5223874270332,
132.642305936428)) ;
#127449 = CARTESIAN_POINT('Ctrl Pts',(-19.7679012234026,13.825017500004,132.575151248593)) ;
#127450 = CARTESIAN_POINT('Ctrl Pts',(-19.7305546086185,14.1019895669497,
132.432709178594)) ;
#127451 = CARTESIAN_POINT('Ctrl Pts',(-19.6717250733561,14.3273312659445,
132.227898463628)) ;
#127452 = CARTESIAN_POINT('Ctrl Pts',(-19.5957391597017,14.4893435493457,
131.972801925455)) ;
#127453 = CARTESIAN_POINT('Ctrl Pts',(-19.5089482125021,14.5749600096558,
131.686164493976)) ;
#127454 = CARTESIAN_POINT('Ctrl Pts',(-19.417900802232,14.5779281254001,131.386950092277)) ;
#127455 = CARTESIAN_POINT('Ctrl Pts',(-19.3308419334919,14.4983365281884,
131.099618335491)) ;
#127456 = CARTESIAN_POINT('Ctrl Pts',(-19.2537905566691,14.3420896185929,
130.841432757655)) ;
#127457 = CARTESIAN_POINT('Ctrl Pts',(-19.1930145272651,14.1180211548404,
130.630556327185)) ;
#127458 = CARTESIAN_POINT('Ctrl Pts',(-19.154480323418,13.8471808602615,130.485062911182)) ;
#127459 = CARTESIAN_POINT('Ctrl Pts',(-19.1407432544812,13.5439413026185,
130.411739692858)) ;
#127460 = CARTESIAN_POINT('Ctrl Pts',(-19.15388806011,13.2331634650753,130.417082866503)) ;
#127461 = CARTESIAN_POINT('Ctrl Pts',(-19.1938580856356,12.9343808446189,
130.500600026674)) ;
#127462 = CARTESIAN_POINT('Ctrl Pts',(-19.2581221044548,12.672197812707,130.655272820994)) ;
#127463 = CARTESIAN_POINT('Ctrl Pts',(-19.3430998639908,12.4632419540624,
130.870384738628)) ;
#127464 = CARTESIAN_POINT('Ctrl Pts',(-19.4431486006855,12.3231158661213,
131.129588810294)) ;
#127465 = CARTESIAN_POINT('Ctrl Pts',(-19.5527011367039,12.2616017897263,
131.416345012905)) ;
#127466 = CARTESIAN_POINT('Ctrl Pts',(-19.6628580182651,12.2833201820527,
131.705210375093)) ;
#127467 = CARTESIAN_POINT('Ctrl Pts',(-19.7685636148286,12.3868877345153,
131.980760889968)) ;
#127468 = CARTESIAN_POINT('Ctrl Pts',(-19.8616044368723,12.5648231371291,
132.219418056293)) ;
#127469 = CARTESIAN_POINT('Ctrl Pts',(-19.9363026361166,12.8039602179339,
132.404522691316)) ;
#127470 = CARTESIAN_POINT('Ctrl Pts',(-19.9881245670103,13.0864729050957,
132.522897300744)) ;
#127471 = CARTESIAN_POINT('Ctrl Pts',(-20.0143271197124,13.3957238460679,
132.566138555961)) ;
#127472 = CARTESIAN_POINT('Ctrl Pts',(-20.0133509573114,13.7038340446914,
132.530324240887)) ;
#127473 = CARTESIAN_POINT('Ctrl Pts',(-19.9863447007775,13.9936201440332,
132.418290739287)) ;
#127474 = CARTESIAN_POINT('Ctrl Pts',(-19.9353998662376,14.2431366555827,
132.236196148023)) ;
#127475 = CARTESIAN_POINT('Ctrl Pts',(-19.8660196038327,14.4318623927357,
132.000605777573)) ;
#127476 = CARTESIAN_POINT('Ctrl Pts',(-19.7823664836586,14.5502397441639,
131.722943739338)) ;
#127477 = CARTESIAN_POINT('Ctrl Pts',(-19.6923571646773,14.5868194745111,
131.426895066885)) ;
#127478 = CARTESIAN_POINT('Ctrl Pts',(-19.6028197002359,14.5403267792944,
131.132230972924)) ;
#127479 = CARTESIAN_POINT('Ctrl Pts',(-19.5208138211862,14.4138414926087,
130.859561159112)) ;
#127480 = CARTESIAN_POINT('Ctrl Pts',(-19.4529603624471,14.2163546967306,
130.62822332568)) ;
#127481 = CARTESIAN_POINT('Ctrl Pts',(-19.404898468416,13.962464783628,130.454747355412)) ;
#127482 = CARTESIAN_POINT('Ctrl Pts',(-19.3806595868205,13.6693367580008,
130.35078618193)) ;
#127483 = CARTESIAN_POINT('Ctrl Pts',(-19.3828689401698,13.3586798418074,
130.324104636)) ;
#127484 = CARTESIAN_POINT('Ctrl Pts',(-19.4120401332624,13.0526929530247,
130.376190283202)) ;
#127485 = CARTESIAN_POINT('Ctrl Pts',(-19.4668451940639,12.7731728077457,
130.503149233202)) ;
#127486 = CARTESIAN_POINT('Ctrl Pts',(-19.5440168549277,12.5404162023862,
130.695468362471)) ;
#127487 = CARTESIAN_POINT('Ctrl Pts',(-19.6387913027967,12.3707607989948,
130.939204508807)) ;
#127488 = CARTESIAN_POINT('Ctrl Pts',(-19.7452133373752,12.2766729601255,
131.216934024696)) ;
#127489 = CARTESIAN_POINT('Ctrl Pts',(-19.8556874181351,12.2643218460961,
131.506684005263)) ;
#127490 = CARTESIAN_POINT('Ctrl Pts',(-19.9649749082845,12.3360206522436,
131.792531104291)) ;
#127491 = CARTESIAN_POINT('Ctrl Pts',(-20.0628344188298,12.4836397048973,
132.045586237291)) ;
#127492 = CARTESIAN_POINT('Ctrl Pts',(-20.1460777106979,12.7003319185399,
132.255494068561)) ;
#127493 = CARTESIAN_POINT('Ctrl Pts',(-20.2076327001099,12.9678917727225,
132.402235467722)) ;
#127494 = CARTESIAN_POINT('Ctrl Pts',(-20.2445186297781,13.2687869300656,
132.476808723273)) ;
#127495 = CARTESIAN_POINT('Ctrl Pts',(-20.2545206843836,13.5800035034693,
132.472934888553)) ;
#127496 = CARTESIAN_POINT('Ctrl Pts',(-20.2378647958217,13.8799729722643,
132.391189049575)) ;
#127497 = CARTESIAN_POINT('Ctrl Pts',(-20.196316210114,14.14769940646,132.236667861987)) ;
#127498 = CARTESIAN_POINT('Ctrl Pts',(-20.1336983474538,14.3632524598664,
132.020637059241)) ;
#127499 = CARTESIAN_POINT('Ctrl Pts',(-20.0549288300243,14.511933585639,131.757324538327)) ;
#127500 = CARTESIAN_POINT('Ctrl Pts',(-19.9666034114372,14.5819602156047,
131.46611590328)) ;
#127501 = CARTESIAN_POINT('Ctrl Pts',(-19.8763877159582,14.5692454320411,
131.169609312389)) ;
#127502 = CARTESIAN_POINT('Ctrl Pts',(-19.7902646702084,14.4742854665662,
130.884826946412)) ;
#127503 = CARTESIAN_POINT('Ctrl Pts',(-19.7161283689557,14.3047439211162,
130.635239983571)) ;
#127504 = CARTESIAN_POINT('Ctrl Pts',(-19.6592322243353,14.0710831127117,
130.435827411304)) ;
#127505 = CARTESIAN_POINT('Ctrl Pts',(-19.62494311501,13.7914036460412,130.302538232877)) ;
#127506 = CARTESIAN_POINT('Ctrl Pts',(-19.6162934482715,13.4850123175133,
130.244106124328)) ;
#127507 = CARTESIAN_POINT('Ctrl Pts',(-19.6344889863082,13.1755843986706,
130.264253212252)) ;
#127508 = CARTESIAN_POINT('Ctrl Pts',(-19.6791913673902,12.8823157698566,
130.361653440408)) ;
#127509 = CARTESIAN_POINT('Ctrl Pts',(-19.7476537533918,12.628436297888,130.528560046345)) ;
#127510 = CARTESIAN_POINT('Ctrl Pts',(-19.8365476312442,12.4304595196238,
130.754910983151)) ;
#127511 = CARTESIAN_POINT('Ctrl Pts',(-19.9382808494003,12.3053999531995,
131.019209738796)) ;
#127512 = CARTESIAN_POINT('Ctrl Pts',(-20.048899562009,12.2593484395974,131.309018103742)) ;
#127513 = CARTESIAN_POINT('Ctrl Pts',(-20.1583951299693,12.2965483924972,
131.596013137775)) ;
#127514 = CARTESIAN_POINT('Ctrl Pts',(-20.2627239903333,12.4156949312687,
131.86738401474)) ;
#127515 = CARTESIAN_POINT('Ctrl Pts',(-20.3521217577948,12.6050470802083,
132.095633239782)) ;
#127516 = CARTESIAN_POINT('Ctrl Pts',(-20.4232557357957,12.8553420969347,
132.270128746928)) ;
#127517 = CARTESIAN_POINT('Ctrl Pts',(-20.4701295915053,13.14294545291,132.374185521651)) ;
#127518 = CARTESIAN_POINT('Ctrl Pts',(-20.4913439775976,13.4543916932758,
132.402838218576)) ;
#127519 = CARTESIAN_POINT('Ctrl Pts',(-20.4852807985954,13.7614619882681,
132.352049896115)) ;
#127520 = CARTESIAN_POINT('Ctrl Pts',(-20.4534599308289,14.0447128123048,
132.225967144145)) ;
#127521 = CARTESIAN_POINT('Ctrl Pts',(-20.3989422258876,14.2828872878416,
132.033662002677)) ;
#127522 = CARTESIAN_POINT('Ctrl Pts',(-20.3261747565817,14.4603132279032,
131.78796988944)) ;
#127523 = CARTESIAN_POINT('Ctrl Pts',(-20.2406405035968,14.5634617408265,
131.504807990948)) ;
#127524 = CARTESIAN_POINT('Ctrl Pts',(-20.1506934552704,14.5844329912441,
131.209131937478)) ;
#127525 = CARTESIAN_POINT('Ctrl Pts',(-20.0617033623463,14.5225343527704,
130.915946521996)) ;
#127526 = CARTESIAN_POINT('Ctrl Pts',(-19.9818420485813,14.3815448492318,
130.649512810055)) ;
#127527 = CARTESIAN_POINT('Ctrl Pts',(-19.917408267804,14.172575531033,130.428222467957)) ;
#127528 = CARTESIAN_POINT('Ctrl Pts',(-19.8735004975879,13.9093041266096,
130.266803762146)) ;
#127529 = CARTESIAN_POINT('Ctrl Pts',(-19.8541245956283,13.6121559231782,
130.177157387992)) ;
#127530 = CARTESIAN_POINT('Ctrl Pts',(-19.8614969291783,13.2990171970743,
130.165379607394)) ;
#127531 = CARTESIAN_POINT('Ctrl Pts',(-19.8955170588464,12.998156604328,130.231820441278)) ;
#127532 = CARTESIAN_POINT('Ctrl Pts',(-19.9547262808423,12.7257033246492,
130.371637346986)) ;
#127533 = CARTESIAN_POINT('Ctrl Pts',(-20.0358807184934,12.5030758718665,
130.57549131059)) ;
#127534 = CARTESIAN_POINT('Ctrl Pts',(-20.1330736628754,12.3471530104355,
130.826374526737)) ;
#127535 = CARTESIAN_POINT('Ctrl Pts',(-20.2413837044624,12.2678408684918,
131.109474408019)) ;
#127536 = CARTESIAN_POINT('Ctrl Pts',(-20.3516515581445,12.2715869144481,
131.398702136902)) ;
#127537 = CARTESIAN_POINT('Ctrl Pts',(-20.458990666618,12.3575775842601,131.679074390523)) ;
#127538 = CARTESIAN_POINT('Ctrl Pts',(-20.5551532672935,12.5198591790598,
131.926895826603)) ;
#127539 = CARTESIAN_POINT('Ctrl Pts',(-20.6345267118374,12.7472700388984,
132.125583684159)) ;
#127540 = CARTESIAN_POINT('Ctrl Pts',(-20.6917801462354,13.0233714187906,
132.259655378351)) ;
#127541 = CARTESIAN_POINT('Ctrl Pts',(-20.7235068742326,13.3264774895314,
132.319332952291)) ;
#127542 = CARTESIAN_POINT('Ctrl Pts',(-20.7285581739825,13.6374828806093,
132.300975805749)) ;
#127543 = CARTESIAN_POINT('Ctrl Pts',(-20.7069127156367,13.9340522489258,
132.204521708848)) ;
#127544 = CARTESIAN_POINT('Ctrl Pts',(-20.6610511580448,14.1931239362593,
132.037428877366)) ;
#127545 = CARTESIAN_POINT('Ctrl Pts',(-20.5947281122293,14.3974304653898,
131.810470473005)) ;
#127546 = CARTESIAN_POINT('Ctrl Pts',(-20.5141569428622,14.5309245418109,
131.542118712394)) ;
#127547 = CARTESIAN_POINT('Ctrl Pts',(-20.4250014415483,14.5859814534191,
131.248544133556)) ;
#127548 = CARTESIAN_POINT('Ctrl Pts',(-20.3346292234116,14.5574777864012,
130.951397195989)) ;
#127549 = CARTESIAN_POINT('Ctrl Pts',(-20.2504020006507,14.448015060185,130.672253823311)) ;
#127550 = CARTESIAN_POINT('Ctrl Pts',(-20.1787236467894,14.2640746959558,
130.429615415799)) ;
#127551 = CARTESIAN_POINT('Ctrl Pts',(-20.1261893612446,14.0222278715719,
130.243229810785)) ;
#127552 = CARTESIAN_POINT('Ctrl Pts',(-20.0963035511799,13.733909228241,130.12255396145)) ;
#127553 = CARTESIAN_POINT('Ctrl Pts',(-20.0928006031125,13.4264443346404,
130.079328393741)) ;
#127554 = CARTESIAN_POINT('Ctrl Pts',(-20.1160876756408,13.1179337320863,
130.114262614734)) ;
#127555 = CARTESIAN_POINT('Ctrl Pts',(-20.1654886895204,12.8308236550973,
130.225443140224)) ;
#127556 = CARTESIAN_POINT('Ctrl Pts',(-20.2383169541712,12.5859821218942,
130.405007728628)) ;
#127557 = CARTESIAN_POINT('Ctrl Pts',(-20.3293570118732,12.4020104650746,
130.637967599986)) ;
#127558 = CARTESIAN_POINT('Ctrl Pts',(-20.4343040706677,12.289987565929,130.911234342623)) ;
#127559 = CARTESIAN_POINT('Ctrl Pts',(-20.5445367265671,12.2601247779834,
131.20023242097)) ;
#127560 = CARTESIAN_POINT('Ctrl Pts',(-20.6540586635509,12.3130229005744,
131.487063615784)) ;
#127561 = CARTESIAN_POINT('Ctrl Pts',(-20.7555473479129,12.4457555473525,
131.750394826563)) ;
#127562 = CARTESIAN_POINT('Ctrl Pts',(-20.8422236062708,12.6478748794645,
131.970533838524)) ;
#127563 = CARTESIAN_POINT('Ctrl Pts',(-20.9091717846165,12.9074235012635,
132.132805273435)) ;
#127564 = CARTESIAN_POINT('Ctrl Pts',(-20.9513915274105,13.2015879263547,
132.223135875189)) ;
#127565 = CARTESIAN_POINT('Ctrl Pts',(-20.9673433799513,13.5132462059268,
132.23653666469)) ;
#127566 = CARTESIAN_POINT('Ctrl Pts',(-20.9563186950524,13.8170404321959,
132.171290910233)) ;
#127567 = CARTESIAN_POINT('Ctrl Pts',(-20.9200063586161,14.0930904001558,
132.032130174702)) ;
#127568 = CARTESIAN_POINT('Ctrl Pts',(-20.8615797598591,14.3215764972773,
131.828327874227)) ;
#127569 = CARTESIAN_POINT('Ctrl Pts',(-20.7857303358652,14.4860164278212,
131.573530686186)) ;
#127570 = CARTESIAN_POINT('Ctrl Pts',(-20.6990544102765,14.573742198897,131.287198957879)) ;
#127571 = CARTESIAN_POINT('Ctrl Pts',(-20.6082663915268,14.5789283396522,
130.988830774591)) ;
#127572 = CARTESIAN_POINT('Ctrl Pts',(-20.5209618564176,14.5018180377366,
130.700774166513)) ;
#127573 = CARTESIAN_POINT('Ctrl Pts',(-20.4433002769759,14.346557147794,130.440665580027)) ;
#127574 = CARTESIAN_POINT('Ctrl Pts',(-20.3826208374421,14.1268974997841,
130.23046053949)) ;
#127575 = CARTESIAN_POINT('Ctrl Pts',(-20.3429550525631,13.8551172342444,
130.081370374509)) ;
#127576 = CARTESIAN_POINT('Ctrl Pts',(-20.3285617380619,13.5530513946411,
130.006211437284)) ;
#127577 = CARTESIAN_POINT('Ctrl Pts',(-20.3409618342516,13.2415864711832,
130.009305157595)) ;
#127578 = CARTESIAN_POINT('Ctrl Pts',(-20.3800377984526,12.9431697313624,
130.090333860656)) ;
#127579 = CARTESIAN_POINT('Ctrl Pts',(-20.4437605734203,12.6789856337564,
130.243341345209)) ;
#127580 = CARTESIAN_POINT('Ctrl Pts',(-20.5281215425679,12.4685393883903,
130.456694343348)) ;
#127581 = CARTESIAN_POINT('Ctrl Pts',(-20.6278006359466,12.3261974816525,
130.714816569821)) ;
#127582 = CARTESIAN_POINT('Ctrl Pts',(-20.7371171183746,12.2622045903834,
131.000906852494)) ;
#127583 = CARTESIAN_POINT('Ctrl Pts',(-20.8475355906631,12.2815898228841,
131.29047054978)) ;
#127584 = CARTESIAN_POINT('Ctrl Pts',(-20.9531780974456,12.3824517560788,
131.565944042244)) ;
#127585 = CARTESIAN_POINT('Ctrl Pts',(-21.0468252428417,12.5585396734663,
131.806317421495)) ;
#127586 = CARTESIAN_POINT('Ctrl Pts',(-21.1220933065646,12.7954954768117,
131.993149661609)) ;
#127587 = CARTESIAN_POINT('Ctrl Pts',(-21.1749898652116,13.0796939956766,
132.114357782116)) ;
#127588 = CARTESIAN_POINT('Ctrl Pts',(-21.2016446674372,13.3852304275537,
132.159287548806)) ;
#127589 = CARTESIAN_POINT('Ctrl Pts',(-21.2015540163802,13.6960444491442,
132.125795477662)) ;
#127590 = CARTESIAN_POINT('Ctrl Pts',(-21.1751743778786,13.9858667293059,
132.015671444373)) ;
#127591 = CARTESIAN_POINT('Ctrl Pts',(-21.1251728129277,14.2358877355362,
131.836479960103)) ;
#127592 = CARTESIAN_POINT('Ctrl Pts',(-21.0559870451211,14.4275999351318,
131.601303111379)) ;
#127593 = CARTESIAN_POINT('Ctrl Pts',(-20.9724777469102,14.5480862866817,
131.324017047238)) ;
#127594 = CARTESIAN_POINT('Ctrl Pts',(-20.8828738981426,14.5868446716621,
131.029266002422)) ;
#127595 = CARTESIAN_POINT('Ctrl Pts',(-20.793319864488,14.5430357669594,130.734593108709)) ;
#127596 = CARTESIAN_POINT('Ctrl Pts',(-20.7108832857753,14.4187440206734,
130.460625240054)) ;
#127597 = CARTESIAN_POINT('Ctrl Pts',(-20.6424522460287,14.2230681613756,
130.227576513237)) ;
#127598 = CARTESIAN_POINT('Ctrl Pts',(-20.5936752517832,13.9697197628044,
130.05191339845)) ;
#127599 = CARTESIAN_POINT('Ctrl Pts',(-20.5688082976389,13.6787523584359,
129.946270287874)) ;
#127600 = CARTESIAN_POINT('Ctrl Pts',(-20.5702148377031,13.3668523124778,
129.917087134561)) ;
#127601 = CARTESIAN_POINT('Ctrl Pts',(-20.5987307960509,13.0606725090592,
129.967279841455)) ;
#127602 = CARTESIAN_POINT('Ctrl Pts',(-20.6526299718924,12.7810811423454,
130.091709533223)) ;
#127603 = CARTESIAN_POINT('Ctrl Pts',(-20.7291627181641,12.5467077639777,
130.282168756974)) ;
#127604 = CARTESIAN_POINT('Ctrl Pts',(-20.8232989589554,12.3750360607571,
130.524096085743)) ;
#127605 = CARTESIAN_POINT('Ctrl Pts',(-20.9301073743537,12.2779852511976,
130.802757831994)) ;
#127606 = CARTESIAN_POINT('Ctrl Pts',(-21.0403994395651,12.2637459485192,
131.092020590387)) ;
#127607 = CARTESIAN_POINT('Ctrl Pts',(-21.1491494132192,12.3321871592446,
131.376524953412)) ;
#127608 = CARTESIAN_POINT('Ctrl Pts',(-21.2482582669085,12.4786899759448,
131.632949826684)) ;
#127609 = CARTESIAN_POINT('Ctrl Pts',(-21.3319658991696,12.6941598777831,
131.84419829175)) ;
#127610 = CARTESIAN_POINT('Ctrl Pts',(-21.393934752169,12.9594897352697,131.992273232436)) ;
#127611 = CARTESIAN_POINT('Ctrl Pts',(-21.4316059764268,13.2597801817525,
132.06913270801)) ;
#127612 = CARTESIAN_POINT('Ctrl Pts',(-21.4423915229943,13.5705932837916,
132.067589188532)) ;
#127613 = CARTESIAN_POINT('Ctrl Pts',(-21.4265327050768,13.8717554022753,
131.988120022536)) ;
#127614 = CARTESIAN_POINT('Ctrl Pts',(-21.3853703707677,14.1416796116284,
131.834580510575)) ;
#127615 = CARTESIAN_POINT('Ctrl Pts',(-21.3236598644603,14.3575208228019,
131.621411940782)) ;
#127616 = CARTESIAN_POINT('Ctrl Pts',(-21.2450552710407,14.5088742490897,
131.358477246909)) ;
#127617 = CARTESIAN_POINT('Ctrl Pts',(-21.1571003571,14.5810485839828,131.068431346942)) ;
#127618 = CARTESIAN_POINT('Ctrl Pts',(-21.0667207705511,14.57070182657,130.771389000615)) ;
#127619 = CARTESIAN_POINT('Ctrl Pts',(-20.9806138390254,14.4785662715794,
130.486765690707)) ;
#127620 = CARTESIAN_POINT('Ctrl Pts',(-20.9054510209352,14.3096046389662,
130.233904652389)) ;
#127621 = CARTESIAN_POINT('Ctrl Pts',(-20.8482642268115,14.0777450263891,
130.033732777931)) ;
#127622 = CARTESIAN_POINT('Ctrl Pts',(-20.8134138256627,13.8001342055984,
129.898917449703)) ;
#127623 = CARTESIAN_POINT('Ctrl Pts',(-20.8039194104589,13.4946153250832,
129.838060557703)) ;
#127624 = CARTESIAN_POINT('Ctrl Pts',(-20.8214390457908,13.1837407036183,
129.856093267552)) ;
#127625 = CARTESIAN_POINT('Ctrl Pts',(-20.8653324231382,12.8901082598339,
129.951191666946)) ;
#127626 = CARTESIAN_POINT('Ctrl Pts',(-20.9336506448477,12.6339160902113,
130.117500460749)) ;
#127627 = CARTESIAN_POINT('Ctrl Pts',(-21.0207516195137,12.4365925755612,
130.339087571425)) ;
#127628 = CARTESIAN_POINT('Ctrl Pts',(-21.1233219210523,12.3075969620248,
130.605430834854)) ;
#127629 = CARTESIAN_POINT('Ctrl Pts',(-21.2328407338124,12.2595413696365,
130.892337856127)) ;
#127630 = CARTESIAN_POINT('Ctrl Pts',(-21.3434469460394,12.294598124244,131.182256793643)) ;
#127631 = CARTESIAN_POINT('Ctrl Pts',(-21.4469834297355,12.4101972582257,
131.451676254649)) ;
#127632 = CARTESIAN_POINT('Ctrl Pts',(-21.537599854355,12.5987159467278,131.683227158455)) ;
#127633 = CARTESIAN_POINT('Ctrl Pts',(-21.6090537188666,12.8461743732165,
131.858838519072)) ;
#127634 = CARTESIAN_POINT('Ctrl Pts',(-21.6571326896814,13.1359262373299,
131.96605982225)) ;
#127635 = CARTESIAN_POINT('Ctrl Pts',(-21.6788474695644,13.4447581486374,
131.996439162296)) ;
#127636 = CARTESIAN_POINT('Ctrl Pts',(-21.673602265646,13.7530929107791,131.947938343351)) ;
#127637 = CARTESIAN_POINT('Ctrl Pts',(-21.6426240443624,14.0362080368137,
131.824455207463)) ;
#127638 = CARTESIAN_POINT('Ctrl Pts',(-21.5886001898267,14.2769559920641,
131.633477987096)) ;
#127639 = CARTESIAN_POINT('Ctrl Pts',(-21.5160865529743,14.4563581826417,
131.388470091183)) ;
#127640 = CARTESIAN_POINT('Ctrl Pts',(-21.431392796522,14.5613193473425,131.107980334053)) ;
#127641 = CARTESIAN_POINT('Ctrl Pts',(-21.3409007771702,14.5851466761501,
130.810490619039)) ;
#127642 = CARTESIAN_POINT('Ctrl Pts',(-21.2517127735891,14.5250094388502,
130.516696471002)) ;
#127643 = CARTESIAN_POINT('Ctrl Pts',(-21.1719209058277,14.3871119239881,
130.250653678118)) ;
#127644 = CARTESIAN_POINT('Ctrl Pts',(-21.1066172396742,14.1786613718342,
130.026624221542)) ;
#127645 = CARTESIAN_POINT('Ctrl Pts',(-21.0622775095093,13.9181922141156,
129.864140105175)) ;
#127646 = CARTESIAN_POINT('Ctrl Pts',(-21.0420566901638,13.6189923508217,
129.771715761541)) ;
#127647 = CARTESIAN_POINT('Ctrl Pts',(-21.0486722738493,13.3089361907061,
129.758056012422)) ;
#127648 = CARTESIAN_POINT('Ctrl Pts',(-21.0820016252292,13.0058325903369,
129.822298008375)) ;
#127649 = CARTESIAN_POINT('Ctrl Pts',(-21.1407902952181,12.7318652754408,
129.960821602405)) ;
#127650 = CARTESIAN_POINT('Ctrl Pts',(-21.2212926096035,12.5082426893396,
130.162837341344)) ;
#127651 = CARTESIAN_POINT('Ctrl Pts',(-21.3177723068254,12.3508732586718,
130.411748644509)) ;
#127652 = CARTESIAN_POINT('Ctrl Pts',(-21.4255147925088,12.269103649341,130.693293438078)) ;
#127653 = CARTESIAN_POINT('Ctrl Pts',(-21.5363349094351,12.2702137268432,
130.983972752155)) ;
#127654 = CARTESIAN_POINT('Ctrl Pts',(-21.6440245158506,12.3542929865281,
131.265319916063)) ;
#127655 = CARTESIAN_POINT('Ctrl Pts',(-21.7402989030464,12.5141176451976,
131.513562592344)) ;
#127656 = CARTESIAN_POINT('Ctrl Pts',(-21.8201848811006,12.739523408871,131.71378207008)) ;
#127657 = CARTESIAN_POINT('Ctrl Pts',(-21.8781683976227,13.0142279275944,
131.850005585261)) ;
#127658 = CARTESIAN_POINT('Ctrl Pts',(-21.9107820680664,13.3177662597612,
131.912168548991)) ;
#127659 = CARTESIAN_POINT('Ctrl Pts',(-21.9165496071981,13.6286637364164,
131.895925722029)) ;
#127660 = CARTESIAN_POINT('Ctrl Pts',(-21.895755349626,13.925291864832,131.802042167994)) ;
#127661 = CARTESIAN_POINT('Ctrl Pts',(-21.8505085895,14.1860949701751,131.636697482391)) ;
#127662 = CARTESIAN_POINT('Ctrl Pts',(-21.7849733875124,14.39173242129,131.412152981576)) ;
#127663 = CARTESIAN_POINT('Ctrl Pts',(-21.704423221989,14.5282787439252,131.143714000168)) ;
#127664 = CARTESIAN_POINT('Ctrl Pts',(-21.6152238330637,14.5855538698207,
130.849950873151)) ;
#127665 = CARTESIAN_POINT('Ctrl Pts',(-21.5250468841582,14.5594424200451,
130.553468394234)) ;
#127666 = CARTESIAN_POINT('Ctrl Pts',(-21.4406201743331,14.4525338341733,
130.273776294927)) ;
#127667 = CARTESIAN_POINT('Ctrl Pts',(-21.3683352223517,14.2704301925612,
130.029318459583)) ;
#127668 = CARTESIAN_POINT('Ctrl Pts',(-21.3151538916505,14.029440480781,129.840972115584)) ;
#127669 = CARTESIAN_POINT('Ctrl Pts',(-21.2846746834487,13.743952252976,129.718772593527)) ;
#127670 = CARTESIAN_POINT('Ctrl Pts',(-21.2802918665529,13.4354033018238,
129.672814580744)) ;
#127671 = CARTESIAN_POINT('Ctrl Pts',(-21.3027839973428,13.1268757888795,
129.705465440526)) ;
#127672 = CARTESIAN_POINT('Ctrl Pts',(-21.3516511623997,12.8380942338867,
129.814985941014)) ;
#127673 = CARTESIAN_POINT('Ctrl Pts',(-21.4234141670206,12.5930207357232,
129.991631283737)) ;
#127674 = CARTESIAN_POINT('Ctrl Pts',(-21.5145447970548,12.406038862873,130.224648155705)) ;
#127675 = CARTESIAN_POINT('Ctrl Pts',(-21.6183299011303,12.2925312371157,
130.494801725081)) ;
#127676 = CARTESIAN_POINT('Ctrl Pts',(-21.729396915745,12.2597001754449,130.785954171696)) ;
#127677 = CARTESIAN_POINT('Ctrl Pts',(-21.8388056410497,12.3104428537015,
131.072530147179)) ;
#127678 = CARTESIAN_POINT('Ctrl Pts',(-21.9407275385059,12.4411375499462,
131.337087912855)) ;
#127679 = CARTESIAN_POINT('Ctrl Pts',(-22.0276878186148,12.6410412531594,
131.558133447522)) ;
#127680 = CARTESIAN_POINT('Ctrl Pts',(-22.0953288876102,12.8990709835383,
131.722434059242)) ;
#127681 = CARTESIAN_POINT('Ctrl Pts',(-22.1383620574179,13.1932158971754,
131.815059128077)) ;
#127682 = CARTESIAN_POINT('Ctrl Pts',(-22.155034431918,13.5039483796779,131.830649183986)) ;
#127683 = CARTESIAN_POINT('Ctrl Pts',(-22.1448038549081,13.8084630012421,
131.767699528723)) ;
#127684 = CARTESIAN_POINT('Ctrl Pts',(-22.109186119241,14.0856215177356,131.630569916654)) ;
#127685 = CARTESIAN_POINT('Ctrl Pts',(-22.0513385084274,14.3156974280267,
131.428460450475)) ;
#127686 = CARTESIAN_POINT('Ctrl Pts',(-21.9760632390203,14.4820692905758,
131.175400152384)) ;
#127687 = CARTESIAN_POINT('Ctrl Pts',(-21.8894445481827,14.5722583385509,
130.88916664676)) ;
#127688 = CARTESIAN_POINT('Ctrl Pts',(-21.7991282105243,14.5801736907429,
130.592348168938)) ;
#127689 = CARTESIAN_POINT('Ctrl Pts',(-21.7109828267676,14.5050113905237,
130.301588988458)) ;
#127690 = CARTESIAN_POINT('Ctrl Pts',(-21.6332169174199,14.3522165397239,
130.04129242342)) ;
#127691 = CARTESIAN_POINT('Ctrl Pts',(-21.5718716896646,14.1339603470577,
129.829082114643)) ;
#127692 = CARTESIAN_POINT('Ctrl Pts',(-21.5316011710367,13.8641113715177,
129.678314299176)) ;
#127693 = CARTESIAN_POINT('Ctrl Pts',(-21.516371458328,13.5616226074544,129.600594418002)) ;
#127694 = CARTESIAN_POINT('Ctrl Pts',(-21.528026070481,13.2502935266874,129.601533510366)) ;
#127695 = CARTESIAN_POINT('Ctrl Pts',(-21.5664271373857,12.9509783477542,
129.680559417768)) ;
#127696 = CARTESIAN_POINT('Ctrl Pts',(-21.6292751697968,12.686394956267,129.831121353527)) ;
#127697 = CARTESIAN_POINT('Ctrl Pts',(-21.71326832387,12.4734606665479,130.043316396619)) ;
#127698 = CARTESIAN_POINT('Ctrl Pts',(-21.81304630685,12.3287824012662,130.301595784484)) ;
#127699 = CARTESIAN_POINT('Ctrl Pts',(-21.9216720916824,12.2629634134795,
130.585834457607)) ;
#127700 = CARTESIAN_POINT('Ctrl Pts',(-22.0323190208263,12.2798963226628,
130.87600840922)) ;
#127701 = CARTESIAN_POINT('Ctrl Pts',(-22.1382631328561,12.3786943874465,
131.152344623819)) ;
#127702 = CARTESIAN_POINT('Ctrl Pts',(-22.2324381892803,12.5532637132079,
131.394210928517)) ;
#127703 = CARTESIAN_POINT('Ctrl Pts',(-22.307930733872,12.7879391796142,131.581823885359)) ;
#127704 = CARTESIAN_POINT('Ctrl Pts',(-22.3614093552365,13.0695371271683,
131.704894335283)) ;
#127705 = CARTESIAN_POINT('Ctrl Pts',(-22.3890801459065,13.3764287043337,
131.752596913402)) ;
#127706 = CARTESIAN_POINT('Ctrl Pts',(-22.3896950038745,13.6873693766845,
131.72117697511)) ;
#127707 = CARTESIAN_POINT('Ctrl Pts',(-22.3640937155925,13.9780097436375,
131.613337884262)) ;
#127708 = CARTESIAN_POINT('Ctrl Pts',(-22.3144461748257,14.2303816884254,
131.435040211327)) ;
#127709 = CARTESIAN_POINT('Ctrl Pts',(-22.2459325294148,14.4229832272402,
131.201951144948)) ;
#127710 = CARTESIAN_POINT('Ctrl Pts',(-22.1629423958746,14.5456071982134,
130.926254854072)) ;
#127711 = CARTESIAN_POINT('Ctrl Pts',(-22.0732786583332,14.5869244372791,
130.631268978178)) ;
#127712 = CARTESIAN_POINT('Ctrl Pts',(-21.9835550064987,14.5454139986495,
130.336078615688)) ;
#127713 = CARTESIAN_POINT('Ctrl Pts',(-21.9007965838892,14.423161531977,130.061157179146)) ;
#127714 = CARTESIAN_POINT('Ctrl Pts',(-21.8320921977162,14.2299646036066,
129.827410664978)) ;
#127715 = CARTESIAN_POINT('Ctrl Pts',(-21.7825910759239,13.9782380445369,
129.64963445589)) ;
#127716 = CARTESIAN_POINT('Ctrl Pts',(-21.7569463800142,13.6869896878631,
129.541595864683)) ;
#127717 = CARTESIAN_POINT('Ctrl Pts',(-21.7575526251693,13.3772462538757,
129.510281572766)) ;
#127718 = CARTESIAN_POINT('Ctrl Pts',(-21.7851625426909,13.0701026679002,
129.557778994613)) ;
#127719 = CARTESIAN_POINT('Ctrl Pts',(-21.838567285868,12.7883758090077,129.680637101522)) ;
#127720 = CARTESIAN_POINT('Ctrl Pts',(-21.9145185360536,12.5524788411572,
129.869403118959)) ;
#127721 = CARTESIAN_POINT('Ctrl Pts',(-22.008423797552,12.3787206196838,130.11059742698)) ;
#127722 = CARTESIAN_POINT('Ctrl Pts',(-22.1143427284911,12.2799428497071,
130.386861315047)) ;
#127723 = CARTESIAN_POINT('Ctrl Pts',(-22.2248374459482,12.262781441409,130.676641434297)) ;
#127724 = CARTESIAN_POINT('Ctrl Pts',(-22.3343454192335,12.3295044155471,
130.963177642968)) ;
#127725 = CARTESIAN_POINT('Ctrl Pts',(-22.4332832043384,12.4735104244077,
131.219259972441)) ;
#127726 = CARTESIAN_POINT('Ctrl Pts',(-22.5172516297272,12.6859035463297,
131.431419830921)) ;
#127727 = CARTESIAN_POINT('Ctrl Pts',(-22.5802700498489,12.9511127833356,
131.58240078474)) ;
#127728 = CARTESIAN_POINT('Ctrl Pts',(-22.6186978514235,13.2510041848706,
131.661446782256)) ;
#127729 = CARTESIAN_POINT('Ctrl Pts',(-22.6302490272601,13.5624347972365,
131.662072128067)) ;
#127730 = CARTESIAN_POINT('Ctrl Pts',(-22.6150771567607,13.8634350892771,
131.584681894005)) ;
#127731 = CARTESIAN_POINT('Ctrl Pts',(-22.5749490142225,14.1332613456827,
131.434354396493)) ;
#127732 = CARTESIAN_POINT('Ctrl Pts',(-22.5133593020274,14.352640956948,131.221284043712)) ;
#127733 = CARTESIAN_POINT('Ctrl Pts',(-22.4352729860133,14.5054039533886,
130.959949323257)) ;
#127734 = CARTESIAN_POINT('Ctrl Pts',(-22.3478811125609,14.5799567622948,
130.671675925426)) ;
#127735 = CARTESIAN_POINT('Ctrl Pts',(-22.2571262594832,14.5723714233898,
130.373415016701)) ;
#127736 = CARTESIAN_POINT('Ctrl Pts',(-22.1705066821009,14.4818104569399,
130.087167993693)) ;
#127737 = CARTESIAN_POINT('Ctrl Pts',(-22.0955412959604,14.3163443098713,
129.835162366206)) ;
#127738 = CARTESIAN_POINT('Ctrl Pts',(-22.0375088402051,14.085912079338,129.632435530077)) ;
#127739 = CARTESIAN_POINT('Ctrl Pts',(-22.0018499381263,13.8088758328653,
129.495197588548)) ;
#127740 = CARTESIAN_POINT('Ctrl Pts',(-21.9916250136062,13.502841633218,129.432098950623)) ;
#127741 = CARTESIAN_POINT('Ctrl Pts',(-22.0082934021031,13.1931031291703,
129.447788449584)) ;
#127742 = CARTESIAN_POINT('Ctrl Pts',(-22.0515574069593,12.8979592502217,
129.540960648325)) ;
#127743 = CARTESIAN_POINT('Ctrl Pts',(-22.1188207375362,12.6415806855276,
129.704364437549)) ;
#127744 = CARTESIAN_POINT('Ctrl Pts',(-22.2060107640497,12.4408172190554,
129.925969921115)) ;
#127745 = CARTESIAN_POINT('Ctrl Pts',(-22.3082900601043,12.3100401605785,
130.191475830034)) ;
#127746 = CARTESIAN_POINT('Ctrl Pts',(-22.4174544888081,12.2598615755304,
130.477414065444)) ;
#127747 = CARTESIAN_POINT('Ctrl Pts',(-22.527907294651,12.2922205439251,130.766961293267)) ;
#127748 = CARTESIAN_POINT('Ctrl Pts',(-22.6322782382144,12.4062484936796,
131.038640430295)) ;
#127749 = CARTESIAN_POINT('Ctrl Pts',(-22.7231027875419,12.5927140648452,
131.270873729385)) ;
#127750 = CARTESIAN_POINT('Ctrl Pts',(-22.7949984498098,12.8381488980971,
131.447846084438)) ;
#127751 = CARTESIAN_POINT('Ctrl Pts',(-22.843787932828,13.1260095389923,131.557242126977)) ;
#127752 = CARTESIAN_POINT('Ctrl Pts',(-22.8664230727776,13.4367097243977,
131.590076325101)) ;
#127753 = CARTESIAN_POINT('Ctrl Pts',(-22.861921411388,13.7438376738668,131.543917878659)) ;
#127754 = CARTESIAN_POINT('Ctrl Pts',(-22.8316397070447,14.0287736481255,
131.42237783867)) ;
#127755 = CARTESIAN_POINT('Ctrl Pts',(-22.778155770167,14.2709621687312,131.232973634128)) ;
#127756 = CARTESIAN_POINT('Ctrl Pts',(-22.7062333019467,14.4520607897228,
130.989750404344)) ;
#127757 = CARTESIAN_POINT('Ctrl Pts',(-22.6216704946962,14.5594794390157,
130.709590559647)) ;
#127758 = CARTESIAN_POINT('Ctrl Pts',(-22.5314212575681,14.5855261762896,
130.412873670548)) ;
#127759 = CARTESIAN_POINT('Ctrl Pts',(-22.4422960022349,14.5283738832722,
130.119356279925)) ;
#127760 = CARTESIAN_POINT('Ctrl Pts',(-22.3616462327386,14.391653643749,129.850584082527)) ;
#127761 = CARTESIAN_POINT('Ctrl Pts',(-22.2962167251037,14.1863633435458,
129.626404074533)) ;
#127762 = CARTESIAN_POINT('Ctrl Pts',(-22.2509351230502,13.9255968705726,
129.460952363105)) ;
#127763 = CARTESIAN_POINT('Ctrl Pts',(-22.230115271223,13.6292801101744,129.367025070917)) ;
#127764 = CARTESIAN_POINT('Ctrl Pts',(-22.2358443462118,13.3179690043923,
129.350624868831)) ;
#127765 = CARTESIAN_POINT('Ctrl Pts',(-22.268461938418,13.0144329118731,129.412800062026)) ;
#127766 = CARTESIAN_POINT('Ctrl Pts',(-22.3263092006397,12.7401667840787,
129.548682574508)) ;
#127767 = CARTESIAN_POINT('Ctrl Pts',(-22.4061509855269,12.5144107338462,
129.748760348764)) ;
#127768 = CARTESIAN_POINT('Ctrl Pts',(-22.5028521991577,12.3540784671315,
129.998111153004)) ;
#127769 = CARTESIAN_POINT('Ctrl Pts',(-22.6098851930669,12.2704506823876,
130.277743640538)) ;
#127770 = CARTESIAN_POINT('Ctrl Pts',(-22.7210593635,12.2689820893059,130.569348124059)) ;
#127771 = CARTESIAN_POINT('Ctrl Pts',(-22.8288745913513,12.3508509488233,
130.85108559455)) ;
#127772 = CARTESIAN_POINT('Ctrl Pts',(-22.9255783208102,12.5086055311564,
131.100573560609)) ;
#127773 = CARTESIAN_POINT('Ctrl Pts',(-23.0062047553353,12.7330676993537,
131.302868223054)) ;
#127774 = CARTESIAN_POINT('Ctrl Pts',(-23.0647146527384,13.0066123960221,
131.440652814153)) ;
#127775 = CARTESIAN_POINT('Ctrl Pts',(-23.0979542086672,13.3082725062707,
131.504787867336)) ;
#127776 = CARTESIAN_POINT('Ctrl Pts',(-23.1045786952682,13.6201712444572,
131.490952868656)) ;
#127777 = CARTESIAN_POINT('Ctrl Pts',(-23.0843643957598,13.9183340301052,
131.39866546306)) ;
#127778 = CARTESIAN_POINT('Ctrl Pts',(-23.0397557463822,14.1797387715242,
131.235247293697)) ;
#127779 = CARTESIAN_POINT('Ctrl Pts',(-22.9749516558702,14.3864986993276,
131.012946095585)) ;
#127780 = CARTESIAN_POINT('Ctrl Pts',(-22.8947964654787,14.5252641571149,
130.745671070089)) ;
#127781 = CARTESIAN_POINT('Ctrl Pts',(-22.8057244267908,14.5851721018435,
130.452271746797)) ;
#127782 = CARTESIAN_POINT('Ctrl Pts',(-22.7149747642661,14.5610669254243,
130.153926197287)) ;
#127783 = CARTESIAN_POINT('Ctrl Pts',(-22.6307834813211,14.4566509961662,
129.875100662719)) ;
#127784 = CARTESIAN_POINT('Ctrl Pts',(-22.5580747125729,14.2771545373181,
129.629455783231)) ;
#127785 = CARTESIAN_POINT('Ctrl Pts',(-22.5040373563515,14.0362065449594,
129.438421285664)) ;
#127786 = CARTESIAN_POINT('Ctrl Pts',(-22.4730618127373,13.7533987258428,
129.314975683587)) ;
#127787 = CARTESIAN_POINT('Ctrl Pts',(-22.4677748338582,13.4441283625548,
129.266255047909)) ;
#127788 = CARTESIAN_POINT('Ctrl Pts',(-22.4897115438146,13.1346408964387,
129.297202552698)) ;
#127789 = CARTESIAN_POINT('Ctrl Pts',(-22.5374240746914,12.8470251714903,
129.403602462889)) ;
#127790 = CARTESIAN_POINT('Ctrl Pts',(-22.6091262891195,12.5984937845751,
129.579801716748)) ;
#127791 = CARTESIAN_POINT('Ctrl Pts',(-22.6993019984946,12.4108688271007,
129.810228777973)) ;
#127792 = CARTESIAN_POINT('Ctrl Pts',(-22.8030088050855,12.2946081104034,
130.080071075194)) ;
#127793 = CARTESIAN_POINT('Ctrl Pts',(-22.9140804384845,12.2594450538074,
130.371216687278)) ;
#127794 = CARTESIAN_POINT('Ctrl Pts',(-23.0236936524705,12.308048143484,130.658359184517)) ;
#127795 = CARTESIAN_POINT('Ctrl Pts',(-23.1255992046416,12.4360760888544,
130.922984180032)) ;
#127796 = CARTESIAN_POINT('Ctrl Pts',(-23.2132516276065,12.6345258024436,
131.145978362189)) ;
#127797 = CARTESIAN_POINT('Ctrl Pts',(-23.2813071846408,12.8902136692482,
131.311612557012)) ;
#127798 = CARTESIAN_POINT('Ctrl Pts',(-23.325204251601,13.1836914998379,131.406732048559)) ;
#127799 = CARTESIAN_POINT('Ctrl Pts',(-23.3427326214628,13.4943233710872,
131.424816929959)) ;
#127800 = CARTESIAN_POINT('Ctrl Pts',(-23.3332319190002,13.8008444309758,
131.363837246129)) ;
#127801 = CARTESIAN_POINT('Ctrl Pts',(-23.2980903408811,14.0793169977329,
131.228040467186)) ;
#127802 = CARTESIAN_POINT('Ctrl Pts',(-23.2410734955542,14.3098744793808,
131.028516471564)) ;
#127803 = CARTESIAN_POINT('Ctrl Pts',(-23.1658736155029,14.4788324369104,
130.775532824613)) ;
#127804 = CARTESIAN_POINT('Ctrl Pts',(-23.079898197243,14.5706779961945,130.491349631505)) ;
#127805 = CARTESIAN_POINT('Ctrl Pts',(-22.989421112829,14.5811216657767,130.193989675222)) ;
#127806 = CARTESIAN_POINT('Ctrl Pts',(-22.9012597147346,14.508299186415,129.903244922961)) ;
#127807 = CARTESIAN_POINT('Ctrl Pts',(-22.8231629825048,14.3580058494818,
129.642018923582)) ;
#127808 = CARTESIAN_POINT('Ctrl Pts',(-22.7610067688908,14.1405257747425,
129.427299582576)) ;
#127809 = CARTESIAN_POINT('Ctrl Pts',(-22.7202146255786,13.8719962112454,
129.275043026832)) ;
#127810 = CARTESIAN_POINT('Ctrl Pts',(-22.7042294788993,13.571629068225,129.1952761277)) ;
#127811 = CARTESIAN_POINT('Ctrl Pts',(-22.7150970762887,13.2591263892434,
129.193790879608)) ;
#127812 = CARTESIAN_POINT('Ctrl Pts',(-22.7526267524281,12.9599152020145,
129.270362472223)) ;
#127813 = CARTESIAN_POINT('Ctrl Pts',(-22.8149940316731,12.693080122514,129.419401646017)) ;
#127814 = CARTESIAN_POINT('Ctrl Pts',(-22.8983825031158,12.478823817929,129.629876557537)) ;
#127815 = CARTESIAN_POINT('Ctrl Pts',(-22.9974758723708,12.3322479297148,
129.886249770476)) ;
#127816 = CARTESIAN_POINT('Ctrl Pts',(-23.1060580485817,12.2636849635138,
130.170316728691)) ;
#127817 = CARTESIAN_POINT('Ctrl Pts',(-23.2170452381193,12.2782423656434,
130.461397665353)) ;
#127818 = CARTESIAN_POINT('Ctrl Pts',(-23.323119274888,12.3748788450642,130.738138642281)) ;
#127819 = CARTESIAN_POINT('Ctrl Pts',(-23.4173862913371,12.5463734718221,
130.980420347811)) ;
#127820 = CARTESIAN_POINT('Ctrl Pts',(-23.4940244074986,12.7810696504838,
131.171144587366)) ;
#127821 = CARTESIAN_POINT('Ctrl Pts',(-23.5479571630979,13.0608633247241,
131.295649840523)) ;
#127822 = CARTESIAN_POINT('Ctrl Pts',(-23.5764346562346,13.3671882747387,
131.345715854469)) ;
#127823 = CARTESIAN_POINT('Ctrl Pts',(-23.5778620636875,13.6783220863787,
131.316677624504)) ;
#127824 = CARTESIAN_POINT('Ctrl Pts',(-23.5529353685211,13.970110064652,131.210766412908)) ;
#127825 = CARTESIAN_POINT('Ctrl Pts',(-23.5041893664155,14.223034525395,131.03524141122)) ;
#127826 = CARTESIAN_POINT('Ctrl Pts',(-23.4358087814074,14.4186168883369,
130.802357638557)) ;
#127827 = CARTESIAN_POINT('Ctrl Pts',(-23.3535062382914,14.5428705869547,
130.528828840875)) ;
#127828 = CARTESIAN_POINT('Ctrl Pts',(-23.2637737223295,14.5869069848455,
130.233565716766)) ;
#127829 = CARTESIAN_POINT('Ctrl Pts',(-23.1740246734248,14.5480013176435,
129.938339046236)) ;
#127830 = CARTESIAN_POINT('Ctrl Pts',(-23.0904931811877,14.4271740770577,
129.660963874949)) ;
#127831 = CARTESIAN_POINT('Ctrl Pts',(-23.0216173815687,14.2362638791343,
129.42683436767)) ;
#127832 = CARTESIAN_POINT('Ctrl Pts',(-22.97149729033,13.9863048386446,129.247280599084)) ;
#127833 = CARTESIAN_POINT('Ctrl Pts',(-22.9451285454645,13.6957298215624,
129.13710573599)) ;
#127834 = CARTESIAN_POINT('Ctrl Pts',(-22.9448828449131,13.3866515753752,
129.103351428825)) ;
#127835 = CARTESIAN_POINT('Ctrl Pts',(-22.9719981332692,13.0771469727204,
129.149182977873)) ;
#127836 = CARTESIAN_POINT('Ctrl Pts',(-23.0243913022096,12.796392103063,129.269316634301)) ;
#127837 = CARTESIAN_POINT('Ctrl Pts',(-23.1000578815261,12.5578779370545,
129.457104362804)) ;
#127838 = CARTESIAN_POINT('Ctrl Pts',(-23.193168555688,12.383073568111,129.696120245286)) ;
#127839 = CARTESIAN_POINT('Ctrl Pts',(-23.2988396055172,12.2815115204251,
129.97164656702)) ;
#127840 = CARTESIAN_POINT('Ctrl Pts',(-23.4100862971625,12.2623682395224,
130.263384452453)) ;
#127841 = CARTESIAN_POINT('Ctrl Pts',(-23.5183860259816,12.3259184217804,
130.546811307489)) ;
#127842 = CARTESIAN_POINT('Ctrl Pts',(-23.6184046272942,12.4680809238775,
130.805840329846)) ;
#127843 = CARTESIAN_POINT('Ctrl Pts',(-23.7030502858861,12.6795623120404,
131.019893309845)) ;
#127844 = CARTESIAN_POINT('Ctrl Pts',(-23.7664918164668,12.9425894685416,
131.17222579836)) ;
#127845 = CARTESIAN_POINT('Ctrl Pts',(-23.8057196011872,13.2417282929866,
131.253609119574)) ;
#127846 = CARTESIAN_POINT('Ctrl Pts',(-23.8180970159282,13.5531902629317,
131.25664309866)) ;
#127847 = CARTESIAN_POINT('Ctrl Pts',(-23.8036286080686,13.8554128204607,
131.181234076418)) ;
#127848 = CARTESIAN_POINT('Ctrl Pts',(-23.7642341023557,14.1261608663375,
131.033092417043)) ;
#127849 = CARTESIAN_POINT('Ctrl Pts',(-23.7028856469184,14.3478084668955,
130.820595747378)) ;
#127850 = CARTESIAN_POINT('Ctrl Pts',(-23.6259266939486,14.5013886643306,
130.562866353902)) ;
#127851 = CARTESIAN_POINT('Ctrl Pts',(-23.5380160909599,14.5792263009218,
130.272795735233)) ;
#127852 = CARTESIAN_POINT('Ctrl Pts',(-23.4474366584794,14.5735423327803,
129.975118371017)) ;
#127853 = CARTESIAN_POINT('Ctrl Pts',(-23.3608254158504,14.4859392223761,
129.688999940543)) ;
#127854 = CARTESIAN_POINT('Ctrl Pts',(-23.2849259341146,14.32102399054,129.434009796257)) ;
#127855 = CARTESIAN_POINT('Ctrl Pts',(-23.2267844317318,14.0938129483377,
129.231217994417)) ;
#127856 = CARTESIAN_POINT('Ctrl Pts',(-23.1902647637919,13.8165579803482,
129.091295361189)) ;
#127857 = CARTESIAN_POINT('Ctrl Pts',(-23.1792948148417,13.5127264652926,
129.026216186509)) ;
#127858 = CARTESIAN_POINT('Ctrl Pts',(-23.1954081556563,13.2000971837,129.039978991797)) ;
#127859 = CARTESIAN_POINT('Ctrl Pts',(-23.2375272937591,12.9073427141145,
129.130166593091)) ;
#127860 = CARTESIAN_POINT('Ctrl Pts',(-23.3044251896452,12.6479572594797,
129.292307415425)) ;
#127861 = CARTESIAN_POINT('Ctrl Pts',(-23.3908615355677,12.4461100388149,
129.511823532986)) ;
#127862 = CARTESIAN_POINT('Ctrl Pts',(-23.4928607963202,12.3127706272653,
129.776477891717)) ;
#127863 = CARTESIAN_POINT('Ctrl Pts',(-23.602008442908,12.2601401090579,130.06233625634)) ;
#127864 = CARTESIAN_POINT('Ctrl Pts',(-23.7125630788762,12.2901733213181,
130.352170428386)) ;
#127865 = CARTESIAN_POINT('Ctrl Pts',(-23.8170338930274,12.4015833019759,
130.624208061731)) ;
#127866 = CARTESIAN_POINT('Ctrl Pts',(-23.9085880633688,12.586648376757,130.858472179333)) ;
#127867 = CARTESIAN_POINT('Ctrl Pts',(-23.9810480513961,12.8302723293176,
131.037137178046)) ;
#127868 = CARTESIAN_POINT('Ctrl Pts',(-24.0307108386532,13.1192440292328,
131.148863734522)) ;
#127869 = CARTESIAN_POINT('Ctrl Pts',(-24.0538260173367,13.4254781947616,
131.183551991699)) ;
#127870 = CARTESIAN_POINT('Ctrl Pts',(-24.0502594742195,13.73535968212,131.139866666903)) ;
#127871 = CARTESIAN_POINT('Ctrl Pts',(-24.0206309578773,14.0210481979202,
131.020256948829)) ;
#127872 = CARTESIAN_POINT('Ctrl Pts',(-23.9677020137862,14.2649914654817,
130.832435384233)) ;
#127873 = CARTESIAN_POINT('Ctrl Pts',(-23.8963530256599,14.4476746957159,
130.590949554297)) ;
#127874 = CARTESIAN_POINT('Ctrl Pts',(-23.8121017373058,14.5574099985375,
130.311706751319)) ;
#127875 = CARTESIAN_POINT('Ctrl Pts',(-23.7218925496199,14.5860647518339,
130.015099966965)) ;
#127876 = CARTESIAN_POINT('Ctrl Pts',(-23.6322614174443,14.5307819376324,
129.719958907671)) ;
#127877 = CARTESIAN_POINT('Ctrl Pts',(-23.5517321495787,14.3969445347875,
129.451729386716)) ;
#127878 = CARTESIAN_POINT('Ctrl Pts',(-23.4855198577195,14.1927449402103,
129.225129973419)) ;
#127879 = CARTESIAN_POINT('Ctrl Pts',(-23.439751943325,13.9340124552338,129.058360127469)) ;
#127880 = CARTESIAN_POINT('Ctrl Pts',(-23.4181259338223,13.638112171606,128.962032739013)) ;
#127881 = CARTESIAN_POINT('Ctrl Pts',(-23.4230787477534,13.3270743083993,
128.94338373326)) ;
#127882 = CARTESIAN_POINT('Ctrl Pts',(-23.4549668538357,13.0225106928389,
129.003376011957)) ;
#127883 = CARTESIAN_POINT('Ctrl Pts',(-23.5123117766841,12.7468020423806,
129.137735089545)) ;
#127884 = CARTESIAN_POINT('Ctrl Pts',(-23.5911924067347,12.520588791344,129.335174272644)) ;
#127885 = CARTESIAN_POINT('Ctrl Pts',(-23.6874775426794,12.3578209708367,
129.583292114684)) ;
#127886 = CARTESIAN_POINT('Ctrl Pts',(-23.7945910392982,12.2716454872787,
129.863072070572)) ;
#127887 = CARTESIAN_POINT('Ctrl Pts',(-23.9056421843192,12.26795429664,130.154349589356)) ;
#127888 = CARTESIAN_POINT('Ctrl Pts',(-24.0133024715846,12.3469221787347,
130.435753067591)) ;
#127889 = CARTESIAN_POINT('Ctrl Pts',(-24.1107977682431,12.5030898153774,
130.687423495081)) ;
#127890 = CARTESIAN_POINT('Ctrl Pts',(-24.1916810620096,12.725018199882,130.890594344483)) ;
#127891 = CARTESIAN_POINT('Ctrl Pts',(-24.2510283580468,12.997182809166,131.030820292085)) ;
#127892 = CARTESIAN_POINT('Ctrl Pts',(-24.2851967719419,13.2997828332168,
131.097506231202)) ;
#127893 = CARTESIAN_POINT('Ctrl Pts',(-24.2925138699755,13.6108910238796,
131.085784821839)) ;
#127894 = CARTESIAN_POINT('Ctrl Pts',(-24.2732507948885,13.9087323450299,
130.996403294879)) ;
#127895 = CARTESIAN_POINT('Ctrl Pts',(-24.2292529784254,14.1725576107312,
130.834655232453)) ;
#127896 = CARTESIAN_POINT('Ctrl Pts',(-24.1648088256482,14.3815587835512,
130.613331131915)) ;
#127897 = CARTESIAN_POINT('Ctrl Pts',(-24.0850031771026,14.522329585323,130.34708336163)) ;
#127898 = CARTESIAN_POINT('Ctrl Pts',(-23.9963495919697,14.5844939655697,
130.055002294867)) ;
#127899 = CARTESIAN_POINT('Ctrl Pts',(-23.9055571285422,14.5631534313931,
129.756539085882)) ;
#127900 = CARTESIAN_POINT('Ctrl Pts',(-23.8207486179396,14.4606751117259,
129.475779639024)) ;
#127901 = CARTESIAN_POINT('Ctrl Pts',(-23.7476052970787,14.2826954166288,
129.22883457488)) ;
#127902 = CARTESIAN_POINT('Ctrl Pts',(-23.6932165752473,14.0447463561046,
129.036960257282)) ;
#127903 = CARTESIAN_POINT('Ctrl Pts',(-23.6613458241508,13.7613771216005,
128.9107117013)) ;
#127904 = CARTESIAN_POINT('Ctrl Pts',(-23.6553469120595,13.4542323350155,
128.860103266821)) ;
#127905 = CARTESIAN_POINT('Ctrl Pts',(-23.6763806836081,13.1437994657192,
128.888346071975)) ;
#127906 = CARTESIAN_POINT('Ctrl Pts',(-23.7237152114361,12.8538469194028,
128.993465947334)) ;
#127907 = CARTESIAN_POINT('Ctrl Pts',(-23.7944141862397,12.6054873478473,
129.166932874837)) ;
#127908 = CARTESIAN_POINT('Ctrl Pts',(-23.8841019581323,12.4153273189239,
129.395903874998)) ;
#127909 = CARTESIAN_POINT('Ctrl Pts',(-23.988399633529,12.2964112456076,129.667208190599)) ;
#127910 = CARTESIAN_POINT('Ctrl Pts',(-24.0981665990773,12.2594155903617,
129.954911925008)) ;
#127911 = CARTESIAN_POINT('Ctrl Pts',(-24.2083351517853,12.3053349430094,
130.24354607889)) ;
#127912 = CARTESIAN_POINT('Ctrl Pts',(-24.3105348444765,12.431225904051,130.509039975804)) ;
#127913 = CARTESIAN_POINT('Ctrl Pts',(-24.3987955308139,12.6279597128561,
130.733773861238)) ;
#127914 = CARTESIAN_POINT('Ctrl Pts',(-24.4674982287085,12.8824932881055,
130.901278513894)) ;
#127915 = CARTESIAN_POINT('Ctrl Pts',(-24.5120404655204,13.1745455481659,
130.998350424472)) ;
#127916 = CARTESIAN_POINT('Ctrl Pts',(-24.5304051673806,13.4851755770177,
131.018859009724)) ;
#127917 = CARTESIAN_POINT('Ctrl Pts',(-24.5216421560698,13.7921379427258,
130.960030715897)) ;
#127918 = CARTESIAN_POINT('Ctrl Pts',(-24.4874090511905,14.0710147871215,
130.826992612308)) ;
#127919 = CARTESIAN_POINT('Ctrl Pts',(-24.4305784964973,14.3045452092941,
130.627796028043)) ;
#127920 = CARTESIAN_POINT('Ctrl Pts',(-24.3565159379346,14.4740866003594,
130.378447984024)) ;
#127921 = CARTESIAN_POINT('Ctrl Pts',(-24.2702543034482,14.5693022408221,
130.093202410812)) ;
#127922 = CARTESIAN_POINT('Ctrl Pts',(-24.1798204674234,14.5820126324711,
129.79598471706)) ;
#127923 = CARTESIAN_POINT('Ctrl Pts',(-24.0912634781252,14.5112271142504,
129.503993434432)) ;
#127924 = CARTESIAN_POINT('Ctrl Pts',(-24.0131302168525,14.3635591504594,
129.242799204596)) ;
#127925 = CARTESIAN_POINT('Ctrl Pts',(-23.9503807773228,14.147953964214,129.026340635967)) ;
#127926 = CARTESIAN_POINT('Ctrl Pts',(-23.9088544481149,13.88065471692,128.871932632537)) ;
#127927 = CARTESIAN_POINT('Ctrl Pts',(-23.8920756438526,13.5796273902736,
128.789707331385)) ;
#127928 = CARTESIAN_POINT('Ctrl Pts',(-23.9022581492905,13.2675902134212,
128.786271223279)) ;
#127929 = CARTESIAN_POINT('Ctrl Pts',(-23.9389132296133,12.9685392965924,
128.860377903106)) ;
#127930 = CARTESIAN_POINT('Ctrl Pts',(-24.0006495136898,12.7001827589766,
129.007541244204)) ;
#127931 = CARTESIAN_POINT('Ctrl Pts',(-24.0833864908175,12.4843513873254,
129.216152177106)) ;
#127932 = CARTESIAN_POINT('Ctrl Pts',(-24.1822650759013,12.3354377885734,
129.471842874753)) ;
#127933 = CARTESIAN_POINT('Ctrl Pts',(-24.2903495731683,12.2645466561417,
129.754554666612)) ;
#127934 = CARTESIAN_POINT('Ctrl Pts',(-24.4018767251112,12.2767400465521,
130.047057632449)) ;
#127935 = CARTESIAN_POINT('Ctrl Pts',(-24.5078077262226,12.3708038942679,
130.323503077836)) ;
#127936 = CARTESIAN_POINT('Ctrl Pts',(-24.6026999902857,12.540571419273,130.567539761247)) ;
#127937 = CARTESIAN_POINT('Ctrl Pts',(-24.6796997232066,12.7727636471261,
130.759437881883)) ;
#127938 = CARTESIAN_POINT('Ctrl Pts',(-24.7347272254126,13.0532482388654,
130.88692702108)) ;
#127939 = CARTESIAN_POINT('Ctrl Pts',(-24.7637896702919,13.3594503778047,
130.938680040336)) ;
#127940 = CARTESIAN_POINT('Ctrl Pts',(-24.7659951782845,13.6687250636368,
130.912133764155)) ;
#127941 = CARTESIAN_POINT('Ctrl Pts',(-24.7417954210052,13.9622484171183,
130.808248655707)) ;
#127942 = CARTESIAN_POINT('Ctrl Pts',(-24.6937033542677,14.2163837288721,
130.634658424453)) ;
#127943 = CARTESIAN_POINT('Ctrl Pts',(-24.6256339881966,14.4143549429609,
130.402596636616)) ;
#127944 = CARTESIAN_POINT('Ctrl Pts',(-24.5436158358015,14.5404303833534,
130.12990348296)) ;
#127945 = CARTESIAN_POINT('Ctrl Pts',(-24.4543794560575,14.5868747915152,
129.836232596245)) ;
#127946 = CARTESIAN_POINT('Ctrl Pts',(-24.3640228701984,14.5499212466532,
129.539030418213)) ;
#127947 = CARTESIAN_POINT('Ctrl Pts',(-24.280896141805,14.4324626296397,129.263132296661)) ;
#127948 = CARTESIAN_POINT('Ctrl Pts',(-24.2108898214641,14.2419356946445,
129.025401963845)) ;
#127949 = CARTESIAN_POINT('Ctrl Pts',(-24.1604214713888,13.9939564786199,
128.844943866652)) ;
#127950 = CARTESIAN_POINT('Ctrl Pts',(-24.1332885043249,13.7043181806052,
128.732534256686)) ;
#127951 = CARTESIAN_POINT('Ctrl Pts',(-24.1323414963115,13.3953697990708,
128.696719141255)) ;
#127952 = CARTESIAN_POINT('Ctrl Pts',(-24.158488653808,13.0868083993376,128.739872370214)) ;
#127953 = CARTESIAN_POINT('Ctrl Pts',(-24.2104044223131,12.8035341762303,
128.858438904681)) ;
#127954 = CARTESIAN_POINT('Ctrl Pts',(-24.2853987784994,12.5639567579486,
129.044317559609)) ;
#127955 = CARTESIAN_POINT('Ctrl Pts',(-24.3782440503395,12.3867441444795,
129.282492155211)) ;
#127956 = CARTESIAN_POINT('Ctrl Pts',(-24.4838725815493,12.2832559742793,
129.557840662036)) ;
#127957 = CARTESIAN_POINT('Ctrl Pts',(-24.5941053818413,12.2616345635869,
129.846906977435)) ;
#127958 = CARTESIAN_POINT('Ctrl Pts',(-24.7034456841776,12.3231638748032,
130.133102368156)) ;
#127959 = CARTESIAN_POINT('Ctrl Pts',(-24.8033441928373,12.4627499804897,
130.391934160841)) ;
#127960 = CARTESIAN_POINT('Ctrl Pts',(-24.8887683921659,12.6729053346686,
130.608167335739)) ;
#127961 = CARTESIAN_POINT('Ctrl Pts',(-24.9527937676412,12.9344260025205,
130.762243391538)) ;
#127962 = CARTESIAN_POINT('Ctrl Pts',(-24.9928526876402,13.2340774716611,
130.845923250404)) ;
#127963 = CARTESIAN_POINT('Ctrl Pts',(-25.005863736651,13.5439038566318,130.850977779988)) ;
#127964 = CARTESIAN_POINT('Ctrl Pts',(-24.9922543333113,13.8465581380597,
130.778099436776)) ;
#127965 = CARTESIAN_POINT('Ctrl Pts',(-24.9535025647549,14.1188039564303,
130.631797082968)) ;
#127966 = CARTESIAN_POINT('Ctrl Pts',(-24.8928191741207,14.3420290763671,
130.421283969974)) ;
#127967 = CARTESIAN_POINT('Ctrl Pts',(-24.8160182494298,14.4980360356998,
130.163918366139)) ;
#127968 = CARTESIAN_POINT('Ctrl Pts',(-24.7287353277153,14.5780642406309,
129.875843754235)) ;
#127969 = CARTESIAN_POINT('Ctrl Pts',(-24.637437547289,14.574764467068,129.575805260189)) ;
#127970 = CARTESIAN_POINT('Ctrl Pts',(-24.5511068206059,14.4895501192037,
129.29068562796)) ;
#127971 = CARTESIAN_POINT('Ctrl Pts',(-24.4749030425151,14.3274511862454,
129.034880720137)) ;
#127972 = CARTESIAN_POINT('Ctrl Pts',(-24.4159592227421,14.1012131862614,
128.829634055848)) ;
#127973 = CARTESIAN_POINT('Ctrl Pts',(-24.3787401330336,13.8249844629114,
128.687661505586)) ;
#127974 = CARTESIAN_POINT('Ctrl Pts',(-24.3670602425512,13.5214321679055,
128.620482163558)) ;
#127975 = CARTESIAN_POINT('Ctrl Pts',(-24.3822219174402,13.2103012172843,
128.631642932602)) ;
#127976 = CARTESIAN_POINT('Ctrl Pts',(-24.4237994899699,12.914853162699,128.720037352722)) ;
#127977 = CARTESIAN_POINT('Ctrl Pts',(-24.4901243602526,12.6543477666719,
128.880514172549)) ;
#127978 = CARTESIAN_POINT('Ctrl Pts',(-24.5759154007368,12.4511188727926,
129.098200503442)) ;
#127979 = CARTESIAN_POINT('Ctrl Pts',(-24.677341344801,12.3156705463735,129.36124902759)) ;
#127980 = CARTESIAN_POINT('Ctrl Pts',(-24.7868457011832,12.2603783295909,
129.648000508501)) ;
#127981 = CARTESIAN_POINT('Ctrl Pts',(-24.897405454224,12.2883877263298,129.937866175656)) ;
#127982 = CARTESIAN_POINT('Ctrl Pts',(-25.0017261192026,12.396958257867,130.2096033973)) ;
#127983 = CARTESIAN_POINT('Ctrl Pts',(-25.0940920844729,12.5805839699868,
130.446125385117)) ;
#127984 = CARTESIAN_POINT('Ctrl Pts',(-25.166956841923,12.8225431227576,130.62601982101)) ;
#127985 = CARTESIAN_POINT('Ctrl Pts',(-25.2172418557937,13.1085293602937,
130.739774451968)) ;
#127986 = CARTESIAN_POINT('Ctrl Pts',(-25.2413929556375,13.4184312850536,
130.777054839255)) ;
#127987 = CARTESIAN_POINT('Ctrl Pts',(-25.2385539434156,13.725396858395,130.73584896447)) ;
#127988 = CARTESIAN_POINT('Ctrl Pts',(-25.2095431304425,14.0140710244904,
130.617811479396)) ;
#127989 = CARTESIAN_POINT('Ctrl Pts',(-25.1572824387476,14.2586953063536,
130.432036477139)) ;
#127990 = CARTESIAN_POINT('Ctrl Pts',(-25.0863214415307,14.4435712353924,
130.191639130538)) ;
#127991 = CARTESIAN_POINT('Ctrl Pts',(-25.0023566464057,14.5554638044199,
129.913246807571)) ;
#127992 = CARTESIAN_POINT('Ctrl Pts',(-24.9121278134356,14.5862678502014,
129.616544620099)) ;
#127993 = CARTESIAN_POINT('Ctrl Pts',(-24.8229602070216,14.5339455357937,
129.322988050977)) ;
#127994 = CARTESIAN_POINT('Ctrl Pts',(-24.7416470766687,14.4019055778879,
129.052297983318)) ;
#127995 = CARTESIAN_POINT('Ctrl Pts',(-24.6750091878945,14.1996929646046,
128.824495532666)) ;
#127996 = CARTESIAN_POINT('Ctrl Pts',(-24.6284968285961,13.9418840250199,
128.655489614543)) ;
#127997 = CARTESIAN_POINT('Ctrl Pts',(-24.6061667098172,13.6467946138759,
128.557116414343)) ;
#127998 = CARTESIAN_POINT('Ctrl Pts',(-24.6103571111199,13.3358858072713,
128.536238086489)) ;
#127999 = CARTESIAN_POINT('Ctrl Pts',(-24.6414467209892,13.0311284107843,
128.593934068535)) ;
#128000 = CARTESIAN_POINT('Ctrl Pts',(-24.6980852187812,12.7543595776973,
128.726232777758)) ;
#128001 = CARTESIAN_POINT('Ctrl Pts',(-24.7762983426224,12.5263864421984,
128.921740016822)) ;
#128002 = CARTESIAN_POINT('Ctrl Pts',(-24.8729692419651,12.360701809008,129.170730735271)) ;
#128003 = CARTESIAN_POINT('Ctrl Pts',(-24.9789044892542,12.2732420187478,
129.447377219646)) ;
#128004 = CARTESIAN_POINT('Ctrl Pts',(-25.0903755269925,12.2668291176247,
129.739745721998)) ;
#128005 = CARTESIAN_POINT('Ctrl Pts',(-25.1981552719378,12.3436152080196,
130.021521791637)) ;
#128006 = CARTESIAN_POINT('Ctrl Pts',(-25.2961464818128,12.4979167345461,
130.274599644604)) ;
#128007 = CARTESIAN_POINT('Ctrl Pts',(-25.3774937525285,12.7181780575431,
130.47914395372)) ;
#128008 = CARTESIAN_POINT('Ctrl Pts',(-25.4374226974674,12.9887184060059,
130.621122559274)) ;
#128009 = CARTESIAN_POINT('Ctrl Pts',(-25.4723758382109,13.2908826927602,
130.690083038664)) ;
#128010 = CARTESIAN_POINT('Ctrl Pts',(-25.4804804344778,13.6021683784905,
130.680651142204)) ;
#128011 = CARTESIAN_POINT('Ctrl Pts',(-25.4618568415719,13.9015373279121,
130.593040688394)) ;
#128012 = CARTESIAN_POINT('Ctrl Pts',(-25.4184566237588,14.1661757603649,
130.433070382521)) ;
#128013 = CARTESIAN_POINT('Ctrl Pts',(-25.3547428693436,14.3763136740977,
130.213982932893)) ;
#128014 = CARTESIAN_POINT('Ctrl Pts',(-25.2750987849152,14.519537909018,129.948127317248)) ;
#128015 = CARTESIAN_POINT('Ctrl Pts',(-25.1868226991851,14.5837467731856,
129.657234324434)) ;
#128016 = CARTESIAN_POINT('Ctrl Pts',(-25.0960577100225,14.5651055600629,
129.358881947955)) ;
#128017 = CARTESIAN_POINT('Ctrl Pts',(-25.0107197946272,14.4645028782859,
129.076465778453)) ;
#128018 = CARTESIAN_POINT('Ctrl Pts',(-24.937386896527,14.2890439916082,128.829076935974)) ;
#128019 = CARTESIAN_POINT('Ctrl Pts',(-24.8823176595351,14.0526944829589,
128.635198343514)) ;
#128020 = CARTESIAN_POINT('Ctrl Pts',(-24.8497013606514,13.7699865905546,
128.506730368574)) ;
#128021 = CARTESIAN_POINT('Ctrl Pts',(-24.8428940134075,13.4631529317897,
128.453754283766)) ;
#128022 = CARTESIAN_POINT('Ctrl Pts',(-24.8633570486409,13.1513621002968,
128.480200728338)) ;
#128023 = CARTESIAN_POINT('Ctrl Pts',(-24.9095615347108,12.8627668300252,
128.582285450555)) ;
#128024 = CARTESIAN_POINT('Ctrl Pts',(-24.9801882856006,12.6109028722605,
128.755266775312)) ;
#128025 = CARTESIAN_POINT('Ctrl Pts',(-25.0690534743675,12.4200193070119,
128.981995044836)) ;
#128026 = CARTESIAN_POINT('Ctrl Pts',(-25.1730899556213,12.2986947240349,
129.25251180551)) ;
#128027 = CARTESIAN_POINT('Ctrl Pts',(-25.2826141954889,12.2592723923921,
129.539555750781)) ;
#128028 = CARTESIAN_POINT('Ctrl Pts',(-25.3932290191672,12.3030853474788,
129.829385193708)) ;
#128029 = CARTESIAN_POINT('Ctrl Pts',(-25.4952065717163,12.4259705775221,
130.094414362096)) ;
#128030 = CARTESIAN_POINT('Ctrl Pts',(-25.584551513735,12.6220549960923,130.322094334834)) ;
#128031 = CARTESIAN_POINT('Ctrl Pts',(-25.653592832138,12.8744669266435,130.490706005762)) ;
#128032 = CARTESIAN_POINT('Ctrl Pts',(-25.6989762677483,13.1663405887179,
130.590157332786)) ;
#128033 = CARTESIAN_POINT('Ctrl Pts',(-25.7179831336094,13.4758788590996,
130.612636803496)) ;
#128034 = CARTESIAN_POINT('Ctrl Pts',(-25.7101797421068,13.7823952671727,
130.556721850523)) ;
#128035 = CARTESIAN_POINT('Ctrl Pts',(-25.6763506271671,14.0644181714752,
130.424604261457)) ;
#128036 = CARTESIAN_POINT('Ctrl Pts',(-25.6205406548785,14.2977471019388,
130.228651586956)) ;
#128037 = CARTESIAN_POINT('Ctrl Pts',(-25.5464475856731,14.4706193874242,
129.978984296464)) ;
#128038 = CARTESIAN_POINT('Ctrl Pts',(-25.460677945702,14.5675955014972,129.695290809472)) ;
#128039 = CARTESIAN_POINT('Ctrl Pts',(-25.3702300380859,14.5827756049051,
129.398006359781)) ;
#128040 = CARTESIAN_POINT('Ctrl Pts',(-25.2818560211881,14.5148008720864,
129.106690050431)) ;
#128041 = CARTESIAN_POINT('Ctrl Pts',(-25.2030490646069,14.3692243405837,
128.843429932205)) ;
#128042 = CARTESIAN_POINT('Ctrl Pts',(-25.1395076712243,14.1540994987709,
128.624494501162)) ;
#128043 = CARTESIAN_POINT('Ctrl Pts',(-25.0975798520609,13.8891946725912,
128.469071398168)) ;
#128044 = CARTESIAN_POINT('Ctrl Pts',(-25.0799823163942,13.5894849367596,
128.384515560491)) ;
#128045 = CARTESIAN_POINT('Ctrl Pts',(-25.089317375755,13.2771022770821,128.3785662278)) ;
#128046 = CARTESIAN_POINT('Ctrl Pts',(-25.1252553002292,12.9767129861419,
128.450507417475)) ;
#128047 = CARTESIAN_POINT('Ctrl Pts',(-25.1866265754372,12.7063602426885,
128.596486814777)) ;
#128048 = CARTESIAN_POINT('Ctrl Pts',(-25.2683748597299,12.490160978819,128.802401379313)) ;
#128049 = CARTESIAN_POINT('Ctrl Pts',(-25.3669237030102,12.3386882499648,
129.057094955999)) ;
#128050 = CARTESIAN_POINT('Ctrl Pts',(-25.4750438935506,12.2654833312748,
129.339847657555)) ;
#128051 = CARTESIAN_POINT('Ctrl Pts',(-25.5862280103804,12.2750423779192,
129.631462856753)) ;
#128052 = CARTESIAN_POINT('Ctrl Pts',(-25.6929338455416,12.3673309106593,
129.90999802218)) ;
#128053 = CARTESIAN_POINT('Ctrl Pts',(-25.7877694292322,12.534346926541,130.154033164579)) ;
#128054 = CARTESIAN_POINT('Ctrl Pts',(-25.8655711174805,12.7652871002756,
130.348199040054)) ;
#128055 = CARTESIAN_POINT('Ctrl Pts',(-25.9212064365725,13.0444119027006,
130.477502422996)) ;
#128056 = CARTESIAN_POINT('Ctrl Pts',(-25.9511258449652,13.3498617149792,
130.531785727571)) ;
#128057 = CARTESIAN_POINT('Ctrl Pts',(-25.9540442725774,13.6613614956128,
130.507099881275)) ;
#128058 = CARTESIAN_POINT('Ctrl Pts',(-25.9306476029736,13.9537822109427,
130.4057698744)) ;
#128059 = CARTESIAN_POINT('Ctrl Pts',(-25.8832256006458,14.2096141501914,
130.234109824226)) ;
#128060 = CARTESIAN_POINT('Ctrl Pts',(-25.8158001807284,14.409057323901,130.003996520483)) ;
#128061 = CARTESIAN_POINT('Ctrl Pts',(-25.7341641419467,14.5378227740497,
129.732422677828)) ;
#128062 = CARTESIAN_POINT('Ctrl Pts',(-25.6443470911794,14.5866410235712,
129.436796365213)) ;
#128063 = CARTESIAN_POINT('Ctrl Pts',(-25.5547638150537,14.5524956980778,
129.142180912862)) ;
#128064 = CARTESIAN_POINT('Ctrl Pts',(-25.4705811162127,14.436335978299,128.862889568447)) ;
#128065 = CARTESIAN_POINT('Ctrl Pts',(-25.4006244003216,14.2487612510743,
128.625535064057)) ;
#128066 = CARTESIAN_POINT('Ctrl Pts',(-25.3493716847571,14.0019963644833,
128.442718956111)) ;
#128067 = CARTESIAN_POINT('Ctrl Pts',(-25.321482404065,13.7133413739479,128.328114199707)) ;
#128068 = CARTESIAN_POINT('Ctrl Pts',(-25.3198401069144,13.4034231112183,
128.290130687378)) ;
#128069 = CARTESIAN_POINT('Ctrl Pts',(-25.3449983181151,13.0966156086416,
128.330632354685)) ;
#128070 = CARTESIAN_POINT('Ctrl Pts',(-25.3964989597862,12.8104956344232,
128.447768053659)) ;
#128071 = CARTESIAN_POINT('Ctrl Pts',(-25.4705334308323,12.5707042508866,
128.631021712006)) ;
#128072 = CARTESIAN_POINT('Ctrl Pts',(-25.5630356046663,12.3910193805736,
128.868133701558)) ;
#128073 = CARTESIAN_POINT('Ctrl Pts',(-25.6681544066941,12.2853288734926,
129.142069440953)) ;
#128074 = CARTESIAN_POINT('Ctrl Pts',(-25.778694693908,12.2609818511097,129.431921558708)) ;
#128075 = CARTESIAN_POINT('Ctrl Pts',(-25.8884709129135,12.3204757411683,
129.719304966435)) ;
#128076 = CARTESIAN_POINT('Ctrl Pts',(-25.9886740073855,12.4582515561699,
129.979020191138)) ;
#128077 = CARTESIAN_POINT('Ctrl Pts',(-26.0743372008251,12.665899809485,130.196066145188)) ;
#128078 = CARTESIAN_POINT('Ctrl Pts',(-26.1391179757226,12.926809546633,130.352268079656)) ;
#128079 = CARTESIAN_POINT('Ctrl Pts',(-26.1796732755739,13.2233761024273,
130.437657929989)) ;
#128080 = CARTESIAN_POINT('Ctrl Pts',(-26.1937046974809,13.5346576099115,
130.445524568179)) ;
#128081 = CARTESIAN_POINT('Ctrl Pts',(-26.1807569035134,13.8387960624651,
130.374479587911)) ;
#128082 = CARTESIAN_POINT('Ctrl Pts',(-26.1425724297029,14.1123017262305,
130.229804146074)) ;
#128083 = CARTESIAN_POINT('Ctrl Pts',(-26.0825726076526,14.3364686788982,
130.021376384275)) ;
#128084 = CARTESIAN_POINT('Ctrl Pts',(-26.0061672037188,14.4947707919197,
129.76515900541)) ;
#128085 = CARTESIAN_POINT('Ctrl Pts',(-25.9186915378375,14.5769227854228,
129.476380890809)) ;
#128086 = CARTESIAN_POINT('Ctrl Pts',(-25.828437185311,14.5762675559882,129.179779749649)) ;
#128087 = CARTESIAN_POINT('Ctrl Pts',(-25.7411174774271,14.4930554599536,
128.891479940059)) ;
#128088 = CARTESIAN_POINT('Ctrl Pts',(-25.6647114903275,14.3331651015145,
128.63516567355)) ;
#128089 = CARTESIAN_POINT('Ctrl Pts',(-25.6050905510217,14.1081176905962,
128.427867003823)) ;
#128090 = CARTESIAN_POINT('Ctrl Pts',(-25.5673123091255,13.8340179533061,
128.28438435414)) ;
#128091 = CARTESIAN_POINT('Ctrl Pts',(-25.5547989687703,13.5302899691965,
128.21468609169)) ;
#128092 = CARTESIAN_POINT('Ctrl Pts',(-25.5691793862707,13.2194242274908,
128.223607489868)) ;
#128093 = CARTESIAN_POINT('Ctrl Pts',(-25.6099882053418,12.9232188670747,
128.309754159081)) ;
#128094 = CARTESIAN_POINT('Ctrl Pts',(-25.6755761765933,12.661461296016,128.468101957688)) ;
#128095 = CARTESIAN_POINT('Ctrl Pts',(-25.7610234535684,12.4560560459253,
128.684718224714)) ;
#128096 = CARTESIAN_POINT('Ctrl Pts',(-25.8617752670754,12.3187614615208,
128.945904715609)) ;
#128097 = CARTESIAN_POINT('Ctrl Pts',(-25.9712898119601,12.2608758926762,
129.232630942734)) ;
#128098 = CARTESIAN_POINT('Ctrl Pts',(-26.0817469151749,12.2860567497161,
129.522259623789)) ;
#128099 = CARTESIAN_POINT('Ctrl Pts',(-26.1872408236699,12.3936760762178,
129.797118439097)) ;
#128100 = CARTESIAN_POINT('Ctrl Pts',(-26.2790423656848,12.5734427117125,
130.032358969761)) ;
#128101 = CARTESIAN_POINT('Ctrl Pts',(-26.3531762412792,12.8155556757963,
130.215696265957)) ;
#128102 = CARTESIAN_POINT('Ctrl Pts',(-26.4039053292045,13.1001458923633,
130.330827106248)) ;
#128103 = CARTESIAN_POINT('Ctrl Pts',(-26.4288254379187,13.4082451874709,
130.370501539131)) ;
#128104 = CARTESIAN_POINT('Ctrl Pts',(-26.426822031636,13.7170001828003,130.331582040945)) ;
#128105 = CARTESIAN_POINT('Ctrl Pts',(-26.3984000431209,14.0068803431456,
130.215220499312)) ;
#128106 = CARTESIAN_POINT('Ctrl Pts',(-26.3469149274336,14.2520830304775,
130.031824301073)) ;
#128107 = CARTESIAN_POINT('Ctrl Pts',(-26.2765535613933,14.4388654821964,
129.793218238151)) ;
#128108 = CARTESIAN_POINT('Ctrl Pts',(-26.1927905162966,14.5532758713035,
129.515375412257)) ;
#128109 = CARTESIAN_POINT('Ctrl Pts',(-26.1025705013195,14.5866372917137,
129.218675357135)) ;
#128110 = CARTESIAN_POINT('Ctrl Pts',(-26.013030368013,14.5363254229255,128.923932390282)) ;
#128111 = CARTESIAN_POINT('Ctrl Pts',(-25.9317546338566,14.4070821758454,
128.653504394788)) ;
#128112 = CARTESIAN_POINT('Ctrl Pts',(-25.8642785654878,14.2058492351143,
128.42309702246)) ;
#128113 = CARTESIAN_POINT('Ctrl Pts',(-25.8172570002977,13.9493210351354,
128.252624752721)) ;
#128114 = CARTESIAN_POINT('Ctrl Pts',(-25.7942597880218,13.6560816946818,
128.152419866967)) ;
#128115 = CARTESIAN_POINT('Ctrl Pts',(-25.7976276043833,13.345421430163,128.129145084191)) ;
#128116 = CARTESIAN_POINT('Ctrl Pts',(-25.8277991868315,13.040595844376,128.18421481984)) ;
#128117 = CARTESIAN_POINT('Ctrl Pts',(-25.8840495582596,12.7610203807177,
128.315183220205)) ;
#128118 = CARTESIAN_POINT('Ctrl Pts',(-25.9616974256306,12.5320805251594,
128.509083689549)) ;
#128119 = CARTESIAN_POINT('Ctrl Pts',(-26.0572216139122,12.3651153632671,
128.754952054418)) ;
#128120 = CARTESIAN_POINT('Ctrl Pts',(-26.16380926824,12.2743250028136,129.033224471676)) ;
#128121 = CARTESIAN_POINT('Ctrl Pts',(-26.2753298606958,12.2660445158075,
129.325721909756)) ;
#128122 = CARTESIAN_POINT('Ctrl Pts',(-26.3828799962309,12.3402671255805,
129.606951767026)) ;
#128123 = CARTESIAN_POINT('Ctrl Pts',(-26.4812883874454,12.4924311460887,
129.861240484378)) ;
#128124 = CARTESIAN_POINT('Ctrl Pts',(-26.5630932377152,12.7106680938423,
130.067163032861)) ;
#128125 = CARTESIAN_POINT('Ctrl Pts',(-26.6238634402305,12.9803449580317,
130.211547393049)) ;
#128126 = CARTESIAN_POINT('Ctrl Pts',(-26.6596062976098,13.2833170370261,
130.282668176157)) ;
#128127 = CARTESIAN_POINT('Ctrl Pts',(-26.6683992001938,13.5926827772034,
130.275458609873)) ;
#128128 = CARTESIAN_POINT('Ctrl Pts',(-26.6505137795868,13.8936497726217,
130.189900592151)) ;
#128129 = CARTESIAN_POINT('Ctrl Pts',(-26.6078602763148,14.1589430320387,
130.032192029423)) ;
#128130 = CARTESIAN_POINT('Ctrl Pts',(-26.5445783612324,14.3711507440271,
129.814309109576)) ;
#128131 = CARTESIAN_POINT('Ctrl Pts',(-26.4655827230832,14.5162610526243,
129.550459758268)) ;
#128132 = CARTESIAN_POINT('Ctrl Pts',(-26.376738727669,14.5833063446483,129.257632402111)) ;
#128133 = CARTESIAN_POINT('Ctrl Pts',(-26.2861729331064,14.566512972423,128.959951686922)) ;
#128134 = CARTESIAN_POINT('Ctrl Pts',(-26.2009020705313,14.4685224251672,
128.67784492761)) ;
#128135 = CARTESIAN_POINT('Ctrl Pts',(-26.1271681583346,14.295496638092,128.429327566497)) ;
#128136 = CARTESIAN_POINT('Ctrl Pts',(-26.0713023155461,14.0596946684097,
128.232981990481)) ;
#128137 = CARTESIAN_POINT('Ctrl Pts',(-26.0380253527417,13.7784556311811,
128.102645526396)) ;
#128138 = CARTESIAN_POINT('Ctrl Pts',(-26.0306021104224,13.4704205664196,
128.047693579746)) ;
#128139 = CARTESIAN_POINT('Ctrl Pts',(-26.0499050772378,13.1626907003778,
128.071224875015)) ;
#128140 = CARTESIAN_POINT('Ctrl Pts',(-26.0958353944327,12.8697533326654,
128.172107844854)) ;
#128141 = CARTESIAN_POINT('Ctrl Pts',(-26.1651975859897,12.6186668419938,
128.341706812271)) ;
#128142 = CARTESIAN_POINT('Ctrl Pts',(-26.2543855123382,12.4240570557475,
128.56905730259)) ;
#128143 = CARTESIAN_POINT('Ctrl Pts',(-26.3570165493029,12.3017129015635,
128.835831715512)) ;
#128144 = CARTESIAN_POINT('Ctrl Pts',(-26.4672343576536,12.259212443294,129.124643417402)) ;
#128145 = CARTESIAN_POINT('Ctrl Pts',(-26.5774090635175,12.3002004247184,
129.413368541245)) ;
#128146 = CARTESIAN_POINT('Ctrl Pts',(-26.6807625992197,12.4222100082891,
129.682061388604)) ;
#128147 = CARTESIAN_POINT('Ctrl Pts',(-26.7698384246454,12.6151763777399,
129.90922006221)) ;
#128148 = CARTESIAN_POINT('Ctrl Pts',(-26.8397567435722,12.8667635442981,
130.080291665491)) ;
#128149 = CARTESIAN_POINT('Ctrl Pts',(-26.8856922490943,13.156608287975,130.181493757996)) ;
#128150 = CARTESIAN_POINT('Ctrl Pts',(-26.905648091964,13.4669634913823,130.206630694337)) ;
#128151 = CARTESIAN_POINT('Ctrl Pts',(-26.8984820418813,13.7743605544172,
130.152520289261)) ;
#128152 = CARTESIAN_POINT('Ctrl Pts',(-26.8656427954947,14.0556835364492,
130.023511196521)) ;
#128153 = CARTESIAN_POINT('Ctrl Pts',(-26.8101219407047,14.2923698340539,
129.828181452464)) ;
#128154 = CARTESIAN_POINT('Ctrl Pts',(-26.7362953067133,14.4669398089711,
129.579261905855)) ;
#128155 = CARTESIAN_POINT('Ctrl Pts',(-26.6512662787074,14.5658237072004,
129.297919990246)) ;
#128156 = CARTESIAN_POINT('Ctrl Pts',(-26.5603402007787,14.5834030804103,
128.99904072882)) ;
#128157 = CARTESIAN_POINT('Ctrl Pts',(-26.4722852743979,14.5182209640518,
128.70885302489)) ;
#128158 = CARTESIAN_POINT('Ctrl Pts',(-26.3924389121312,14.3732472744243,
128.4422467857)) ;
#128159 = CARTESIAN_POINT('Ctrl Pts',(-26.3290394001796,14.1617341160313,
128.22405452454)) ;
#128160 = CARTESIAN_POINT('Ctrl Pts',(-26.2861256992153,13.8968739581495,
128.065570508626)) ;
#128161 = CARTESIAN_POINT('Ctrl Pts',(-26.2678898569706,13.5970561201623,
127.979085240886)) ;
#128162 = CARTESIAN_POINT('Ctrl Pts',(-26.2765300087796,13.2853498772371,
127.971172699377)) ;
#128163 = CARTESIAN_POINT('Ctrl Pts',(-26.3116223620029,12.9854214225964,
128.040755422592)) ;
#128164 = CARTESIAN_POINT('Ctrl Pts',(-26.3720202123015,12.7145026725385,
128.18399408205)) ;
#128165 = CARTESIAN_POINT('Ctrl Pts',(-26.4535694094826,12.4953422799607,
128.389165339747)) ;
#128166 = CARTESIAN_POINT('Ctrl Pts',(-26.5519324421244,12.341785792788,128.643267128277)) ;
#128167 = CARTESIAN_POINT('Ctrl Pts',(-26.6595602095204,12.2665368205457,
128.924676014665)) ;
#128168 = CARTESIAN_POINT('Ctrl Pts',(-26.7706440836229,12.2735361579836,
129.216032753461)) ;
#128169 = CARTESIAN_POINT('Ctrl Pts',(-26.8775441666754,12.3632299170458,
129.49515442713)) ;
#128170 = CARTESIAN_POINT('Ctrl Pts',(-26.9731151455713,12.5286847379392,
129.741232249963)) ;
#128171 = CARTESIAN_POINT('Ctrl Pts',(-27.0513963528373,12.7579694052531,
129.936820922564)) ;
#128172 = CARTESIAN_POINT('Ctrl Pts',(-27.1076391987102,13.0352202264865,
130.067983012539)) ;
#128173 = CARTESIAN_POINT('Ctrl Pts',(-27.1383941250434,13.3405828522819,
130.124659245561)) ;
#128174 = CARTESIAN_POINT('Ctrl Pts',(-27.142164217804,13.6512271404406,130.102573741676)) ;
#128175 = CARTESIAN_POINT('Ctrl Pts',(-27.1194950619664,13.945858673121,130.003220415338)) ;
#128176 = CARTESIAN_POINT('Ctrl Pts',(-27.0725556914897,14.2033946436315,
129.832909918837)) ;
#128177 = CARTESIAN_POINT('Ctrl Pts',(-27.0058079309889,14.4040391097263,
129.60487026237)) ;
#128178 = CARTESIAN_POINT('Ctrl Pts',(-26.9246130375758,14.5350227363909,
129.334619148942)) ;
#128179 = CARTESIAN_POINT('Ctrl Pts',(-26.8347923397077,14.5864958768454,
129.038934787031)) ;
#128180 = CARTESIAN_POINT('Ctrl Pts',(-26.7449544652946,14.554416926093,128.743505036233)) ;
#128181 = CARTESIAN_POINT('Ctrl Pts',(-26.6609820117157,14.4414134388981,
128.465037672866)) ;
#128182 = CARTESIAN_POINT('Ctrl Pts',(-26.5901696168786,14.2551029689439,
128.225021388413)) ;
#128183 = CARTESIAN_POINT('Ctrl Pts',(-26.5383476891214,14.0100365387615,
128.040581334637)) ;
#128184 = CARTESIAN_POINT('Ctrl Pts',(-26.5097071652286,13.7214335720741,
127.923681487066)) ;
#128185 = CARTESIAN_POINT('Ctrl Pts',(-26.5072415117763,13.4135493080175,
127.883485393481)) ;
#128186 = CARTESIAN_POINT('Ctrl Pts',(-26.5317926987144,13.1045553567054,
127.922006198238)) ;
#128187 = CARTESIAN_POINT('Ctrl Pts',(-26.5821066591862,12.8197359120567,
128.035956491399)) ;
#128188 = CARTESIAN_POINT('Ctrl Pts',(-26.6560761824492,12.576213522993,128.218737407166)) ;
#128189 = CARTESIAN_POINT('Ctrl Pts',(-26.7479977099995,12.3952019972504,
128.454228677948)) ;
#128190 = CARTESIAN_POINT('Ctrl Pts',(-26.852959270396,12.2871509168402,128.727666098665)) ;
#128191 = CARTESIAN_POINT('Ctrl Pts',(-26.9631857583284,12.2605661250461,
129.016678346631)) ;
#128192 = CARTESIAN_POINT('Ctrl Pts',(-27.0731032377883,12.3174696014915,
129.304479474258)) ;
#128193 = CARTESIAN_POINT('Ctrl Pts',(-27.1738841185141,12.45350954949,129.565800797398)) ;
#128194 = CARTESIAN_POINT('Ctrl Pts',(-27.2598368577993,12.6588730933983,
129.783777023258)) ;
#128195 = CARTESIAN_POINT('Ctrl Pts',(-27.3253460720657,12.9185732452431,
129.942083221898)) ;
#128196 = CARTESIAN_POINT('Ctrl Pts',(-27.3666461043042,13.2144047021654,
130.029650643336)) ;
#128197 = CARTESIAN_POINT('Ctrl Pts',(-27.3814508616359,13.5255441654578,
130.039777855938)) ;
#128198 = CARTESIAN_POINT('Ctrl Pts',(-27.3693461451008,13.8297539954917,
129.971255359995)) ;
#128199 = CARTESIAN_POINT('Ctrl Pts',(-27.3317726975183,14.1049217876101,
129.828295911421)) ;
#128200 = CARTESIAN_POINT('Ctrl Pts',(-27.2727161189021,14.329872377713,129.622795412737)) ;
#128201 = CARTESIAN_POINT('Ctrl Pts',(-27.1961848662824,14.491552798162,129.365964164441)) ;
#128202 = CARTESIAN_POINT('Ctrl Pts',(-27.1091899784791,14.5755974464537,
129.078707325624)) ;
#128203 = CARTESIAN_POINT('Ctrl Pts',(-27.01879203794,14.5774288314458,128.781626400399)) ;
#128204 = CARTESIAN_POINT('Ctrl Pts',(-26.9314794185646,14.4968431442199,
128.493436234079)) ;
#128205 = CARTESIAN_POINT('Ctrl Pts',(-26.8543959535475,14.3385595684728,
128.235025271593)) ;
#128206 = CARTESIAN_POINT('Ctrl Pts',(-26.7942771704595,14.1152210821619,
128.026295396246)) ;
#128207 = CARTESIAN_POINT('Ctrl Pts',(-26.7558188879496,13.8419814694385,
127.880794925919)) ;
#128208 = CARTESIAN_POINT('Ctrl Pts',(-26.7425859508397,13.5398085198315,
127.809104336374)) ;
#128209 = CARTESIAN_POINT('Ctrl Pts',(-26.7561438538663,13.2280435921434,
127.81553948295)) ;
#128210 = CARTESIAN_POINT('Ctrl Pts',(-26.7964991026641,12.9300591046375,
127.900229432936)) ;
#128211 = CARTESIAN_POINT('Ctrl Pts',(-26.8611655938303,12.6684084427586,
128.056051445632)) ;
#128212 = CARTESIAN_POINT('Ctrl Pts',(-26.9462176040478,12.4608091594121,
128.27145590624)) ;
#128213 = CARTESIAN_POINT('Ctrl Pts',(-27.0467113671397,12.3214093535999,
128.53187021786)) ;
#128214 = CARTESIAN_POINT('Ctrl Pts',(-27.1562555166034,12.261330300397,128.818633686213)) ;
#128215 = CARTESIAN_POINT('Ctrl Pts',(-27.2663375886122,12.2843254988424,
129.107291751522)) ;
#128216 = CARTESIAN_POINT('Ctrl Pts',(-27.3716324986393,12.3887269721217,
129.381731211064)) ;
#128217 = CARTESIAN_POINT('Ctrl Pts',(-27.4644801364651,12.5673627436567,
129.619832504695)) ;
#128218 = CARTESIAN_POINT('Ctrl Pts',(-27.5391406638283,12.8080166806353,
129.804719444648)) ;
#128219 = CARTESIAN_POINT('Ctrl Pts',(-27.5906063032235,13.0914774354823,
129.922013122237)) ;
#128220 = CARTESIAN_POINT('Ctrl Pts',(-27.616327879176,13.4005589670674,129.963888465317)) ;
#128221 = CARTESIAN_POINT('Ctrl Pts',(-27.6149921031721,13.7083911596742,
129.927043626821)) ;
#128222 = CARTESIAN_POINT('Ctrl Pts',(-27.5874202378808,13.9985991378762,
129.813238675445)) ;
#128223 = CARTESIAN_POINT('Ctrl Pts',(-27.536484449555,14.2457812559265,129.631387326717)) ;
#128224 = CARTESIAN_POINT('Ctrl Pts',(-27.4665317915239,14.4345734153115,
129.393953237947)) ;
#128225 = CARTESIAN_POINT('Ctrl Pts',(-27.383009709236,14.5511370879547,129.116800950602)) ;
#128226 = CARTESIAN_POINT('Ctrl Pts',(-27.2931554129536,14.5867802187907,
128.821269985454)) ;
#128227 = CARTESIAN_POINT('Ctrl Pts',(-27.2034748698954,14.5391948483821,
128.526119117529)) ;
#128228 = CARTESIAN_POINT('Ctrl Pts',(-27.1215961718606,14.411534541166,128.253806213587)) ;
#128229 = CARTESIAN_POINT('Ctrl Pts',(-27.0540300153367,14.2134355911455,
128.023342403406)) ;
#128230 = CARTESIAN_POINT('Ctrl Pts',(-27.0061516223831,13.9582377807151,
127.850318612923)) ;
#128231 = CARTESIAN_POINT('Ctrl Pts',(-26.9823271114248,13.6646542857207,
127.747569753109)) ;
#128232 = CARTESIAN_POINT('Ctrl Pts',(-26.9849343677111,13.354183694307,127.722078671003)) ;
#128233 = CARTESIAN_POINT('Ctrl Pts',(-27.0144698797521,13.0484269475921,
127.775232008199)) ;
#128234 = CARTESIAN_POINT('Ctrl Pts',(-27.0696778910055,12.7694396144753,
127.903355960201)) ;
#128235 = CARTESIAN_POINT('Ctrl Pts',(-27.1468061921369,12.5380417818578,
128.095664000225)) ;
#128236 = CARTESIAN_POINT('Ctrl Pts',(-27.2424888343211,12.3683286103215,
128.341812779954)) ;
#128237 = CARTESIAN_POINT('Ctrl Pts',(-27.3483693988791,12.2760420301782,
128.618176794529)) ;
#128238 = CARTESIAN_POINT('Ctrl Pts',(-27.4593559365058,12.2649171956023,
128.909263666053)) ;
#128239 = CARTESIAN_POINT('Ctrl Pts',(-27.567634623934,12.3368690602114,129.192461766527)) ;
#128240 = CARTESIAN_POINT('Ctrl Pts',(-27.666488441497,12.4871142426883,129.448028051994)) ;
#128241 = CARTESIAN_POINT('Ctrl Pts',(-27.7489819874493,12.7041605723025,
129.655894722522)) ;
#128242 = CARTESIAN_POINT('Ctrl Pts',(-27.8101941453054,12.9721742229255,
129.80164232834)) ;
#128243 = CARTESIAN_POINT('Ctrl Pts',(-27.846628352146,13.2726902909237,129.874973593325)) ;
#128244 = CARTESIAN_POINT('Ctrl Pts',(-27.8563402142155,13.5844634712024,
129.870193895069)) ;
#128245 = CARTESIAN_POINT('Ctrl Pts',(-27.8391363324445,13.8852370935213,
129.786712780349)) ;
#128246 = CARTESIAN_POINT('Ctrl Pts',(-27.7974142447192,14.1508960461137,
129.631852840205)) ;
#128247 = CARTESIAN_POINT('Ctrl Pts',(-27.734510775802,14.3659570347197,129.414953151005)) ;
#128248 = CARTESIAN_POINT('Ctrl Pts',(-27.6555249095009,14.513384444757,129.151006206137)) ;
#128249 = CARTESIAN_POINT('Ctrl Pts',(-27.5675962898643,14.58228249035,128.861131563589)) ;
#128250 = CARTESIAN_POINT('Ctrl Pts',(-27.4767674367506,14.5684017700248,
128.562597823583)) ;
#128251 = CARTESIAN_POINT('Ctrl Pts',(-27.3910622500698,14.4726240352221,
128.279161519902)) ;
#128252 = CARTESIAN_POINT('Ctrl Pts',(-27.3167036437953,14.3009018256013,
128.028711527011)) ;
#128253 = CARTESIAN_POINT('Ctrl Pts',(-27.2604835702691,14.0676662021592,
127.831474654868)) ;
#128254 = CARTESIAN_POINT('Ctrl Pts',(-27.2264233622165,13.7867923428731,
127.698762487331)) ;
#128255 = CARTESIAN_POINT('Ctrl Pts',(-27.2181959748588,13.4808115770732,
127.641638031402)) ;
#128256 = CARTESIAN_POINT('Ctrl Pts',(-27.2367954548246,13.1706177379304,
127.662872485548)) ;
#128257 = CARTESIAN_POINT('Ctrl Pts',(-27.2821107930129,12.8770484120512,
127.761971688995)) ;
#128258 = CARTESIAN_POINT('Ctrl Pts',(-27.3507301309266,12.6251910549939,
127.929467048696)) ;
#128259 = CARTESIAN_POINT('Ctrl Pts',(-27.4391846595436,12.4289584768191,
128.154751522028)) ;
#128260 = CARTESIAN_POINT('Ctrl Pts',(-27.5420614810931,12.3038002387545,
128.42206593562)) ;
#128261 = CARTESIAN_POINT('Ctrl Pts',(-27.6519492987896,12.2593442699651,
128.709988056267)) ;
#128262 = CARTESIAN_POINT('Ctrl Pts',(-27.7619662940764,12.2978898769658,
128.998322853002)) ;
#128263 = CARTESIAN_POINT('Ctrl Pts',(-27.865379784088,12.4169444283248,129.267289988982)) ;
#128264 = CARTESIAN_POINT('Ctrl Pts',(-27.9555551516384,12.6093773195972,
129.497426958593)) ;
#128265 = CARTESIAN_POINT('Ctrl Pts',(-28.0257071874864,12.8583734122104,
129.669351599666)) ;
#128266 = CARTESIAN_POINT('Ctrl Pts',(-28.0725603911615,13.1480449714035,
129.773142916573)) ;
#128267 = CARTESIAN_POINT('Ctrl Pts',(-28.0932282711231,13.4582417931766,
129.800355674883)) ;
#128268 = CARTESIAN_POINT('Ctrl Pts',(-28.0868635394014,13.7655079117814,
129.748643838575)) ;
#128269 = CARTESIAN_POINT('Ctrl Pts',(-28.0546846226306,14.0483169670967,
129.621511117713)) ;
#128270 = CARTESIAN_POINT('Ctrl Pts',(-27.9998381490793,14.285999002941,129.428215013828)) ;
#128271 = CARTESIAN_POINT('Ctrl Pts',(-27.9267313668262,14.4624790496655,
129.18149179678)) ;
#128272 = CARTESIAN_POINT('Ctrl Pts',(-27.8413857863696,14.5642183911393,
128.899001900319)) ;
#128273 = CARTESIAN_POINT('Ctrl Pts',(-27.7510753292932,14.5841609498882,
128.602138093997)) ;
#128274 = CARTESIAN_POINT('Ctrl Pts',(-27.6623060110327,14.520970734674,128.309647323951)) ;
#128275 = CARTESIAN_POINT('Ctrl Pts',(-27.5826746424944,14.3791779358065,
128.0439161209)) ;
#128276 = CARTESIAN_POINT('Ctrl Pts',(-27.518374582185,14.1688151362551,127.822942393228)) ;
#128277 = CARTESIAN_POINT('Ctrl Pts',(-27.4748576193926,13.9051957088918,
127.662708523844)) ;
#128278 = CARTESIAN_POINT('Ctrl Pts',(-27.455878155537,13.60715006879,127.574159959947)) ;
#128279 = CARTESIAN_POINT('Ctrl Pts',(-27.4635634033647,13.2953843814918,
127.563449508453)) ;
#128280 = CARTESIAN_POINT('Ctrl Pts',(-27.4981521378243,12.9930169526984,
127.631353422156)) ;
#128281 = CARTESIAN_POINT('Ctrl Pts',(-27.557608395534,12.7222273700058,127.772001748044)) ;
#128282 = CARTESIAN_POINT('Ctrl Pts',(-27.6388268171335,12.500544093303,127.97609760927)) ;
#128283 = CARTESIAN_POINT('Ctrl Pts',(-27.7367701007511,12.3451353324325,
128.228996533809)) ;
#128284 = CARTESIAN_POINT('Ctrl Pts',(-27.8442278309089,12.2674914285865,
128.509899764783)) ;
#128285 = CARTESIAN_POINT('Ctrl Pts',(-27.9556267443121,12.2722652657277,
128.802088932825)) ;
#128286 = CARTESIAN_POINT('Ctrl Pts',(-28.0626310256601,12.3599738467364,
129.081538376024)) ;
#128287 = CARTESIAN_POINT('Ctrl Pts',(-28.1582011213712,12.5226378491769,
129.327757332152)) ;
#128288 = CARTESIAN_POINT('Ctrl Pts',(-28.2373259873122,12.7508222616319,
129.525715012972)) ;
#128289 = CARTESIAN_POINT('Ctrl Pts',(-28.2943391587573,13.0279565462644,
129.659029364955)) ;
#128290 = CARTESIAN_POINT('Ctrl Pts',(-28.3256773216857,13.3323087573567,
129.71747181238)) ;
#128291 = CARTESIAN_POINT('Ctrl Pts',(-28.3302116619813,13.6420774120511,
129.697726410344)) ;
#128292 = CARTESIAN_POINT('Ctrl Pts',(-28.3083291946858,13.9374078331077,
129.600681337831)) ;
#128293 = CARTESIAN_POINT('Ctrl Pts',(-28.2620837924338,14.1965319396346,
129.432389885247)) ;
#128294 = CARTESIAN_POINT('Ctrl Pts',(-28.1954079952008,14.3999725779251,
129.204370428957)) ;
#128295 = CARTESIAN_POINT('Ctrl Pts',(-28.1149345373054,14.5320840128439,
128.936405639346)) ;
#128296 = CARTESIAN_POINT('Ctrl Pts',(-28.0254070588349,14.5862914481129,
128.641628884545)) ;
#128297 = CARTESIAN_POINT('Ctrl Pts',(-27.9349905698168,14.5562373183141,
128.344321370437)) ;
#128298 = CARTESIAN_POINT('Ctrl Pts',(-27.8512631288849,14.4460760086482,
128.066773599745)) ;
#128299 = CARTESIAN_POINT('Ctrl Pts',(-27.7796573084958,14.2613118690052,
127.824318182641)) ;
#128300 = CARTESIAN_POINT('Ctrl Pts',(-27.7272301440332,14.0168342944471,
127.638029248606)) ;
#128301 = CARTESIAN_POINT('Ctrl Pts',(-27.6980179864544,13.7314084921459,
127.519711908543)) ;
#128302 = CARTESIAN_POINT('Ctrl Pts',(-27.694741233829,13.4213927772855,127.476877876191)) ;
#128303 = CARTESIAN_POINT('Ctrl Pts',(-27.7184522170526,13.1138964811438,
127.513143988576)) ;
#128304 = CARTESIAN_POINT('Ctrl Pts',(-27.7680874772327,12.8273574964974,
127.625029075045)) ;
#128305 = CARTESIAN_POINT('Ctrl Pts',(-27.8415277932473,12.5821904273637,
127.806243710016)) ;
#128306 = CARTESIAN_POINT('Ctrl Pts',(-27.9331064049308,12.3992406636329,
128.040702389871)) ;
#128307 = CARTESIAN_POINT('Ctrl Pts',(-28.0374350862425,12.2892635372044,
128.312405983018)) ;
#128308 = CARTESIAN_POINT('Ctrl Pts',(-28.1478242152573,12.2601882731061,
128.601820064507)) ;
#128309 = CARTESIAN_POINT('Ctrl Pts',(-28.2574870562922,12.3144490332909,
128.889000080819)) ;
#128310 = CARTESIAN_POINT('Ctrl Pts',(-28.3587283063992,12.4481500310982,
129.151637015902)) ;
#128311 = CARTESIAN_POINT('Ctrl Pts',(-28.4452635080364,12.6515765338915,
129.371309005377)) ;
#128312 = CARTESIAN_POINT('Ctrl Pts',(-28.5117628591178,12.9112090409297,
129.532345469997)) ;
#128313 = CARTESIAN_POINT('Ctrl Pts',(-28.5537057225309,13.2069680634014,
129.621732622069)) ;
#128314 = CARTESIAN_POINT('Ctrl Pts',(-28.5691937316055,13.5165270688446,
129.634014378779)) ;
#128315 = CARTESIAN_POINT('Ctrl Pts',(-28.5577477153071,13.8224961105202,
129.5672725385)) ;
#128316 = CARTESIAN_POINT('Ctrl Pts',(-28.5209930737035,14.0973150070006,
129.426876181682)) ;
#128317 = CARTESIAN_POINT('Ctrl Pts',(-28.4624086215617,14.3244517952957,
129.222682993721)) ;
#128318 = CARTESIAN_POINT('Ctrl Pts',(-28.3863966418976,14.4877799553715,
128.967429888637)) ;
#128319 = CARTESIAN_POINT('Ctrl Pts',(-28.2997377511392,14.5742904873528,
128.681191571893)) ;
#128320 = CARTESIAN_POINT('Ctrl Pts',(-28.2089570194485,14.5785355411289,
128.382852483818)) ;
#128321 = CARTESIAN_POINT('Ctrl Pts',(-28.1215748771768,14.4999983215905,
128.09449428547)) ;
#128322 = CARTESIAN_POINT('Ctrl Pts',(-28.0444292301552,14.3447574247582,
127.836061476381)) ;
#128323 = CARTESIAN_POINT('Ctrl Pts',(-27.9834965686545,14.1223924190304,
127.624828784792)) ;
#128324 = CARTESIAN_POINT('Ctrl Pts',(-27.9444380366247,13.8510686498015,
127.477666074581)) ;
#128325 = CARTESIAN_POINT('Ctrl Pts',(-27.930360050621,13.5484336095185,127.403388519421)) ;
#128326 = CARTESIAN_POINT('Ctrl Pts',(-27.9431835233612,13.2370241566132,
127.407724507392)) ;
#128327 = CARTESIAN_POINT('Ctrl Pts',(-27.9826117035251,12.9391311523709,
127.489800007884)) ;
#128328 = CARTESIAN_POINT('Ctrl Pts',(-28.0466226653077,12.6756660362993,
127.643662724159)) ;
#128329 = CARTESIAN_POINT('Ctrl Pts',(-28.1313787129563,12.4657027909829,
127.858115595181)) ;
#128330 = CARTESIAN_POINT('Ctrl Pts',(-28.2314667834269,12.324474551251,128.117369989925)) ;
#128331 = CARTESIAN_POINT('Ctrl Pts',(-28.3403582781537,12.2619232759168,
128.402373643518)) ;
#128332 = CARTESIAN_POINT('Ctrl Pts',(-28.4512758924128,12.2825882347195,
128.693237314343)) ;
#128333 = CARTESIAN_POINT('Ctrl Pts',(-28.5564686671438,12.3846501160854,
128.967486567491)) ;
#128334 = CARTESIAN_POINT('Ctrl Pts',(-28.6497560237034,12.5611187121008,
129.206879240928)) ;
#128335 = CARTESIAN_POINT('Ctrl Pts',(-28.7250343701191,12.800128888062,129.39357903039)) ;
#128336 = CARTESIAN_POINT('Ctrl Pts',(-28.7772435757727,13.0829558390025,
129.513002075926)) ;
#128337 = CARTESIAN_POINT('Ctrl Pts',(-28.803716434952,13.3903655442342,129.557211154603)) ;
#128338 = CARTESIAN_POINT('Ctrl Pts',(-28.803174137136,13.7001366182577,129.522500863899)) ;
#128339 = CARTESIAN_POINT('Ctrl Pts',(-28.7764473676396,13.9898881867711,
129.411323520338)) ;
#128340 = CARTESIAN_POINT('Ctrl Pts',(-28.7260928299473,14.2391934618933,
129.231093829253)) ;
#128341 = CARTESIAN_POINT('Ctrl Pts',(-28.656715613741,14.4298567293758,128.995378640907)) ;
#128342 = CARTESIAN_POINT('Ctrl Pts',(-28.5729912432793,14.5492471460414,
128.717440021589)) ;
#128343 = CARTESIAN_POINT('Ctrl Pts',(-28.4835291438219,14.5868020956478,
128.423172517193)) ;
#128344 = CARTESIAN_POINT('Ctrl Pts',(-28.3938133452937,14.5417975160937,
128.127949271842)) ;
#128345 = CARTESIAN_POINT('Ctrl Pts',(-28.3115790793439,14.416208825978,127.854576526063)) ;
#128346 = CARTESIAN_POINT('Ctrl Pts',(-28.2435588146913,14.22040833296,127.622834888852)) ;
#128347 = CARTESIAN_POINT('Ctrl Pts',(-28.1948097328007,13.9647701256438,
127.447046656053)) ;
#128348 = CARTESIAN_POINT('Ctrl Pts',(-28.1704722438048,13.6739288758575,
127.343029876413)) ;
#128349 = CARTESIAN_POINT('Ctrl Pts',(-28.1722918388017,13.3623285139176,
127.315091138043)) ;
#128350 = CARTESIAN_POINT('Ctrl Pts',(-28.2010132389493,13.0574724687543,
127.366009013332)) ;
#128351 = CARTESIAN_POINT('Ctrl Pts',(-28.2554093381646,12.7770677304932,
127.49174771629)) ;
#128352 = CARTESIAN_POINT('Ctrl Pts',(-28.3326365056277,12.5427865194022,
127.684105622645)) ;
#128353 = CARTESIAN_POINT('Ctrl Pts',(-28.426700494125,12.3731888439483,127.925946135446)) ;
#128354 = CARTESIAN_POINT('Ctrl Pts',(-28.5329415022504,12.2773794382998,
128.203152444927)) ;
#128355 = CARTESIAN_POINT('Ctrl Pts',(-28.6442054584027,12.2641879645069,
128.494964474125)) ;
#128356 = CARTESIAN_POINT('Ctrl Pts',(-28.7522728606296,12.3335960528712,
128.777660872691)) ;
#128357 = CARTESIAN_POINT('Ctrl Pts',(-28.8515196262173,12.4815616516049,
129.034375425197)) ;
#128358 = CARTESIAN_POINT('Ctrl Pts',(-28.9346047736369,12.6968287193189,
129.243965291323)) ;
#128359 = CARTESIAN_POINT('Ctrl Pts',(-28.9966007920383,12.9642190193072,
129.391928972392)) ;
#128360 = CARTESIAN_POINT('Ctrl Pts',(-29.033760876432,13.2637554960381,129.467423408639)) ;
#128361 = CARTESIAN_POINT('Ctrl Pts',(-29.0441746643463,13.5766923878532,
129.464563129082)) ;
#128362 = CARTESIAN_POINT('Ctrl Pts',(-29.0279267762062,13.875372212648,129.384186726206)) ;
#128363 = CARTESIAN_POINT('Ctrl Pts',(-28.9866159966681,14.1446745454968,
129.230246450064)) ;
#128364 = CARTESIAN_POINT('Ctrl Pts',(-28.9242657580172,14.3606486125631,
129.015033986799)) ;
#128365 = CARTESIAN_POINT('Ctrl Pts',(-28.8459541094201,14.5100785842148,
128.753160853726)) ;
#128366 = CARTESIAN_POINT('Ctrl Pts',(-28.7575144988308,14.581577583442,128.46153769434)) ;
#128367 = CARTESIAN_POINT('Ctrl Pts',(-28.6673238167247,14.5700419857243,
128.165121807893)) ;
#128368 = CARTESIAN_POINT('Ctrl Pts',(-28.58097543859,14.4761037677004,127.879636404591)) ;
#128369 = CARTESIAN_POINT('Ctrl Pts',(-28.5065773394975,14.3074346492421,
127.629266918375)) ;
#128370 = CARTESIAN_POINT('Ctrl Pts',(-28.4493300740461,14.0735726196759,
127.428724095027)) ;
#128371 = CARTESIAN_POINT('Ctrl Pts',(-28.4149758226597,13.7966474612173,
127.295512809063)) ;
#128372 = CARTESIAN_POINT('Ctrl Pts',(-28.4058187870782,13.4894705422107,
127.235477170096)) ;
#128373 = CARTESIAN_POINT('Ctrl Pts',(-28.4236271856564,13.1800818443726,
127.254513000672)) ;
#128374 = CARTESIAN_POINT('Ctrl Pts',(-28.4681605342844,12.8853356216509,
127.351294313502)) ;
#128375 = CARTESIAN_POINT('Ctrl Pts',(-28.5362090045899,12.6318026022688,
127.517091172939)) ;
#128376 = CARTESIAN_POINT('Ctrl Pts',(-28.6242035815314,12.4337108519891,
127.741021478077)) ;
#128377 = CARTESIAN_POINT('Ctrl Pts',(-28.7265451726035,12.3064394714406,
128.006839090709)) ;
#128378 = CARTESIAN_POINT('Ctrl Pts',(-28.8366368301537,12.2594672533841,
128.29525608479)) ;
#128379 = CARTESIAN_POINT('Ctrl Pts',(-28.9466338123818,12.2954707769561,
128.583576517785)) ;
#128380 = CARTESIAN_POINT('Ctrl Pts',(-29.0509389176622,12.4135506751844,
128.854927659037)) ;
#128381 = CARTESIAN_POINT('Ctrl Pts',(-29.1403897390576,12.6014761711869,
129.083399778371)) ;
#128382 = CARTESIAN_POINT('Ctrl Pts',(-29.2118568087512,12.8505488628237,
129.258907374417)) ;
#128383 = CARTESIAN_POINT('Ctrl Pts',(-29.2593420955227,13.1393106619413,
129.364567360262)) ;
#128384 = CARTESIAN_POINT('Ctrl Pts',(-29.2808077434692,13.4495612623856,
129.394071968734)) ;
#128385 = CARTESIAN_POINT('Ctrl Pts',(-29.2752058123139,13.756653092605,129.344650587175)) ;
#128386 = CARTESIAN_POINT('Ctrl Pts',(-29.2437772223513,14.0404143429371,
129.219716781372)) ;
#128387 = CARTESIAN_POINT('Ctrl Pts',(-29.1895572127953,14.279856789825,129.0282438534)) ;
#128388 = CARTESIAN_POINT('Ctrl Pts',(-29.1165343233898,14.458860778503,128.781619840087)) ;
#128389 = CARTESIAN_POINT('Ctrl Pts',(-29.031917285075,14.5622468104248,128.501448866349)) ;
#128390 = CARTESIAN_POINT('Ctrl Pts',(-28.9413153955084,14.5847589311911,
128.20360102239)) ;
#128391 = CARTESIAN_POINT('Ctrl Pts',(-28.852659173099,14.5239999496504,127.911543146827)) ;
#128392 = CARTESIAN_POINT('Ctrl Pts',(-28.7725575058144,14.3842926160759,
127.644392979789)) ;
#128393 = CARTESIAN_POINT('Ctrl Pts',(-28.7077697133043,14.1758059361387,
127.42201331714)) ;
#128394 = CARTESIAN_POINT('Ctrl Pts',(-28.6635064080337,13.9130884623637,
127.259547291412)) ;
#128395 = CARTESIAN_POINT('Ctrl Pts',(-28.6438464264205,13.6151580257587,
127.168954786691)) ;
#128396 = CARTESIAN_POINT('Ctrl Pts',(-28.6507323999107,13.3050554492312,
127.156078639561)) ;
#128397 = CARTESIAN_POINT('Ctrl Pts',(-28.6844706073222,13.0018871941951,
127.221480450194)) ;
#128398 = CARTESIAN_POINT('Ctrl Pts',(-28.7434079227776,12.7291798147193,
127.360525108011)) ;
#128399 = CARTESIAN_POINT('Ctrl Pts',(-28.8240272464479,12.5061726886818,
127.562903271445)) ;
#128400 = CARTESIAN_POINT('Ctrl Pts',(-28.9211857020816,12.3489726322612,
127.813628136945)) ;
#128401 = CARTESIAN_POINT('Ctrl Pts',(-29.0288509697157,12.2685650125514,
128.095007724897)) ;
#128402 = CARTESIAN_POINT('Ctrl Pts',(-29.1398395878935,12.2709027437165,
128.386124146203)) ;
#128403 = CARTESIAN_POINT('Ctrl Pts',(-29.2471199620601,12.3558100296643,
128.666375223964)) ;
#128404 = CARTESIAN_POINT('Ctrl Pts',(-29.3435765060887,12.5172181925544,
128.915021176286)) ;
#128405 = CARTESIAN_POINT('Ctrl Pts',(-29.4230016530534,12.7432705327431,
129.113946346094)) ;
#128406 = CARTESIAN_POINT('Ctrl Pts',(-29.4806020538058,13.0180147425716,
129.249103251234)) ;
#128407 = CARTESIAN_POINT('Ctrl Pts',(-29.5129367891446,13.3228199509295,
129.310342652135)) ;
#128408 = CARTESIAN_POINT('Ctrl Pts',(-29.5182457127061,13.6334362143055,
129.292785636343)) ;
#128409 = CARTESIAN_POINT('Ctrl Pts',(-29.4970691972156,13.9294163259488,
129.197808986286)) ;
#128410 = CARTESIAN_POINT('Ctrl Pts',(-29.4516279224043,14.18915702975,129.031962445103)) ;
#128411 = CARTESIAN_POINT('Ctrl Pts',(-29.38555463668,14.3946402056162,128.805710456645)) ;
#128412 = CARTESIAN_POINT('Ctrl Pts',(-29.3051006300722,14.5295568967571,
128.537671661422)) ;
#128413 = CARTESIAN_POINT('Ctrl Pts',(-29.2156162984668,14.5858061312981,
128.24299020634)) ;
#128414 = CARTESIAN_POINT('Ctrl Pts',(-29.1256218105219,14.5585141748975,
127.947102079717)) ;
#128415 = CARTESIAN_POINT('Ctrl Pts',(-29.0411499046358,14.4500372195652,
127.6671917137)) ;
#128416 = CARTESIAN_POINT('Ctrl Pts',(-28.9695106659263,14.268202021056,127.424830618279)) ;
#128417 = CARTESIAN_POINT('Ctrl Pts',(-28.916234737592,14.0250734165881,127.23599524268)) ;
#128418 = CARTESIAN_POINT('Ctrl Pts',(-28.886235807132,13.7389393522913,127.115203743576)) ;
#128419 = CARTESIAN_POINT('Ctrl Pts',(-28.8822715294914,13.4311037013635,
127.070559670291)) ;
#128420 = CARTESIAN_POINT('Ctrl Pts',(-28.9050595797916,13.1229020286871,
127.104098985504)) ;
#128421 = CARTESIAN_POINT('Ctrl Pts',(-28.9545277915126,12.8333723840705,
127.215232014648)) ;
#128422 = CARTESIAN_POINT('Ctrl Pts',(-29.0265929326767,12.5895126798869,
127.392798802451)) ;
#128423 = CARTESIAN_POINT('Ctrl Pts',(-29.1179608932549,12.4035405009807,
127.626511481168)) ;
#128424 = CARTESIAN_POINT('Ctrl Pts',(-29.2220069817726,12.2914040510789,
127.897399185991)) ;
#128425 = CARTESIAN_POINT('Ctrl Pts',(-29.3324362163145,12.2598122659222,
128.186893232235)) ;
#128426 = CARTESIAN_POINT('Ctrl Pts',(-29.4422937713978,12.3118570167027,
128.474622048651)) ;
#128427 = CARTESIAN_POINT('Ctrl Pts',(-29.543658306718,12.4430958660728,128.737686840452)) ;
#128428 = CARTESIAN_POINT('Ctrl Pts',(-29.6307859317786,12.6447072426792,
128.959070012672)) ;
#128429 = CARTESIAN_POINT('Ctrl Pts',(-29.6979080984891,12.9030426920416,
129.121922285674)) ;
#128430 = CARTESIAN_POINT('Ctrl Pts',(-29.7405762601076,13.1970328957413,
129.21353301064)) ;
#128431 = CARTESIAN_POINT('Ctrl Pts',(-29.7568965621962,13.5084312803207,
129.228029321592)) ;
#128432 = CARTESIAN_POINT('Ctrl Pts',(-29.7463599115322,13.8121187578149,
129.164257165231)) ;
#128433 = CARTESIAN_POINT('Ctrl Pts',(-29.7101954494671,14.0900961815241,
129.025358610877)) ;
#128434 = CARTESIAN_POINT('Ctrl Pts',(-29.6521594765737,14.318729906323,128.822783597689)) ;
#128435 = CARTESIAN_POINT('Ctrl Pts',(-29.5763427713784,14.4844226904234,
128.568010036296)) ;
#128436 = CARTESIAN_POINT('Ctrl Pts',(-29.4902471364353,14.5727758768623,
128.283555618442)) ;
#128437 = CARTESIAN_POINT('Ctrl Pts',(-29.3994772571984,14.5796460537581,
127.985241974566)) ;
#128438 = CARTESIAN_POINT('Ctrl Pts',(-29.3118586977747,14.5035865884274,
127.696186441973)) ;
#128439 = CARTESIAN_POINT('Ctrl Pts',(-29.2340134258281,14.3497063605797,
127.435569924992)) ;
#128440 = CARTESIAN_POINT('Ctrl Pts',(-29.1726986774846,14.1291330540675,
127.223271531018)) ;
#128441 = CARTESIAN_POINT('Ctrl Pts',(-29.1330506360304,13.8597727323871,
127.074476720364)) ;
#128442 = CARTESIAN_POINT('Ctrl Pts',(-29.1181810101493,13.5574624461298,
126.997854047056)) ;
#128443 = CARTESIAN_POINT('Ctrl Pts',(-29.1301796266018,13.2463366204199,
126.999819620482)) ;
#128444 = CARTESIAN_POINT('Ctrl Pts',(-29.168925343338,12.9472974044437,127.079846391549)) ;
#128445 = CARTESIAN_POINT('Ctrl Pts',(-29.2320422705623,12.6832078495132,
127.231196082457)) ;
#128446 = CARTESIAN_POINT('Ctrl Pts',(-29.3166522738459,12.4704982882043,
127.44506697642)) ;
#128447 = CARTESIAN_POINT('Ctrl Pts',(-29.4160388288635,12.3276823498278,
127.702394373232)) ;
#128448 = CARTESIAN_POINT('Ctrl Pts',(-29.5249829531837,12.2625925248945,
127.987480236836)) ;
#128449 = CARTESIAN_POINT('Ctrl Pts',(-29.6355718959069,12.2806192118825,
128.277501275059)) ;
#128450 = CARTESIAN_POINT('Ctrl Pts',(-29.7417159522391,12.3809214505585,
128.554315315188)) ;
#128451 = CARTESIAN_POINT('Ctrl Pts',(-29.8353905585785,12.5560400972574,
128.794817454638)) ;
#128452 = CARTESIAN_POINT('Ctrl Pts',(-29.9107732205239,12.7918901255773,
128.9820408941)) ;
#128453 = CARTESIAN_POINT('Ctrl Pts',(-29.963902573747,13.0744209582552,129.104054461065)) ;
#128454 = CARTESIAN_POINT('Ctrl Pts',(-29.9911128268477,13.3812416621058,
129.150442107192)) ;
#128455 = CARTESIAN_POINT('Ctrl Pts',(-29.9913457221614,13.6920797035989,
129.117909219499)) ;
#128456 = CARTESIAN_POINT('Ctrl Pts',(-29.9652366276384,13.9824941706661,
129.008541028235)) ;
#128457 = CARTESIAN_POINT('Ctrl Pts',(-29.9157726640117,14.2323227455577,
128.831056214545)) ;
#128458 = CARTESIAN_POINT('Ctrl Pts',(-29.846427467267,14.4258243493526,128.595232400767)) ;
#128459 = CARTESIAN_POINT('Ctrl Pts',(-29.7637490145916,14.5465247232896,
128.320649149057)) ;
#128460 = CARTESIAN_POINT('Ctrl Pts',(-29.6735483660244,14.5869806832562,
128.023905947573)) ;
#128461 = CARTESIAN_POINT('Ctrl Pts',(-29.5842319211393,14.5442058471831,
127.730036702735)) ;
#128462 = CARTESIAN_POINT('Ctrl Pts',(-29.5014998391875,14.4209679601538,
127.455153408588)) ;
#128463 = CARTESIAN_POINT('Ctrl Pts',(-29.4328113829598,14.2257906584797,
127.221317947719)) ;
#128464 = CARTESIAN_POINT('Ctrl Pts',(-29.3838992065976,13.9741287735189,
127.045386859972)) ;
#128465 = CARTESIAN_POINT('Ctrl Pts',(-29.3585749953142,13.6829512518686,
126.938330736026)) ;
#128466 = CARTESIAN_POINT('Ctrl Pts',(-29.3596330007189,13.3714665393579,
126.90816420681)) ;
#128467 = CARTESIAN_POINT('Ctrl Pts',(-29.3876542453033,13.0656058649526,
126.956972860961)) ;
#128468 = CARTESIAN_POINT('Ctrl Pts',(-29.4412418248995,12.7850334641615,
127.080442878594)) ;
#128469 = CARTESIAN_POINT('Ctrl Pts',(-29.5174858728615,12.5496673057456,
127.270047670741)) ;
#128470 = CARTESIAN_POINT('Ctrl Pts',(-29.6117756090028,12.3766688601944,
127.512307064252)) ;
#128471 = CARTESIAN_POINT('Ctrl Pts',(-29.7177855631625,12.2789529253499,
127.788850188799)) ;
#128472 = CARTESIAN_POINT('Ctrl Pts',(-29.8288201491775,12.2634413511376,
128.080046508042)) ;
#128473 = CARTESIAN_POINT('Ctrl Pts',(-29.9370813812663,12.330415688247,128.363307355518)) ;
#128474 = CARTESIAN_POINT('Ctrl Pts',(-30.0370100677037,12.4770343788681,
128.621893210598)) ;
#128475 = CARTESIAN_POINT('Ctrl Pts',(-30.1201623965983,12.6896430070817,
128.831846013391)) ;
#128476 = CARTESIAN_POINT('Ctrl Pts',(-30.1828600429885,12.9554491336733,
128.981881400564)) ;
#128477 = CARTESIAN_POINT('Ctrl Pts',(-30.220821672093,13.2546655218149,129.059678855952)) ;
#128478 = CARTESIAN_POINT('Ctrl Pts',(-30.2320631082474,13.5672374700513,
129.059277137002)) ;
#128479 = CARTESIAN_POINT('Ctrl Pts',(-30.2164917611136,13.8673527502542,
128.980779221117)) ;
#128480 = CARTESIAN_POINT('Ctrl Pts',(-30.1761119033239,14.1367235720608,
128.829720800878)) ;
#128481 = CARTESIAN_POINT('Ctrl Pts',(-30.1138238135701,14.3561276375805,
128.614427243316)) ;
#128482 = CARTESIAN_POINT('Ctrl Pts',(-30.0362416171714,14.5065131525026,
128.354864369659)) ;
#128483 = CARTESIAN_POINT('Ctrl Pts',(-29.9482255340251,14.58061768968,128.06455261143)) ;
#128484 = CARTESIAN_POINT('Ctrl Pts',(-29.8577007140995,14.5715966995796,
127.767049538238)) ;
#128485 = CARTESIAN_POINT('Ctrl Pts',(-29.7710937353391,14.4799160826423,
127.480801972411)) ;
#128486 = CARTESIAN_POINT('Ctrl Pts',(-29.6962601987287,14.3130126299592,
127.229134217292)) ;
#128487 = CARTESIAN_POINT('Ctrl Pts',(-29.6386676158855,14.0821691922297,
127.027760661239)) ;
#128488 = CARTESIAN_POINT('Ctrl Pts',(-29.6033324240906,13.8046645474474,
126.891472664739)) ;
#128489 = CARTESIAN_POINT('Ctrl Pts',(-29.5935128975474,13.4979411063597,
126.829511671003)) ;
#128490 = CARTESIAN_POINT('Ctrl Pts',(-29.6105436734211,13.1889484059184,
126.846331182922)) ;
#128491 = CARTESIAN_POINT('Ctrl Pts',(-29.6541824416548,12.8939178579835,
126.940568159584)) ;
#128492 = CARTESIAN_POINT('Ctrl Pts',(-29.7218865320693,12.637823938518,127.105210089528)) ;
#128493 = CARTESIAN_POINT('Ctrl Pts',(-29.8094196831743,12.4382802201008,
127.327808914552)) ;
#128494 = CARTESIAN_POINT('Ctrl Pts',(-29.9109916726465,12.3092349682175,
127.591516833014)) ;
#128495 = CARTESIAN_POINT('Ctrl Pts',(-30.0213393689754,12.2595575247746,
127.880567063978)) ;
#128496 = CARTESIAN_POINT('Ctrl Pts',(-30.1312298450494,12.2934341304884,
128.168627556378)) ;
#128497 = CARTESIAN_POINT('Ctrl Pts',(-30.2352976730363,12.4080333824313,
128.439480287819)) ;
#128498 = CARTESIAN_POINT('Ctrl Pts',(-30.326263456122,12.5960960423707,128.672002337126)) ;
#128499 = CARTESIAN_POINT('Ctrl Pts',(-30.3979051357112,12.8430835958632,
128.848156216935)) ;
#128500 = CARTESIAN_POINT('Ctrl Pts',(-30.4460602471863,13.1299282675871,
128.955872602164)) ;
#128501 = CARTESIAN_POINT('Ctrl Pts',(-30.4683932727674,13.4413370820985,
128.987758396516)) ;
#128502 = CARTESIAN_POINT('Ctrl Pts',(-30.4634997449438,13.7480777778484,
128.940482113583)) ;
#128503 = CARTESIAN_POINT('Ctrl Pts',(-30.4328079191952,14.0327532847483,
128.817708039455)) ;
#128504 = CARTESIAN_POINT('Ctrl Pts',(-30.379231368512,14.2736050816731,128.628136710123)) ;
#128505 = CARTESIAN_POINT('Ctrl Pts',(-30.3066075793135,14.454731415087,128.382652806639)) ;
#128506 = CARTESIAN_POINT('Ctrl Pts',(-30.2223698139022,14.5602675657722,
128.103634816694)) ;
#128507 = CARTESIAN_POINT('Ctrl Pts',(-30.1317618838712,14.5853381818847,
127.805744051885)) ;
#128508 = CARTESIAN_POINT('Ctrl Pts',(-30.0428613703553,14.5268296040502,
127.512936641818)) ;
#128509 = CARTESIAN_POINT('Ctrl Pts',(-29.962463860033,14.3893357844739,127.244942389594)) ;
#128510 = CARTESIAN_POINT('Ctrl Pts',(-29.8971381429269,14.1825587222419,
127.020978714071)) ;
#128511 = CARTESIAN_POINT('Ctrl Pts',(-29.8522544707252,13.9213688559687,
126.856729894108)) ;
#128512 = CARTESIAN_POINT('Ctrl Pts',(-29.8318542419191,13.6242448062503,
126.763980055816)) ;
#128513 = CARTESIAN_POINT('Ctrl Pts',(-29.8378630021939,13.3143404196874,
126.748558862791)) ;
#128514 = CARTESIAN_POINT('Ctrl Pts',(-29.8712285537645,13.0084390891239,
126.812618139704)) ;
#128515 = CARTESIAN_POINT('Ctrl Pts',(-29.929011094758,12.7371909250803,126.948597866911)) ;
#128516 = CARTESIAN_POINT('Ctrl Pts',(-30.0093157978428,12.5114338285413,
127.149921316815)) ;
#128517 = CARTESIAN_POINT('Ctrl Pts',(-30.1060566735137,12.3524149668545,
127.399449942956)) ;
#128518 = CARTESIAN_POINT('Ctrl Pts',(-30.2136485926951,12.2696328079286,
127.680573993983)) ;
#128519 = CARTESIAN_POINT('Ctrl Pts',(-30.3245815643694,12.2697667262583,
127.971545918026)) ;
#128520 = CARTESIAN_POINT('Ctrl Pts',(-30.4318960813969,12.352219690353,128.251950244621)) ;
#128521 = CARTESIAN_POINT('Ctrl Pts',(-30.5288090204638,12.5116177208884,
128.501911593616)) ;
#128522 = CARTESIAN_POINT('Ctrl Pts',(-30.6088324049079,12.7360826900141,
128.702573395884)) ;
#128523 = CARTESIAN_POINT('Ctrl Pts',(-30.6672434975921,13.0105746787141,
128.840001522892)) ;
#128524 = CARTESIAN_POINT('Ctrl Pts',(-30.7001840342553,13.3146278251872,
128.903042642514)) ;
#128525 = CARTESIAN_POINT('Ctrl Pts',(-30.7062603799839,13.6243831521928,
128.887830433908)) ;
#128526 = CARTESIAN_POINT('Ctrl Pts',(-30.6857673468596,13.9217978,128.794770598986)) ;
#128527 = CARTESIAN_POINT('Ctrl Pts',(-30.6410536399538,14.1821018146301,
128.631134773941)) ;
#128528 = CARTESIAN_POINT('Ctrl Pts',(-30.5756154839279,14.389412327527,128.406768739336)) ;
#128529 = CARTESIAN_POINT('Ctrl Pts',(-30.4952269467035,14.5268848285114,
128.138811005496)) ;
#128530 = CARTESIAN_POINT('Ctrl Pts',(-30.4061762996858,14.5852561648766,
127.845506483541)) ;
#128531 = CARTESIAN_POINT('Ctrl Pts',(-30.3160687878258,14.5605921402289,
127.54927187433)) ;
#128532 = CARTESIAN_POINT('Ctrl Pts',(-30.2312252040183,14.4542388550499,
127.268234257609)) ;
#128533 = CARTESIAN_POINT('Ctrl Pts',(-30.1590863849219,14.2743936343232,
127.024407772696)) ;
#128534 = CARTESIAN_POINT('Ctrl Pts',(-30.105107623007,14.0316377250169,126.833390090339)) ;
#128535 = CARTESIAN_POINT('Ctrl Pts',(-30.074596777505,13.7487556151288,126.711369355274)) ;
#128536 = CARTESIAN_POINT('Ctrl Pts',(-30.0698043518736,13.4387761363986,
126.664030655711)) ;
#128537 = CARTESIAN_POINT('Ctrl Pts',(-30.0918266077804,13.1317846555727,
126.695496010489)) ;
#128538 = CARTESIAN_POINT('Ctrl Pts',(-30.1405764170373,12.8410201879509,
126.804495127875)) ;
#128539 = CARTESIAN_POINT('Ctrl Pts',(-30.2118505192796,12.5963885995688,
126.97984040817)) ;
#128540 = CARTESIAN_POINT('Ctrl Pts',(-30.3025467713188,12.4083250165559,
127.211632452948)) ;
#128541 = CARTESIAN_POINT('Ctrl Pts',(-30.4070074692118,12.2932606232103,
127.483511429842)) ;
#128542 = CARTESIAN_POINT('Ctrl Pts',(-30.5168319442806,12.2596773192959,
127.771399740132)) ;
#128543 = CARTESIAN_POINT('Ctrl Pts',(-30.6267559112214,12.3089369828892,
128.05934301133)) ;
#128544 = CARTESIAN_POINT('Ctrl Pts',(-30.7288700245111,12.4384179061081,
128.324470423332)) ;
#128545 = CARTESIAN_POINT('Ctrl Pts',(-30.8165456041534,12.6389284410988,
128.547392027086)) ;
#128546 = CARTESIAN_POINT('Ctrl Pts',(-30.8838110091402,12.893636868565,128.710941823021)) ;
#128547 = CARTESIAN_POINT('Ctrl Pts',(-30.9276213515713,13.1890353043008,
128.805628637926)) ;
#128548 = CARTESIAN_POINT('Ctrl Pts',(-30.9445789357736,13.4997523656822,
128.822052819352)) ;
#128549 = CARTESIAN_POINT('Ctrl Pts',(-30.9347706434733,13.8039808891053,
128.760392828068)) ;
#128550 = CARTESIAN_POINT('Ctrl Pts',(-30.8994647064315,14.0820721620834,
128.624129866457)) ;
#128551 = CARTESIAN_POINT('Ctrl Pts',(-30.8418621446897,14.3130040763869,
128.422725422754)) ;
#128552 = CARTESIAN_POINT('Ctrl Pts',(-30.7668395761858,14.4800545179009,
128.170430933106)) ;
#128553 = CARTESIAN_POINT('Ctrl Pts',(-30.680746802464,14.5714591887958,127.885882008623)) ;
#128554 = CARTESIAN_POINT('Ctrl Pts',(-30.5895443226898,14.5804983866051,
127.586142612422)) ;
#128555 = CARTESIAN_POINT('Ctrl Pts',(-30.5021757835081,14.5069052438345,
127.297974852668)) ;
#128556 = CARTESIAN_POINT('Ctrl Pts',(-30.4240484083233,14.3557029930728,
127.036595527731)) ;
#128557 = CARTESIAN_POINT('Ctrl Pts',(-30.3620588834699,14.1367619821381,
126.822288296533)) ;
#128558 = CARTESIAN_POINT('Ctrl Pts',(-30.3216036763726,13.868069374817,126.671065060371)) ;
#128559 = CARTESIAN_POINT('Ctrl Pts',(-30.3060292758437,13.5652242868234,
126.592265896191)) ;
#128560 = CARTESIAN_POINT('Ctrl Pts',(-30.3172275810128,13.2558696695954,
126.592085413816)) ;
#128561 = CARTESIAN_POINT('Ctrl Pts',(-30.3551569478567,12.9557646560496,
126.669693553558)) ;
#128562 = CARTESIAN_POINT('Ctrl Pts',(-30.4177746688459,12.6900042149153,
126.819521572026)) ;
#128563 = CARTESIAN_POINT('Ctrl Pts',(-30.5015283801077,12.4761055498728,
127.031005340898)) ;
#128564 = CARTESIAN_POINT('Ctrl Pts',(-30.6010714282225,12.3304586673531,
127.288616121173)) ;
#128565 = CARTESIAN_POINT('Ctrl Pts',(-30.7093303383292,12.2634381617438,
127.571864331077)) ;
#128566 = CARTESIAN_POINT('Ctrl Pts',(-30.8202059528667,12.278878358219,127.862647845452)) ;
#128567 = CARTESIAN_POINT('Ctrl Pts',(-30.9264645765518,12.3768659810513,
128.139835217685)) ;
#128568 = CARTESIAN_POINT('Ctrl Pts',(-31.020570079013,12.5495630151977,128.381622987538)) ;
#128569 = CARTESIAN_POINT('Ctrl Pts',(-31.0969863841414,12.7855771404834,
128.571643774732)) ;
#128570 = CARTESIAN_POINT('Ctrl Pts',(-31.1504119228565,13.0654345066809,
128.694731648829)) ;
#128571 = CARTESIAN_POINT('Ctrl Pts',(-31.178486934808,13.3720089206918,128.743618229046)) ;
#128572 = CARTESIAN_POINT('Ctrl Pts',(-31.1795061531803,13.682435682329,128.713449748328)) ;
#128573 = CARTESIAN_POINT('Ctrl Pts',(-31.1542831813261,13.9739144742565,
128.606673201807)) ;
#128574 = CARTESIAN_POINT('Ctrl Pts',(-31.1049759678819,14.2268633708939,
128.429387198208)) ;
#128575 = CARTESIAN_POINT('Ctrl Pts',(-31.0367913472421,14.4204385553042,
128.197281287674)) ;
#128576 = CARTESIAN_POINT('Ctrl Pts',(-30.9536916763409,14.5445800987763,
127.921159574163)) ;
#128577 = CARTESIAN_POINT('Ctrl Pts',(-30.864182473291,14.5868220518321,127.626665385691)) ;
#128578 = CARTESIAN_POINT('Ctrl Pts',(-30.7745931280078,14.5468039105965,
127.331938979369)) ;
#128579 = CARTESIAN_POINT('Ctrl Pts',(-30.6912840406938,14.4251034051228,
127.055252613028)) ;
#128580 = CARTESIAN_POINT('Ctrl Pts',(-30.6224350856795,14.2325286580178,
126.821087436355)) ;
#128581 = CARTESIAN_POINT('Ctrl Pts',(-30.5727594385633,13.9823226151408,
126.642904834629)) ;
#128582 = CARTESIAN_POINT('Ctrl Pts',(-30.5466732188835,13.6900857770298,
126.533419749319)) ;
#128583 = CARTESIAN_POINT('Ctrl Pts',(-30.5470186669781,13.3811330160851,
126.501422391633)) ;
#128584 = CARTESIAN_POINT('Ctrl Pts',(-30.5742267919639,13.0742212220075,
126.547788430997)) ;
#128585 = CARTESIAN_POINT('Ctrl Pts',(-30.6272128351288,12.7922256015956,
126.669455909412)) ;
#128586 = CARTESIAN_POINT('Ctrl Pts',(-30.7031024608963,12.5548594273492,
126.857944851666)) ;
#128587 = CARTESIAN_POINT('Ctrl Pts',(-30.796900428706,12.3804086470547,127.098812566014)) ;
#128588 = CARTESIAN_POINT('Ctrl Pts',(-30.9021655709172,12.2809059803651,
127.373332007797)) ;
#128589 = CARTESIAN_POINT('Ctrl Pts',(-31.0130340334026,12.2624888492441,
127.664081167876)) ;
#128590 = CARTESIAN_POINT('Ctrl Pts',(-31.122092423042,12.3276777056696,127.949470767987)) ;
#128591 = CARTESIAN_POINT('Ctrl Pts',(-31.2215356799451,12.4707929028479,
128.206930407151)) ;
#128592 = CARTESIAN_POINT('Ctrl Pts',(-31.3057861593304,12.6823314150819,
128.41991397547)) ;
#128593 = CARTESIAN_POINT('Ctrl Pts',(-31.3692927733241,12.9478031848441,
128.572215489217)) ;
#128594 = CARTESIAN_POINT('Ctrl Pts',(-31.4079487674031,13.2466923660168,
128.652010448141)) ;
#128595 = CARTESIAN_POINT('Ctrl Pts',(-31.4198806266106,13.5583772827196,
128.653714268614)) ;
#128596 = CARTESIAN_POINT('Ctrl Pts',(-31.4051154738825,13.8592556728242,
128.577564219372)) ;
#128597 = CARTESIAN_POINT('Ctrl Pts',(-31.3650985633522,14.1306425332548,
128.42742562908)) ;
#128598 = CARTESIAN_POINT('Ctrl Pts',(-31.3041188903048,14.3493759860233,
128.216343523251)) ;
#128599 = CARTESIAN_POINT('Ctrl Pts',(-31.2263226071039,14.5035317541652,
127.955864143457)) ;
#128600 = CARTESIAN_POINT('Ctrl Pts',(-31.1386623199781,14.5795845052791,
127.666673105791)) ;
#128601 = CARTESIAN_POINT('Ctrl Pts',(-31.0479383571274,14.5729335586883,
127.368514322624)) ;
#128602 = CARTESIAN_POINT('Ctrl Pts',(-30.9614128878974,14.4838964903463,
127.082628198769)) ;
#128603 = CARTESIAN_POINT('Ctrl Pts',(-30.8859576009587,14.3187457579905,
126.829059953283)) ;
#128604 = CARTESIAN_POINT('Ctrl Pts',(-30.827869755057,14.0897675929633,126.626282491058)) ;
#128605 = CARTESIAN_POINT('Ctrl Pts',(-30.7918178978922,13.8134082777409,
126.487898906566)) ;
#128606 = CARTESIAN_POINT('Ctrl Pts',(-30.7811885297415,13.5073936360873,
126.423595807509)) ;
#128607 = CARTESIAN_POINT('Ctrl Pts',(-30.7974836212486,13.1976577168155,
126.438200350331)) ;
#128608 = CARTESIAN_POINT('Ctrl Pts',(-30.8402132756921,12.9027229695694,
126.529888850786)) ;
#128609 = CARTESIAN_POINT('Ctrl Pts',(-30.9073353624577,12.6448108497487,
126.692775559665)) ;
#128610 = CARTESIAN_POINT('Ctrl Pts',(-30.9941421316234,12.4434495713625,
126.913315381037)) ;
#128611 = CARTESIAN_POINT('Ctrl Pts',(-31.0963533136014,12.311375978469,127.1785845358)) ;
#128612 = CARTESIAN_POINT('Ctrl Pts',(-31.2053832704872,12.2599503304442,
127.464153622351)) ;
#128613 = CARTESIAN_POINT('Ctrl Pts',(-31.3162358384633,12.2913693228783,
127.754756534569)) ;
#128614 = CARTESIAN_POINT('Ctrl Pts',(-31.4202678196451,12.4038516035479,
128.025596697049)) ;
#128615 = CARTESIAN_POINT('Ctrl Pts',(-31.5114357995679,12.5892626487071,
128.258807733841)) ;
#128616 = CARTESIAN_POINT('Ctrl Pts',(-31.5837749041298,12.8342966709516,
128.43702813475)) ;
#128617 = CARTESIAN_POINT('Ctrl Pts',(-31.6329366574186,13.122430567382,128.547436490595)) ;
#128618 = CARTESIAN_POINT('Ctrl Pts',(-31.6558392024168,13.4307504322514,
128.58129064855)) ;
#128619 = CARTESIAN_POINT('Ctrl Pts',(-31.651838811182,13.7394115392885,128.53645443935)) ;
#128620 = CARTESIAN_POINT('Ctrl Pts',(-31.6218261093011,14.0250582517609,
128.415667947021)) ;
#128621 = CARTESIAN_POINT('Ctrl Pts',(-31.568744981883,14.2676857548662,128.227489788221)) ;
#128622 = CARTESIAN_POINT('Ctrl Pts',(-31.4969069521766,14.4501343766899,
127.984446191423)) ;
#128623 = CARTESIAN_POINT('Ctrl Pts',(-31.4125135319878,14.5585281665325,
127.704800678518)) ;
#128624 = CARTESIAN_POINT('Ctrl Pts',(-31.3222180587387,14.5857500272389,
127.407919510387)) ;
#128625 = CARTESIAN_POINT('Ctrl Pts',(-31.2330255116186,14.5296138269876,
127.114203416447)) ;
#128626 = CARTESIAN_POINT('Ctrl Pts',(-31.152297925257,14.3940563657681,126.845238279208)) ;
#128627 = CARTESIAN_POINT('Ctrl Pts',(-31.0866327665665,14.1896706330216,
126.620373125619)) ;
#128628 = CARTESIAN_POINT('Ctrl Pts',(-31.0410079108427,13.9296795635546,
126.453929783066)) ;
#128629 = CARTESIAN_POINT('Ctrl Pts',(-31.0198252619641,13.6325613783442,
126.358817925513)) ;
#128630 = CARTESIAN_POINT('Ctrl Pts',(-31.0251775966313,13.3229079884786,
126.341491446272)) ;
#128631 = CARTESIAN_POINT('Ctrl Pts',(-31.0574272726707,13.018526691074,126.402527072906)) ;
#128632 = CARTESIAN_POINT('Ctrl Pts',(-31.1149307246031,12.7436673997071,
126.537409276898)) ;
#128633 = CARTESIAN_POINT('Ctrl Pts',(-31.1948445839553,12.5164978954953,
126.737575762028)) ;
#128634 = CARTESIAN_POINT('Ctrl Pts',(-31.2908244908384,12.3560840259889,
126.985005769363)) ;
#128635 = CARTESIAN_POINT('Ctrl Pts',(-31.3982222730911,12.2708854791944,
127.265554907763)) ;
#128636 = CARTESIAN_POINT('Ctrl Pts',(-31.5090110903784,12.2685612121641,
127.556147236131)) ;
#128637 = CARTESIAN_POINT('Ctrl Pts',(-31.6167270045284,12.3486009748257,
127.837672372458)) ;
#128638 = CARTESIAN_POINT('Ctrl Pts',(-31.7143963508923,12.5069430780995,
128.089696718975)) ;
#128639 = CARTESIAN_POINT('Ctrl Pts',(-31.7944473102828,12.7284059514765,
128.290650681508)) ;
#128640 = CARTESIAN_POINT('Ctrl Pts',(-31.8537556036786,13.0024845577893,
128.430595808369)) ;
#128641 = CARTESIAN_POINT('Ctrl Pts',(-31.8873667080622,13.3053156304276,
128.495676226259)) ;
#128642 = CARTESIAN_POINT('Ctrl Pts',(-31.8942276117398,13.6156286955051,
128.482698931289)) ;
#128643 = CARTESIAN_POINT('Ctrl Pts',(-31.874614953271,13.9128849931579,128.392322884504)) ;
#128644 = CARTESIAN_POINT('Ctrl Pts',(-31.8301744732298,14.1766185287715,
128.229209877233)) ;
#128645 = CARTESIAN_POINT('Ctrl Pts',(-31.7652924085922,14.3847398624139,
128.00655809334)) ;
#128646 = CARTESIAN_POINT('Ctrl Pts',(-31.6855395448521,14.5238361005913,
127.740570860147)) ;
#128647 = CARTESIAN_POINT('Ctrl Pts',(-31.5967590744194,14.5847743012247,
127.448098544404)) ;
#128648 = CARTESIAN_POINT('Ctrl Pts',(-31.506226561888,14.5623309410939,127.150482506814)) ;
#128649 = CARTESIAN_POINT('Ctrl Pts',(-31.4212470448233,14.4584178167976,
126.869109281522)) ;
#128650 = CARTESIAN_POINT('Ctrl Pts',(-31.3484135635736,14.2791868777477,
126.623076819461)) ;
#128651 = CARTESIAN_POINT('Ctrl Pts',(-31.2945026699446,14.0415187113142,
126.43273117346)) ;
#128652 = CARTESIAN_POINT('Ctrl Pts',(-31.2628395727632,13.7564325349983,
126.306943352975)) ;
#128653 = CARTESIAN_POINT('Ctrl Pts',(-31.2573021812649,13.4495648560064,
126.25774099448)) ;
#128654 = CARTESIAN_POINT('Ctrl Pts',(-31.2787325571399,13.1394167838631,
126.287153636745)) ;
#128655 = CARTESIAN_POINT('Ctrl Pts',(-31.3262043092987,12.8508801265976,
126.392794087326)) ;
#128656 = CARTESIAN_POINT('Ctrl Pts',(-31.3973555378242,12.6022770159485,
126.567478978667)) ;
#128657 = CARTESIAN_POINT('Ctrl Pts',(-31.4875544873303,12.4127865779696,
126.797861062289)) ;
#128658 = CARTESIAN_POINT('Ctrl Pts',(-31.5916801030867,12.2953916612225,
127.068766817743)) ;
#128659 = CARTESIAN_POINT('Ctrl Pts',(-31.7016585324409,12.2594835082488,
127.357036513685)) ;
#128660 = CARTESIAN_POINT('Ctrl Pts',(-31.8114792326934,12.3065006906036,
127.644739812586)) ;
#128661 = CARTESIAN_POINT('Ctrl Pts',(-31.9136506042724,12.4331949897075,
127.910131486488)) ;
#128662 = CARTESIAN_POINT('Ctrl Pts',(-32.0021581499909,12.6325251060339,
128.135361000495)) ;
#128663 = CARTESIAN_POINT('Ctrl Pts',(-32.0699206406892,12.8854153923965,
128.300428648216)) ;
#128664 = CARTESIAN_POINT('Ctrl Pts',(-32.1145088127622,13.1803566705807,
128.397344288992)) ;
#128665 = CARTESIAN_POINT('Ctrl Pts',(-32.1322228503466,13.4893561125358,
128.416143886401)) ;
#128666 = CARTESIAN_POINT('Ctrl Pts',(-32.1232591607492,13.7954470549273,
128.3568066441)) ;
#128667 = CARTESIAN_POINT('Ctrl Pts',(-32.0884938852697,14.0751705086754,
128.222048043325)) ;
#128668 = CARTESIAN_POINT('Ctrl Pts',(-32.0316136936814,14.3069080353192,
128.022850396701)) ;
#128669 = CARTESIAN_POINT('Ctrl Pts',(-31.9571154459696,14.4762412985565,
127.772108801005)) ;
#128670 = CARTESIAN_POINT('Ctrl Pts',(-31.8705406479889,14.5702449672957,
127.485888969575)) ;
#128671 = CARTESIAN_POINT('Ctrl Pts',(-31.7802131912547,14.5813885693018,
127.18902186086)) ;
#128672 = CARTESIAN_POINT('Ctrl Pts',(-31.6921805635413,14.5100796907114,
126.898736602283)) ;
#128673 = CARTESIAN_POINT('Ctrl Pts',(-31.6135814334297,14.3602445312062,
126.635913485129)) ;
#128674 = CARTESIAN_POINT('Ctrl Pts',(-31.5512501881816,14.143253231573,126.420675039755)) ;
#128675 = CARTESIAN_POINT('Ctrl Pts',(-31.5102927844524,13.8766590298569,
126.268096359863)) ;
#128676 = CARTESIAN_POINT('Ctrl Pts',(-31.4938914974148,13.575471217549,126.186984552435)) ;
#128677 = CARTESIAN_POINT('Ctrl Pts',(-31.5042851715475,13.2645668941717,
126.184291805469)) ;
#128678 = CARTESIAN_POINT('Ctrl Pts',(-31.5416101926573,12.9634277851347,
126.260085507192)) ;
#128679 = CARTESIAN_POINT('Ctrl Pts',(-31.603403047589,12.6972349094739,126.407598556958)) ;
#128680 = CARTESIAN_POINT('Ctrl Pts',(-31.6864963503388,12.4817230619034,
126.617187473906)) ;
#128681 = CARTESIAN_POINT('Ctrl Pts',(-31.7855804706592,12.3338051971936,
126.873476664401)) ;
#128682 = CARTESIAN_POINT('Ctrl Pts',(-31.8940109328035,12.2641456022445,
127.157120420535)) ;
#128683 = CARTESIAN_POINT('Ctrl Pts',(-32.0048441796899,12.2773535712523,
127.447802163778)) ;
#128684 = CARTESIAN_POINT('Ctrl Pts',(-32.1110952849965,12.3726334671979,
127.725051534391)) ;
#128685 = CARTESIAN_POINT('Ctrl Pts',(-32.2057756328295,12.5434758401697,
127.968470739376)) ;
#128686 = CARTESIAN_POINT('Ctrl Pts',(-32.2825877687635,12.7769497642035,
128.159760257596)) ;
#128687 = CARTESIAN_POINT('Ctrl Pts',(-32.3370473742439,13.0568799766939,
128.285720331795)) ;
#128688 = CARTESIAN_POINT('Ctrl Pts',(-32.3658593623225,13.3636449455261,
128.336699481122)) ;
#128689 = CARTESIAN_POINT('Ctrl Pts',(-32.367624242602,13.6733774469028,128.308803267629)) ;
#128690 = CARTESIAN_POINT('Ctrl Pts',(-32.3432185179846,13.9654380896254,
128.204448266785)) ;
#128691 = CARTESIAN_POINT('Ctrl Pts',(-32.2945201685348,14.220301269476,128.028893057304)) ;
#128692 = CARTESIAN_POINT('Ctrl Pts',(-32.2266394712445,14.415947045335,127.797606163458)) ;
#128693 = CARTESIAN_POINT('Ctrl Pts',(-32.1443774332964,14.5416943673476,
127.524134752044)) ;
#128694 = CARTESIAN_POINT('Ctrl Pts',(-32.0546246272659,14.586901890039,127.228790865626)) ;
#128695 = CARTESIAN_POINT('Ctrl Pts',(-31.9648061180443,14.5489491303822,
126.933344138451)) ;
#128696 = CARTESIAN_POINT('Ctrl Pts',(-31.8814753129527,14.4300240451422,
126.656711926884)) ;
#128697 = CARTESIAN_POINT('Ctrl Pts',(-31.8118574558951,14.2387296185005,
126.420176396939)) ;
#128698 = CARTESIAN_POINT('Ctrl Pts',(-31.761673966027,13.9899469010905,126.24053385049)) ;
#128699 = CARTESIAN_POINT('Ctrl Pts',(-31.7349367720515,13.7002922366985,
126.129329442407)) ;
#128700 = CARTESIAN_POINT('Ctrl Pts',(-31.7343309734707,13.3909003145637,
126.094475834364)) ;
#128701 = CARTESIAN_POINT('Ctrl Pts',(-31.7609570476832,13.0819914408663,
126.138968768874)) ;
#128702 = CARTESIAN_POINT('Ctrl Pts',(-31.8131240309607,12.8000707339927,
126.258359081467)) ;
#128703 = CARTESIAN_POINT('Ctrl Pts',(-31.888138344661,12.5616134870626,126.444378873037)) ;
#128704 = CARTESIAN_POINT('Ctrl Pts',(-31.9816543195415,12.384449895012,126.684347395518)) ;
#128705 = CARTESIAN_POINT('Ctrl Pts',(-32.0872024405474,12.2824628240901,
126.959534123693)) ;
#128706 = CARTESIAN_POINT('Ctrl Pts',(-32.1974420894517,12.2618989594336,
127.24862212855)) ;
#128707 = CARTESIAN_POINT('Ctrl Pts',(-32.3067993093919,12.3245801439636,
127.534843652708)) ;
#128708 = CARTESIAN_POINT('Ctrl Pts',(-32.4066055596616,12.4655889841413,
127.793363677931)) ;
#128709 = CARTESIAN_POINT('Ctrl Pts',(-32.4913685339639,12.6753258327154,
128.007846379507)) ;
#128710 = CARTESIAN_POINT('Ctrl Pts',(-32.5554823861655,12.9389695306945,
128.16198128378)) ;
#128711 = CARTESIAN_POINT('Ctrl Pts',(-32.5949571555968,13.2377441429055,
128.244099164765)) ;
#128712 = CARTESIAN_POINT('Ctrl Pts',(-32.6077198111152,13.5478077720715,
128.248401750288)) ;
#128713 = CARTESIAN_POINT('Ctrl Pts',(-32.5936618530778,13.8515135114459,
128.17407137325)) ;
#128714 = CARTESIAN_POINT('Ctrl Pts',(-32.5544078906928,14.1231097110526,
128.026278350984)) ;
#128715 = CARTESIAN_POINT('Ctrl Pts',(-32.4939018766822,14.3439546593352,
127.816519602292)) ;
#128716 = CARTESIAN_POINT('Ctrl Pts',(-32.4167043659917,14.4998916999394,
127.557878330328)) ;
#128717 = CARTESIAN_POINT('Ctrl Pts',(-32.3289439608214,14.5786386436238,
127.268277216763)) ;
#128718 = CARTESIAN_POINT('Ctrl Pts',(-32.2382575988989,14.5742675055765,
126.970251402823)) ;
#128719 = CARTESIAN_POINT('Ctrl Pts',(-32.1514513694804,14.4873447057953,
126.683513861479)) ;
#128720 = CARTESIAN_POINT('Ctrl Pts',(-32.0758339074813,14.324791387065,126.429581664298)) ;
#128721 = CARTESIAN_POINT('Ctrl Pts',(-32.0169662101716,14.0970302215938,
126.22444258051)) ;
#128722 = CARTESIAN_POINT('Ctrl Pts',(-31.9801979886195,13.8204923791666,
126.083834586045)) ;
#128723 = CARTESIAN_POINT('Ctrl Pts',(-31.9689269120259,13.5164549549645,
126.017822987684)) ;
#128724 = CARTESIAN_POINT('Ctrl Pts',(-31.9844450832782,13.2060699844781,
126.030100813649)) ;
#128725 = CARTESIAN_POINT('Ctrl Pts',(-32.0265116602543,12.9102232608784,
126.119833944972)) ;
#128726 = CARTESIAN_POINT('Ctrl Pts',(-32.0931565382583,12.6507291621381,
126.281277357209)) ;
#128727 = CARTESIAN_POINT('Ctrl Pts',(-32.1791862247539,12.4485585677655,
126.499672075653)) ;
#128728 = CARTESIAN_POINT('Ctrl Pts',(-32.2805050319855,12.3145373825205,
126.762496297742)) ;
#128729 = CARTESIAN_POINT('Ctrl Pts',(-32.3900324574915,12.2601564012495,
127.049323626435)) ;
#128730 = CARTESIAN_POINT('Ctrl Pts',(-32.5009231094152,12.2893926145907,
127.34004832186)) ;
#128731 = CARTESIAN_POINT('Ctrl Pts',(-32.6052118557404,12.3994366582283,
127.611652113728)) ;
#128732 = CARTESIAN_POINT('Ctrl Pts',(-32.6971979489033,12.5839727611718,
127.847103732541)) ;
#128733 = CARTESIAN_POINT('Ctrl Pts',(-32.7697374400747,12.8264919442356,
128.026067460127)) ;
#128734 = CARTESIAN_POINT('Ctrl Pts',(-32.8197428070764,13.1141227557289,
128.138887683343)) ;
#128735 = CARTESIAN_POINT('Ctrl Pts',(-32.8354546045722,13.3194869799383,
128.162746032927)) ;
#128736 = CARTESIAN_POINT('Ctrl Pts',(-32.8388677653298,13.4222384087837,
128.161696006566)) ;
#128737 = CARTESIAN_POINT('Ctrl Pts',(-11.2577234899685,13.1368456608817,
133.156546946693)) ;
#128738 = CARTESIAN_POINT('Ctrl Pts',(-11.2584977422668,13.1302434100695,
133.158077773235)) ;
#128739 = CARTESIAN_POINT('Ctrl Pts',(-11.2711317675039,13.0249711622575,
133.183302490093)) ;
#128740 = CARTESIAN_POINT('Ctrl Pts',(-11.3056487140165,12.8263018173041,
133.261160287319)) ;
#128741 = CARTESIAN_POINT('Ctrl Pts',(-11.378449880765,12.5833995397257,133.440808382067)) ;
#128742 = CARTESIAN_POINT('Ctrl Pts',(-11.4699936456372,12.3996267675037,
133.675124851034)) ;
#128743 = CARTESIAN_POINT('Ctrl Pts',(-11.5749944367631,12.2890731746127,
133.948585197779)) ;
#128744 = CARTESIAN_POINT('Ctrl Pts',(-11.6849550113911,12.2602312933653,
134.236878590562)) ;
#128745 = CARTESIAN_POINT('Ctrl Pts',(-11.7947913325518,12.3144254327404,
134.524512184654)) ;
#128746 = CARTESIAN_POINT('Ctrl Pts',(-11.8959713006331,12.4480642485612,
134.78699239796)) ;
#128747 = CARTESIAN_POINT('Ctrl Pts',(-11.9825623500535,12.6516399128533,
135.006803074901)) ;
#128748 = CARTESIAN_POINT('Ctrl Pts',(-12.048871242094,12.9104451953934,135.167384670857)) ;
#128749 = CARTESIAN_POINT('Ctrl Pts',(-12.0909139091436,13.2058491339696,
135.25708775867)) ;
#128750 = CARTESIAN_POINT('Ctrl Pts',(-12.1065078256121,13.5166184158111,
135.269550983787)) ;
#128751 = CARTESIAN_POINT('Ctrl Pts',(-12.0950209690494,13.822409942281,135.202705290103)) ;
#128752 = CARTESIAN_POINT('Ctrl Pts',(-12.0583944517229,14.0967864271645,
135.062748314668)) ;
#128753 = CARTESIAN_POINT('Ctrl Pts',(-11.9996901173169,14.3244562376795,
134.858128955177)) ;
#128754 = CARTESIAN_POINT('Ctrl Pts',(-11.9238941091653,14.4874741588536,
134.603594989759)) ;
#128755 = CARTESIAN_POINT('Ctrl Pts',(-11.8369189889969,14.5744204782189,
134.316306456094)) ;
#128756 = CARTESIAN_POINT('Ctrl Pts',(-11.746203405536,14.5784621865543,134.018183591682)) ;
#128757 = CARTESIAN_POINT('Ctrl Pts',(-11.6588757290822,14.5000470189108,
133.730007295683)) ;
#128758 = CARTESIAN_POINT('Ctrl Pts',(-11.5816779592207,14.3445727913024,
133.471389657961)) ;
#128759 = CARTESIAN_POINT('Ctrl Pts',(-11.5208530443649,14.1228339214572,
133.260553481405)) ;
#128760 = CARTESIAN_POINT('Ctrl Pts',(-11.4816410741325,13.850151796375,133.112780950454)) ;
#128761 = CARTESIAN_POINT('Ctrl Pts',(-11.467692327045,13.5490424798657,133.039054244321)) ;
#128762 = CARTESIAN_POINT('Ctrl Pts',(-11.4803987084794,13.2374718016147,
133.043030817363)) ;
#128763 = CARTESIAN_POINT('Ctrl Pts',(-11.5199946658805,12.9386845516003,
133.125492572852)) ;
#128764 = CARTESIAN_POINT('Ctrl Pts',(-11.5837788008953,12.6761377912153,
133.278810795145)) ;
#128765 = CARTESIAN_POINT('Ctrl Pts',(-11.6686447392389,12.4657587239521,
133.493527758041)) ;
#128766 = CARTESIAN_POINT('Ctrl Pts',(-11.7685433992697,12.3246285907277,
133.752289114269)) ;
#128767 = CARTESIAN_POINT('Ctrl Pts',(-11.8778587918771,12.2619062274696,
134.038399188115)) ;
#128768 = CARTESIAN_POINT('Ctrl Pts',(-11.98827945464,12.2824388238971,134.327963742059)) ;
#128769 = CARTESIAN_POINT('Ctrl Pts',(-12.0940128949218,12.3848777352211,
134.603625594352)) ;
#128770 = CARTESIAN_POINT('Ctrl Pts',(-12.1871312124463,12.5614991526439,
134.84255860207)) ;
#128771 = CARTESIAN_POINT('Ctrl Pts',(-12.2622218143172,12.7995867932639,
135.02881848202)) ;
#128772 = CARTESIAN_POINT('Ctrl Pts',(-12.3146869562127,13.0840299785093,
135.148804148266)) ;
#128773 = CARTESIAN_POINT('Ctrl Pts',(-12.3409445105552,13.3899587126068,
135.192549574632)) ;
#128774 = CARTESIAN_POINT('Ctrl Pts',(-12.3405172946369,13.6996411315525,
135.15818716667)) ;
#128775 = CARTESIAN_POINT('Ctrl Pts',(-12.3136761245736,13.9903747332587,
135.046560923732)) ;
#128776 = CARTESIAN_POINT('Ctrl Pts',(-12.263351660098,14.2393240400609,134.86646186996)) ;
#128777 = CARTESIAN_POINT('Ctrl Pts',(-12.193924449354,14.4298400308443,134.630589033284)) ;
#128778 = CARTESIAN_POINT('Ctrl Pts',(-12.1108448938615,14.5487685214643,
134.354775496619)) ;
#128779 = CARTESIAN_POINT('Ctrl Pts',(-12.0206426776565,14.5869290459119,
134.058065629562)) ;
#128780 = CARTESIAN_POINT('Ctrl Pts',(-11.9311958117229,14.5417666883846,
133.763725950696)) ;
#128781 = CARTESIAN_POINT('Ctrl Pts',(-11.848852525887,14.4163781247343,133.490009785098)) ;
#128782 = CARTESIAN_POINT('Ctrl Pts',(-11.7806588005147,14.2194053349132,
133.257622965532)) ;
#128783 = CARTESIAN_POINT('Ctrl Pts',(-11.7323693114602,13.9666437223108,
133.0835399063)) ;
#128784 = CARTESIAN_POINT('Ctrl Pts',(-11.7077161248384,13.6737230615468,
132.978341072132)) ;
#128785 = CARTESIAN_POINT('Ctrl Pts',(-11.7095613308164,13.3629183562335,
132.950571917867)) ;
#128786 = CARTESIAN_POINT('Ctrl Pts',(-11.7383478402933,13.0570541926124,
133.001567102361)) ;
#128787 = CARTESIAN_POINT('Ctrl Pts',(-11.7926724382674,12.7772474882028,
133.127165265906)) ;
#128788 = CARTESIAN_POINT('Ctrl Pts',(-11.8699199411722,12.5427680986525,
133.319560793352)) ;
#128789 = CARTESIAN_POINT('Ctrl Pts',(-11.9640477954549,12.3730788782687,
133.561569728364)) ;
#128790 = CARTESIAN_POINT('Ctrl Pts',(-12.0703540727819,12.2773830666973,
133.838948640795)) ;
#128791 = CARTESIAN_POINT('Ctrl Pts',(-12.1812907705461,12.2641121652248,
134.129904369605)) ;
#128792 = CARTESIAN_POINT('Ctrl Pts',(-12.2897321496588,12.3337583003129,
134.413576291279)) ;
#128793 = CARTESIAN_POINT('Ctrl Pts',(-12.3886537440222,12.481316017211,134.669448938114)) ;
#128794 = CARTESIAN_POINT('Ctrl Pts',(-12.4718652582287,12.6966779051232,
134.879370255133)) ;
#128795 = CARTESIAN_POINT('Ctrl Pts',(-12.5338644427472,12.96405838434,135.027347390407)) ;
#128796 = CARTESIAN_POINT('Ctrl Pts',(-12.5709815279252,13.2633620040759,
135.102737093753)) ;
#128797 = CARTESIAN_POINT('Ctrl Pts',(-12.5815244475118,13.5752566966047,
135.100371228404)) ;
#128798 = CARTESIAN_POINT('Ctrl Pts',(-12.5650970124809,13.8766501658651,
135.019163196537)) ;
#128799 = CARTESIAN_POINT('Ctrl Pts',(-12.5240386339325,14.1438625345399,
134.866211806807)) ;
#128800 = CARTESIAN_POINT('Ctrl Pts',(-12.4614606242008,14.3611557729943,
134.650168617088)) ;
#128801 = CARTESIAN_POINT('Ctrl Pts',(-12.382977010877,14.5102070639316,134.387759126822)) ;
#128802 = CARTESIAN_POINT('Ctrl Pts',(-12.2953587366625,14.5813677790431,
134.098836666124)) ;
#128803 = CARTESIAN_POINT('Ctrl Pts',(-12.2045170609747,14.5701315167375,
133.800277368628)) ;
#128804 = CARTESIAN_POINT('Ctrl Pts',(-12.1181642794546,14.4759919392145,
133.51478205914)) ;
#128805 = CARTESIAN_POINT('Ctrl Pts',(-12.0436987557635,14.3066893243029,
133.264144105982)) ;
#128806 = CARTESIAN_POINT('Ctrl Pts',(-11.9869151341152,14.075187939402,133.065272807165)) ;
#128807 = CARTESIAN_POINT('Ctrl Pts',(-11.9522067331107,13.7962287438528,
132.930759808628)) ;
#128808 = CARTESIAN_POINT('Ctrl Pts',(-11.9430693364966,13.4897393556908,
132.870870600982)) ;
#128809 = CARTESIAN_POINT('Ctrl Pts',(-11.9611565578198,13.1781057377786,
132.890466222449)) ;
#128810 = CARTESIAN_POINT('Ctrl Pts',(-12.0051369072121,12.8871395007703,
132.986063729264)) ;
#128811 = CARTESIAN_POINT('Ctrl Pts',(-12.0735337638993,12.6313543298591,
133.152625547031)) ;
#128812 = CARTESIAN_POINT('Ctrl Pts',(-12.1617954477986,12.4333423964865,
133.377283802115)) ;
#128813 = CARTESIAN_POINT('Ctrl Pts',(-12.2635234037695,12.3067788295905,
133.641500686264)) ;
#128814 = CARTESIAN_POINT('Ctrl Pts',(-12.373902244889,12.2592790110699,133.930667889296)) ;
#128815 = CARTESIAN_POINT('Ctrl Pts',(-12.4842564290935,12.2958890741667,
134.219915229999)) ;
#128816 = CARTESIAN_POINT('Ctrl Pts',(-12.5875537880349,12.412515964046,134.488658951895)) ;
#128817 = CARTESIAN_POINT('Ctrl Pts',(-12.6778899409315,12.6017795231482,
134.719420077916)) ;
#128818 = CARTESIAN_POINT('Ctrl Pts',(-12.7491733635404,12.8508820416093,
134.894428325394)) ;
#128819 = CARTESIAN_POINT('Ctrl Pts',(-12.7966035607827,13.1389626246921,
134.999995033177)) ;
#128820 = CARTESIAN_POINT('Ctrl Pts',(-12.818140672535,13.4502019068506,135.029605683406)) ;
#128821 = CARTESIAN_POINT('Ctrl Pts',(-12.8124254227046,13.7571545047615,
134.97985899907)) ;
#128822 = CARTESIAN_POINT('Ctrl Pts',(-12.7811740697528,14.0399279502617,
134.855572397321)) ;
#128823 = CARTESIAN_POINT('Ctrl Pts',(-12.7266312200537,14.2804627240583,
134.662980887093)) ;
#128824 = CARTESIAN_POINT('Ctrl Pts',(-12.6542449467316,14.4580430249791,
134.418505620157)) ;
#128825 = CARTESIAN_POINT('Ctrl Pts',(-12.5692017225138,14.5623041717052,
134.136899220113)) ;
#128826 = CARTESIAN_POINT('Ctrl Pts',(-12.4788691012162,14.5848738329504,
133.839946789707)) ;
#128827 = CARTESIAN_POINT('Ctrl Pts',(-12.3895760994411,14.5236285487513,
133.545783898715)) ;
#128828 = CARTESIAN_POINT('Ctrl Pts',(-12.3099194108957,14.3842859128116,
133.280100234544)) ;
#128829 = CARTESIAN_POINT('Ctrl Pts',(-12.2450643301526,14.1760037258481,
133.057519313321)) ;
#128830 = CARTESIAN_POINT('Ctrl Pts',(-12.2007227509484,13.9123646323485,
132.894723585747)) ;
#128831 = CARTESIAN_POINT('Ctrl Pts',(-12.1811617332779,13.6155080091082,
132.80454288444)) ;
#128832 = CARTESIAN_POINT('Ctrl Pts',(-12.1880080885275,13.3048787604148,
132.791493362742)) ;
#128833 = CARTESIAN_POINT('Ctrl Pts',(-12.2218568341941,13.0013159560589,
132.857171513992)) ;
#128834 = CARTESIAN_POINT('Ctrl Pts',(-12.2807527580712,12.7290185702227,
132.996137319577)) ;
#128835 = CARTESIAN_POINT('Ctrl Pts',(-12.361411062945,12.5059453720444,133.198616695887)) ;
#128836 = CARTESIAN_POINT('Ctrl Pts',(-12.4585666028295,12.348935712054,133.449341626127)) ;
#128837 = CARTESIAN_POINT('Ctrl Pts',(-12.5660032842499,12.2685725815048,
133.730122349131)) ;
#128838 = CARTESIAN_POINT('Ctrl Pts',(-12.6773948799817,12.2709800121234,
134.022294144479)) ;
#128839 = CARTESIAN_POINT('Ctrl Pts',(-12.7844046898859,12.3558596886437,
134.30183548448)) ;
#128840 = CARTESIAN_POINT('Ctrl Pts',(-12.8809331266172,12.5173148322773,
134.55066838557)) ;
#128841 = CARTESIAN_POINT('Ctrl Pts',(-12.9604049280866,12.7436532410187,
134.749701673785)) ;
#128842 = CARTESIAN_POINT('Ctrl Pts',(-13.0179363384229,13.0184389835147,
134.884661471726)) ;
#128843 = CARTESIAN_POINT('Ctrl Pts',(-13.0502008445833,13.3224258162056,
134.945784440126)) ;
#128844 = CARTESIAN_POINT('Ctrl Pts',(-13.0555467014002,13.6337495707095,
134.928259254628)) ;
#128845 = CARTESIAN_POINT('Ctrl Pts',(-13.0343105414423,13.9298381021214,
134.8330936576)) ;
#128846 = CARTESIAN_POINT('Ctrl Pts',(-12.9888314749578,14.1894305566765,
134.667140294163)) ;
#128847 = CARTESIAN_POINT('Ctrl Pts',(-12.9229180456801,14.394475711673,134.441433971172)) ;
#128848 = CARTESIAN_POINT('Ctrl Pts',(-12.8423867584635,14.5294751286176,
134.173134382948)) ;
#128849 = CARTESIAN_POINT('Ctrl Pts',(-12.7533105459994,14.5857784674847,
133.879795104212)) ;
#128850 = CARTESIAN_POINT('Ctrl Pts',(-12.6627280066615,14.5584758053027,
133.581971600338)) ;
#128851 = CARTESIAN_POINT('Ctrl Pts',(-12.5784004724766,14.4499269628754,
133.302534971488)) ;
#128852 = CARTESIAN_POINT('Ctrl Pts',(-12.5066920227855,14.2678362538152,
133.059930399529)) ;
#128853 = CARTESIAN_POINT('Ctrl Pts',(-12.4535716004615,14.025181469635,132.871626399327)) ;
#128854 = CARTESIAN_POINT('Ctrl Pts',(-12.4235648768297,13.7395989406437,
132.750864375356)) ;
#128855 = CARTESIAN_POINT('Ctrl Pts',(-12.4195271153669,13.4312396287892,
132.705949634697)) ;
#128856 = CARTESIAN_POINT('Ctrl Pts',(-12.4424256321316,13.1225497292761,
132.739753354196)) ;
#128857 = CARTESIAN_POINT('Ctrl Pts',(-12.4915723419793,12.8344723647331,
132.850125775633)) ;
#128858 = CARTESIAN_POINT('Ctrl Pts',(-12.5638932332728,12.5894057804916,
133.028292890665)) ;
#128859 = CARTESIAN_POINT('Ctrl Pts',(-12.6550789543492,12.40386696018,133.261545560757)) ;
#128860 = CARTESIAN_POINT('Ctrl Pts',(-12.7592412635636,12.2913271454925,
133.532726136242)) ;
#128861 = CARTESIAN_POINT('Ctrl Pts',(-12.8699890943141,12.2598830910962,
133.823057346396)) ;
#128862 = CARTESIAN_POINT('Ctrl Pts',(-12.9793995134526,12.3117248665292,
134.109616003847)) ;
#128863 = CARTESIAN_POINT('Ctrl Pts',(-13.0810869398604,12.4432581620118,
134.373522926903)) ;
#128864 = CARTESIAN_POINT('Ctrl Pts',(-13.1680418025667,12.6447767866554,
134.594446826779)) ;
#128865 = CARTESIAN_POINT('Ctrl Pts',(-13.2350120772362,12.9020426127521,
134.756972372431)) ;
#128866 = CARTESIAN_POINT('Ctrl Pts',(-13.2778449973924,13.1969219794908,
134.84895528723)) ;
#128867 = CARTESIAN_POINT('Ctrl Pts',(-13.2942160406864,13.5073632860462,
134.863709263387)) ;
#128868 = CARTESIAN_POINT('Ctrl Pts',(-13.2835289768122,13.813502723387,134.799217091499)) ;
#128869 = CARTESIAN_POINT('Ctrl Pts',(-13.2476676966464,14.089063380816,134.661503408302)) ;
#128870 = CARTESIAN_POINT('Ctrl Pts',(-13.1892561306851,14.319268429037,134.457595503743)) ;
#128871 = CARTESIAN_POINT('Ctrl Pts',(-13.1141385106108,14.4835637196257,
134.205174492886)) ;
#128872 = CARTESIAN_POINT('Ctrl Pts',(-13.0274042527108,14.5730187968723,
133.918585740495)) ;
#128873 = CARTESIAN_POINT('Ctrl Pts',(-12.9366798206149,14.5795967994517,
133.620433125244)) ;
#128874 = CARTESIAN_POINT('Ctrl Pts',(-12.8489781193153,14.5032854437543,
133.331090114902)) ;
#128875 = CARTESIAN_POINT('Ctrl Pts',(-12.7714680695992,14.350115255618,133.071602998426)) ;
#128876 = CARTESIAN_POINT('Ctrl Pts',(-12.7099485961889,14.1289953523701,
132.858606720622)) ;
#128877 = CARTESIAN_POINT('Ctrl Pts',(-12.6703752161743,13.8600885343661,
132.710090425404)) ;
#128878 = CARTESIAN_POINT('Ctrl Pts',(-12.6554495566048,13.5571077993043,
132.633228023965)) ;
#128879 = CARTESIAN_POINT('Ctrl Pts',(-12.6675181766786,13.2461442417419,
132.635412623524)) ;
#128880 = CARTESIAN_POINT('Ctrl Pts',(-12.7061242005164,12.9474785821981,
132.715086767085)) ;
#128881 = CARTESIAN_POINT('Ctrl Pts',(-12.7698092342811,12.6818051231589,
132.86785971074)) ;
#128882 = CARTESIAN_POINT('Ctrl Pts',(-12.8535542604601,12.4713262557242,
133.079555782508)) ;
#128883 = CARTESIAN_POINT('Ctrl Pts',(-12.9535767545019,12.3273775591191,
133.338508722271)) ;
#128884 = CARTESIAN_POINT('Ctrl Pts',(-13.062119391893,12.2625380497534,133.622557250429)) ;
#128885 = CARTESIAN_POINT('Ctrl Pts',(-13.1735704256936,12.2810707437097,
133.914826535872)) ;
#128886 = CARTESIAN_POINT('Ctrl Pts',(-13.2784207174052,12.3803128917833,
134.188268338219)) ;
#128887 = CARTESIAN_POINT('Ctrl Pts',(-13.3725731541865,12.5556238817755,
134.430026844874)) ;
#128888 = CARTESIAN_POINT('Ctrl Pts',(-13.4479809967805,12.7914916788268,
134.617325799491)) ;
#128889 = CARTESIAN_POINT('Ctrl Pts',(-13.5012865616176,13.075040960321,134.73973307701)) ;
#128890 = CARTESIAN_POINT('Ctrl Pts',(-13.5283476037201,13.3808908357546,
134.785794826102)) ;
#128891 = CARTESIAN_POINT('Ctrl Pts',(-13.5286770966046,13.6908804801079,
134.753632549337)) ;
#128892 = CARTESIAN_POINT('Ctrl Pts',(-13.5026619759082,13.9819858711707,
134.644485736166)) ;
#128893 = CARTESIAN_POINT('Ctrl Pts',(-13.4528259609757,14.2331023132834,
134.465714564662)) ;
#128894 = CARTESIAN_POINT('Ctrl Pts',(-13.3839536191554,14.4253737396298,
134.231500815278)) ;
#128895 = CARTESIAN_POINT('Ctrl Pts',(-13.3006466187109,14.54690254864,133.954824347393)) ;
#128896 = CARTESIAN_POINT('Ctrl Pts',(-13.2111465830334,14.5868798000434,
133.660396959844)) ;
#128897 = CARTESIAN_POINT('Ctrl Pts',(-13.121472385501,14.5442430109602,133.365347539629)) ;
#128898 = CARTESIAN_POINT('Ctrl Pts',(-13.038917836058,14.4211466700167,133.091054193852)) ;
#128899 = CARTESIAN_POINT('Ctrl Pts',(-12.970223038156,14.2262607777735,132.857214381594)) ;
#128900 = CARTESIAN_POINT('Ctrl Pts',(-12.9211951552716,13.9744157685803,
132.680910401444)) ;
#128901 = CARTESIAN_POINT('Ctrl Pts',(-12.8958788774826,13.6824770382547,
132.573794609031)) ;
#128902 = CARTESIAN_POINT('Ctrl Pts',(-12.8968484596315,13.3726811668738,
132.54355335689)) ;
#128903 = CARTESIAN_POINT('Ctrl Pts',(-12.9250788219677,13.06445534207,132.592712283102)) ;
#128904 = CARTESIAN_POINT('Ctrl Pts',(-12.9785271121994,12.7851438246932,
132.715917599892)) ;
#128905 = CARTESIAN_POINT('Ctrl Pts',(-13.0549176634622,12.5493640778092,
132.905881907071)) ;
#128906 = CARTESIAN_POINT('Ctrl Pts',(-13.1488400728833,12.3769707838731,
133.147199881218)) ;
#128907 = CARTESIAN_POINT('Ctrl Pts',(-13.255197241319,12.2789143225366,133.424641623102)) ;
#128908 = CARTESIAN_POINT('Ctrl Pts',(-13.3657745952221,12.2633331212568,
133.71464458178)) ;
#128909 = CARTESIAN_POINT('Ctrl Pts',(-13.4746365736454,12.3306602276622,
133.99947236187)) ;
#128910 = CARTESIAN_POINT('Ctrl Pts',(-13.5740239071654,12.4766202323596,
134.256655193809)) ;
#128911 = CARTESIAN_POINT('Ctrl Pts',(-13.6573376158806,12.6891735601127,
134.467042740179)) ;
#128912 = CARTESIAN_POINT('Ctrl Pts',(-13.7201299804399,12.9552554154068,
134.617319875805)) ;
#128913 = CARTESIAN_POINT('Ctrl Pts',(-13.7580993715032,13.2547269193452,
134.69511157972)) ;
#128914 = CARTESIAN_POINT('Ctrl Pts',(-13.7693521902213,13.5662745338838,
134.694851970239)) ;
#128915 = CARTESIAN_POINT('Ctrl Pts',(-13.7538280753497,13.8673045434185,
134.616401396385)) ;
#128916 = CARTESIAN_POINT('Ctrl Pts',(-13.7133227526897,14.1368395947381,
134.46493571588)) ;
#128917 = CARTESIAN_POINT('Ctrl Pts',(-13.6515265216066,14.355047357882,134.251302140233)) ;
#128918 = CARTESIAN_POINT('Ctrl Pts',(-13.5734905931613,14.5066809215218,
133.990195550223)) ;
#128919 = CARTESIAN_POINT('Ctrl Pts',(-13.4856168957243,14.5805549818753,
133.700364378538)) ;
#128920 = CARTESIAN_POINT('Ctrl Pts',(-13.3950029122098,14.5715434476004,
133.402560518914)) ;
#128921 = CARTESIAN_POINT('Ctrl Pts',(-13.3087143692411,14.4804615024267,
133.117379969011)) ;
#128922 = CARTESIAN_POINT('Ctrl Pts',(-13.233499398185,14.3129345410317,132.864438386254)) ;
#128923 = CARTESIAN_POINT('Ctrl Pts',(-13.1760123828882,14.0824720621631,
132.663437914386)) ;
#128924 = CARTESIAN_POINT('Ctrl Pts',(-13.1406523017996,13.8045960831527,
132.527027338209)) ;
#128925 = CARTESIAN_POINT('Ctrl Pts',(-13.1307543289692,13.4994873044745,
132.465012131804)) ;
#128926 = CARTESIAN_POINT('Ctrl Pts',(-13.1479439577104,13.1877259359498,
132.481993019375)) ;
#128927 = CARTESIAN_POINT('Ctrl Pts',(-13.1913374539631,12.8947282234829,
132.575745357319)) ;
#128928 = CARTESIAN_POINT('Ctrl Pts',(-13.2592530179144,12.6375710763399,
132.740870405993)) ;
#128929 = CARTESIAN_POINT('Ctrl Pts',(-13.3464861608597,12.438646888205,132.962710793394)) ;
#128930 = CARTESIAN_POINT('Ctrl Pts',(-13.4484558008074,12.3091461051662,
133.227445286792)) ;
#128931 = CARTESIAN_POINT('Ctrl Pts',(-13.5580827475339,12.2596124817515,
133.514610177686)) ;
#128932 = CARTESIAN_POINT('Ctrl Pts',(-13.6687842386363,12.2934287573512,
133.804796814901)) ;
#128933 = CARTESIAN_POINT('Ctrl Pts',(-13.7728190474512,12.4085128318244,
134.075550006677)) ;
#128934 = CARTESIAN_POINT('Ctrl Pts',(-13.8633144747704,12.5956557318582,
134.306859221739)) ;
#128935 = CARTESIAN_POINT('Ctrl Pts',(-13.9350011449069,12.8419007286425,
134.483200818981)) ;
#128936 = CARTESIAN_POINT('Ctrl Pts',(-13.9834527110846,13.131017500255,134.5915261146)) ;
#128937 = CARTESIAN_POINT('Ctrl Pts',(-14.005618946637,13.4394174344068,134.623252886023)) ;
#128938 = CARTESIAN_POINT('Ctrl Pts',(-14.0007870350482,13.7489280786131,
134.575855496463)) ;
#128939 = CARTESIAN_POINT('Ctrl Pts',(-13.9700930567108,14.0326636171821,
134.453180433329)) ;
#128940 = CARTESIAN_POINT('Ctrl Pts',(-13.9164201828627,14.2739040584896,
134.26326367921)) ;
#128941 = CARTESIAN_POINT('Ctrl Pts',(-13.8441170998093,14.4542738931404,
134.018865228188)) ;
#128942 = CARTESIAN_POINT('Ctrl Pts',(-13.7597088982733,14.5602989567159,
133.739268293097)) ;
#128943 = CARTESIAN_POINT('Ctrl Pts',(-13.6691129770032,14.5853165181453,
133.441420203372)) ;
#128944 = CARTESIAN_POINT('Ctrl Pts',(-13.5802373274275,14.5269567294315,
133.148695949413)) ;
#128945 = CARTESIAN_POINT('Ctrl Pts',(-13.4996367966222,14.3891798235028,
132.880031479941)) ;
#128946 = CARTESIAN_POINT('Ctrl Pts',(-13.4342778247782,14.1817903606507,
132.655913729344)) ;
#128947 = CARTESIAN_POINT('Ctrl Pts',(-13.3896410373865,13.9219442821041,
132.492558783544)) ;
#128948 = CARTESIAN_POINT('Ctrl Pts',(-13.3691125413019,13.6244334028394,
132.399380837347)) ;
#128949 = CARTESIAN_POINT('Ctrl Pts',(-13.3752053017507,13.313830933939,132.384130977037)) ;
#128950 = CARTESIAN_POINT('Ctrl Pts',(-13.4084264932242,13.0089908308966,
132.447888942027)) ;
#128951 = CARTESIAN_POINT('Ctrl Pts',(-13.4664286619536,12.7367006174924,
132.584381270711)) ;
#128952 = CARTESIAN_POINT('Ctrl Pts',(-13.5464825070529,12.511790352846,132.785088887304)) ;
#128953 = CARTESIAN_POINT('Ctrl Pts',(-13.6432422546615,12.3525056557872,
133.034650830282)) ;
#128954 = CARTESIAN_POINT('Ctrl Pts',(-13.7509364249438,12.2695603711095,
133.316043846998)) ;
#128955 = CARTESIAN_POINT('Ctrl Pts',(-13.8621624158612,12.2698997293224,
133.60778233543)) ;
#128956 = CARTESIAN_POINT('Ctrl Pts',(-13.9690935338641,12.3521639545542,
133.887183808814)) ;
#128957 = CARTESIAN_POINT('Ctrl Pts',(-14.0661252891564,12.5116414320552,
134.137454505603)) ;
#128958 = CARTESIAN_POINT('Ctrl Pts',(-14.1460957894673,12.7360068046191,
134.337983832077)) ;
#128959 = CARTESIAN_POINT('Ctrl Pts',(-14.2044014009858,13.0100794462922,
134.475150201071)) ;
#128960 = CARTESIAN_POINT('Ctrl Pts',(-14.237390124937,13.3126251519116,134.538487484907)) ;
#128961 = CARTESIAN_POINT('Ctrl Pts',(-14.2435487462307,13.6254713838339,
134.523181255199)) ;
#128962 = CARTESIAN_POINT('Ctrl Pts',(-14.2231083995741,13.9212363983898,
134.430462751386)) ;
#128963 = CARTESIAN_POINT('Ctrl Pts',(-14.1782100391862,14.182693359551,134.266134248419)) ;
#128964 = CARTESIAN_POINT('Ctrl Pts',(-14.1130711823717,14.388968587839,134.042808158454)) ;
#128965 = CARTESIAN_POINT('Ctrl Pts',(-14.0323807826771,14.5271449828327,
133.773829605151)) ;
#128966 = CARTESIAN_POINT('Ctrl Pts',(-13.9433504875457,14.5852339313446,
133.480602666319)) ;
#128967 = CARTESIAN_POINT('Ctrl Pts',(-13.8533021601708,14.5605427839008,
133.184558668845)) ;
#128968 = CARTESIAN_POINT('Ctrl Pts',(-13.768441910465,14.4541441821425,132.903468307066)) ;
#128969 = CARTESIAN_POINT('Ctrl Pts',(-13.6963328067855,14.2740963581792,
132.659717985775)) ;
#128970 = CARTESIAN_POINT('Ctrl Pts',(-13.6424665927511,14.0323113149494,
132.469147368739)) ;
#128971 = CARTESIAN_POINT('Ctrl Pts',(-13.6118627409455,13.7476340244825,
132.346648809093)) ;
#128972 = CARTESIAN_POINT('Ctrl Pts',(-13.6070208398731,13.4408490996929,
132.299516778095)) ;
#128973 = CARTESIAN_POINT('Ctrl Pts',(-13.6292745184613,13.1304291597349,
132.33127737453)) ;
#128974 = CARTESIAN_POINT('Ctrl Pts',(-13.6775184445424,12.8426172775068,
132.439152830702)) ;
#128975 = CARTESIAN_POINT('Ctrl Pts',(-13.7495368284921,12.5951022403137,
132.616294095416)) ;
#128976 = CARTESIAN_POINT('Ctrl Pts',(-13.839810595063,12.4086451366238,132.847055099998)) ;
#128977 = CARTESIAN_POINT('Ctrl Pts',(-13.9439529657996,12.2933533554013,
133.118081240053)) ;
#128978 = CARTESIAN_POINT('Ctrl Pts',(-14.0545907378869,12.2596356648428,
133.408104864409)) ;
#128979 = CARTESIAN_POINT('Ctrl Pts',(-14.1640727575126,12.3091205496962,
133.694884889222)) ;
#128980 = CARTESIAN_POINT('Ctrl Pts',(-14.2659054115225,12.4379929184033,
133.959287417802)) ;
#128981 = CARTESIAN_POINT('Ctrl Pts',(-14.3537948932701,12.6386444733354,
134.182778472271)) ;
#128982 = CARTESIAN_POINT('Ctrl Pts',(-14.4211964420494,12.8942394600066,
134.346627354086)) ;
#128983 = CARTESIAN_POINT('Ctrl Pts',(-14.4647242552601,13.1876523061434,
134.440710147854)) ;
#128984 = CARTESIAN_POINT('Ctrl Pts',(-14.4818974987982,13.4984174202856,
134.457753581522)) ;
#128985 = CARTESIAN_POINT('Ctrl Pts',(-14.4720621585198,13.804322851742,134.39583623639)) ;
#128986 = CARTESIAN_POINT('Ctrl Pts',(-14.4366876007892,14.0825043451859,
134.259358010074)) ;
#128987 = CARTESIAN_POINT('Ctrl Pts',(-14.3789691813199,14.3134150870924,
134.057582409301)) ;
#128988 = CARTESIAN_POINT('Ctrl Pts',(-14.3042641459132,14.4799819682822,
133.806350659583)) ;
#128989 = CARTESIAN_POINT('Ctrl Pts',(-14.2174203005974,14.5717628794977,
133.519324818323)) ;
#128990 = CARTESIAN_POINT('Ctrl Pts',(-14.1271684585799,14.5804902548306,
133.222718423381)) ;
#128991 = CARTESIAN_POINT('Ctrl Pts',(-14.039320812417,14.5068426765183,132.932971409604)) ;
#128992 = CARTESIAN_POINT('Ctrl Pts',(-13.9613365017552,14.3556216409034,
132.672060274999)) ;
#128993 = CARTESIAN_POINT('Ctrl Pts',(-13.8992930942413,14.1365917034713,
132.45757424989)) ;
#128994 = CARTESIAN_POINT('Ctrl Pts',(-13.8589636050019,13.8680781333687,
132.306751288209)) ;
#128995 = CARTESIAN_POINT('Ctrl Pts',(-13.843278106268,13.5671870152877,132.227831586699)) ;
#128996 = CARTESIAN_POINT('Ctrl Pts',(-13.854655788299,13.253754715573,132.227735126529)) ;
#128997 = CARTESIAN_POINT('Ctrl Pts',(-13.8924329041369,12.9561226298826,
132.305167149537)) ;
#128998 = CARTESIAN_POINT('Ctrl Pts',(-13.9551833680437,12.689577131159,132.455284134854)) ;
#128999 = CARTESIAN_POINT('Ctrl Pts',(-14.0386480780972,12.4765149553713,
132.666050247211)) ;
#129000 = CARTESIAN_POINT('Ctrl Pts',(-14.1383409216431,12.330399344862,132.924033469083)) ;
#129001 = CARTESIAN_POINT('Ctrl Pts',(-14.2468018422879,12.2633426723701,
133.207817039776)) ;
#129002 = CARTESIAN_POINT('Ctrl Pts',(-14.3577139049087,12.2791039533646,
133.498689878789)) ;
#129003 = CARTESIAN_POINT('Ctrl Pts',(-14.4635018226789,12.3764766971553,
133.774659608197)) ;
#129004 = CARTESIAN_POINT('Ctrl Pts',(-14.558014452373,12.5500288330121,134.017480287725)) ;
#129005 = CARTESIAN_POINT('Ctrl Pts',(-14.6338534265181,12.7839577704924,
134.206094016471)) ;
#129006 = CARTESIAN_POINT('Ctrl Pts',(-14.6878213327676,13.0658040445484,
134.330505122389)) ;
#129007 = CARTESIAN_POINT('Ctrl Pts',(-14.7157899465591,13.3726170007347,
134.379069272578)) ;
#129008 = CARTESIAN_POINT('Ctrl Pts',(-14.7167690922712,13.6826397065971,
134.348821079552)) ;
#129009 = CARTESIAN_POINT('Ctrl Pts',(-14.6916340008505,13.973415999198,134.242384284039)) ;
#129010 = CARTESIAN_POINT('Ctrl Pts',(-14.6422882532958,14.2269288255441,
134.064927957567)) ;
#129011 = CARTESIAN_POINT('Ctrl Pts',(-14.5739775160678,14.4205112234245,
133.832415829536)) ;
#129012 = CARTESIAN_POINT('Ctrl Pts',(-14.491433377866,14.5441065980074,133.558125918887)) ;
#129013 = CARTESIAN_POINT('Ctrl Pts',(-14.4013960964376,14.5870792667271,
133.261890403336)) ;
#129014 = CARTESIAN_POINT('Ctrl Pts',(-14.3115236434716,14.5462510446376,
132.966219015162)) ;
#129015 = CARTESIAN_POINT('Ctrl Pts',(-14.2290767314148,14.4261089740706,
132.69241253439)) ;
#129016 = CARTESIAN_POINT('Ctrl Pts',(-14.1595049968999,14.2320089324099,
132.455820348673)) ;
#129017 = CARTESIAN_POINT('Ctrl Pts',(-14.1100842696443,13.9821035017428,
132.278468403181)) ;
#129018 = CARTESIAN_POINT('Ctrl Pts',(-14.0840475701039,13.6914861208152,
132.169293177253)) ;
#129019 = CARTESIAN_POINT('Ctrl Pts',(-14.0842086433358,13.3820427303129,
132.136703583224)) ;
#129020 = CARTESIAN_POINT('Ctrl Pts',(-14.1116571089248,13.0731825073203,
132.183557060288)) ;
#129021 = CARTESIAN_POINT('Ctrl Pts',(-14.1644100089108,12.792789184468,132.304724839785)) ;
#129022 = CARTESIAN_POINT('Ctrl Pts',(-14.2402131138955,12.5553087421356,
132.492964483192)) ;
#129023 = CARTESIAN_POINT('Ctrl Pts',(-14.3338706395137,12.3807971817362,
132.733457127888)) ;
#129024 = CARTESIAN_POINT('Ctrl Pts',(-14.4395838490114,12.2807361570638,
133.009141245256)) ;
#129025 = CARTESIAN_POINT('Ctrl Pts',(-14.5504678733731,12.2625961451368,
133.299932577075)) ;
#129026 = CARTESIAN_POINT('Ctrl Pts',(-14.6593212686416,12.32755343176,133.584790172201)) ;
#129027 = CARTESIAN_POINT('Ctrl Pts',(-14.7590679467847,12.4713199441997,
133.843021054121)) ;
#129028 = CARTESIAN_POINT('Ctrl Pts',(-14.8429423479471,12.6818353121991,
134.055065880925)) ;
#129029 = CARTESIAN_POINT('Ctrl Pts',(-14.9067580971644,12.9488694906299,
134.208078195182)) ;
#129030 = CARTESIAN_POINT('Ctrl Pts',(-14.9450496053253,13.2449963341531,
134.287119488308)) ;
#129031 = CARTESIAN_POINT('Ctrl Pts',(-14.9572251863606,13.5577145851588,
134.289419851131)) ;
#129032 = CARTESIAN_POINT('Ctrl Pts',(-14.9424003027303,13.8591378593898,
134.213035546637)) ;
#129033 = CARTESIAN_POINT('Ctrl Pts',(-14.9025115504108,14.130166831006,134.063329760966)) ;
#129034 = CARTESIAN_POINT('Ctrl Pts',(-14.8412492507378,14.349825857909,133.851274000908)) ;
#129035 = CARTESIAN_POINT('Ctrl Pts',(-14.7637224121309,14.5033075139511,
133.591708104607)) ;
#129036 = CARTESIAN_POINT('Ctrl Pts',(-14.6759945760978,14.5795880781192,
133.302285179212)) ;
#129037 = CARTESIAN_POINT('Ctrl Pts',(-14.5853257363459,14.5729975365321,
133.004310093488)) ;
#129038 = CARTESIAN_POINT('Ctrl Pts',(-14.4985716015393,14.4837968841282,
132.717672404837)) ;
#129039 = CARTESIAN_POINT('Ctrl Pts',(-14.4230828934808,14.3181446441766,
132.463963177981)) ;
#129040 = CARTESIAN_POINT('Ctrl Pts',(-14.3651954605715,14.0900337543834,
132.261895946104)) ;
#129041 = CARTESIAN_POINT('Ctrl Pts',(-14.3290651199569,13.8125788202494,
132.123155422561)) ;
#129042 = CARTESIAN_POINT('Ctrl Pts',(-14.3184784895599,13.5087144247666,
132.059213765231)) ;
#129043 = CARTESIAN_POINT('Ctrl Pts',(-14.3347844930772,13.1970642860529,
132.073643923704)) ;
#129044 = CARTESIAN_POINT('Ctrl Pts',(-14.3776048210991,12.9023259165876,
132.165611695719)) ;
#129045 = CARTESIAN_POINT('Ctrl Pts',(-14.4446704149023,12.6446851896536,
132.32836378006)) ;
#129046 = CARTESIAN_POINT('Ctrl Pts',(-14.5313911331387,12.4436426987833,
132.54869094617)) ;
#129047 = CARTESIAN_POINT('Ctrl Pts',(-14.6331600881906,12.311800617446,132.812797644459)) ;
#129048 = CARTESIAN_POINT('Ctrl Pts',(-14.7426885619788,12.2597626710197,
133.099669110203)) ;
#129049 = CARTESIAN_POINT('Ctrl Pts',(-14.8538711248284,12.2917039117493,
133.391131103677)) ;
#129050 = CARTESIAN_POINT('Ctrl Pts',(-14.9573815637939,12.4035190207528,
133.660621795252)) ;
#129051 = CARTESIAN_POINT('Ctrl Pts',(-15.049112181755,12.5902948819765,133.895252296706)) ;
#129052 = CARTESIAN_POINT('Ctrl Pts',(-15.1209253149525,12.8337324593119,
134.072169901694)) ;
#129053 = CARTESIAN_POINT('Ctrl Pts',(-15.1703867081126,13.1235886512336,
134.183247742845)) ;
#129054 = CARTESIAN_POINT('Ctrl Pts',(-15.1930624887373,13.4302519465087,
134.216624541758)) ;
#129055 = CARTESIAN_POINT('Ctrl Pts',(-15.1892010995764,13.7390104769504,
134.172188842912)) ;
#129056 = CARTESIAN_POINT('Ctrl Pts',(-15.1589633431141,14.026006220093,134.050578201791)) ;
#129057 = CARTESIAN_POINT('Ctrl Pts',(-15.1061157318474,14.267226887447,133.863258556503)) ;
#129058 = CARTESIAN_POINT('Ctrl Pts',(-15.0343759397028,14.4498458774909,
133.620514200202)) ;
#129059 = CARTESIAN_POINT('Ctrl Pts',(-14.9498214158949,14.5586319222976,
133.340333419483)) ;
#129060 = CARTESIAN_POINT('Ctrl Pts',(-14.8592614584468,14.5856242109288,
133.04258213399)) ;
#129061 = CARTESIAN_POINT('Ctrl Pts',(-14.7706278929769,14.5299078426425,
132.750710027517)) ;
#129062 = CARTESIAN_POINT('Ctrl Pts',(-14.6894779497955,14.3940108170827,
132.480354976961)) ;
#129063 = CARTESIAN_POINT('Ctrl Pts',(-14.6237443816963,14.1888421373124,
132.255216550352)) ;
#129064 = CARTESIAN_POINT('Ctrl Pts',(-14.5783921093744,13.9299825539778,
132.089723243472)) ;
#129065 = CARTESIAN_POINT('Ctrl Pts',(-14.5571335436849,13.6339609889882,
131.994496348785)) ;
#129066 = CARTESIAN_POINT('Ctrl Pts',(-14.5624517005765,13.322716019869,131.976899875698)) ;
#129067 = CARTESIAN_POINT('Ctrl Pts',(-14.5947146637798,13.0187245278142,
132.038014645956)) ;
#129068 = CARTESIAN_POINT('Ctrl Pts',(-14.6520713746526,12.7442185255371,
132.172519400802)) ;
#129069 = CARTESIAN_POINT('Ctrl Pts',(-14.7320201612289,12.5167189734132,
132.372757875477)) ;
#129070 = CARTESIAN_POINT('Ctrl Pts',(-14.8279565154633,12.3563386644065,
132.620071928308)) ;
#129071 = CARTESIAN_POINT('Ctrl Pts',(-14.9352059362097,12.2709228506509,
132.900226988222)) ;
#129072 = CARTESIAN_POINT('Ctrl Pts',(-15.0465561535837,12.268610094108,133.192290741623)) ;
#129073 = CARTESIAN_POINT('Ctrl Pts',(-15.1539430166123,12.3485945923255,
133.47295308261)) ;
#129074 = CARTESIAN_POINT('Ctrl Pts',(-15.2516577056561,12.5068355789937,
133.725101150116)) ;
#129075 = CARTESIAN_POINT('Ctrl Pts',(-15.3316894364652,12.7283300538896,
133.926001210879)) ;
#129076 = CARTESIAN_POINT('Ctrl Pts',(-15.3908345605777,13.0013549210284,
134.065586158473)) ;
#129077 = CARTESIAN_POINT('Ctrl Pts',(-15.4245920438632,13.3039530597295,
134.131105830834)) ;
#129078 = CARTESIAN_POINT('Ctrl Pts',(-15.4315691009249,13.615850743561,134.118304796452)) ;
#129079 = CARTESIAN_POINT('Ctrl Pts',(-15.4117562915314,13.9138454553417,
134.02724572002)) ;
#129080 = CARTESIAN_POINT('Ctrl Pts',(-15.3676987993894,14.1752851805425,
133.865537651657)) ;
#129081 = CARTESIAN_POINT('Ctrl Pts',(-15.302987683393,14.3839668392215,133.643386137514)) ;
#129082 = CARTESIAN_POINT('Ctrl Pts',(-15.2227252518571,14.5240578226957,
133.375696442509)) ;
#129083 = CARTESIAN_POINT('Ctrl Pts',(-15.1339295668703,14.584818929902,133.083181731107)) ;
#129084 = CARTESIAN_POINT('Ctrl Pts',(-15.0432280820715,14.5621167472896,
132.785007493075)) ;
#129085 = CARTESIAN_POINT('Ctrl Pts',(-14.9586600655153,14.4583966602146,
132.504979892596)) ;
#129086 = CARTESIAN_POINT('Ctrl Pts',(-14.8860092123973,14.2803904178195,
132.259619724696)) ;
#129087 = CARTESIAN_POINT('Ctrl Pts',(-14.8316450061125,14.0406559765549,
132.067661691774)) ;
#129088 = CARTESIAN_POINT('Ctrl Pts',(-14.8001686976109,13.7571590399429,
131.942617503947)) ;
#129089 = CARTESIAN_POINT('Ctrl Pts',(-14.7946378325009,13.4483332736025,
131.893213729335)) ;
#129090 = CARTESIAN_POINT('Ctrl Pts',(-14.8158814426119,13.1406103992417,
131.922351205196)) ;
#129091 = CARTESIAN_POINT('Ctrl Pts',(-14.8637978713857,12.8492377170497,
132.028961983023)) ;
#129092 = CARTESIAN_POINT('Ctrl Pts',(-14.9347982932636,12.6021186018862,
132.203358631515)) ;
#129093 = CARTESIAN_POINT('Ctrl Pts',(-15.0246662575928,12.4130744412516,
132.432874233369)) ;
#129094 = CARTESIAN_POINT('Ctrl Pts',(-15.1289271190847,12.2953575367152,
132.704129028341)) ;
#129095 = CARTESIAN_POINT('Ctrl Pts',(-15.2390105465142,12.2595400052722,
132.9926724095)) ;
#129096 = CARTESIAN_POINT('Ctrl Pts',(-15.3487113523538,12.3063152816415,
133.280070351324)) ;
#129097 = CARTESIAN_POINT('Ctrl Pts',(-15.4514320482357,12.4341408158502,
133.546864149425)) ;
#129098 = CARTESIAN_POINT('Ctrl Pts',(-15.5391158365436,12.6316134537437,
133.770005058121)) ;
#129099 = CARTESIAN_POINT('Ctrl Pts',(-15.6073687443637,12.8861349922411,
133.9362737051)) ;
#129100 = CARTESIAN_POINT('Ctrl Pts',(-15.6516716819306,13.1792138645797,
134.032575547946)) ;
#129101 = CARTESIAN_POINT('Ctrl Pts',(-15.6695953949056,13.4905686905893,
134.051730810821)) ;
#129102 = CARTESIAN_POINT('Ctrl Pts',(-15.6604169021637,13.7964603430473,
133.991777195623)) ;
#129103 = CARTESIAN_POINT('Ctrl Pts',(-15.6258987359129,14.0743847640953,
133.857952822959)) ;
#129104 = CARTESIAN_POINT('Ctrl Pts',(-15.5689424529067,14.3070162131528,
133.658441754643)) ;
#129105 = CARTESIAN_POINT('Ctrl Pts',(-15.4941859183638,14.4764518119822,
133.406859608136)) ;
#129106 = CARTESIAN_POINT('Ctrl Pts',(-15.4083342578243,14.5698501625241,
133.123024051053)) ;
#129107 = CARTESIAN_POINT('Ctrl Pts',(-15.3176422912758,14.5816111326668,
132.82495471565)) ;
#129108 = CARTESIAN_POINT('Ctrl Pts',(-15.2293490886526,14.5098992068035,
132.53380903365)) ;
#129109 = CARTESIAN_POINT('Ctrl Pts',(-15.1509641087805,14.3604030985763,
132.271696519676)) ;
#129110 = CARTESIAN_POINT('Ctrl Pts',(-15.0885882766536,14.1435657734104,
132.056328026894)) ;
#129111 = CARTESIAN_POINT('Ctrl Pts',(-15.0475171969358,13.8762647134096,
131.90333144506)) ;
#129112 = CARTESIAN_POINT('Ctrl Pts',(-15.0311871549161,13.5746435358358,
131.822388428591)) ;
#129113 = CARTESIAN_POINT('Ctrl Pts',(-15.0415879944804,13.2647987939523,
131.819827576964)) ;
#129114 = CARTESIAN_POINT('Ctrl Pts',(-15.0788068560028,12.9638357563477,
131.895337689995)) ;
#129115 = CARTESIAN_POINT('Ctrl Pts',(-15.1408172739775,12.6967407948571,
132.043374153266)) ;
#129116 = CARTESIAN_POINT('Ctrl Pts',(-15.2239197092677,12.481516798795,132.253008004637)) ;
#129117 = CARTESIAN_POINT('Ctrl Pts',(-15.3228857413039,12.3337893926253,
132.50899135009)) ;
#129118 = CARTESIAN_POINT('Ctrl Pts',(-15.431430165252,12.264079799943,132.792934661794)) ;
#129119 = CARTESIAN_POINT('Ctrl Pts',(-15.5422439139297,12.2774691330631,
133.08356318742)) ;
#129120 = CARTESIAN_POINT('Ctrl Pts',(-15.6482784383748,12.3724670081561,
133.360251299871)) ;
#129121 = CARTESIAN_POINT('Ctrl Pts',(-15.7431900439343,12.5437673872502,
133.604261147898)) ;
#129122 = CARTESIAN_POINT('Ctrl Pts',(-15.8197543818073,12.7765746367498,
133.794928013366)) ;
#129123 = CARTESIAN_POINT('Ctrl Pts',(-15.8742879735741,13.056442650052,133.921098919805)) ;
#129124 = CARTESIAN_POINT('Ctrl Pts',(-15.9031133081289,13.3632373960093,
133.972110741397)) ;
#129125 = CARTESIAN_POINT('Ctrl Pts',(-15.9049895115739,13.6730054777402,
133.944546039053)) ;
#129126 = CARTESIAN_POINT('Ctrl Pts',(-15.8802545110404,13.9671153090071,
133.838972001116)) ;
#129127 = CARTESIAN_POINT('Ctrl Pts',(-15.8320488758174,14.2192390976399,
133.665214561811)) ;
#129128 = CARTESIAN_POINT('Ctrl Pts',(-15.7637592246223,14.4164802278466,
133.432495927919)) ;
#129129 = CARTESIAN_POINT('Ctrl Pts',(-15.6816763634688,14.5415580379271,
133.159645677855)) ;
#129130 = CARTESIAN_POINT('Ctrl Pts',(-15.5920508372998,14.5869148385537,
132.864711325066)) ;
#129131 = CARTESIAN_POINT('Ctrl Pts',(-15.5021160215326,14.5490099524811,
132.56888691804)) ;
#129132 = CARTESIAN_POINT('Ctrl Pts',(-15.4187916392682,14.4299835675068,
132.292268421048)) ;
#129133 = CARTESIAN_POINT('Ctrl Pts',(-15.3493635815801,14.2395160245118,
132.056400600707)) ;
#129134 = CARTESIAN_POINT('Ctrl Pts',(-15.2989597100586,13.9900850970595,
131.876007619012)) ;
#129135 = CARTESIAN_POINT('Ctrl Pts',(-15.272218093911,13.7002631215164,131.764776828578)) ;
#129136 = CARTESIAN_POINT('Ctrl Pts',(-15.2716505882856,13.3906063614652,
131.730004772905)) ;
#129137 = CARTESIAN_POINT('Ctrl Pts',(-15.2981644321246,13.0826197728353,
131.774272870496)) ;
#129138 = CARTESIAN_POINT('Ctrl Pts',(-15.3504644959401,12.799748141124,131.893944982008)) ;
#129139 = CARTESIAN_POINT('Ctrl Pts',(-15.4255037118289,12.5614903219102,
132.080049932649)) ;
#129140 = CARTESIAN_POINT('Ctrl Pts',(-15.5188545837591,12.3846250484045,
132.319591184362)) ;
#129141 = CARTESIAN_POINT('Ctrl Pts',(-15.6243621794924,12.2824688023076,
132.594668003759)) ;
#129142 = CARTESIAN_POINT('Ctrl Pts',(-15.7348925303378,12.2619556296945,
132.884516282295)) ;
#129143 = CARTESIAN_POINT('Ctrl Pts',(-15.8440119597469,12.3244284918516,
133.170121702575)) ;
#129144 = CARTESIAN_POINT('Ctrl Pts',(-15.9443512957769,12.4664339674621,
133.430007529672)) ;
#129145 = CARTESIAN_POINT('Ctrl Pts',(-16.0286266715396,12.6753486557463,
133.64323601442)) ;
#129146 = CARTESIAN_POINT('Ctrl Pts',(-16.0927613820503,12.9390313518122,
133.797416214201)) ;
#129147 = CARTESIAN_POINT('Ctrl Pts',(-16.1322240438312,13.2369182053758,
133.879596524475)) ;
#129148 = CARTESIAN_POINT('Ctrl Pts',(-16.1450073393233,13.5497742859679,
133.883656973668)) ;
#129149 = CARTESIAN_POINT('Ctrl Pts',(-16.1309752238549,13.8506093508767,
133.809712924713)) ;
#129150 = CARTESIAN_POINT('Ctrl Pts',(-16.0917806117036,14.1229208970494,
133.662027117479)) ;
#129151 = CARTESIAN_POINT('Ctrl Pts',(-16.0311608129876,14.3440340084818,
133.451889788938)) ;
#129152 = CARTESIAN_POINT('Ctrl Pts',(-15.9539287114878,14.5000650086301,
133.193133120408)) ;
#129153 = CARTESIAN_POINT('Ctrl Pts',(-15.8659835029665,14.5786444496306,
132.902928525626)) ;
#129154 = CARTESIAN_POINT('Ctrl Pts',(-15.7758709261625,14.5743811791395,
132.606790036893)) ;
#129155 = CARTESIAN_POINT('Ctrl Pts',(-15.6886304289123,14.4873599141627,
132.318627596167)) ;
#129156 = CARTESIAN_POINT('Ctrl Pts',(-15.6129042871571,14.3240887387416,
132.064305156587)) ;
#129157 = CARTESIAN_POINT('Ctrl Pts',(-15.5543635865499,14.0972553768965,
131.860272571408)) ;
#129158 = CARTESIAN_POINT('Ctrl Pts',(-15.517587454923,13.8219068186535,131.719757504624)) ;
#129159 = CARTESIAN_POINT('Ctrl Pts',(-15.5061671790112,13.5160257304535,
131.653105199681)) ;
#129160 = CARTESIAN_POINT('Ctrl Pts',(-15.5218470098257,13.2050738330625,
131.665795904458)) ;
#129161 = CARTESIAN_POINT('Ctrl Pts',(-15.5637864688922,12.9106474660782,
131.755303957723)) ;
#129162 = CARTESIAN_POINT('Ctrl Pts',(-15.6300512629826,12.6518068845878,
131.915759644786)) ;
#129163 = CARTESIAN_POINT('Ctrl Pts',(-15.7166383035372,12.4481718764226,
132.135556413603)) ;
#129164 = CARTESIAN_POINT('Ctrl Pts',(-15.8179132984019,12.314346622866,132.398281612479)) ;
#129165 = CARTESIAN_POINT('Ctrl Pts',(-15.9278856597735,12.2602411291599,
132.686273104354)) ;
#129166 = CARTESIAN_POINT('Ctrl Pts',(-16.0376086994621,12.289044210784,132.973945221982)) ;
#129167 = CARTESIAN_POINT('Ctrl Pts',(-16.1426489958405,12.3996398985986,
133.247503974334)) ;
#129168 = CARTESIAN_POINT('Ctrl Pts',(-16.2340318975309,12.5827969028938,
133.481431287424)) ;
#129169 = CARTESIAN_POINT('Ctrl Pts',(-16.3071554186046,12.8269629878668,
133.661853204856)) ;
#129170 = CARTESIAN_POINT('Ctrl Pts',(-16.3568161319852,13.1127056220744,
133.773888186978)) ;
#129171 = CARTESIAN_POINT('Ctrl Pts',(-16.3806449236658,13.4217118821407,
133.810331791983)) ;
#129172 = CARTESIAN_POINT('Ctrl Pts',(-16.377439581411,13.73042511485,133.767855369085)) ;
#129173 = CARTESIAN_POINT('Ctrl Pts',(-16.3479691030351,14.0183443112805,
133.648491790716)) ;
#129174 = CARTESIAN_POINT('Ctrl Pts',(-16.2955799140703,14.2615011985034,
133.462442962247)) ;
#129175 = CARTESIAN_POINT('Ctrl Pts',(-16.2243937788781,14.4455241600489,
133.221377680409)) ;
#129176 = CARTESIAN_POINT('Ctrl Pts',(-16.1403852077266,14.5564730484766,
132.942888766388)) ;
#129177 = CARTESIAN_POINT('Ctrl Pts',(-16.049570185435,14.5860332576142,132.644269887885)) ;
#129178 = CARTESIAN_POINT('Ctrl Pts',(-15.9609660140179,14.5327319969804,
132.352549382835)) ;
#129179 = CARTESIAN_POINT('Ctrl Pts',(-15.879392560384,14.3988255377981,132.080913727718)) ;
#129180 = CARTESIAN_POINT('Ctrl Pts',(-15.8134294633956,14.1966329987979,
131.855270403513)) ;
#129181 = CARTESIAN_POINT('Ctrl Pts',(-15.7671288771727,13.9381995065902,
131.686862264582)) ;
#129182 = CARTESIAN_POINT('Ctrl Pts',(-15.7451534934309,13.64215083048,131.589466301994)) ;
#129183 = CARTESIAN_POINT('Ctrl Pts',(-15.7497253677879,13.3319748624789,
131.569786305151)) ;
#129184 = CARTESIAN_POINT('Ctrl Pts',(-15.7810839054332,13.0275242268779,
131.628280225436)) ;
#129185 = CARTESIAN_POINT('Ctrl Pts',(-15.8383251199372,12.7499513876655,
131.762184797718)) ;
#129186 = CARTESIAN_POINT('Ctrl Pts',(-15.9170076046053,12.5230806555812,
131.959040186424)) ;
#129187 = CARTESIAN_POINT('Ctrl Pts',(-16.0129847307109,12.3595163887299,
132.206295823084)) ;
#129188 = CARTESIAN_POINT('Ctrl Pts',(-16.1202899369408,12.2720601229367,
132.486548175091)) ;
#129189 = CARTESIAN_POINT('Ctrl Pts',(-16.2314011652386,12.2676665272562,
132.77798081952)) ;
#129190 = CARTESIAN_POINT('Ctrl Pts',(-16.3386053442053,12.3451447883363,
133.058221097043)) ;
#129191 = CARTESIAN_POINT('Ctrl Pts',(-16.4364726934134,12.5004781878849,
133.310918034804)) ;
#129192 = CARTESIAN_POINT('Ctrl Pts',(-16.5175132252489,12.7212076725333,
133.514603343061)) ;
#129193 = CARTESIAN_POINT('Ctrl Pts',(-16.5773484087044,12.9936144334216,
133.656155150364)) ;
#129194 = CARTESIAN_POINT('Ctrl Pts',(-16.6117393173517,13.2947836175078,
133.723619906867)) ;
#129195 = CARTESIAN_POINT('Ctrl Pts',(-16.6195349325509,13.6064067051063,
133.713244471192)) ;
#129196 = CARTESIAN_POINT('Ctrl Pts',(-16.6005564591254,13.9050216556666,
133.624641768626)) ;
#129197 = CARTESIAN_POINT('Ctrl Pts',(-16.5570362865346,14.1686336001984,
133.464397749618)) ;
#129198 = CARTESIAN_POINT('Ctrl Pts',(-16.4928541402158,14.378818223522,133.243813490969)) ;
#129199 = CARTESIAN_POINT('Ctrl Pts',(-16.4131723103661,14.520866250274,132.977903847769)) ;
#129200 = CARTESIAN_POINT('Ctrl Pts',(-16.324418752034,14.5841619926364,132.685464359958)) ;
#129201 = CARTESIAN_POINT('Ctrl Pts',(-16.2339590586159,14.5641966334699,
132.388108863399)) ;
#129202 = CARTESIAN_POINT('Ctrl Pts',(-16.1487199252297,14.4625802261662,
132.105972172714)) ;
#129203 = CARTESIAN_POINT('Ctrl Pts',(-16.0755352121241,14.2860055470816,
131.858992129095)) ;
#129204 = CARTESIAN_POINT('Ctrl Pts',(-16.0207525963594,14.0484512040757,
131.665905798097)) ;
#129205 = CARTESIAN_POINT('Ctrl Pts',(-15.988546581059,13.7663469877686,131.538764120789)) ;
#129206 = CARTESIAN_POINT('Ctrl Pts',(-15.9821721421647,13.4574608016115,
131.486848095998)) ;
#129207 = CARTESIAN_POINT('Ctrl Pts',(-16.0027619761264,13.1488899436826,
131.514007237781)) ;
#129208 = CARTESIAN_POINT('Ctrl Pts',(-16.049615622405,12.8583365068185,131.617715430164)) ;
#129209 = CARTESIAN_POINT('Ctrl Pts',(-16.1201676913662,12.6085157636358,
131.790669007322)) ;
#129210 = CARTESIAN_POINT('Ctrl Pts',(-16.2098079305234,12.4173946881525,
132.019450745302)) ;
#129211 = CARTESIAN_POINT('Ctrl Pts',(-16.3131800358718,12.2980452511377,
132.288293077009)) ;
#129212 = CARTESIAN_POINT('Ctrl Pts',(-16.423261619167,12.2592457783441,132.576798899315)) ;
#129213 = CARTESIAN_POINT('Ctrl Pts',(-16.5335959230037,12.3040208599772,
132.865888151637)) ;
#129214 = CARTESIAN_POINT('Ctrl Pts',(-16.6359277149238,12.42869393012,133.131777211617)) ;
#129215 = CARTESIAN_POINT('Ctrl Pts',(-16.7244699466103,12.6243589904513,
133.357335318922)) ;
#129216 = CARTESIAN_POINT('Ctrl Pts',(-16.7936703717637,12.8789083134422,
133.52620265048)) ;
#129217 = CARTESIAN_POINT('Ctrl Pts',(-16.8384788441524,13.1702260749438,
133.624095874272)) ;
#129218 = CARTESIAN_POINT('Ctrl Pts',(-16.857225046346,13.4805036565043,133.645741963258)) ;
#129219 = CARTESIAN_POINT('Ctrl Pts',(-16.8489063138927,13.7876510907378,
133.588224449993)) ;
#129220 = CARTESIAN_POINT('Ctrl Pts',(-16.8148392702879,14.0678452038592,
133.455558574279)) ;
#129221 = CARTESIAN_POINT('Ctrl Pts',(-16.7587271978749,14.3007432153336,
133.258689436977)) ;
#129222 = CARTESIAN_POINT('Ctrl Pts',(-16.684354006604,14.4725786028925,133.00818610044)) ;
#129223 = CARTESIAN_POINT('Ctrl Pts',(-16.5987270141233,14.5682598705244,
132.725006844455)) ;
#129224 = CARTESIAN_POINT('Ctrl Pts',(-16.508083118961,14.582415300085,132.427079939102)) ;
#129225 = CARTESIAN_POINT('Ctrl Pts',(-16.4197468519132,14.5133615021942,
132.13586794255)) ;
#129226 = CARTESIAN_POINT('Ctrl Pts',(-16.3408443778437,14.3656856001402,
131.872174755778)) ;
#129227 = CARTESIAN_POINT('Ctrl Pts',(-16.2781611136979,14.1519224163712,
131.656079963678)) ;
#129228 = CARTESIAN_POINT('Ctrl Pts',(-16.2360715647158,13.8839966757843,
131.499861935695)) ;
#129229 = CARTESIAN_POINT('Ctrl Pts',(-16.2190922770335,13.5839687082689,
131.417139097658)) ;
#129230 = CARTESIAN_POINT('Ctrl Pts',(-16.228706420837,13.2736212101871,131.412219775263)) ;
#129231 = CARTESIAN_POINT('Ctrl Pts',(-16.2650473903063,12.972761740788,131.485254270493)) ;
#129232 = CARTESIAN_POINT('Ctrl Pts',(-16.3265741277852,12.7034621724925,
131.631760171048)) ;
#129233 = CARTESIAN_POINT('Ctrl Pts',(-16.4091164711671,12.4867212726039,
131.839780973645)) ;
#129234 = CARTESIAN_POINT('Ctrl Pts',(-16.5078141561467,12.33686375234,132.094949163634)) ;
#129235 = CARTESIAN_POINT('Ctrl Pts',(-16.6158219520768,12.2650347020363,
132.377434648052)) ;
#129236 = CARTESIAN_POINT('Ctrl Pts',(-16.7269532891186,12.2758062427332,
132.668907462376)) ;
#129237 = CARTESIAN_POINT('Ctrl Pts',(-16.8336048391349,12.3692806824326,
132.947266347668)) ;
#129238 = CARTESIAN_POINT('Ctrl Pts',(-16.9284317414451,12.5378928700438,
133.191194855104)) ;
#129239 = CARTESIAN_POINT('Ctrl Pts',(-17.0057245470623,12.7694276671961,
133.383932637994)) ;
#129240 = CARTESIAN_POINT('Ctrl Pts',(-17.0609458230703,13.0484835222186,
133.512094105767)) ;
#129241 = CARTESIAN_POINT('Ctrl Pts',(-17.0904966230258,13.3553251323831,
133.565175957741)) ;
#129242 = CARTESIAN_POINT('Ctrl Pts',(-17.0930427512237,13.6640555528138,
133.539693243404)) ;
#129243 = CARTESIAN_POINT('Ctrl Pts',(-17.0693003062227,13.9577070020221,
133.437180645655)) ;
#129244 = CARTESIAN_POINT('Ctrl Pts',(-17.0215202195115,14.2128779574234,
133.264471361795)) ;
#129245 = CARTESIAN_POINT('Ctrl Pts',(-16.9536976019041,14.4117544090383,
133.033127560494)) ;
#129246 = CARTESIAN_POINT('Ctrl Pts',(-16.8719823256452,14.5391282978367,
132.761364728031)) ;
#129247 = CARTESIAN_POINT('Ctrl Pts',(-16.7820589422562,14.5867879388137,
132.465410805386)) ;
#129248 = CARTESIAN_POINT('Ctrl Pts',(-16.6924665130693,14.5512051558335,
132.17074476344)) ;
#129249 = CARTESIAN_POINT('Ctrl Pts',(-16.6087056500292,14.4343419868163,
131.892798100955)) ;
#129250 = CARTESIAN_POINT('Ctrl Pts',(-16.538832091035,14.2455278890041,131.65562031777)) ;
#129251 = CARTESIAN_POINT('Ctrl Pts',(-16.4879190259306,13.9981929113896,
131.47382165514)) ;
#129252 = CARTESIAN_POINT('Ctrl Pts',(-16.4603768158028,13.7085066713852,
131.360165716165)) ;
#129253 = CARTESIAN_POINT('Ctrl Pts',(-16.4591129437466,13.399579397686,131.323410336661)) ;
#129254 = CARTESIAN_POINT('Ctrl Pts',(-16.484691657851,13.0919774800644,131.365036261441)) ;
#129255 = CARTESIAN_POINT('Ctrl Pts',(-16.5365613200866,12.8067303941414,
131.483283731596)) ;
#129256 = CARTESIAN_POINT('Ctrl Pts',(-16.6106299167186,12.5682009002538,
131.666727984921)) ;
#129257 = CARTESIAN_POINT('Ctrl Pts',(-16.703661484763,12.3888212381261,131.905270268361)) ;
#129258 = CARTESIAN_POINT('Ctrl Pts',(-16.8087651880266,12.2844119567793,
132.179212799551)) ;
#129259 = CARTESIAN_POINT('Ctrl Pts',(-16.9195860446724,12.2613333921228,
132.469805102314)) ;
#129260 = CARTESIAN_POINT('Ctrl Pts',(-17.0287241594816,12.3215794364131,
132.755502128305)) ;
#129261 = CARTESIAN_POINT('Ctrl Pts',(-17.1290959969068,12.460691871722,133.015600065389)) ;
#129262 = CARTESIAN_POINT('Ctrl Pts',(-17.2142928173378,12.6684213350559,
133.231391682523)) ;
#129263 = CARTESIAN_POINT('Ctrl Pts',(-17.2792269999154,12.9319194586172,
133.387791946882)) ;
#129264 = CARTESIAN_POINT('Ctrl Pts',(-17.3191658999381,13.227908152673,133.471502696313)) ;
#129265 = CARTESIAN_POINT('Ctrl Pts',(-17.3328145145393,13.5392232276546,
133.478245333532)) ;
#129266 = CARTESIAN_POINT('Ctrl Pts',(-17.319569038104,13.842168223521,133.406437925368)) ;
#129267 = CARTESIAN_POINT('Ctrl Pts',(-17.2810019534039,14.115831938889,133.260561997188)) ;
#129268 = CARTESIAN_POINT('Ctrl Pts',(-17.2207880893722,14.3390092448437,
133.0515426788)) ;
#129269 = CARTESIAN_POINT('Ctrl Pts',(-17.1440720435031,14.4964745213525,
132.794365747161)) ;
#129270 = CARTESIAN_POINT('Ctrl Pts',(-17.0568630848371,14.5773715613601,
132.506502793467)) ;
#129271 = CARTESIAN_POINT('Ctrl Pts',(-16.9660480537129,14.5757025452078,
132.208057598299)) ;
#129272 = CARTESIAN_POINT('Ctrl Pts',(-16.8788431858424,14.4908671565799,
131.920085188668)) ;
#129273 = CARTESIAN_POINT('Ctrl Pts',(-16.8029585654165,14.3305923822081,
131.665427504091)) ;
#129274 = CARTESIAN_POINT('Ctrl Pts',(-16.7435309388087,14.104809150226,131.458681664569)) ;
#129275 = CARTESIAN_POINT('Ctrl Pts',(-16.7060430507986,13.8293692517449,
131.315961230469)) ;
#129276 = CARTESIAN_POINT('Ctrl Pts',(-16.693936404888,13.5265764588792,131.247582518376)) ;
#129277 = CARTESIAN_POINT('Ctrl Pts',(-16.708699103235,13.2147295864641,131.25750947637)) ;
#129278 = CARTESIAN_POINT('Ctrl Pts',(-16.749940948686,12.9189025959915,131.344918847352)) ;
#129279 = CARTESIAN_POINT('Ctrl Pts',(-16.8158171841197,12.6580300058624,
131.504131716298)) ;
#129280 = CARTESIAN_POINT('Ctrl Pts',(-16.9015293870053,12.4534346092271,
131.721516359276)) ;
#129281 = CARTESIAN_POINT('Ctrl Pts',(-17.0027137249338,12.3171076875182,
131.983889087043)) ;
#129282 = CARTESIAN_POINT('Ctrl Pts',(-17.1119673542446,12.2606844041001,
132.269957584545)) ;
#129283 = CARTESIAN_POINT('Ctrl Pts',(-17.2225632011221,12.28708894542,132.559937626368)) ;
#129284 = CARTESIAN_POINT('Ctrl Pts',(-17.3278048536779,12.3957982979784,
132.834097357884)) ;
#129285 = CARTESIAN_POINT('Ctrl Pts',(-17.4194176571879,12.5767256931705,
133.068762679094)) ;
#129286 = CARTESIAN_POINT('Ctrl Pts',(-17.493044253941,12.8186993090181,133.250730862918)) ;
#129287 = CARTESIAN_POINT('Ctrl Pts',(-17.5436697534756,13.1050418122632,
133.365405420034)) ;
#129288 = CARTESIAN_POINT('Ctrl Pts',(-17.5681129690375,13.4130762774239,
133.40372138138)) ;
#129289 = CARTESIAN_POINT('Ctrl Pts',(-17.5656637238399,13.7214651922854,
133.36351270507)) ;
#129290 = CARTESIAN_POINT('Ctrl Pts',(-17.5371700854611,14.0093161803211,
133.247144420446)) ;
#129291 = CARTESIAN_POINT('Ctrl Pts',(-17.4849725016858,14.2560736745197,
133.061372547591)) ;
#129292 = CARTESIAN_POINT('Ctrl Pts',(-17.4143885017694,14.4412184324741,
132.822170207149)) ;
#129293 = CARTESIAN_POINT('Ctrl Pts',(-17.3306747567121,14.5543182486296,
132.544541120772)) ;
#129294 = CARTESIAN_POINT('Ctrl Pts',(-17.2403639651478,14.5864671226158,
132.247555986274)) ;
#129295 = CARTESIAN_POINT('Ctrl Pts',(-17.1510139448171,14.5351930483474,
131.953422292404)) ;
#129296 = CARTESIAN_POINT('Ctrl Pts',(-17.0696123032485,14.4042256836979,
131.682497044218)) ;
#129297 = CARTESIAN_POINT('Ctrl Pts',(-17.0028303657657,14.2033620376663,
131.454334310528)) ;
#129298 = CARTESIAN_POINT('Ctrl Pts',(-16.9559126255241,13.9460943554148,
131.284116174304)) ;
#129299 = CARTESIAN_POINT('Ctrl Pts',(-16.9332167115845,13.6510940707038,
131.184642433927)) ;
#129300 = CARTESIAN_POINT('Ctrl Pts',(-16.9369769560301,13.340963323575,131.162583892338)) ;
#129301 = CARTESIAN_POINT('Ctrl Pts',(-16.9676993284991,13.0355469770442,
131.219159783569)) ;
#129302 = CARTESIAN_POINT('Ctrl Pts',(-17.0238499504818,12.7584810816834,
131.3500834927)) ;
#129303 = CARTESIAN_POINT('Ctrl Pts',(-17.1022027786305,12.5287899159639,
131.545836377495)) ;
#129304 = CARTESIAN_POINT('Ctrl Pts',(-17.1977759409222,12.3633457442531,
131.791921351567)) ;
#129305 = CARTESIAN_POINT('Ctrl Pts',(-17.3044741521689,12.2737023514909,
132.070510336543)) ;
#129306 = CARTESIAN_POINT('Ctrl Pts',(-17.4156081788106,12.2663504443872,
132.362000980484)) ;
#129307 = CARTESIAN_POINT('Ctrl Pts',(-17.5236663849567,12.3420800967331,
132.644528547353)) ;
#129308 = CARTESIAN_POINT('Ctrl Pts',(-17.6214436234339,12.4946575605773,
132.897122538516)) ;
#129309 = CARTESIAN_POINT('Ctrl Pts',(-17.7033350086812,12.7142648856192,
133.103184303582)) ;
#129310 = CARTESIAN_POINT('Ctrl Pts',(-17.7637633207662,12.9853993961476,
133.246492127846)) ;
#129311 = CARTESIAN_POINT('Ctrl Pts',(-17.7989327686341,13.2860373557687,
133.316222270595)) ;
#129312 = CARTESIAN_POINT('Ctrl Pts',(-17.8074758097156,13.5985521220417,
133.307942379033)) ;
#129313 = CARTESIAN_POINT('Ctrl Pts',(-17.7891330033214,13.8975127829307,
133.221220006)) ;
#129314 = CARTESIAN_POINT('Ctrl Pts',(-17.7464726108498,14.1612605834451,
133.063631344191)) ;
#129315 = CARTESIAN_POINT('Ctrl Pts',(-17.6826753131341,14.3739607965711,
132.844075788855)) ;
#129316 = CARTESIAN_POINT('Ctrl Pts',(-17.603060579253,14.5182946770733,132.578264088989)) ;
#129317 = CARTESIAN_POINT('Ctrl Pts',(-17.5146145686403,14.5834512789115,
132.286785455906)) ;
#129318 = CARTESIAN_POINT('Ctrl Pts',(-17.4244047684484,14.5659482327596,
131.990267496769)) ;
#129319 = CARTESIAN_POINT('Ctrl Pts',(-17.3389354411882,14.4667698012676,
131.707468479579)) ;
#129320 = CARTESIAN_POINT('Ctrl Pts',(-17.2652382607785,14.2923286042259,
131.458983161722)) ;
#129321 = CARTESIAN_POINT('Ctrl Pts',(-17.2096082359978,14.0548140829524,
131.26323131239)) ;
#129322 = CARTESIAN_POINT('Ctrl Pts',(-17.1769815564138,13.7751054623822,
131.135039548468)) ;
#129323 = CARTESIAN_POINT('Ctrl Pts',(-17.1697052026753,13.4671707180117,
131.080539965422)) ;
#129324 = CARTESIAN_POINT('Ctrl Pts',(-17.1896989356781,13.1566326950211,
131.105769753584)) ;
#129325 = CARTESIAN_POINT('Ctrl Pts',(-17.2355632547082,12.867030876862,131.206793603253)) ;
#129326 = CARTESIAN_POINT('Ctrl Pts',(-17.3056751958271,12.6146257470566,
131.378333046807)) ;
#129327 = CARTESIAN_POINT('Ctrl Pts',(-17.3950652766615,12.4216271704312,
131.606329591747)) ;
#129328 = CARTESIAN_POINT('Ctrl Pts',(-17.4976480194487,12.300493633533,131.873019824707)) ;
#129329 = CARTESIAN_POINT('Ctrl Pts',(-17.6082564491324,12.2591976943658,
132.162874367726)) ;
#129330 = CARTESIAN_POINT('Ctrl Pts',(-17.7179433027061,12.3014766472521,
132.450298613622)) ;
#129331 = CARTESIAN_POINT('Ctrl Pts',(-17.8208530116508,12.4236752420719,
132.717812378939)) ;
#129332 = CARTESIAN_POINT('Ctrl Pts',(-17.9104061848678,12.619137551761,132.946096908335)) ;
#129333 = CARTESIAN_POINT('Ctrl Pts',(-17.9797132762857,12.8707902283033,
133.115494618903)) ;
#129334 = CARTESIAN_POINT('Ctrl Pts',(-18.0253753807221,13.1617413070734,
133.215817708573)) ;
#129335 = CARTESIAN_POINT('Ctrl Pts',(-18.0448283846108,13.4713352459494,
133.239583447541)) ;
#129336 = CARTESIAN_POINT('Ctrl Pts',(-18.0373267145574,13.778502178637,133.18449510648)) ;
#129337 = CARTESIAN_POINT('Ctrl Pts',(-18.0040868616542,14.0596468984735,
133.054277364002)) ;
#129338 = CARTESIAN_POINT('Ctrl Pts',(-17.9482804203993,14.2953142204187,
132.858131971183)) ;
#129339 = CARTESIAN_POINT('Ctrl Pts',(-17.8743218367002,14.4689647045759,
132.608853860417)) ;
#129340 = CARTESIAN_POINT('Ctrl Pts',(-17.7886594980501,14.5668407202151,
132.325472650321)) ;
#129341 = CARTESIAN_POINT('Ctrl Pts',(-17.6984985567359,14.5831863672356,
132.029126031664)) ;
#129342 = CARTESIAN_POINT('Ctrl Pts',(-17.6096304985475,14.5160479467046,
131.736214040919)) ;
#129343 = CARTESIAN_POINT('Ctrl Pts',(-17.5307892260312,14.371057406114,131.472871564187)) ;
#129344 = CARTESIAN_POINT('Ctrl Pts',(-17.4674191397048,14.1586832935138,
131.254698279897)) ;
#129345 = CARTESIAN_POINT('Ctrl Pts',(-17.4247767870597,13.8924169027706,
131.096926633318)) ;
#129346 = CARTESIAN_POINT('Ctrl Pts',(-17.4069871935266,13.5934591668299,
131.01187365005)) ;
#129347 = CARTESIAN_POINT('Ctrl Pts',(-17.4158629113068,13.2817950572783,
131.004657265815)) ;
#129348 = CARTESIAN_POINT('Ctrl Pts',(-17.4515297582126,12.9807521840059,
131.07575753327)) ;
#129349 = CARTESIAN_POINT('Ctrl Pts',(-17.5120221179879,12.7114089548823,
131.219401548135)) ;
#129350 = CARTESIAN_POINT('Ctrl Pts',(-17.5942883632725,12.4920356351317,
131.426490532179)) ;
#129351 = CARTESIAN_POINT('Ctrl Pts',(-17.6923381457244,12.3404092688171,
131.679857275332)) ;
#129352 = CARTESIAN_POINT('Ctrl Pts',(-17.8005326892055,12.2658594334509,
131.962769942963)) ;
#129353 = CARTESIAN_POINT('Ctrl Pts',(-17.9115353857862,12.2744067631739,
132.253913270118)) ;
#129354 = CARTESIAN_POINT('Ctrl Pts',(-18.0181294194039,12.3651073313828,
132.532197896733)) ;
#129355 = CARTESIAN_POINT('Ctrl Pts',(-18.1135581728837,12.5316552187529,
132.777840247102)) ;
#129356 = CARTESIAN_POINT('Ctrl Pts',(-18.1916435512604,12.7621960771077,
132.972806338441)) ;
#129357 = CARTESIAN_POINT('Ctrl Pts',(-18.2474496440388,13.0400248542652,
133.102701427836)) ;
#129358 = CARTESIAN_POINT('Ctrl Pts',(-18.2777567173541,13.3449924415224,
133.158139314612)) ;
#129359 = CARTESIAN_POINT('Ctrl Pts',(-18.2811288977963,13.6560823827408,
133.134834483101)) ;
#129360 = CARTESIAN_POINT('Ctrl Pts',(-18.2581110947125,13.9495229886617,
133.034546912265)) ;
#129361 = CARTESIAN_POINT('Ctrl Pts',(-18.2110303763221,14.2060601785511,
132.863887514519)) ;
#129362 = CARTESIAN_POINT('Ctrl Pts',(-18.1437370687427,14.406853356067,132.63409799875)) ;
#129363 = CARTESIAN_POINT('Ctrl Pts',(-18.0622395109045,14.5364834433348,
132.362928416151)) ;
#129364 = CARTESIAN_POINT('Ctrl Pts',(-17.9728141363402,14.5865952299809,
132.068568266676)) ;
#129365 = CARTESIAN_POINT('Ctrl Pts',(-17.8826496229748,14.5532896957255,
131.772047908953)) ;
#129366 = CARTESIAN_POINT('Ctrl Pts',(-17.7989857572976,14.4391769984152,
131.494542329969)) ;
#129367 = CARTESIAN_POINT('Ctrl Pts',(-17.7284523059313,14.2521193913653,
131.255364723917)) ;
#129368 = CARTESIAN_POINT('Ctrl Pts',(-17.6769029344046,14.0064609984077,
131.07172935955)) ;
#129369 = CARTESIAN_POINT('Ctrl Pts',(-17.6485455441953,13.7162751815943,
130.955532254004)) ;
#129370 = CARTESIAN_POINT('Ctrl Pts',(-17.6465647200914,13.4088590373153,
130.916820567134)) ;
#129371 = CARTESIAN_POINT('Ctrl Pts',(-17.6713883006356,13.1005339058846,
130.956196977989)) ;
#129372 = CARTESIAN_POINT('Ctrl Pts',(-17.7223049769936,12.8153801533597,
131.071793160456)) ;
#129373 = CARTESIAN_POINT('Ctrl Pts',(-17.7959144365943,12.5742829537778,
131.253789203923)) ;
#129374 = CARTESIAN_POINT('Ctrl Pts',(-17.8889904476805,12.392420790546,131.492309375237)) ;
#129375 = CARTESIAN_POINT('Ctrl Pts',(-17.9933039878901,12.2864008615048,
131.764116093955)) ;
#129376 = CARTESIAN_POINT('Ctrl Pts',(-18.1044185442691,12.2608494064564,
132.055456688157)) ;
#129377 = CARTESIAN_POINT('Ctrl Pts',(-18.2132410021539,12.3186106427626,
132.340370823926)) ;
#129378 = CARTESIAN_POINT('Ctrl Pts',(-18.3141761412567,12.4554522853447,
132.602062304633)) ;
#129379 = CARTESIAN_POINT('Ctrl Pts',(-18.4001753853872,12.6626734835884,
132.820045754456)) ;
#129380 = CARTESIAN_POINT('Ctrl Pts',(-18.4651186131618,12.9221025323028,
132.97681686488)) ;
#129381 = CARTESIAN_POINT('Ctrl Pts',(-18.506216134943,13.2188657935947,133.063721914555)) ;
#129382 = CARTESIAN_POINT('Ctrl Pts',(-18.5205724335731,13.5309968714097,
133.072441184273)) ;
#129383 = CARTESIAN_POINT('Ctrl Pts',(-18.5081122278569,13.833390940375,133.00304473488)) ;
#129384 = CARTESIAN_POINT('Ctrl Pts',(-18.4702838423824,14.1082731705155,
132.859326713092)) ;
#129385 = CARTESIAN_POINT('Ctrl Pts',(-18.4106469707941,14.3332733281916,
132.651988018231)) ;
#129386 = CARTESIAN_POINT('Ctrl Pts',(-18.3341547682758,14.4930898845826,
132.395391176241)) ;
#129387 = CARTESIAN_POINT('Ctrl Pts',(-18.2472492763834,14.5762694584335,
132.108457428325)) ;
#129388 = CARTESIAN_POINT('Ctrl Pts',(-18.1560969095704,14.5766426622739,
131.80889569352)) ;
#129389 = CARTESIAN_POINT('Ctrl Pts',(-18.0694735665927,14.4950562230295,
131.522934074583)) ;
#129390 = CARTESIAN_POINT('Ctrl Pts',(-17.9924950396233,14.3357813404639,
131.264798925683)) ;
#129391 = CARTESIAN_POINT('Ctrl Pts',(-17.9327493732592,14.1117727148765,
131.05719510321)) ;
#129392 = CARTESIAN_POINT('Ctrl Pts',(-17.8945803168045,13.8385113362907,
130.912589041417)) ;
#129393 = CARTESIAN_POINT('Ctrl Pts',(-17.8817102320289,13.5338963360909,
130.841724345729)) ;
#129394 = CARTESIAN_POINT('Ctrl Pts',(-17.895635047292,13.2242576561067,130.849457214998)) ;
#129395 = CARTESIAN_POINT('Ctrl Pts',(-17.9363339259406,12.9262819739174,
130.935110268932)) ;
#129396 = CARTESIAN_POINT('Ctrl Pts',(-18.0011613255471,12.6654698991639,
131.091455088112)) ;
#129397 = CARTESIAN_POINT('Ctrl Pts',(-18.0871709850437,12.4574146452965,
131.309403426712)) ;
#129398 = CARTESIAN_POINT('Ctrl Pts',(-18.1869663728995,12.3205165730399,
131.56807852545)) ;
#129399 = CARTESIAN_POINT('Ctrl Pts',(-18.2966682093311,12.2610390486759,
131.855260917825)) ;
#129400 = CARTESIAN_POINT('Ctrl Pts',(-18.4069695860607,12.2851065048332,
132.144493068143)) ;
#129401 = CARTESIAN_POINT('Ctrl Pts',(-18.5126034033374,12.3913707363663,
132.419764922562)) ;
#129402 = CARTESIAN_POINT('Ctrl Pts',(-18.6047688956456,12.5705078611999,
132.656013947326)) ;
#129403 = CARTESIAN_POINT('Ctrl Pts',(-18.6790012787559,12.8110530748773,
132.839741264095)) ;
#129404 = CARTESIAN_POINT('Ctrl Pts',(-18.7302911873267,13.0958080893831,
132.956423482839)) ;
#129405 = CARTESIAN_POINT('Ctrl Pts',(-18.7555799964295,13.4043791335754,
132.997109048956)) ;
#129406 = CARTESIAN_POINT('Ctrl Pts',(-18.7539405429472,13.7127503625776,
132.959310086933)) ;
#129407 = CARTESIAN_POINT('Ctrl Pts',(-18.7258293961936,14.003146544252,132.843838523491)) ;
#129408 = CARTESIAN_POINT('Ctrl Pts',(-18.6749537414129,14.2480984913921,
132.662380092603)) ;
#129409 = CARTESIAN_POINT('Ctrl Pts',(-18.6044230138764,14.4370589151547,
132.423074769983)) ;
#129410 = CARTESIAN_POINT('Ctrl Pts',(-18.520996512227,14.5521322459825,132.146306985102)) ;
#129411 = CARTESIAN_POINT('Ctrl Pts',(-18.4306794059455,14.5867077629414,
131.849264763677)) ;
#129412 = CARTESIAN_POINT('Ctrl Pts',(-18.3413660662321,14.5378478997284,
131.555300337176)) ;
#129413 = CARTESIAN_POINT('Ctrl Pts',(-18.2596531854169,14.4092030440239,
131.283472890356)) ;
#129414 = CARTESIAN_POINT('Ctrl Pts',(-18.1923026345111,14.2102655467961,
131.053642197071)) ;
#129415 = CARTESIAN_POINT('Ctrl Pts',(-18.1446121318789,13.9531165249686,
130.881020749285)) ;
#129416 = CARTESIAN_POINT('Ctrl Pts',(-18.1213237510083,13.6605445823028,
130.780006916634)) ;
#129417 = CARTESIAN_POINT('Ctrl Pts',(-18.1242927670225,13.3493860420966,
130.755504301991)) ;
#129418 = CARTESIAN_POINT('Ctrl Pts',(-18.1541961965779,13.0444136066678,
130.809790357298)) ;
#129419 = CARTESIAN_POINT('Ctrl Pts',(-18.2096856771492,12.7658509592001,
130.938737600815)) ;
#129420 = CARTESIAN_POINT('Ctrl Pts',(-18.2874255648017,12.5346699181632,
131.132718784265)) ;
#129421 = CARTESIAN_POINT('Ctrl Pts',(-18.3827232290827,12.3668713397562,
131.37794706254)) ;
#129422 = CARTESIAN_POINT('Ctrl Pts',(-18.4894019331544,12.2750736667704,
131.656423092485)) ;
#129423 = CARTESIAN_POINT('Ctrl Pts',(-18.5999461896796,12.2654123740739,
131.946360057731)) ;
#129424 = CARTESIAN_POINT('Ctrl Pts',(-18.7082699182573,12.338500075334,132.229645795639)) ;
#129425 = CARTESIAN_POINT('Ctrl Pts',(-18.8066956525215,12.4893940348924,
132.484046512348)) ;
#129426 = CARTESIAN_POINT('Ctrl Pts',(-18.8890064060484,12.7071834548376,
132.691365787329)) ;
#129427 = CARTESIAN_POINT('Ctrl Pts',(-18.9499792122234,12.9760085814995,
132.836382852014)) ;
#129428 = CARTESIAN_POINT('Ctrl Pts',(-18.986083387819,13.2771670277102,132.908713665755)) ;
#129429 = CARTESIAN_POINT('Ctrl Pts',(-18.9953771961304,13.5885362669385,
132.902752796309)) ;
#129430 = CARTESIAN_POINT('Ctrl Pts',(-18.9779428841239,13.8883473983697,
132.818679469177)) ;
#129431 = CARTESIAN_POINT('Ctrl Pts',(-18.935738241321,14.1546796544185,132.662259619512)) ;
#129432 = CARTESIAN_POINT('Ctrl Pts',(-18.8726034800023,14.3683944607912,
132.444729796403)) ;
#129433 = CARTESIAN_POINT('Ctrl Pts',(-18.7937232819521,14.5146640106003,
132.181190970799)) ;
#129434 = CARTESIAN_POINT('Ctrl Pts',(-18.7051646808948,14.5827891509108,
131.889269134723)) ;
#129435 = CARTESIAN_POINT('Ctrl Pts',(-18.6147024524246,14.5676066114005,
131.59193939095)) ;
#129436 = CARTESIAN_POINT('Ctrl Pts',(-18.5290201629713,14.4706131467255,
131.308524406706)) ;
#129437 = CARTESIAN_POINT('Ctrl Pts',(-18.4550931376209,14.2987449409649,
131.059463494934)) ;
#129438 = CARTESIAN_POINT('Ctrl Pts',(-18.3987987744585,14.063095845739,130.861778311655)) ;
#129439 = CARTESIAN_POINT('Ctrl Pts',(-18.3653036692505,13.783320877813,130.730918820104)) ;
#129440 = CARTESIAN_POINT('Ctrl Pts',(-18.3573754310237,13.4754883561184,
130.674484167362)) ;
#129441 = CARTESIAN_POINT('Ctrl Pts',(-18.3764169558807,13.1664273020677,
130.697118916392)) ;
#129442 = CARTESIAN_POINT('Ctrl Pts',(-18.4217940683259,12.8743475374644,
130.796531690104)) ;
#129443 = CARTESIAN_POINT('Ctrl Pts',(-18.4908985820318,12.6220180754337,
130.965320118566)) ;
#129444 = CARTESIAN_POINT('Ctrl Pts',(-18.5798731137621,12.4263341505379,
131.192035756237)) ;
#129445 = CARTESIAN_POINT('Ctrl Pts',(-18.6827398919646,12.3026056588691,
131.459379942869)) ;
#129446 = CARTESIAN_POINT('Ctrl Pts',(-18.7925820657954,12.2593725245785,
131.747194451469)) ;
#129447 = CARTESIAN_POINT('Ctrl Pts',(-18.902507639715,12.2987734031186,132.035285394968)) ;
#129448 = CARTESIAN_POINT('Ctrl Pts',(-19.0064670714771,12.4202091784099,
132.305601611935)) ;
#129449 = CARTESIAN_POINT('Ctrl Pts',(-19.0954848269158,12.6117736557302,
132.532691445471)) ;
#129450 = CARTESIAN_POINT('Ctrl Pts',(-19.1658110426442,12.8626551517495,
132.704935652386)) ;
#129451 = CARTESIAN_POINT('Ctrl Pts',(-19.2121697896248,13.1527448205317,
132.807303457746)) ;
#129452 = CARTESIAN_POINT('Ctrl Pts',(-19.2324491817657,13.4624297632054,
132.833446100144)) ;
#129453 = CARTESIAN_POINT('Ctrl Pts',(-19.225671158967,13.7701810558333,132.780451712219)) ;
#129454 = CARTESIAN_POINT('Ctrl Pts',(-19.1932078332292,14.0517728078933,
132.65257011804)) ;
#129455 = CARTESIAN_POINT('Ctrl Pts',(-19.1379946589808,14.2892526496134,
132.458138372292)) ;
#129456 = CARTESIAN_POINT('Ctrl Pts',(-19.0644566698038,14.4648239971076,
132.210085328861)) ;
#129457 = CARTESIAN_POINT('Ctrl Pts',(-18.9793343757348,14.5650402955601,
131.928386517091)) ;
#129458 = CARTESIAN_POINT('Ctrl Pts',(-18.8886434300041,14.5837489624633,
131.630274823525)) ;
#129459 = CARTESIAN_POINT('Ctrl Pts',(-18.8004173888174,14.5197168158782,
131.339551521014)) ;
#129460 = CARTESIAN_POINT('Ctrl Pts',(-18.7206220160406,14.3763315271282,
131.073195599226)) ;
#129461 = CARTESIAN_POINT('Ctrl Pts',(-18.6567617236485,14.1656646034779,
130.853606216677)) ;
#129462 = CARTESIAN_POINT('Ctrl Pts',(-18.6133812442094,13.8999129369224,
130.693587403167)) ;
#129463 = CARTESIAN_POINT('Ctrl Pts',(-18.5949518753934,13.6028236441132,
130.60680394849)) ;
#129464 = CARTESIAN_POINT('Ctrl Pts',(-18.6029793109596,13.291184662554,130.597103250091)) ;
#129465 = CARTESIAN_POINT('Ctrl Pts',(-18.6378459697723,12.9894031508225,
130.665859260079)) ;
#129466 = CARTESIAN_POINT('Ctrl Pts',(-18.697941222039,12.7177660513116,130.808203300005)) ;
#129467 = CARTESIAN_POINT('Ctrl Pts',(-18.7796120718618,12.4972590440602,
131.013603451076)) ;
#129468 = CARTESIAN_POINT('Ctrl Pts',(-18.8769989032459,12.3438957808923,
131.265123551428)) ;
#129469 = CARTESIAN_POINT('Ctrl Pts',(-18.9850989880041,12.2668705331881,
131.547727750457)) ;
#129470 = CARTESIAN_POINT('Ctrl Pts',(-19.0959985748491,12.2729077976525,
131.838609074605)) ;
#129471 = CARTESIAN_POINT('Ctrl Pts',(-19.20298136002,12.3614501040313,132.11797427254)) ;
#129472 = CARTESIAN_POINT('Ctrl Pts',(-19.2985829203928,12.5253314471916,
132.364220122057)) ;
#129473 = CARTESIAN_POINT('Ctrl Pts',(-19.3776055221514,12.7552769702176,
132.561768746383)) ;
#129474 = CARTESIAN_POINT('Ctrl Pts',(-19.4338889635372,13.0310568986237,
132.693180609869)) ;
#129475 = CARTESIAN_POINT('Ctrl Pts',(-19.4650400815724,13.3361216893249,
132.751012638428)) ;
#129476 = CARTESIAN_POINT('Ctrl Pts',(-19.4692309832608,13.6463104400421,
132.730217010446)) ;
#129477 = CARTESIAN_POINT('Ctrl Pts',(-19.4468478616773,13.9424873380838,
132.631569354452)) ;
#129478 = CARTESIAN_POINT('Ctrl Pts',(-19.4002106692333,14.2002008792275,
132.462183820064)) ;
#129479 = CARTESIAN_POINT('Ctrl Pts',(-19.3338735917494,14.4015262359145,
132.235406621368)) ;
#129480 = CARTESIAN_POINT('Ctrl Pts',(-19.2525009705936,14.5339054889456,
131.964504538039)) ;
#129481 = CARTESIAN_POINT('Ctrl Pts',(-19.1632581585291,14.5863178639959,
131.670702154855)) ;
#129482 = CARTESIAN_POINT('Ctrl Pts',(-19.0727741133847,14.5553221796482,
131.373161193195)) ;
#129483 = CARTESIAN_POINT('Ctrl Pts',(-18.9888934197537,14.4431215079252,
131.095027066642)) ;
#129484 = CARTESIAN_POINT('Ctrl Pts',(-18.9181460716304,14.2589451950462,
130.855367504887)) ;
#129485 = CARTESIAN_POINT('Ctrl Pts',(-18.8657380795338,14.0132050908334,
130.66902315173)) ;
#129486 = CARTESIAN_POINT('Ctrl Pts',(-18.836868487838,13.7264814717307,130.551624398978)) ;
#129487 = CARTESIAN_POINT('Ctrl Pts',(-18.8340276274913,13.4166671207193,
130.510102042886)) ;
#129488 = CARTESIAN_POINT('Ctrl Pts',(-18.8581413024745,13.1090562113246,
130.54751765992)) ;
#129489 = CARTESIAN_POINT('Ctrl Pts',(-18.9083034310326,12.8228936758021,
130.660907356979)) ;
#129490 = CARTESIAN_POINT('Ctrl Pts',(-18.9813885580166,12.5803482632518,
130.841359582256)) ;
#129491 = CARTESIAN_POINT('Ctrl Pts',(-19.0735507529948,12.3971382948885,
131.077360101158)) ;
#129492 = CARTESIAN_POINT('Ctrl Pts',(-19.1781196028754,12.2881794831016,
131.349740136877)) ;
#129493 = CARTESIAN_POINT('Ctrl Pts',(-19.2889977456715,12.260444772771,131.640444771833)) ;
#129494 = CARTESIAN_POINT('Ctrl Pts',(-19.3981903193112,12.3158800352752,
131.926374136199)) ;
#129495 = CARTESIAN_POINT('Ctrl Pts',(-19.4995415293124,12.4512315889953,
132.189227462612)) ;
#129496 = CARTESIAN_POINT('Ctrl Pts',(-19.5853658796549,12.6546809056087,
132.406990274991)) ;
#129497 = CARTESIAN_POINT('Ctrl Pts',(-19.6515319436579,12.9147730695688,
132.567062358423)) ;
#129498 = CARTESIAN_POINT('Ctrl Pts',(-19.6931210807734,13.2095558762223,
132.655557138369)) ;
#129499 = CARTESIAN_POINT('Ctrl Pts',(-19.7083399050478,13.5223873446286,
132.666701944993)) ;
#129500 = CARTESIAN_POINT('Ctrl Pts',(-19.69663409254,13.8250174171808,132.599547279371)) ;
#129501 = CARTESIAN_POINT('Ctrl Pts',(-19.6592874859553,14.1019894892023,
132.457105233325)) ;
#129502 = CARTESIAN_POINT('Ctrl Pts',(-19.6004579577044,14.3273312033298,
132.252294538842)) ;
#129503 = CARTESIAN_POINT('Ctrl Pts',(-19.5244720497105,14.4893435077641,
131.997198017204)) ;
#129504 = CARTESIAN_POINT('Ctrl Pts',(-19.437681105912,14.5749599942803,131.710560595662)) ;
#129505 = CARTESIAN_POINT('Ctrl Pts',(-19.3466336963598,14.5779281388509,
131.411346196059)) ;
#129506 = CARTESIAN_POINT('Ctrl Pts',(-19.2595748253476,14.498336569716,131.124014432636)) ;
#129507 = CARTESIAN_POINT('Ctrl Pts',(-19.1825234436999,14.3420896850988,
130.865828840705)) ;
#129508 = CARTESIAN_POINT('Ctrl Pts',(-19.1217474070917,14.1180212398974,
130.65495238919)) ;
#129509 = CARTESIAN_POINT('Ctrl Pts',(-19.0832131949706,13.8471809568527,
130.509458949016)) ;
#129510 = CARTESIAN_POINT('Ctrl Pts',(-19.0694761171171,13.5439414016218,
130.436135704644)) ;
#129511 = CARTESIAN_POINT('Ctrl Pts',(-19.0826209143411,13.2331635587154,
130.441478853736)) ;
#129512 = CARTESIAN_POINT('Ctrl Pts',(-19.1225909328652,12.9343809245396,
130.524995993454)) ;
#129513 = CARTESIAN_POINT('Ctrl Pts',(-19.1868549465641,12.6721978750302,
130.679668772817)) ;
#129514 = CARTESIAN_POINT('Ctrl Pts',(-19.2718327033345,12.4632419957696,
130.894780682372)) ;
#129515 = CARTESIAN_POINT('Ctrl Pts',(-19.3718814394105,12.3231158873288,
131.15398475223)) ;
#129516 = CARTESIAN_POINT('Ctrl Pts',(-19.4814339775529,12.2616017925994,
131.440740961046)) ;
#129517 = CARTESIAN_POINT('Ctrl Pts',(-19.5915908616456,12.2833201710628,
131.729606330629)) ;
#129518 = CARTESIAN_POINT('Ctrl Pts',(-19.6972964626275,12.3868877150975,
132.005156858411)) ;
#129519 = CARTESIAN_POINT('Ctrl Pts',(-19.7903372888288,12.5648231149356,
132.243814036882)) ;
#129520 = CARTESIAN_POINT('Ctrl Pts',(-19.8650354915899,12.8039601972563,
132.428918682179)) ;
#129521 = CARTESIAN_POINT('Ctrl Pts',(-19.9168574250491,13.0864728883471,
132.547293299101)) ;
#129522 = CARTESIAN_POINT('Ctrl Pts',(-19.9430599792711,13.395723837035,132.590534558758)) ;
#129523 = CARTESIAN_POINT('Ctrl Pts',(-19.9420838172202,13.7038340403903,
132.554720244707)) ;
#129524 = CARTESIAN_POINT('Ctrl Pts',(-19.9150775602916,13.9936201443638,
132.442686741954)) ;
#129525 = CARTESIAN_POINT('Ctrl Pts',(-19.8641327250296,14.2431366577781,
132.26059214858)) ;
#129526 = CARTESIAN_POINT('Ctrl Pts',(-19.7947524623111,14.4318623943572,
132.025001777215)) ;
#129527 = CARTESIAN_POINT('Ctrl Pts',(-19.7110993425975,14.5502397442867,
131.747339740325)) ;
#129528 = CARTESIAN_POINT('Ctrl Pts',(-19.6210900248515,14.5868194741509,
131.45129107148)) ;
#129529 = CARTESIAN_POINT('Ctrl Pts',(-19.5315525619792,14.5403267808585,
131.156626982103)) ;
#129530 = CARTESIAN_POINT('Ctrl Pts',(-19.449546684465,14.4138414992085,130.883957172776)) ;
#129531 = CARTESIAN_POINT('Ctrl Pts',(-19.3816932266418,14.2163547115684,
130.65261934202)) ;
#129532 = CARTESIAN_POINT('Ctrl Pts',(-19.3336313323173,13.9624648084783,
130.479143370895)) ;
#129533 = CARTESIAN_POINT('Ctrl Pts',(-19.3093924490461,13.6693367941651,
130.375182192518)) ;
#129534 = CARTESIAN_POINT('Ctrl Pts',(-19.3116017990212,13.3586798877786,
130.34850063673)) ;
#129535 = CARTESIAN_POINT('Ctrl Pts',(-19.3407729872782,13.0526930051948,
130.400586269807)) ;
#129536 = CARTESIAN_POINT('Ctrl Pts',(-19.3955780422064,12.7731728607976,
130.527545202649)) ;
#129537 = CARTESIAN_POINT('Ctrl Pts',(-19.4727496969172,12.5404162495143,
130.719864313944)) ;
#129538 = CARTESIAN_POINT('Ctrl Pts',(-19.5675241391113,12.3707608334166,
130.963600443702)) ;
#129539 = CARTESIAN_POINT('Ctrl Pts',(-19.6739461692788,12.2766729754023,
131.241329946705)) ;
#129540 = CARTESIAN_POINT('Ctrl Pts',(-19.7844202480155,12.2643218379507,
131.531079921362)) ;
#129541 = CARTESIAN_POINT('Ctrl Pts',(-19.8937077378551,12.3360206173623,
131.816927019485)) ;
#129542 = CARTESIAN_POINT('Ctrl Pts',(-19.9915672517583,12.4836396452835,
132.069982162294)) ;
#129543 = CARTESIAN_POINT('Ctrl Pts',(-20.0748105489094,12.7003318361734,
132.279890008997)) ;
#129544 = CARTESIAN_POINT('Ctrl Pts',(-20.1363655459467,12.9678916740203,
132.426631430434)) ;
#129545 = CARTESIAN_POINT('Ctrl Pts',(-20.1732514845702,13.2687868226262,
132.501204712146)) ;
#129546 = CARTESIAN_POINT('Ctrl Pts',(-20.1832535485897,13.5800033962545,
132.497330904926)) ;
#129547 = CARTESIAN_POINT('Ctrl Pts',(-20.1665976689407,13.8799728738773,
132.415585091986)) ;
#129548 = CARTESIAN_POINT('Ctrl Pts',(-20.1250490907357,14.1476993247652,
132.261063926315)) ;
#129549 = CARTESIAN_POINT('Ctrl Pts',(-20.0624312334712,14.3632524005006,
132.045033139331)) ;
#129550 = CARTESIAN_POINT('Ctrl Pts',(-19.9836617187187,14.5119335521308,
131.781720626237)) ;
#129551 = CARTESIAN_POINT('Ctrl Pts',(-19.8953363000053,14.5819602078055,
131.490511990821)) ;
#129552 = CARTESIAN_POINT('Ctrl Pts',(-19.8051206025169,14.5692454474693,
131.19400539406)) ;
#129553 = CARTESIAN_POINT('Ctrl Pts',(-19.7189975522154,14.4742855004693,
130.909223014787)) ;
#129554 = CARTESIAN_POINT('Ctrl Pts',(-19.6448612455928,14.3047439678629,
130.659636036259)) ;
#129555 = CARTESIAN_POINT('Ctrl Pts',(-19.5879650946849,14.0710831645145,
130.460223445624)) ;
#129556 = CARTESIAN_POINT('Ctrl Pts',(-19.5536759796393,13.7914036967699,
130.326934250486)) ;
#129557 = CARTESIAN_POINT('Ctrl Pts',(-19.5450263082221,13.4850123615767,
130.268502128271)) ;
#129558 = CARTESIAN_POINT('Ctrl Pts',(-19.5632218429817,13.1755844342699,
130.28864920662)) ;
#129559 = CARTESIAN_POINT('Ctrl Pts',(-19.6079242224571,12.8823157939158,
130.386049430084)) ;
#129560 = CARTESIAN_POINT('Ctrl Pts',(-19.6763866082576,12.6284363118315,
130.552956035433)) ;
#129561 = CARTESIAN_POINT('Ctrl Pts',(-19.7652804875288,12.430459524885,130.779306976383)) ;
#129562 = CARTESIAN_POINT('Ctrl Pts',(-19.8670137067598,12.3053999545834,
131.043605735168)) ;
#129563 = CARTESIAN_POINT('Ctrl Pts',(-19.9776324212504,12.259348439198,131.333414105612)) ;
#129564 = CARTESIAN_POINT('Ctrl Pts',(-20.0871279899776,12.2965483927982,
131.620409141885)) ;
#129565 = CARTESIAN_POINT('Ctrl Pts',(-20.1914568507578,12.4156949329505,
131.891780020066)) ;
#129566 = CARTESIAN_POINT('Ctrl Pts',(-20.280854617759,12.6050470822163,132.120029243764)) ;
#129567 = CARTESIAN_POINT('Ctrl Pts',(-20.3519885949918,12.8553420961893,
132.294524748666)) ;
#129568 = CARTESIAN_POINT('Ctrl Pts',(-20.3988624504608,13.1429454488516,
132.398581522686)) ;
#129569 = CARTESIAN_POINT('Ctrl Pts',(-20.4200768369222,13.454391681807,132.427234220689)) ;
#129570 = CARTESIAN_POINT('Ctrl Pts',(-20.4140136595561,13.7614619706277,
132.376445903007)) ;
#129571 = CARTESIAN_POINT('Ctrl Pts',(-20.382192794584,14.0447127899292,132.250363159201)) ;
#129572 = CARTESIAN_POINT('Ctrl Pts',(-20.327675093214,14.2828872647388,132.058058028165)) ;
#129573 = CARTESIAN_POINT('Ctrl Pts',(-20.2549076280567,14.4603132079677,
131.812365927047)) ;
#129574 = CARTESIAN_POINT('Ctrl Pts',(-20.1693733796987,14.5634617296136,
131.529204042072)) ;
#129575 = CARTESIAN_POINT('Ctrl Pts',(-20.0794263338298,14.5844329944993,
131.233527995781)) ;
#129576 = CARTESIAN_POINT('Ctrl Pts',(-19.9904362428095,14.5225343745256,
130.94034258586)) ;
#129577 = CARTESIAN_POINT('Ctrl Pts',(-19.910574928501,14.3815448921276,130.673908872332)) ;
#129578 = CARTESIAN_POINT('Ctrl Pts',(-19.8461411447143,14.1725755942996,
130.452618521442)) ;
#129579 = CARTESIAN_POINT('Ctrl Pts',(-19.8022333693109,13.9093042080622,
130.291199800478)) ;
#129580 = CARTESIAN_POINT('Ctrl Pts',(-19.7828574602038,13.6121560169538,
130.201553405444)) ;
#129581 = CARTESIAN_POINT('Ctrl Pts',(-19.7902297852299,13.2990172973707,
130.189775599945)) ;
#129582 = CARTESIAN_POINT('Ctrl Pts',(-19.8242499060709,12.9981567008458,
130.256216408043)) ;
#129583 = CARTESIAN_POINT('Ctrl Pts',(-19.8834591196413,12.7257034100229,
130.396033289139)) ;
#129584 = CARTESIAN_POINT('Ctrl Pts',(-19.9646135502491,12.503075938083,130.599887232167)) ;
#129585 = CARTESIAN_POINT('Ctrl Pts',(-20.061806489816,12.3471530516957,130.850770434248)) ;
#129586 = CARTESIAN_POINT('Ctrl Pts',(-20.1701165293733,12.2678408813101,
131.133870309601)) ;
#129587 = CARTESIAN_POINT('Ctrl Pts',(-20.2803843836627,12.2715868988579,
131.423098040257)) ;
#129588 = CARTESIAN_POINT('Ctrl Pts',(-20.3877234956396,12.3575775425478,
131.703470304113)) ;
#129589 = CARTESIAN_POINT('Ctrl Pts',(-20.4838861019967,12.519859116392,131.95129175679)) ;
#129590 = CARTESIAN_POINT('Ctrl Pts',(-20.563259553875,12.7472699624983,132.149979635772)) ;
#129591 = CARTESIAN_POINT('Ctrl Pts',(-20.6205129961937,13.0233713370029,
132.284051353102)) ;
#129592 = CARTESIAN_POINT('Ctrl Pts',(-20.652239731686,13.3264774087469,132.343728948937)) ;
#129593 = CARTESIAN_POINT('Ctrl Pts',(-20.6572910380726,13.6374828083211,
132.325371821783)) ;
#129594 = CARTESIAN_POINT('Ctrl Pts',(-20.6356455845063,13.9340521911672,
132.228917738845)) ;
#129595 = CARTESIAN_POINT('Ctrl Pts',(-20.589784029738,14.193123894667,132.061824915611)) ;
#129596 = CARTESIAN_POINT('Ctrl Pts',(-20.5234609844462,14.3974304405376,
131.83486651278)) ;
#129597 = CARTESIAN_POINT('Ctrl Pts',(-20.4428898145144,14.5309245304013,
131.566514750519)) ;
#129598 = CARTESIAN_POINT('Ctrl Pts',(-20.3537343109642,14.5859814529116,
131.272940165148)) ;
#129599 = CARTESIAN_POINT('Ctrl Pts',(-20.2633620898879,14.5574777921035,
130.975793218994)) ;
#129600 = CARTESIAN_POINT('Ctrl Pts',(-20.179134864296,14.4480150679812,130.696649838046)) ;
#129601 = CARTESIAN_POINT('Ctrl Pts',(-20.1074565079211,14.2640747016683,
130.454011423191)) ;
#129602 = CARTESIAN_POINT('Ctrl Pts',(-20.0549222211513,14.0222278748094,
130.267625814599)) ;
#129603 = CARTESIAN_POINT('Ctrl Pts',(-20.0250364103788,13.7339092268223,
130.146949963196)) ;
#129604 = CARTESIAN_POINT('Ctrl Pts',(-20.0215334625323,13.4264443315917,
130.103724396133)) ;
#129605 = CARTESIAN_POINT('Ctrl Pts',(-20.0448205353659,13.117933729061,130.138658618017)) ;
#129606 = CARTESIAN_POINT('Ctrl Pts',(-20.0942215492142,12.8308236543942,
130.249839143416)) ;
#129607 = CARTESIAN_POINT('Ctrl Pts',(-20.1670498129061,12.5859821244952,
130.429403729018)) ;
#129608 = CARTESIAN_POINT('Ctrl Pts',(-20.2580898691565,12.4020104693658,
130.662363596137)) ;
#129609 = CARTESIAN_POINT('Ctrl Pts',(-20.3630369251127,12.2899875702474,
130.935630330481)) ;
#129610 = CARTESIAN_POINT('Ctrl Pts',(-20.4732695786483,12.2601247777389,
131.224628401923)) ;
#129611 = CARTESIAN_POINT('Ctrl Pts',(-20.5827915134349,12.3130228920766,
131.511459590319)) ;
#129612 = CARTESIAN_POINT('Ctrl Pts',(-20.6842801965026,12.4457555265159,
131.774790797317)) ;
#129613 = CARTESIAN_POINT('Ctrl Pts',(-20.770956455244,12.6478748445304,131.994929810398)) ;
#129614 = CARTESIAN_POINT('Ctrl Pts',(-20.8379046355006,12.90742344953,132.157201250892)) ;
#129615 = CARTESIAN_POINT('Ctrl Pts',(-20.8801243826187,13.2015878623563,
132.247531865277)) ;
#129616 = CARTESIAN_POINT('Ctrl Pts',(-20.8960762410322,13.513246132059,132.260932671934)) ;
#129617 = CARTESIAN_POINT('Ctrl Pts',(-20.8850515631884,13.8170403560637,
132.195686938087)) ;
#129618 = CARTESIAN_POINT('Ctrl Pts',(-20.8487392341801,14.0930903285622,
132.056526224254)) ;
#129619 = CARTESIAN_POINT('Ctrl Pts',(-20.7903126425234,14.3215764376153,
131.852723944522)) ;
#129620 = CARTESIAN_POINT('Ctrl Pts',(-20.71446322452,14.4860163871687,131.59792677398)) ;
#129621 = CARTESIAN_POINT('Ctrl Pts',(-20.6277873026751,14.5737421831593,
131.31159505661)) ;
#129622 = CARTESIAN_POINT('Ctrl Pts',(-20.5369992850468,14.5789283519424,
131.013226876598)) ;
#129623 = CARTESIAN_POINT('Ctrl Pts',(-20.4496947481666,14.5018180781457,
130.725170263346)) ;
#129624 = CARTESIAN_POINT('Ctrl Pts',(-20.3720331642646,14.3465572138388,
130.465061663831)) ;
#129625 = CARTESIAN_POINT('Ctrl Pts',(-20.3113537180096,14.1268975859946,
130.254856603659)) ;
#129626 = CARTESIAN_POINT('Ctrl Pts',(-20.2716879247288,13.8551173333083,
130.105766414134)) ;
#129627 = CARTESIAN_POINT('Ctrl Pts',(-20.2572946011384,13.5530514979448,
130.030607450358)) ;
#129628 = CARTESIAN_POINT('Ctrl Pts',(-20.2696946884832,13.2415865700778,
130.033701144829)) ;
#129629 = CARTESIAN_POINT('Ctrl Pts',(-20.3087706449792,12.9431698181064,
130.114729825383)) ;
#129630 = CARTESIAN_POINT('Ctrl Pts',(-20.372493414144,12.6789857022783,130.267737292984)) ;
#129631 = CARTESIAN_POINT('Ctrl Pts',(-20.4568543797459,12.4685394355876,
130.481090280765)) ;
#129632 = CARTESIAN_POINT('Ctrl Pts',(-20.5565334718935,12.3261975065515,
130.739212503641)) ;
#129633 = CARTESIAN_POINT('Ctrl Pts',(-20.6658499559575,12.2622045944374,
131.025302791094)) ;
#129634 = CARTESIAN_POINT('Ctrl Pts',(-20.7762684309206,12.2815898104216,
131.314866496193)) ;
#129635 = CARTESIAN_POINT('Ctrl Pts',(-20.8819109420116,12.3824517320663,
131.590340001243)) ;
#129636 = CARTESIAN_POINT('Ctrl Pts',(-20.9755580922554,12.5585396445524,
131.830713394656)) ;
#129637 = CARTESIAN_POINT('Ctrl Pts',(-21.05082616022,12.7954954473237,132.017545647161)) ;
#129638 = CARTESIAN_POINT('Ctrl Pts',(-21.1037227225579,13.0796939722615,
132.13875377845)) ;
#129639 = CARTESIAN_POINT('Ctrl Pts',(-21.1303775268751,13.3852304092896,
132.18368355125)) ;
#129640 = CARTESIAN_POINT('Ctrl Pts',(-21.1302868768095,13.6960444391784,
132.150191483003)) ;
#129641 = CARTESIAN_POINT('Ctrl Pts',(-21.103907238212,13.9858667251667,132.040067449433)) ;
#129642 = CARTESIAN_POINT('Ctrl Pts',(-21.0539056725473,14.2358877354541,
131.860875963079)) ;
#129643 = CARTESIAN_POINT('Ctrl Pts',(-20.9847199038895,14.427599936546,131.625699111867)) ;
#129644 = CARTESIAN_POINT('Ctrl Pts',(-20.9012106052768,14.5480862875162,
131.348413046553)) ;
#129645 = CARTESIAN_POINT('Ctrl Pts',(-20.8116067569838,14.5868446714445,
131.053662003123)) ;
#129646 = CARTESIAN_POINT('Ctrl Pts',(-20.722052724287,14.543035766912,130.758989112208)) ;
#129647 = CARTESIAN_POINT('Ctrl Pts',(-20.6396161469712,14.4187440233768,
130.485021247634)) ;
#129648 = CARTESIAN_POINT('Ctrl Pts',(-20.5711851083752,14.2230681699305,
130.251972524178)) ;
#129649 = CARTESIAN_POINT('Ctrl Pts',(-20.5224081144402,13.9697197802327,
130.076309410298)) ;
#129650 = CARTESIAN_POINT('Ctrl Pts',(-20.4975411592122,13.678752384422,129.970666296557)) ;
#129651 = CARTESIAN_POINT('Ctrl Pts',(-20.49894769684,13.3668523493994,129.941483136126)) ;
#129652 = CARTESIAN_POINT('Ctrl Pts',(-20.5274636510951,13.0606725524935,
129.991675831064)) ;
#129653 = CARTESIAN_POINT('Ctrl Pts',(-20.5813628220163,12.7810811870564,
130.116105508458)) ;
#129654 = CARTESIAN_POINT('Ctrl Pts',(-20.6578955627211,12.5467078049701,
130.306564715947)) ;
#129655 = CARTESIAN_POINT('Ctrl Pts',(-20.7520317982675,12.3750360916392,
130.548492029394)) ;
#129656 = CARTESIAN_POINT('Ctrl Pts',(-20.8588402085985,12.2779852659618,
130.827153760842)) ;
#129657 = CARTESIAN_POINT('Ctrl Pts',(-20.9691322717098,12.2637459415924,
131.1164165131)) ;
#129658 = CARTESIAN_POINT('Ctrl Pts',(-21.0778822448708,12.3321871278704,
131.400920874685)) ;
#129659 = CARTESIAN_POINT('Ctrl Pts',(-21.1769911008549,12.4786899197398,
131.657345754661)) ;
#129660 = CARTESIAN_POINT('Ctrl Pts',(-21.2606987378686,12.6941597985184,
131.86859423361)) ;
#129661 = CARTESIAN_POINT('Ctrl Pts',(-21.3226675980762,12.95948963943,132.016669195354)) ;
#129662 = CARTESIAN_POINT('Ctrl Pts',(-21.3603388309651,13.2597800757016,
132.09352869614)) ;
#129663 = CARTESIAN_POINT('Ctrl Pts',(-21.3711243868775,13.570593176475,132.091985203962)) ;
#129664 = CARTESIAN_POINT('Ctrl Pts',(-21.3552655780944,13.8717553022586,
132.01251606465)) ;
#129665 = CARTESIAN_POINT('Ctrl Pts',(-21.3141032516413,14.1416795276356,
131.858976575639)) ;
#129666 = CARTESIAN_POINT('Ctrl Pts',(-21.2523927513415,14.3575207602719,
131.645808023395)) ;
#129667 = CARTESIAN_POINT('Ctrl Pts',(-21.1737881611546,14.5088742129947,
131.382873338965)) ;
#129668 = CARTESIAN_POINT('Ctrl Pts',(-21.0858332477586,14.5810485747374,
131.092827440589)) ;
#129669 = CARTESIAN_POINT('Ctrl Pts',(-20.9954536594014,14.5707018423974,
130.79578508898)) ;
#129670 = CARTESIAN_POINT('Ctrl Pts',(-20.9093467237376,14.4785663086567,
130.511161766983)) ;
#129671 = CARTESIAN_POINT('Ctrl Pts',(-20.8341838994325,14.3096046901172,
130.258300710511)) ;
#129672 = CARTESIAN_POINT('Ctrl Pts',(-20.7769970988678,14.0777450848623,
130.058128817237)) ;
#129673 = CARTESIAN_POINT('Ctrl Pts',(-20.7421466915136,13.8001342656759,
129.923313470881)) ;
#129674 = CARTESIAN_POINT('Ctrl Pts',(-20.732652270712,13.4946153798022,129.862456562529)) ;
#129675 = CARTESIAN_POINT('Ctrl Pts',(-20.7501719019214,13.1837407483122,
129.880489260335)) ;
#129676 = CARTESIAN_POINT('Ctrl Pts',(-20.7940652768132,12.8901082923596,
129.975587652555)) ;
#129677 = CARTESIAN_POINT('Ctrl Pts',(-20.8623834981418,12.6339161097821,
130.141896445246)) ;
#129678 = CARTESIAN_POINT('Ctrl Pts',(-20.9494844728681,12.43659258656,130.363483556097)) ;
#129679 = CARTESIAN_POINT('Ctrl Pts',(-21.0520547764074,12.3075969650438,
130.629826825371)) ;
#129680 = CARTESIAN_POINT('Ctrl Pts',(-21.1615735908753,12.25954136932,130.916733851634)) ;
#129681 = CARTESIAN_POINT('Ctrl Pts',(-21.2721798049417,12.2945981234014,
131.206652794523)) ;
#129682 = CARTESIAN_POINT('Ctrl Pts',(-21.3757162896064,12.4101972587338,
131.476072258358)) ;
#129683 = CARTESIAN_POINT('Ctrl Pts',(-21.4663327145782,12.5987159490307,
131.707623163194)) ;
#129684 = CARTESIAN_POINT('Ctrl Pts',(-21.5377865787159,12.8461743758197,
131.883234522718)) ;
#129685 = CARTESIAN_POINT('Ctrl Pts',(-21.5858655490026,13.135926237231,131.990455824353)) ;
#129686 = CARTESIAN_POINT('Ctrl Pts',(-21.607580328873,13.4447581443412,132.020835164362)) ;
#129687 = CARTESIAN_POINT('Ctrl Pts',(-21.602335125879,13.7530929006016,131.972334348118)) ;
#129688 = CARTESIAN_POINT('Ctrl Pts',(-21.5713569064062,14.0362080227333,
131.84885121752)) ;
#129689 = CARTESIAN_POINT('Ctrl Pts',(-21.5173330548251,14.2769559751065,
131.657874005784)) ;
#129690 = CARTESIAN_POINT('Ctrl Pts',(-21.4448194217764,14.4563581668246,
131.412866120982)) ;
#129691 = CARTESIAN_POINT('Ctrl Pts',(-21.3601256689141,14.5613193380967,
131.132376374339)) ;
#129692 = CARTESIAN_POINT('Ctrl Pts',(-21.269633652782,14.5851466782009,130.834886668731)) ;
#129693 = CARTESIAN_POINT('Ctrl Pts',(-21.1804456514604,14.5250094575114,
130.541092527295)) ;
#129694 = CARTESIAN_POINT('Ctrl Pts',(-21.1006537832372,14.3871119607425,
130.275049733062)) ;
#129695 = CARTESIAN_POINT('Ctrl Pts',(-21.0353501151795,14.1786614290351,
130.051020270923)) ;
#129696 = CARTESIAN_POINT('Ctrl Pts',(-20.9910103803622,13.9181922877867,
129.888536140965)) ;
#129697 = CARTESIAN_POINT('Ctrl Pts',(-20.9707895546845,13.6189924395308,
129.796111778833)) ;
#129698 = CARTESIAN_POINT('Ctrl Pts',(-20.9774051303695,13.3089362850498,
129.782452006343)) ;
#129699 = CARTESIAN_POINT('Ctrl Pts',(-21.0107344731984,13.0058326835249,
129.846693977316)) ;
#129700 = CARTESIAN_POINT('Ctrl Pts',(-21.069523134724,12.7318653591864,129.985217546622)) ;
#129701 = CARTESIAN_POINT('Ctrl Pts',(-21.150025441934,12.5082427552374,130.1872332646)) ;
#129702 = CARTESIAN_POINT('Ctrl Pts',(-21.2465051340931,12.3508733005898,
130.436144552975)) ;
#129703 = CARTESIAN_POINT('Ctrl Pts',(-21.3542476171135,12.269103663372,130.717689338765)) ;
#129704 = CARTESIAN_POINT('Ctrl Pts',(-21.4650677342557,12.2702137118359,
131.008368653473)) ;
#129705 = CARTESIAN_POINT('Ctrl Pts',(-21.5727573438248,12.3542929443511,
131.289715826593)) ;
#129706 = CARTESIAN_POINT('Ctrl Pts',(-21.669031736396,12.5141175803543,131.537958518578)) ;
#129707 = CARTESIAN_POINT('Ctrl Pts',(-21.7489177217398,12.7395233280602,
131.738178017608)) ;
#129708 = CARTESIAN_POINT('Ctrl Pts',(-21.8069012464984,13.0142278391015,
131.87440155685)) ;
#129709 = CARTESIAN_POINT('Ctrl Pts',(-21.8395149250998,13.3177661715459,
131.936564544412)) ;
#129710 = CARTESIAN_POINT('Ctrl Pts',(-21.8452824715449,13.6286636556953,
131.920321738813)) ;
#129711 = CARTESIAN_POINT('Ctrl Pts',(-21.8244882197182,13.925291797829,131.826438201563)) ;
#129712 = CARTESIAN_POINT('Ctrl Pts',(-21.7792414631911,14.1860949206715,
131.661093526473)) ;
#129713 = CARTESIAN_POINT('Ctrl Pts',(-21.7137062627427,14.3917323897328,
131.436549030154)) ;
#129714 = CARTESIAN_POINT('Ctrl Pts',(-21.633156096691,14.5282787292637,131.168110047203)) ;
#129715 = CARTESIAN_POINT('Ctrl Pts',(-21.5439567054312,14.5855538686264,
130.874346913366)) ;
#129716 = CARTESIAN_POINT('Ctrl Pts',(-21.4537797537119,14.5594424276329,
130.57786442623)) ;
#129717 = CARTESIAN_POINT('Ctrl Pts',(-21.3693530406536,14.4525338463175,
130.298172317477)) ;
#129718 = CARTESIAN_POINT('Ctrl Pts',(-21.297068085247,14.2704302035547,130.053714472127)) ;
#129719 = CARTESIAN_POINT('Ctrl Pts',(-21.2438867525861,14.0294404893197,
129.865368122404)) ;
#129720 = CARTESIAN_POINT('Ctrl Pts',(-21.2134075430614,13.7439522566763,
129.743168596482)) ;
#129721 = CARTESIAN_POINT('Ctrl Pts',(-21.2090247258927,13.4354033012877,
129.697210582902)) ;
#129722 = CARTESIAN_POINT('Ctrl Pts',(-21.231516856981,13.1268757860435,129.729861443556)) ;
#129723 = CARTESIAN_POINT('Ctrl Pts',(-21.2803840223732,12.8380942311381,
129.839381945022)) ;
#129724 = CARTESIAN_POINT('Ctrl Pts',(-21.3521470268813,12.593020734814,130.016027287416)) ;
#129725 = CARTESIAN_POINT('Ctrl Pts',(-21.4432776558791,12.406038864334,130.249044156356)) ;
#129726 = CARTESIAN_POINT('Ctrl Pts',(-21.5470627584207,12.2925312393263,
130.519197721252)) ;
#129727 = CARTESIAN_POINT('Ctrl Pts',(-21.6581297703892,12.2597001756507,
130.810350160136)) ;
#129728 = CARTESIAN_POINT('Ctrl Pts',(-21.7675384937541,12.3104428480306,
131.096926129953)) ;
#129729 = CARTESIAN_POINT('Ctrl Pts',(-21.8694603895899,12.4411375343228,
131.361483890895)) ;
#129730 = CARTESIAN_POINT('Ctrl Pts',(-21.9564206697515,12.6410412260459,
131.582529425716)) ;
#129731 = CARTESIAN_POINT('Ctrl Pts',(-22.0240617398326,12.8990709412412,
131.746830040607)) ;
#129732 = CARTESIAN_POINT('Ctrl Pts',(-22.0670949130516,13.1932158422951,
131.839455119408)) ;
#129733 = CARTESIAN_POINT('Ctrl Pts',(-22.083767292589,13.5039483153196,131.855045190033)) ;
#129734 = CARTESIAN_POINT('Ctrl Pts',(-22.073536721884,13.8084629331276,131.792095553188)) ;
#129735 = CARTESIAN_POINT('Ctrl Pts',(-22.0379189931258,14.0856214522983,
131.654965961301)) ;
#129736 = CARTESIAN_POINT('Ctrl Pts',(-21.9800713891494,14.3156973723363,
131.452856515095)) ;
#129737 = CARTESIAN_POINT('Ctrl Pts',(-21.9047961256862,14.4820692516826,
131.199796234368)) ;
#129738 = CARTESIAN_POINT('Ctrl Pts',(-21.8181774390092,14.5722583226928,
130.913562740899)) ;
#129739 = CARTESIAN_POINT('Ctrl Pts',(-21.7278611027354,14.5801737014987,
130.616744267121)) ;
#129740 = CARTESIAN_POINT('Ctrl Pts',(-21.6397157180103,14.5050114292979,
130.325985083812)) ;
#129741 = CARTESIAN_POINT('Ctrl Pts',(-21.5619498046495,14.3522166044366,
130.065688507051)) ;
#129742 = CARTESIAN_POINT('Ctrl Pts',(-21.5006045705158,14.1339604328417,
129.853478179641)) ;
#129743 = CARTESIAN_POINT('Ctrl Pts',(-21.4603340437159,13.8641114718027,
129.702710340301)) ;
#129744 = CARTESIAN_POINT('Ctrl Pts',(-21.4451043217958,13.5616227135085,
129.624990432218)) ;
#129745 = CARTESIAN_POINT('Ctrl Pts',(-21.4567589247854,13.2502936297686,
129.625929497814)) ;
#129746 = CARTESIAN_POINT('Ctrl Pts',(-21.4951599834877,12.9509784394827,
129.704955381254)) ;
#129747 = CARTESIAN_POINT('Ctrl Pts',(-21.5580080093365,12.6863950306147,
129.855517297843)) ;
#129748 = CARTESIAN_POINT('Ctrl Pts',(-21.6420011592254,12.4734607184327,
130.067712328711)) ;
#129749 = CARTESIAN_POINT('Ctrl Pts',(-21.7417791407559,12.3287824290801,
130.325991712342)) ;
#129750 = CARTESIAN_POINT('Ctrl Pts',(-21.8504049263474,12.2629634188969,
130.610230387682)) ;
#129751 = CARTESIAN_POINT('Ctrl Pts',(-21.9610518581756,12.2798963089147,
130.900404347138)) ;
#129752 = CARTESIAN_POINT('Ctrl Pts',(-22.0669959746994,12.3786943596861,
131.176740574865)) ;
#129753 = CARTESIAN_POINT('Ctrl Pts',(-22.1611710364992,12.5532636786749,
131.418606895266)) ;
#129754 = CARTESIAN_POINT('Ctrl Pts',(-22.2366635856223,12.7879391419199,
131.606219865345)) ;
#129755 = CARTESIAN_POINT('Ctrl Pts',(-22.290142211429,13.0695370930121,131.729290328247)) ;
#129756 = CARTESIAN_POINT('Ctrl Pts',(-22.3178130052509,13.3764286772832,
131.776992915573)) ;
#129757 = CARTESIAN_POINT('Ctrl Pts',(-22.318427864876,13.6873693589622,131.745572982122)) ;
#129758 = CARTESIAN_POINT('Ctrl Pts',(-22.292826577029,13.9780097335569,131.637733892545)) ;
#129759 = CARTESIAN_POINT('Ctrl Pts',(-22.2431790354703,14.2303816852456,
131.459436217296)) ;
#129760 = CARTESIAN_POINT('Ctrl Pts',(-22.1746653892291,14.4229832269157,
131.226347148492)) ;
#129761 = CARTESIAN_POINT('Ctrl Pts',(-22.0916752545479,14.5456071990929,
130.950650854282)) ;
#129762 = CARTESIAN_POINT('Ctrl Pts',(-22.0020115166837,14.5869244372619,
130.655664977446)) ;
#129763 = CARTESIAN_POINT('Ctrl Pts',(-21.9122878651958,14.545413997822,130.360474615968)) ;
#129764 = CARTESIAN_POINT('Ctrl Pts',(-21.8295294436028,14.4231615321001,
130.085553182396)) ;
#129765 = CARTESIAN_POINT('Ctrl Pts',(-21.7608250583823,14.2299646068936,
129.85180667101)) ;
#129766 = CARTESIAN_POINT('Ctrl Pts',(-21.7113239372725,13.9782380541428,
129.674030463916)) ;
#129767 = CARTESIAN_POINT('Ctrl Pts',(-21.6856792409941,13.6869897055948,
129.565991871631)) ;
#129768 = CARTESIAN_POINT('Ctrl Pts',(-21.6862854845015,13.3772462796711,
129.534677574901)) ;
#129769 = CARTESIAN_POINT('Ctrl Pts',(-21.7138953989796,13.0701027009942,
129.582174987858)) ;
#129770 = CARTESIAN_POINT('Ctrl Pts',(-21.7673001378337,12.7883758458207,
129.705033082138)) ;
#129771 = CARTESIAN_POINT('Ctrl Pts',(-21.8432513830499,12.5524788761833,
129.893799085058)) ;
#129772 = CARTESIAN_POINT('Ctrl Pts',(-21.9371566394696,12.3787206471269,
130.134993378243)) ;
#129773 = CARTESIAN_POINT('Ctrl Pts',(-22.0430755659619,12.2799428632339,
130.41125725332)) ;
#129774 = CARTESIAN_POINT('Ctrl Pts',(-22.1535702808427,12.262781436098,130.701037365043)) ;
#129775 = CARTESIAN_POINT('Ctrl Pts',(-22.2630782526847,12.3295043869385,
130.987573569498)) ;
#129776 = CARTESIAN_POINT('Ctrl Pts',(-22.362016039896,12.473510372606,131.243655905125)) ;
#129777 = CARTESIAN_POINT('Ctrl Pts',(-22.4459844694034,12.6859034724392,
131.455815775636)) ;
#129778 = CARTESIAN_POINT('Ctrl Pts',(-22.5090028960007,12.9511126916242,
131.606796748372)) ;
#129779 = CARTESIAN_POINT('Ctrl Pts',(-22.54743070579,13.2510040815984,131.685842769885)) ;
#129780 = CARTESIAN_POINT('Ctrl Pts',(-22.558981890815,13.5624346911567,131.686468142538)) ;
#129781 = CARTESIAN_POINT('Ctrl Pts',(-22.5438100294484,13.863434989198,131.609077935155)) ;
#129782 = CARTESIAN_POINT('Ctrl Pts',(-22.5036818951076,14.1332612598468,
131.45875046159)) ;
#129783 = CARTESIAN_POINT('Ctrl Pts',(-22.4420921893319,14.3526408923895,
131.245680127562)) ;
#129784 = CARTESIAN_POINT('Ctrl Pts',(-22.3640058771557,14.5054039149979,
130.984345418318)) ;
#129785 = CARTESIAN_POINT('Ctrl Pts',(-22.2766140050104,14.5799567514586,
130.696072024306)) ;
#129786 = CARTESIAN_POINT('Ctrl Pts',(-22.1858591503502,14.5723714395277,
130.397811110958)) ;
#129787 = CARTESIAN_POINT('Ctrl Pts',(-22.0992395687441,14.4818104958985,
130.111564075611)) ;
#129788 = CARTESIAN_POINT('Ctrl Pts',(-22.024274176973,14.3163443663444,129.859558431675)) ;
#129789 = CARTESIAN_POINT('Ctrl Pts',(-21.9662417141904,14.0859121454152,
129.656831575018)) ;
#129790 = CARTESIAN_POINT('Ctrl Pts',(-21.9305828051363,13.8088759018265,
129.519593613112)) ;
#129791 = CARTESIAN_POINT('Ctrl Pts',(-21.9203578742062,13.5028416968273,
129.456494956462)) ;
#129792 = CARTESIAN_POINT('Ctrl Pts',(-21.9370262576808,13.1931031843273,
129.472184440752)) ;
#129793 = CARTESIAN_POINT('Ctrl Pts',(-21.9802902593002,12.89795929161,129.565356630037)) ;
#129794 = CARTESIAN_POINT('Ctrl Pts',(-22.047553588434,12.6415807135438,129.728760415045)) ;
#129795 = CARTESIAN_POINT('Ctrl Pts',(-22.1347436150936,12.4408172344946,
129.950365899039)) ;
#129796 = CARTESIAN_POINT('Ctrl Pts',(-22.2370229130925,12.3100401659206,
130.215871813637)) ;
#129797 = CARTESIAN_POINT('Ctrl Pts',(-22.346187343475,12.2598615754433,130.501810053951)) ;
#129798 = CARTESIAN_POINT('Ctrl Pts',(-22.4566401515678,12.2922205414055,
130.791357288347)) ;
#129799 = CARTESIAN_POINT('Ctrl Pts',(-22.5610110970781,12.4062484922091,
131.063036431062)) ;
#129800 = CARTESIAN_POINT('Ctrl Pts',(-22.6518356473151,12.5927140655513,
131.295269732808)) ;
#129801 = CARTESIAN_POINT('Ctrl Pts',(-22.7237313097823,12.8381489007341,
131.472242088444)) ;
#129802 = CARTESIAN_POINT('Ctrl Pts',(-22.7725207924835,13.1260095421298,
131.581638130057)) ;
#129803 = CARTESIAN_POINT('Ctrl Pts',(-22.7951559321079,13.4367097246031,
131.614472327231)) ;
#129804 = CARTESIAN_POINT('Ctrl Pts',(-22.7906542710234,13.7438376703634,
131.56831388168)) ;
#129805 = CARTESIAN_POINT('Ctrl Pts',(-22.7603725677891,14.0287736404421,
131.44677384493)) ;
#129806 = CARTESIAN_POINT('Ctrl Pts',(-22.7068886331561,14.270962157525,131.257369646946)) ;
#129807 = CARTESIAN_POINT('Ctrl Pts',(-22.6349661679253,14.4520607782582,
131.014146425895)) ;
#129808 = CARTESIAN_POINT('Ctrl Pts',(-22.5504033640329,14.5594794315335,
130.733986591008)) ;
#129809 = CARTESIAN_POINT('Ctrl Pts',(-22.4601541297996,14.5855261775524,
130.437269710365)) ;
#129810 = CARTESIAN_POINT('Ctrl Pts',(-22.3710288767078,14.5283738977508,
130.14375232629)) ;
#129811 = CARTESIAN_POINT('Ctrl Pts',(-22.2903791078735,14.391653675229,129.874980130826)) ;
#129812 = CARTESIAN_POINT('Ctrl Pts',(-22.2249495985923,14.1863633924956,
129.650800118023)) ;
#129813 = CARTESIAN_POINT('Ctrl Pts',(-22.1796679930113,13.9255969369485,
129.48534839629)) ;
#129814 = CARTESIAN_POINT('Ctrl Pts',(-22.1588481354936,13.6292801899933,
129.391421087479)) ;
#129815 = CARTESIAN_POINT('Ctrl Pts',(-22.1645772032321,13.3179690921283,
129.375020864213)) ;
#129816 = CARTESIAN_POINT('Ctrl Pts',(-22.1971947872982,13.0144329999001,
129.437196033629)) ;
#129817 = CARTESIAN_POINT('Ctrl Pts',(-22.2550420413868,12.7401668642732,
129.573078522351)) ;
#129818 = CARTESIAN_POINT('Ctrl Pts',(-22.3348838189612,12.5144107984142,
129.773156275244)) ;
#129819 = CARTESIAN_POINT('Ctrl Pts',(-22.4315850270881,12.3540785091182,
130.022507063406)) ;
#129820 = CARTESIAN_POINT('Ctrl Pts',(-22.5386180179821,12.2704506972946,
130.302139542132)) ;
#129821 = CARTESIAN_POINT('Ctrl Pts',(-22.6497921880934,12.2689820751512,
130.593744024713)) ;
#129822 = CARTESIAN_POINT('Ctrl Pts',(-22.7576074186186,12.3508509067205,
130.875481503016)) ;
#129823 = CARTESIAN_POINT('Ctrl Pts',(-22.8543111531987,12.5086054650755,
131.124969484035)) ;
#129824 = CARTESIAN_POINT('Ctrl Pts',(-22.9349375950158,12.7330676157862,
131.327264167781)) ;
#129825 = CARTESIAN_POINT('Ctrl Pts',(-22.9934475007787,13.0066123030749,
131.465048783301)) ;
#129826 = CARTESIAN_POINT('Ctrl Pts',(-23.0266870652074,13.3082724111724,
131.529183861315)) ;
#129827 = CARTESIAN_POINT('Ctrl Pts',(-23.033311559833,13.6201711563921,131.515348886077)) ;
#129828 = CARTESIAN_POINT('Ctrl Pts',(-23.0130972666971,13.9183339563094,
131.423061499097)) ;
#129829 = CARTESIAN_POINT('Ctrl Pts',(-22.9684886216917,14.1797387152336,
131.259643342506)) ;
#129830 = CARTESIAN_POINT('Ctrl Pts',(-22.9036845336627,14.3864986617501,
131.037342151647)) ;
#129831 = CARTESIAN_POINT('Ctrl Pts',(-22.8235293433254,14.5252641386946,
130.77006712631)) ;
#129832 = CARTESIAN_POINT('Ctrl Pts',(-22.7344573025139,14.5851720998815,
130.476667796814)) ;
#129833 = CARTESIAN_POINT('Ctrl Pts',(-22.6437076364381,14.561066934574,130.178322236931)) ;
#129834 = CARTESIAN_POINT('Ctrl Pts',(-22.5595163505151,14.4566510125324,
129.899496693664)) ;
#129835 = CARTESIAN_POINT('Ctrl Pts',(-22.4868075776867,14.2771545547794,
129.653851802256)) ;
#129836 = CARTESIAN_POINT('Ctrl Pts',(-22.4327702184639,14.0362065593723,
129.462817295921)) ;
#129837 = CARTESIAN_POINT('Ctrl Pts',(-22.4017946730085,13.7533987365905,
129.339371688466)) ;
#129838 = CARTESIAN_POINT('Ctrl Pts',(-22.3965076931407,13.444128366597,129.290651049899)) ;
#129839 = CARTESIAN_POINT('Ctrl Pts',(-22.4184444031792,13.1346408962195,
129.321598554928)) ;
#129840 = CARTESIAN_POINT('Ctrl Pts',(-22.4661569344923,12.8470251691959,
129.427998466394)) ;
#129841 = CARTESIAN_POINT('Ctrl Pts',(-22.5378591493393,12.5984937822196,
129.604197721476)) ;
#129842 = CARTESIAN_POINT('Ctrl Pts',(-22.6280348584897,12.4108688263379,
129.834624782045)) ;
#129843 = CARTESIAN_POINT('Ctrl Pts',(-22.7317416641835,12.2946081111199,
130.104467076645)) ;
#129844 = CARTESIAN_POINT('Ctrl Pts',(-22.8428132954771,12.2594450542174,
130.395612682579)) ;
#129845 = CARTESIAN_POINT('Ctrl Pts',(-22.9524265076277,12.3080481401079,
130.682755174456)) ;
#129846 = CARTESIAN_POINT('Ctrl Pts',(-23.0543320583707,12.4360760785603,
130.9473801658)) ;
#129847 = CARTESIAN_POINT('Ctrl Pts',(-23.1419844807782,12.6345257825012,
131.170374346328)) ;
#129848 = CARTESIAN_POINT('Ctrl Pts',(-23.2100400384086,12.8902136369556,
131.336008542892)) ;
#129849 = CARTESIAN_POINT('Ctrl Pts',(-23.2539371077913,13.1836914556234,
131.431128041516)) ;
#129850 = CARTESIAN_POINT('Ctrl Pts',(-23.2714654817158,13.4943233171344,
131.449212934784)) ;
#129851 = CARTESIAN_POINT('Ctrl Pts',(-23.2619647848818,13.800844370543,131.388233267397)) ;
#129852 = CARTESIAN_POINT('Ctrl Pts',(-23.2268232132927,14.0793169381169,
131.25243650753)) ;
#129853 = CARTESIAN_POINT('Ctrl Pts',(-23.1698063741231,14.3098744283553,
131.052912529895)) ;
#129854 = CARTESIAN_POINT('Ctrl Pts',(-23.0946065002962,14.4788323999099,
130.799928901127)) ;
#129855 = CARTESIAN_POINT('Ctrl Pts',(-23.0086310860279,14.5706779805767,
130.51574571968)) ;
#129856 = CARTESIAN_POINT('Ctrl Pts',(-22.9181540035114,14.5811216751553,
130.218385768939)) ;
#129857 = CARTESIAN_POINT('Ctrl Pts',(-22.8299926049286,14.5082992229446,
129.927641015252)) ;
#129858 = CARTESIAN_POINT('Ctrl Pts',(-22.7518958692624,14.3580059118444,
129.666415005834)) ;
#129859 = CARTESIAN_POINT('Ctrl Pts',(-22.68973964975,14.1405258591395,129.451695647597)) ;
#129860 = CARTESIAN_POINT('Ctrl Pts',(-22.6489474985288,13.8719963111484,
129.299439068749)) ;
#129861 = CARTESIAN_POINT('Ctrl Pts',(-22.6329623427693,13.5716291757303,
129.219672143091)) ;
#129862 = CARTESIAN_POINT('Ctrl Pts',(-22.6438299307625,13.2591264952113,
129.218186867551)) ;
#129863 = CARTESIAN_POINT('Ctrl Pts',(-22.6813595982475,12.9599152981085,
129.294758434884)) ;
#129864 = CARTESIAN_POINT('Ctrl Pts',(-22.7437268703939,12.6930802012435,
129.44379758794)) ;
#129865 = CARTESIAN_POINT('Ctrl Pts',(-22.8271153369779,12.4788238742032,
129.654272485267)) ;
#129866 = CARTESIAN_POINT('Ctrl Pts',(-22.9262087039054,12.3322479611375,
129.910645691407)) ;
#129867 = CARTESIAN_POINT('Ctrl Pts',(-23.0347908804482,12.2636849703181,
130.194712650591)) ;
#129868 = CARTESIAN_POINT('Ctrl Pts',(-23.1457780726912,12.2782423508481,
130.485793595157)) ;
#129869 = CARTESIAN_POINT('Ctrl Pts',(-23.2518521138872,12.3748788138008,
130.762534585018)) ;
#129870 = CARTESIAN_POINT('Ctrl Pts',(-23.3461191357027,12.5463734301239,
131.004816306225)) ;
#129871 = CARTESIAN_POINT('Ctrl Pts',(-23.4227572575714,12.7810696053441,
131.195540562452)) ;
#129872 = CARTESIAN_POINT('Ctrl Pts',(-23.4766900181559,13.0608632810621,
131.320045830173)) ;
#129873 = CARTESIAN_POINT('Ctrl Pts',(-23.5051675153737,13.3671882377426,
131.37011185604)) ;
#129874 = CARTESIAN_POINT('Ctrl Pts',(-23.5065949253369,13.6783220595412,
131.341073633408)) ;
#129875 = CARTESIAN_POINT('Ctrl Pts',(-23.4816682311954,13.9701100472944,
131.235162424807)) ;
#129876 = CARTESIAN_POINT('Ctrl Pts',(-23.4329222288376,14.2230345165602,
131.059637422382)) ;
#129877 = CARTESIAN_POINT('Ctrl Pts',(-23.3645416427281,14.4186168854027,
130.826753646501)) ;
#129878 = CARTESIAN_POINT('Ctrl Pts',(-23.2822390982612,14.5428705868712,
130.553224844874)) ;
#129879 = CARTESIAN_POINT('Ctrl Pts',(-23.192506581194,14.5869069851008,130.257961717535)) ;
#129880 = CARTESIAN_POINT('Ctrl Pts',(-23.1027575317741,14.5480013167689,
129.962735045499)) ;
#129881 = CARTESIAN_POINT('Ctrl Pts',(-23.0192260399974,14.4271740757264,
129.685359875558)) ;
#129882 = CARTESIAN_POINT('Ctrl Pts',(-22.9503502410774,14.2362638789622,
129.451230370321)) ;
#129883 = CARTESIAN_POINT('Ctrl Pts',(-22.9002301505869,13.9863048422078,
129.271676603921)) ;
#129884 = CARTESIAN_POINT('Ctrl Pts',(-22.8738614058396,13.6957298315302,
129.161501741172)) ;
#129885 = CARTESIAN_POINT('Ctrl Pts',(-22.8736157044307,13.3866515918627,
129.127747431502)) ;
#129886 = CARTESIAN_POINT('Ctrl Pts',(-22.9007309903636,13.0771469983457,
129.173578973472)) ;
#129887 = CARTESIAN_POINT('Ctrl Pts',(-22.9531241560762,12.7963921312271,
129.29371262047)) ;
#129888 = CARTESIAN_POINT('Ctrl Pts',(-23.0287907307986,12.5578779663261,
129.481500335553)) ;
#129889 = CARTESIAN_POINT('Ctrl Pts',(-23.1219014006858,12.3830735911952,
129.720516205546)) ;
#129890 = CARTESIAN_POINT('Ctrl Pts',(-23.2275724461705,12.2815115328469,
129.99604251459)) ;
#129891 = CARTESIAN_POINT('Ctrl Pts',(-23.3388191343614,12.2623682351307,
130.287780389931)) ;
#129892 = CARTESIAN_POINT('Ctrl Pts',(-23.4471188624795,12.3259183972767,
130.571207242919)) ;
#129893 = CARTESIAN_POINT('Ctrl Pts',(-23.5471374646567,12.4680808771893,
130.830236267802)) ;
#129894 = CARTESIAN_POINT('Ctrl Pts',(-23.6317831266168,12.6795622431896,
131.04428925764)) ;
#129895 = CARTESIAN_POINT('Ctrl Pts',(-23.6952246631273,12.942589382418,131.196621763478)) ;
#129896 = CARTESIAN_POINT('Ctrl Pts',(-23.7344524554603,13.2417281941733,
131.278005106931)) ;
#129897 = CARTESIAN_POINT('Ctrl Pts',(-23.7468298790603,13.5531901597367,
131.281039111896)) ;
#129898 = CARTESIAN_POINT('Ctrl Pts',(-23.7323614802831,13.8554127215433,
131.205630116186)) ;
#129899 = CARTESIAN_POINT('Ctrl Pts',(-23.6929669829259,14.1261607802399,
131.05748848122)) ;
#129900 = CARTESIAN_POINT('Ctrl Pts',(-23.631618534262,14.3478084011447,130.844991831341)) ;
#129901 = CARTESIAN_POINT('Ctrl Pts',(-23.5546595857602,14.5013886239399,
130.587262450918)) ;
#129902 = CARTESIAN_POINT('Ctrl Pts',(-23.4667489844287,14.5792262889595,
130.29719183709)) ;
#129903 = CARTESIAN_POINT('Ctrl Pts',(-23.3761695508235,14.5735423486693,
129.999514469588)) ;
#129904 = CARTESIAN_POINT('Ctrl Pts',(-23.289558304496,14.4859392632534,129.71339602831)) ;
#129905 = CARTESIAN_POINT('Ctrl Pts',(-23.2136588166763,14.3210240501096,
129.458405866252)) ;
#129906 = CARTESIAN_POINT('Ctrl Pts',(-23.1555173074775,14.0938130208259,
129.2556140445)) ;
#129907 = CARTESIAN_POINT('Ctrl Pts',(-23.118997631847,13.8165580564643,129.115691388806)) ;
#129908 = CARTESIAN_POINT('Ctrl Pts',(-23.1080276758516,13.5127265390552,
129.050612193546)) ;
#129909 = CARTESIAN_POINT('Ctrl Pts',(-23.1241410108863,13.2000972464797,
129.064374981949)) ;
#129910 = CARTESIAN_POINT('Ctrl Pts',(-23.1662601446052,12.9073427660881,
129.154562570437)) ;
#129911 = CARTESIAN_POINT('Ctrl Pts',(-23.2331580385046,12.6479572947944,
129.316703386966)) ;
#129912 = CARTESIAN_POINT('Ctrl Pts',(-23.3195943837913,12.4461100602533,
129.53621950267)) ;
#129913 = CARTESIAN_POINT('Ctrl Pts',(-23.4215936463265,12.3127706355445,
129.800873866609)) ;
#129914 = CARTESIAN_POINT('Ctrl Pts',(-23.530741294766,12.2601401093184,130.086732236641)) ;
#129915 = CARTESIAN_POINT('Ctrl Pts',(-23.641295933381,12.2901733170219,130.37656641642)) ;
#129916 = CARTESIAN_POINT('Ctrl Pts',(-23.7457667500472,12.4015832972313,
130.648604057112)) ;
#129917 = CARTESIAN_POINT('Ctrl Pts',(-23.837320922193,12.5866483743453,130.882868179984)) ;
#129918 = CARTESIAN_POINT('Ctrl Pts',(-23.9097809110176,12.8302723297284,
131.061533181026)) ;
#129919 = CARTESIAN_POINT('Ctrl Pts',(-23.9594436984039,13.1192440323379,
131.17325973788)) ;
#129920 = CARTESIAN_POINT('Ctrl Pts',(-23.9825588767331,13.4254781979924,
131.207947994022)) ;
#129921 = CARTESIAN_POINT('Ctrl Pts',(-23.9789923334788,13.735359683146,131.164262668825)) ;
#129922 = CARTESIAN_POINT('Ctrl Pts',(-23.9493638176101,14.0210481955409,
131.044652952135)) ;
#129923 = CARTESIAN_POINT('Ctrl Pts',(-23.8964348750507,14.2649914593589,
130.856831392013)) ;
#129924 = CARTESIAN_POINT('Ctrl Pts',(-23.8250858891093,14.4476746883627,
130.615345568459)) ;
#129925 = CARTESIAN_POINT('Ctrl Pts',(-23.7408346035683,14.5574099930499,
130.3361027737)) ;
#129926 = CARTESIAN_POINT('Ctrl Pts',(-23.6506254186035,14.5860647522522,
130.039495997294)) ;
#129927 = CARTESIAN_POINT('Ctrl Pts',(-23.5609942892391,14.5307819491484,
129.744354946213)) ;
#129928 = CARTESIAN_POINT('Ctrl Pts',(-23.4804650219021,14.3969445600344,
129.476125426802)) ;
#129929 = CARTESIAN_POINT('Ctrl Pts',(-23.4142527293967,14.1927449819674,
129.249526011617)) ;
#129930 = CARTESIAN_POINT('Ctrl Pts',(-23.3684848120887,13.9340125126876,
129.082756157156)) ;
#129931 = CARTESIAN_POINT('Ctrl Pts',(-23.3468587978125,13.6381122428634,
128.986428754755)) ;
#129932 = CARTESIAN_POINT('Ctrl Pts',(-23.3518116052348,13.3270743882958,
128.967779729988)) ;
#129933 = CARTESIAN_POINT('Ctrl Pts',(-23.3836997037052,13.022510775008,129.027771986449)) ;
#129934 = CARTESIAN_POINT('Ctrl Pts',(-23.4410446186167,12.7468021187138,
129.162131040852)) ;
#129935 = CARTESIAN_POINT('Ctrl Pts',(-23.5199252416539,12.5205888533643,
129.359570203463)) ;
#129936 = CARTESIAN_POINT('Ctrl Pts',(-23.6162103718271,12.3578210122937,
129.607688028642)) ;
#129937 = CARTESIAN_POINT('Ctrl Pts',(-23.7233238649532,12.2716455027741,
129.887467974327)) ;
#129938 = CARTESIAN_POINT('Ctrl Pts',(-23.8343750091978,12.2679542835663,
130.178745490843)) ;
#129939 = CARTESIAN_POINT('Ctrl Pts',(-23.9420352985659,12.3469221374096,
130.460148975221)) ;
#129940 = CARTESIAN_POINT('Ctrl Pts',(-24.0395306000166,12.5030897490068,
130.71181941671)) ;
#129941 = CARTESIAN_POINT('Ctrl Pts',(-24.1204139007615,12.7250181142628,
130.914990286498)) ;
#129942 = CARTESIAN_POINT('Ctrl Pts',(-24.1797612052318,12.997182712002,131.055216258735)) ;
#129943 = CARTESIAN_POINT('Ctrl Pts',(-24.2139296280654,13.2997827331154,
131.121902223964)) ;
#129944 = CARTESIAN_POINT('Ctrl Pts',(-24.2212467345928,13.6108909290664,
131.110180839414)) ;
#129945 = CARTESIAN_POINT('Ctrl Pts',(-24.2019836667752,13.9087322628313,
131.020799333689)) ;
#129946 = CARTESIAN_POINT('Ctrl Pts',(-24.1579858554531,14.1725575472539,
130.859051286282)) ;
#129947 = CARTESIAN_POINT('Ctrl Pts',(-24.093541705692,14.3815587405522,130.637727194554)) ;
#129948 = CARTESIAN_POINT('Ctrl Pts',(-24.0137360577577,14.5223295633007,
130.371479426055)) ;
#129949 = CARTESIAN_POINT('Ctrl Pts',(-23.9250824711545,14.5844939623778,
130.079398354997)) ;
#129950 = CARTESIAN_POINT('Ctrl Pts',(-23.8342900042102,14.5631534424975,
129.780935135738)) ;
#129951 = CARTESIAN_POINT('Ctrl Pts',(-23.7494814898801,14.4606751322893,
129.500175677992)) ;
#129952 = CARTESIAN_POINT('Ctrl Pts',(-23.6763381643652,14.2826954398612,
129.253230600252)) ;
#129953 = CARTESIAN_POINT('Ctrl Pts',(-23.6219494390935,14.0447463788915,
129.061356272604)) ;
#129954 = CARTESIAN_POINT('Ctrl Pts',(-23.5900786851126,13.7613771395104,
128.935107708196)) ;
#129955 = CARTESIAN_POINT('Ctrl Pts',(-23.5840797714012,13.4542323467487,
128.884499268984)) ;
#129956 = CARTESIAN_POINT('Ctrl Pts',(-23.6051135424781,13.1437994705374,
128.91274207276)) ;
#129957 = CARTESIAN_POINT('Ctrl Pts',(-23.6524480707265,12.8538469195634,
129.017861949348)) ;
#129958 = CARTESIAN_POINT('Ctrl Pts',(-23.7231470461455,12.6054873461084,
129.191328878648)) ;
#129959 = CARTESIAN_POINT('Ctrl Pts',(-23.812834818571,12.4153273171675,129.420299880366)) ;
#129960 = CARTESIAN_POINT('Ctrl Pts',(-23.9171324935436,12.2964112453651,
129.691604194727)) ;
#129961 = CARTESIAN_POINT('Ctrl Pts',(-24.0268994581797,12.2594155907016,
129.979307926472)) ;
#129962 = CARTESIAN_POINT('Ctrl Pts',(-24.1370680092537,12.3053349417689,
130.267942075581)) ;
#129963 = CARTESIAN_POINT('Ctrl Pts',(-24.2392677005312,12.4312258982637,
130.533435968365)) ;
#129964 = CARTESIAN_POINT('Ctrl Pts',(-24.3275283859303,12.627959699626,130.758169851058)) ;
#129965 = CARTESIAN_POINT('Ctrl Pts',(-24.3962310838253,12.8824932642082,
130.925674503715)) ;
#129966 = CARTESIAN_POINT('Ctrl Pts',(-24.4407733223245,13.1745455141317,
131.022746419222)) ;
#129967 = CARTESIAN_POINT('Ctrl Pts',(-24.4591380272995,13.4851755332174,
131.043255013574)) ;
#129968 = CARTESIAN_POINT('Ctrl Pts',(-24.4503750207915,13.7921378916297,
130.984426733776)) ;
#129969 = CARTESIAN_POINT('Ctrl Pts',(-24.4161419214947,14.0710147358115,
130.851388646496)) ;
#129970 = CARTESIAN_POINT('Ctrl Pts',(-24.3593113729837,14.3045451630866,
130.65219208029)) ;
#129971 = CARTESIAN_POINT('Ctrl Pts',(-24.2852488197019,14.4740865668841,
130.402844051698)) ;
#129972 = CARTESIAN_POINT('Ctrl Pts',(-24.1989871899202,14.5693022255178,
130.11759849223)) ;
#129973 = CARTESIAN_POINT('Ctrl Pts',(-24.1085533561024,14.5820126404232,
129.820380804925)) ;
#129974 = CARTESIAN_POINT('Ctrl Pts',(-24.0199963670256,14.511227148385,129.528389522944)) ;
#129975 = CARTESIAN_POINT('Ctrl Pts',(-23.9418631026754,14.3635592095882,
129.267195284118)) ;
#129976 = CARTESIAN_POINT('Ctrl Pts',(-23.8791136578675,14.1479540457657,
129.05073670007)) ;
#129977 = CARTESIAN_POINT('Ctrl Pts',(-23.8375873211756,13.8806548150988,
128.896328674777)) ;
#129978 = CARTESIAN_POINT('Ctrl Pts',(-23.8208085079993,13.5796274976099,
128.814103347584)) ;
#129979 = CARTESIAN_POINT('Ctrl Pts',(-23.8309910040008,13.2675903207149,
128.810667211912)) ;
#129980 = CARTESIAN_POINT('Ctrl Pts',(-23.8676460753912,12.9685393954342,
128.884773865646)) ;
#129981 = CARTESIAN_POINT('Ctrl Pts',(-23.9293823518697,12.7001828412868,
129.031937184548)) ;
#129982 = CARTESIAN_POINT('Ctrl Pts',(-24.0121193234782,12.484351447388,129.240548101327)) ;
#129983 = CARTESIAN_POINT('Ctrl Pts',(-24.1109979057002,12.3354378229303,
129.496238790614)) ;
#129984 = CARTESIAN_POINT('Ctrl Pts',(-24.2190824025548,12.2645466644513,
129.778950581268)) ;
#129985 = CARTESIAN_POINT('Ctrl Pts',(-24.330609557235,12.2767400310682,130.071453555101)) ;
#129986 = CARTESIAN_POINT('Ctrl Pts',(-24.4365405624164,12.3708038596253,
130.347899012378)) ;
#129987 = CARTESIAN_POINT('Ctrl Pts',(-24.5314328322576,12.5405713719576,
130.591935712668)) ;
#129988 = CARTESIAN_POINT('Ctrl Pts',(-24.6084325711965,12.7727635932404,
130.783833850884)) ;
#129989 = CARTESIAN_POINT('Ctrl Pts',(-24.6634600795244,13.0532481868504,
130.911323007965)) ;
#129990 = CARTESIAN_POINT('Ctrl Pts',(-24.692522529149,13.3594503322591,130.963076041083)) ;
#129991 = CARTESIAN_POINT('Ctrl Pts',(-24.6947280405791,13.6687250263673,
130.936529774944)) ;
#129992 = CARTESIAN_POINT('Ctrl Pts',(-24.6705282850378,13.9622483916866,
130.832644671573)) ;
#129993 = CARTESIAN_POINT('Ctrl Pts',(-24.622436218567,14.216383713817,130.659054441099)) ;
#129994 = CARTESIAN_POINT('Ctrl Pts',(-24.5543668513611,14.4143549366633,
130.426992649947)) ;
#129995 = CARTESIAN_POINT('Ctrl Pts',(-24.4723486974786,14.5404303817965,
130.154299491946)) ;
#129996 = CARTESIAN_POINT('Ctrl Pts',(-24.3831123163456,14.5868747918771,
129.860628601173)) ;
#129997 = CARTESIAN_POINT('Ctrl Pts',(-24.2927557290999,14.5499212465235,
129.56342641909)) ;
#129998 = CARTESIAN_POINT('Ctrl Pts',(-24.2096290003052,14.4324626280189,
129.287528296366)) ;
#129999 = CARTESIAN_POINT('Ctrl Pts',(-24.1396226803011,14.2419356925952,
129.049797964534)) ;
#130000 = CARTESIAN_POINT('Ctrl Pts',(-24.0891543308482,13.9939564781135,
128.869339869159)) ;
#130001 = CARTESIAN_POINT('Ctrl Pts',(-24.0620213641921,13.704318184283,128.756930260385)) ;
#130002 = CARTESIAN_POINT('Ctrl Pts',(-24.0610743558635,13.3953698080797,
128.721115144032)) ;
#130003 = CARTESIAN_POINT('Ctrl Pts',(-24.0872215118966,13.0868084154143,
128.764268368717)) ;
#130004 = CARTESIAN_POINT('Ctrl Pts',(-24.1391372778054,12.8035341969557,
128.882834895599)) ;
#130005 = CARTESIAN_POINT('Ctrl Pts',(-24.2141316302003,12.5639567807414,
129.068713539452)) ;
#130006 = CARTESIAN_POINT('Ctrl Pts',(-24.3069768980926,12.3867441637874,
129.306888123521)) ;
#130007 = CARTESIAN_POINT('Ctrl Pts',(-24.4126054249827,12.2832559851663,
129.582236617727)) ;
#130008 = CARTESIAN_POINT('Ctrl Pts',(-24.5228382226761,12.2616345605918,
129.871302925535)) ;
#130009 = CARTESIAN_POINT('Ctrl Pts',(-24.6321785231031,12.3231638536054,
130.157498310678)) ;
#130010 = CARTESIAN_POINT('Ctrl Pts',(-24.7320770324703,12.4627499394219,
130.41633010543)) ;
#130011 = CARTESIAN_POINT('Ctrl Pts',(-24.8175012342038,12.6729052718455,
130.632563287353)) ;
#130012 = CARTESIAN_POINT('Ctrl Pts',(-24.8815266149577,12.9344259227914,
130.786639358572)) ;
#130013 = CARTESIAN_POINT('Ctrl Pts',(-24.9215855419147,13.2340773776093,
130.870319237765)) ;
#130014 = CARTESIAN_POINT('Ctrl Pts',(-24.9345965993483,13.5439037579597,
130.875373791953)) ;
#130015 = CARTESIAN_POINT('Ctrl Pts',(-24.9209872048283,13.8465580418888,
130.802495474506)) ;
#130016 = CARTESIAN_POINT('Ctrl Pts',(-24.8822354446801,14.1188038713519,
130.656193145261)) ;
#130017 = CARTESIAN_POINT('Ctrl Pts',(-24.8215520611578,14.3420290100945,
130.445680053042)) ;
#130018 = CARTESIAN_POINT('Ctrl Pts',(-24.7447511412938,14.4980359942342,
130.188314463308)) ;
#130019 = CARTESIAN_POINT('Ctrl Pts',(-24.6574682218922,14.5780642273586,
129.900239858161)) ;
#130020 = CARTESIAN_POINT('Ctrl Pts',(-24.5661704406245,14.5747644826435,
129.600201361656)) ;
#130021 = CARTESIAN_POINT('Ctrl Pts',(-24.4798397107362,14.4895501610045,
129.315081720064)) ;
#130022 = CARTESIAN_POINT('Ctrl Pts',(-24.4036359268958,14.3274512492284,
129.059276795445)) ;
#130023 = CARTESIAN_POINT('Ctrl Pts',(-24.3446920999538,14.1012132638127,
128.854030110214)) ;
#130024 = CARTESIAN_POINT('Ctrl Pts',(-24.3074730021535,13.8249845460598,
128.712057536314)) ;
#130025 = CARTESIAN_POINT('Ctrl Pts',(-24.2957931040204,13.5214322498008,
128.644878171936)) ;
#130026 = CARTESIAN_POINT('Ctrl Pts',(-24.3109547722312,13.2103012906498,
128.656038921471)) ;
#130027 = CARTESIAN_POINT('Ctrl Pts',(-24.3525323396269,12.9148532229271,
128.744433326594)) ;
#130028 = CARTESIAN_POINT('Ctrl Pts',(-24.41885720721,12.6543478093024,128.904910138534)) ;
#130029 = CARTESIAN_POINT('Ctrl Pts',(-24.5046482463071,12.4511189000955,
129.122596465375)) ;
#130030 = CARTESIAN_POINT('Ctrl Pts',(-24.6060741915631,12.3156705580683,
129.385644993005)) ;
#130031 = CARTESIAN_POINT('Ctrl Pts',(-24.7155785502479,12.2603783302423,
129.672396480643)) ;
#130032 = CARTESIAN_POINT('Ctrl Pts',(-24.8261383061215,12.2883877203707,
129.962262156073)) ;
#130033 = CARTESIAN_POINT('Ctrl Pts',(-24.9304589738136,12.396958249081,130.233999385643)) ;
#130034 = CARTESIAN_POINT('Ctrl Pts',(-25.022824941926,12.5805839633338,130.470521381763)) ;
#130035 = CARTESIAN_POINT('Ctrl Pts',(-25.0956897007076,12.8225431186843,
130.650415821546)) ;
#130036 = CARTESIAN_POINT('Ctrl Pts',(-25.1459747153606,13.1085293603561,
130.764170454789)) ;
#130037 = CARTESIAN_POINT('Ctrl Pts',(-25.1701258151212,13.4184312880114,
130.801450841833)) ;
#130038 = CARTESIAN_POINT('Ctrl Pts',(-25.1672868025462,13.725396861632,130.760244966017)) ;
#130039 = CARTESIAN_POINT('Ctrl Pts',(-25.1382759895552,14.0140710256624,
130.642207480891)) ;
#130040 = CARTESIAN_POINT('Ctrl Pts',(-25.0860152986228,14.2586953044857,
130.45643248086)) ;
#130041 = CARTESIAN_POINT('Ctrl Pts',(-25.0150543029557,14.4435712314573,
130.216035138787)) ;
#130042 = CARTESIAN_POINT('Ctrl Pts',(-24.9310895100697,14.5554638006899,
129.93764282236)) ;
#130043 = CARTESIAN_POINT('Ctrl Pts',(-24.8408606796343,14.5862678502932,
129.640940642294)) ;
#130044 = CARTESIAN_POINT('Ctrl Pts',(-24.7516930753071,14.5339455436029,
129.347384079267)) ;
#130045 = CARTESIAN_POINT('Ctrl Pts',(-24.6703799463621,14.4019055973539,
129.076694015721)) ;
#130046 = CARTESIAN_POINT('Ctrl Pts',(-24.60374205745,14.1996929983724,128.848891564666)) ;
#130047 = CARTESIAN_POINT('Ctrl Pts',(-24.5572296961542,13.9418840737313,
128.679885640708)) ;
#130048 = CARTESIAN_POINT('Ctrl Pts',(-24.5348995734261,13.6467946760401,
128.581512428971)) ;
#130049 = CARTESIAN_POINT('Ctrl Pts',(-24.5390899690228,13.3358858786889,
128.560634084449)) ;
#130050 = CARTESIAN_POINT('Ctrl Pts',(-24.5701795719701,13.0311284856173,
128.618330046274)) ;
#130051 = CARTESIAN_POINT('Ctrl Pts',(-24.6268180622581,12.7543596486341,
128.750628733576)) ;
#130052 = CARTESIAN_POINT('Ctrl Pts',(-24.7050311793029,12.5263865010007,
128.946135952786)) ;
#130053 = CARTESIAN_POINT('Ctrl Pts',(-24.8017020723011,12.3607018495905,
129.1951266527)) ;
#130054 = CARTESIAN_POINT('Ctrl Pts',(-24.9076373162968,12.2732420345152,
129.471773127455)) ;
#130055 = CARTESIAN_POINT('Ctrl Pts',(-25.019108352556,12.2668291057712,129.764141625486)) ;
#130056 = CARTESIAN_POINT('Ctrl Pts',(-25.1268880991479,12.3436151679642,
130.045917699935)) ;
#130057 = CARTESIAN_POINT('Ctrl Pts',(-25.2248793133505,12.4979166687538,
130.298995565544)) ;
#130058 = CARTESIAN_POINT('Ctrl Pts',(-25.3062265907711,12.7181779713464,
130.503539894247)) ;
#130059 = CARTESIAN_POINT('Ctrl Pts',(-25.3661555440321,12.9887183065796,
130.645518524112)) ;
#130060 = CARTESIAN_POINT('Ctrl Pts',(-25.4011086939028,13.2908825887428,
130.714479030165)) ;
#130061 = CARTESIAN_POINT('Ctrl Pts',(-25.4092132990991,13.6021682784688,
130.70504715979)) ;
#130062 = CARTESIAN_POINT('Ctrl Pts',(-25.3905897140097,13.9015372403182,
130.617436728814)) ;
#130063 = CARTESIAN_POINT('Ctrl Pts',(-25.3471895019976,14.1661756912177,
130.457466439887)) ;
#130064 = CARTESIAN_POINT('Ctrl Pts',(-25.283475751484,14.3763136257562,130.238379001657)) ;
#130065 = CARTESIAN_POINT('Ctrl Pts',(-25.2038316680715,14.5195378836765,
129.972523388979)) ;
#130066 = CARTESIAN_POINT('Ctrl Pts',(-25.1155555814888,14.5837467686513,
129.681630393675)) ;
#130067 = CARTESIAN_POINT('Ctrl Pts',(-25.0247905890407,14.5651055728363,
129.383278007598)) ;
#130068 = CARTESIAN_POINT('Ctrl Pts',(-24.9394526693564,14.4645029027952,
129.100861825567)) ;
#130069 = CARTESIAN_POINT('Ctrl Pts',(-24.8661197664223,14.2890440216263,
128.853472968967)) ;
#130070 = CARTESIAN_POINT('Ctrl Pts',(-24.8110505251749,14.0526945141533,
128.659594364076)) ;
#130071 = CARTESIAN_POINT('Ctrl Pts',(-24.7784342225117,13.769986617102,128.531126378095)) ;
#130072 = CARTESIAN_POINT('Ctrl Pts',(-24.771626872808,13.4631529516268,128.478150286101)) ;
#130073 = CARTESIAN_POINT('Ctrl Pts',(-24.7920899070549,13.1513621108982,
128.504596727791)) ;
#130074 = CARTESIAN_POINT('Ctrl Pts',(-24.8382943929961,12.8627668355385,
128.606681449633)) ;
#130075 = CARTESIAN_POINT('Ctrl Pts',(-24.9089211448075,12.6109028724027,
128.779662777081)) ;
#130076 = CARTESIAN_POINT('Ctrl Pts',(-24.9977863342769,12.420019305974,129.006391048658)) ;
#130077 = CARTESIAN_POINT('Ctrl Pts',(-25.1018228161412,12.2986947230639,
129.276907811114)) ;
#130078 = CARTESIAN_POINT('Ctrl Pts',(-25.2113470557582,12.259272392657,129.563951755654)) ;
#130079 = CARTESIAN_POINT('Ctrl Pts',(-25.3219618782627,12.3030853474754,
129.853781195152)) ;
#130080 = CARTESIAN_POINT('Ctrl Pts',(-25.4239394298828,12.4259705757025,
130.118810360826)) ;
#130081 = CARTESIAN_POINT('Ctrl Pts',(-25.5132843704644,12.6220549882292,
130.346490329366)) ;
#130082 = CARTESIAN_POINT('Ctrl Pts',(-25.5823256886098,12.8744669108447,
130.515101999542)) ;
#130083 = CARTESIAN_POINT('Ctrl Pts',(-25.6277091251102,13.1663405634683,
130.614553329165)) ;
#130084 = CARTESIAN_POINT('Ctrl Pts',(-25.6467159933288,13.4758788255352,
130.637032806762)) ;
#130085 = CARTESIAN_POINT('Ctrl Pts',(-25.638912605484,13.7823952267848,130.581117864475)) ;
#130086 = CARTESIAN_POINT('Ctrl Pts',(-25.605083495813,14.0644181271455,130.4490002908)) ;
#130087 = CARTESIAN_POINT('Ctrl Pts',(-25.5492735285762,14.2977470624668,
130.253047631057)) ;
#130088 = CARTESIAN_POINT('Ctrl Pts',(-25.475180464955,14.470619356869,130.003380356877)) ;
#130089 = CARTESIAN_POINT('Ctrl Pts',(-25.3894108294434,14.5675954870708,
129.719686882913)) ;
#130090 = CARTESIAN_POINT('Ctrl Pts',(-25.2989629243675,14.5827756114501,
129.422402440643)) ;
#130091 = CARTESIAN_POINT('Ctrl Pts',(-25.2105889079703,14.5148009028155,
129.131086132755)) ;
#130092 = CARTESIAN_POINT('Ctrl Pts',(-25.1317819491608,14.369224395635,128.867826008019)) ;
#130093 = CARTESIAN_POINT('Ctrl Pts',(-25.0682405512477,14.1540995770501,
128.648890563742)) ;
#130094 = CARTESIAN_POINT('Ctrl Pts',(-25.0263127249798,13.8891947674814,
128.493467439993)) ;
#130095 = CARTESIAN_POINT('Ctrl Pts',(-25.0087151808049,13.5894850421774,
128.408911577462)) ;
#130096 = CARTESIAN_POINT('Ctrl Pts',(-25.0180502307985,13.2771023843451,
128.402962217407)) ;
#130097 = CARTESIAN_POINT('Ctrl Pts',(-25.0539881461516,12.9767130862842,
128.474903380437)) ;
#130098 = CARTESIAN_POINT('Ctrl Pts',(-25.1153594134085,12.7063603271624,
128.620882754512)) ;
#130099 = CARTESIAN_POINT('Ctrl Pts',(-25.1971076916216,12.4901610418877,
128.826797301287)) ;
#130100 = CARTESIAN_POINT('Ctrl Pts',(-25.2956565313931,12.3386882869186,
129.081490867723)) ;
#130101 = CARTESIAN_POINT('Ctrl Pts',(-25.4037767211478,12.2654833410071,
129.364243566983)) ;
#130102 = CARTESIAN_POINT('Ctrl Pts',(-25.5149608400151,12.2750423619251,
129.655858772134)) ;
#130103 = CARTESIAN_POINT('Ctrl Pts',(-25.62166667954,12.3673308735559,129.934393950309)) ;
#130104 = CARTESIAN_POINT('Ctrl Pts',(-25.7165022687578,12.5343468737747,
130.178429108854)) ;
#130105 = CARTESIAN_POINT('Ctrl Pts',(-25.7943039636434,12.7652870390172,
130.372595003719)) ;
#130106 = CARTESIAN_POINT('Ctrl Pts',(-25.8499392894425,13.0444118412715,
130.501898406253)) ;
#130107 = CARTESIAN_POINT('Ctrl Pts',(-25.8798587035347,13.3498616588083,
130.556181727478)) ;
#130108 = CARTESIAN_POINT('Ctrl Pts',(-25.8827771353525,13.6613614501294,
130.531495893468)) ;
#130109 = CARTESIAN_POINT('Ctrl Pts',(-25.8593804684295,13.9537821761938,
130.430165894424)) ;
#130110 = CARTESIAN_POINT('Ctrl Pts',(-25.8119584670191,14.2096141280325,
130.25850584693)) ;
#130111 = CARTESIAN_POINT('Ctrl Pts',(-25.7445330464467,14.4090573125523,
130.028392541274)) ;
#130112 = CARTESIAN_POINT('Ctrl Pts',(-25.6628970061439,14.5378227703646,
129.756818694175)) ;
#130113 = CARTESIAN_POINT('Ctrl Pts',(-25.5730799531226,14.586641023904,129.461192374976)) ;
#130114 = CARTESIAN_POINT('Ctrl Pts',(-25.483496675564,14.5524956993372,129.166576918439)) ;
#130115 = CARTESIAN_POINT('Ctrl Pts',(-25.3993139751561,14.4363359778134,
128.887285569447)) ;
#130116 = CARTESIAN_POINT('Ctrl Pts',(-25.3293572590476,14.2487612489542,
128.649931064422)) ;
#130117 = CARTESIAN_POINT('Ctrl Pts',(-25.2781045437042,14.001996361713,128.467114957121)) ;
#130118 = CARTESIAN_POINT('Ctrl Pts',(-25.250215263522,13.7133413728872,128.352510202207)) ;
#130119 = CARTESIAN_POINT('Ctrl Pts',(-25.2485729664507,13.4034231145874,
128.31452669011)) ;
#130120 = CARTESIAN_POINT('Ctrl Pts',(-25.2737311770127,13.096615616376,128.35502835555)) ;
#130121 = CARTESIAN_POINT('Ctrl Pts',(-25.3252318166841,12.8104956483767,
128.472164048683)) ;
#130122 = CARTESIAN_POINT('Ctrl Pts',(-25.399266285014,12.5707042667784,128.655417699095)) ;
#130123 = CARTESIAN_POINT('Ctrl Pts',(-25.491768455404,12.391019395432,128.892529678587)) ;
#130124 = CARTESIAN_POINT('Ctrl Pts',(-25.5968872536902,12.2853288824572,
129.166465407052)) ;
#130125 = CARTESIAN_POINT('Ctrl Pts',(-25.7074275379451,12.2609818492728,
129.456317516163)) ;
#130126 = CARTESIAN_POINT('Ctrl Pts',(-25.8172037544521,12.320475723284,129.74370091659)) ;
#130127 = CARTESIAN_POINT('Ctrl Pts',(-25.9174068491702,12.4582515201719,
130.003416142013)) ;
#130128 = CARTESIAN_POINT('Ctrl Pts',(-26.0030700444993,12.6658997536836,
130.220462101582)) ;
#130129 = CARTESIAN_POINT('Ctrl Pts',(-26.0678508238643,12.9268094738204,
130.3766640491)) ;
#130130 = CARTESIAN_POINT('Ctrl Pts',(-26.1084061300055,13.2233760165972,
130.462053917808)) ;
#130131 = CARTESIAN_POINT('Ctrl Pts',(-26.1224375596645,13.5346575170046,
130.469920578644)) ;
#130132 = CARTESIAN_POINT('Ctrl Pts',(-26.1094897742864,13.8387959699086,
130.398875623468)) ;
#130133 = CARTESIAN_POINT('Ctrl Pts',(-26.0713053088302,14.1123016431052,
130.254200206036)) ;
#130134 = CARTESIAN_POINT('Ctrl Pts',(-26.0113054939942,14.3364686131329,
130.045772465312)) ;
#130135 = CARTESIAN_POINT('Ctrl Pts',(-25.9349000952512,14.4947707498965,
129.789555101611)) ;
#130136 = CARTESIAN_POINT('Ctrl Pts',(-25.847424432091,14.5769227712613,129.500776994959)) ;
#130137 = CARTESIAN_POINT('Ctrl Pts',(-25.7571700794344,14.5762675707607,
129.204175853418)) ;
#130138 = CARTESIAN_POINT('Ctrl Pts',(-25.6698503685572,14.493055502163,128.915876035084)) ;
#130139 = CARTESIAN_POINT('Ctrl Pts',(-25.593444376005,14.3331651665745,128.659561752647)) ;
#130140 = CARTESIAN_POINT('Ctrl Pts',(-25.5338234294376,14.1081177718604,
128.452263061707)) ;
#130141 = CARTESIAN_POINT('Ctrl Pts',(-25.4960451793118,13.8340180428126,
128.308780387983)) ;
#130142 = CARTESIAN_POINT('Ctrl Pts',(-25.4835318306803,13.5302900584997,
128.239082101355)) ;
#130143 = CARTESIAN_POINT('Ctrl Pts',(-25.4979122407888,13.2194243094674,
128.24800347794)) ;
#130144 = CARTESIAN_POINT('Ctrl Pts',(-25.5387210538809,12.9232189359804,
128.334150129687)) ;
#130145 = CARTESIAN_POINT('Ctrl Pts',(-25.6043090215129,12.6614613466154,
128.492497917721)) ;
#130146 = CARTESIAN_POINT('Ctrl Pts',(-25.6897562965941,12.4560560790089,
128.709114179214)) ;
#130147 = CARTESIAN_POINT('Ctrl Pts',(-25.7905081105,12.3187614770299,128.970300671274)) ;
#130148 = CARTESIAN_POINT('Ctrl Pts',(-25.9000226576879,12.2608758941321,
129.257026905128)) ;
#130149 = CARTESIAN_POINT('Ctrl Pts',(-26.0104797637691,12.2860567415008,
129.546655594556)) ;
#130150 = CARTESIAN_POINT('Ctrl Pts',(-26.1159736762641,12.3936760642326,
129.821514421549)) ;
#130151 = CARTESIAN_POINT('Ctrl Pts',(-26.2077752209374,12.5734426987992,
130.056754959979)) ;
#130152 = CARTESIAN_POINT('Ctrl Pts',(-26.2819090991338,12.8155556665824,
130.240092263776)) ;
#130153 = CARTESIAN_POINT('Ctrl Pts',(-26.3326381883263,13.1001458874772,
130.355223107769)) ;
#130154 = CARTESIAN_POINT('Ctrl Pts',(-26.3575582974656,13.4082451870112,
130.394897541893)) ;
#130155 = CARTESIAN_POINT('Ctrl Pts',(-26.3555548909241,13.7170001852575,
130.355978042951)) ;
#130156 = CARTESIAN_POINT('Ctrl Pts',(-26.3271329019922,14.0068803460707,
130.239616500101)) ;
#130157 = CARTESIAN_POINT('Ctrl Pts',(-26.2756477863993,14.2520830316222,
130.056220302137)) ;
#130158 = CARTESIAN_POINT('Ctrl Pts',(-26.2052864210748,14.4388654813696,
129.817614241307)) ;
#130159 = CARTESIAN_POINT('Ctrl Pts',(-26.1215233775957,14.5532758693692,
129.539771420139)) ;
#130160 = CARTESIAN_POINT('Ctrl Pts',(-26.0313033647725,14.5866372914021,
129.243071371308)) ;
#130161 = CARTESIAN_POINT('Ctrl Pts',(-25.9417632337185,14.536325428207,128.948328411036)) ;
#130162 = CARTESIAN_POINT('Ctrl Pts',(-25.8604875007569,14.4070821895425,
128.677900419032)) ;
#130163 = CARTESIAN_POINT('Ctrl Pts',(-25.7930114331716,14.2058492618622,
128.447493048992)) ;
#130164 = CARTESIAN_POINT('Ctrl Pts',(-25.745989866581,13.9493210754263,128.277020775163)) ;
#130165 = CARTESIAN_POINT('Ctrl Pts',(-25.7229926511202,13.6560817466226,
128.176815880105)) ;
#130166 = CARTESIAN_POINT('Ctrl Pts',(-25.7263604626951,13.3454214916358,
128.153541083346)) ;
#130167 = CARTESIAN_POINT('Ctrl Pts',(-25.75653203912,13.0405959101595,128.208610801399)) ;
#130168 = CARTESIAN_POINT('Ctrl Pts',(-25.8127824032737,12.7610204461784,
128.339579180513)) ;
#130169 = CARTESIAN_POINT('Ctrl Pts',(-25.8904302641907,12.5320805798767,
128.533479631004)) ;
#130170 = CARTESIAN_POINT('Ctrl Pts',(-25.9859544465224,12.3651154017827,
128.779347978492)) ;
#130171 = CARTESIAN_POINT('Ctrl Pts',(-26.092542096783,12.2743250187668,129.057620383868)) ;
#130172 = CARTESIAN_POINT('Ctrl Pts',(-26.2040626873145,12.2660445050815,
129.350117816326)) ;
#130173 = CARTESIAN_POINT('Ctrl Pts',(-26.3116128241466,12.3402670873944,
129.631347677385)) ;
#130174 = CARTESIAN_POINT('Ctrl Pts',(-26.4100212191217,12.4924310818324,
129.885636405723)) ;
#130175 = CARTESIAN_POINT('Ctrl Pts',(-26.4918260757063,12.7106680082788,
130.091558972653)) ;
#130176 = CARTESIAN_POINT('Ctrl Pts',(-26.5525962863501,12.9803448576749,
130.235943356586)) ;
#130177 = CARTESIAN_POINT('Ctrl Pts',(-26.5883391529532,13.2833169308344,
130.30706416664)) ;
#130178 = CARTESIAN_POINT('Ctrl Pts',(-26.5971320647006,13.5926826730587,
130.299854627125)) ;
#130179 = CARTESIAN_POINT('Ctrl Pts',(-26.5792466524351,13.8936496800992,
130.21429663377)) ;
#130180 = CARTESIAN_POINT('Ctrl Pts',(-26.5365931556998,14.1589429573028,
130.056588090138)) ;
#130181 = CARTESIAN_POINT('Ctrl Pts',(-26.4733112450839,14.371150690962,129.838705183338)) ;
#130182 = CARTESIAN_POINT('Ctrl Pts',(-26.3943156088787,14.5162610236172,
129.574855837709)) ;
#130183 = CARTESIAN_POINT('Ctrl Pts',(-26.3054716122965,14.5833063391636,
129.282028478141)) ;
#130184 = CARTESIAN_POINT('Ctrl Pts',(-26.2149058148592,14.5665129861826,
128.984347754554)) ;
#130185 = CARTESIAN_POINT('Ctrl Pts',(-26.1296349482658,14.4685224536154,
128.702240983504)) ;
#130186 = CARTESIAN_POINT('Ctrl Pts',(-26.055901030885,14.2954966749806,128.453723607246)) ;
#130187 = CARTESIAN_POINT('Ctrl Pts',(-26.000035182886,14.0596947072176,128.257378016009)) ;
#130188 = CARTESIAN_POINT('Ctrl Pts',(-25.9667582155581,13.7784556667528,
128.12704153871)) ;
#130189 = CARTESIAN_POINT('Ctrl Pts',(-25.9593349700014,13.4704205936671,
128.072089582602)) ;
#130190 = CARTESIAN_POINT('Ctrl Pts',(-25.9786379348954,13.1626907214352,
128.095620872259)) ;
#130191 = CARTESIAN_POINT('Ctrl Pts',(-26.024568251676,12.8697533437124,128.196503840888)) ;
#130192 = CARTESIAN_POINT('Ctrl Pts',(-26.0939304436759,12.618666846953,128.366102809598)) ;
#130193 = CARTESIAN_POINT('Ctrl Pts',(-26.1831183712039,12.424057056317,128.593453303362)) ;
#130194 = CARTESIAN_POINT('Ctrl Pts',(-26.2857494091626,12.301712900972,128.860227719189)) ;
#130195 = CARTESIAN_POINT('Ctrl Pts',(-26.3959672181736,12.2592124432014,
129.149039423007)) ;
#130196 = CARTESIAN_POINT('Ctrl Pts',(-26.5061419238419,12.300200425655,129.437764546279)) ;
#130197 = CARTESIAN_POINT('Ctrl Pts',(-26.6094954585518,12.4222100084694,
129.706457390739)) ;
#130198 = CARTESIAN_POINT('Ctrl Pts',(-26.6985712830069,12.6151763749812,
129.93361606151)) ;
#130199 = CARTESIAN_POINT('Ctrl Pts',(-26.7684896012397,12.8667635353633,
130.104687662764)) ;
#130200 = CARTESIAN_POINT('Ctrl Pts',(-26.8144251071473,13.1566082723263,
130.205889756394)) ;
#130201 = CARTESIAN_POINT('Ctrl Pts',(-26.834380951446,13.4669634672463,130.23102669691)) ;
#130202 = CARTESIAN_POINT('Ctrl Pts',(-26.827214904313,13.7743605227785,130.176916300451)) ;
#130203 = CARTESIAN_POINT('Ctrl Pts',(-26.7943756619693,14.0556835016132,
130.047907219521)) ;
#130204 = CARTESIAN_POINT('Ctrl Pts',(-26.7388548120431,14.2923698001693,
129.852577489673)) ;
#130205 = CARTESIAN_POINT('Ctrl Pts',(-26.6650281834544,14.4669397818909,
129.603657958846)) ;
#130206 = CARTESIAN_POINT('Ctrl Pts',(-26.5799991592676,14.5658236939165,
129.322316054393)) ;
#130207 = CARTESIAN_POINT('Ctrl Pts',(-26.4890730846777,14.5834030857371,
129.023436802721)) ;
#130208 = CARTESIAN_POINT('Ctrl Pts',(-26.4010181587823,14.5182209911816,
128.733249100209)) ;
#130209 = CARTESIAN_POINT('Ctrl Pts',(-26.3211717954855,14.3732473260144,
128.466642858011)) ;
#130210 = CARTESIAN_POINT('Ctrl Pts',(-26.2577722791704,14.1617341890797,
128.248450584103)) ;
#130211 = CARTESIAN_POINT('Ctrl Pts',(-26.2148585718976,13.8968740490593,
128.08996654976)) ;
#130212 = CARTESIAN_POINT('Ctrl Pts',(-26.1966227215079,13.5970562228853,
128.003481258227)) ;
#130213 = CARTESIAN_POINT('Ctrl Pts',(-26.2052628641563,13.2853499830191,
127.995568689957)) ;
#130214 = CARTESIAN_POINT('Ctrl Pts',(-26.2403552083071,12.9854215224893,
128.065151386669)) ;
#130215 = CARTESIAN_POINT('Ctrl Pts',(-26.3007530503343,12.7145027585382,
128.208390021964)) ;
#130216 = CARTESIAN_POINT('Ctrl Pts',(-26.3823022410149,12.4953423449653,
128.413561260671)) ;
#130217 = CARTESIAN_POINT('Ctrl Pts',(-26.4806652696605,12.3417858317011,
128.667663037527)) ;
#130218 = CARTESIAN_POINT('Ctrl Pts',(-26.5882930356624,12.2665368316973,
128.949071919843)) ;
#130219 = CARTESIAN_POINT('Ctrl Pts',(-26.6993769112587,12.2735361419267,
129.240428663002)) ;
#130220 = CARTESIAN_POINT('Ctrl Pts',(-26.8062769983724,12.363229877568,129.519550348536)) ;
#130221 = CARTESIAN_POINT('Ctrl Pts',(-26.9018479830977,12.5286846808382,
129.765628188398)) ;
#130222 = CARTESIAN_POINT('Ctrl Pts',(-26.9801291972496,12.7579693374739,
129.961216881114)) ;
#130223 = CARTESIAN_POINT('Ctrl Pts',(-27.0363720503262,13.0352201558529,
130.092378992134)) ;
#130224 = CARTESIAN_POINT('Ctrl Pts',(-27.0671269832124,13.3405827861553,
130.149055244298)) ;
#130225 = CARTESIAN_POINT('Ctrl Pts',(-27.0708970811726,13.6512270836361,
130.126969755603)) ;
#130226 = CARTESIAN_POINT('Ctrl Pts',(-27.0482279288328,13.9458586294117,
130.027616439483)) ;
#130227 = CARTESIAN_POINT('Ctrl Pts',(-27.0012885597917,14.2033946145398,
129.857305947176)) ;
#130228 = CARTESIAN_POINT('Ctrl Pts',(-26.9345407993142,14.4040390929878,
129.629266290777)) ;
#130229 = CARTESIAN_POINT('Ctrl Pts',(-26.85334590466,14.5350227299355,129.359015173723)) ;
#130230 = CARTESIAN_POINT('Ctrl Pts',(-26.7635252041074,14.5864958770583,
129.06333080397)) ;
#130231 = CARTESIAN_POINT('Ctrl Pts',(-26.6736873277468,14.5544169288515,
128.767901047483)) ;
#130232 = CARTESIAN_POINT('Ctrl Pts',(-26.5897148721243,14.4414134411267,
128.489433678146)) ;
#130233 = CARTESIAN_POINT('Ctrl Pts',(-26.5189024761237,14.2551029687745,
128.249417390294)) ;
#130234 = CARTESIAN_POINT('Ctrl Pts',(-26.4670805480505,14.0100365363148,
128.064977335595)) ;
#130235 = CARTESIAN_POINT('Ctrl Pts',(-26.4384400244146,13.7214335689568,
127.948077488775)) ;
#130236 = CARTESIAN_POINT('Ctrl Pts',(-26.435974371304,13.4135493064467,127.907881396188)) ;
#130237 = CARTESIAN_POINT('Ctrl Pts',(-26.4605255580527,13.1045553590735,
127.946402200391)) ;
#130238 = CARTESIAN_POINT('Ctrl Pts',(-26.5108395176121,12.8197359183053,
128.060352490887)) ;
#130239 = CARTESIAN_POINT('Ctrl Pts',(-26.5848090385455,12.5762135336046,
128.243133399849)) ;
#130240 = CARTESIAN_POINT('Ctrl Pts',(-26.6767305633784,12.3952020079458,
128.478624662692)) ;
#130241 = CARTESIAN_POINT('Ctrl Pts',(-26.7816921203493,12.2871509240411,
128.752062073402)) ;
#130242 = CARTESIAN_POINT('Ctrl Pts',(-26.8919186056864,12.260566124011,129.041074313787)) ;
#130243 = CARTESIAN_POINT('Ctrl Pts',(-27.0018360824349,12.3174695873532,
129.328875433493)) ;
#130244 = CARTESIAN_POINT('Ctrl Pts',(-27.1026169626887,12.453509519007,129.590196755254)) ;
#130245 = CARTESIAN_POINT('Ctrl Pts',(-27.1885697033625,12.6588730452131,
129.80817298517)) ;
#130246 = CARTESIAN_POINT('Ctrl Pts',(-27.2540789212245,12.918573180631,129.966479194314)) ;
#130247 = CARTESIAN_POINT('Ctrl Pts',(-27.2953789589594,13.2144046243544,
130.054046631809)) ;
#130248 = CARTESIAN_POINT('Ctrl Pts',(-27.3101837233567,13.5255440796009,
130.064173865051)) ;
#130249 = CARTESIAN_POINT('Ctrl Pts',(-27.2980790148711,13.829753908523,129.995651392622)) ;
#130250 = CARTESIAN_POINT('Ctrl Pts',(-27.2605055755069,14.1049217078337,
129.852691968057)) ;
#130251 = CARTESIAN_POINT('Ctrl Pts',(-27.201449003967,14.3298723137222,129.647191490044)) ;
#130252 = CARTESIAN_POINT('Ctrl Pts',(-27.1249177570824,14.4915527560892,
129.390360258502)) ;
#130253 = CARTESIAN_POINT('Ctrl Pts',(-27.0379228723855,14.5755974314799,
129.103103428759)) ;
#130254 = CARTESIAN_POINT('Ctrl Pts',(-26.9475249321661,14.5774288452973,
128.806022504469)) ;
#130255 = CARTESIAN_POINT('Ctrl Pts',(-26.8602123103374,14.4968431861705,
128.517832330982)) ;
#130256 = CARTESIAN_POINT('Ctrl Pts',(-26.7831288401317,14.338559634622,128.259421353338)) ;
#130257 = CARTESIAN_POINT('Ctrl Pts',(-26.7230100498861,14.1152211662258,
128.050691457082)) ;
#130258 = CARTESIAN_POINT('Ctrl Pts',(-26.6845517589779,13.8419815633955,
127.905190962222)) ;
#130259 = CARTESIAN_POINT('Ctrl Pts',(-26.6713188132477,13.5398086158385,
127.833500347495)) ;
#130260 = CARTESIAN_POINT('Ctrl Pts',(-26.6848767081703,13.2280436814142,
127.839935470396)) ;
#130261 = CARTESIAN_POINT('Ctrl Pts',(-26.7252319504286,12.9300591800615,
127.924625401279)) ;
#130262 = CARTESIAN_POINT('Ctrl Pts',(-26.789898437,12.6684085006953,128.080447400552)) ;
#130263 = CARTESIAN_POINT('Ctrl Pts',(-26.8749504447235,12.4608091979395,
128.295851853874)) ;
#130264 = CARTESIAN_POINT('Ctrl Pts',(-26.9754442077812,12.3214093724075,
128.556266165395)) ;
#130265 = CARTESIAN_POINT('Ctrl Pts',(-27.0849883594925,12.2613303026755,
128.843029640314)) ;
#130266 = CARTESIAN_POINT('Ctrl Pts',(-27.1950704339796,12.2843254889888,
129.131687712862)) ;
#130267 = CARTESIAN_POINT('Ctrl Pts',(-27.300365347957,12.3887269550652,129.406127183944)) ;
#130268 = CARTESIAN_POINT('Ctrl Pts',(-27.3932129896385,12.5673627247375,
129.644228488839)) ;
#130269 = CARTESIAN_POINT('Ctrl Pts',(-27.4678735203102,12.8080166646894,
129.829115438456)) ;
#130270 = CARTESIAN_POINT('Ctrl Pts',(-27.5193391617637,13.0914774239872,
129.946409122059)) ;
#130271 = CARTESIAN_POINT('Ctrl Pts',(-27.5450607387376,13.4005589621793,
129.988284468122)) ;
#130272 = CARTESIAN_POINT('Ctrl Pts',(-27.543724962801,13.7083911586178,129.951439629823)) ;
#130273 = CARTESIAN_POINT('Ctrl Pts',(-27.5161530969791,13.9985991401632,
129.837634676897)) ;
#130274 = CARTESIAN_POINT('Ctrl Pts',(-27.4652173082198,14.2457812582848,
129.655783326903)) ;
#130275 = CARTESIAN_POINT('Ctrl Pts',(-27.3952646502479,14.4345734163401,
129.418349238306)) ;
#130276 = CARTESIAN_POINT('Ctrl Pts',(-27.3117425688963,14.5511370874347,
129.141196953696)) ;
#130277 = CARTESIAN_POINT('Ctrl Pts',(-27.221888274012,14.5867802184263,128.845665992633)) ;
#130278 = CARTESIAN_POINT('Ctrl Pts',(-27.1322077328839,14.5391948509929,
128.550515130345)) ;
#130279 = CARTESIAN_POINT('Ctrl Pts',(-27.0503290364503,14.4115345503253,
128.278202231081)) ;
#130280 = CARTESIAN_POINT('Ctrl Pts',(-26.9827628806094,14.2134356096031,
128.047738422895)) ;
#130281 = CARTESIAN_POINT('Ctrl Pts',(-26.9348844871769,13.9582378109792,
127.874714631013)) ;
#130282 = CARTESIAN_POINT('Ctrl Pts',(-26.9110599740153,13.6646543280563,
127.771965764763)) ;
#130283 = CARTESIAN_POINT('Ctrl Pts',(-26.91366722638,13.3541837462344,127.746474671201)) ;
#130284 = CARTESIAN_POINT('Ctrl Pts',(-26.9432027330941,13.0484270052538,
127.799627992835)) ;
#130285 = CARTESIAN_POINT('Ctrl Pts',(-26.9984107380162,12.7694396720145,
127.927751926342)) ;
#130286 = CARTESIAN_POINT('Ctrl Pts',(-27.0755390330106,12.5380418317107,
128.120059948438)) ;
#130287 = CARTESIAN_POINT('Ctrl Pts',(-27.171221668837,12.3683286468607,128.366208709594)) ;
#130288 = CARTESIAN_POINT('Ctrl Pts',(-27.2771022295698,12.276042045724,128.642572712994)) ;
#130289 = CARTESIAN_POINT('Ctrl Pts',(-27.3880887650464,12.2649171865401,
128.933659578238)) ;
#130290 = CARTESIAN_POINT('Ctrl Pts',(-27.4963674529684,12.3368690244089,
129.216857680154)) ;
#130291 = CARTESIAN_POINT('Ctrl Pts',(-27.5952212736886,12.4871141807711,
129.472423974844)) ;
#130292 = CARTESIAN_POINT('Ctrl Pts',(-27.6777148254917,12.7041604883304,
129.680290662464)) ;
#130293 = CARTESIAN_POINT('Ctrl Pts',(-27.7389269911776,12.9721741232452,
129.826038291155)) ;
#130294 = CARTESIAN_POINT('Ctrl Pts',(-27.7753612070752,13.2726901834042,
129.899369582598)) ;
#130295 = CARTESIAN_POINT('Ctrl Pts',(-27.7850730785568,13.5844633646991,
129.894589911837)) ;
#130296 = CARTESIAN_POINT('Ctrl Pts',(-27.7678692054937,13.8852369971297,
129.811108822555)) ;
#130297 = CARTESIAN_POINT('Ctrl Pts',(-27.7261471250055,14.1508959663415,
129.656248903553)) ;
#130298 = CARTESIAN_POINT('Ctrl Pts',(-27.6632436611501,14.3659569774688,
129.43934922914)) ;
#130299 = CARTESIAN_POINT('Ctrl Pts',(-27.5842577970922,14.5133844128615,
129.175402290824)) ;
#130300 = CARTESIAN_POINT('Ctrl Pts',(-27.4963291774889,14.5822824831324,
128.885527648374)) ;
#130301 = CARTESIAN_POINT('Ctrl Pts',(-27.405500321609,14.5684017849453,128.586993900287)) ;
#130302 = CARTESIAN_POINT('Ctrl Pts',(-27.319795130659,14.4726240674175,128.303557584134)) ;
#130303 = CARTESIAN_POINT('Ctrl Pts',(-27.2454365186279,14.3009018680156,
128.053107574427)) ;
#130304 = CARTESIAN_POINT('Ctrl Pts',(-27.1892164396155,14.06766624957,127.855870686258)) ;
#130305 = CARTESIAN_POINT('Ctrl Pts',(-27.1551562261205,13.7867923876229,
127.723158502822)) ;
#130306 = CARTESIAN_POINT('Ctrl Pts',(-27.1469288346791,13.4808116155242,
127.666034034963)) ;
#130307 = CARTESIAN_POINT('Ctrl Pts',(-27.1655283118666,13.170617767173,127.687268480993)) ;
#130308 = CARTESIAN_POINT('Ctrl Pts',(-27.2108436491157,12.8770484299103,
127.786367681697)) ;
#130309 = CARTESIAN_POINT('Ctrl Pts',(-27.2794629869719,12.6251910653491,
127.95386304123)) ;
#130310 = CARTESIAN_POINT('Ctrl Pts',(-27.3679175166217,12.4289584805404,
128.179147517579)) ;
#130311 = CARTESIAN_POINT('Ctrl Pts',(-27.4707943397875,12.3038002389648,
128.446461935893)) ;
#130312 = CARTESIAN_POINT('Ctrl Pts',(-27.5806821586256,12.2593442697271,
128.734384059874)) ;
#130313 = CARTESIAN_POINT('Ctrl Pts',(-27.6906991544956,12.297889877657,129.022718858313)) ;
#130314 = CARTESIAN_POINT('Ctrl Pts',(-27.7941126443979,12.4169444300621,
129.291685993974)) ;
#130315 = CARTESIAN_POINT('Ctrl Pts',(-27.8842880110467,12.6093773199724,
129.521822960951)) ;
#130316 = CARTESIAN_POINT('Ctrl Pts',(-27.9544400462606,12.858373409298,129.693747600172)) ;
#130317 = CARTESIAN_POINT('Ctrl Pts',(-28.0012932497617,13.1480449631144,
129.797538916571)) ;
#130318 = CARTESIAN_POINT('Ctrl Pts',(-28.0219611305027,13.4582417774946,
129.824751677157)) ;
#130319 = CARTESIAN_POINT('Ctrl Pts',(-28.0155964008347,13.7655078893865,
129.773039846849)) ;
#130320 = CARTESIAN_POINT('Ctrl Pts',(-27.9834174873497,14.0483169401814,
129.645907135585)) ;
#130321 = CARTESIAN_POINT('Ctrl Pts',(-27.9285710178481,14.2859989758831,
129.45261104353)) ;
#130322 = CARTESIAN_POINT('Ctrl Pts',(-27.855464240207,14.4624790270523,129.205887839955)) ;
#130323 = CARTESIAN_POINT('Ctrl Pts',(-27.7701186641137,14.5642183790962,
128.923397956241)) ;
#130324 = CARTESIAN_POINT('Ctrl Pts',(-27.6798082098764,14.5841609537885,
128.626534158212)) ;
#130325 = CARTESIAN_POINT('Ctrl Pts',(-27.5910388931153,14.5209707585958,
128.334043392546)) ;
#130326 = CARTESIAN_POINT('Ctrl Pts',(-27.5114075236351,14.3791779816594,
128.068312186743)) ;
#130327 = CARTESIAN_POINT('Ctrl Pts',(-27.4471074600154,14.1688152035408,
127.847338449402)) ;
#130328 = CARTESIAN_POINT('Ctrl Pts',(-27.4035904915364,13.905195794164,127.687104563405)) ;
#130329 = CARTESIAN_POINT('Ctrl Pts',(-27.384611020138,13.6071501662918,127.598555977474)) ;
#130330 = CARTESIAN_POINT('Ctrl Pts',(-27.3922962592168,13.2953844839231,
127.587845500422)) ;
#130331 = CARTESIAN_POINT('Ctrl Pts',(-27.4268849846127,12.9930170511922,
127.655749387647)) ;
#130332 = CARTESIAN_POINT('Ctrl Pts',(-27.4863412339869,12.7222274559466,
127.796397689186)) ;
#130333 = CARTESIAN_POINT('Ctrl Pts',(-27.5675596487005,12.5005441594065,
128.000493530296)) ;
#130334 = CARTESIAN_POINT('Ctrl Pts',(-27.6655029278047,12.3451353729422,
128.25339244165)) ;
#130335 = CARTESIAN_POINT('Ctrl Pts',(-27.7729606560881,12.2674914409628,
128.534295667148)) ;
#130336 = CARTESIAN_POINT('Ctrl Pts',(-27.8843595706386,12.2722652498167,
128.826484838542)) ;
#130337 = CARTESIAN_POINT('Ctrl Pts',(-27.9913638557461,12.3599738059354,
129.105934292724)) ;
#130338 = CARTESIAN_POINT('Ctrl Pts',(-28.0869339569718,12.5226377882888,
129.352153264961)) ;
#130339 = CARTESIAN_POINT('Ctrl Pts',(-28.1660588301959,12.7508221881861,
129.550110967057)) ;
#130340 = CARTESIAN_POINT('Ctrl Pts',(-28.2230720094142,13.0279564689842,
129.683425341747)) ;
#130341 = CARTESIAN_POINT('Ctrl Pts',(-28.2544101794435,13.3323086828982,
129.741867809916)) ;
#130342 = CARTESIAN_POINT('Ctrl Pts',(-28.2589445257815,13.6420773453948,
129.722122425532)) ;
#130343 = CARTESIAN_POINT('Ctrl Pts',(-28.2370620629136,13.9374077798728,
129.625077365952)) ;
#130344 = CARTESIAN_POINT('Ctrl Pts',(-28.1908166629315,14.1965319026708,
129.456785919999)) ;
#130345 = CARTESIAN_POINT('Ctrl Pts',(-28.1241408657345,14.3999725565714,
129.228766463816)) ;
#130346 = CARTESIAN_POINT('Ctrl Pts',(-28.0436674073878,14.5320840030957,
128.960801672885)) ;
#130347 = CARTESIAN_POINT('Ctrl Pts',(-27.9541399262844,14.5862914480512,
128.666024910394)) ;
#130348 = CARTESIAN_POINT('Ctrl Pts',(-27.8637234344466,14.5562373226541,
128.368717388047)) ;
#130349 = CARTESIAN_POINT('Ctrl Pts',(-27.7799959913736,14.4460760144195,
128.091169611102)) ;
#130350 = CARTESIAN_POINT('Ctrl Pts',(-27.7083901687493,14.2613118721967,
127.848714187468)) ;
#130351 = CARTESIAN_POINT('Ctrl Pts',(-27.6559630033685,14.0168342944474,
127.662425250751)) ;
#130352 = CARTESIAN_POINT('Ctrl Pts',(-27.6267508456225,13.7314084897265,
127.5441079102)) ;
#130353 = CARTESIAN_POINT('Ctrl Pts',(-27.6234740932792,13.421392773908,127.501273878671)) ;
#130354 = CARTESIAN_POINT('Ctrl Pts',(-27.6471850767089,13.1138964793829,
127.537539991659)) ;
#130355 = CARTESIAN_POINT('Ctrl Pts',(-27.6968203365939,12.8273574977414,
127.649425077265)) ;
#130356 = CARTESIAN_POINT('Ctrl Pts',(-27.7702606510501,12.5821904329902,
127.830639707684)) ;
#130357 = CARTESIAN_POINT('Ctrl Pts',(-27.861839260569,12.3992406705926,128.065098381216)) ;
#130358 = CARTESIAN_POINT('Ctrl Pts',(-27.9661679392864,12.289263542394,128.336801966784)) ;
#130359 = CARTESIAN_POINT('Ctrl Pts',(-28.0765570656966,12.260188272694,128.626216040664)) ;
#130360 = CARTESIAN_POINT('Ctrl Pts',(-28.1862199043233,12.3144490228481,
128.913396049941)) ;
#130361 = CARTESIAN_POINT('Ctrl Pts',(-28.2874611534108,12.4481500069378,
129.176032982046)) ;
#130362 = CARTESIAN_POINT('Ctrl Pts',(-28.3739963556883,12.6515764939739,
129.395704973391)) ;
#130363 = CARTESIAN_POINT('Ctrl Pts',(-28.4404957092632,12.9112089841373,
129.556741445295)) ;
#130364 = CARTESIAN_POINT('Ctrl Pts',(-28.4824385774787,13.2069679929226,
129.646128611396)) ;
#130365 = CARTESIAN_POINT('Ctrl Pts',(-28.4979265928733,13.5165269909875,
129.658410386569)) ;
#130366 = CARTESIAN_POINT('Ctrl Pts',(-28.4864805841876,13.8224960289794,
129.591668568529)) ;
#130367 = CARTESIAN_POINT('Ctrl Pts',(-28.4497259503042,14.0973149318537,
129.451272234263)) ;
#130368 = CARTESIAN_POINT('Ctrl Pts',(-28.3911415052306,14.3244517336708,
129.24707906695)) ;
#130369 = CARTESIAN_POINT('Ctrl Pts',(-28.3151295314421,14.4877799140032,
128.99182597903)) ;
#130370 = CARTESIAN_POINT('Ctrl Pts',(-28.2284706441736,14.5742904717488,
128.705587672482)) ;
#130371 = CARTESIAN_POINT('Ctrl Pts',(-28.1376899133625,14.5785355539825,
128.407248586976)) ;
#130372 = CARTESIAN_POINT('Ctrl Pts',(-28.0503077690536,14.4999983626793,
128.118890382677)) ;
#130373 = CARTESIAN_POINT('Ctrl Pts',(-27.9731621173562,14.3447574910545,
127.860457559928)) ;
#130374 = CARTESIAN_POINT('Ctrl Pts',(-27.9122294488622,14.1223925047645,
127.64922484791)) ;
#130375 = CARTESIAN_POINT('Ctrl Pts',(-27.8731709084535,13.8510687474612,
127.502062113222)) ;
#130376 = CARTESIAN_POINT('Ctrl Pts',(-27.8590929134541,13.5484337104113,
127.427784531783)) ;
#130377 = CARTESIAN_POINT('Ctrl Pts',(-27.8719163776156,13.237024252248,127.432120494693)) ;
#130378 = CARTESIAN_POINT('Ctrl Pts',(-27.9113445504404,12.9391312355254,
127.514195973746)) ;
#130379 = CARTESIAN_POINT('Ctrl Pts',(-27.9753555068171,12.6756661013292,
127.668058674229)) ;
#130380 = CARTESIAN_POINT('Ctrl Pts',(-28.0601115514291,12.465702834837,127.88251153638)) ;
#130381 = CARTESIAN_POINT('Ctrl Pts',(-28.1601996212556,12.3244745737951,
128.141765929243)) ;
#130382 = CARTESIAN_POINT('Ctrl Pts',(-28.2690911173844,12.261923279364,128.426769586932)) ;
#130383 = CARTESIAN_POINT('Ctrl Pts',(-28.3800087348888,12.2825882232678,
128.717633267237)) ;
#130384 = CARTESIAN_POINT('Ctrl Pts',(-28.4852015134817,12.3846500947886,
128.991882531666)) ;
#130385 = CARTESIAN_POINT('Ctrl Pts',(-28.5784888744531,12.5611186866008,
129.231275217992)) ;
#130386 = CARTESIAN_POINT('Ctrl Pts',(-28.6537672249704,12.8001288642586,
129.417975019435)) ;
#130387 = CARTESIAN_POINT('Ctrl Pts',(-28.7059764335205,13.0829558196603,
129.537398073433)) ;
#130388 = CARTESIAN_POINT('Ctrl Pts',(-28.7324492944742,13.3903655314665,
129.581607157294)) ;
#130389 = CARTESIAN_POINT('Ctrl Pts',(-28.7319069972317,13.7001366120665,
129.546896868265)) ;
#130390 = CARTESIAN_POINT('Ctrl Pts',(-28.7051802274337,13.9898881855453,
129.435719523823)) ;
#130391 = CARTESIAN_POINT('Ctrl Pts',(-28.6548256890378,14.2391934633215,
129.255489830682)) ;
#130392 = CARTESIAN_POINT('Ctrl Pts',(-28.5854484722084,14.4298567311308,
129.019774640516)) ;
#130393 = CARTESIAN_POINT('Ctrl Pts',(-28.5017241019675,14.549247146468,128.741836021843)) ;
#130394 = CARTESIAN_POINT('Ctrl Pts',(-28.4122620032697,14.5868020953667,
128.447568519666)) ;
#130395 = CARTESIAN_POINT('Ctrl Pts',(-28.3225462061262,14.5417975168182,
128.15234527836)) ;
#130396 = CARTESIAN_POINT('Ctrl Pts',(-28.2403119417274,14.4162088309709,
127.878972537112)) ;
#130397 = CARTESIAN_POINT('Ctrl Pts',(-28.1722916779625,14.2204083444341,
127.647230902494)) ;
#130398 = CARTESIAN_POINT('Ctrl Pts',(-28.1235425964528,13.9647701488693,
127.471442670808)) ;
#130399 = CARTESIAN_POINT('Ctrl Pts',(-28.0992051057573,13.6739289079279,
127.367425886203)) ;
#130400 = CARTESIAN_POINT('Ctrl Pts',(-28.1010246977608,13.3623285568061,
127.339487139088)) ;
#130401 = CARTESIAN_POINT('Ctrl Pts',(-28.1297460934695,13.0574725166072,
127.39040500141)) ;
#130402 = CARTESIAN_POINT('Ctrl Pts',(-28.1841421871714,12.7770677802999,
127.516143688262)) ;
#130403 = CARTESIAN_POINT('Ctrl Pts',(-28.2613693483408,12.5427865648713,
127.708501576232)) ;
#130404 = CARTESIAN_POINT('Ctrl Pts',(-28.3554333317346,12.3731888767337,
127.950342074124)) ;
#130405 = CARTESIAN_POINT('Ctrl Pts',(-28.4616743353883,12.2773794535172,
128.227548370542)) ;
#130406 = CARTESIAN_POINT('Ctrl Pts',(-28.5729382888434,12.2641879567031,
128.519360391861)) ;
#130407 = CARTESIAN_POINT('Ctrl Pts',(-28.6810056913039,12.3335960199066,
128.802056791109)) ;
#130408 = CARTESIAN_POINT('Ctrl Pts',(-28.7802524593645,12.481561593043,129.058771350839)) ;
#130409 = CARTESIAN_POINT('Ctrl Pts',(-28.8633376120415,12.6968286383091,
129.268361232323)) ;
#130410 = CARTESIAN_POINT('Ctrl Pts',(-28.9253336378422,12.9642189214816,
129.416324935008)) ;
#130411 = CARTESIAN_POINT('Ctrl Pts',(-28.9624937310787,13.2637553890215,
129.491819397087)) ;
#130412 = CARTESIAN_POINT('Ctrl Pts',(-28.972907528442,13.576692280422,129.488959145133)) ;
#130413 = CARTESIAN_POINT('Ctrl Pts',(-28.9566596492702,13.8753721133811,
129.408582768456)) ;
#130414 = CARTESIAN_POINT('Ctrl Pts',(-28.9153488774168,14.1446744627024,
129.254642514762)) ;
#130415 = CARTESIAN_POINT('Ctrl Pts',(-28.8529986443521,14.36064855191,129.039430067817)) ;
#130416 = CARTESIAN_POINT('Ctrl Pts',(-28.7746869988663,14.5100785493016,
128.777556943832)) ;
#130417 = CARTESIAN_POINT('Ctrl Pts',(-28.6862473882598,14.5815775750292,
128.485933784396)) ;
#130418 = CARTESIAN_POINT('Ctrl Pts',(-28.5960567042962,14.5700420013307,
128.189517892522)) ;
#130419 = CARTESIAN_POINT('Ctrl Pts',(-28.5097083215572,14.4761038026697,
127.90403247577)) ;
#130420 = CARTESIAN_POINT('Ctrl Pts',(-28.4353102169461,14.307434697937,127.653662973433)) ;
#130421 = CARTESIAN_POINT('Ctrl Pts',(-28.3780629448932,14.0735726732338,
127.453120130801)) ;
#130422 = CARTESIAN_POINT('Ctrl Pts',(-28.3437086879326,13.7966475167134,
127.319908828553)) ;
#130423 = CARTESIAN_POINT('Ctrl Pts',(-28.3345516471301,13.4894705902725,
127.259873174334)) ;
#130424 = CARTESIAN_POINT('Ctrl Pts',(-28.3523600420796,13.1800818840159,
127.278908994309)) ;
#130425 = CARTESIAN_POINT('Ctrl Pts',(-28.3968933889525,12.8853356480997,
127.375690302013)) ;
#130426 = CARTESIAN_POINT('Ctrl Pts',(-28.4649418587295,12.6318026190054,
127.541487159906)) ;
#130427 = CARTESIAN_POINT('Ctrl Pts',(-28.5529364364977,12.4337108597235,
127.765417467458)) ;
#130428 = CARTESIAN_POINT('Ctrl Pts',(-28.6552780292447,12.3064394733644,
128.031235084983)) ;
#130429 = CARTESIAN_POINT('Ctrl Pts',(-28.7653696886047,12.2594672530152,
128.319652084352)) ;
#130430 = CARTESIAN_POINT('Ctrl Pts',(-28.8753666720429,12.2954707768407,
128.607972520882)) ;
#130431 = CARTESIAN_POINT('Ctrl Pts',(-28.979671778032,12.4135506766909,128.879323664204)) ;
#130432 = CARTESIAN_POINT('Ctrl Pts',(-29.0691225992057,12.6014761735562,
129.10779578289)) ;
#130433 = CARTESIAN_POINT('Ctrl Pts',(-29.1405896682972,12.8505488639341,
129.283303377178)) ;
#130434 = CARTESIAN_POINT('Ctrl Pts',(-29.1880749546232,13.1393106596108,
129.388963361721)) ;
#130435 = CARTESIAN_POINT('Ctrl Pts',(-29.2095406027946,13.4495612540633,
129.41846797085)) ;
#130436 = CARTESIAN_POINT('Ctrl Pts',(-29.2039386729016,13.7566530786408,
129.369046592978)) ;
#130437 = CARTESIAN_POINT('Ctrl Pts',(-29.1725100853546,14.0404143241467,
129.244112794232)) ;
#130438 = CARTESIAN_POINT('Ctrl Pts',(-29.118290079075,14.2798567692648,129.052639875831)) ;
#130439 = CARTESIAN_POINT('Ctrl Pts',(-29.0452671941991,14.458860759646,128.806015875749)) ;
#130440 = CARTESIAN_POINT('Ctrl Pts',(-28.9606501594039,14.5622468001176,
128.525844912294)) ;
#130441 = CARTESIAN_POINT('Ctrl Pts',(-28.8700482731633,14.5847589339645,
128.227997078051)) ;
#130442 = CARTESIAN_POINT('Ctrl Pts',(-28.781392052291,14.5239999698819,127.935939206979)) ;
#130443 = CARTESIAN_POINT('Ctrl Pts',(-28.7012903847953,14.3842926564904,
127.668789039323)) ;
#130444 = CARTESIAN_POINT('Ctrl Pts',(-28.6365025896643,14.1758059968765,
127.446409369018)) ;
#130445 = CARTESIAN_POINT('Ctrl Pts',(-28.5922392795345,13.9130885413349,
127.283943329095)) ;
#130446 = CARTESIAN_POINT('Ctrl Pts',(-28.5725792909746,13.615158117942,127.193350804081)) ;
#130447 = CARTESIAN_POINT('Ctrl Pts',(-28.5794652562286,13.3050555466183,
127.180474632891)) ;
#130448 = CARTESIAN_POINT('Ctrl Pts',(-28.6132034548497,13.0018872896554,
127.245876417844)) ;
#130449 = CARTESIAN_POINT('Ctrl Pts',(-28.6721407618882,12.7291798994599,
127.384921051073)) ;
#130450 = CARTESIAN_POINT('Ctrl Pts',(-28.7527600784641,12.5061727549264,
127.587299193783)) ;
#130451 = CARTESIAN_POINT('Ctrl Pts',(-28.8499185291111,12.3489726739453,
127.838024044716)) ;
#130452 = CARTESIAN_POINT('Ctrl Pts',(-28.9575837943938,12.2685650260664,
128.119403625798)) ;
#130453 = CARTESIAN_POINT('Ctrl Pts',(-29.0685724130936,12.2709027283838,
128.410520048629)) ;
#130454 = CARTESIAN_POINT('Ctrl Pts',(-29.1758527905754,12.3558099877511,
128.690771136075)) ;
#130455 = CARTESIAN_POINT('Ctrl Pts',(-29.2723093402486,12.5172181290402,
128.939417104886)) ;
#130456 = CARTESIAN_POINT('Ctrl Pts',(-29.3517344944281,12.7432704544133,
129.138342295771)) ;
#130457 = CARTESIAN_POINT('Ctrl Pts',(-29.4093349032086,13.0180146572784,
129.273499224363)) ;
#130458 = CARTESIAN_POINT('Ctrl Pts',(-29.4416696464702,13.3228198676384,
129.334738648409)) ;
#130459 = CARTESIAN_POINT('Ctrl Pts',(-29.4469785768553,13.6334361388998,
129.31718165255)) ;
#130460 = CARTESIAN_POINT('Ctrl Pts',(-29.425802066603,13.9294162640336,129.222205017795)) ;
#130461 = CARTESIAN_POINT('Ctrl Pts',(-29.3803607950668,14.1891569843553,
129.05635848618)) ;
#130462 = CARTESIAN_POINT('Ctrl Pts',(-29.3142875101324,14.3946401780078,
128.830106500029)) ;
#130463 = CARTESIAN_POINT('Ctrl Pts',(-29.2338335030574,14.529556883976,128.562067703441)) ;
#130464 = CARTESIAN_POINT('Ctrl Pts',(-29.1443491687741,14.5858061305694,
128.267386240536)) ;
#130465 = CARTESIAN_POINT('Ctrl Pts',(-29.0543546782956,14.5585141813688,
127.971498106513)) ;
#130466 = CARTESIAN_POINT('Ctrl Pts',(-28.9698827692536,14.4500372288901,
127.691587731276)) ;
#130467 = CARTESIAN_POINT('Ctrl Pts',(-28.8982435279839,14.2682020295539,
127.449226628376)) ;
#130468 = CARTESIAN_POINT('Ctrl Pts',(-28.8449675977318,14.0250734212292,
127.260391247175)) ;
#130469 = CARTESIAN_POINT('Ctrl Pts',(-28.8149686665018,13.7389393527222,
127.139599745821)) ;
#130470 = CARTESIAN_POINT('Ctrl Pts',(-28.8110043888609,13.4311036991076,
127.094955672536)) ;
#130471 = CARTESIAN_POINT('Ctrl Pts',(-28.8337924395339,13.1229020252546,
127.128494988837)) ;
#130472 = CARTESIAN_POINT('Ctrl Pts',(-28.8832606513019,12.8333723826346,
127.239628018119)) ;
#130473 = CARTESIAN_POINT('Ctrl Pts',(-28.9553257919547,12.5895126808553,
127.417194804428)) ;
#130474 = CARTESIAN_POINT('Ctrl Pts',(-29.0466937510159,12.4035405044014,
127.650907478714)) ;
#130475 = CARTESIAN_POINT('Ctrl Pts',(-29.1507398374928,12.2914040543739,
127.921795177575)) ;
#130476 = CARTESIAN_POINT('Ctrl Pts',(-29.2611690696662,12.2598122660064,
128.2112892169)) ;
#130477 = CARTESIAN_POINT('Ctrl Pts',(-29.3710266223058,12.3118570092467,
128.499018026177)) ;
#130478 = CARTESIAN_POINT('Ctrl Pts',(-29.4723911564959,12.4430958477667,
128.762082814677)) ;
#130479 = CARTESIAN_POINT('Ctrl Pts',(-29.5595187815204,12.6447072106669,
128.983465986791)) ;
#130480 = CARTESIAN_POINT('Ctrl Pts',(-29.6266409499539,12.9030426443817,
129.146318264826)) ;
#130481 = CARTESIAN_POINT('Ctrl Pts',(-29.6693091154689,13.1970328357363,
129.237929001175)) ;
#130482 = CARTESIAN_POINT('Ctrl Pts',(-29.685629423096,13.508431210418,129.252425328306)) ;
#130483 = CARTESIAN_POINT('Ctrl Pts',(-29.6750927790816,13.8121186853756,
129.18865319137)) ;
#130484 = CARTESIAN_POINT('Ctrl Pts',(-29.6389283245049,14.0900961116511,
129.049754658892)) ;
#130485 = CARTESIAN_POINT('Ctrl Pts',(-29.5808923584998,14.3187298480659,
128.847179665827)) ;
#130486 = CARTESIAN_POINT('Ctrl Pts',(-29.5050756594598,14.4844226501879,
128.592406122416)) ;
#130487 = CARTESIAN_POINT('Ctrl Pts',(-29.4189800280682,14.5727758610145,
128.307951714936)) ;
#130488 = CARTESIAN_POINT('Ctrl Pts',(-29.3282101502383,14.5796460652876,
128.00963807517)) ;
#130489 = CARTESIAN_POINT('Ctrl Pts',(-29.2405915893346,14.5035866280562,
127.720582538253)) ;
#130490 = CARTESIAN_POINT('Ctrl Pts',(-29.1627463131859,14.3497064261521,
127.459966008998)) ;
#130491 = CARTESIAN_POINT('Ctrl Pts',(-29.1014315581632,14.1291331402223,
127.247667595512)) ;
#130492 = CARTESIAN_POINT('Ctrl Pts',(-29.0617835084594,13.8597728320795,
127.098872760759)) ;
#130493 = CARTESIAN_POINT('Ctrl Pts',(-29.0469138734206,13.5574625507345,
127.022250060698)) ;
#130494 = CARTESIAN_POINT('Ctrl Pts',(-29.0589124808749,13.2463367213565,
127.024215607838)) ;
#130495 = CARTESIAN_POINT('Ctrl Pts',(-29.0976581896989,12.9472974934633,
127.104242355792)) ;
#130496 = CARTESIAN_POINT('Ctrl Pts',(-29.1607751106638,12.6832079210241,
127.255592028414)) ;
#130497 = CARTESIAN_POINT('Ctrl Pts',(-29.2453851104306,12.4704983369195,
127.469462912104)) ;
#130498 = CARTESIAN_POINT('Ctrl Pts',(-29.3447716639353,12.3276823761117,
127.726790304496)) ;
#130499 = CARTESIAN_POINT('Ctrl Pts',(-29.4537157894357,12.2625925296001,
128.011876171548)) ;
#130500 = CARTESIAN_POINT('Ctrl Pts',(-29.5643047349069,12.2806191987991,
128.301897217799)) ;
#130501 = CARTESIAN_POINT('Ctrl Pts',(-29.6704487959945,12.3809214254249,
128.57871127182)) ;
#130502 = CARTESIAN_POINT('Ctrl Pts',(-29.76412340717,12.5560400663307,128.819213425397)) ;
#130503 = CARTESIAN_POINT('Ctrl Pts',(-29.8395060734412,12.7918900929914,
129.006436877495)) ;
#130504 = CARTESIAN_POINT('Ctrl Pts',(-29.8926354306049,13.0744209302394,
129.128450455972)) ;
#130505 = CARTESIAN_POINT('Ctrl Pts',(-29.9198456862715,13.3812416408414,
129.174838109595)) ;
#130506 = CARTESIAN_POINT('Ctrl Pts',(-29.9200785827897,13.6920796910028,
129.14230522542)) ;
#130507 = CARTESIAN_POINT('Ctrl Pts',(-29.8939694883016,13.9824941646698,
129.032937034259)) ;
#130508 = CARTESIAN_POINT('Ctrl Pts',(-29.8445055241324,14.2323227439513,
128.855452218984)) ;
#130509 = CARTESIAN_POINT('Ctrl Pts',(-29.7751603262968,14.4258243504284,
128.619628402019)) ;
#130510 = CARTESIAN_POINT('Ctrl Pts',(-29.6924818729896,14.5465247241855,
128.345045148463)) ;
#130511 = CARTESIAN_POINT('Ctrl Pts',(-29.6022812245865,14.5869806831231,
128.048301947459)) ;
#130512 = CARTESIAN_POINT('Ctrl Pts',(-29.5129647804047,14.5442058467449,
127.754432704675)) ;
#130513 = CARTESIAN_POINT('Ctrl Pts',(-29.4302326997558,14.4209679616749,
127.479549414334)) ;
#130514 = CARTESIAN_POINT('Ctrl Pts',(-29.361544244752,14.2257906653135,127.245713957041)) ;
#130515 = CARTESIAN_POINT('Ctrl Pts',(-29.3126320686624,13.9741287874761,
127.06978287009)) ;
#130516 = CARTESIAN_POINT('Ctrl Pts',(-29.2873078566729,13.6829512743861,
126.962726744081)) ;
#130517 = CARTESIAN_POINT('Ctrl Pts',(-29.2883658599329,13.3714665722058,
126.9325602086)) ;
#130518 = CARTESIAN_POINT('Ctrl Pts',(-29.3163871008899,13.0656059038766,
126.981368852155)) ;
#130519 = CARTESIAN_POINT('Ctrl Pts',(-29.3699746758538,12.7850335054103,
127.104838856256)) ;
#130520 = CARTESIAN_POINT('Ctrl Pts',(-29.4462187184721,12.54966734435,127.294443632792)) ;
#130521 = CARTESIAN_POINT('Ctrl Pts',(-29.5405084491528,12.3766688899815,
127.536703010351)) ;
#130522 = CARTESIAN_POINT('Ctrl Pts',(-29.6465183988453,12.2789529397111,
127.813246121849)) ;
#130523 = CARTESIAN_POINT('Ctrl Pts',(-29.7575529820162,12.2634413447035,
128.104442432783)) ;
#130524 = CARTESIAN_POINT('Ctrl Pts',(-29.8658142138442,12.3304156583785,
128.387703279497)) ;
#130525 = CARTESIAN_POINT('Ctrl Pts',(-29.9657429019495,12.477034323666,128.646289139449)) ;
#130526 = CARTESIAN_POINT('Ctrl Pts',(-30.04889523573,12.6896429302191,128.856241956516)) ;
#130527 = CARTESIAN_POINT('Ctrl Pts',(-30.1115928889291,12.9554490393123,
129.006277363579)) ;
#130528 = CARTESIAN_POINT('Ctrl Pts',(-30.1495545265171,13.2546654169279,
129.08407484375)) ;
#130529 = CARTESIAN_POINT('Ctrl Pts',(-30.160795972007,13.5672373629207,129.08367315207)) ;
#130530 = CARTESIAN_POINT('Ctrl Pts',(-30.1452246339684,13.867352650113,129.005175262755)) ;
#130531 = CARTESIAN_POINT('Ctrl Pts',(-30.1048447842729,14.1367234867938,
128.854116866161)) ;
#130532 = CARTESIAN_POINT('Ctrl Pts',(-30.042556700534,14.3561275745404,128.638823326171)) ;
#130533 = CARTESIAN_POINT('Ctrl Pts',(-29.9649745078786,14.5065131149989,
128.379260463449)) ;
#130534 = CARTESIAN_POINT('Ctrl Pts',(-29.8769584255218,14.5806176797064,
128.088948707526)) ;
#130535 = CARTESIAN_POINT('Ctrl Pts',(-29.7864336038671,14.5715967155624,
127.791445629283)) ;
#130536 = CARTESIAN_POINT('Ctrl Pts',(-29.69982662067,14.4799161202559,127.505198050496)) ;
#130537 = CARTESIAN_POINT('Ctrl Pts',(-29.6249930783652,14.3130126833991,
127.253530278741)) ;
#130538 = CARTESIAN_POINT('Ctrl Pts',(-29.5674004888477,14.0821692542283,
127.052156703191)) ;
#130539 = CARTESIAN_POINT('Ctrl Pts',(-29.5320652904142,13.8046646113754,
126.915868687298)) ;
#130540 = CARTESIAN_POINT('Ctrl Pts',(-29.522245757931,13.4979411637468,126.85390767621)) ;
#130541 = CARTESIAN_POINT('Ctrl Pts',(-29.5392765293126,13.1889484555023,
126.870727175006)) ;
#130542 = CARTESIAN_POINT('Ctrl Pts',(-29.5829152948127,12.8939178939325,
126.964964143682)) ;
#130543 = CARTESIAN_POINT('Ctrl Pts',(-29.6506193843243,12.6378239616322,
127.129606070988)) ;
#130544 = CARTESIAN_POINT('Ctrl Pts',(-29.738152535917,12.4382802323548,127.352204897437)) ;
#130545 = CARTESIAN_POINT('Ctrl Pts',(-29.8397245266592,12.3092349725469,
127.615912819609)) ;
#130546 = CARTESIAN_POINT('Ctrl Pts',(-29.9500722254853,12.2595575244022,
127.904963057869)) ;
#130547 = CARTESIAN_POINT('Ctrl Pts',(-30.0599627030921,12.2934341290355,
128.193023554747)) ;
#130548 = CARTESIAN_POINT('Ctrl Pts',(-30.1640305325771,12.4080333821748,
128.463876290564)) ;
#130549 = CARTESIAN_POINT('Ctrl Pts',(-30.254996316276,12.5960960444092,128.696398341662)) ;
#130550 = CARTESIAN_POINT('Ctrl Pts',(-30.3266379956478,12.8430835986194,
128.872552220836)) ;
#130551 = CARTESIAN_POINT('Ctrl Pts',(-30.3747931066949,13.1299282695534,
128.980268604815)) ;
#130552 = CARTESIAN_POINT('Ctrl Pts',(-30.3971261320801,13.4413370794651,
129.012154398595)) ;
#130553 = CARTESIAN_POINT('Ctrl Pts',(-30.3922326048791,13.7480777708716,
128.96487811748)) ;
#130554 = CARTESIAN_POINT('Ctrl Pts',(-30.3615407807411,14.0327532731281,
128.842104048057)) ;
#130555 = CARTESIAN_POINT('Ctrl Pts',(-30.3079642325184,14.2736050674125,
128.652532725912)) ;
#130556 = CARTESIAN_POINT('Ctrl Pts',(-30.2353404472758,14.4547314005176,
128.407048833985)) ;
#130557 = CARTESIAN_POINT('Ctrl Pts',(-30.1511026849128,14.560267557326,128.128030852945)) ;
#130558 = CARTESIAN_POINT('Ctrl Pts',(-30.0604947582532,14.5853381835963,
127.830140097985)) ;
#130559 = CARTESIAN_POINT('Ctrl Pts',(-29.9715942466692,14.5268296207526,
127.537332693561)) ;
#130560 = CARTESIAN_POINT('Ctrl Pts',(-29.8911967366192,14.3893358191871,
127.269338442133)) ;
#130561 = CARTESIAN_POINT('Ctrl Pts',(-29.8258710176355,14.1825587760216,
127.045374761125)) ;
#130562 = CARTESIAN_POINT('Ctrl Pts',(-29.7809873413325,13.9213689273391,
126.881125929181)) ;
#130563 = CARTESIAN_POINT('Ctrl Pts',(-29.7605871063278,13.624244891243,126.788376072781)) ;
#130564 = CARTESIAN_POINT('Ctrl Pts',(-29.7665958590195,13.3143405109537,
126.772954857604)) ;
#130565 = CARTESIAN_POINT('Ctrl Pts',(-29.7999614019313,13.0084391813705,
126.837014109222)) ;
#130566 = CARTESIAN_POINT('Ctrl Pts',(-29.8577439349117,12.7371910069822,
126.972993813021)) ;
#130567 = CARTESIAN_POINT('Ctrl Pts',(-29.9380486306226,12.5114338941523,
127.174317241384)) ;
#130568 = CARTESIAN_POINT('Ctrl Pts',(-30.0347895009958,12.3524150089363,
127.423845852049)) ;
#130569 = CARTESIAN_POINT('Ctrl Pts',(-30.1423814173391,12.2696328223672,
127.704969894785)) ;
#130570 = CARTESIAN_POINT('Ctrl Pts',(-30.2533143890773,12.2697667116298,
127.995941819015)) ;
#130571 = CARTESIAN_POINT('Ctrl Pts',(-30.3606289089555,12.3522196481958,
128.276346153937)) ;
#130572 = CARTESIAN_POINT('Ctrl Pts',(-30.4575418534214,12.5116176555494,
128.526307518704)) ;
#130573 = CARTESIAN_POINT('Ctrl Pts',(-30.5375652450921,12.7360826079941,
128.726969342083)) ;
#130574 = CARTESIAN_POINT('Ctrl Pts',(-30.5959763461482,13.0105745884039,
128.864397493548)) ;
#130575 = CARTESIAN_POINT('Ctrl Pts',(-30.6289168911378,13.3146277352433,
128.927438637494)) ;
#130576 = CARTESIAN_POINT('Ctrl Pts',(-30.6349932443909,13.6243830684314,
128.912226450868)) ;
#130577 = CARTESIAN_POINT('Ctrl Pts',(-30.6145002172543,13.9217977302755,
128.819166633438)) ;
#130578 = CARTESIAN_POINT('Ctrl Pts',(-30.5697865145131,14.182101761474,128.655530820559)) ;
#130579 = CARTESIAN_POINT('Ctrl Pts',(-30.5043483601306,14.38941229378,128.431164790754)) ;
#130580 = CARTESIAN_POINT('Ctrl Pts',(-30.4239598225637,14.5268848124279,
128.163207055914)) ;
#130581 = CARTESIAN_POINT('Ctrl Pts',(-30.3349091733917,14.5852561632452,
127.869902527666)) ;
#130582 = CARTESIAN_POINT('Ctrl Pts',(-30.2448016587935,14.5605921487245,
127.573667910456)) ;
#130583 = CARTESIAN_POINT('Ctrl Pts',(-30.1599580712501,14.4542388685168,
127.292630282821)) ;
#130584 = CARTESIAN_POINT('Ctrl Pts',(-30.0878192488777,14.2743936484204,
127.048803788339)) ;
#130585 = CARTESIAN_POINT('Ctrl Pts',(-30.0338404841497,14.0316377347413,
126.857786097763)) ;
#130586 = CARTESIAN_POINT('Ctrl Pts',(-30.0033296373907,13.748755621538,126.735765359026)) ;
#130587 = CARTESIAN_POINT('Ctrl Pts',(-29.9985372111809,13.4387761369995,
126.688426657773)) ;
#130588 = CARTESIAN_POINT('Ctrl Pts',(-30.0205594673105,13.1317846538023,
126.719892013202)) ;
#130589 = CARTESIAN_POINT('Ctrl Pts',(-30.0693092770263,12.8410201849047,
126.828891131929)) ;
#130590 = CARTESIAN_POINT('Ctrl Pts',(-30.1405833793293,12.5963885979045,
127.004236412401)) ;
#130591 = CARTESIAN_POINT('Ctrl Pts',(-30.2312796308035,12.4083250169264,
127.236028455529)) ;
#130592 = CARTESIAN_POINT('Ctrl Pts',(-30.335740326897,12.2932606250205,127.507907427166)) ;
#130593 = CARTESIAN_POINT('Ctrl Pts',(-30.4455648003633,12.2596773195356,
127.795795732775)) ;
#130594 = CARTESIAN_POINT('Ctrl Pts',(-30.5554887651398,12.3089369784701,
128.083738997651)) ;
#130595 = CARTESIAN_POINT('Ctrl Pts',(-30.6576028767063,12.4384178929668,
128.348866404619)) ;
#130596 = CARTESIAN_POINT('Ctrl Pts',(-30.7452784557848,12.6389284156292,
128.571788006726)) ;
#130597 = CARTESIAN_POINT('Ctrl Pts',(-30.8125438621909,12.8936368315776,
128.735337806806)) ;
#130598 = CARTESIAN_POINT('Ctrl Pts',(-30.8563542073147,13.189035253119,128.830024629578)) ;
#130599 = CARTESIAN_POINT('Ctrl Pts',(-30.8733117963159,13.4997523048697,
128.846448825023)) ;
#130600 = CARTESIAN_POINT('Ctrl Pts',(-30.8635035099321,13.80398082463,128.784788851022)) ;
#130601 = CARTESIAN_POINT('Ctrl Pts',(-30.8281975796196,14.0820720991441,
128.648525909069)) ;
#130602 = CARTESIAN_POINT('Ctrl Pts',(-30.7705950246315,14.3130040222785,
128.447121485095)) ;
#130603 = CARTESIAN_POINT('Ctrl Pts',(-30.6955724619812,14.4800544799105,
128.194827012547)) ;
#130604 = CARTESIAN_POINT('Ctrl Pts',(-30.6094796922681,14.5714591728311,
127.910278099775)) ;
#130605 = CARTESIAN_POINT('Ctrl Pts',(-30.5182772146109,14.5804983969621,
127.610538709757)) ;
#130606 = CARTESIAN_POINT('Ctrl Pts',(-30.4309086742145,14.5069052814483,
127.322370946456)) ;
#130607 = CARTESIAN_POINT('Ctrl Pts',(-30.3527812954282,14.3557030567126,
127.060991610997)) ;
#130608 = CARTESIAN_POINT('Ctrl Pts',(-30.290791764377,14.1367620675431,126.846684361694)) ;
#130609 = CARTESIAN_POINT('Ctrl Pts',(-30.2503365492017,13.868069475113,126.695461101934)) ;
#130610 = CARTESIAN_POINT('Ctrl Pts',(-30.2347621394633,13.5652243934133,
126.616661910851)) ;
#130611 = CARTESIAN_POINT('Ctrl Pts',(-30.2459604354312,13.2558697743365,
126.616481401596)) ;
#130612 = CARTESIAN_POINT('Ctrl Pts',(-30.2838897938117,12.9557647499979,
126.694089516615)) ;
#130613 = CARTESIAN_POINT('Ctrl Pts',(-30.3465075080088,12.6900042913403,
126.843917515241)) ;
#130614 = CARTESIAN_POINT('Ctrl Pts',(-30.4302612148162,12.4761056036643,
127.055401271101)) ;
#130615 = CARTESIAN_POINT('Ctrl Pts',(-30.5298042611788,12.3304586966932,
127.313012046257)) ;
#130616 = CARTESIAN_POINT('Ctrl Pts',(-30.6380631716033,12.2634381679405,
127.59626025709)) ;
#130617 = CARTESIAN_POINT('Ctrl Pts',(-30.7489387888862,12.2788783439155,
127.887043779485)) ;
#130618 = CARTESIAN_POINT('Ctrl Pts',(-30.8551974172725,12.3768659519767,
128.164231165451)) ;
#130619 = CARTESIAN_POINT('Ctrl Pts',(-30.9493029249669,12.5495629773897,
128.406018950591)) ;
#130620 = CARTESIAN_POINT('Ctrl Pts',(-31.0257192355162,12.7855771010426,
128.596039753622)) ;
#130621 = CARTESIAN_POINT('Ctrl Pts',(-31.0791447785856,13.0654344689711,
128.719127640439)) ;
#130622 = CARTESIAN_POINT('Ctrl Pts',(-31.10721979407,13.3720088898766,128.768014230976)) ;
#130623 = CARTESIAN_POINT('Ctrl Pts',(-31.1082390144562,13.6824356605847,
128.737845756141)) ;
#130624 = CARTESIAN_POINT('Ctrl Pts',(-31.0830160432829,13.9739144612511,
128.63106921161)) ;
#130625 = CARTESIAN_POINT('Ctrl Pts',(-31.0337088291658,14.2268633656514,
128.453783206045)) ;
#130626 = CARTESIAN_POINT('Ctrl Pts',(-30.9655242077267,14.4204385538483,
128.221677293176)) ;
#130627 = CARTESIAN_POINT('Ctrl Pts',(-30.8824245353142,14.5445800995036,
127.94555557525)) ;
#130628 = CARTESIAN_POINT('Ctrl Pts',(-30.7929153317515,14.5868220519023,
127.65106138528)) ;
#130629 = CARTESIAN_POINT('Ctrl Pts',(-30.7033259864182,14.5468039096368,
127.356334978812)) ;
#130630 = CARTESIAN_POINT('Ctrl Pts',(-30.6200169000235,14.4251034045477,
127.079648615156)) ;
#130631 = CARTESIAN_POINT('Ctrl Pts',(-30.5511679459364,14.2325286601305,
126.845483441192)) ;
#130632 = CARTESIAN_POINT('Ctrl Pts',(-30.5014922994488,13.9823226220566,
126.667300841302)) ;
#130633 = CARTESIAN_POINT('Ctrl Pts',(-30.4754060797272,13.6900857926319,
126.55781575587)) ;
#130634 = CARTESIAN_POINT('Ctrl Pts',(-30.4757515263436,13.3811330388435,
126.525818393865)) ;
#130635 = CARTESIAN_POINT('Ctrl Pts',(-30.5029596486349,13.0742212515847,
126.572184425358)) ;
#130636 = CARTESIAN_POINT('Ctrl Pts',(-30.5559456878785,12.7922256350364,
126.693851892319)) ;
#130637 = CARTESIAN_POINT('Ctrl Pts',(-30.6318353087,12.5548594605115,126.882340820124)) ;
#130638 = CARTESIAN_POINT('Ctrl Pts',(-30.7256332714889,12.3804086732527,
127.123208519804)) ;
#130639 = CARTESIAN_POINT('Ctrl Pts',(-30.8308984098131,12.2809059933595,
127.397727950232)) ;
#130640 = CARTESIAN_POINT('Ctrl Pts',(-30.9417668692838,12.2624888444475,
127.688477101505)) ;
#130641 = CARTESIAN_POINT('Ctrl Pts',(-31.0508252577136,12.3276776788202,
127.973866698083)) ;
#130642 = CARTESIAN_POINT('Ctrl Pts',(-31.1502685162055,12.4707928531316,
128.231326341888)) ;
#130643 = CARTESIAN_POINT('Ctrl Pts',(-31.2345189994147,12.6823313434113,
128.444309921377)) ;
#130644 = CARTESIAN_POINT('Ctrl Pts',(-31.2980256195684,12.9478030946643,
128.596611453119)) ;
#130645 = CARTESIAN_POINT('Ctrl Pts',(-31.3366816217105,13.2466922642525,
128.676406435598)) ;
#130646 = CARTESIAN_POINT('Ctrl Pts',(-31.348613489995,13.5583771774669,128.678110282587)) ;
#130647 = CARTESIAN_POINT('Ctrl Pts',(-31.3338483463751,13.8592555730131,
128.601960259952)) ;
#130648 = CARTESIAN_POINT('Ctrl Pts',(-31.2938314441516,14.130642447192,128.451821693927)) ;
#130649 = CARTESIAN_POINT('Ctrl Pts',(-31.2328517776415,14.3493759206944,
128.240739607194)) ;
#130650 = CARTESIAN_POINT('Ctrl Pts',(-31.1550554986113,14.5035317147663,
127.980260239585)) ;
#130651 = CARTESIAN_POINT('Ctrl Pts',(-31.0673952128672,14.5795844939409,
127.691069205955)) ;
#130652 = CARTESIAN_POINT('Ctrl Pts',(-30.9766712485968,14.5729335746648,
127.39291041864)) ;
#130653 = CARTESIAN_POINT('Ctrl Pts',(-30.8901457754388,14.4838965301244,
127.10702428331)) ;
#130654 = CARTESIAN_POINT('Ctrl Pts',(-30.814690482604,14.3187458157033,126.8534560206)) ;
#130655 = CARTESIAN_POINT('Ctrl Pts',(-30.7566026297993,14.089767661644,126.65067853821)) ;
#130656 = CARTESIAN_POINT('Ctrl Pts',(-30.7205507654139,13.8134083502436,
126.512294932625)) ;
#130657 = CARTESIAN_POINT('Ctrl Pts',(-30.7099213905107,13.507393703558,126.447991813842)) ;
#130658 = CARTESIAN_POINT('Ctrl Pts',(-30.7262164766661,13.1976577760434,
126.46259634103)) ;
#130659 = CARTESIAN_POINT('Ctrl Pts',(-30.7689461273649,12.9027230155048,
126.554284830547)) ;
#130660 = CARTESIAN_POINT('Ctrl Pts',(-30.8360682125386,12.6448108807206,
126.717171534774)) ;
#130661 = CARTESIAN_POINT('Ctrl Pts',(-30.9228749815143,12.4434495892378,
126.937711355592)) ;
#130662 = CARTESIAN_POINT('Ctrl Pts',(-31.0250861654557,12.3113759849424,
127.20298051609)) ;
#130663 = CARTESIAN_POINT('Ctrl Pts',(-31.1341161240077,12.2599503304548,
127.488549607509)) ;
#130664 = CARTESIAN_POINT('Ctrl Pts',(-31.2449686946706,12.2913693198197,
127.779152527576)) ;
#130665 = CARTESIAN_POINT('Ctrl Pts',(-31.3490006777393,12.4038516007803,
128.049992695568)) ;
#130666 = CARTESIAN_POINT('Ctrl Pts',(-31.4401686589773,12.589262648139,128.283203736203)) ;
#130667 = CARTESIAN_POINT('Ctrl Pts',(-31.5125077640223,12.834296673012,128.461424138523)) ;
#130668 = CARTESIAN_POINT('Ctrl Pts',(-31.5616695171324,13.122430570677,128.571832493846)) ;
#130669 = CARTESIAN_POINT('Ctrl Pts',(-31.584572061778,13.4307504343076,128.60568665077)) ;
#130670 = CARTESIAN_POINT('Ctrl Pts',(-31.5805716706129,13.7394115379672,
128.560850441774)) ;
#130671 = CARTESIAN_POINT('Ctrl Pts',(-31.5505589696301,14.0250582462743,
128.440063952068)) ;
#130672 = CARTESIAN_POINT('Ctrl Pts',(-31.4974778440457,14.267685746029,128.251885798625)) ;
#130673 = CARTESIAN_POINT('Ctrl Pts',(-31.425639817206,14.4501343666904,128.008842210201)) ;
#130674 = CARTESIAN_POINT('Ctrl Pts',(-31.3412464001568,14.5585281597601,
127.729196706468)) ;
#130675 = CARTESIAN_POINT('Ctrl Pts',(-31.2509509298363,14.5857500281756,
127.432315546893)) ;
#130676 = CARTESIAN_POINT('Ctrl Pts',(-31.1617583850195,14.5296138402308,
127.138599459681)) ;
#130677 = CARTESIAN_POINT('Ctrl Pts',(-31.0810307993938,14.3940563949584,
126.869634324592)) ;
#130678 = CARTESIAN_POINT('Ctrl Pts',(-31.015365639309,14.1896706789709,126.644769166929)) ;
#130679 = CARTESIAN_POINT('Ctrl Pts',(-30.9697407804104,13.9296796265153,
126.478325815102)) ;
#130680 = CARTESIAN_POINT('Ctrl Pts',(-30.9485581261753,13.632561455883,126.383213941901)) ;
#130681 = CARTESIAN_POINT('Ctrl Pts',(-30.9539104538573,13.3229080728124,
126.365887442255)) ;
#130682 = CARTESIAN_POINT('Ctrl Pts',(-30.9861601219692,13.0185267768755,
126.42692304573)) ;
#130683 = CARTESIAN_POINT('Ctrl Pts',(-31.0436635658604,12.7436674784671,
126.561805226232)) ;
#130684 = CARTESIAN_POINT('Ctrl Pts',(-31.1235774177391,12.516497959597,126.761971689529)) ;
#130685 = CARTESIAN_POINT('Ctrl Pts',(-31.2195573192475,12.3560840678509,
127.009401681164)) ;
#130686 = CARTESIAN_POINT('Ctrl Pts',(-31.3269550981851,12.2708854944156,
127.289950809879)) ;
#130687 = CARTESIAN_POINT('Ctrl Pts',(-31.4377439150536,12.2685611985324,
127.580543137024)) ;
#130688 = CARTESIAN_POINT('Ctrl Pts',(-31.5454598315593,12.3486009329829,
127.862068280233)) ;
#130689 = CARTESIAN_POINT('Ctrl Pts',(-31.6431291831054,12.5069430119851,
128.114092641889)) ;
#130690 = CARTESIAN_POINT('Ctrl Pts',(-31.7231801494414,12.7284058667927,
128.31504662471)) ;
#130691 = CARTESIAN_POINT('Ctrl Pts',(-31.7824884513957,13.0024844630991,
128.454991776573)) ;
#130692 = CARTESIAN_POINT('Ctrl Pts',(-31.8160995644744,13.3053155340302,
128.520072219864)) ;
#130693 = CARTESIAN_POINT('Ctrl Pts',(-31.8229604762739,13.6156286046676,
128.507094948621)) ;
#130694 = CARTESIAN_POINT('Ctrl Pts',(-31.8033478246911,13.9128849150777,
128.416718921952)) ;
#130695 = CARTESIAN_POINT('Ctrl Pts',(-31.7589073492138,14.1766184698676,
128.253605928012)) ;
#130696 = CARTESIAN_POINT('Ctrl Pts',(-31.6940252869537,14.3847398233907,
128.030954151065)) ;
#130697 = CARTESIAN_POINT('Ctrl Pts',(-31.6142724237389,14.523836080727,127.764966919406)) ;
#130698 = CARTESIAN_POINT('Ctrl Pts',(-31.5254919515761,14.5847742986496,
127.47249459861)) ;
#130699 = CARTESIAN_POINT('Ctrl Pts',(-31.4349594358017,14.5623309512569,
127.174878551546)) ;
#130700 = CARTESIAN_POINT('Ctrl Pts',(-31.3499799147985,14.4584178345544,
126.893505314748)) ;
#130701 = CARTESIAN_POINT('Ctrl Pts',(-31.2771464293534,14.2791868966926,
126.647472840431)) ;
#130702 = CARTESIAN_POINT('Ctrl Pts',(-31.2232355329482,14.0415187300811,
126.45712718632)) ;
#130703 = CARTESIAN_POINT('Ctrl Pts',(-31.1915724331804,13.7564325475948,
126.33133935828)) ;
#130704 = CARTESIAN_POINT('Ctrl Pts',(-31.1860350406004,13.4495648633329,
126.282136996625)) ;
#130705 = CARTESIAN_POINT('Ctrl Pts',(-31.207465416303,13.139416785511,126.311549638386)) ;
#130706 = CARTESIAN_POINT('Ctrl Pts',(-31.2549371688994,12.8508801252525,
126.417190090246)) ;
#130707 = CARTESIAN_POINT('Ctrl Pts',(-31.3260883980019,12.6022770135179,
126.591874983273)) ;
#130708 = CARTESIAN_POINT('Ctrl Pts',(-31.4162873476206,12.4127865766784,
126.822257067223)) ;
#130709 = CARTESIAN_POINT('Ctrl Pts',(-31.5204129624464,12.2953916616204,
127.093162819959)) ;
#130710 = CARTESIAN_POINT('Ctrl Pts',(-31.6303913905,12.2594835085984,127.381432512102)) ;
#130711 = CARTESIAN_POINT('Ctrl Pts',(-31.7402120890356,12.3065006883116,
127.669135805987)) ;
#130712 = CARTESIAN_POINT('Ctrl Pts',(-31.8423834591039,12.4331949818184,
127.934527475475)) ;
#130713 = CARTESIAN_POINT('Ctrl Pts',(-31.9308910035952,12.6325250875222,
128.159756985898)) ;
#130714 = CARTESIAN_POINT('Ctrl Pts',(-31.9986534951646,12.8854153645511,
128.324824636163)) ;
#130715 = CARTESIAN_POINT('Ctrl Pts',(-32.0432416690704,13.1803566291491,
128.421740282294)) ;
#130716 = CARTESIAN_POINT('Ctrl Pts',(-32.0609557105027,13.4893560631302,
128.440539890944)) ;
#130717 = CARTESIAN_POINT('Ctrl Pts',(-32.0519920259812,13.7954469993451,
128.38120266347)) ;
#130718 = CARTESIAN_POINT('Ctrl Pts',(-32.0172267567837,14.0751704523599,
128.246444081047)) ;
#130719 = CARTESIAN_POINT('Ctrl Pts',(-31.9603465713458,14.3069079863902,
128.04724645239)) ;
#130720 = CARTESIAN_POINT('Ctrl Pts',(-31.8858483293298,14.4762412630358,
127.796504873332)) ;
#130721 = CARTESIAN_POINT('Ctrl Pts',(-31.7992735361296,14.5702449515651,
127.510285055868)) ;
#130722 = CARTESIAN_POINT('Ctrl Pts',(-31.7089460812534,14.5813885782014,
127.213417952581)) ;
#130723 = CARTESIAN_POINT('Ctrl Pts',(-31.6209134531669,14.5100797260329,
126.923132692913)) ;
#130724 = CARTESIAN_POINT('Ctrl Pts',(-31.542314320007,14.3602445926638,126.660309566855)) ;
#130725 = CARTESIAN_POINT('Ctrl Pts',(-31.4799830689848,14.1432533152037,
126.445071104613)) ;
#130726 = CARTESIAN_POINT('Ctrl Pts',(-31.4390256574942,13.8766591291424,
126.292492402048)) ;
#130727 = CARTESIAN_POINT('Ctrl Pts',(-31.4226243614274,13.5754713250829,
126.211380568243)) ;
#130728 = CARTESIAN_POINT('Ctrl Pts',(-31.4330180261553,13.2645670010663,
126.208687793803)) ;
#130729 = CARTESIAN_POINT('Ctrl Pts',(-31.4703430384628,12.9634278823174,
126.284481469812)) ;
#130730 = CARTESIAN_POINT('Ctrl Pts',(-31.5321358860487,12.6972349900806,
126.431994498119)) ;
#130731 = CARTESIAN_POINT('Ctrl Pts',(-31.6152291836202,12.481723120017,126.64158339994)) ;
#130732 = CARTESIAN_POINT('Ctrl Pts',(-31.7143133014449,12.3338052298827,
126.897872583145)) ;
#130733 = CARTESIAN_POINT('Ctrl Pts',(-31.8227437636715,12.2641456097446,
127.181516339519)) ;
#130734 = CARTESIAN_POINT('Ctrl Pts',(-31.9335770129781,12.277353556164,127.472198089832)) ;
#130735 = CARTESIAN_POINT('Ctrl Pts',(-32.0398281227222,12.3726334343567,
127.749447473408)) ;
#130736 = CARTESIAN_POINT('Ctrl Pts',(-32.1345084762193,12.5434757962,127.992866694939)) ;
#130737 = CARTESIAN_POINT('Ctrl Pts',(-32.2113206179641,12.7769497154647,
128.184156230134)) ;
#130738 = CARTESIAN_POINT('Ctrl Pts',(-32.2657802289169,13.0568799295701,
128.31011632032)) ;
#130739 = CARTESIAN_POINT('Ctrl Pts',(-32.2945922213593,13.3636449055978,
128.361095482394)) ;
#130740 = CARTESIAN_POINT('Ctrl Pts',(-32.2963571044857,13.6733774156544,
128.333199277218)) ;
#130741 = CARTESIAN_POINT('Ctrl Pts',(-32.271951381347,13.965438068356,128.228844280693)) ;
#130742 = CARTESIAN_POINT('Ctrl Pts',(-32.2232530315277,14.2203012587836,
128.053289070133)) ;
#130743 = CARTESIAN_POINT('Ctrl Pts',(-32.155372333444,14.4159470406951,127.82200217397)) ;
#130744 = CARTESIAN_POINT('Ctrl Pts',(-32.0731102939308,14.5416943667992,
127.548530757984)) ;
#130745 = CARTESIAN_POINT('Ctrl Pts',(-31.9833574865262,14.5869018903293,
127.253186867552)) ;
#130746 = CARTESIAN_POINT('Ctrl Pts',(-31.8935389765681,14.5489491297832,
126.957740138225)) ;
#130747 = CARTESIAN_POINT('Ctrl Pts',(-31.8102081714722,14.4300240433963,
126.681107926645)) ;
#130748 = CARTESIAN_POINT('Ctrl Pts',(-31.7405903151456,14.2387296175427,
126.444572398836)) ;
#130749 = CARTESIAN_POINT('Ctrl Pts',(-31.6904068259423,13.9899469029636,
126.264929854329)) ;
#130750 = CARTESIAN_POINT('Ctrl Pts',(-31.6636696322021,13.7002922437487,
126.153725446933)) ;
#130751 = CARTESIAN_POINT('Ctrl Pts',(-31.6630638330101,13.3909003280038,
126.118871837105)) ;
#130752 = CARTESIAN_POINT('Ctrl Pts',(-31.68968990522,13.0819914624154,126.163364765764)) ;
#130753 = CARTESIAN_POINT('Ctrl Pts',(-31.7418568854852,12.8000707590593,
126.282755069558)) ;
#130754 = CARTESIAN_POINT('Ctrl Pts',(-31.816871195244,12.5616135129792,126.468774849614)) ;
#130755 = CARTESIAN_POINT('Ctrl Pts',(-31.9103871654035,12.3844499171478,
126.708743358304)) ;
#130756 = CARTESIAN_POINT('Ctrl Pts',(-32.0159352821582,12.2824628358376,
126.98393007406)) ;
#130757 = CARTESIAN_POINT('Ctrl Pts',(-32.1261749285063,12.2618989558539,
127.27301807145)) ;
#130758 = CARTESIAN_POINT('Ctrl Pts',(-32.2355321466552,12.3245801207235,
127.559239590374)) ;
#130759 = CARTESIAN_POINT('Ctrl Pts',(-32.335338397919,12.4655889395947,127.817759618502)) ;
#130760 = CARTESIAN_POINT('Ctrl Pts',(-32.4201013753358,12.6753257670411,
128.032242329175)) ;
#130761 = CARTESIAN_POINT('Ctrl Pts',(-32.4842152329815,12.9389694466535,
128.186377249352)) ;
#130762 = CARTESIAN_POINT('Ctrl Pts',(-32.5236900098666,13.2377440459955,
128.268495152112)) ;
#130763 = CARTESIAN_POINT('Ctrl Pts',(-32.5364526740039,13.5478076708615,
128.272797762813)) ;
#130764 = CARTESIAN_POINT('Ctrl Pts',(-32.5223947250415,13.8515134131997,
128.198467412285)) ;
#130765 = CARTESIAN_POINT('Ctrl Pts',(-32.4831407710608,14.1231096251736,
128.050674414571)) ;
#130766 = CARTESIAN_POINT('Ctrl Pts',(-32.4226347638806,14.3439545931311,
127.840915685831)) ;
#130767 = CARTESIAN_POINT('Ctrl Pts',(-32.3454372578941,14.4998916589537,
127.58227442761)) ;
#130768 = CARTESIAN_POINT('Ctrl Pts',(-32.2576768546008,14.5786386310749,
127.292673319528)) ;
#130769 = CARTESIAN_POINT('Ctrl Pts',(-32.1669904917241,14.5742675213239,
126.9946475028)) ;
#130770 = CARTESIAN_POINT('Ctrl Pts',(-32.0801842586365,14.4873447468798,
126.707909950738)) ;
#130771 = CARTESIAN_POINT('Ctrl Pts',(-32.0045667910146,14.3247914484279,
126.453977737131)) ;
#130772 = CARTESIAN_POINT('Ctrl Pts',(-31.9456990864337,14.0970302958978,
126.248838632102)) ;
#130773 = CARTESIAN_POINT('Ctrl Pts',(-31.9089308570874,13.8204924579681,
126.108230614868)) ;
#130774 = CARTESIAN_POINT('Ctrl Pts',(-31.8976597732386,13.5164550314446,
126.042218995313)) ;
#130775 = CARTESIAN_POINT('Ctrl Pts',(-31.9131779382847,13.2060700526839,
126.054496803148)) ;
#130776 = CARTESIAN_POINT('Ctrl Pts',(-31.9552445107061,12.9102233152311,
126.144229921165)) ;
#130777 = CARTESIAN_POINT('Ctrl Pts',(-32.0218893865554,12.6507291998818,
126.305673327108)) ;
#130778 = CARTESIAN_POINT('Ctrl Pts',(-32.1079190718772,12.448558591514,126.524068042123)) ;
#130779 = CARTESIAN_POINT('Ctrl Pts',(-32.2092378807032,12.3145373927892,
126.78689226887)) ;
#130780 = CARTESIAN_POINT('Ctrl Pts',(-32.3187653072149,12.2601564003865,
127.0737196005)) ;
#130781 = CARTESIAN_POINT('Ctrl Pts',(-32.4296559654795,12.2893926143671,
127.364444314449)) ;
#130782 = CARTESIAN_POINT('Ctrl Pts',(-32.5339447068146,12.399436637318,127.636048091739)) ;
#130783 = CARTESIAN_POINT('Ctrl Pts',(-32.6259308163714,12.5839727968354,
127.871499758443)) ;
#130784 = CARTESIAN_POINT('Ctrl Pts',(-32.6984702869464,12.8264918557582,
128.050463425862)) ;
#130785 = CARTESIAN_POINT('Ctrl Pts',(-32.7484756801105,13.1141229255637,
128.163283725505)) ;
#130786 = CARTESIAN_POINT('Ctrl Pts',(-32.7641874562103,13.3194868174309,
128.187142012586)) ;
#130787 = CARTESIAN_POINT('Ctrl Pts',(-32.7676006247655,13.4222383333956,
128.186092009004)) ;
#130788 = CARTESIAN_POINT('Ctrl Pts',(-11.2812798643659,13.1551399285885,
133.225361312885)) ;
#130789 = CARTESIAN_POINT('Ctrl Pts',(-11.2820187647633,13.1489709609094,
133.226788867079)) ;
#130790 = CARTESIAN_POINT('Ctrl Pts',(-11.2940725891313,13.0505878441039,
133.250318667877)) ;
#130791 = CARTESIAN_POINT('Ctrl Pts',(-11.3268196692865,12.8648900473044,
133.323006215356)) ;
#130792 = CARTESIAN_POINT('Ctrl Pts',(-11.3955581347561,12.6378996894465,
133.490786092827)) ;
#130793 = CARTESIAN_POINT('Ctrl Pts',(-11.4818126038911,12.4661938442505,
133.709651137204)) ;
#130794 = CARTESIAN_POINT('Ctrl Pts',(-11.5806418499012,12.3629468779938,
133.965082777503)) ;
#130795 = CARTESIAN_POINT('Ctrl Pts',(-11.6840920756584,12.3360866578135,
134.234357728742)) ;
#130796 = CARTESIAN_POINT('Ctrl Pts',(-11.7874232958009,12.3868467815327,
134.502988211751)) ;
#130797 = CARTESIAN_POINT('Ctrl Pts',(-11.8826517586958,12.5118616193735,
134.748082512994)) ;
#130798 = CARTESIAN_POINT('Ctrl Pts',(-11.9642364503466,12.7022376314793,
134.953268302114)) ;
#130799 = CARTESIAN_POINT('Ctrl Pts',(-12.0268555159077,12.9442211340136,
135.103070944459)) ;
#130800 = CARTESIAN_POINT('Ctrl Pts',(-12.0667868417897,13.2203922331636,
135.186606249474)) ;
#130801 = CARTESIAN_POINT('Ctrl Pts',(-12.0819921567622,13.5109001041669,
135.197934267535)) ;
#130802 = CARTESIAN_POINT('Ctrl Pts',(-12.0718871830781,13.7967277450532,
135.135125417403)) ;
#130803 = CARTESIAN_POINT('Ctrl Pts',(-12.0382787552941,14.0531634695327,
135.003985075531)) ;
#130804 = CARTESIAN_POINT('Ctrl Pts',(-11.984040511163,14.2659161102292,134.812412340654)) ;
#130805 = CARTESIAN_POINT('Ctrl Pts',(-11.9138317313736,14.4182155312585,
134.574200139104)) ;
#130806 = CARTESIAN_POINT('Ctrl Pts',(-11.8331828494072,14.4993926065239,
134.305392211434)) ;
#130807 = CARTESIAN_POINT('Ctrl Pts',(-11.7490444838035,14.5030674016304,
134.026483130585)) ;
#130808 = CARTESIAN_POINT('Ctrl Pts',(-11.6680809986179,14.4296658181567,
133.756898311423)) ;
#130809 = CARTESIAN_POINT('Ctrl Pts',(-11.5965958202758,14.2842405620309,
133.514968656249)) ;
#130810 = CARTESIAN_POINT('Ctrl Pts',(-11.5404239481228,14.0768885755418,
133.31772524141)) ;
#130811 = CARTESIAN_POINT('Ctrl Pts',(-11.5044626643021,13.821937566696,133.179448820527)) ;
#130812 = CARTESIAN_POINT('Ctrl Pts',(-11.492115437901,13.5404397832619,133.110400577556)) ;
#130813 = CARTESIAN_POINT('Ctrl Pts',(-11.5046895368218,13.2491903771815,
133.113990718504)) ;
#130814 = CARTESIAN_POINT('Ctrl Pts',(-11.5423996819585,12.9699188880577,
133.190943520196)) ;
#130815 = CARTESIAN_POINT('Ctrl Pts',(-11.6027127193453,12.7245502986717,
133.33412175314)) ;
#130816 = CARTESIAN_POINT('Ctrl Pts',(-11.6827307770101,12.5279694687298,
133.534676781188)) ;
#130817 = CARTESIAN_POINT('Ctrl Pts',(-11.7767909409935,12.3961377043517,
133.7763823545)) ;
#130818 = CARTESIAN_POINT('Ctrl Pts',(-11.8796482494039,12.3376103677892,
134.043626665423)) ;
#130819 = CARTESIAN_POINT('Ctrl Pts',(-11.9835249356267,12.3569098529355,
134.314074542349)) ;
#130820 = CARTESIAN_POINT('Ctrl Pts',(-12.0830151650733,12.452769019898,134.571498333322)) ;
#130821 = CARTESIAN_POINT('Ctrl Pts',(-12.1707022339469,12.6179593573441,
134.794565234874)) ;
#130822 = CARTESIAN_POINT('Ctrl Pts',(-12.2415306520725,12.8405880377693,
134.968374154773)) ;
#130823 = CARTESIAN_POINT('Ctrl Pts',(-12.2912076318387,13.1065246421439,
135.080214865833)) ;
#130824 = CARTESIAN_POINT('Ctrl Pts',(-12.3163775691246,13.3925179674891,
135.12078307657)) ;
#130825 = CARTESIAN_POINT('Ctrl Pts',(-12.3166058496797,13.6819916651313,
135.088335546118)) ;
#130826 = CARTESIAN_POINT('Ctrl Pts',(-12.2921472081091,13.9537242418059,
134.983669295533)) ;
#130827 = CARTESIAN_POINT('Ctrl Pts',(-12.2457390773696,14.1863734291659,
134.815010882744)) ;
#130828 = CARTESIAN_POINT('Ctrl Pts',(-12.1814800516644,14.3643807985693,
134.59423567404)) ;
#130829 = CARTESIAN_POINT('Ctrl Pts',(-12.1044683457898,14.4754559850244,
134.336147922274)) ;
#130830 = CARTESIAN_POINT('Ctrl Pts',(-12.0208090250937,14.5110246739577,
134.058551574174)) ;
#130831 = CARTESIAN_POINT('Ctrl Pts',(-11.9378612224862,14.4687063588107,
133.783197368949)) ;
#130832 = CARTESIAN_POINT('Ctrl Pts',(-11.8615647632541,14.3514018815055,
133.527145574601)) ;
#130833 = CARTESIAN_POINT('Ctrl Pts',(-11.798502564401,14.1671964752596,133.309749293991)) ;
#130834 = CARTESIAN_POINT('Ctrl Pts',(-11.754049052173,13.9308608041133,133.146872132253)) ;
#130835 = CARTESIAN_POINT('Ctrl Pts',(-11.7316977644638,13.6570089999716,
133.048397750488)) ;
#130836 = CARTESIAN_POINT('Ctrl Pts',(-11.7341180951435,13.3664659574419,
133.022308686926)) ;
#130837 = CARTESIAN_POINT('Ctrl Pts',(-11.761720921654,13.0805681472547,133.069846022257)) ;
#130838 = CARTESIAN_POINT('Ctrl Pts',(-11.8131936002259,12.8190539470386,
133.187112979174)) ;
#130839 = CARTESIAN_POINT('Ctrl Pts',(-11.886092857491,12.5999338423892,133.366806137464)) ;
#130840 = CARTESIAN_POINT('Ctrl Pts',(-11.9747587487869,12.4413957528131,
133.592859241921)) ;
#130841 = CARTESIAN_POINT('Ctrl Pts',(-12.0748052338517,12.3520378265489,
133.85195165464)) ;
#130842 = CARTESIAN_POINT('Ctrl Pts',(-12.1791704719716,12.339734386482,134.123710421306)) ;
#130843 = CARTESIAN_POINT('Ctrl Pts',(-12.2811942198852,12.4049383167358,
134.388634754176)) ;
#130844 = CARTESIAN_POINT('Ctrl Pts',(-12.3743104910804,12.5429634979505,
134.627548525017)) ;
#130845 = CARTESIAN_POINT('Ctrl Pts',(-12.4527350962615,12.7443553986761,
134.823486021638)) ;
#130846 = CARTESIAN_POINT('Ctrl Pts',(-12.5113245953194,12.9943521537239,
134.961502568807)) ;
#130847 = CARTESIAN_POINT('Ctrl Pts',(-12.5466491191103,13.2741647768729,
135.031655728832)) ;
#130848 = CARTESIAN_POINT('Ctrl Pts',(-12.557133530808,13.565720269456,135.029118946566)) ;
#130849 = CARTESIAN_POINT('Ctrl Pts',(-12.5424084976818,13.8474315556546,
134.952884078473)) ;
#130850 = CARTESIAN_POINT('Ctrl Pts',(-12.504658245782,14.0971649669908,134.809596596871)) ;
#130851 = CARTESIAN_POINT('Ctrl Pts',(-12.4468015681524,14.3002122843455,
134.607345660129)) ;
#130852 = CARTESIAN_POINT('Ctrl Pts',(-12.3740820116557,14.4394509674979,
134.361774496034)) ;
#130853 = CARTESIAN_POINT('Ctrl Pts',(-12.2928286579386,14.5058688200503,
134.091445642351)) ;
#130854 = CARTESIAN_POINT('Ctrl Pts',(-12.2085754911848,14.4952594831202,
133.812133112469)) ;
#130855 = CARTESIAN_POINT('Ctrl Pts',(-12.1285286312613,14.4071576912799,
133.54505905862)) ;
#130856 = CARTESIAN_POINT('Ctrl Pts',(-12.0595995840032,14.2488070341169,
133.310594609379)) ;
#130857 = CARTESIAN_POINT('Ctrl Pts',(-12.007204001394,14.032332595662,133.124541926762)) ;
#130858 = CARTESIAN_POINT('Ctrl Pts',(-11.9754518623539,13.7715185673777,
132.998664946929)) ;
#130859 = CARTESIAN_POINT('Ctrl Pts',(-11.9676077024159,13.4849968555095,
132.942553623633)) ;
#130860 = CARTESIAN_POINT('Ctrl Pts',(-11.9852141495617,13.1936954317484,
132.960744777079)) ;
#130861 = CARTESIAN_POINT('Ctrl Pts',(-12.0270155274854,12.9217410981826,
133.049976934939)) ;
#130862 = CARTESIAN_POINT('Ctrl Pts',(-12.0916442917843,12.6826993167214,
133.205531163459)) ;
#130863 = CARTESIAN_POINT('Ctrl Pts',(-12.1748344849184,12.4976839220085,
133.415374259801)) ;
#130864 = CARTESIAN_POINT('Ctrl Pts',(-12.2706003786281,12.3794711428103,
133.662174391645)) ;
#130865 = CARTESIAN_POINT('Ctrl Pts',(-12.3744503899862,12.3351744196322,
133.932269165389)) ;
#130866 = CARTESIAN_POINT('Ctrl Pts',(-12.4782650208009,12.3695012763354,
134.202412750315)) ;
#130867 = CARTESIAN_POINT('Ctrl Pts',(-12.5754721648271,12.4786183736045,
134.453365352351)) ;
#130868 = CARTESIAN_POINT('Ctrl Pts',(-12.6605578265862,12.6556201701116,
134.668788412585)) ;
#130869 = CARTESIAN_POINT('Ctrl Pts',(-12.7278290779799,12.8885376957079,
134.832076052564)) ;
#130870 = CARTESIAN_POINT('Ctrl Pts',(-12.7727942038789,13.1578672277872,
134.93044163856)) ;
#130871 = CARTESIAN_POINT('Ctrl Pts',(-12.7935589960753,13.4488181058444,
134.957796140316)) ;
#130872 = CARTESIAN_POINT('Ctrl Pts',(-12.7888443918457,13.7357351250712,
134.91097260511)) ;
#130873 = CARTESIAN_POINT('Ctrl Pts',(-12.7602605916963,14.0000244154435,
134.794478626913)) ;
#130874 = CARTESIAN_POINT('Ctrl Pts',(-12.7099141607957,14.2248063693443,
134.614145960045)) ;
#130875 = CARTESIAN_POINT('Ctrl Pts',(-12.6428897963242,14.3907221531774,
134.385334239461)) ;
#130876 = CARTESIAN_POINT('Ctrl Pts',(-12.5640447774941,14.4880878052934,
134.121834427977)) ;
#130877 = CARTESIAN_POINT('Ctrl Pts',(-12.4802617689659,14.5090844515927,
133.844015139513)) ;
#130878 = CARTESIAN_POINT('Ctrl Pts',(-12.3974642832698,14.4517331277302,
133.568827359843)) ;
#130879 = CARTESIAN_POINT('Ctrl Pts',(-12.3236763447296,14.3213873494252,
133.320287858352)) ;
#130880 = CARTESIAN_POINT('Ctrl Pts',(-12.2637347152158,14.1266126254878,
133.112060420808)) ;
#130881 = CARTESIAN_POINT('Ctrl Pts',(-12.2229774667805,13.8801113803002,
132.959735466426)) ;
#130882 = CARTESIAN_POINT('Ctrl Pts',(-12.2053838579744,13.6025840232108,
132.875302084043)) ;
#130883 = CARTESIAN_POINT('Ctrl Pts',(-12.2124772397581,13.3122088978665,
132.862974191922)) ;
#130884 = CARTESIAN_POINT('Ctrl Pts',(-12.2448145015933,13.0284665595888,
132.924236901387)) ;
#130885 = CARTESIAN_POINT('Ctrl Pts',(-12.3005599019218,12.7739765033465,
133.053999198988)) ;
#130886 = CARTESIAN_POINT('Ctrl Pts',(-12.3766445028271,12.5655228915478,
133.243117582921)) ;
#130887 = CARTESIAN_POINT('Ctrl Pts',(-12.4681423855166,12.4188418488155,
133.47731500825)) ;
#130888 = CARTESIAN_POINT('Ctrl Pts',(-12.5692422546882,12.3438198182334,
133.739584235759)) ;
#130889 = CARTESIAN_POINT('Ctrl Pts',(-12.6740334889537,12.3461749880073,
134.012474638995)) ;
#130890 = CARTESIAN_POINT('Ctrl Pts',(-12.7747162224539,12.4256199459212,
134.273532924423)) ;
#130891 = CARTESIAN_POINT('Ctrl Pts',(-12.8655945356852,12.5766359900473,
134.505860328425)) ;
#130892 = CARTESIAN_POINT('Ctrl Pts',(-12.9405208029623,12.7882864475543,
134.691614915467)) ;
#130893 = CARTESIAN_POINT('Ctrl Pts',(-12.9949316879518,13.0452019382586,
134.817458837911)) ;
#130894 = CARTESIAN_POINT('Ctrl Pts',(-13.025720643168,13.3293877258915,134.874271333741)) ;
#130895 = CARTESIAN_POINT('Ctrl Pts',(-13.0313457796955,13.6204035856812,
134.857561997613)) ;
#130896 = CARTESIAN_POINT('Ctrl Pts',(-13.0121238177563,13.8971496153171,
134.768280402699)) ;
#130897 = CARTESIAN_POINT('Ctrl Pts',(-12.9702433337836,14.1397539052331,
134.612839445253)) ;
#130898 = CARTESIAN_POINT('Ctrl Pts',(-12.9092683557999,14.3313464702874,
134.401559637406)) ;
#130899 = CARTESIAN_POINT('Ctrl Pts',(-12.8346344667875,14.4574458616527,
134.150487900523)) ;
#130900 = CARTESIAN_POINT('Ctrl Pts',(-12.7520232585293,14.5099723944026,
133.876034599555)) ;
#130901 = CARTESIAN_POINT('Ctrl Pts',(-12.6680149991839,14.4843439695083,
133.597416296755)) ;
#130902 = CARTESIAN_POINT('Ctrl Pts',(-12.5898605639027,14.3827749410654,
133.336012913517)) ;
#130903 = CARTESIAN_POINT('Ctrl Pts',(-12.5235110131134,14.2124739950545,
133.109063094795)) ;
#130904 = CARTESIAN_POINT('Ctrl Pts',(-12.47454385575,13.9855789386979,132.932891873958)) ;
#130905 = CARTESIAN_POINT('Ctrl Pts',(-12.44718714331,13.7185805864342,132.819871229684)) ;
#130906 = CARTESIAN_POINT('Ctrl Pts',(-12.4441083202369,13.4303185636673,
132.777757800251)) ;
#130907 = CARTESIAN_POINT('Ctrl Pts',(-12.4662081675216,13.1417758325219,
132.809228396078)) ;
#130908 = CARTESIAN_POINT('Ctrl Pts',(-12.5128438608682,12.8725286043858,
132.912265477798)) ;
#130909 = CARTESIAN_POINT('Ctrl Pts',(-12.5811355936144,12.6435096258014,
133.078662360882)) ;
#130910 = CARTESIAN_POINT('Ctrl Pts',(-12.6670557983815,12.4701546223289,
133.296533072804)) ;
#130911 = CARTESIAN_POINT('Ctrl Pts',(-12.7650980875458,12.3650501876111,
133.549835459936)) ;
#130912 = CARTESIAN_POINT('Ctrl Pts',(-12.8692895553206,12.3357586674927,
133.821013809302)) ;
#130913 = CARTESIAN_POINT('Ctrl Pts',(-12.9722194636702,12.3843195509594,
134.088641190149)) ;
#130914 = CARTESIAN_POINT('Ctrl Pts',(-13.0679235169665,12.5073666683789,
134.335069106556)) ;
#130915 = CARTESIAN_POINT('Ctrl Pts',(-13.1498474421669,12.6958200369819,
134.541296314724)) ;
#130916 = CARTESIAN_POINT('Ctrl Pts',(-13.2130846476701,12.9363649293222,
134.692916583502)) ;
#130917 = CARTESIAN_POINT('Ctrl Pts',(-13.2537553284003,13.212046231595,134.778583028313)) ;
#130918 = CARTESIAN_POINT('Ctrl Pts',(-13.2696867588976,13.5022481067603,
134.792052779991)) ;
#130919 = CARTESIAN_POINT('Ctrl Pts',(-13.2603291226857,13.7884016128943,
134.731444216182)) ;
#130920 = CARTESIAN_POINT('Ctrl Pts',(-13.2274358441086,14.045945075732,134.602400846472)) ;
#130921 = CARTESIAN_POINT('Ctrl Pts',(-13.1734739345736,14.2610680704969,
134.41149155897)) ;
#130922 = CARTESIAN_POINT('Ctrl Pts',(-13.1038966633744,14.4145624165552,
134.175255364668)) ;
#130923 = CARTESIAN_POINT('Ctrl Pts',(-13.0234728088093,14.4980852125695,
133.907100960487)) ;
#130924 = CARTESIAN_POINT('Ctrl Pts',(-12.939325995419,14.5041312739862,133.628163299805)) ;
#130925 = CARTESIAN_POINT('Ctrl Pts',(-12.8580140805557,14.4326962339747,
133.357486536545)) ;
#130926 = CARTESIAN_POINT('Ctrl Pts',(-12.7862358410937,14.289424830309,133.114743545619)) ;
#130927 = CARTESIAN_POINT('Ctrl Pts',(-12.7294171395877,14.0826507854277,
132.915479459106)) ;
#130928 = CARTESIAN_POINT('Ctrl Pts',(-12.6931113261045,13.8312291814697,
132.77650858526)) ;
#130929 = CARTESIAN_POINT('Ctrl Pts',(-12.6798565616288,13.5479805821752,
132.704527307887)) ;
#130930 = CARTESIAN_POINT('Ctrl Pts',(-12.6918329131031,13.2572981016289,
132.706442366543)) ;
#130931 = CARTESIAN_POINT('Ctrl Pts',(-12.7286154648152,12.9781391944844,
132.780789668285)) ;
#130932 = CARTESIAN_POINT('Ctrl Pts',(-12.788841308569,12.7298471383749,132.923457407859)) ;
#130933 = CARTESIAN_POINT('Ctrl Pts',(-12.8678064119023,12.5331718510569,
133.121190067536)) ;
#130934 = CARTESIAN_POINT('Ctrl Pts',(-12.9619860922532,12.3987050488903,
133.3630746114)) ;
#130935 = CARTESIAN_POINT('Ctrl Pts',(-13.0641173669679,12.3381977133859,
133.628393862531)) ;
#130936 = CARTESIAN_POINT('Ctrl Pts',(-13.1689636586994,12.3556285786372,
133.901368958815)) ;
#130937 = CARTESIAN_POINT('Ctrl Pts',(-13.2676215267395,12.448498640132,134.156721062578)) ;
#130938 = CARTESIAN_POINT('Ctrl Pts',(-13.3562794099848,12.6124651727369,
134.382428532808)) ;
#130939 = CARTESIAN_POINT('Ctrl Pts',(-13.4274024159188,12.8330193864531,
134.55721035227)) ;
#130940 = CARTESIAN_POINT('Ctrl Pts',(-13.4778657839761,13.0981216515098,
134.671314825157)) ;
#130941 = CARTESIAN_POINT('Ctrl Pts',(-13.5037873702561,13.3840423616995,
134.714047923931)) ;
#130942 = CARTESIAN_POINT('Ctrl Pts',(-13.5047230832927,13.6738043197191,
134.683656575562)) ;
#130943 = CARTESIAN_POINT('Ctrl Pts',(-13.4810350619758,13.9458856450603,
134.581307831703)) ;
#130944 = CARTESIAN_POINT('Ctrl Pts',(-13.4350850950003,14.1805609741337,
134.413888828413)) ;
#130945 = CARTESIAN_POINT('Ctrl Pts',(-13.3713435625267,14.3602096703021,
134.19466352274)) ;
#130946 = CARTESIAN_POINT('Ctrl Pts',(-13.2941228668166,14.4737146563849,
133.935766751957)) ;
#130947 = CARTESIAN_POINT('Ctrl Pts',(-13.2111150371913,14.510981736058,133.660304806086)) ;
#130948 = CARTESIAN_POINT('Ctrl Pts',(-13.1279555516473,14.4710234538019,
133.384286573336)) ;
#130949 = CARTESIAN_POINT('Ctrl Pts',(-13.0514607207591,14.3558611755068,
133.127695259553)) ;
#130950 = CARTESIAN_POINT('Ctrl Pts',(-12.987929872837,14.1736059642118,132.908940703681)) ;
#130951 = CARTESIAN_POINT('Ctrl Pts',(-12.9427874558613,13.9381264816024,
132.743987191645)) ;
#130952 = CARTESIAN_POINT('Ctrl Pts',(-12.9198159126567,13.665192099168,132.643720985883)) ;
#130953 = CARTESIAN_POINT('Ctrl Pts',(-12.9214159568252,13.3755914984187,
132.615321479283)) ;
#130954 = CARTESIAN_POINT('Ctrl Pts',(-12.9485033871058,13.0874857506397,
132.661141600498)) ;
#130955 = CARTESIAN_POINT('Ctrl Pts',(-12.9991534842726,12.8264337657975,
132.776172659393)) ;
#130956 = CARTESIAN_POINT('Ctrl Pts',(-13.0712502877118,12.6060974389448,
132.953593799865)) ;
#130957 = CARTESIAN_POINT('Ctrl Pts',(-13.1597261697062,12.4450313389733,
133.179001034814)) ;
#130958 = CARTESIAN_POINT('Ctrl Pts',(-13.2598221399245,12.3534666197661,
133.438152169847)) ;
#130959 = CARTESIAN_POINT('Ctrl Pts',(-13.3638496997786,12.3390029903486,
133.709021457282)) ;
#130960 = CARTESIAN_POINT('Ctrl Pts',(-13.466268319613,12.4020392430349,133.975026492123)) ;
#130961 = CARTESIAN_POINT('Ctrl Pts',(-13.5598211640111,12.5385711173323,
134.215165246668)) ;
#130962 = CARTESIAN_POINT('Ctrl Pts',(-13.6383382505058,12.737337324062,134.411540597844)) ;
#130963 = CARTESIAN_POINT('Ctrl Pts',(-13.6976697861643,12.9861206892308,
134.551707741949)) ;
#130964 = CARTESIAN_POINT('Ctrl Pts',(-13.7337928936498,13.2660910782566,
134.62410596592)) ;
#130965 = CARTESIAN_POINT('Ctrl Pts',(-13.7449404119012,13.5573227840952,
134.623538746113)) ;
#130966 = CARTESIAN_POINT('Ctrl Pts',(-13.731057609949,13.8386952169897,134.549882879065)) ;
#130967 = CARTESIAN_POINT('Ctrl Pts',(-13.6938267710482,14.0906007554108,
134.407982826979)) ;
#130968 = CARTESIAN_POINT('Ctrl Pts',(-13.6366983945426,14.2945039762926,
134.207985282423)) ;
#130969 = CARTESIAN_POINT('Ctrl Pts',(-13.5643971905334,14.4361574187858,
133.963631330981)) ;
#130970 = CARTESIAN_POINT('Ctrl Pts',(-13.4829079562931,14.5051117570611,
133.692450855681)) ;
#130971 = CARTESIAN_POINT('Ctrl Pts',(-13.398865589322,14.496582620466,133.413844416583)) ;
#130972 = CARTESIAN_POINT('Ctrl Pts',(-13.3188758691256,14.4113394819302,
133.147064384826)) ;
#130973 = CARTESIAN_POINT('Ctrl Pts',(-13.2492482094451,14.2546479447355,
132.910444808226)) ;
#130974 = CARTESIAN_POINT('Ctrl Pts',(-13.1961963849046,14.039143877786,132.722400695126)) ;
#130975 = CARTESIAN_POINT('Ctrl Pts',(-13.1638347550569,13.7793416572316,
132.594749383636)) ;
#130976 = CARTESIAN_POINT('Ctrl Pts',(-13.1552775077889,13.4941095874199,
132.536650789137)) ;
#130977 = CARTESIAN_POINT('Ctrl Pts',(-13.1720447629105,13.2026874966814,
132.552397812081)) ;
#130978 = CARTESIAN_POINT('Ctrl Pts',(-13.2133004298939,12.928833346161,132.639904988231)) ;
#130979 = CARTESIAN_POINT('Ctrl Pts',(-13.2774801251183,12.6885083712283,
132.794116581438)) ;
#130980 = CARTESIAN_POINT('Ctrl Pts',(-13.3597053837363,12.5026390795781,
133.001327621254)) ;
#130981 = CARTESIAN_POINT('Ctrl Pts',(-13.455701350823,12.3816810236162,133.248611444686)) ;
#130982 = CARTESIAN_POINT('Ctrl Pts',(-13.5588450701788,12.3354826595071,
133.516837122875)) ;
#130983 = CARTESIAN_POINT('Ctrl Pts',(-13.662986257812,12.3671988660942,133.787859387829)) ;
#130984 = CARTESIAN_POINT('Ctrl Pts',(-13.7608857501055,12.4748749581507,
134.040689706046)) ;
#130985 = CARTESIAN_POINT('Ctrl Pts',(-13.8461189502053,12.6498955190515,
134.256626571108)) ;
#130986 = CARTESIAN_POINT('Ctrl Pts',(-13.9137641762851,12.8801431332148,
134.421162047123)) ;
#130987 = CARTESIAN_POINT('Ctrl Pts',(-13.959688118663,13.1504415297617,134.52210348875)) ;
#130988 = CARTESIAN_POINT('Ctrl Pts',(-13.9810355826832,13.438739202615,134.551438413197)) ;
#130989 = CARTESIAN_POINT('Ctrl Pts',(-13.9771509252308,13.7280473502378,
134.50680820225)) ;
#130990 = CARTESIAN_POINT('Ctrl Pts',(-13.9490883356948,13.9932362064335,
134.391820118097)) ;
#130991 = CARTESIAN_POINT('Ctrl Pts',(-13.899552383743,14.2186783745982,134.213988401194)) ;
#130992 = CARTESIAN_POINT('Ctrl Pts',(-13.8326088799132,14.3872014330787,
133.985246691092)) ;
#130993 = CARTESIAN_POINT('Ctrl Pts',(-13.754354251272,14.486216521528,133.723625961275)) ;
#130994 = CARTESIAN_POINT('Ctrl Pts',(-13.6703274653614,14.5095010567365,
133.444968044136)) ;
#130995 = CARTESIAN_POINT('Ctrl Pts',(-13.587915515568,14.4548476689191,133.171125957688)) ;
#130996 = CARTESIAN_POINT('Ctrl Pts',(-13.5132496102258,14.3259646517619,
132.919798090487)) ;
#130997 = CARTESIAN_POINT('Ctrl Pts',(-13.4528381497739,14.1320240566172,
132.710133322283)) ;
#130998 = CARTESIAN_POINT('Ctrl Pts',(-13.4117984923924,13.8890687487633,
132.557286539592)) ;
#130999 = CARTESIAN_POINT('Ctrl Pts',(-13.3933038950219,13.6109288487181,
132.470050146704)) ;
#131000 = CARTESIAN_POINT('Ctrl Pts',(-13.3996927101153,13.3205780973656,
132.455665139994)) ;
#131001 = CARTESIAN_POINT('Ctrl Pts',(-13.4314451231204,13.0356410236252,
132.515132416829)) ;
#131002 = CARTESIAN_POINT('Ctrl Pts',(-13.4863521726588,12.7811568557338,
132.642583088239)) ;
#131003 = CARTESIAN_POINT('Ctrl Pts',(-13.5618719439237,12.5709851276515,
132.830045482527)) ;
#131004 = CARTESIAN_POINT('Ctrl Pts',(-13.6530001533805,12.4221766619671,
133.063156221214)) ;
#131005 = CARTESIAN_POINT('Ctrl Pts',(-13.7543438242653,12.3447406812541,
133.325997758698)) ;
#131006 = CARTESIAN_POINT('Ctrl Pts',(-13.858979447707,12.3451621602759,133.598484050117)) ;
#131007 = CARTESIAN_POINT('Ctrl Pts',(-13.9595871058779,12.4221617733591,
133.859413033911)) ;
#131008 = CARTESIAN_POINT('Ctrl Pts',(-14.0509368702114,12.5713293574021,
134.093085140404)) ;
#131009 = CARTESIAN_POINT('Ctrl Pts',(-14.1263288360547,12.7811357471148,
134.280239363245)) ;
#131010 = CARTESIAN_POINT('Ctrl Pts',(-14.181464730297,13.037385413305,134.408146154191)) ;
#131011 = CARTESIAN_POINT('Ctrl Pts',(-14.2129289597319,13.3202247802994,
134.46702998844)) ;
#131012 = CARTESIAN_POINT('Ctrl Pts',(-14.2193168783918,13.6126649497902,
134.452393596522)) ;
#131013 = CARTESIAN_POINT('Ctrl Pts',(-14.2008364796894,13.889109539137,134.365400616144)) ;
#131014 = CARTESIAN_POINT('Ctrl Pts',(-14.1595000662705,14.1334576219234,
134.211477497111)) ;
#131015 = CARTESIAN_POINT('Ctrl Pts',(-14.0992466494206,14.3262010857029,
134.002423062281)) ;
#131016 = CARTESIAN_POINT('Ctrl Pts',(-14.0244678789738,14.4552702241494,
133.750713932904)) ;
#131017 = CARTESIAN_POINT('Ctrl Pts',(-13.9418997721999,14.5094659873619,
133.476364746001)) ;
#131018 = CARTESIAN_POINT('Ctrl Pts',(-13.8583861168424,14.48627928254,133.199410244325)) ;
#131019 = CARTESIAN_POINT('Ctrl Pts',(-13.7797353567973,14.3867194330965,
132.936459435104)) ;
#131020 = CARTESIAN_POINT('Ctrl Pts',(-13.7130105219871,14.2183273389604,
132.708437979387)) ;
#131021 = CARTESIAN_POINT('Ctrl Pts',(-13.6633479068396,13.9922441011096,
132.530147180322)) ;
#131022 = CARTESIAN_POINT('Ctrl Pts',(-13.6354328184579,13.7260908863955,
132.415503205816)) ;
#131023 = CARTESIAN_POINT('Ctrl Pts',(-13.6315996421401,13.4392990683917,
132.371317925094)) ;
#131024 = CARTESIAN_POINT('Ctrl Pts',(-13.6531002743803,13.1491383926391,
132.400878674979)) ;
#131025 = CARTESIAN_POINT('Ctrl Pts',(-13.6988895423874,12.880138144259,132.501583429181)) ;
#131026 = CARTESIAN_POINT('Ctrl Pts',(-13.7669016038619,12.6488312040692,
132.66702117208)) ;
#131027 = CARTESIAN_POINT('Ctrl Pts',(-13.8519661020191,12.4746173052797,
132.882564533349)) ;
#131028 = CARTESIAN_POINT('Ctrl Pts',(-13.9499918537797,12.3669410581914,
133.13572242046)) ;
#131029 = CARTESIAN_POINT('Ctrl Pts',(-14.0540803057466,12.3355244467329,
133.406613758036)) ;
#131030 = CARTESIAN_POINT('Ctrl Pts',(-14.1570770496498,12.3818824637266,
133.674448586604)) ;
#131031 = CARTESIAN_POINT('Ctrl Pts',(-14.2529156063067,12.502442440452,133.921340780179)) ;
#131032 = CARTESIAN_POINT('Ctrl Pts',(-14.3357164299663,12.6900860359651,
134.129966525958)) ;
#131033 = CARTESIAN_POINT('Ctrl Pts',(-14.3993556473891,12.9290693621117,
134.282824648329)) ;
#131034 = CARTESIAN_POINT('Ctrl Pts',(-14.4406746427025,13.2033802627449,
134.370454904131)) ;
#131035 = CARTESIAN_POINT('Ctrl Pts',(-14.4573570221151,13.493885424346,134.386064394722)) ;
#131036 = CARTESIAN_POINT('Ctrl Pts',(-14.4487939272164,13.7798208359641,
134.327863613174)) ;
#131037 = CARTESIAN_POINT('Ctrl Pts',(-14.4163591296665,14.0398147256928,
134.199973199807)) ;
#131038 = CARTESIAN_POINT('Ctrl Pts',(-14.3630430477874,14.2555980954836,
134.011057985321)) ;
#131039 = CARTESIAN_POINT('Ctrl Pts',(-14.2938516112464,14.4112165057251,
133.775932908363)) ;
#131040 = CARTESIAN_POINT('Ctrl Pts',(-14.213327419341,14.4969135755094,133.50736843725)) ;
#131041 = CARTESIAN_POINT('Ctrl Pts',(-14.1296189321524,14.5049696810031,
133.229876903082)) ;
#131042 = CARTESIAN_POINT('Ctrl Pts',(-14.0481698596881,14.4360249735447,
132.958821806314)) ;
#131043 = CARTESIAN_POINT('Ctrl Pts',(-13.9759487851369,14.2945754362065,
132.714746600477)) ;
#131044 = CARTESIAN_POINT('Ctrl Pts',(-13.9186392005941,14.0897548858671,
132.514089317548)) ;
#131045 = CARTESIAN_POINT('Ctrl Pts',(-13.8816283734556,13.8387001375239,
132.372961040856)) ;
#131046 = CARTESIAN_POINT('Ctrl Pts',(-13.86765973633,13.5574044598577,132.299056743724)) ;
#131047 = CARTESIAN_POINT('Ctrl Pts',(-13.8789956043886,13.2644130009093,
132.2988381339)) ;
#131048 = CARTESIAN_POINT('Ctrl Pts',(-13.9149994984909,12.9862195730077,
132.371090109727)) ;
#131049 = CARTESIAN_POINT('Ctrl Pts',(-13.9743502243685,12.7371111819008,
132.511275565875)) ;
#131050 = CARTESIAN_POINT('Ctrl Pts',(-14.0530557762854,12.5380203242925,
132.708138925323)) ;
#131051 = CARTESIAN_POINT('Ctrl Pts',(-14.1469276806553,12.4015272632005,
132.949117652525)) ;
#131052 = CARTESIAN_POINT('Ctrl Pts',(-14.2489833656644,12.3389470103484,
133.214189844898)) ;
#131053 = CARTESIAN_POINT('Ctrl Pts',(-14.3533226131928,12.3537864997403,
133.485861761893)) ;
#131054 = CARTESIAN_POINT('Ctrl Pts',(-14.4528614890508,12.4449099176858,
133.743576395913)) ;
#131055 = CARTESIAN_POINT('Ctrl Pts',(-14.5418561425685,12.6072327563546,
133.97027761533)) ;
#131056 = CARTESIAN_POINT('Ctrl Pts',(-14.6133813155202,12.8259751420657,
134.146289595912)) ;
#131057 = CARTESIAN_POINT('Ctrl Pts',(-14.6644626717837,13.0894865209779,
134.262268329824)) ;
#131058 = CARTESIAN_POINT('Ctrl Pts',(-14.6912354788188,13.3763086244584,
134.307339213758)) ;
#131059 = CARTESIAN_POINT('Ctrl Pts',(-14.6927780845657,13.666102426872,134.278737035569)) ;
#131060 = CARTESIAN_POINT('Ctrl Pts',(-14.6699098049705,13.9378774393092,
134.178922193569)) ;
#131061 = CARTESIAN_POINT('Ctrl Pts',(-14.6244200591529,14.174793298913,134.012730262355)) ;
#131062 = CARTESIAN_POINT('Ctrl Pts',(-14.5612019536203,14.355667987911,133.795095051057)) ;
#131063 = CARTESIAN_POINT('Ctrl Pts',(-14.4846906294762,14.4711053294092,
133.538428577137)) ;
#131064 = CARTESIAN_POINT('Ctrl Pts',(-14.4011850462511,14.511170979715,133.261273870169)) ;
#131065 = CARTESIAN_POINT('Ctrl Pts',(-14.3178410780268,14.4729025341711,
132.984673903261)) ;
#131066 = CARTESIAN_POINT('Ctrl Pts',(-14.2414431710577,14.3605014183323,
132.728538157581)) ;
#131067 = CARTESIAN_POINT('Ctrl Pts',(-14.1770966200207,14.1789799497678,
132.507210107387)) ;
#131068 = CARTESIAN_POINT('Ctrl Pts',(-14.1315848885081,13.9453130755044,
132.341277366815)) ;
#131069 = CARTESIAN_POINT('Ctrl Pts',(-14.1079390036142,13.673613297581,132.239086339493)) ;
#131070 = CARTESIAN_POINT('Ctrl Pts',(-14.1087830481224,13.3843416477693,
132.208491884339)) ;
#131071 = CARTESIAN_POINT('Ctrl Pts',(-14.1351400941846,13.0956424787648,
132.252157038047)) ;
#131072 = CARTESIAN_POINT('Ctrl Pts',(-14.1851403795369,12.8335787485534,
132.365283706234)) ;
#131073 = CARTESIAN_POINT('Ctrl Pts',(-14.2566883427613,12.6116522531053,
132.541092961402)) ;
#131074 = CARTESIAN_POINT('Ctrl Pts',(-14.3449178102994,12.4486058050818,
132.765728820733)) ;
#131075 = CARTESIAN_POINT('Ctrl Pts',(-14.4444094609299,12.3551665981467,
133.023238128206)) ;
#131076 = CARTESIAN_POINT('Ctrl Pts',(-14.5487260750023,12.3383111368361,
133.294844327139)) ;
#131077 = CARTESIAN_POINT('Ctrl Pts',(-14.651135777708,12.3991318667188,133.560878201396)) ;
#131078 = CARTESIAN_POINT('Ctrl Pts',(-14.7450247980916,12.5336133546432,
133.801997324254)) ;
#131079 = CARTESIAN_POINT('Ctrl Pts',(-14.8240658891889,12.7304747525644,
133.999922781035)) ;
#131080 = CARTESIAN_POINT('Ctrl Pts',(-14.8843591623108,12.9801493565206,
134.142645016146)) ;
#131081 = CARTESIAN_POINT('Ctrl Pts',(-14.9207776314118,13.2569930870622,
134.216214669517)) ;
#131082 = CARTESIAN_POINT('Ctrl Pts',(-14.9327904526555,13.5493201067258,
134.218039568247)) ;
#131083 = CARTESIAN_POINT('Ctrl Pts',(-14.9195608823309,13.8310609228274,
134.146315593606)) ;
#131084 = CARTESIAN_POINT('Ctrl Pts',(-14.8829071658904,14.0843638099265,
134.006060198745)) ;
#131085 = CARTESIAN_POINT('Ctrl Pts',(-14.8262774665716,14.2896244491401,
133.807537482938)) ;
#131086 = CARTESIAN_POINT('Ctrl Pts',(-14.7544509561564,14.4330063116879,
133.564623744753)) ;
#131087 = CARTESIAN_POINT('Ctrl Pts',(-14.6730981695364,14.5042107415309,
133.293824015626)) ;
#131088 = CARTESIAN_POINT('Ctrl Pts',(-14.5890044461905,14.4979449999679,
133.015056574469)) ;
#131089 = CARTESIAN_POINT('Ctrl Pts',(-14.5085811345525,14.4144601779744,
132.746912885546)) ;
#131090 = CARTESIAN_POINT('Ctrl Pts',(-14.4386966820867,14.2595209902124,
132.509575163383)) ;
#131091 = CARTESIAN_POINT('Ctrl Pts',(-14.3852681727933,14.046214919979,132.32053362023)) ;
#131092 = CARTESIAN_POINT('Ctrl Pts',(-14.3521879692475,13.7868053449528,
132.190703349274)) ;
#131093 = CARTESIAN_POINT('Ctrl Pts',(-14.3429850788203,13.5027357390144,
132.130803960272)) ;
#131094 = CARTESIAN_POINT('Ctrl Pts',(-14.3589256787532,13.2114164567146,
132.144166678592)) ;
#131095 = CARTESIAN_POINT('Ctrl Pts',(-14.3996479591576,12.9359342983456,
132.230005501464)) ;
#131096 = CARTESIAN_POINT('Ctrl Pts',(-14.4630310316759,12.6951562018299,
132.381999972268)) ;
#131097 = CARTESIAN_POINT('Ctrl Pts',(-14.5447779273386,12.5073061272103,
132.587797294127)) ;
#131098 = CARTESIAN_POINT('Ctrl Pts',(-14.6405874915994,12.3841592686752,
132.834495044115)) ;
#131099 = CARTESIAN_POINT('Ctrl Pts',(-14.7436396651289,12.3356200239572,
133.102447533053)) ;
#131100 = CARTESIAN_POINT('Ctrl Pts',(-14.8482334000072,12.3655842279676,
133.374661826652)) ;
#131101 = CARTESIAN_POINT('Ctrl Pts',(-14.9456378863924,12.4702048591763,
133.62631542447)) ;
#131102 = CARTESIAN_POINT('Ctrl Pts',(-15.032031341998,12.6448837976238,133.845354670619)) ;
#131103 = CARTESIAN_POINT('Ctrl Pts',(-15.0997909854076,12.872508423284,134.010430965611)) ;
#131104 = CARTESIAN_POINT('Ctrl Pts',(-15.1466624677231,13.1434988331289,
134.11394299587)) ;
#131105 = CARTESIAN_POINT('Ctrl Pts',(-15.1684830221252,13.4301737780494,
134.144821454034)) ;
#131106 = CARTESIAN_POINT('Ctrl Pts',(-15.1655029363779,13.7187795914099,
134.102960274335)) ;
#131107 = CARTESIAN_POINT('Ctrl Pts',(-15.137871807278,13.9870154433738,133.988964277523)) ;
#131108 = CARTESIAN_POINT('Ctrl Pts',(-15.089103500937,14.2124398345738,133.813561355081)) ;
#131109 = CARTESIAN_POINT('Ctrl Pts',(-15.0226861816082,14.3830654461858,
133.586365342099)) ;
#131110 = CARTESIAN_POINT('Ctrl Pts',(-14.9442977084689,14.4846609541733,
133.324197217531)) ;
#131111 = CARTESIAN_POINT('Ctrl Pts',(-14.8603045751173,14.5097913616969,
133.045629352813)) ;
#131112 = CARTESIAN_POINT('Ctrl Pts',(-14.7781158124174,14.4576093080194,
132.772584210679)) ;
#131113 = CARTESIAN_POINT('Ctrl Pts',(-14.7029379087114,14.3304831317374,
132.519675058584)) ;
#131114 = CARTESIAN_POINT('Ctrl Pts',(-14.6421746060609,14.1386183822934,
132.309056084948)) ;
#131115 = CARTESIAN_POINT('Ctrl Pts',(-14.6004669656827,13.8965846856625,
132.154209706835)) ;
#131116 = CARTESIAN_POINT('Ctrl Pts',(-14.5812880337956,13.6198365630073,
132.065057969682)) ;
#131117 = CARTESIAN_POINT('Ctrl Pts',(-14.5869544254102,13.3288844737818,
132.048478781958)) ;
#131118 = CARTESIAN_POINT('Ctrl Pts',(-14.6178077703533,13.0447399832046,
132.105475686592)) ;
#131119 = CARTESIAN_POINT('Ctrl Pts',(-14.6721136258845,12.7881836368688,
132.231068090543)) ;
#131120 = CARTESIAN_POINT('Ctrl Pts',(-14.7475386699193,12.5755910115287,
132.418091523374)) ;
#131121 = CARTESIAN_POINT('Ctrl Pts',(-14.8378940236856,12.4257574465567,
132.649102005788)) ;
#131122 = CARTESIAN_POINT('Ctrl Pts',(-14.9388209084364,12.3460112405744,
132.910787274949)) ;
#131123 = CARTESIAN_POINT('Ctrl Pts',(-15.0435737078647,12.3439532504127,
133.183578235088)) ;
#131124 = CARTESIAN_POINT('Ctrl Pts',(-15.1446091167616,12.4188218900739,
133.445686307793)) ;
#131125 = CARTESIAN_POINT('Ctrl Pts',(-15.2365998734713,12.5668341062151,
133.681113263233)) ;
#131126 = CARTESIAN_POINT('Ctrl Pts',(-15.3120455807105,12.7739565310488,
133.868616342754)) ;
#131127 = CARTESIAN_POINT('Ctrl Pts',(-15.3679671650309,13.0292275295923,
133.998784482597)) ;
#131128 = CARTESIAN_POINT('Ctrl Pts',(-15.4001513908772,13.3121167714202,
134.059708256056)) ;
#131129 = CARTESIAN_POINT('Ctrl Pts',(-15.407302294284,13.6036711588795,134.047415072482)) ;
#131130 = CARTESIAN_POINT('Ctrl Pts',(-15.3894117903854,13.8822010088686,
133.961971555951)) ;
#131131 = CARTESIAN_POINT('Ctrl Pts',(-15.3488581880954,14.126534024312,133.810499271449)) ;
#131132 = CARTESIAN_POINT('Ctrl Pts',(-15.2890058404676,14.3215277156221,
133.602541497692)) ;
#131133 = CARTESIAN_POINT('Ctrl Pts',(-15.2146261037101,14.4523872469144,
133.352036701433)) ;
#131134 = CARTESIAN_POINT('Ctrl Pts',(-15.132276398967,14.509081269933,133.078352393805)) ;
#131135 = CARTESIAN_POINT('Ctrl Pts',(-15.048156334803,14.4877530584647,132.799404216537)) ;
#131136 = CARTESIAN_POINT('Ctrl Pts',(-14.9697741972722,14.3906972492053,
132.537447195776)) ;
#131137 = CARTESIAN_POINT('Ctrl Pts',(-14.9025432118204,14.2242127265294,
132.307919886886)) ;
#131138 = CARTESIAN_POINT('Ctrl Pts',(-14.8524134830202,14.0000453961231,
132.128331876439)) ;
#131139 = CARTESIAN_POINT('Ctrl Pts',(-14.8236827135926,13.7349941187306,
132.011308130338)) ;
#131140 = CARTESIAN_POINT('Ctrl Pts',(-14.8192110157222,13.4462938086935,
131.964998461715)) ;
#131141 = CARTESIAN_POINT('Ctrl Pts',(-14.8397608257614,13.1586524064852,
131.992109164985)) ;
#131142 = CARTESIAN_POINT('Ctrl Pts',(-14.8852506544382,12.8863235925418,
132.091631205511)) ;
#131143 = CARTESIAN_POINT('Ctrl Pts',(-14.952306886852,12.6553854575325,132.254505839022)) ;
#131144 = CARTESIAN_POINT('Ctrl Pts',(-15.036993538522,12.4787538591612,132.468885463633)) ;
#131145 = CARTESIAN_POINT('Ctrl Pts',(-15.1351325127102,12.3688114822916,
132.722256615459)) ;
#131146 = CARTESIAN_POINT('Ctrl Pts',(-15.2387002100067,12.3354319136936,
132.991765834986)) ;
#131147 = CARTESIAN_POINT('Ctrl Pts',(-15.3419020299315,12.3792576310417,
133.260178529464)) ;
#131148 = CARTESIAN_POINT('Ctrl Pts',(-15.4385746866519,12.4988398999205,
133.509304414363)) ;
#131149 = CARTESIAN_POINT('Ctrl Pts',(-15.5211785051019,12.6835118512005,
133.71760539492)) ;
#131150 = CARTESIAN_POINT('Ctrl Pts',(-15.585614912484,12.9214923912795,133.872725040323)) ;
#131151 = CARTESIAN_POINT('Ctrl Pts',(-15.6276593796861,13.1954916424955,
133.96242929729)) ;
#131152 = CARTESIAN_POINT('Ctrl Pts',(-15.6450448286836,13.4865485670219,
133.980012149667)) ;
#131153 = CARTESIAN_POINT('Ctrl Pts',(-15.6370948847114,13.772471589557,133.923647448758)) ;
#131154 = CARTESIAN_POINT('Ctrl Pts',(-15.6054576941134,14.0322259092952,
133.798239163953)) ;
#131155 = CARTESIAN_POINT('Ctrl Pts',(-15.5528532090993,14.2496185339524,
133.611440842472)) ;
#131156 = CARTESIAN_POINT('Ctrl Pts',(-15.483617346609,14.4079186586772,133.375986031408)) ;
#131157 = CARTESIAN_POINT('Ctrl Pts',(-15.4040148005417,14.495128940057,133.110405781656)) ;
#131158 = CARTESIAN_POINT('Ctrl Pts',(-15.3198980850125,14.5060206783235,
132.831544484233)) ;
#131159 = CARTESIAN_POINT('Ctrl Pts',(-15.2380342056834,14.4388851972431,
132.55918054693)) ;
#131160 = CARTESIAN_POINT('Ctrl Pts',(-15.1654389797841,14.2990479598781,
132.313981427395)) ;
#131161 = CARTESIAN_POINT('Ctrl Pts',(-15.107816605712,14.096277092635,132.112499036057)) ;
#131162 = CARTESIAN_POINT('Ctrl Pts',(-15.0701124492741,13.8463552274942,
131.969338122834)) ;
#131163 = CARTESIAN_POINT('Ctrl Pts',(-15.05554407707,13.5643762793268,131.893541407323)) ;
#131164 = CARTESIAN_POINT('Ctrl Pts',(-15.0659585050918,13.2747380866486,
131.891020251149)) ;
#131165 = CARTESIAN_POINT('Ctrl Pts',(-15.101446630055,12.9934296976024,131.961474427387)) ;
#131166 = CARTESIAN_POINT('Ctrl Pts',(-15.1601039100246,12.7438068041656,
132.099715492444)) ;
#131167 = CARTESIAN_POINT('Ctrl Pts',(-15.2384724882155,12.5426943442427,
132.295520501906)) ;
#131168 = CARTESIAN_POINT('Ctrl Pts',(-15.3316626347415,12.4046936236787,
132.534630966333)) ;
#131169 = CARTESIAN_POINT('Ctrl Pts',(-15.4337983976848,12.3396331759052,
132.799852893319)) ;
#131170 = CARTESIAN_POINT('Ctrl Pts',(-15.5380451833256,12.3522550875064,
133.071297592341)) ;
#131171 = CARTESIAN_POINT('Ctrl Pts',(-15.6378149553019,12.441158614988,133.329684714748)) ;
#131172 = CARTESIAN_POINT('Ctrl Pts',(-15.7271824288003,12.6013769713038,
133.55749869446)) ;
#131173 = CARTESIAN_POINT('Ctrl Pts',(-15.799387164279,12.819071640269,133.735430014399)) ;
#131174 = CARTESIAN_POINT('Ctrl Pts',(-15.8509954325536,13.0807346140254,
133.853055281245)) ;
#131175 = CARTESIAN_POINT('Ctrl Pts',(-15.8785701981475,13.3675408612144,
133.900413861765)) ;
#131176 = CARTESIAN_POINT('Ctrl Pts',(-15.880950069095,13.6570979280699,133.874320504545)) ;
#131177 = CARTESIAN_POINT('Ctrl Pts',(-15.8584614917164,13.9319893911641,
133.775308859387)) ;
#131178 = CARTESIAN_POINT('Ctrl Pts',(-15.8140300794619,14.1676085258846,
133.612576918087)) ;
#131179 = CARTESIAN_POINT('Ctrl Pts',(-15.7508365618172,14.3519029604138,
133.394745430706)) ;
#131180 = CARTESIAN_POINT('Ctrl Pts',(-15.6747542377325,14.4687263868581,
133.139424327783)) ;
#131181 = CARTESIAN_POINT('Ctrl Pts',(-15.5916310901521,14.5110206744739,
132.86348513324)) ;
#131182 = CARTESIAN_POINT('Ctrl Pts',(-15.5082277554707,14.4754839101951,
132.586740900539)) ;
#131183 = CARTESIAN_POINT('Ctrl Pts',(-15.4310148106346,14.3641243881349,
132.327975519891)) ;
#131184 = CARTESIAN_POINT('Ctrl Pts',(-15.366796148105,14.1859981150162,132.10732571318)) ;
#131185 = CARTESIAN_POINT('Ctrl Pts',(-15.3203690301936,13.9527739629267,
131.938549874937)) ;
#131186 = CARTESIAN_POINT('Ctrl Pts',(-15.2960642034895,13.6818171869407,
131.83443758756)) ;
#131187 = CARTESIAN_POINT('Ctrl Pts',(-15.2962284106988,13.3923456599437,
131.801803057666)) ;
#131188 = CARTESIAN_POINT('Ctrl Pts',(-15.3217088635482,13.1044625348289,
131.843052348479)) ;
#131189 = CARTESIAN_POINT('Ctrl Pts',(-15.3712895624886,12.8400820200563,
131.954780479996)) ;
#131190 = CARTESIAN_POINT('Ctrl Pts',(-15.4421215709794,12.6174283224968,
132.128595071256)) ;
#131191 = CARTESIAN_POINT('Ctrl Pts',(-15.5300656767636,12.4521814963559,
132.352341736955)) ;
#131192 = CARTESIAN_POINT('Ctrl Pts',(-15.6293654089259,12.3567835155047,
132.609283754024)) ;
#131193 = CARTESIAN_POINT('Ctrl Pts',(-15.7333497867975,12.3377092271658,
132.880009523703)) ;
#131194 = CARTESIAN_POINT('Ctrl Pts',(-15.8360089773108,12.3962076032604,
133.146742886939)) ;
#131195 = CARTESIAN_POINT('Ctrl Pts',(-15.930453723468,12.5290432373042,133.389409066584)) ;
#131196 = CARTESIAN_POINT('Ctrl Pts',(-16.009869584066,12.7244085230837,133.588441629327)) ;
#131197 = CARTESIAN_POINT('Ctrl Pts',(-16.0704566796156,12.9709500550387,
133.732258312717)) ;
#131198 = CARTESIAN_POINT('Ctrl Pts',(-16.1079755146477,13.2494402817627,
133.808760193825)) ;
#131199 = CARTESIAN_POINT('Ctrl Pts',(-16.1205567949924,13.5418967084717,
133.812230503726)) ;
#131200 = CARTESIAN_POINT('Ctrl Pts',(-16.1080660019669,13.8230883914708,
133.742789063125)) ;
#131201 = CARTESIAN_POINT('Ctrl Pts',(-16.0720612901439,14.0775910910953,
133.604421793909)) ;
#131202 = CARTESIAN_POINT('Ctrl Pts',(-16.016031312662,14.2842118886259,133.407692540579)) ;
#131203 = CARTESIAN_POINT('Ctrl Pts',(-15.9444811188164,14.4299775435325,
133.165534218954)) ;
#131204 = CARTESIAN_POINT('Ctrl Pts',(-15.8629277653847,14.503331032243,132.894001914259)) ;
#131205 = CARTESIAN_POINT('Ctrl Pts',(-15.7793496289803,14.4992417837061,
132.616952244808)) ;
#131206 = CARTESIAN_POINT('Ctrl Pts',(-15.6984734089822,14.4177939822546,
132.347381532007)) ;
#131207 = CARTESIAN_POINT('Ctrl Pts',(-15.6283650852396,14.2650806147523,
132.109470216545)) ;
#131208 = CARTESIAN_POINT('Ctrl Pts',(-15.5743268050137,14.0529681509037,
131.918590385591)) ;
#131209 = CARTESIAN_POINT('Ctrl Pts',(-15.5406403700371,13.7955270319932,
131.787101135372)) ;
#131210 = CARTESIAN_POINT('Ctrl Pts',(-15.5306638256876,13.5095709535078,
131.724666349948)) ;
#131211 = CARTESIAN_POINT('Ctrl Pts',(-15.5460171831695,13.2189036520177,
131.736403340103)) ;
#131212 = CARTESIAN_POINT('Ctrl Pts',(-15.5859137154081,12.9437120966298,
131.819943466577)) ;
#131213 = CARTESIAN_POINT('Ctrl Pts',(-15.6485475179313,12.7018113312773,
131.969792071976)) ;
#131214 = CARTESIAN_POINT('Ctrl Pts',(-15.7301725881226,12.5115374792667,
132.175093619939)) ;
#131215 = CARTESIAN_POINT('Ctrl Pts',(-15.8255194984171,12.3865362509785,
132.420501324227)) ;
#131216 = CARTESIAN_POINT('Ctrl Pts',(-15.9289904176059,12.3360647683775,
132.689500393083)) ;
#131217 = CARTESIAN_POINT('Ctrl Pts',(-16.0322109432962,12.3630945002041,
132.958176956719)) ;
#131218 = CARTESIAN_POINT('Ctrl Pts',(-16.1310535797055,12.4665769548229,
133.213630713827)) ;
#131219 = CARTESIAN_POINT('Ctrl Pts',(-16.2171162898203,12.637873730405,133.432016347732)) ;
#131220 = CARTESIAN_POINT('Ctrl Pts',(-16.2861070614099,12.8661806742055,
133.600365416687)) ;
#131221 = CARTESIAN_POINT('Ctrl Pts',(-16.3331577984964,13.1333277515124,
133.704775971435)) ;
#131222 = CARTESIAN_POINT('Ctrl Pts',(-16.3560616077762,13.4221934836715,
133.738517459493)) ;
#131223 = CARTESIAN_POINT('Ctrl Pts',(-16.3536937500244,13.7107571318464,
133.698487549138)) ;
#131224 = CARTESIAN_POINT('Ctrl Pts',(-16.3267795290435,13.9798563780996,
133.58659147111)) ;
#131225 = CARTESIAN_POINT('Ctrl Pts',(-16.2784408821239,14.2070905580459,
133.412375341533)) ;
#131226 = CARTESIAN_POINT('Ctrl Pts',(-16.2125397227886,14.3790287482914,
133.186748864503)) ;
#131227 = CARTESIAN_POINT('Ctrl Pts',(-16.1346594708171,14.4826462514907,
132.926162382995)) ;
#131228 = CARTESIAN_POINT('Ctrl Pts',(-16.0504302213959,14.5101765749395,
132.646782279628)) ;
#131229 = CARTESIAN_POINT('Ctrl Pts',(-15.9682674268405,14.4602521093363,
132.373878730922)) ;
#131230 = CARTESIAN_POINT('Ctrl Pts',(-15.892694390541,14.3349863303821,132.119771873462)) ;
#131231 = CARTESIAN_POINT('Ctrl Pts',(-15.8317129503708,14.1459036519263,
131.908681279387)) ;
#131232 = CARTESIAN_POINT('Ctrl Pts',(-15.7891216920241,13.9042674567381,
131.751109063095)) ;
#131233 = CARTESIAN_POINT('Ctrl Pts',(-15.7692741641614,13.6274934121279,
131.659929127433)) ;
#131234 = CARTESIAN_POINT('Ctrl Pts',(-15.774240842792,13.3375401227482,131.641402457855)) ;
#131235 = CARTESIAN_POINT('Ctrl Pts',(-15.8042482653973,13.0529656397982,
131.695949415826)) ;
#131236 = CARTESIAN_POINT('Ctrl Pts',(-15.8584516986935,12.793542004979,131.820979830249)) ;
#131237 = CARTESIAN_POINT('Ctrl Pts',(-15.9326864597706,12.5815361452067,
132.004842248444)) ;
#131238 = CARTESIAN_POINT('Ctrl Pts',(-16.0230837910625,12.4287258471182,
132.235797836759)) ;
#131239 = CARTESIAN_POINT('Ctrl Pts',(-16.1240643432101,12.3470719994747,
132.497574210549)) ;
#131240 = CARTESIAN_POINT('Ctrl Pts',(-16.2285925774014,12.3430683223392,
132.769776197563)) ;
#131241 = CARTESIAN_POINT('Ctrl Pts',(-16.3294552263757,12.4155936091128,
133.031491197843)) ;
#131242 = CARTESIAN_POINT('Ctrl Pts',(-16.42158697565,12.5608875783812,133.267432939441)) ;
#131243 = CARTESIAN_POINT('Ctrl Pts',(-16.4979791687381,12.7672957855937,
133.457539227448)) ;
#131244 = CARTESIAN_POINT('Ctrl Pts',(-16.5545469684218,13.0219896288371,
133.589546147221)) ;
#131245 = CARTESIAN_POINT('Ctrl Pts',(-16.5873216769804,13.3035436342973,
133.652289558074)) ;
#131246 = CARTESIAN_POINT('Ctrl Pts',(-16.5952372158022,13.5948422510341,
133.642264450776)) ;
#131247 = CARTESIAN_POINT('Ctrl Pts',(-16.5781262828345,13.8739529691167,
133.559117325056)) ;
#131248 = CARTESIAN_POINT('Ctrl Pts',(-16.5380768677347,14.1203174233417,
133.409012301568)) ;
#131249 = CARTESIAN_POINT('Ctrl Pts',(-16.4787184094645,14.3167168643634,
133.20251930448)) ;
#131250 = CARTESIAN_POINT('Ctrl Pts',(-16.4048795075091,14.4494066861711,
132.953678390524)) ;
#131251 = CARTESIAN_POINT('Ctrl Pts',(-16.3225697948458,14.5084702688582,
132.680063070833)) ;
#131252 = CARTESIAN_POINT('Ctrl Pts',(-16.2386731326133,14.489700746972,132.401879914645)) ;
#131253 = CARTESIAN_POINT('Ctrl Pts',(-16.159666302226,14.3946106074975,132.13794942029)) ;
#131254 = CARTESIAN_POINT('Ctrl Pts',(-16.0919372674924,14.2294635345246,
131.906906848158)) ;
#131255 = CARTESIAN_POINT('Ctrl Pts',(-16.0414142644033,14.0073333887475,
131.726263966149)) ;
#131256 = CARTESIAN_POINT('Ctrl Pts',(-16.0120005571222,13.7435828448799,
131.607279354952)) ;
#131257 = CARTESIAN_POINT('Ctrl Pts',(-16.0067413555039,13.454824745877,131.558621231445)) ;
#131258 = CARTESIAN_POINT('Ctrl Pts',(-16.0266816029947,13.1663898496403,
131.58388276017)) ;
#131259 = CARTESIAN_POINT('Ctrl Pts',(-16.071174096646,12.8948251888563,131.680693404511)) ;
#131260 = CARTESIAN_POINT('Ctrl Pts',(-16.1378143759152,12.6613614393991,
131.842219614895)) ;
#131261 = CARTESIAN_POINT('Ctrl Pts',(-16.2222899580583,12.4827884864443,
132.055914031115)) ;
#131262 = CARTESIAN_POINT('Ctrl Pts',(-16.3195947643377,12.3713198999723,
132.307032186213)) ;
#131263 = CARTESIAN_POINT('Ctrl Pts',(-16.42316155049,12.3351536539427,132.576506572357)) ;
#131264 = CARTESIAN_POINT('Ctrl Pts',(-16.5269587087536,12.3771106003778,
132.846499102918)) ;
#131265 = CARTESIAN_POINT('Ctrl Pts',(-16.6232634802675,12.493746042562,133.094781650953)) ;
#131266 = CARTESIAN_POINT('Ctrl Pts',(-16.7066715515362,12.6767291405437,
133.30534152523)) ;
#131267 = CARTESIAN_POINT('Ctrl Pts',(-16.7719969184263,12.9147362953278,
133.462888792416)) ;
#131268 = CARTESIAN_POINT('Ctrl Pts',(-16.8145117924752,13.1870897175325,
133.554081812245)) ;
#131269 = CARTESIAN_POINT('Ctrl Pts',(-16.832664410647,13.4771402294594,133.573993886311)) ;
#131270 = CARTESIAN_POINT('Ctrl Pts',(-16.8255195547471,13.7642376991577,
133.519905575425)) ;
#131271 = CARTESIAN_POINT('Ctrl Pts',(-16.7943070458963,14.0261140050281,
133.395578546783)) ;
#131272 = CARTESIAN_POINT('Ctrl Pts',(-16.7424882598997,14.2437566095146,
133.211251228587)) ;
#131273 = CARTESIAN_POINT('Ctrl Pts',(-16.6736113908412,14.4043004510961,
132.976804095223)) ;
#131274 = CARTESIAN_POINT('Ctrl Pts',(-16.5942186823598,14.4936451763547,
132.711836822872)) ;
#131275 = CARTESIAN_POINT('Ctrl Pts',(-16.5101466580755,14.5067755223083,
132.433108081231)) ;
#131276 = CARTESIAN_POINT('Ctrl Pts',(-16.4282410882398,14.4421251633059,
132.160681842967)) ;
#131277 = CARTESIAN_POINT('Ctrl Pts',(-16.3551632521983,14.3039891726026,
131.914003956164)) ;
#131278 = CARTESIAN_POINT('Ctrl Pts',(-16.2972497108617,14.1040922169467,
131.711842779145)) ;
#131279 = CARTESIAN_POINT('Ctrl Pts',(-16.2585983326173,13.8535852347893,
131.565668552377)) ;
#131280 = CARTESIAN_POINT('Ctrl Pts',(-16.243420453165,13.5730952435811,131.488208101679)) ;
#131281 = CARTESIAN_POINT('Ctrl Pts',(-16.2531006198612,13.2829861782011,
131.483481649537)) ;
#131282 = CARTESIAN_POINT('Ctrl Pts',(-16.2877661805878,13.0017737284941,
131.551621835108)) ;
#131283 = CARTESIAN_POINT('Ctrl Pts',(-16.3459738367156,12.7500890797144,
131.688431825914)) ;
#131284 = CARTESIAN_POINT('Ctrl Pts',(-16.4238184818004,12.5475577998432,
131.882729415997)) ;
#131285 = CARTESIAN_POINT('Ctrl Pts',(-16.5167586194788,12.4075652478031,
132.121078295711)) ;
#131286 = CARTESIAN_POINT('Ctrl Pts',(-16.6183907518262,12.3405227377109,
132.384938789592)) ;
#131287 = CARTESIAN_POINT('Ctrl Pts',(-16.7229364475564,12.3506975715296,
132.657173213167)) ;
#131288 = CARTESIAN_POINT('Ctrl Pts',(-16.8232859030364,12.438177489278,132.917122022405)) ;
#131289 = CARTESIAN_POINT('Ctrl Pts',(-16.9125712124386,12.5958827964123,
133.1448620791)) ;
#131290 = CARTESIAN_POINT('Ctrl Pts',(-16.9854582743437,12.8123887822574,
133.324729525533)) ;
#131291 = CARTESIAN_POINT('Ctrl Pts',(-17.037709893631,13.0732934241726,133.444215844693)) ;
#131292 = CARTESIAN_POINT('Ctrl Pts',(-17.0659638164382,13.3601444544887,
133.493509177191)) ;
#131293 = CARTESIAN_POINT('Ctrl Pts',(-17.0689675284249,13.6487324697402,
133.469363185352)) ;
#131294 = CARTESIAN_POINT('Ctrl Pts',(-17.0474035047278,13.9231969052117,
133.37321432911)) ;
#131295 = CARTESIAN_POINT('Ctrl Pts',(-17.0033733673897,14.1616648845749,
133.211459633651)) ;
#131296 = CARTESIAN_POINT('Ctrl Pts',(-16.9406158991401,14.3474885130478,
132.994912465869)) ;
#131297 = CARTESIAN_POINT('Ctrl Pts',(-16.864876505793,14.4664584587802,132.740606759249)) ;
#131298 = CARTESIAN_POINT('Ctrl Pts',(-16.7814776117931,14.5109046603937,
132.463712586271)) ;
#131299 = CARTESIAN_POINT('Ctrl Pts',(-16.6983907346783,14.477538406395,132.188050973166)) ;
#131300 = CARTESIAN_POINT('Ctrl Pts',(-16.6207705482251,14.3681997132881,
131.928042842248)) ;
#131301 = CARTESIAN_POINT('Ctrl Pts',(-16.5561356079281,14.19161807787,131.706168442298)) ;
#131302 = CARTESIAN_POINT('Ctrl Pts',(-16.5092308734292,13.9603524956053,
131.536079167786)) ;
#131303 = CARTESIAN_POINT('Ctrl Pts',(-16.4841796106604,13.6895220911817,
131.429699941359)) ;
#131304 = CARTESIAN_POINT('Ctrl Pts',(-16.4836919093705,13.4007319641459,
131.395211960917)) ;
#131305 = CARTESIAN_POINT('Ctrl Pts',(-16.5082964988508,13.1132078283894,
131.433992211526)) ;
#131306 = CARTESIAN_POINT('Ctrl Pts',(-16.5574784700436,12.8466068578935,
131.544388229293)) ;
#131307 = CARTESIAN_POINT('Ctrl Pts',(-16.6273997075169,12.6236984730367,
131.715716955648)) ;
#131308 = CARTESIAN_POINT('Ctrl Pts',(-16.7150468521775,12.4561011970055,
131.938529922164)) ;
#131309 = CARTESIAN_POINT('Ctrl Pts',(-16.8139682824648,12.3585968124196,
132.194412407875)) ;
#131310 = CARTESIAN_POINT('Ctrl Pts',(-16.9182265147246,12.3371246735504,
132.465833558649)) ;
#131311 = CARTESIAN_POINT('Ctrl Pts',(-17.0209026074425,12.3935413485491,
132.732653318412)) ;
#131312 = CARTESIAN_POINT('Ctrl Pts',(-17.1153756443262,12.5236723848828,
132.975519307564)) ;
#131313 = CARTESIAN_POINT('Ctrl Pts',(-17.1956555914022,12.7179304240541,
133.176947444366)) ;
#131314 = CARTESIAN_POINT('Ctrl Pts',(-17.2569924030211,12.9643000603806,
133.322838842009)) ;
#131315 = CARTESIAN_POINT('Ctrl Pts',(-17.2949538933717,13.2410161239663,
133.400773057716)) ;
#131316 = CARTESIAN_POINT('Ctrl Pts',(-17.3083412632257,13.5320326358814,
133.40675253041)) ;
#131317 = CARTESIAN_POINT('Ctrl Pts',(-17.2965889183178,13.8151976332958,
133.339306952295)) ;
#131318 = CARTESIAN_POINT('Ctrl Pts',(-17.2611712342104,14.070965110173,133.202631251777)) ;
#131319 = CARTESIAN_POINT('Ctrl Pts',(-17.2055219190199,14.2795161854134,
133.006946181317)) ;
#131320 = CARTESIAN_POINT('Ctrl Pts',(-17.1344526197165,14.4266233568165,
132.766264881813)) ;
#131321 = CARTESIAN_POINT('Ctrl Pts',(-17.0535835623515,14.5021444966585,
132.496922447555)) ;
#131322 = CARTESIAN_POINT('Ctrl Pts',(-16.9693534559784,14.5004799279669,
132.217713549754)) ;
#131323 = CARTESIAN_POINT('Ctrl Pts',(-16.8885085804287,14.4210758361391,
131.948320350664)) ;
#131324 = CARTESIAN_POINT('Ctrl Pts',(-16.818249196986,14.2711637356508,131.710095463003)) ;
#131325 = CARTESIAN_POINT('Ctrl Pts',(-16.7633840110066,14.0600320259714,
131.516677712646)) ;
#131326 = CARTESIAN_POINT('Ctrl Pts',(-16.729034656478,13.8025046463563,131.383125760343)) ;
#131327 = CARTESIAN_POINT('Ctrl Pts',(-16.7184105236858,13.5194350300881,
131.319077858953)) ;
#131328 = CARTESIAN_POINT('Ctrl Pts',(-16.7329082611137,13.227929848522,131.328230796269)) ;
#131329 = CARTESIAN_POINT('Ctrl Pts',(-16.7721540100418,12.9514279979351,
131.409809044102)) ;
#131330 = CARTESIAN_POINT('Ctrl Pts',(-16.834426980546,12.7076270254922,131.558495828173)) ;
#131331 = CARTESIAN_POINT('Ctrl Pts',(-16.9152315370478,12.5164543914562,
131.761543944961)) ;
#131332 = CARTESIAN_POINT('Ctrl Pts',(-17.0104958015721,12.3891143889345,
132.006622580848)) ;
#131333 = CARTESIAN_POINT('Ctrl Pts',(-17.1132917121907,12.3364756158918,
132.273826383176)) ;
#131334 = CARTESIAN_POINT('Ctrl Pts',(-17.2173332534644,12.3612642231578,
132.54465957405)) ;
#131335 = CARTESIAN_POINT('Ctrl Pts',(-17.3163641429157,12.4629838840005,
132.800676032605)) ;
#131336 = CARTESIAN_POINT('Ctrl Pts',(-17.4026407183266,12.6321971699934,
133.01975282772)) ;
#131337 = CARTESIAN_POINT('Ctrl Pts',(-17.472100457449,12.8584558798932,133.189548524182)) ;
#131338 = CARTESIAN_POINT('Ctrl Pts',(-17.5200564206003,13.1261648647243,
133.296424663186)) ;
#131339 = CARTESIAN_POINT('Ctrl Pts',(-17.5435329958318,13.4141234552309,
133.331916813786)) ;
#131340 = CARTESIAN_POINT('Ctrl Pts',(-17.5418705107985,13.7023852342343,
133.294006470842)) ;
#131341 = CARTESIAN_POINT('Ctrl Pts',(-17.515866367185,13.9714212012371,133.184910655295)) ;
#131342 = CARTESIAN_POINT('Ctrl Pts',(-17.4677121548387,14.202020081249,133.01095053406)) ;
#131343 = CARTESIAN_POINT('Ctrl Pts',(-17.4023716167183,14.3750071736422,
132.787065724901)) ;
#131344 = CARTESIAN_POINT('Ctrl Pts',(-17.3247668097447,14.4806351346196,
132.527282453733)) ;
#131345 = CARTESIAN_POINT('Ctrl Pts',(-17.2410054869792,14.5105855297535,
132.24943004058)) ;
#131346 = CARTESIAN_POINT('Ctrl Pts',(-17.1581501091636,14.4625550657111,
131.974268906069)) ;
#131347 = CARTESIAN_POINT('Ctrl Pts',(-17.0827332780509,14.3400369417443,
131.720826863696)) ;
#131348 = CARTESIAN_POINT('Ctrl Pts',(-17.0209888868574,14.1521957535254,
131.507380128005)) ;
#131349 = CARTESIAN_POINT('Ctrl Pts',(-16.9778207788142,13.9116489154345,
131.348115653949)) ;
#131350 = CARTESIAN_POINT('Ctrl Pts',(-16.9572990580186,13.6358544266559,
131.25499330384)) ;
#131351 = CARTESIAN_POINT('Ctrl Pts',(-16.9615071381463,13.3459427675745,
131.23424300822)) ;
#131352 = CARTESIAN_POINT('Ctrl Pts',(-16.9909211180614,13.0604649745041,
131.286996740778)) ;
#131353 = CARTESIAN_POINT('Ctrl Pts',(-17.0441007990242,12.8015143832803,
131.409241549806)) ;
#131354 = CARTESIAN_POINT('Ctrl Pts',(-17.1180304186239,12.586871423154,131.592073079015)) ;
#131355 = CARTESIAN_POINT('Ctrl Pts',(-17.2080500636742,12.4323032180318,
131.821934768459)) ;
#131356 = CARTESIAN_POINT('Ctrl Pts',(-17.3084611337155,12.348604012381,132.082157360211)) ;
#131357 = CARTESIAN_POINT('Ctrl Pts',(-17.4130111461555,12.3418345254331,
132.3544143668)) ;
#131358 = CARTESIAN_POINT('Ctrl Pts',(-17.5146765749007,12.4127257697425,
132.618266949295)) ;
#131359 = CARTESIAN_POINT('Ctrl Pts',(-17.606721170884,12.5554430365515,132.854114383774)) ;
#131360 = CARTESIAN_POINT('Ctrl Pts',(-17.6839111619126,12.7608029240068,
133.046442139626)) ;
#131361 = CARTESIAN_POINT('Ctrl Pts',(-17.7410331806284,13.0143079229722,
133.180091411217)) ;
#131362 = CARTESIAN_POINT('Ctrl Pts',(-17.7745360164768,13.2953661026702,
133.244952941826)) ;
#131363 = CARTESIAN_POINT('Ctrl Pts',(-17.7831520054483,13.587499191953,133.236886150184)) ;
#131364 = CARTESIAN_POINT('Ctrl Pts',(-17.7666348632763,13.8669338626205,
133.155497022517)) ;
#131365 = CARTESIAN_POINT('Ctrl Pts',(-17.7273863718362,14.1134263503453,
133.007875421063)) ;
#131366 = CARTESIAN_POINT('Ctrl Pts',(-17.6683893078491,14.3121780897716,
132.802342611055)) ;
#131367 = CARTESIAN_POINT('Ctrl Pts',(-17.5946147982464,14.4470050265316,
132.553591742459)) ;
#131368 = CARTESIAN_POINT('Ctrl Pts',(-17.5125911040324,14.5078086325279,
132.280874384855)) ;
#131369 = CARTESIAN_POINT('Ctrl Pts',(-17.4289255794743,14.4913412737729,
132.003473976216)) ;
#131370 = CARTESIAN_POINT('Ctrl Pts',(-17.3497030184291,14.3985299043882,
131.738923406222)) ;
#131371 = CARTESIAN_POINT('Ctrl Pts',(-17.2814947859058,14.2353764928408,
131.506472748856)) ;
#131372 = CARTESIAN_POINT('Ctrl Pts',(-17.2301833982271,14.0132824388172,
131.32333677435)) ;
#131373 = CARTESIAN_POINT('Ctrl Pts',(-17.2003726149901,13.751770584179,131.203370984278)) ;
#131374 = CARTESIAN_POINT('Ctrl Pts',(-17.1942692410409,13.4639004603942,
131.15229798358)) ;
#131375 = CARTESIAN_POINT('Ctrl Pts',(-17.2136563233809,13.1736259559936,
131.175755585428)) ;
#131376 = CARTESIAN_POINT('Ctrl Pts',(-17.2572199771084,12.9029494351804,
131.270058586451)) ;
#131377 = CARTESIAN_POINT('Ctrl Pts',(-17.3234518657098,12.6670694829694,
131.430263375814)) ;
#131378 = CARTESIAN_POINT('Ctrl Pts',(-17.4076950363158,12.4867414535482,
131.643224441991)) ;
#131379 = CARTESIAN_POINT('Ctrl Pts',(-17.5042594533731,12.3736046950475,
131.892333562312)) ;
#131380 = CARTESIAN_POINT('Ctrl Pts',(-17.6083225797878,12.3351061359291,
132.163067552705)) ;
#131381 = CARTESIAN_POINT('Ctrl Pts',(-17.7115102747659,12.3747297412366,
132.431506046747)) ;
#131382 = CARTESIAN_POINT('Ctrl Pts',(-17.80835655534,12.4890530273647,132.681306942846)) ;
#131383 = CARTESIAN_POINT('Ctrl Pts',(-17.8927139370083,12.6718473822343,
132.894413198474)) ;
#131384 = CARTESIAN_POINT('Ctrl Pts',(-17.9581348743092,12.9071471042355,
133.05245843071)) ;
#131385 = CARTESIAN_POINT('Ctrl Pts',(-18.0014489044881,13.1791583633753,
133.145922177929)) ;
#131386 = CARTESIAN_POINT('Ctrl Pts',(-18.020261151911,13.4685703303894,133.16781609884)) ;
#131387 = CARTESIAN_POINT('Ctrl Pts',(-18.0138792132709,13.7556865610863,
133.115998787948)) ;
#131388 = CARTESIAN_POINT('Ctrl Pts',(-17.9834392562243,14.0184520779736,
132.993960277943)) ;
#131389 = CARTESIAN_POINT('Ctrl Pts',(-17.9319093006337,14.2386835545227,
132.810307624848)) ;
#131390 = CARTESIAN_POINT('Ctrl Pts',(-17.8634196060343,14.4009245247973,
132.577005577925)) ;
#131391 = CARTESIAN_POINT('Ctrl Pts',(-17.7839956342627,14.4923209079493,
132.311848278652)) ;
#131392 = CARTESIAN_POINT('Ctrl Pts',(-17.7003715420016,14.5074993821674,
132.034597515729)) ;
#131393 = CARTESIAN_POINT('Ctrl Pts',(-17.6179715693461,14.4446391320812,
131.760580504429)) ;
#131394 = CARTESIAN_POINT('Ctrl Pts',(-17.5449472629492,14.309013886893,131.514230915999)) ;
#131395 = CARTESIAN_POINT('Ctrl Pts',(-17.4863929079662,14.1104149351794,
131.310125649846)) ;
#131396 = CARTESIAN_POINT('Ctrl Pts',(-17.4472233098488,13.8614588559076,
131.162498832848)) ;
#131397 = CARTESIAN_POINT('Ctrl Pts',(-17.4312869960412,13.5819687002437,
131.082859767227)) ;
#131398 = CARTESIAN_POINT('Ctrl Pts',(-17.4402797073093,13.2906279013141,
131.075985151787)) ;
#131399 = CARTESIAN_POINT('Ctrl Pts',(-17.4743143198391,13.009243305788,131.142317233284)) ;
#131400 = CARTESIAN_POINT('Ctrl Pts',(-17.5315517099284,12.7575168112921,
131.276452625469)) ;
#131401 = CARTESIAN_POINT('Ctrl Pts',(-17.6091410096472,12.5525240138587,
131.469879021206)) ;
#131402 = CARTESIAN_POINT('Ctrl Pts',(-17.7014737885802,12.4108770336832,
131.706544893167)) ;
#131403 = CARTESIAN_POINT('Ctrl Pts',(-17.8032831969416,12.3412909140522,
131.97080490142)) ;
#131404 = CARTESIAN_POINT('Ctrl Pts',(-17.9077079735701,12.3493861735078,
132.242732393973)) ;
#131405 = CARTESIAN_POINT('Ctrl Pts',(-18.0080021312736,12.4342727909203,
132.502613425746)) ;
#131406 = CARTESIAN_POINT('Ctrl Pts',(-18.097851259794,12.5900489009072,132.731956223757)) ;
#131407 = CARTESIAN_POINT('Ctrl Pts',(-18.1714811565311,12.8056265995217,
132.913906681068)) ;
#131408 = CARTESIAN_POINT('Ctrl Pts',(-18.2242791522083,13.0653848746049,
133.035014327401)) ;
#131409 = CARTESIAN_POINT('Ctrl Pts',(-18.2532373491338,13.3504851063388,
133.086511791274)) ;
#131410 = CARTESIAN_POINT('Ctrl Pts',(-18.2570176970517,13.6412798147236,
133.064399324168)) ;
#131411 = CARTESIAN_POINT('Ctrl Pts',(-18.2361288879767,13.915548156852,132.970331104728)) ;
#131412 = CARTESIAN_POINT('Ctrl Pts',(-18.1927521468012,14.1552942040558,
132.810491998612)) ;
#131413 = CARTESIAN_POINT('Ctrl Pts',(-18.1304889717146,14.3429101935435,
132.595396822877)) ;
#131414 = CARTESIAN_POINT('Ctrl Pts',(-18.0549535994053,14.4639893047867,
132.341644352442)) ;
#131415 = CARTESIAN_POINT('Ctrl Pts',(-17.9720169774795,14.5107279953385,
132.066239556179)) ;
#131416 = CARTESIAN_POINT('Ctrl Pts',(-17.88839874123,14.4794893752074,131.788842595817)) ;
#131417 = CARTESIAN_POINT('Ctrl Pts',(-17.8108656194136,14.3727211578977,
131.529246532274)) ;
#131418 = CARTESIAN_POINT('Ctrl Pts',(-17.7456151211965,14.1977799584113,
131.305501822006)) ;
#131419 = CARTESIAN_POINT('Ctrl Pts',(-17.6981151394564,13.9680803032242,
131.13369579038)) ;
#131420 = CARTESIAN_POINT('Ctrl Pts',(-17.6723054333923,13.6967826933105,
131.024941140418)) ;
#131421 = CARTESIAN_POINT('Ctrl Pts',(-17.6711447708163,13.4094043760888,
130.98862536116)) ;
#131422 = CARTESIAN_POINT('Ctrl Pts',(-17.6950445630246,13.1212039321583,
131.025303143358)) ;
#131423 = CARTESIAN_POINT('Ctrl Pts',(-17.74333311896,12.8546896237207,131.133221894845)) ;
#131424 = CARTESIAN_POINT('Ctrl Pts',(-17.81282756458,12.6293810356165,131.303196900116)) ;
#131425 = CARTESIAN_POINT('Ctrl Pts',(-17.9005194706817,12.4594635396626,
131.525988684649)) ;
#131426 = CARTESIAN_POINT('Ctrl Pts',(-17.9986989569018,12.3604529302704,
131.779876218196)) ;
#131427 = CARTESIAN_POINT('Ctrl Pts',(-18.1032340963646,12.3366695079855,
132.05199660503)) ;
#131428 = CARTESIAN_POINT('Ctrl Pts',(-18.2056125319901,12.3907630606801,
132.318086056791)) ;
#131429 = CARTESIAN_POINT('Ctrl Pts',(-18.300613364825,12.5187717527639,132.562441868016)) ;
#131430 = CARTESIAN_POINT('Ctrl Pts',(-18.3816465085652,12.7125553045139,
132.765918032423)) ;
#131431 = CARTESIAN_POINT('Ctrl Pts',(-18.4429853099616,12.9551208485313,
132.912159665352)) ;
#131432 = CARTESIAN_POINT('Ctrl Pts',(-18.4820336765163,13.2325620060974,
132.993078593711)) ;
#131433 = CARTESIAN_POINT('Ctrl Pts',(-18.496084383933,13.5243419796884,133.00090515124)) ;
#131434 = CARTESIAN_POINT('Ctrl Pts',(-18.4850639350324,13.8069926528057,
132.935714610325)) ;
#131435 = CARTESIAN_POINT('Ctrl Pts',(-18.4503367662865,14.0639000199269,
132.801056058483)) ;
#131436 = CARTESIAN_POINT('Ctrl Pts',(-18.3952268191814,14.2741558930926,
132.606941700926)) ;
#131437 = CARTESIAN_POINT('Ctrl Pts',(-18.3243680288223,14.4234615625839,
132.366801537788)) ;
#131438 = CARTESIAN_POINT('Ctrl Pts',(-18.2437816042926,14.5011170686614,
132.098327447916)) ;
#131439 = CARTESIAN_POINT('Ctrl Pts',(-18.1592384984199,14.5013614779113,
131.81807310291)) ;
#131440 = CARTESIAN_POINT('Ctrl Pts',(-18.0789307375107,14.4249956630962,
131.550560960519)) ;
#131441 = CARTESIAN_POINT('Ctrl Pts',(-18.0076541118125,14.2760171565871,
131.309082565097)) ;
#131442 = CARTESIAN_POINT('Ctrl Pts',(-17.9524899575172,14.0665442400002,
131.114862544505)) ;
#131443 = CARTESIAN_POINT('Ctrl Pts',(-17.9175014310239,13.8110528410318,
130.979547647309)) ;
#131444 = CARTESIAN_POINT('Ctrl Pts',(-17.9061688391216,13.5262786463887,
130.913174372637)) ;
#131445 = CARTESIAN_POINT('Ctrl Pts',(-17.919877948496,13.2368369901033,130.920277108179)) ;
#131446 = CARTESIAN_POINT('Ctrl Pts',(-17.9586197277239,12.9583255903659,
131.000212959745)) ;
#131447 = CARTESIAN_POINT('Ctrl Pts',(-18.0199083066583,12.7145800096232,
131.146219952724)) ;
#131448 = CARTESIAN_POINT('Ctrl Pts',(-18.1009974511921,12.5201730384604,
131.349794172582)) ;
#131449 = CARTESIAN_POINT('Ctrl Pts',(-18.1949562384929,12.392297716127,131.59141902566)) ;
#131450 = CARTESIAN_POINT('Ctrl Pts',(-18.2981754606917,12.3368042043637,
131.859663996403)) ;
#131451 = CARTESIAN_POINT('Ctrl Pts',(-18.4019398290045,12.3594079574846,
132.129799825424)) ;
#131452 = CARTESIAN_POINT('Ctrl Pts',(-18.5013383418749,12.4588426243277,
132.386856715267)) ;
#131453 = CARTESIAN_POINT('Ctrl Pts',(-18.5881323912535,12.6263832935465,
132.607414342136)) ;
#131454 = CARTESIAN_POINT('Ctrl Pts',(-18.6581587702516,12.8513078071139,
132.778854814353)) ;
#131455 = CARTESIAN_POINT('Ctrl Pts',(-18.7067345904951,13.1175341941134,
132.887608467018)) ;
#131456 = CARTESIAN_POINT('Ctrl Pts',(-18.731003412201,13.4059954970849,132.925314381533)) ;
#131457 = CARTESIAN_POINT('Ctrl Pts',(-18.7300968071152,13.6942419645787,
132.889656262388)) ;
#131458 = CARTESIAN_POINT('Ctrl Pts',(-18.7044541735128,13.9656571359195,
132.781395875164)) ;
#131459 = CARTESIAN_POINT('Ctrl Pts',(-18.6575265026644,14.1945698215837,
132.611470543872)) ;
#131460 = CARTESIAN_POINT('Ctrl Pts',(-18.5922406519204,14.3711224528334,
132.387486886082)) ;
#131461 = CARTESIAN_POINT('Ctrl Pts',(-18.5149037393986,14.4785950091488,
132.128508392993)) ;
#131462 = CARTESIAN_POINT('Ctrl Pts',(-18.4311371510558,14.5108133112394,
131.850601957705)) ;
#131463 = CARTESIAN_POINT('Ctrl Pts',(-18.3483146549276,14.4650394200622,
131.575598992863)) ;
#131464 = CARTESIAN_POINT('Ctrl Pts',(-18.2726066198908,14.3446919400874,
131.321313280288)) ;
#131465 = CARTESIAN_POINT('Ctrl Pts',(-18.2103307361537,14.1586507898245,
131.106307024848)) ;
#131466 = CARTESIAN_POINT('Ctrl Pts',(-18.1664432390162,13.9182142591253,
130.944795156692)) ;
#131467 = CARTESIAN_POINT('Ctrl Pts',(-18.1453636366719,13.6446894301756,
130.850233747273)) ;
#131468 = CARTESIAN_POINT('Ctrl Pts',(-18.1488348343508,13.3538163555555,
130.82719813754)) ;
#131469 = CARTESIAN_POINT('Ctrl Pts',(-18.1774811245967,13.0687529323482,
130.877811758373)) ;
#131470 = CARTESIAN_POINT('Ctrl Pts',(-18.2300437642224,12.8084025711039,
130.998208929724)) ;
#131471 = CARTESIAN_POINT('Ctrl Pts',(-18.3034001053734,12.5923662507696,
131.179384620874)) ;
#131472 = CARTESIAN_POINT('Ctrl Pts',(-18.3931634370597,12.4355966936421,
131.408445657945)) ;
#131473 = CARTESIAN_POINT('Ctrl Pts',(-18.4935575860177,12.3498834173245,
131.668562849344)) ;
#131474 = CARTESIAN_POINT('Ctrl Pts',(-18.5975530541275,12.3409542808635,
131.939369081028)) ;
#131475 = CARTESIAN_POINT('Ctrl Pts',(-18.6994673351223,12.4093757248112,
132.203931136602)) ;
#131476 = CARTESIAN_POINT('Ctrl Pts',(-18.7921201529756,12.5505196315372,
132.441467645947)) ;
#131477 = CARTESIAN_POINT('Ctrl Pts',(-18.8697017731338,12.7541803006072,
132.634971878383)) ;
#131478 = CARTESIAN_POINT('Ctrl Pts',(-18.9273307484839,13.0055267425044,
132.770220733639)) ;
#131479 = CARTESIAN_POINT('Ctrl Pts',(-18.9617100390982,13.2870724884799,
132.83751270461)) ;
#131480 = CARTESIAN_POINT('Ctrl Pts',(-18.9710255677151,13.5781354317469,
132.831615285865)) ;
#131481 = CARTESIAN_POINT('Ctrl Pts',(-18.9553578084607,13.8583662507443,
132.752702523973)) ;
#131482 = CARTESIAN_POINT('Ctrl Pts',(-18.9165383575917,14.1072755060793,
132.606171710367)) ;
#131483 = CARTESIAN_POINT('Ctrl Pts',(-18.8581587772242,14.3069765889331,
132.4025330216)) ;
#131484 = CARTESIAN_POINT('Ctrl Pts',(-18.7850681968336,14.443614067786,132.155907192059)) ;
#131485 = CARTESIAN_POINT('Ctrl Pts',(-18.702941141321,14.5071928082345,131.882773592227)) ;
#131486 = CARTESIAN_POINT('Ctrl Pts',(-18.6190408117616,14.4928945220509,
131.604612881179)) ;
#131487 = CARTESIAN_POINT('Ctrl Pts',(-18.5396187459799,14.4021254936154,
131.339485656911)) ;
#131488 = CARTESIAN_POINT('Ctrl Pts',(-18.4711933901986,14.2413770477371,
131.106496569037)) ;
#131489 = CARTESIAN_POINT('Ctrl Pts',(-18.4192605637911,14.0210258594474,
130.921552581758)) ;
#131490 = CARTESIAN_POINT('Ctrl Pts',(-18.3886405960536,13.7594508415378,
130.799092122936)) ;
#131491 = CARTESIAN_POINT('Ctrl Pts',(-18.381928462571,13.4716753030503,130.746210031867)) ;
#131492 = CARTESIAN_POINT('Ctrl Pts',(-18.4004216312574,13.18278007244,130.767242888151)) ;
#131493 = CARTESIAN_POINT('Ctrl Pts',(-18.4435339670258,12.9097866347109,
130.860039653288)) ;
#131494 = CARTESIAN_POINT('Ctrl Pts',(-18.5088204983959,12.6739761120234,
131.017674750893)) ;
#131495 = CARTESIAN_POINT('Ctrl Pts',(-18.5926770612546,12.4911376353209,
131.229439455072)) ;
#131496 = CARTESIAN_POINT('Ctrl Pts',(-18.6895108158381,12.3755758788311,
131.479159592622)) ;
#131497 = CARTESIAN_POINT('Ctrl Pts',(-18.7928542788589,12.3352662329562,
131.747989657394)) ;
#131498 = CARTESIAN_POINT('Ctrl Pts',(-18.8962659376777,12.3722006143293,
132.017051741353)) ;
#131499 = CARTESIAN_POINT('Ctrl Pts',(-18.9940984306609,12.4858118722087,
132.26946955847)) ;
#131500 = CARTESIAN_POINT('Ctrl Pts',(-19.0779483654093,12.6649628027199,
132.481462828409)) ;
#131501 = CARTESIAN_POINT('Ctrl Pts',(-19.144324386781,12.8995424291904,132.64216747859)) ;
#131502 = CARTESIAN_POINT('Ctrl Pts',(-19.1882893988472,13.1707489990253,
132.73754255469)) ;
#131503 = CARTESIAN_POINT('Ctrl Pts',(-19.2078747746244,13.4602465419289,
132.76165779285)) ;
#131504 = CARTESIAN_POINT('Ctrl Pts',(-19.2021695943243,13.7479094104328,
132.711797460233)) ;
#131505 = CARTESIAN_POINT('Ctrl Pts',(-19.1724541288044,14.0110933638022,
132.591943088721)) ;
#131506 = CARTESIAN_POINT('Ctrl Pts',(-19.1214789970609,14.2330195298938,
132.409891780119)) ;
#131507 = CARTESIAN_POINT('Ctrl Pts',(-19.0533824116154,14.397056415232,132.177734508543)) ;
#131508 = CARTESIAN_POINT('Ctrl Pts',(-18.9744610193818,14.4906410938832,
131.914150162339)) ;
#131509 = CARTESIAN_POINT('Ctrl Pts',(-18.890345578861,14.5080280130628,131.635247249356)) ;
#131510 = CARTESIAN_POINT('Ctrl Pts',(-18.8085392860132,14.4480725424633,
131.363277720596)) ;
#131511 = CARTESIAN_POINT('Ctrl Pts',(-18.7346273925197,14.3139470607326,
131.114108989611)) ;
#131512 = CARTESIAN_POINT('Ctrl Pts',(-18.6756142626322,14.1169437524237,
130.908679443903)) ;
#131513 = CARTESIAN_POINT('Ctrl Pts',(-18.6357563526766,13.8684682048696,
130.758950982595)) ;
#131514 = CARTESIAN_POINT('Ctrl Pts',(-18.6192189361488,13.5907243651,130.677694418299)) ;
#131515 = CARTESIAN_POINT('Ctrl Pts',(-18.6274186795787,13.2994062522709,
130.668497076563)) ;
#131516 = CARTESIAN_POINT('Ctrl Pts',(-18.6607053713449,13.0173302811176,
130.732637587237)) ;
#131517 = CARTESIAN_POINT('Ctrl Pts',(-18.7175745221499,12.7634586998748,
130.865557336184)) ;
#131518 = CARTESIAN_POINT('Ctrl Pts',(-18.7946062779487,12.5574053612187,
131.057405473283)) ;
#131519 = CARTESIAN_POINT('Ctrl Pts',(-18.8863176363417,12.4141338116398,
131.292346024062)) ;
#131520 = CARTESIAN_POINT('Ctrl Pts',(-18.9880396659882,12.342233208706,131.556318246303)) ;
#131521 = CARTESIAN_POINT('Ctrl Pts',(-19.092367557879,12.3479816385131,131.828001920729)) ;
#131522 = CARTESIAN_POINT('Ctrl Pts',(-19.1930265312653,12.4308508598937,
132.088893600864)) ;
#131523 = CARTESIAN_POINT('Ctrl Pts',(-19.2830355733598,12.5841342714032,
132.318802233278)) ;
#131524 = CARTESIAN_POINT('Ctrl Pts',(-19.3575448753726,12.7991564308112,
132.503166321675)) ;
#131525 = CARTESIAN_POINT('Ctrl Pts',(-19.410786935153,13.0569999610756,132.625693509338)) ;
#131526 = CARTESIAN_POINT('Ctrl Pts',(-19.4405356262244,13.3421921034464,
132.679428679679)) ;
#131527 = CARTESIAN_POINT('Ctrl Pts',(-19.4450790880921,13.6321454574867,
132.659662972591)) ;
#131528 = CARTESIAN_POINT('Ctrl Pts',(-19.4247875387373,13.9089725412032,
132.567125349093)) ;
#131529 = CARTESIAN_POINT('Ctrl Pts',(-19.381825668748,14.1498188340954,132.408476398238)) ;
#131530 = CARTESIAN_POINT('Ctrl Pts',(-19.3204518279194,14.3379335225619,
132.196198119276)) ;
#131531 = CARTESIAN_POINT('Ctrl Pts',(-19.2450347897687,14.4615825769609,
131.942693860373)) ;
#131532 = CARTESIAN_POINT('Ctrl Pts',(-19.162267963524,14.5104718339952,131.667809535155)) ;
#131533 = CARTESIAN_POINT('Ctrl Pts',(-19.0783524563333,14.4813917081873,
131.389457000585)) ;
#131534 = CARTESIAN_POINT('Ctrl Pts',(-19.0006162859046,14.3764101476522,
131.129272642533)) ;
#131535 = CARTESIAN_POINT('Ctrl Pts',(-18.9351626104612,14.2041613001764,
130.905077291113)) ;
#131536 = CARTESIAN_POINT('Ctrl Pts',(-18.8868641696125,13.9743839791119,
130.730738018104)) ;
#131537 = CARTESIAN_POINT('Ctrl Pts',(-18.8605695212481,13.7063210401926,
130.620861352139)) ;
#131538 = CARTESIAN_POINT('Ctrl Pts',(-18.8586114405782,13.416701167449,130.581917827711)) ;
#131539 = CARTESIAN_POINT('Ctrl Pts',(-18.8818454285258,13.1291677758352,
130.616763647551)) ;
#131540 = CARTESIAN_POINT('Ctrl Pts',(-18.9294289009308,12.86171027905,130.722620411742)) ;
#131541 = CARTESIAN_POINT('Ctrl Pts',(-18.9984336324713,12.6350478480017,
130.891152728659)) ;
#131542 = CARTESIAN_POINT('Ctrl Pts',(-19.0852684560724,12.4638699665219,
131.111590594525)) ;
#131543 = CARTESIAN_POINT('Ctrl Pts',(-19.1836902605787,12.3621126869917,
131.366013493841)) ;
#131544 = CARTESIAN_POINT('Ctrl Pts',(-19.2880034593845,12.336288293437,131.637540200635)) ;
#131545 = CARTESIAN_POINT('Ctrl Pts',(-19.3907293591919,12.3882079133966,
131.9045787098)) ;
#131546 = CARTESIAN_POINT('Ctrl Pts',(-19.4861202999562,12.5148240028862,
132.150020522081)) ;
#131547 = CARTESIAN_POINT('Ctrl Pts',(-19.566984502277,12.7050812653244,132.353293437429)) ;
#131548 = CARTESIAN_POINT('Ctrl Pts',(-19.6294717703468,12.9482677220772,
132.502618790391)) ;
#131549 = CARTESIAN_POINT('Ctrl Pts',(-19.6689768655333,13.2238578222556,
132.585025535771)) ;
#131550 = CARTESIAN_POINT('Ctrl Pts',(-19.6838357324499,13.5162932448957,
132.595118812429)) ;
#131551 = CARTESIAN_POINT('Ctrl Pts',(-19.6735197937544,13.799165239793,132.532024333921)) ;
#131552 = CARTESIAN_POINT('Ctrl Pts',(-19.6392454600331,14.0580267764743,
132.398557205212)) ;
#131553 = CARTESIAN_POINT('Ctrl Pts',(-19.5848869196862,14.2686028129511,
132.206807442572)) ;
#131554 = CARTESIAN_POINT('Ctrl Pts',(-19.5145008411043,14.4199618502008,
131.968069495771)) ;
#131555 = CARTESIAN_POINT('Ctrl Pts',(-19.4340220268986,14.4998958219189,
131.699871465245)) ;
#131556 = CARTESIAN_POINT('Ctrl Pts',(-19.3495759662661,14.5025664794371,
131.419941342377)) ;
#131557 = CARTESIAN_POINT('Ctrl Pts',(-19.2688627445457,14.4280652825415,
131.151146889785)) ;
#131558 = CARTESIAN_POINT('Ctrl Pts',(-19.197514432747,14.2819177513075,130.909621465088)) ;
#131559 = CARTESIAN_POINT('Ctrl Pts',(-19.1413921728409,14.0723877227319,
130.712339919469)) ;
#131560 = CARTESIAN_POINT('Ctrl Pts',(-19.1060584048045,13.8191595273478,
130.576195818314)) ;
#131561 = CARTESIAN_POINT('Ctrl Pts',(-19.0939136018658,13.5356702848312,
130.507524027747)) ;
#131562 = CARTESIAN_POINT('Ctrl Pts',(-19.1068958007053,13.2451626614465,
130.512392184105)) ;
#131563 = CARTESIAN_POINT('Ctrl Pts',(-19.1449564065195,12.9658959397094,
130.5903314269)) ;
#131564 = CARTESIAN_POINT('Ctrl Pts',(-19.2057189790489,12.720867949973,130.73477557543)) ;
#131565 = CARTESIAN_POINT('Ctrl Pts',(-19.2858400354675,12.5256178596935,
130.935699785553)) ;
#131566 = CARTESIAN_POINT('Ctrl Pts',(-19.3800402811628,12.3947249390078,
131.177818876414)) ;
#131567 = CARTESIAN_POINT('Ctrl Pts',(-19.4831200353959,12.3373274128747,
131.445666380565)) ;
#131568 = CARTESIAN_POINT('Ctrl Pts',(-19.5867485454506,12.3577351376061,
131.715460652154)) ;
#131569 = CARTESIAN_POINT('Ctrl Pts',(-19.6862131801358,12.4546492514378,
131.972779675498)) ;
#131570 = CARTESIAN_POINT('Ctrl Pts',(-19.7738286134021,12.6210676591383,
132.195587853881)) ;
#131571 = CARTESIAN_POINT('Ctrl Pts',(-19.8442902702029,12.8446766854148,
132.368316433847)) ;
#131572 = CARTESIAN_POINT('Ctrl Pts',(-19.8933608798738,13.108808163257,132.478653710118)) ;
#131573 = CARTESIAN_POINT('Ctrl Pts',(-19.9184859283659,13.3979062620311,
132.518747291947)) ;
#131574 = CARTESIAN_POINT('Ctrl Pts',(-19.9181983031023,13.6859097607706,
132.484944374893)) ;
#131575 = CARTESIAN_POINT('Ctrl Pts',(-19.8935840118438,13.9567565280856,
132.379898432991)) ;
#131576 = CARTESIAN_POINT('Ctrl Pts',(-19.8465997978561,14.1899349125241,
132.209373856163)) ;
#131577 = CARTESIAN_POINT('Ctrl Pts',(-19.7823820361551,14.3662692626876,
131.988864508273)) ;
#131578 = CARTESIAN_POINT('Ctrl Pts',(-19.7048377925854,14.4768289979695,
131.729048105592)) ;
#131579 = CARTESIAN_POINT('Ctrl Pts',(-19.621356858463,14.5109207090365,131.452070562692)) ;
#131580 = CARTESIAN_POINT('Ctrl Pts',(-19.5383256537918,14.4673589954117,
131.176412965102)) ;
#131581 = CARTESIAN_POINT('Ctrl Pts',(-19.462343360731,14.3490298117359,130.921339630599)) ;
#131582 = CARTESIAN_POINT('Ctrl Pts',(-19.399598094763,14.1643442573792,130.70492417211)) ;
#131583 = CARTESIAN_POINT('Ctrl Pts',(-19.3553585530389,13.9269540764464,
130.542614298548)) ;
#131584 = CARTESIAN_POINT('Ctrl Pts',(-19.3333939719036,13.6529087066834,
130.44529695513)) ;
#131585 = CARTESIAN_POINT('Ctrl Pts',(-19.3361541913265,13.3625040426011,
130.420224634067)) ;
#131586 = CARTESIAN_POINT('Ctrl Pts',(-19.3641172961552,13.0764917625792,
130.468781137817)) ;
#131587 = CARTESIAN_POINT('Ctrl Pts',(-19.4160399610195,12.8152457852602,
130.587319851219)) ;
#131588 = CARTESIAN_POINT('Ctrl Pts',(-19.4888652574942,12.5977360848388,
130.766942106929)) ;
#131589 = CARTESIAN_POINT('Ctrl Pts',(-19.5781388686584,12.4392301767845,
130.994608862376)) ;
#131590 = CARTESIAN_POINT('Ctrl Pts',(-19.6782931891438,12.3513755992719,
131.254028736787)) ;
#131591 = CARTESIAN_POINT('Ctrl Pts',(-19.7822229405507,12.3399316332142,
131.524661009902)) ;
#131592 = CARTESIAN_POINT('Ctrl Pts',(-19.88504344773,12.4070554351268,131.791616350641)) ;
#131593 = CARTESIAN_POINT('Ctrl Pts',(-19.9771610745846,12.5451369869361,
132.027897931008)) ;
#131594 = CARTESIAN_POINT('Ctrl Pts',(-20.0556173721215,12.7477726868892,
132.223821692675)) ;
#131595 = CARTESIAN_POINT('Ctrl Pts',(-20.1137903255926,12.9979367372735,
132.360683275234)) ;
#131596 = CARTESIAN_POINT('Ctrl Pts',(-20.1489013724765,13.2792370978739,
132.430071631305)) ;
#131597 = CARTESIAN_POINT('Ctrl Pts',(-20.1588787384282,13.5701580555343,
132.426125674529)) ;
#131598 = CARTESIAN_POINT('Ctrl Pts',(-20.143937682242,13.8505377724051,132.349389311992)) ;
#131599 = CARTESIAN_POINT('Ctrl Pts',(-20.1057318059421,14.1007512372239,
132.20463305785)) ;
#131600 = CARTESIAN_POINT('Ctrl Pts',(-20.0478354950526,14.3021715583994,
132.002395149785)) ;
#131601 = CARTESIAN_POINT('Ctrl Pts',(-19.9748500391882,14.4410638226486,
131.755979394128)) ;
#131602 = CARTESIAN_POINT('Ctrl Pts',(-19.892940104349,14.506420576945,131.483512074612)) ;
#131603 = CARTESIAN_POINT('Ctrl Pts',(-19.8092678890523,14.4944296739133,
131.206120710523)) ;
#131604 = CARTESIAN_POINT('Ctrl Pts',(-19.7294350859359,14.4055611915821,
130.939713797808)) ;
#131605 = CARTESIAN_POINT('Ctrl Pts',(-19.66081208133,14.2469875620131,130.706232624641)) ;
#131606 = CARTESIAN_POINT('Ctrl Pts',(-19.6083158027718,14.0284942715184,
130.519673218377)) ;
#131607 = CARTESIAN_POINT('Ctrl Pts',(-19.5769557514165,13.7670074742828,
130.394940588624)) ;
#131608 = CARTESIAN_POINT('Ctrl Pts',(-19.5695668686991,13.4805781215048,
130.340191561689)) ;
#131609 = CARTESIAN_POINT('Ctrl Pts',(-19.5872696261961,13.1913388058783,
130.358899107894)) ;
#131610 = CARTESIAN_POINT('Ctrl Pts',(-19.6297522740938,12.9172330933754,
130.449814911348)) ;
#131611 = CARTESIAN_POINT('Ctrl Pts',(-19.6944389773908,12.6799728703758,
130.60569175476)) ;
#131612 = CARTESIAN_POINT('Ctrl Pts',(-19.7782230780513,12.4949910418975,
130.817115688087)) ;
#131613 = CARTESIAN_POINT('Ctrl Pts',(-19.8739923402946,12.3781840447206,
131.063992159593)) ;
#131614 = CARTESIAN_POINT('Ctrl Pts',(-19.9780674608701,12.3352411023339,
131.33468497079)) ;
#131615 = CARTESIAN_POINT('Ctrl Pts',(-20.0810744379286,12.3701183957634,
131.602725123913)) ;
#131616 = CARTESIAN_POINT('Ctrl Pts',(-20.179252895713,12.4815908370187,131.85612905703)) ;
#131617 = CARTESIAN_POINT('Ctrl Pts',(-20.2634570739637,12.6586744463426,
132.069206441814)) ;
#131618 = CARTESIAN_POINT('Ctrl Pts',(-20.3305901520664,12.8927064505131,
132.232014267973)) ;
#131619 = CARTESIAN_POINT('Ctrl Pts',(-20.3750331233153,13.1615895986342,
132.328969789793)) ;
#131620 = CARTESIAN_POINT('Ctrl Pts',(-20.3954965997089,13.4527337961883,
132.355428882089)) ;
#131621 = CARTESIAN_POINT('Ctrl Pts',(-20.3904573045894,13.7397606263225,
132.307631593907)) ;
#131622 = CARTESIAN_POINT('Ctrl Pts',(-20.3613437715797,14.0044956878458,
132.189457679076)) ;
#131623 = CARTESIAN_POINT('Ctrl Pts',(-20.3110168045734,14.2270717047825,
132.009394785638)) ;
#131624 = CARTESIAN_POINT('Ctrl Pts',(-20.2436381751946,14.3928428531141,
131.779444891534)) ;
#131625 = CARTESIAN_POINT('Ctrl Pts',(-20.164336633125,14.4891679896536,131.51449038135)) ;
#131626 = CARTESIAN_POINT('Ctrl Pts',(-20.0809111882638,14.5086708936273,
131.237865647246)) ;
#131627 = CARTESIAN_POINT('Ctrl Pts',(-19.9983950566067,14.4507091204102,
130.963592375788)) ;
#131628 = CARTESIAN_POINT('Ctrl Pts',(-19.9244190141413,14.318823465338,130.714351089596)) ;
#131629 = CARTESIAN_POINT('Ctrl Pts',(-19.8648700988791,14.1234067424229,
130.507330724768)) ;
#131630 = CARTESIAN_POINT('Ctrl Pts',(-19.8245161746179,13.8772496577341,
130.356293737963)) ;
#131631 = CARTESIAN_POINT('Ctrl Pts',(-19.8070957881005,13.5994498547175,
130.272359938913)) ;
#131632 = CARTESIAN_POINT('Ctrl Pts',(-19.8146864693653,13.3067289539218,
130.261220009531)) ;
#131633 = CARTESIAN_POINT('Ctrl Pts',(-19.8471784531872,13.025513208076,130.323196727465)) ;
#131634 = CARTESIAN_POINT('Ctrl Pts',(-19.9032180692331,12.7708776887036,
130.453754380472)) ;
#131635 = CARTESIAN_POINT('Ctrl Pts',(-19.9797679754465,12.5628412979246,
130.644157296538)) ;
#131636 = CARTESIAN_POINT('Ctrl Pts',(-20.0712997390683,12.4171764122364,
130.878502714501)) ;
#131637 = CARTESIAN_POINT('Ctrl Pts',(-20.173220666744,12.3431378359771,131.142938313351)) ;
#131638 = CARTESIAN_POINT('Ctrl Pts',(-20.2769543623743,12.3467434972734,
131.413078047708)) ;
#131639 = CARTESIAN_POINT('Ctrl Pts',(-20.3779474556413,12.4272274658185,
131.674911921515)) ;
#131640 = CARTESIAN_POINT('Ctrl Pts',(-20.4684824931614,12.5790158149027,
131.906293765199)) ;
#131641 = CARTESIAN_POINT('Ctrl Pts',(-20.5433178346082,12.7916687829571,
132.091724629749)) ;
#131642 = CARTESIAN_POINT('Ctrl Pts',(-20.59747019779,13.0498138992039,132.216737279054)) ;
#131643 = CARTESIAN_POINT('Ctrl Pts',(-20.6277539698486,13.3331756720239,
132.272199599018)) ;
#131644 = CARTESIAN_POINT('Ctrl Pts',(-20.63310319697,13.6238935345468,132.254712776567)) ;
#131645 = CARTESIAN_POINT('Ctrl Pts',(-20.6135004102223,13.9010885274901,
132.164225860573)) ;
#131646 = CARTESIAN_POINT('Ctrl Pts',(-20.5712628793398,14.1432054793993,
132.007719764268)) ;
#131647 = CARTESIAN_POINT('Ctrl Pts',(-20.5099062183509,14.3341070280144,
131.795269476235)) ;
#131648 = CARTESIAN_POINT('Ctrl Pts',(-20.4352339689786,14.4587991787124,
131.544150012527)) ;
#131649 = CARTESIAN_POINT('Ctrl Pts',(-20.3525489079931,14.5101605081857,
131.269477291802)) ;
#131650 = CARTESIAN_POINT('Ctrl Pts',(-20.2687361872864,14.4834097576633,
130.991492371573)) ;
#131651 = CARTESIAN_POINT('Ctrl Pts',(-20.1906756501309,14.380986704451,130.730363509583)) ;
#131652 = CARTESIAN_POINT('Ctrl Pts',(-20.1243569260148,14.2089571607828,
130.503381990289)) ;
#131653 = CARTESIAN_POINT('Ctrl Pts',(-20.0759333865454,13.9828180453883,
130.329004955831)) ;
#131654 = CARTESIAN_POINT('Ctrl Pts',(-20.0486953445985,13.7132629209954,
130.216063933579)) ;
#131655 = CARTESIAN_POINT('Ctrl Pts',(-20.0461136758052,13.42583764063,130.175529664949)) ;
#131656 = CARTESIAN_POINT('Ctrl Pts',(-20.0685766436055,13.1374631065902,
130.208056459246)) ;
#131657 = CARTESIAN_POINT('Ctrl Pts',(-20.1154485813734,12.8691197006536,
130.31184888817)) ;
#131658 = CARTESIAN_POINT('Ctrl Pts',(-20.1842161886027,12.6403113443668,
130.479551228157)) ;
#131659 = CARTESIAN_POINT('Ctrl Pts',(-20.2699974667944,12.468420702256,130.697148821309)) ;
#131660 = CARTESIAN_POINT('Ctrl Pts',(-20.368777345651,12.3638000217504,130.952399609198)) ;
#131661 = CARTESIAN_POINT('Ctrl Pts',(-20.4724837589939,12.3359859144704,
131.22233281641)) ;
#131662 = CARTESIAN_POINT('Ctrl Pts',(-20.5755189014966,12.3855342690204,
131.490214378318)) ;
#131663 = CARTESIAN_POINT('Ctrl Pts',(-20.6710370148352,12.5097023136888,
131.736103980719)) ;
#131664 = CARTESIAN_POINT('Ctrl Pts',(-20.7526999022241,12.6987169895182,
131.941597617443)) ;
#131665 = CARTESIAN_POINT('Ctrl Pts',(-20.8159200282362,12.9413958856346,
132.092978431002)) ;
#131666 = CARTESIAN_POINT('Ctrl Pts',(-20.8560148207953,13.2164083911014,
132.177101494275)) ;
#131667 = CARTESIAN_POINT('Ctrl Pts',(-20.8715568106971,13.5077476116907,
132.18930496735)) ;
#131668 = CARTESIAN_POINT('Ctrl Pts',(-20.8618791478333,13.7917084995172,
132.127994218716)) ;
#131669 = CARTESIAN_POINT('Ctrl Pts',(-20.8285666993428,14.0497089633418,
131.997596945122)) ;
#131670 = CARTESIAN_POINT('Ctrl Pts',(-20.7745879228126,14.2632250030891,
131.806787903495)) ;
#131671 = CARTESIAN_POINT('Ctrl Pts',(-20.7043311974277,14.4168537708596,
131.568328459368)) ;
#131672 = CARTESIAN_POINT('Ctrl Pts',(-20.6239603167272,14.4987598986465,
131.300415425815)) ;
#131673 = CARTESIAN_POINT('Ctrl Pts',(-20.539754785129,14.5035045718472,131.021276419093)) ;
#131674 = CARTESIAN_POINT('Ctrl Pts',(-20.4588117616689,14.4313229997249,
130.751803459987)) ;
#131675 = CARTESIAN_POINT('Ctrl Pts',(-20.3868956375626,14.286096674379,130.508478859911)) ;
#131676 = CARTESIAN_POINT('Ctrl Pts',(-20.3308554449234,14.0806888556304,
130.311826279916)) ;
#131677 = CARTESIAN_POINT('Ctrl Pts',(-20.2944696102375,13.8265805447723,
130.172317712221)) ;
#131678 = CARTESIAN_POINT('Ctrl Pts',(-20.2817095072984,13.5441879409374,
130.101929815543)) ;
#131679 = CARTESIAN_POINT('Ctrl Pts',(-20.2939970046262,13.2530370689606,
130.104694604891)) ;
#131680 = CARTESIAN_POINT('Ctrl Pts',(-20.3312192505214,12.9741114175935,
130.18030810907)) ;
#131681 = CARTESIAN_POINT('Ctrl Pts',(-20.391477731723,12.7272119216586,130.323195480133)) ;
#131682 = CARTESIAN_POINT('Ctrl Pts',(-20.4710215017653,12.5305677659782,
130.522476172394)) ;
#131683 = CARTESIAN_POINT('Ctrl Pts',(-20.5648765077218,12.3976028767503,
130.763584707341)) ;
#131684 = CARTESIAN_POINT('Ctrl Pts',(-20.6677354645716,12.3378877564715,
131.030810858964)) ;
#131685 = CARTESIAN_POINT('Ctrl Pts',(-20.771610142133,12.3561146457162,131.301258410359)) ;
#131686 = CARTESIAN_POINT('Ctrl Pts',(-20.8710140356471,12.4504996091204,
131.558507272223)) ;
#131687 = CARTESIAN_POINT('Ctrl Pts',(-20.9591976245712,12.6151918179393,
131.782920165643)) ;
#131688 = CARTESIAN_POINT('Ctrl Pts',(-21.0301909969835,12.8367627956422,
131.957264907826)) ;
#131689 = CARTESIAN_POINT('Ctrl Pts',(-21.0802720431719,13.102471284239,132.070248175628)) ;
#131690 = CARTESIAN_POINT('Ctrl Pts',(-21.1058128562322,13.388098474674,132.11192368682)) ;
#131691 = CARTESIAN_POINT('Ctrl Pts',(-21.1063578527298,13.6786302634614,
132.08028850925)) ;
#131692 = CARTESIAN_POINT('Ctrl Pts',(-21.0823275663731,13.9495118019851,
131.977027551482)) ;
#131693 = CARTESIAN_POINT('Ctrl Pts',(-21.0362217842379,14.1831630717315,
131.809216673534)) ;
#131694 = CARTESIAN_POINT('Ctrl Pts',(-20.9721884045855,14.3622887251467,
131.589091305906)) ;
#131695 = CARTESIAN_POINT('Ctrl Pts',(-20.8947792880245,14.4748192529362,
131.32962547702)) ;
#131696 = CARTESIAN_POINT('Ctrl Pts',(-20.8116749026299,14.5109473630978,
131.053861074448)) ;
#131697 = CARTESIAN_POINT('Ctrl Pts',(-20.7286272549608,14.46989386631,130.778195045776)) ;
#131698 = CARTESIAN_POINT('Ctrl Pts',(-20.6522431108941,14.3536144736526,
130.521907930923)) ;
#131699 = CARTESIAN_POINT('Ctrl Pts',(-20.5889583813436,14.17062113719,130.303892930056)) ;
#131700 = CARTESIAN_POINT('Ctrl Pts',(-20.5440524129988,13.933736573907,130.13953810035)) ;
#131701 = CARTESIAN_POINT('Ctrl Pts',(-20.5214975045223,13.6617104442443,
130.040649083481)) ;
#131702 = CARTESIAN_POINT('Ctrl Pts',(-20.5235105668905,13.3701432171844,
130.013237741548)) ;
#131703 = CARTESIAN_POINT('Ctrl Pts',(-20.5508607538459,13.0839501475181,
130.0600249237)) ;
#131704 = CARTESIAN_POINT('Ctrl Pts',(-20.6019342296123,12.8226369063403,
130.176200002378)) ;
#131705 = CARTESIAN_POINT('Ctrl Pts',(-20.674162245095,12.6036153158418,130.354083975274)) ;
#131706 = CARTESIAN_POINT('Ctrl Pts',(-20.7628382753172,12.4432239429731,
130.580060592785)) ;
#131707 = CARTESIAN_POINT('Ctrl Pts',(-20.8633579914741,12.3525997513282,
130.840351394468)) ;
#131708 = CARTESIAN_POINT('Ctrl Pts',(-20.9671168641114,12.3393903655815,
131.110528978872)) ;
#131709 = CARTESIAN_POINT('Ctrl Pts',(-21.0694306011919,12.403468098602,131.376231401918)) ;
#131710 = CARTESIAN_POINT('Ctrl Pts',(-21.1627219404933,12.5405072085783,
131.615661785443)) ;
#131711 = CARTESIAN_POINT('Ctrl Pts',(-21.2416127937835,12.7420005519616,
131.812839172161)) ;
#131712 = CARTESIAN_POINT('Ctrl Pts',(-21.3001704333997,12.9900801149227,
131.950949061272)) ;
#131713 = CARTESIAN_POINT('Ctrl Pts',(-21.3360159038547,13.2708158721555,
132.022475029764)) ;
#131714 = CARTESIAN_POINT('Ctrl Pts',(-21.3467250085586,13.5613604134334,
132.020708203514)) ;
#131715 = CARTESIAN_POINT('Ctrl Pts',(-21.332530072888,13.8428560081929,131.946099675255)) ;
#131716 = CARTESIAN_POINT('Ctrl Pts',(-21.2946880005883,14.0951246502648,
131.802259522002)) ;
#131717 = CARTESIAN_POINT('Ctrl Pts',(-21.2376357521135,14.2968154125605,
131.602698948677)) ;
#131718 = CARTESIAN_POINT('Ctrl Pts',(-21.164806246768,14.4382062812648,131.356634806151)) ;
#131719 = CARTESIAN_POINT('Ctrl Pts',(-21.0832408338308,14.5055713938207,
131.085254319312)) ;
#131720 = CARTESIAN_POINT('Ctrl Pts',(-20.9994162423038,14.4957941932041,
130.807360837672)) ;
#131721 = CARTESIAN_POINT('Ctrl Pts',(-20.9195959138854,14.4095662340998,
130.541102349046)) ;
#131722 = CARTESIAN_POINT('Ctrl Pts',(-20.8500186277359,14.2515335127425,
130.304558118666)) ;
#131723 = CARTESIAN_POINT('Ctrl Pts',(-20.7972486154139,14.0347236874785,
130.11728882556)) ;
#131724 = CARTESIAN_POINT('Ctrl Pts',(-20.7653613268004,13.7751700114088,
129.991129528377)) ;
#131725 = CARTESIAN_POINT('Ctrl Pts',(-20.7571817990629,13.489555102194,129.934113768398)) ;
#131726 = CARTESIAN_POINT('Ctrl Pts',(-20.7742556911792,13.1989624545804,
129.950844344899)) ;
#131727 = CARTESIAN_POINT('Ctrl Pts',(-20.8159809707414,12.9245155762064,
130.03960916018)) ;
#131728 = CARTESIAN_POINT('Ctrl Pts',(-20.8805367450398,12.6850932088169,
130.194926855194)) ;
#131729 = CARTESIAN_POINT('Ctrl Pts',(-20.9626356003938,12.5007200500438,
130.401901459438)) ;
#131730 = CARTESIAN_POINT('Ctrl Pts',(-21.0591957946408,12.3802348015134,
130.650687618331)) ;
#131731 = CARTESIAN_POINT('Ctrl Pts',(-21.1622370545661,12.3354177830535,
130.918672003733)) ;
#131732 = CARTESIAN_POINT('Ctrl Pts',(-21.2662887681593,12.3682931650198,
131.189443526458)) ;
#131733 = CARTESIAN_POINT('Ctrl Pts',(-21.3637199956931,12.4764500222757,
131.44102792815)) ;
#131734 = CARTESIAN_POINT('Ctrl Pts',(-21.4490683123423,12.6527561756398,
131.657189302748)) ;
#131735 = CARTESIAN_POINT('Ctrl Pts',(-21.5164968590452,12.8841372675975,
131.821041651181)) ;
#131736 = CARTESIAN_POINT('Ctrl Pts',(-21.5620729321248,13.1550291136418,
131.920951331736)) ;
#131737 = CARTESIAN_POINT('Ctrl Pts',(-21.5829990360394,13.4437302360126,
131.949026741888)) ;
#131738 = CARTESIAN_POINT('Ctrl Pts',(-21.5787261653874,13.7319393007276,
131.903366364301)) ;
#131739 = CARTESIAN_POINT('Ctrl Pts',(-21.5503975227815,13.9965481623833,
131.787623344815)) ;
#131740 = CARTESIAN_POINT('Ctrl Pts',(-21.5005342471165,14.2215298170475,
131.608800269925)) ;
#131741 = CARTESIAN_POINT('Ctrl Pts',(-21.4333938850247,14.3891483272759,
131.379489123203)) ;
#131742 = CARTESIAN_POINT('Ctrl Pts',(-21.3548735774567,14.4871687024338,
131.117033634355)) ;
#131743 = CARTESIAN_POINT('Ctrl Pts',(-21.2709428978837,14.5093408079897,
130.838711318976)) ;
#131744 = CARTESIAN_POINT('Ctrl Pts',(-21.1882422406468,14.4530254583256,
130.563868416307)) ;
#131745 = CARTESIAN_POINT('Ctrl Pts',(-21.1143270880585,14.3240305585518,
130.31499305445)) ;
#131746 = CARTESIAN_POINT('Ctrl Pts',(-21.0539688868397,14.1290979717854,
130.105410602035)) ;
#131747 = CARTESIAN_POINT('Ctrl Pts',(-21.0132069302916,13.8855604155571,
129.953378103653)) ;
#131748 = CARTESIAN_POINT('Ctrl Pts',(-20.9950030451873,13.6058416707122,
129.866845755651)) ;
#131749 = CARTESIAN_POINT('Ctrl Pts',(-21.0018793397198,13.3160021377259,
129.853947611582)) ;
#131750 = CARTESIAN_POINT('Ctrl Pts',(-21.0337293398582,13.0326886676077,
129.913868033499)) ;
#131751 = CARTESIAN_POINT('Ctrl Pts',(-21.0893772116349,12.7766372190837,
130.043216529831)) ;
#131752 = CARTESIAN_POINT('Ctrl Pts',(-21.1653161877122,12.5676698161814,
130.231901557219)) ;
#131753 = CARTESIAN_POINT('Ctrl Pts',(-21.2561790285771,12.4206517790888,
130.464404545457)) ;
#131754 = CARTESIAN_POINT('Ctrl Pts',(-21.3575675366688,12.3443150505119,
130.727387699059)) ;
#131755 = CARTESIAN_POINT('Ctrl Pts',(-21.4618210845223,12.3454567433165,
130.998884337509)) ;
#131756 = CARTESIAN_POINT('Ctrl Pts',(-21.5631430702427,12.4241540146565,
131.261630006307)) ;
#131757 = CARTESIAN_POINT('Ctrl Pts',(-21.6537810155053,12.5736454649868,
131.493407152973)) ;
#131758 = CARTESIAN_POINT('Ctrl Pts',(-21.7290950924145,12.7844244258342,
131.680270904741)) ;
#131759 = CARTESIAN_POINT('Ctrl Pts',(-21.7839298109933,13.041264478038,131.807295952736)) ;
#131760 = CARTESIAN_POINT('Ctrl Pts',(-21.8150448539116,13.3250313838274,
131.865081031141)) ;
#131761 = CARTESIAN_POINT('Ctrl Pts',(-21.8210632536644,13.6156492492809,
131.849571033927)) ;
#131762 = CARTESIAN_POINT('Ctrl Pts',(-21.8022545212773,13.8929002803611,
131.761487721122)) ;
#131763 = CARTESIAN_POINT('Ctrl Pts',(-21.7605924585031,14.1366366428793,
131.606614879296)) ;
#131764 = CARTESIAN_POINT('Ctrl Pts',(-21.6999698317163,14.3287833833703,
131.396421302764)) ;
#131765 = CARTESIAN_POINT('Ctrl Pts',(-21.6253197774301,14.4563288342089,
131.145218098165)) ;
#131766 = CARTESIAN_POINT('Ctrl Pts',(-21.5425945750513,14.5097636463918,
130.870367772935)) ;
#131767 = CARTESIAN_POINT('Ctrl Pts',(-21.4589621479375,14.4852491819093,
130.593003563587)) ;
#131768 = CARTESIAN_POINT('Ctrl Pts',(-21.380714091029,14.385213180382,130.331360934625)) ;
#131769 = CARTESIAN_POINT('Ctrl Pts',(-21.3138290434139,14.2148994362801,
130.102677640231)) ;
#131770 = CARTESIAN_POINT('Ctrl Pts',(-21.264802027938,13.9895605141043,129.92646714371)) ;
#131771 = CARTESIAN_POINT('Ctrl Pts',(-21.2370048320792,13.7226496289756,
129.812102485109)) ;
#131772 = CARTESIAN_POINT('Ctrl Pts',(-21.2336042417307,13.4342098859693,
129.769013814372)) ;
#131773 = CARTESIAN_POINT('Ctrl Pts',(-21.2553236046358,13.1458182759752,
129.799407215841)) ;
#131774 = CARTESIAN_POINT('Ctrl Pts',(-21.3016988392798,12.8759127132536,
129.901648132077)) ;
#131775 = CARTESIAN_POINT('Ctrl Pts',(-21.3694669987003,12.6468868556867,
130.066623481143)) ;
#131776 = CARTESIAN_POINT('Ctrl Pts',(-21.4553373193102,12.4721832296684,
130.284273605613)) ;
#131777 = CARTESIAN_POINT('Ctrl Pts',(-21.5530256217249,12.3661739274481,
130.536616813639)) ;
#131778 = CARTESIAN_POINT('Ctrl Pts',(-21.6575177270796,12.3355863385396,
130.808562220896)) ;
#131779 = CARTESIAN_POINT('Ctrl Pts',(-21.7604456918656,12.3831198658751,
131.076206190241)) ;
#131780 = CARTESIAN_POINT('Ctrl Pts',(-21.8563696469902,12.5053833023315,
131.323242388746)) ;
#131781 = CARTESIAN_POINT('Ctrl Pts',(-21.9382966693068,12.6923270702948,
131.529584453516)) ;
#131782 = CARTESIAN_POINT('Ctrl Pts',(-22.0021645015312,12.9335865705139,
131.682862448256)) ;
#131783 = CARTESIAN_POINT('Ctrl Pts',(-22.0430213128192,13.2085814539572,
131.769129801508)) ;
#131784 = CARTESIAN_POINT('Ctrl Pts',(-22.0592352836556,13.4990557588074,
131.783380739882)) ;
#131785 = CARTESIAN_POINT('Ctrl Pts',(-22.0503004073671,13.7836907462661,
131.724216167399)) ;
#131786 = CARTESIAN_POINT('Ctrl Pts',(-22.0176371901026,14.0427281414566,
131.595717480909)) ;
#131787 = CARTESIAN_POINT('Ctrl Pts',(-21.9641995370827,14.2577309750281,
131.406490661624)) ;
#131788 = CARTESIAN_POINT('Ctrl Pts',(-21.8944782363852,14.4131664617501,
131.169654967239)) ;
#131789 = CARTESIAN_POINT('Ctrl Pts',(-21.8141620072022,14.4973755702956,
130.901832610092)) ;
#131790 = CARTESIAN_POINT('Ctrl Pts',(-21.7303937720881,14.5046724130054,
130.624142862364)) ;
#131791 = CARTESIAN_POINT('Ctrl Pts',(-21.6486693225774,14.4343111747756,
130.352140919931)) ;
#131792 = CARTESIAN_POINT('Ctrl Pts',(-21.5766530687314,14.2913904033354,
130.108640611113)) ;
#131793 = CARTESIAN_POINT('Ctrl Pts',(-21.5199914526865,14.0872940403586,
129.910112364196)) ;
#131794 = CARTESIAN_POINT('Ctrl Pts',(-21.4830382408884,13.8349907742835,
129.769035274606)) ;
#131795 = CARTESIAN_POINT('Ctrl Pts',(-21.4694985396213,13.5522018199285,
129.696252361388)) ;
#131796 = CARTESIAN_POINT('Ctrl Pts',(-21.4810885813508,13.2611771320633,
129.697002826515)) ;
#131797 = CARTESIAN_POINT('Ctrl Pts',(-21.5176805732444,12.9814107201437,
129.770743949859)) ;
#131798 = CARTESIAN_POINT('Ctrl Pts',(-21.5771191123903,12.7341369610279,
129.911345858839)) ;
#131799 = CARTESIAN_POINT('Ctrl Pts',(-21.6563209788842,12.535166216503,130.109544290444)) ;
#131800 = CARTESIAN_POINT('Ctrl Pts',(-21.7502713534583,12.4000170891871,
130.350799701057)) ;
#131801 = CARTESIAN_POINT('Ctrl Pts',(-21.8524815344102,12.3385941106561,
130.616296707476)) ;
#131802 = CARTESIAN_POINT('Ctrl Pts',(-21.9565712501459,12.3545286685026,
130.887315313701)) ;
#131803 = CARTESIAN_POINT('Ctrl Pts',(-22.0562577481496,12.4469846430608,
131.14537139149)) ;
#131804 = CARTESIAN_POINT('Ctrl Pts',(-22.1449360417052,12.6102579412087,
131.371180205731)) ;
#131805 = CARTESIAN_POINT('Ctrl Pts',(-22.2161370464207,12.8296977311719,
131.546256445573)) ;
#131806 = CARTESIAN_POINT('Ctrl Pts',(-22.2667592690025,13.0929763552362,
131.660982603106)) ;
#131807 = CARTESIAN_POINT('Ctrl Pts',(-22.2932535098378,13.3798715107165,
131.705248169509)) ;
#131808 = CARTESIAN_POINT('Ctrl Pts',(-22.2944576782056,13.6705227535771,
131.675549761758)) ;
#131809 = CARTESIAN_POINT('Ctrl Pts',(-22.2711545117995,13.9421700423004,
131.57442408932)) ;
#131810 = CARTESIAN_POINT('Ctrl Pts',(-22.2253820822901,14.1780191011813,
131.407446635602)) ;
#131811 = CARTESIAN_POINT('Ctrl Pts',(-22.1619741826909,14.3579768124892,
131.189272795754)) ;
#131812 = CARTESIAN_POINT('Ctrl Pts',(-22.0850483275451,14.4725057553617,
130.931291857228)) ;
#131813 = CARTESIAN_POINT('Ctrl Pts',(-22.0018889458697,14.5110248787396,
130.655306915796)) ;
#131814 = CARTESIAN_POINT('Ctrl Pts',(-21.9186831269904,14.4721191969269,
130.37915685792)) ;
#131815 = CARTESIAN_POINT('Ctrl Pts',(-21.8419983594231,14.3577454336847,
130.121978165508)) ;
#131816 = CARTESIAN_POINT('Ctrl Pts',(-21.7784559689967,14.1770688666527,
129.90331119887)) ;
#131817 = CARTESIAN_POINT('Ctrl Pts',(-21.7328730623761,13.9416997327419,
129.73698112711)) ;
#131818 = CARTESIAN_POINT('Ctrl Pts',(-21.7095937547817,13.6694104353782,
129.635852457523)) ;
#131819 = CARTESIAN_POINT('Ctrl Pts',(-21.7108544164153,13.3798585935035,
129.60644988842)) ;
#131820 = CARTESIAN_POINT('Ctrl Pts',(-21.7373587408651,13.0927640382574,
129.650717582232)) ;
#131821 = CARTESIAN_POINT('Ctrl Pts',(-21.7879727694938,12.8294542733058,
129.765423278)) ;
#131822 = CARTESIAN_POINT('Ctrl Pts',(-21.8596572059499,12.6090080043084,
129.941724810289)) ;
#131823 = CARTESIAN_POINT('Ctrl Pts',(-21.9481186483126,12.4466659582347,
130.167016290758)) ;
#131824 = CARTESIAN_POINT('Ctrl Pts',(-22.0478029406896,12.3544265354386,
130.425067159699)) ;
#131825 = CARTESIAN_POINT('Ctrl Pts',(-22.1517530143636,12.338485550426,130.695728652991)) ;
#131826 = CARTESIAN_POINT('Ctrl Pts',(-22.2547791723717,12.4009576070215,
130.963329774343)) ;
#131827 = CARTESIAN_POINT('Ctrl Pts',(-22.3479076849026,12.5356622675021,
131.202441690569)) ;
#131828 = CARTESIAN_POINT('Ctrl Pts',(-22.427039674185,12.7342792931547,131.400473047047)) ;
#131829 = CARTESIAN_POINT('Ctrl Pts',(-22.4865817751364,12.9822470405306,
131.541298758196)) ;
#131830 = CARTESIAN_POINT('Ctrl Pts',(-22.5231351067208,13.2626104241267,
131.614868935857)) ;
#131831 = CARTESIAN_POINT('Ctrl Pts',(-22.5345613145019,13.5537330357078,
131.615129217148)) ;
#131832 = CARTESIAN_POINT('Ctrl Pts',(-22.5210072175352,13.8350780443648,
131.542464925158)) ;
#131833 = CARTESIAN_POINT('Ctrl Pts',(-22.4841282635127,14.0872562376869,
131.401629162015)) ;
#131834 = CARTESIAN_POINT('Ctrl Pts',(-22.4271936380161,14.2922552735091,
131.202157542)) ;
#131835 = CARTESIAN_POINT('Ctrl Pts',(-22.3548468095764,14.4349645919609,
130.957589374496)) ;
#131836 = CARTESIAN_POINT('Ctrl Pts',(-22.2738049730186,14.5045540577175,
130.687866104784)) ;
#131837 = CARTESIAN_POINT('Ctrl Pts',(-22.1896316409164,14.4973581396257,
130.408831550043)) ;
#131838 = CARTESIAN_POINT('Ctrl Pts',(-22.1093343470203,14.4126016842873,
130.14105358009)) ;
#131839 = CARTESIAN_POINT('Ctrl Pts',(-22.0399356599868,14.2578370889756,
129.905309744937)) ;
#131840 = CARTESIAN_POINT('Ctrl Pts',(-21.9863765422796,14.0423606370671,
129.715650705837)) ;
#131841 = CARTESIAN_POINT('Ctrl Pts',(-21.9537345461485,13.7833430848993,
129.58722594006)) ;
#131842 = CARTESIAN_POINT('Ctrl Pts',(-21.9448743026681,13.4972454461382,
129.528113894271)) ;
#131843 = CARTESIAN_POINT('Ctrl Pts',(-21.9611494569257,13.2077137971034,
129.542654652447)) ;
#131844 = CARTESIAN_POINT('Ctrl Pts',(-22.002288346979,12.9318531124,129.629618831657)) ;
#131845 = CARTESIAN_POINT('Ctrl Pts',(-22.0658546135328,12.6922552108513,
129.782222524194)) ;
#131846 = CARTESIAN_POINT('Ctrl Pts',(-22.1480419825475,12.504666487009,129.989213929092)) ;
#131847 = CARTESIAN_POINT('Ctrl Pts',(-22.2443302147763,12.3825157199122,
130.237218364436)) ;
#131848 = CARTESIAN_POINT('Ctrl Pts',(-22.3470392380216,12.3357140444497,
130.504298662281)) ;
#131849 = CARTESIAN_POINT('Ctrl Pts',(-22.4509464733217,12.3660679541908,
130.774724556597)) ;
#131850 = CARTESIAN_POINT('Ctrl Pts',(-22.549161413923,12.4727573812884,131.028420389511)) ;
#131851 = CARTESIAN_POINT('Ctrl Pts',(-22.6347030566716,12.6471452986828,
131.245220928735)) ;
#131852 = CARTESIAN_POINT('Ctrl Pts',(-22.7025433269035,12.8766362181276,
131.410346416835)) ;
#131853 = CARTESIAN_POINT('Ctrl Pts',(-22.7487814948906,13.1457609561308,
131.512289397035)) ;
#131854 = CARTESIAN_POINT('Ctrl Pts',(-22.7705721874272,13.436208516762,131.542656742186)) ;
#131855 = CARTESIAN_POINT('Ctrl Pts',(-22.7669909559281,13.7232902020091,
131.499187113643)) ;
#131856 = CARTESIAN_POINT('Ctrl Pts',(-22.739314974999,13.9896012284326,131.385259077282)) ;
#131857 = CARTESIAN_POINT('Ctrl Pts',(-22.6899563353196,14.2159296230216,
131.207905951156)) ;
#131858 = CARTESIAN_POINT('Ctrl Pts',(-22.6233672864789,14.3851342144556,
130.980263042488)) ;
#131859 = CARTESIAN_POINT('Ctrl Pts',(-22.5449702570784,14.4854516976048,
130.718115056966)) ;
#131860 = CARTESIAN_POINT('Ctrl Pts',(-22.461265093064,14.5096986607512,130.440515127017)) ;
#131861 = CARTESIAN_POINT('Ctrl Pts',(-22.378621004999,14.4561737731647,130.165930931039)) ;
#131862 = CARTESIAN_POINT('Ctrl Pts',(-22.3039082628437,14.3282785458503,
129.914502352423)) ;
#131863 = CARTESIAN_POINT('Ctrl Pts',(-22.2434277952934,14.1363003864466,
129.704779792514)) ;
#131864 = CARTESIAN_POINT('Ctrl Pts',(-22.2017896977858,13.8924839857025,
129.549971716453)) ;
#131865 = CARTESIAN_POINT('Ctrl Pts',(-22.1830205641406,13.6154602436594,
129.462035111654)) ;
#131866 = CARTESIAN_POINT('Ctrl Pts',(-22.1890712067793,13.3244466531158,
129.446574293387)) ;
#131867 = CARTESIAN_POINT('Ctrl Pts',(-22.2202555636145,13.0407282159145,
129.504562629151)) ;
#131868 = CARTESIAN_POINT('Ctrl Pts',(-22.2750211321796,12.7843965627726,
129.631442703902)) ;
#131869 = CARTESIAN_POINT('Ctrl Pts',(-22.3503429335631,12.5734338880589,
129.818316417424)) ;
#131870 = CARTESIAN_POINT('Ctrl Pts',(-22.4414173268538,12.4236459559127,
130.051229799352)) ;
#131871 = CARTESIAN_POINT('Ctrl Pts',(-22.5421394962141,12.3455712635568,
130.312426708327)) ;
#131872 = CARTESIAN_POINT('Ctrl Pts',(-22.6467265172187,12.3443023671055,
130.584788395612)) ;
#131873 = CARTESIAN_POINT('Ctrl Pts',(-22.7481657330948,12.420933178294,130.847899857883)) ;
#131874 = CARTESIAN_POINT('Ctrl Pts',(-22.8392055009209,12.5684896870098,
131.080841902066)) ;
#131875 = CARTESIAN_POINT('Ctrl Pts',(-22.9152137261507,12.7783872300958,
131.269645560269)) ;
#131876 = CARTESIAN_POINT('Ctrl Pts',(-22.9705402435953,13.0341435528073,
131.398130661038)) ;
#131877 = CARTESIAN_POINT('Ctrl Pts',(-23.0022377817911,13.3161552682329,
131.457761074721)) ;
#131878 = CARTESIAN_POINT('Ctrl Pts',(-23.009059140071,13.6077102167408,131.444501189894)) ;
#131879 = CARTESIAN_POINT('Ctrl Pts',(-22.9907943770449,13.8863966863271,
131.357908893058)) ;
#131880 = CARTESIAN_POINT('Ctrl Pts',(-22.9497275238959,14.1306963082603,
131.204837242028)) ;
#131881 = CARTESIAN_POINT('Ctrl Pts',(-22.8897860606364,14.3238933046915,
130.996741057129)) ;
#131882 = CARTESIAN_POINT('Ctrl Pts',(-22.8155047276147,14.4535137780173,
130.746625113997)) ;
#131883 = CARTESIAN_POINT('Ctrl Pts',(-22.7328983548189,14.5094099168095,
130.47211370142)) ;
#131884 = CARTESIAN_POINT('Ctrl Pts',(-22.6487340748289,14.4867701673882,
130.193005786419)) ;
#131885 = CARTESIAN_POINT('Ctrl Pts',(-22.5707021703194,14.3890643828725,
129.932173416396)) ;
#131886 = CARTESIAN_POINT('Ctrl Pts',(-22.5034195621283,14.2211869107964,
129.70237977909)) ;
#131887 = CARTESIAN_POINT('Ctrl Pts',(-22.4535961395973,13.9958858020985,
129.523655290175)) ;
#131888 = CARTESIAN_POINT('Ctrl Pts',(-22.4253306349521,13.7314793548645,
129.40812642471)) ;
#131889 = CARTESIAN_POINT('Ctrl Pts',(-22.4210875175899,13.4423639400344,
129.362455182987)) ;
#131890 = CARTESIAN_POINT('Ctrl Pts',(-22.4422895478426,13.1530743203904,
129.391256495026)) ;
#131891 = CARTESIAN_POINT('Ctrl Pts',(-22.487580667877,12.8842566111771,129.490582827144)) ;
#131892 = CARTESIAN_POINT('Ctrl Pts',(-22.5552977498778,12.6519995362001,
129.655140460866)) ;
#131893 = CARTESIAN_POINT('Ctrl Pts',(-22.6402716313289,12.4766942436469,
129.870371614395)) ;
#131894 = CARTESIAN_POINT('Ctrl Pts',(-22.7378885944903,12.3681120678918,
130.122423877062)) ;
#131895 = CARTESIAN_POINT('Ctrl Pts',(-22.8423855341256,12.3353450096833,
130.394363079284)) ;
#131896 = CARTESIAN_POINT('Ctrl Pts',(-22.9455053804218,12.3808789292608,
130.66253674151)) ;
#131897 = CARTESIAN_POINT('Ctrl Pts',(-23.0414119491019,12.5006496739186,
130.90963712832)) ;
#131898 = CARTESIAN_POINT('Ctrl Pts',(-23.1239874820464,12.6862348924807,
131.117800379368)) ;
#131899 = CARTESIAN_POINT('Ctrl Pts',(-23.1882404954987,12.9253055289241,
131.272326344278)) ;
#131900 = CARTESIAN_POINT('Ctrl Pts',(-23.2299054869804,13.1996774467986,
131.360925356354)) ;
#131901 = CARTESIAN_POINT('Ctrl Pts',(-23.2469197712831,13.4900583198245,
131.37750845876)) ;
#131902 = CARTESIAN_POINT('Ctrl Pts',(-23.2386702442009,13.7765694769724,
131.320183787516)) ;
#131903 = CARTESIAN_POINT('Ctrl Pts',(-23.2064532063664,14.036835662277,131.192930360202)) ;
#131904 = CARTESIAN_POINT('Ctrl Pts',(-23.1537890318512,14.2522894974628,
131.006121661116)) ;
#131905 = CARTESIAN_POINT('Ctrl Pts',(-23.0841408392017,14.410142650821,130.769355953609)) ;
#131906 = CARTESIAN_POINT('Ctrl Pts',(-23.0044224542759,14.4959011359271,
130.503451200898)) ;
#131907 = CARTESIAN_POINT('Ctrl Pts',(-22.9205051252153,14.5055615596735,
130.225254015656)) ;
#131908 = CARTESIAN_POINT('Ctrl Pts',(-22.8387642579551,14.4373879166647,
129.953265322989)) ;
#131909 = CARTESIAN_POINT('Ctrl Pts',(-22.7664377143828,14.2968056087925,
129.708895562602)) ;
#131910 = CARTESIAN_POINT('Ctrl Pts',(-22.7090205846332,14.0934340145334,
129.508020332236)) ;
#131911 = CARTESIAN_POINT('Ctrl Pts',(-22.6715788423865,13.8423638114029,
129.365551179356)) ;
#131912 = CARTESIAN_POINT('Ctrl Pts',(-22.6573294356865,13.5615577206812,
129.290854833297)) ;
#131913 = CARTESIAN_POINT('Ctrl Pts',(-22.6681862864359,13.2694348944804,
129.289338191419)) ;
#131914 = CARTESIAN_POINT('Ctrl Pts',(-22.7039617574597,12.9897647818979,
129.360785289403)) ;
#131915 = CARTESIAN_POINT('Ctrl Pts',(-22.7629534424542,12.7403852471457,
129.499963464368)) ;
#131916 = CARTESIAN_POINT('Ctrl Pts',(-22.8415892215112,12.5401778472151,
129.696554511139)) ;
#131917 = CARTESIAN_POINT('Ctrl Pts',(-22.9348979213409,12.4032538731495,
129.936029182917)) ;
#131918 = CARTESIAN_POINT('Ctrl Pts',(-23.0370685674519,12.3392654765734,
130.201366375023)) ;
#131919 = CARTESIAN_POINT('Ctrl Pts',(-23.141478431911,12.3529795705707,130.473233214815)) ;
#131920 = CARTESIAN_POINT('Ctrl Pts',(-23.2412861780916,12.44341496887,130.731668708428)) ;
#131921 = CARTESIAN_POINT('Ctrl Pts',(-23.330047912579,12.6038142404483,130.957868037024)) ;
#131922 = CARTESIAN_POINT('Ctrl Pts',(-23.4023245485338,12.8232746698558,
131.135851245433)) ;
#131923 = CARTESIAN_POINT('Ctrl Pts',(-23.4533693512746,13.0848674095602,
131.251920028465)) ;
#131924 = CARTESIAN_POINT('Ctrl Pts',(-23.4806176034136,13.3712340427374,
131.298395105942)) ;
#131925 = CARTESIAN_POINT('Ctrl Pts',(-23.4825810779044,13.6620670155129,
131.270922868641)) ;
#131926 = CARTESIAN_POINT('Ctrl Pts',(-23.4599091408466,13.9347879219274,
131.171598398464)) ;
#131927 = CARTESIAN_POINT('Ctrl Pts',(-23.4149763968351,14.1711547034761,
131.007212926626)) ;
#131928 = CARTESIAN_POINT('Ctrl Pts',(-23.3516961209413,14.3538985958079,
130.789228498426)) ;
#131929 = CARTESIAN_POINT('Ctrl Pts',(-23.2754093744269,14.4699515410886,
130.533273425003)) ;
#131930 = CARTESIAN_POINT('Ctrl Pts',(-23.1921867842084,14.511011729743,130.257027506385)) ;
#131931 = CARTESIAN_POINT('Ctrl Pts',(-23.1089561500767,14.4745400421894,
129.980842840064)) ;
#131932 = CARTESIAN_POINT('Ctrl Pts',(-23.031552894356,14.3614974996119,129.721369859714)) ;
#131933 = CARTESIAN_POINT('Ctrl Pts',(-22.9678477580129,14.1829580277845,
129.502345220066)) ;
#131934 = CARTESIAN_POINT('Ctrl Pts',(-22.9216856506781,13.9492404929465,
129.334353763701)) ;
#131935 = CARTESIAN_POINT('Ctrl Pts',(-22.8977300159152,13.6775800982586,
129.231228230102)) ;
#131936 = CARTESIAN_POINT('Ctrl Pts',(-22.8981933527482,13.3886494635436,
129.19954520776)) ;
#131937 = CARTESIAN_POINT('Ctrl Pts',(-22.9242400045738,13.0993478015478,
129.242254988579)) ;
#131938 = CARTESIAN_POINT('Ctrl Pts',(-22.9739037222349,12.8369458310676,
129.354415199943)) ;
#131939 = CARTESIAN_POINT('Ctrl Pts',(-23.0453252131747,12.6140529768099,
129.529801908795)) ;
#131940 = CARTESIAN_POINT('Ctrl Pts',(-23.1330410816671,12.4507323341902,
129.753058144926)) ;
#131941 = CARTESIAN_POINT('Ctrl Pts',(-23.2324941335687,12.3558899306528,
130.010420059215)) ;
#131942 = CARTESIAN_POINT('Ctrl Pts',(-23.3371521212107,12.3380969081111,
130.282910607247)) ;
#131943 = CARTESIAN_POINT('Ctrl Pts',(-23.4390406262999,12.3976016694818,
130.547608591386)) ;
#131944 = CARTESIAN_POINT('Ctrl Pts',(-23.5331839274626,12.530583824708,130.789474316628)) ;
#131945 = CARTESIAN_POINT('Ctrl Pts',(-23.6129508354768,12.7283490506027,
130.989275182951)) ;
#131946 = CARTESIAN_POINT('Ctrl Pts',(-23.6728864226876,12.9742771227128,
131.13136588872)) ;
#131947 = CARTESIAN_POINT('Ctrl Pts',(-23.71018774412,13.2539376227601,131.207121504005)) ;
#131948 = CARTESIAN_POINT('Ctrl Pts',(-23.7223865299285,13.5450903335013,
131.209633661058)) ;
#131949 = CARTESIAN_POINT('Ctrl Pts',(-23.7094914718236,13.8275787514848,
131.138820807372)) ;
#131950 = CARTESIAN_POINT('Ctrl Pts',(-23.6732974807833,14.080619519853,131.000028693289)) ;
#131951 = CARTESIAN_POINT('Ctrl Pts',(-23.616590785082,14.2877392133105,130.801091824847)) ;
#131952 = CARTESIAN_POINT('Ctrl Pts',(-23.5452916636683,14.431213841156,130.559896288173)) ;
#131953 = CARTESIAN_POINT('Ctrl Pts',(-23.4637700924587,14.5038738166411,
130.288489711948)) ;
#131954 = CARTESIAN_POINT('Ctrl Pts',(-23.3797591259085,14.4984557576167,
130.010000564517)) ;
#131955 = CARTESIAN_POINT('Ctrl Pts',(-23.2994671912968,14.4164646825051,
129.742342495005)) ;
#131956 = CARTESIAN_POINT('Ctrl Pts',(-23.2292002172557,14.2622140461571,
129.503806387235)) ;
#131957 = CARTESIAN_POINT('Ctrl Pts',(-23.1755337197615,14.0497489487789,
129.314087251754)) ;
#131958 = CARTESIAN_POINT('Ctrl Pts',(-23.1420903990703,13.7905258352839,
129.183151437944)) ;
#131959 = CARTESIAN_POINT('Ctrl Pts',(-23.1325295042077,13.506486494377,129.12218848079)) ;
#131960 = CARTESIAN_POINT('Ctrl Pts',(-23.1482921851681,13.2142515667239,
129.134926916223)) ;
#131961 = CARTESIAN_POINT('Ctrl Pts',(-23.188353413262,12.9406232851689,129.219102820939)) ;
#131962 = CARTESIAN_POINT('Ctrl Pts',(-23.2515823582444,12.6982138740687,
129.370525672368)) ;
#131963 = CARTESIAN_POINT('Ctrl Pts',(-23.3330631497147,12.5096112048297,
129.575565311669)) ;
#131964 = CARTESIAN_POINT('Ctrl Pts',(-23.4290906890084,12.3850648620669,
129.822774700949)) ;
#131965 = CARTESIAN_POINT('Ctrl Pts',(-23.531784997696,12.3359713268051,130.089781167871)) ;
#131966 = CARTESIAN_POINT('Ctrl Pts',(-23.6357879798494,12.3641515700291,
130.360476235555)) ;
#131967 = CARTESIAN_POINT('Ctrl Pts',(-23.7340953356143,12.4683944776065,
130.614508785511)) ;
#131968 = CARTESIAN_POINT('Ctrl Pts',(-23.8203211365081,12.6414744910879,
130.833207334208)) ;
#131969 = CARTESIAN_POINT('Ctrl Pts',(-23.8886881736005,12.8692739707259,
130.99991574651)) ;
#131970 = CARTESIAN_POINT('Ctrl Pts',(-23.9357467861378,13.1394382839076,
131.104034823546)) ;
#131971 = CARTESIAN_POINT('Ctrl Pts',(-23.9579774455155,13.4257125423889,
131.136139167156)) ;
#131972 = CARTESIAN_POINT('Ctrl Pts',(-23.9552750237727,13.7153678926771,
131.094978168242)) ;
#131973 = CARTESIAN_POINT('Ctrl Pts',(-23.9282090173285,13.9823826092166,
130.982854215722)) ;
#131974 = CARTESIAN_POINT('Ctrl Pts',(-23.8793697422226,14.210351268189,130.806979650137)) ;
#131975 = CARTESIAN_POINT('Ctrl Pts',(-23.8133153702057,14.3810373513132,
130.58096078673)) ;
#131976 = CARTESIAN_POINT('Ctrl Pts',(-23.735209224892,14.4835203874639,130.319669563206)) ;
#131977 = CARTESIAN_POINT('Ctrl Pts',(-23.6515414522142,14.5102051470099,
130.042171972968)) ;
#131978 = CARTESIAN_POINT('Ctrl Pts',(-23.5684272969825,14.4584272467564,
129.766068717826)) ;
#131979 = CARTESIAN_POINT('Ctrl Pts',(-23.4938231437372,14.3332271538461,
129.515148015428)) ;
#131980 = CARTESIAN_POINT('Ctrl Pts',(-23.4326135115301,14.1422679027751,
129.303162687106)) ;
#131981 = CARTESIAN_POINT('Ctrl Pts',(-23.3905185584406,13.9003526545792,
129.147122527455)) ;
#131982 = CARTESIAN_POINT('Ctrl Pts',(-23.3709966570516,13.6237176044633,
129.056941792442)) ;
#131983 = CARTESIAN_POINT('Ctrl Pts',(-23.3763211847102,13.3329588361478,
129.039378660403)) ;
#131984 = CARTESIAN_POINT('Ctrl Pts',(-23.4068246825045,13.0482791472687,
129.095326134194)) ;
#131985 = CARTESIAN_POINT('Ctrl Pts',(-23.4611218639704,12.7905984211716,
129.220781957599)) ;
#131986 = CARTESIAN_POINT('Ctrl Pts',(-23.5355417145057,12.5792074314873,
129.405190030391)) ;
#131987 = CARTESIAN_POINT('Ctrl Pts',(-23.6262276903051,12.4271420328258,
129.636951252849)) ;
#131988 = CARTESIAN_POINT('Ctrl Pts',(-23.72702713312,12.3466854620337,129.898286196702)) ;
#131989 = CARTESIAN_POINT('Ctrl Pts',(-23.8314987159718,12.3433384451733,
130.170343083653)) ;
#131990 = CARTESIAN_POINT('Ctrl Pts',(-23.9327910170219,12.417256873973,130.433143999051)) ;
#131991 = CARTESIAN_POINT('Ctrl Pts',(-24.0245736232509,12.5633304568432,
130.668126155051)) ;
#131992 = CARTESIAN_POINT('Ctrl Pts',(-24.1008197720403,12.7708593905581,
130.857750684135)) ;
#131993 = CARTESIAN_POINT('Ctrl Pts',(-24.1569294635632,13.025326349885,130.988518737243)) ;
#131994 = CARTESIAN_POINT('Ctrl Pts',(-24.1894985627988,13.3082178025067,
131.05053265747)) ;
#131995 = CARTESIAN_POINT('Ctrl Pts',(-24.196965740994,13.5990344955289,131.039249671657)) ;
#131996 = CARTESIAN_POINT('Ctrl Pts',(-24.1795877670942,13.8774216043795,
130.955375021049)) ;
#131997 = CARTESIAN_POINT('Ctrl Pts',(-24.1390939585473,14.1239848990119,
130.803863087357)) ;
#131998 = CARTESIAN_POINT('Ctrl Pts',(-24.0794901932382,14.3192776170792,
130.596679031769)) ;
#131999 = CARTESIAN_POINT('Ctrl Pts',(-24.0055352361048,14.4507732360595,
130.347522670003)) ;
#132000 = CARTESIAN_POINT('Ctrl Pts',(-23.9233178114793,14.5087792678555,
130.074243320989)) ;
#132001 = CARTESIAN_POINT('Ctrl Pts',(-23.8391129704671,14.4887238336712,
129.795024289797)) ;
#132002 = CARTESIAN_POINT('Ctrl Pts',(-23.7605064372372,14.3928285084541,
129.532382450158)) ;
#132003 = CARTESIAN_POINT('Ctrl Pts',(-23.6928180061624,14.2263682040696,
129.30137255382)) ;
#132004 = CARTESIAN_POINT('Ctrl Pts',(-23.6426620351328,14.0038696460673,
129.121863214626)) ;
#132005 = CARTESIAN_POINT('Ctrl Pts',(-23.613563581647,13.7389372008462,129.003713269081)) ;
#132006 = CARTESIAN_POINT('Ctrl Pts',(-23.6086509708226,13.4518073715824,
128.956278206236)) ;
#132007 = CARTESIAN_POINT('Ctrl Pts',(-23.6290105898186,13.1616327439453,
128.982551634326)) ;
#132008 = CARTESIAN_POINT('Ctrl Pts',(-23.6739522585566,12.8906304372966,
129.080681338749)) ;
#132009 = CARTESIAN_POINT('Ctrl Pts',(-23.7407279250101,12.6585325321797,
129.242687250476)) ;
#132010 = CARTESIAN_POINT('Ctrl Pts',(-23.8252467089156,12.4808578746759,
129.456558276985)) ;
#132011 = CARTESIAN_POINT('Ctrl Pts',(-23.9234212908845,12.369794968941,129.709975426016)) ;
#132012 = CARTESIAN_POINT('Ctrl Pts',(-24.0266916219991,12.3353140243209,
129.978700782335)) ;
#132013 = CARTESIAN_POINT('Ctrl Pts',(-24.1303332495694,12.3783402005982,
130.248268071055)) ;
#132014 = CARTESIAN_POINT('Ctrl Pts',(-24.2265146825975,12.4961137906607,
130.496181048475)) ;
#132015 = CARTESIAN_POINT('Ctrl Pts',(-24.3096595921357,12.6800956082709,
130.705970404282)) ;
#132016 = CARTESIAN_POINT('Ctrl Pts',(-24.3745179631744,12.9180877152906,
130.862244767084)) ;
#132017 = CARTESIAN_POINT('Ctrl Pts',(-24.4167847945233,13.1911275173993,
130.952669619891)) ;
#132018 = CARTESIAN_POINT('Ctrl Pts',(-24.4345812423772,13.4815072415882,
130.971518185869)) ;
#132019 = CARTESIAN_POINT('Ctrl Pts',(-24.4270213519574,13.7684314308885,
130.916204524826)) ;
#132020 = CARTESIAN_POINT('Ctrl Pts',(-24.3956514842814,14.029076308477,130.791530690429)) ;
#132021 = CARTESIAN_POINT('Ctrl Pts',(-24.343165506001,14.2473093926041,130.605025756878)) ;
#132022 = CARTESIAN_POINT('Ctrl Pts',(-24.2745743047042,14.4057091519906,
130.371660986809)) ;
#132023 = CARTESIAN_POINT('Ctrl Pts',(-24.1945925450092,14.4946178708306,
130.104760579953)) ;
#132024 = CARTESIAN_POINT('Ctrl Pts',(-24.11071512251,14.5063975208026,129.826695894897)) ;
#132025 = CARTESIAN_POINT('Ctrl Pts',(-24.0286060386776,14.4401278585609,
129.553540640394)) ;
#132026 = CARTESIAN_POINT('Ctrl Pts',(-23.9562423178897,14.3020001323071,
129.309200756072)) ;
#132027 = CARTESIAN_POINT('Ctrl Pts',(-23.8982704981956,14.100380875427,129.106698871819)) ;
#132028 = CARTESIAN_POINT('Ctrl Pts',(-23.8601423404147,13.8504602239821,
128.962217821069)) ;
#132029 = CARTESIAN_POINT('Ctrl Pts',(-23.8451537683981,13.5690360496352,
128.88522225926)) ;
#132030 = CARTESIAN_POINT('Ctrl Pts',(-23.85536903869,13.277347744237,128.881881865911)) ;
#132031 = CARTESIAN_POINT('Ctrl Pts',(-23.8903250024146,12.9978265767653,
128.951024979183)) ;
#132032 = CARTESIAN_POINT('Ctrl Pts',(-23.9487275671782,12.747023860199,129.088449649182)) ;
#132033 = CARTESIAN_POINT('Ctrl Pts',(-24.0267536508702,12.5453431667421,
129.283298823089)) ;
#132034 = CARTESIAN_POINT('Ctrl Pts',(-24.1198629233628,12.4062333259034,
129.52213584094)) ;
#132035 = CARTESIAN_POINT('Ctrl Pts',(-24.2215666079949,12.3400677949455,
129.786207600519)) ;
#132036 = CARTESIAN_POINT('Ctrl Pts',(-24.3264846884265,12.3515722965719,
130.059403729799)) ;
#132037 = CARTESIAN_POINT('Ctrl Pts',(-24.4261565993231,12.4396025465946,
130.317564726088)) ;
#132038 = CARTESIAN_POINT('Ctrl Pts',(-24.515504520949,12.5983879462257,130.545404926639)) ;
#132039 = CARTESIAN_POINT('Ctrl Pts',(-24.5881171815504,12.8155081778463,
130.724487254865)) ;
#132040 = CARTESIAN_POINT('Ctrl Pts',(-24.6401896035301,13.0777480891852,
130.8433438272)) ;
#132041 = CARTESIAN_POINT('Ctrl Pts',(-24.6679851185762,13.3640007134148,
130.891395810982)) ;
#132042 = CARTESIAN_POINT('Ctrl Pts',(-24.6706717433523,13.6530970190172,
130.866255003353)) ;
#132043 = CARTESIAN_POINT('Ctrl Pts',(-24.6486810155768,13.9274410550996,
130.768823051012)) ;
#132044 = CARTESIAN_POINT('Ctrl Pts',(-24.6043588117149,14.1649405448642,
130.60624558075)) ;
#132045 = CARTESIAN_POINT('Ctrl Pts',(-24.5413708101056,14.3499176915205,
130.389027795027)) ;
#132046 = CARTESIAN_POINT('Ctrl Pts',(-24.4653494690363,14.4676736740884,
130.133852904625)) ;
#132047 = CARTESIAN_POINT('Ctrl Pts',(-24.3825873013246,14.5109849198275,
129.859094894237)) ;
#132048 = CARTESIAN_POINT('Ctrl Pts',(-24.2987925768636,14.4763368011369,
129.58106163939)) ;
#132049 = CARTESIAN_POINT('Ctrl Pts',(-24.2217612201684,14.3664425274482,
129.322969701944)) ;
#132050 = CARTESIAN_POINT('Ctrl Pts',(-24.1570057110458,14.1882602546085,
129.100578369949)) ;
#132051 = CARTESIAN_POINT('Ctrl Pts',(-24.1105157071068,13.9563928712726,
128.931742068379)) ;
#132052 = CARTESIAN_POINT('Ctrl Pts',(-24.0858458393616,13.6856075071528,
128.826527819527)) ;
#132053 = CARTESIAN_POINT('Ctrl Pts',(-24.0856539585114,13.3967978155194,
128.792918629269)) ;
#132054 = CARTESIAN_POINT('Ctrl Pts',(-24.1107926076059,13.1083772147109,
128.833125740032)) ;
#132055 = CARTESIAN_POINT('Ctrl Pts',(-24.1600137825134,12.8436201216384,
128.943820657913)) ;
#132056 = CARTESIAN_POINT('Ctrl Pts',(-24.2308058798189,12.6197329650473,
129.117423409396)) ;
#132057 = CARTESIAN_POINT('Ctrl Pts',(-24.3182751718309,12.4541610182818,
129.339893353894)) ;
#132058 = CARTESIAN_POINT('Ctrl Pts',(-24.4176896908462,12.3575181073951,
129.59708909666)) ;
#132059 = CARTESIAN_POINT('Ctrl Pts',(-24.5213942641841,12.337407534574,129.86708474398)) ;
#132060 = CARTESIAN_POINT('Ctrl Pts',(-24.6242611097352,12.3950240477661,
130.134369464736)) ;
#132061 = CARTESIAN_POINT('Ctrl Pts',(-24.7182893080511,12.5255974682326,
130.376052536827)) ;
#132062 = CARTESIAN_POINT('Ctrl Pts',(-24.7987860343519,12.7221236513144,
130.577891266987)) ;
#132063 = CARTESIAN_POINT('Ctrl Pts',(-24.8592668458931,12.966643820031,130.721612719223)) ;
#132064 = CARTESIAN_POINT('Ctrl Pts',(-24.8973477603996,13.2467842966359,
130.799514303858)) ;
#132065 = CARTESIAN_POINT('Ctrl Pts',(-24.9101357439362,13.5364084867458,
130.803917200582)) ;
#132066 = CARTESIAN_POINT('Ctrl Pts',(-24.8980433329888,13.819301352246,130.735470391269)) ;
#132067 = CARTESIAN_POINT('Ctrl Pts',(-24.8624508729161,14.0737430594077,
130.598397208659)) ;
#132068 = CARTESIAN_POINT('Ctrl Pts',(-24.8063650001413,14.2823383256047,
130.401314654759)) ;
#132069 = CARTESIAN_POINT('Ctrl Pts',(-24.7352153152331,14.4280819786068,
130.160457808913)) ;
#132070 = CARTESIAN_POINT('Ctrl Pts',(-24.654277110767,14.5027907188546,129.890917785084)) ;
#132071 = CARTESIAN_POINT('Ctrl Pts',(-24.569599491767,14.4996009182714,129.610218523976)) ;
#132072 = CARTESIAN_POINT('Ctrl Pts',(-24.4895659727805,14.4198435135005,
129.343494691889)) ;
#132073 = CARTESIAN_POINT('Ctrl Pts',(-24.4190126879205,14.2682255575811,
129.104196361098)) ;
#132074 = CARTESIAN_POINT('Ctrl Pts',(-24.364598178107,14.0566692320112,128.91218100257)) ;
#132075 = CARTESIAN_POINT('Ctrl Pts',(-24.3305009683015,13.7984046917339,
128.779328284604)) ;
#132076 = CARTESIAN_POINT('Ctrl Pts',(-24.3202768420663,13.5146255183712,
128.716401612773)) ;
#132077 = CARTESIAN_POINT('Ctrl Pts',(-24.3351461344103,13.22379017507,128.726708255358)) ;
#132078 = CARTESIAN_POINT('Ctrl Pts',(-24.3747056074861,12.9476430099182,
128.809207275973)) ;
#132079 = CARTESIAN_POINT('Ctrl Pts',(-24.4373988447194,12.7041858709694,
128.959075140171)) ;
#132080 = CARTESIAN_POINT('Ctrl Pts',(-24.5182754986541,12.5142908380612,
129.162405255088)) ;
#132081 = CARTESIAN_POINT('Ctrl Pts',(-24.6137660742652,12.3877724329813,
129.408115006488)) ;
#132082 = CARTESIAN_POINT('Ctrl Pts',(-24.7167971690515,12.3361912043238,
129.675956387308)) ;
#132083 = CARTESIAN_POINT('Ctrl Pts',(-24.8208049085079,12.3624798224069,
129.946681899111)) ;
#132084 = CARTESIAN_POINT('Ctrl Pts',(-24.9189695732058,12.4640688022784,
130.200435824458)) ;
#132085 = CARTESIAN_POINT('Ctrl Pts',(-25.005956640633,12.6358046245907,130.421244636591)) ;
#132086 = CARTESIAN_POINT('Ctrl Pts',(-25.0747012664645,12.862048858162,130.589103084132)) ;
#132087 = CARTESIAN_POINT('Ctrl Pts',(-25.1223375525266,13.1294243703739,
130.69512008432)) ;
#132088 = CARTESIAN_POINT('Ctrl Pts',(-25.1455445896858,13.419127554444,130.729642616116)) ;
#132089 = CARTESIAN_POINT('Ctrl Pts',(-25.1435152363736,13.7060585256719,
130.690801967982)) ;
#132090 = CARTESIAN_POINT('Ctrl Pts',(-25.1170308827865,13.9758635071568,
130.580144935401)) ;
#132091 = CARTESIAN_POINT('Ctrl Pts',(-25.0688142460135,14.2044690811379,
130.40618368144)) ;
#132092 = CARTESIAN_POINT('Ctrl Pts',(-25.003123247664,14.3772046466544,130.18118138791)) ;
#132093 = CARTESIAN_POINT('Ctrl Pts',(-24.9252844700022,14.4817041640368,
129.920684773534)) ;
#132094 = CARTESIAN_POINT('Ctrl Pts',(-24.8415989541778,14.5103977605507,
129.643097336818)) ;
#132095 = CARTESIAN_POINT('Ctrl Pts',(-24.7589132492041,14.461387716176,129.368476107022)) ;
#132096 = CARTESIAN_POINT('Ctrl Pts',(-24.6835796855055,14.3378670523305,
129.115253926662)) ;
#132097 = CARTESIAN_POINT('Ctrl Pts',(-24.6219712562161,14.1487649480966,
128.902143850339)) ;
#132098 = CARTESIAN_POINT('Ctrl Pts',(-24.5791815584349,13.9077124472436,
128.744012805924)) ;
#132099 = CARTESIAN_POINT('Ctrl Pts',(-24.5590011432879,13.6318349091011,
128.651919455676)) ;
#132100 = CARTESIAN_POINT('Ctrl Pts',(-24.5636129562954,13.3411961915081,
128.632272182411)) ;
#132101 = CARTESIAN_POINT('Ctrl Pts',(-24.5933692421231,13.0563347009616,
128.686073174335)) ;
#132102 = CARTESIAN_POINT('Ctrl Pts',(-24.6470060166101,12.7976622253545,
128.809603060301)) ;
#132103 = CARTESIAN_POINT('Ctrl Pts',(-24.7208016129616,12.584625305209,128.992205539617)) ;
#132104 = CARTESIAN_POINT('Ctrl Pts',(-24.8118536009071,12.429833286881,129.224781939929)) ;
#132105 = CARTESIAN_POINT('Ctrl Pts',(-24.911545430168,12.3481748757021,129.483189757942)) ;
#132106 = CARTESIAN_POINT('Ctrl Pts',(-25.0164125625319,12.3422836205948,
129.75626651559)) ;
#132107 = CARTESIAN_POINT('Ctrl Pts',(-25.117816306108,12.414162317258,130.019416608038)) ;
#132108 = CARTESIAN_POINT('Ctrl Pts',(-25.2100635855326,12.55849168118,130.255714929222)) ;
#132109 = CARTESIAN_POINT('Ctrl Pts',(-25.2867433505999,12.7644624942609,
130.446624226534)) ;
#132110 = CARTESIAN_POINT('Ctrl Pts',(-25.3433959651672,13.0174115077838,
130.579031809203)) ;
#132111 = CARTESIAN_POINT('Ctrl Pts',(-25.3766991434267,13.2998964348547,
130.643172314106)) ;
#132112 = CARTESIAN_POINT('Ctrl Pts',(-25.3849027762527,13.5908799629275,
130.634029729427)) ;
#132113 = CARTESIAN_POINT('Ctrl Pts',(-25.3681244270798,13.8706960081611,
130.551809717868)) ;
#132114 = CARTESIAN_POINT('Ctrl Pts',(-25.3281885696402,14.1180202656557,
130.401959719847)) ;
#132115 = CARTESIAN_POINT('Ctrl Pts',(-25.2692654377525,14.3143765894564,
130.196866938718)) ;
#132116 = CARTESIAN_POINT('Ctrl Pts',(-25.1954627990625,14.4481660809184,
129.948075722546)) ;
#132117 = CARTESIAN_POINT('Ctrl Pts',(-25.1135963031033,14.5080838606745,
129.675906827394)) ;
#132118 = CARTESIAN_POINT('Ctrl Pts',(-25.0294161558255,14.4905518531177,
129.396790506061)) ;
#132119 = CARTESIAN_POINT('Ctrl Pts',(-24.9503166631056,14.3964092296967,
129.132598410075)) ;
#132120 = CARTESIAN_POINT('Ctrl Pts',(-24.8824484698929,14.232304987228,128.901173407916)) ;
#132121 = CARTESIAN_POINT('Ctrl Pts',(-24.831656485841,14.0113006854444,128.719789796304)) ;
#132122 = CARTESIAN_POINT('Ctrl Pts',(-24.8018618709668,13.7469853282518,
128.599564702445)) ;
#132123 = CARTESIAN_POINT('Ctrl Pts',(-24.7961937055128,13.4601451324146,
128.54991646717)) ;
#132124 = CARTESIAN_POINT('Ctrl Pts',(-24.8160226315964,13.1687003200991,
128.574510511953)) ;
#132125 = CARTESIAN_POINT('Ctrl Pts',(-24.859902739483,12.8989650919222,128.669805113981)) ;
#132126 = CARTESIAN_POINT('Ctrl Pts',(-24.9266168659618,12.6635916504989,
128.831356633498)) ;
#132127 = CARTESIAN_POINT('Ctrl Pts',(-25.0103639202873,12.485239800862,129.043133485935)) ;
#132128 = CARTESIAN_POINT('Ctrl Pts',(-25.1082951885594,12.3719259500599,
129.295815313463)) ;
#132129 = CARTESIAN_POINT('Ctrl Pts',(-25.2113378058678,12.3351771032852,
129.563924734244)) ;
#132130 = CARTESIAN_POINT('Ctrl Pts',(-25.3153987713946,12.3762351050997,
129.834608633564)) ;
#132131 = CARTESIAN_POINT('Ctrl Pts',(-25.4113691303234,12.4911992435135,
130.082089209234)) ;
#132132 = CARTESIAN_POINT('Ctrl Pts',(-25.4955318190917,12.6745749260732,
130.29463045715)) ;
#132133 = CARTESIAN_POINT('Ctrl Pts',(-25.560704508805,12.9105841176317,130.451940846143)) ;
#132134 = CARTESIAN_POINT('Ctrl Pts',(-25.6037591586016,13.1834575472762,
130.544589177351)) ;
#132135 = CARTESIAN_POINT('Ctrl Pts',(-25.6221540731369,13.4728172007292,
130.565280977399)) ;
#132136 = CARTESIAN_POINT('Ctrl Pts',(-25.6154890774634,13.7593252111675,
130.512691578256)) ;
#132137 = CARTESIAN_POINT('Ctrl Pts',(-25.5845017414514,14.0229111380707,
130.388875573167)) ;
#132138 = CARTESIAN_POINT('Ctrl Pts',(-25.5329646548234,14.2409568530166,
130.205405121793)) ;
#132139 = CARTESIAN_POINT('Ctrl Pts',(-25.4643492210366,14.4024702596202,
129.971739445436)) ;
#132140 = CARTESIAN_POINT('Ctrl Pts',(-25.3848249850593,14.4930252918819,
129.706290426526)) ;
#132141 = CARTESIAN_POINT('Ctrl Pts',(-25.3009346998094,14.5071138077779,
129.428162516891)) ;
#132142 = CARTESIAN_POINT('Ctrl Pts',(-25.2189936227422,14.4434722304718,
129.155638517111)) ;
#132143 = CARTESIAN_POINT('Ctrl Pts',(-25.1460018098747,14.3072991508372,
128.909365963459)) ;
#132144 = CARTESIAN_POINT('Ctrl Pts',(-25.0872927957611,14.1061281755834,
128.704547183538)) ;
#132145 = CARTESIAN_POINT('Ctrl Pts',(-25.0487858755379,13.8584458365122,
128.559117426276)) ;
#132146 = CARTESIAN_POINT('Ctrl Pts',(-25.0330304801592,13.5782527615593,
128.479942965013)) ;
#132147 = CARTESIAN_POINT('Ctrl Pts',(-25.0424542208566,13.2862405830432,
128.474252693863)) ;
#132148 = CARTESIAN_POINT('Ctrl Pts',(-25.0767412324267,13.0054673407222,
128.541371132674)) ;
#132149 = CARTESIAN_POINT('Ctrl Pts',(-25.1348051000407,12.7527978446706,
128.67768872235)) ;
#132150 = CARTESIAN_POINT('Ctrl Pts',(-25.2119030388808,12.5507722085017,
128.870018404504)) ;
#132151 = CARTESIAN_POINT('Ctrl Pts',(-25.3047050008252,12.4092693590586,
129.107923829017)) ;
#132152 = CARTESIAN_POINT('Ctrl Pts',(-25.406443595545,12.3409406073707,129.37203421041)) ;
#132153 = CARTESIAN_POINT('Ctrl Pts',(-25.5110390200225,12.3499819194409,
129.644402105975)) ;
#132154 = CARTESIAN_POINT('Ctrl Pts',(-25.6114390222507,12.4363532158425,
129.904516274518)) ;
#132155 = CARTESIAN_POINT('Ctrl Pts',(-25.7007310200177,12.5925663631045,
130.132357144071)) ;
#132156 = CARTESIAN_POINT('Ctrl Pts',(-25.7740950725506,12.8085170384963,
130.313559518156)) ;
#132157 = CARTESIAN_POINT('Ctrl Pts',(-25.8267351162025,13.0694866152918,
130.434112913458)) ;
#132158 = CARTESIAN_POINT('Ctrl Pts',(-25.8553312907165,13.3550371201656,
130.48453070364)) ;
#132159 = CARTESIAN_POINT('Ctrl Pts',(-25.8586885366147,13.6462143005165,
130.461126760816)) ;
#132160 = CARTESIAN_POINT('Ctrl Pts',(-25.837444412916,13.9195287631536,130.366084906634)) ;
#132161 = CARTESIAN_POINT('Ctrl Pts',(-25.7937488394422,14.1586150899391,
130.205310735235)) ;
#132162 = CARTESIAN_POINT('Ctrl Pts',(-25.7313611315605,14.3449689837057,
129.989913913384)) ;
#132163 = CARTESIAN_POINT('Ctrl Pts',(-25.6556964572195,14.465239738532,129.735783996914)) ;
#132164 = CARTESIAN_POINT('Ctrl Pts',(-25.5723964230934,14.5107689866746,
129.459195604095)) ;
#132165 = CARTESIAN_POINT('Ctrl Pts',(-25.4893174125801,14.4787461978325,
129.183580822489)) ;
#132166 = CARTESIAN_POINT('Ctrl Pts',(-25.4113051186338,14.3700644324197,
128.922314853824)) ;
#132167 = CARTESIAN_POINT('Ctrl Pts',(-25.3465909420863,14.1946408166751,
128.700275185896)) ;
#132168 = CARTESIAN_POINT('Ctrl Pts',(-25.299369271165,13.963907732595,128.529234819729)) ;
#132169 = CARTESIAN_POINT('Ctrl Pts',(-25.2739922523,13.6940409321305,128.421969041019)) ;
#132170 = CARTESIAN_POINT('Ctrl Pts',(-25.2731534451911,13.4043243937501,
128.386332734542)) ;
#132171 = CARTESIAN_POINT('Ctrl Pts',(-25.2973628386527,13.1175424358185,
128.424062655725)) ;
#132172 = CARTESIAN_POINT('Ctrl Pts',(-25.3462006392316,12.8501254079525,
128.533419495547)) ;
#132173 = CARTESIAN_POINT('Ctrl Pts',(-25.4160919098287,12.6260375389968,
128.704569775621)) ;
#132174 = CARTESIAN_POINT('Ctrl Pts',(-25.5032418915579,12.4581545252769,
128.926046604269)) ;
#132175 = CARTESIAN_POINT('Ctrl Pts',(-25.6021785519615,12.3594525497003,
129.181922681907)) ;
#132176 = CARTESIAN_POINT('Ctrl Pts',(-25.7061730224389,12.3367944069397,
129.452652747223)) ;
#132177 = CARTESIAN_POINT('Ctrl Pts',(-25.8094492173163,12.3925085409291,
129.721047874811)) ;
#132178 = CARTESIAN_POINT('Ctrl Pts',(-25.9037624326914,12.5213898755188,
129.963557213451)) ;
#132179 = CARTESIAN_POINT('Ctrl Pts',(-25.9844805178092,12.7155724021421,
130.166157205425)) ;
#132180 = CARTESIAN_POINT('Ctrl Pts',(-26.0456691934443,12.9595220676015,
130.311865673155)) ;
#132181 = CARTESIAN_POINT('Ctrl Pts',(-26.0842093042236,13.2367788940881,
130.391368626224)) ;
#132182 = CARTESIAN_POINT('Ctrl Pts',(-26.0979544525776,13.5277643625836,
130.39839898417)) ;
#132183 = CARTESIAN_POINT('Ctrl Pts',(-26.0864824258526,13.8120453761231,
130.331665108325)) ;
#132184 = CARTESIAN_POINT('Ctrl Pts',(-26.05142082645,14.0676654739834,130.196112404188)) ;
#132185 = CARTESIAN_POINT('Ctrl Pts',(-25.9959721958356,14.2771419928287,
130.000979869832)) ;
#132186 = CARTESIAN_POINT('Ctrl Pts',(-25.9251922030581,14.425031880978,129.761195796767)) ;
#132187 = CARTESIAN_POINT('Ctrl Pts',(-25.8440763649555,14.5017260060049,
129.490996412094)) ;
#132188 = CARTESIAN_POINT('Ctrl Pts',(-25.7603662435499,14.5010099059246,
129.213512691512)) ;
#132189 = CARTESIAN_POINT('Ctrl Pts',(-25.6794136560246,14.4231233705973,
128.943812915352)) ;
#132190 = CARTESIAN_POINT('Ctrl Pts',(-25.6086694413268,14.2735700722065,
128.704038175328)) ;
#132191 = CARTESIAN_POINT('Ctrl Pts',(-25.5536232001884,14.0631260843178,
128.510103402269)) ;
#132192 = CARTESIAN_POINT('Ctrl Pts',(-25.5190005221295,13.8068513237717,
128.37583898455)) ;
#132193 = CARTESIAN_POINT('Ctrl Pts',(-25.5079988886962,13.5229068768556,
128.310556815572)) ;
#132194 = CARTESIAN_POINT('Ctrl Pts',(-25.522136912891,13.2323185296325,128.31877011903)) ;
#132195 = CARTESIAN_POINT('Ctrl Pts',(-25.5609778387885,12.955462422634,128.399168054502)) ;
#132196 = CARTESIAN_POINT('Ctrl Pts',(-25.622981897995,12.7108337306576,128.547046303102)) ;
#132197 = CARTESIAN_POINT('Ctrl Pts',(-25.7035387876594,12.5189036902296,
128.749376462235)) ;
#132198 = CARTESIAN_POINT('Ctrl Pts',(-25.7983973245378,12.3906586207823,
128.993347141695)) ;
#132199 = CARTESIAN_POINT('Ctrl Pts',(-25.9014394205249,12.3366531336248,
129.261165642822)) ;
#132200 = CARTESIAN_POINT('Ctrl Pts',(-26.0053503635526,12.360297772879,129.531671267842)) ;
#132201 = CARTESIAN_POINT('Ctrl Pts',(-26.1046179703446,12.4609988515391,
129.788341417843)) ;
#132202 = CARTESIAN_POINT('Ctrl Pts',(-26.1910706407531,12.6291274638668,
130.0079564874)) ;
#132203 = CARTESIAN_POINT('Ctrl Pts',(-26.2610067862353,12.8555169755094,
130.179031109569)) ;
#132204 = CARTESIAN_POINT('Ctrl Pts',(-26.3090567054831,13.1215885522129,
130.286335393292)) ;
#132205 = CARTESIAN_POINT('Ctrl Pts',(-26.3329796835872,13.4096083938423,
130.323096945283)) ;
#132206 = CARTESIAN_POINT('Ctrl Pts',(-26.3317340747676,13.698212942693,130.286391172774)) ;
#132207 = CARTESIAN_POINT('Ctrl Pts',(-26.3058007346478,13.9691452295141,
130.177299627734)) ;
#132208 = CARTESIAN_POINT('Ctrl Pts',(-26.2583066398341,14.1982918407705,
130.005562251346)) ;
#132209 = CARTESIAN_POINT('Ctrl Pts',(-26.1931751350795,14.3728095621698,
129.782233989023)) ;
#132210 = CARTESIAN_POINT('Ctrl Pts',(-26.1155255616385,14.479662285758,129.522250222093)) ;
#132211 = CARTESIAN_POINT('Ctrl Pts',(-26.0318486038747,14.5107460879228,
129.244664158376)) ;
#132212 = CARTESIAN_POINT('Ctrl Pts',(-25.9488165487381,14.4636147982726,
128.968932999966)) ;
#132213 = CARTESIAN_POINT('Ctrl Pts',(-25.8735146658894,14.3427084720644,
128.715956195703)) ;
#132214 = CARTESIAN_POINT('Ctrl Pts',(-25.811125852612,14.1545214106307,128.500410033898)) ;
#132215 = CARTESIAN_POINT('Ctrl Pts',(-25.767859635489,13.914665784431,128.340908123874)) ;
#132216 = CARTESIAN_POINT('Ctrl Pts',(-25.7470531048229,13.6405172708492,
128.247102795506)) ;
#132217 = CARTESIAN_POINT('Ctrl Pts',(-25.7508957888745,13.3501102818962,
128.225215226321)) ;
#132218 = CARTESIAN_POINT('Ctrl Pts',(-25.7797927372613,13.0651843315454,
128.276561420719)) ;
#132219 = CARTESIAN_POINT('Ctrl Pts',(-25.8330708547357,12.80388772374,128.398847085602)) ;
#132220 = CARTESIAN_POINT('Ctrl Pts',(-25.9063371941856,12.5899465270377,
128.579947959411)) ;
#132221 = CARTESIAN_POINT('Ctrl Pts',(-25.9963126660368,12.4339563210189,
128.809607064104)) ;
#132222 = CARTESIAN_POINT('Ctrl Pts',(-26.0966203558645,12.3491846989202,
129.069534053189)) ;
#132223 = CARTESIAN_POINT('Ctrl Pts',(-26.2015343109458,12.3415474281895,
129.342731765695)) ;
#132224 = CARTESIAN_POINT('Ctrl Pts',(-26.3027211617629,12.4110292201394,
129.60537279447)) ;
#132225 = CARTESIAN_POINT('Ctrl Pts',(-26.3953588574291,12.5533605448057,
129.842803792173)) ;
#132226 = CARTESIAN_POINT('Ctrl Pts',(-26.4724658228993,12.7574391512257,
130.035002583383)) ;
#132227 = CARTESIAN_POINT('Ctrl Pts',(-26.5299060950814,13.0095817126533,
130.169659341123)) ;
#132228 = CARTESIAN_POINT('Ctrl Pts',(-26.5639504532064,13.2928226801242,
130.235818361087)) ;
#132229 = CARTESIAN_POINT('Ctrl Pts',(-26.5727935985865,13.5820119966617,
130.228755567199)) ;
#132230 = CARTESIAN_POINT('Ctrl Pts',(-26.5567072828717,13.8633229249982,
130.148453208055)) ;
#132231 = CARTESIAN_POINT('Ctrl Pts',(-26.5174678494182,14.1112602779132,
130.000718041267)) ;
#132232 = CARTESIAN_POINT('Ctrl Pts',(-26.4589493371831,14.3095521754014,
129.79675027408)) ;
#132233 = CARTESIAN_POINT('Ctrl Pts',(-26.3857504408749,14.4451057235358,
129.549834730436)) ;
#132234 = CARTESIAN_POINT('Ctrl Pts',(-26.3033581527554,14.5076745769451,
129.275854508276)) ;
#132235 = CARTESIAN_POINT('Ctrl Pts',(-26.2193621817028,14.4918702514085,
128.997365975633)) ;
#132236 = CARTESIAN_POINT('Ctrl Pts',(-26.1403227598029,14.4001695900989,
128.733462893607)) ;
#132237 = CARTESIAN_POINT('Ctrl Pts',(-26.0720785017029,14.238339270588,128.500982256028)) ;
#132238 = CARTESIAN_POINT('Ctrl Pts',(-26.0205445494064,14.0178457541506,
128.317291271494)) ;
#132239 = CARTESIAN_POINT('Ctrl Pts',(-25.9901309545097,13.7549024704848,
128.195319458128)) ;
#132240 = CARTESIAN_POINT('Ctrl Pts',(-25.9838907425677,13.4669383655623,
128.143823454231)) ;
#132241 = CARTESIAN_POINT('Ctrl Pts',(-26.002625472959,13.1792878389568,128.165694781332)) ;
#132242 = CARTESIAN_POINT('Ctrl Pts',(-26.0462578585361,12.9054935275296,
128.259864888277)) ;
#132243 = CARTESIAN_POINT('Ctrl Pts',(-26.1117838862911,12.6708451835732,
128.418257412013)) ;
#132244 = CARTESIAN_POINT('Ctrl Pts',(-26.1958394673662,12.4890109361581,
128.630614971608)) ;
#132245 = CARTESIAN_POINT('Ctrl Pts',(-26.292450313642,12.3747427440592,128.879802823841)) ;
#132246 = CARTESIAN_POINT('Ctrl Pts',(-26.3961466629634,12.335118127865,129.149563628382)) ;
#132247 = CARTESIAN_POINT('Ctrl Pts',(-26.4997927945682,12.3735357257966,
129.41921706946)) ;
#132248 = CARTESIAN_POINT('Ctrl Pts',(-26.5970562066531,12.4876827050984,
129.670119063763)) ;
#132249 = CARTESIAN_POINT('Ctrl Pts',(-26.6809623236233,12.668143871092,129.882175659137)) ;
#132250 = CARTESIAN_POINT('Ctrl Pts',(-26.7469567383412,12.9033827829949,
130.041784506141)) ;
#132251 = CARTESIAN_POINT('Ctrl Pts',(-26.7905248136644,13.1743601664502,
130.136070712378)) ;
#132252 = CARTESIAN_POINT('Ctrl Pts',(-26.8098089341939,13.4644840041335,
130.159245371207)) ;
#132253 = CARTESIAN_POINT('Ctrl Pts',(-26.8037407483827,13.7518155739233,
130.108342116625)) ;
#132254 = CARTESIAN_POINT('Ctrl Pts',(-26.7736744947239,14.0147480425275,
129.987433665233)) ;
#132255 = CARTESIAN_POINT('Ctrl Pts',(-26.7224117937105,14.2359322469135,
129.804543108639)) ;
#132256 = CARTESIAN_POINT('Ctrl Pts',(-26.6540459121311,14.3990328419962,
129.571575856472)) ;
#132257 = CARTESIAN_POINT('Ctrl Pts',(-26.5752101350165,14.4913721211862,
129.308326055989)) ;
#132258 = CARTESIAN_POINT('Ctrl Pts',(-26.4908765753451,14.5077030613306,
129.028705274742)) ;
#132259 = CARTESIAN_POINT('Ctrl Pts',(-26.4092296365473,14.4466726935246,
128.757236988289)) ;
#132260 = CARTESIAN_POINT('Ctrl Pts',(-26.3352722351391,14.3110620977678,
128.507833953029)) ;
#132261 = CARTESIAN_POINT('Ctrl Pts',(-26.2766889458892,14.1132680684101,
128.303711145387)) ;
#132262 = CARTESIAN_POINT('Ctrl Pts',(-26.2372639174626,13.8656264960883,
128.15541845975)) ;
#132263 = CARTESIAN_POINT('Ctrl Pts',(-26.2209130537975,13.5853317318957,
128.074439710367)) ;
#132264 = CARTESIAN_POINT('Ctrl Pts',(-26.2296856924358,13.2939513094312,
128.066914197785)) ;
#132265 = CARTESIAN_POINT('Ctrl Pts',(-26.2631798636915,13.0136081090702,
128.131828211089)) ;
#132266 = CARTESIAN_POINT('Ctrl Pts',(-26.3203316415523,12.7604084565328,
128.265584239078)) ;
#132267 = CARTESIAN_POINT('Ctrl Pts',(-26.397246993967,12.5556140537718,128.457218817256)) ;
#132268 = CARTESIAN_POINT('Ctrl Pts',(-26.4898764488098,12.412162783817,128.694571316763)) ;
#132269 = CARTESIAN_POINT('Ctrl Pts',(-26.5911530122536,12.3419224833159,
128.957426665658)) ;
#132270 = CARTESIAN_POINT('Ctrl Pts',(-26.6956543409951,12.3485705631489,
129.229554057824)) ;
#132271 = CARTESIAN_POINT('Ctrl Pts',(-26.7962358912617,12.4325162173742,
129.490217635024)) ;
#132272 = CARTESIAN_POINT('Ctrl Pts',(-26.8862177213639,12.5872706018155,
129.719968083883)) ;
#132273 = CARTESIAN_POINT('Ctrl Pts',(-26.9600298412944,12.8016741765326,
129.902501376654)) ;
#132274 = CARTESIAN_POINT('Ctrl Pts',(-27.0132363984096,13.0608926757193,
130.024793668328)) ;
#132275 = CARTESIAN_POINT('Ctrl Pts',(-27.0426146311277,13.3463627388947,
130.077448217005)) ;
#132276 = CARTESIAN_POINT('Ctrl Pts',(-27.0467658686963,13.6367413735624,
130.056476137218)) ;
#132277 = CARTESIAN_POINT('Ctrl Pts',(-27.0262045189193,13.912123441329,129.96328026669)) ;
#132278 = CARTESIAN_POINT('Ctrl Pts',(-26.9829610646689,14.1528033236638,
129.803766513539)) ;
#132279 = CARTESIAN_POINT('Ctrl Pts',(-26.9212047054132,14.3402810134416,
129.590308052972)) ;
#132280 = CARTESIAN_POINT('Ctrl Pts',(-26.8459513519056,14.4626257099404,
129.33741374041)) ;
#132281 = CARTESIAN_POINT('Ctrl Pts',(-26.7626484303445,14.5106364099982,
129.060769517447)) ;
#132282 = CARTESIAN_POINT('Ctrl Pts',(-26.6793325739832,14.4805445966973,
128.784392296914)) ;
#132283 = CARTESIAN_POINT('Ctrl Pts',(-26.6015120722546,14.3748126779467,
128.523896403084)) ;
#132284 = CARTESIAN_POINT('Ctrl Pts',(-26.5360012381168,14.2005693776624,
128.299367371948)) ;
#132285 = CARTESIAN_POINT('Ctrl Pts',(-26.4882466006821,13.9714224956824,
128.126808943075)) ;
#132286 = CARTESIAN_POINT('Ctrl Pts',(-26.4621696395529,13.7016038456452,
128.017397936684)) ;
#132287 = CARTESIAN_POINT('Ctrl Pts',(-26.4605573044593,13.4137877720204,
127.979694610522)) ;
#132288 = CARTESIAN_POINT('Ctrl Pts',(-26.4842037814474,13.1249621059971,
128.015572519599)) ;
#132289 = CARTESIAN_POINT('Ctrl Pts',(-26.5319266616535,12.858759801946,128.121953585796)) ;
#132290 = CARTESIAN_POINT('Ctrl Pts',(-26.601763218089,12.6311849064932,128.292661018411)) ;
#132291 = CARTESIAN_POINT('Ctrl Pts',(-26.6883690358658,12.4620614418067,
128.512623702752)) ;
#132292 = CARTESIAN_POINT('Ctrl Pts',(-26.7871596601743,12.3611529243014,
128.768034196029)) ;
#132293 = CARTESIAN_POINT('Ctrl Pts',(-26.8908594338048,12.336402737043,129.037980194775)) ;
#132294 = CARTESIAN_POINT('Ctrl Pts',(-26.9942677499415,12.3896954767389,
129.30676634427)) ;
#132295 = CARTESIAN_POINT('Ctrl Pts',(-27.0891228503658,12.5169545730866,
129.550776904504)) ;
#132296 = CARTESIAN_POINT('Ctrl Pts',(-27.170110122641,12.7090014500136,129.754247695197)) ;
#132297 = CARTESIAN_POINT('Ctrl Pts',(-27.2319803579197,12.9518209129291,
129.901923479105)) ;
#132298 = CARTESIAN_POINT('Ctrl Pts',(-27.2712167263555,13.2283911259786,
129.983462395853)) ;
#132299 = CARTESIAN_POINT('Ctrl Pts',(-27.2856848450787,13.5192444476926,
129.992606198651)) ;
#132300 = CARTESIAN_POINT('Ctrl Pts',(-27.2749998341,13.8035929406365,129.928231036212)) ;
#132301 = CARTESIAN_POINT('Ctrl Pts',(-27.2405107086992,14.0607675161601,
129.794281704174)) ;
#132302 = CARTESIAN_POINT('Ctrl Pts',(-27.1859404561386,14.2709776513911,
129.601886944103)) ;
#132303 = CARTESIAN_POINT('Ctrl Pts',(-27.1150473623168,14.4220258151157,
129.36152624086)) ;
#132304 = CARTESIAN_POINT('Ctrl Pts',(-27.0343785010806,14.5004899933202,
129.09274938976)) ;
#132305 = CARTESIAN_POINT('Ctrl Pts',(-26.950535069012,14.5020985766214,128.814815907977)) ;
#132306 = CARTESIAN_POINT('Ctrl Pts',(-26.8695870479016,14.426667623352,128.545218407416)) ;
#132307 = CARTESIAN_POINT('Ctrl Pts',(-26.798211588555,14.2786158189735,128.303482030973)) ;
#132308 = CARTESIAN_POINT('Ctrl Pts',(-26.7426992360049,14.0697690186074,
128.108208750919)) ;
#132309 = CARTESIAN_POINT('Ctrl Pts',(-26.7074412852036,13.8142976320865,
127.972057291302)) ;
#132310 = CARTESIAN_POINT('Ctrl Pts',(-26.6957645215905,13.5318062075926,
127.904912693824)) ;
#132311 = CARTESIAN_POINT('Ctrl Pts',(-26.7091353370237,13.2403761874523,
127.91080130822)) ;
#132312 = CARTESIAN_POINT('Ctrl Pts',(-26.74755505738,12.9618561593774,127.989837070354)) ;
#132313 = CARTESIAN_POINT('Ctrl Pts',(-26.8086943560285,12.7173263730279,
128.135355225743)) ;
#132314 = CARTESIAN_POINT('Ctrl Pts',(-26.8888831517,12.5233446886838,128.33655295725)) ;
#132315 = CARTESIAN_POINT('Ctrl Pts',(-26.9835011120047,12.3931312315505,
128.579802503126)) ;
#132316 = CARTESIAN_POINT('Ctrl Pts',(-27.0865721816442,12.337075246258,128.847656402371)) ;
#132317 = CARTESIAN_POINT('Ctrl Pts',(-27.1901303578273,12.3586764449227,
129.117256451724)) ;
#132318 = CARTESIAN_POINT('Ctrl Pts',(-27.2892091804132,12.4563696314589,
129.373537084527)) ;
#132319 = CARTESIAN_POINT('Ctrl Pts',(-27.3766437558911,12.6234424170359,
129.595825398964)) ;
#132320 = CARTESIAN_POINT('Ctrl Pts',(-27.447072154312,12.8484690314232,129.768349176844)) ;
#132321 = CARTESIAN_POINT('Ctrl Pts',(-27.4958104255805,13.1134860607375,
129.877675494575)) ;
#132322 = CARTESIAN_POINT('Ctrl Pts',(-27.5204851717528,13.402425050447,129.916492772369)) ;
#132323 = CARTESIAN_POINT('Ctrl Pts',(-27.5198611034755,13.6901681944769,
129.881727019293)) ;
#132324 = CARTESIAN_POINT('Ctrl Pts',(-27.4947206170695,13.9614083380647,
129.775024765156)) ;
#132325 = CARTESIAN_POINT('Ctrl Pts',(-27.4477408524357,14.1924050674132,
129.604730002262)) ;
#132326 = CARTESIAN_POINT('Ctrl Pts',(-27.3829916295066,14.3688010159201,
129.382496516221)) ;
#132327 = CARTESIAN_POINT('Ctrl Pts',(-27.305567395489,14.4776662097744,129.123157647789)) ;
#132328 = CARTESIAN_POINT('Ctrl Pts',(-27.2222300887403,14.5108828480259,
128.84666452346)) ;
#132329 = CARTESIAN_POINT('Ctrl Pts',(-27.1390665957671,14.4662997711349,
128.570551673275)) ;
#132330 = CARTESIAN_POINT('Ctrl Pts',(-27.063203525044,14.3468724358185,128.315811999268)) ;
#132331 = CARTESIAN_POINT('Ctrl Pts',(-27.000726116674,14.161614932188,128.10021376119)) ;
#132332 = CARTESIAN_POINT('Ctrl Pts',(-26.9566598775861,13.9230022753498,
127.938326275104)) ;
#132333 = CARTESIAN_POINT('Ctrl Pts',(-26.9350826150652,13.6485314062169,
127.842142219284)) ;
#132334 = CARTESIAN_POINT('Ctrl Pts',(-26.9382141999983,13.3583011743042,
127.818182839235)) ;
#132335 = CARTESIAN_POINT('Ctrl Pts',(-26.9665177873497,13.072504270402,127.867737400507)) ;
#132336 = CARTESIAN_POINT('Ctrl Pts',(-27.0188173523961,12.8117566735177,
127.987365016217)) ;
#132337 = CARTESIAN_POINT('Ctrl Pts',(-27.0915996802834,12.5955171582893,
128.166977325295)) ;
#132338 = CARTESIAN_POINT('Ctrl Pts',(-27.1817271815024,12.4369580568928,
128.396898077135)) ;
#132339 = CARTESIAN_POINT('Ctrl Pts',(-27.2813708056134,12.3507869630092,
128.655042348106)) ;
#132340 = CARTESIAN_POINT('Ctrl Pts',(-27.3857827418417,12.3404899643528,
128.926923079581)) ;
#132341 = CARTESIAN_POINT('Ctrl Pts',(-27.4876541467364,12.4078494476239,
129.191403822402)) ;
#132342 = CARTESIAN_POINT('Ctrl Pts',(-27.5807089481865,12.5483871977687,
129.430029656426)) ;
#132343 = CARTESIAN_POINT('Ctrl Pts',(-27.6584612758746,12.7513533086917,
129.624045981255)) ;
#132344 = CARTESIAN_POINT('Ctrl Pts',(-27.7163134902441,13.001941318222,129.759978308328)) ;
#132345 = CARTESIAN_POINT('Ctrl Pts',(-27.7510006841768,13.2828868274063,
129.828206089058)) ;
#132346 = CARTESIAN_POINT('Ctrl Pts',(-27.7607078220157,13.5743278631276,
129.823412590067)) ;
#132347 = CARTESIAN_POINT('Ctrl Pts',(-27.7452570064132,13.8554587804339,
129.745052642731)) ;
#132348 = CARTESIAN_POINT('Ctrl Pts',(-27.7068857846591,14.103739100914,129.599981463497)) ;
#132349 = CARTESIAN_POINT('Ctrl Pts',(-27.6487231943859,14.3046990175591,
129.396931127844)) ;
#132350 = CARTESIAN_POINT('Ctrl Pts',(-27.5755356695319,14.4424188711516,
129.149922663509)) ;
#132351 = CARTESIAN_POINT('Ctrl Pts',(-27.4939933548379,14.5067209234145,
128.878704097542)) ;
#132352 = CARTESIAN_POINT('Ctrl Pts',(-27.4097527588653,14.4936392684735,
128.599416389571)) ;
#132353 = CARTESIAN_POINT('Ctrl Pts',(-27.3303082230943,14.404006740505,128.334269093954)) ;
#132354 = CARTESIAN_POINT('Ctrl Pts',(-27.2614819305869,14.2433942656814,
128.099980444704)) ;
#132355 = CARTESIAN_POINT('Ctrl Pts',(-27.2096136486434,14.0252993056693,
127.915456300396)) ;
#132356 = CARTESIAN_POINT('Ctrl Pts',(-27.178469556164,13.7626963119846,127.791262873367)) ;
#132357 = CARTESIAN_POINT('Ctrl Pts',(-27.1714738989522,13.4766513624265,
127.737736625053)) ;
#132358 = CARTESIAN_POINT('Ctrl Pts',(-27.1895561727833,13.1866966293381,
127.757460183878)) ;
#132359 = CARTESIAN_POINT('Ctrl Pts',(-27.2326135994264,12.9123106961637,
127.849963433579)) ;
#132360 = CARTESIAN_POINT('Ctrl Pts',(-27.2974441217088,12.6769408805555,
128.006390666055)) ;
#132361 = CARTESIAN_POINT('Ctrl Pts',(-27.3808130116155,12.4935889535621,
128.216818650803)) ;
#132362 = CARTESIAN_POINT('Ctrl Pts',(-27.4776575476475,12.3766908568814,
128.466511171481)) ;
#132363 = CARTESIAN_POINT('Ctrl Pts',(-27.5810443505466,12.3352383862452,
128.735442117728)) ;
#132364 = CARTESIAN_POINT('Ctrl Pts',(-27.6845420847214,12.3713736006973,
129.004732437811)) ;
#132365 = CARTESIAN_POINT('Ctrl Pts',(-27.7818596677854,12.4827590293817,
129.255891826048)) ;
#132366 = CARTESIAN_POINT('Ctrl Pts',(-27.8667979944307,12.6627224306716,
129.47073002161)) ;
#132367 = CARTESIAN_POINT('Ctrl Pts',(-27.9330076414952,12.8955397849013,
129.631137908056)) ;
#132368 = CARTESIAN_POINT('Ctrl Pts',(-27.9774352268445,13.1663558963296,
129.72784335586)) ;
#132369 = CARTESIAN_POINT('Ctrl Pts',(-27.9973849513202,13.4563321062043,
129.752958193208)) ;
#132370 = CARTESIAN_POINT('Ctrl Pts',(-27.9920646322741,13.74354179735,129.704297361198)) ;
#132371 = CARTESIAN_POINT('Ctrl Pts',(-27.9626165416411,14.007863745204,129.585142101985)) ;
#132372 = CARTESIAN_POINT('Ctrl Pts',(-27.9119828992553,14.2299792391956,
129.404152786278)) ;
#132373 = CARTESIAN_POINT('Ctrl Pts',(-27.844287943155,14.3948659481182,129.173238937185)) ;
#132374 = CARTESIAN_POINT('Ctrl Pts',(-27.7651604606475,14.4898740802148,
128.908913740689)) ;
#132375 = CARTESIAN_POINT('Ctrl Pts',(-27.681397890891,14.5084149248409,128.631178035807)) ;
#132376 = CARTESIAN_POINT('Ctrl Pts',(-27.5990872491488,14.4492459338564,
128.357554758999)) ;
#132377 = CARTESIAN_POINT('Ctrl Pts',(-27.5253256223266,14.316609488643,128.108970615685)) ;
#132378 = CARTESIAN_POINT('Ctrl Pts',(-27.4659033295799,14.1198900556279,
127.9022461303)) ;
#132379 = CARTESIAN_POINT('Ctrl Pts',(-27.42591393932,13.8734079349303,127.752317228327)) ;
#132380 = CARTESIAN_POINT('Ctrl Pts',(-27.408865491139,13.5947694158123,127.669409669264)) ;
#132381 = CARTESIAN_POINT('Ctrl Pts',(-27.4167455300075,13.3033325180628,
127.659268253717)) ;
#132382 = CARTESIAN_POINT('Ctrl Pts',(-27.4497732461264,13.0207084742087,
127.722612022269)) ;
#132383 = CARTESIAN_POINT('Ctrl Pts',(-27.5060414733426,12.767628690545,127.853947272495)) ;
#132384 = CARTESIAN_POINT('Ctrl Pts',(-27.5826500146593,12.5604751539345,
128.044576460787)) ;
#132385 = CARTESIAN_POINT('Ctrl Pts',(-27.6748867687302,12.4152916729436,
128.280805111389)) ;
#132386 = CARTESIAN_POINT('Ctrl Pts',(-27.7760048062591,12.3428120631862,
128.543188432493)) ;
#132387 = CARTESIAN_POINT('Ctrl Pts',(-27.880802690774,12.3473797413046,128.816094258677)) ;
#132388 = CARTESIAN_POINT('Ctrl Pts',(-27.9814814316689,12.4294695368143,
129.077065134186)) ;
#132389 = CARTESIAN_POINT('Ctrl Pts',(-28.0714598999934,12.5816148375682,
129.306949475753)) ;
#132390 = CARTESIAN_POINT('Ctrl Pts',(-28.1460628162166,12.7949907280796,
129.491697351825)) ;
#132391 = CARTESIAN_POINT('Ctrl Pts',(-28.1999915303535,13.054101177031,129.616001192498)) ;
#132392 = CARTESIAN_POINT('Ctrl Pts',(-28.2299138854955,13.3386274126212,
129.670307692816)) ;
#132393 = CARTESIAN_POINT('Ctrl Pts',(-28.2347775216737,13.6281884734652,
129.651524250556)) ;
#132394 = CARTESIAN_POINT('Ctrl Pts',(-28.2149512862949,13.9042249218154,
129.560485972219)) ;
#132395 = CARTESIAN_POINT('Ctrl Pts',(-28.1723564864184,14.1463903457502,
129.402858889307)) ;
#132396 = CARTESIAN_POINT('Ctrl Pts',(-28.1106708276455,14.3364819716926,
129.189416939951)) ;
#132397 = CARTESIAN_POINT('Ctrl Pts',(-28.0360880693673,14.4598817702337,
128.938660433378)) ;
#132398 = CARTESIAN_POINT('Ctrl Pts',(-27.953057765994,14.5104486170863,128.662863635966)) ;
#132399 = CARTESIAN_POINT('Ctrl Pts',(-27.8692045369708,14.4822486369166,
128.384729130641)) ;
#132400 = CARTESIAN_POINT('Ctrl Pts',(-27.791608538637,14.3791733041028,128.125092916574)) ;
#132401 = CARTESIAN_POINT('Ctrl Pts',(-27.7253583208721,14.2063740303146,
127.898282623416)) ;
#132402 = CARTESIAN_POINT('Ctrl Pts',(-27.6770395587882,13.9777765864427,
127.723995413382)) ;
#132403 = CARTESIAN_POINT('Ctrl Pts',(-27.6504229397667,13.7109259499415,
127.613260324166)) ;
#132404 = CARTESIAN_POINT('Ctrl Pts',(-27.6480583043497,13.4211174151953,
127.573090826099)) ;
#132405 = CARTESIAN_POINT('Ctrl Pts',(-27.6709154004622,13.1336909339448,
127.606862509643)) ;
#132406 = CARTESIAN_POINT('Ctrl Pts',(-27.7180057890291,12.8658812639418,
127.711313356748)) ;
#132407 = CARTESIAN_POINT('Ctrl Pts',(-27.7873482366324,12.6367690190525,
127.880557040248)) ;
#132408 = CARTESIAN_POINT('Ctrl Pts',(-27.8736342999947,12.4658337897599,
128.099554794345)) ;
#132409 = CARTESIAN_POINT('Ctrl Pts',(-27.9718311891268,12.3631245211514,
128.353345809671)) ;
#132410 = CARTESIAN_POINT('Ctrl Pts',(-28.0756846325717,12.3360466241608,
128.623667434511)) ;
#132411 = CARTESIAN_POINT('Ctrl Pts',(-28.1788526517052,12.3868688002356,
128.891874367728)) ;
#132412 = CARTESIAN_POINT('Ctrl Pts',(-28.2741388501772,12.5119418325269,
129.137115030646)) ;
#132413 = CARTESIAN_POINT('Ctrl Pts',(-28.3556708751438,12.7021783709845,
129.342171425122)) ;
#132414 = CARTESIAN_POINT('Ctrl Pts',(-28.4184699311589,12.9449353770794,
129.492398354652)) ;
#132415 = CARTESIAN_POINT('Ctrl Pts',(-28.4583084084869,13.2214383784226,
129.575638041553)) ;
#132416 = CARTESIAN_POINT('Ctrl Pts',(-28.4734122859081,13.5108147708277,
129.586797648768)) ;
#132417 = CARTESIAN_POINT('Ctrl Pts',(-28.4633457731125,13.7968084175674,
129.524085701258)) ;
#132418 = CARTESIAN_POINT('Ctrl Pts',(-28.4296187997626,14.0536576083437,
129.392533959943)) ;
#132419 = CARTESIAN_POINT('Ctrl Pts',(-28.3754911658076,14.2659120564335,
129.201360310375)) ;
#132420 = CARTESIAN_POINT('Ctrl Pts',(-28.3050821824441,14.4185012516542,
128.962475031458)) ;
#132421 = CARTESIAN_POINT('Ctrl Pts',(-28.2247264730961,14.4992712221482,
128.694649965742)) ;
#132422 = CARTESIAN_POINT('Ctrl Pts',(-28.1405276912772,14.5031360116066,
128.415538484686)) ;
#132423 = CARTESIAN_POINT('Ctrl Pts',(-28.059513753469,14.4296202074177,128.145783486771)) ;
#132424 = CARTESIAN_POINT('Ctrl Pts',(-27.9880766403289,14.2844131247839,
127.904026806799)) ;
#132425 = CARTESIAN_POINT('Ctrl Pts',(-27.9318057397691,14.0764755685082,
127.706412345186)) ;
#132426 = CARTESIAN_POINT('Ctrl Pts',(-27.8959845576815,13.8227947339683,
127.568706785711)) ;
#132427 = CARTESIAN_POINT('Ctrl Pts',(-27.8835201350609,13.5398702989391,
127.499142873583)) ;
#132428 = CARTESIAN_POINT('Ctrl Pts',(-27.8962033555758,13.2487717783427,
127.50306914783)) ;
#132429 = CARTESIAN_POINT('Ctrl Pts',(-27.9337544855272,12.9703362151756,
127.579661290793)) ;
#132430 = CARTESIAN_POINT('Ctrl Pts',(-27.9942820451289,12.7241092781338,
127.723348072863)) ;
#132431 = CARTESIAN_POINT('Ctrl Pts',(-28.0741961867263,12.5279171433205,
127.923656462501)) ;
#132432 = CARTESIAN_POINT('Ctrl Pts',(-28.1684346295129,12.3959938665945,
128.165822555878)) ;
#132433 = CARTESIAN_POINT('Ctrl Pts',(-28.2708930006534,12.3376260980812,
128.432033363079)) ;
#132434 = CARTESIAN_POINT('Ctrl Pts',(-28.3752372703154,12.3570497794023,
128.703694565037)) ;
#132435 = CARTESIAN_POINT('Ctrl Pts',(-28.474218780803,12.4525559733436,128.959799081295)) ;
#132436 = CARTESIAN_POINT('Ctrl Pts',(-28.5620645646479,12.6176036105847,
129.183295489253)) ;
#132437 = CARTESIAN_POINT('Ctrl Pts',(-28.6330705369593,12.8410947019102,
129.357514549927)) ;
#132438 = CARTESIAN_POINT('Ctrl Pts',(-28.6825047729054,13.1055203518464,
129.468831178845)) ;
#132439 = CARTESIAN_POINT('Ctrl Pts',(-28.7078791143123,13.3928980327512,
129.509831198009)) ;
#132440 = CARTESIAN_POINT('Ctrl Pts',(-28.7080000857972,13.6824543649216,
129.477058491295)) ;
#132441 = CARTESIAN_POINT('Ctrl Pts',(-28.6836462060832,13.9532692757644,
129.372812982897)) ;
#132442 = CARTESIAN_POINT('Ctrl Pts',(-28.637210824604,14.1862511235797,129.204032177995)) ;
#132443 = CARTESIAN_POINT('Ctrl Pts',(-28.5729983268859,14.3643962082537,
128.983404490918)) ;
#132444 = CARTESIAN_POINT('Ctrl Pts',(-28.4953888433576,14.4759024807437,
128.723329064892)) ;
#132445 = CARTESIAN_POINT('Ctrl Pts',(-28.4124155755593,14.5109062464403,
128.448017144722)) ;
#132446 = CARTESIAN_POINT('Ctrl Pts',(-28.3292183756258,14.4687351628052,
128.171836440681)) ;
#132447 = CARTESIAN_POINT('Ctrl Pts',(-28.2530232843449,14.351243796897,127.916105712843)) ;
#132448 = CARTESIAN_POINT('Ctrl Pts',(-28.19012029587,14.1681343550178,127.699312985571)) ;
#132449 = CARTESIAN_POINT('Ctrl Pts',(-28.1452447510838,13.9291093552066,
127.534840373785)) ;
#132450 = CARTESIAN_POINT('Ctrl Pts',(-28.123183101824,13.6572015399983,127.437471920795)) ;
#132451 = CARTESIAN_POINT('Ctrl Pts',(-28.1255814706017,13.3659146668707,
127.411223933066)) ;
#132452 = CARTESIAN_POINT('Ctrl Pts',(-28.1531210645832,13.0809591455927,
127.458689441797)) ;
#132453 = CARTESIAN_POINT('Ctrl Pts',(-28.2046620168687,12.8188859308948,
127.576087509683)) ;
#132454 = CARTESIAN_POINT('Ctrl Pts',(-28.277541817743,12.5999510440463,127.755745614815)) ;
#132455 = CARTESIAN_POINT('Ctrl Pts',(-28.3661476402695,12.4414984825018,
127.981641389139)) ;
#132456 = CARTESIAN_POINT('Ctrl Pts',(-28.4661327647063,12.3520343108791,
128.240572616874)) ;
#132457 = CARTESIAN_POINT('Ctrl Pts',(-28.5708059444941,12.3398054622105,
128.513131254719)) ;
#132458 = CARTESIAN_POINT('Ctrl Pts',(-28.6724777538977,12.4047865271677,
128.777144444355)) ;
#132459 = CARTESIAN_POINT('Ctrl Pts',(-28.7659001413954,12.5431933869583,
129.016844456436)) ;
#132460 = CARTESIAN_POINT('Ctrl Pts',(-28.8442058560459,12.7444965603529,
129.212472342267)) ;
#132461 = CARTESIAN_POINT('Ctrl Pts',(-28.9027924661007,12.9945025224571,
129.350476244749)) ;
#132462 = CARTESIAN_POINT('Ctrl Pts',(-28.9381575691283,13.2745329094811,
129.420727068277)) ;
#132463 = CARTESIAN_POINT('Ctrl Pts',(-28.9485234575593,13.5670626370277,
129.417726861736)) ;
#132464 = CARTESIAN_POINT('Ctrl Pts',(-28.933960447473,13.8462370772247,129.342272430857)) ;
#132465 = CARTESIAN_POINT('Ctrl Pts',(-28.8959789907869,14.0979241250953,
129.198057982517)) ;
#132466 = CARTESIAN_POINT('Ctrl Pts',(-28.838332105253,14.2997383418867,128.996585250886)) ;
#132467 = CARTESIAN_POINT('Ctrl Pts',(-28.7657725957652,14.4393312193764,
128.7515156292)) ;
#132468 = CARTESIAN_POINT('Ctrl Pts',(-28.6837573347161,14.5060643569228,
128.478659684657)) ;
#132469 = CARTESIAN_POINT('Ctrl Pts',(-28.6001080114847,14.4951758782706,
128.201352828122)) ;
#132470 = CARTESIAN_POINT('Ctrl Pts',(-28.5200653111137,14.4072623281432,
127.934287968157)) ;
#132471 = CARTESIAN_POINT('Ctrl Pts',(-28.4511978062007,14.2495039694875,
127.70007480226)) ;
#132472 = CARTESIAN_POINT('Ctrl Pts',(-28.3983753819167,14.0308221258824,
127.512458103752)) ;
#132473 = CARTESIAN_POINT('Ctrl Pts',(-28.3669487720982,13.7719100664948,
127.38779922883)) ;
#132474 = CARTESIAN_POINT('Ctrl Pts',(-28.3590881011533,13.4847456450531,
127.331550611793)) ;
#132475 = CARTESIAN_POINT('Ctrl Pts',(-28.3764285791946,13.1955425031336,
127.349219523261)) ;
#132476 = CARTESIAN_POINT('Ctrl Pts',(-28.4187558984065,12.9200552968874,
127.439556443674)) ;
#132477 = CARTESIAN_POINT('Ctrl Pts',(-28.4830536897966,12.6831184385928,
127.594396583248)) ;
#132478 = CARTESIAN_POINT('Ctrl Pts',(-28.5659931747335,12.4980281206389,
127.803559634745)) ;
#132479 = CARTESIAN_POINT('Ctrl Pts',(-28.6623364928729,12.3791543430107,
128.051854714151)) ;
#132480 = CARTESIAN_POINT('Ctrl Pts',(-28.7659162180442,12.3353503717386,
128.321248640665)) ;
#132481 = CARTESIAN_POINT('Ctrl Pts',(-28.869394759317,12.3691099621928,128.590526992868)) ;
#132482 = CARTESIAN_POINT('Ctrl Pts',(-28.9675502196224,12.4795856785055,
128.843913403417)) ;
#132483 = CARTESIAN_POINT('Ctrl Pts',(-29.0518027446978,12.6553361009926,
129.057199931773)) ;
#132484 = CARTESIAN_POINT('Ctrl Pts',(-29.1192464163454,12.8882259217544,
129.220954123798)) ;
#132485 = CARTESIAN_POINT('Ctrl Pts',(-29.1642643498932,13.1581921393272,
129.319406321897)) ;
#132486 = CARTESIAN_POINT('Ctrl Pts',(-29.1849604313943,13.4482190387101,
129.34666282445)) ;
#132487 = CARTESIAN_POINT('Ctrl Pts',(-29.1803518618151,13.7352663202425,
129.300143313471)) ;
#132488 = CARTESIAN_POINT('Ctrl Pts',(-29.1516048942262,14.0004787425337,
129.183043232165)) ;
#132489 = CARTESIAN_POINT('Ctrl Pts',(-29.1015568370635,14.2242401467777,
129.003757674716)) ;
#132490 = CARTESIAN_POINT('Ctrl Pts',(-29.0339430184054,14.391486003047,128.772934980117)) ;
#132491 = CARTESIAN_POINT('Ctrl Pts',(-28.955492652777,14.4880341837757,128.510778479589)) ;
#132492 = CARTESIAN_POINT('Ctrl Pts',(-28.8714600975796,14.5089767222778,
128.232121389573)) ;
#132493 = CARTESIAN_POINT('Ctrl Pts',(-28.7892529362311,14.4520807364783,
127.958902917957)) ;
#132494 = CARTESIAN_POINT('Ctrl Pts',(-28.7150523793816,14.3213934969356,
127.708991446956)) ;
#132495 = CARTESIAN_POINT('Ctrl Pts',(-28.6551735760367,14.126427628205,127.500952233118)) ;
#132496 = CARTESIAN_POINT('Ctrl Pts',(-28.6144873955634,13.8807880817665,
127.348935930026)) ;
#132497 = CARTESIAN_POINT('Ctrl Pts',(-28.5968038371001,13.6022566506269,
127.264117077343)) ;
#132498 = CARTESIAN_POINT('Ctrl Pts',(-28.6039330637587,13.3123739575692,
127.251951536785)) ;
#132499 = CARTESIAN_POINT('Ctrl Pts',(-28.6361660227389,13.0290004002489,
127.312956120869)) ;
#132500 = CARTESIAN_POINT('Ctrl Pts',(-28.6919510174919,12.7741270713226,
127.442792020744)) ;
#132501 = CARTESIAN_POINT('Ctrl Pts',(-28.7679989254335,12.5657352250487,
127.631815876347)) ;
#132502 = CARTESIAN_POINT('Ctrl Pts',(-28.8594997341221,12.4188762117679,
127.866013266875)) ;
#132503 = CARTESIAN_POINT('Ctrl Pts',(-28.9608147014607,12.3438128452305,
128.128841957193)) ;
#132504 = CARTESIAN_POINT('Ctrl Pts',(-29.0652267516056,12.3461025205116,
128.400746493264)) ;
#132505 = CARTESIAN_POINT('Ctrl Pts',(-29.1661640470906,12.4255735874937,
128.662467769584)) ;
#132506 = CARTESIAN_POINT('Ctrl Pts',(-29.2569746802431,12.5765456735502,
128.894620530997)) ;
#132507 = CARTESIAN_POINT('Ctrl Pts',(-29.3318567873601,12.7879286592572,
129.080274286269)) ;
#132508 = CARTESIAN_POINT('Ctrl Pts',(-29.3863322538626,13.0448054046113,
129.206302436344)) ;
#132509 = CARTESIAN_POINT('Ctrl Pts',(-29.4171885363179,13.329756321322,129.26322288733)) ;
#132510 = CARTESIAN_POINT('Ctrl Pts',(-29.4227776954555,13.6201107178654,
129.246484513251)) ;
#132511 = CARTESIAN_POINT('Ctrl Pts',(-29.4036112081965,13.8967554382586,
129.157379684264)) ;
#132512 = CARTESIAN_POINT('Ctrl Pts',(-29.3617661068054,14.1394983367384,
129.002038511481)) ;
#132513 = CARTESIAN_POINT('Ctrl Pts',(-29.3006432267773,14.3315001569242,
128.790247960104)) ;
#132514 = CARTESIAN_POINT('Ctrl Pts',(-29.2260808954585,14.4575222943013,
128.539420298087)) ;
#132515 = CARTESIAN_POINT('Ctrl Pts',(-29.1430912249785,14.5099977938908,
128.263711456409)) ;
#132516 = CARTESIAN_POINT('Ctrl Pts',(-29.0596283023754,14.4843800867397,
127.986903750172)) ;
#132517 = CARTESIAN_POINT('Ctrl Pts',(-28.9813399566608,14.3828781461486,
127.725057189875)) ;
#132518 = CARTESIAN_POINT('Ctrl Pts',(-28.9150542416882,14.212816168216,127.498335145429)) ;
#132519 = CARTESIAN_POINT('Ctrl Pts',(-28.8659433323491,13.9854781681749,
127.321666885816)) ;
#132520 = CARTESIAN_POINT('Ctrl Pts',(-28.8385949971052,13.7179644909653,
127.2086184725)) ;
#132521 = CARTESIAN_POINT('Ctrl Pts',(-28.835583635112,13.4301920376034,127.166758116441)) ;
#132522 = CARTESIAN_POINT('Ctrl Pts',(-28.8575789748189,13.1421055633853,
127.197981715462)) ;
#132523 = CARTESIAN_POINT('Ctrl Pts',(-28.9045188244626,12.87150128464,127.301728733917)) ;
#132524 = CARTESIAN_POINT('Ctrl Pts',(-28.9725684665303,12.6436097991943,
127.46756519262)) ;
#132525 = CARTESIAN_POINT('Ctrl Pts',(-29.0586604842472,12.4698498437503,
127.68586545448)) ;
#132526 = CARTESIAN_POINT('Ctrl Pts',(-29.1565931939368,12.3651221856613,
127.938894371706)) ;
#132527 = CARTESIAN_POINT('Ctrl Pts',(-29.2604850351592,12.335692224637,128.209290972507)) ;
#132528 = CARTESIAN_POINT('Ctrl Pts',(-29.3638355952977,12.3844432071478,
128.478011145159)) ;
#132529 = CARTESIAN_POINT('Ctrl Pts',(-29.4592358664342,12.5072147901112,
128.723652752499)) ;
#132530 = CARTESIAN_POINT('Ctrl Pts',(-29.5413221888135,12.6957550150873,
128.930308953615)) ;
#132531 = CARTESIAN_POINT('Ctrl Pts',(-29.6047036187767,12.9372999479051,
129.082233550744)) ;
#132532 = CARTESIAN_POINT('Ctrl Pts',(-29.6452182047899,13.2121499543988,
129.167553115)) ;
#132533 = CARTESIAN_POINT('Ctrl Pts',(-29.6611042764023,13.5032465104466,
129.180780924663)) ;
#132534 = CARTESIAN_POINT('Ctrl Pts',(-29.6518819161121,13.7871080328991,
129.120848156331)) ;
#132535 = CARTESIAN_POINT('Ctrl Pts',(-29.6187108954398,14.0469104745439,
128.990694231868)) ;
#132536 = CARTESIAN_POINT('Ctrl Pts',(-29.5650955851099,14.2605649124229,
128.801033137001)) ;
#132537 = CARTESIAN_POINT('Ctrl Pts',(-29.494870755953,14.4153649488043,128.562594916595)) ;
#132538 = CARTESIAN_POINT('Ctrl Pts',(-29.4150387131859,14.4978582783663,
128.296438099207)) ;
#132539 = CARTESIAN_POINT('Ctrl Pts',(-29.3308499416307,14.5041773990225,
128.017349602118)) ;
#132540 = CARTESIAN_POINT('Ctrl Pts',(-29.2496148451093,14.4329779197685,
127.746941843894)) ;
#132541 = CARTESIAN_POINT('Ctrl Pts',(-29.1775262666222,14.2890422314917,
127.503142142852)) ;
#132542 = CARTESIAN_POINT('Ctrl Pts',(-29.1208969337368,14.082779433517,127.304531079944)) ;
#132543 = CARTESIAN_POINT('Ctrl Pts',(-29.0845225826136,13.8309337098099,
127.165299579887)) ;
#132544 = CARTESIAN_POINT('Ctrl Pts',(-29.0713186329842,13.5483120187831,
127.093542785031)) ;
#132545 = CARTESIAN_POINT('Ctrl Pts',(-29.083229857648,13.2574777531019,127.095253063998)) ;
#132546 = CARTESIAN_POINT('Ctrl Pts',(-29.1201441678816,12.9779697529959,
127.169929814834)) ;
#132547 = CARTESIAN_POINT('Ctrl Pts',(-29.1798340071233,12.7311580251373,
127.311268080156)) ;
#132548 = CARTESIAN_POINT('Ctrl Pts',(-29.259615046753,12.5323980592304,127.511032300878)) ;
#132549 = CARTESIAN_POINT('Ctrl Pts',(-29.3531954363121,12.3989897288854,
127.751398360947)) ;
#132550 = CARTESIAN_POINT('Ctrl Pts',(-29.4557047728638,12.3382487603058,
128.017686516644)) ;
#132551 = CARTESIAN_POINT('Ctrl Pts',(-29.5597398015999,12.3552058083452,
128.288561847953)) ;
#132552 = CARTESIAN_POINT('Ctrl Pts',(-29.6596151268484,12.4490680703867,
128.547063275398)) ;
#132553 = CARTESIAN_POINT('Ctrl Pts',(-29.747823539621,12.612854304799,128.771597225379)) ;
#132554 = CARTESIAN_POINT('Ctrl Pts',(-29.8189230473542,12.8333918295054,
128.946308444558)) ;
#132555 = CARTESIAN_POINT('Ctrl Pts',(-29.8692193933531,13.0975419155814,
129.060046052025)) ;
#132556 = CARTESIAN_POINT('Ctrl Pts',(-29.8952825556904,13.3843701567211,
129.103082744144)) ;
#132557 = CARTESIAN_POINT('Ctrl Pts',(-29.8961296754756,13.6749248626015,
129.072344167559)) ;
#132558 = CARTESIAN_POINT('Ctrl Pts',(-29.872352875635,13.9463602578246,128.969789222471)) ;
#132559 = CARTESIAN_POINT('Ctrl Pts',(-29.8267467901644,14.1798324379302,
128.803574285622)) ;
#132560 = CARTESIAN_POINT('Ctrl Pts',(-29.762567848699,14.3606302769089,128.582842462436)) ;
#132561 = CARTESIAN_POINT('Ctrl Pts',(-29.6859295100925,14.4733618864566,
128.325903972762)) ;
#132562 = CARTESIAN_POINT('Ctrl Pts',(-29.6022723165312,14.5110756600993,
128.048275924638)) ;
#132563 = CARTESIAN_POINT('Ctrl Pts',(-29.5194444158079,14.4709889009811,
127.773361424165)) ;
#132564 = CARTESIAN_POINT('Ctrl Pts',(-29.4427850873383,14.3556941984043,
127.516218240476)) ;
#132565 = CARTESIAN_POINT('Ctrl Pts',(-29.379260435332,14.1731666486328,127.297467610204)) ;
#132566 = CARTESIAN_POINT('Ctrl Pts',(-29.3342254132114,13.9378584167298,
127.132862710005)) ;
#132567 = CARTESIAN_POINT('Ctrl Pts',(-29.3112446912435,13.6656355311939,
127.03265253494)) ;
#132568 = CARTESIAN_POINT('Ctrl Pts',(-29.3129312287784,13.3744563081115,
127.004322113587)) ;
#132569 = CARTESIAN_POINT('Ctrl Pts',(-29.3398177129572,13.0885611803192,
127.049815834232)) ;
#132570 = CARTESIAN_POINT('Ctrl Pts',(-29.3906009924672,12.8263306498725,
127.165093753781)) ;
#132571 = CARTESIAN_POINT('Ctrl Pts',(-29.4625594349018,12.6063807769631,
127.342179164998)) ;
#132572 = CARTESIAN_POINT('Ctrl Pts',(-29.5513814104012,12.4447492933123,
127.568465791526)) ;
#132573 = CARTESIAN_POINT('Ctrl Pts',(-29.6511504516607,12.3535025882306,
127.826777567947)) ;
#132574 = CARTESIAN_POINT('Ctrl Pts',(-29.7556083087904,12.3391045054194,
128.098761532225)) ;
#132575 = CARTESIAN_POINT('Ctrl Pts',(-29.8574615889439,12.4018104241151,
128.363303066571)) ;
#132576 = CARTESIAN_POINT('Ctrl Pts',(-29.9515240336887,12.5389586489687,
128.604752086664)) ;
#132577 = CARTESIAN_POINT('Ctrl Pts',(-30.0298895040687,12.7377764458565,
128.800721216607)) ;
#132578 = CARTESIAN_POINT('Ctrl Pts',(-30.0891318078393,12.9863019722805,
128.940662639121)) ;
#132579 = CARTESIAN_POINT('Ctrl Pts',(-30.1252471064463,13.2660338630659,
129.013066477495)) ;
#132580 = CARTESIAN_POINT('Ctrl Pts',(-30.1363860269831,13.5582232268191,
129.012365283493)) ;
#132581 = CARTESIAN_POINT('Ctrl Pts',(-30.1224573425596,13.8387404070693,
128.9386660175)) ;
#132582 = CARTESIAN_POINT('Ctrl Pts',(-30.0853429984546,14.0904925183414,
128.797147021732)) ;
#132583 = CARTESIAN_POINT('Ctrl Pts',(-30.0277590711992,14.2955136011611,
128.595595560232)) ;
#132584 = CARTESIAN_POINT('Ctrl Pts',(-29.9558778598522,14.4360006812449,
128.352686763533)) ;
#132585 = CARTESIAN_POINT('Ctrl Pts',(-29.8742567679805,14.5051702931602,
128.081056456965)) ;
#132586 = CARTESIAN_POINT('Ctrl Pts',(-29.7902969630137,14.4966323764384,
127.802731519334)) ;
#132587 = CARTESIAN_POINT('Ctrl Pts',(-29.7100123387406,14.4108291399258,
127.534953213959)) ;
#132588 = CARTESIAN_POINT('Ctrl Pts',(-29.6407380446541,14.2547209501546,
127.299525468516)) ;
#132589 = CARTESIAN_POINT('Ctrl Pts',(-29.5875888674703,14.0388606089928,
127.111132269111)) ;
#132590 = CARTESIAN_POINT('Ctrl Pts',(-29.5552494813085,13.779405578044,126.983595808789)) ;
#132591 = CARTESIAN_POINT('Ctrl Pts',(-29.5467692399988,13.4926641580088,
126.925547219345)) ;
#132592 = CARTESIAN_POINT('Ctrl Pts',(-29.5633816541989,13.2038302112353,
126.941144586643)) ;
#132593 = CARTESIAN_POINT('Ctrl Pts',(-29.6048714410533,12.9280759931688,
127.02910382322)) ;
#132594 = CARTESIAN_POINT('Ctrl Pts',(-29.6688506403303,12.6887447492448,
127.182864366148)) ;
#132595 = CARTESIAN_POINT('Ctrl Pts',(-29.7513587249347,12.5022966343227,
127.39078364992)) ;
#132596 = CARTESIAN_POINT('Ctrl Pts',(-29.8469802454942,12.381763978882,127.637108683278)) ;
#132597 = CARTESIAN_POINT('Ctrl Pts',(-29.9508020024135,12.3354318114705,
127.907094928409)) ;
#132598 = CARTESIAN_POINT('Ctrl Pts',(-30.0541803012317,12.3672035513488,
128.176131637916)) ;
#132599 = CARTESIAN_POINT('Ctrl Pts',(-30.1521106585629,12.474426481286,128.429055203006)) ;
#132600 = CARTESIAN_POINT('Ctrl Pts',(-30.2377865470727,12.6503068829769,
128.646124078682)) ;
#132601 = CARTESIAN_POINT('Ctrl Pts',(-30.3053907898611,12.8812481424524,
128.810483543534)) ;
#132602 = CARTESIAN_POINT('Ctrl Pts',(-30.3510328505262,13.1494231082653,
128.910858646302)) ;
#132603 = CARTESIAN_POINT('Ctrl Pts',(-30.3725424728725,13.4405328283774,
128.94033906329)) ;
#132604 = CARTESIAN_POINT('Ctrl Pts',(-30.3685945252647,13.7272524095848,
128.895825068985)) ;
#132605 = CARTESIAN_POINT('Ctrl Pts',(-30.3405359677795,13.9933197786215,
128.780743464257)) ;
#132606 = CARTESIAN_POINT('Ctrl Pts',(-30.2910888155488,14.2183989061991,
128.603235194175)) ;
#132607 = CARTESIAN_POINT('Ctrl Pts',(-30.2238484293931,14.3876287517767,
128.373477627282)) ;
#132608 = CARTESIAN_POINT('Ctrl Pts',(-30.1457515284424,14.4861870970875,
128.112398717919)) ;
#132609 = CARTESIAN_POINT('Ctrl Pts',(-30.0617136501863,14.5095212297327,
127.833700802789)) ;
#132610 = CARTESIAN_POINT('Ctrl Pts',(-29.9792786676799,14.4547287275128,
127.559780909732)) ;
#132611 = CARTESIAN_POINT('Ctrl Pts',(-29.9048009680584,14.3261105544631,
127.309079981945)) ;
#132612 = CARTESIAN_POINT('Ctrl Pts',(-29.844419395189,14.1327425032557,127.099559452458)) ;
#132613 = CARTESIAN_POINT('Ctrl Pts',(-29.803152525388,13.8885306001009,126.945876263857)) ;
#132614 = CARTESIAN_POINT('Ctrl Pts',(-29.7847767393562,13.6107524410049,
126.859040355574)) ;
#132615 = CARTESIAN_POINT('Ctrl Pts',(-29.7910854802672,13.3210542583331,
126.844495484992)) ;
#132616 = CARTESIAN_POINT('Ctrl Pts',(-29.8229753868191,13.0351251235983,
126.904244014759)) ;
#132617 = CARTESIAN_POINT('Ctrl Pts',(-29.8776744286432,12.7816150209491,
127.031216029816)) ;
#132618 = CARTESIAN_POINT('Ctrl Pts',(-29.9534311716552,12.5706518061014,
127.219253692065)) ;
#132619 = CARTESIAN_POINT('Ctrl Pts',(-30.0445412838822,12.422091900903,127.452333377032)) ;
#132620 = CARTESIAN_POINT('Ctrl Pts',(-30.1457887502779,12.3448083833829,
127.714923612566)) ;
#132621 = CARTESIAN_POINT('Ctrl Pts',(-30.250148655895,12.3450375607664,127.986693881587)) ;
#132622 = CARTESIAN_POINT('Ctrl Pts',(-30.3511170822601,12.4222140372622,
128.248559607977)) ;
#132623 = CARTESIAN_POINT('Ctrl Pts',(-30.4423550067095,12.5713072693593,
128.481942746401)) ;
#132624 = CARTESIAN_POINT('Ctrl Pts',(-30.5177968325665,12.7812068465324,
128.669220610782)) ;
#132625 = CARTESIAN_POINT('Ctrl Pts',(-30.5730322088188,13.0378486801572,
128.797371634622)) ;
#132626 = CARTESIAN_POINT('Ctrl Pts',(-30.6044543099339,13.3220972424203,
128.855977004469)) ;
#132627 = CARTESIAN_POINT('Ctrl Pts',(-30.6107589621473,13.6116477161832,
128.841431739069)) ;
#132628 = CARTESIAN_POINT('Ctrl Pts',(-30.5922328646922,13.8896343949454,
128.754117840507)) ;
#132629 = CARTESIAN_POINT('Ctrl Pts',(-30.5510661396947,14.1329048293709,
128.60084368254)) ;
#132630 = CARTESIAN_POINT('Ctrl Pts',(-30.4905361238725,14.3266157424045,
128.390815616408)) ;
#132631 = CARTESIAN_POINT('Ctrl Pts',(-30.4160368539188,14.4550271923226,
128.140061981301)) ;
#132632 = CARTESIAN_POINT('Ctrl Pts',(-30.333450058965,14.5094869156272,127.865640071397)) ;
#132633 = CARTESIAN_POINT('Ctrl Pts',(-30.2498814405861,14.4863255111229,
127.588507289986)) ;
#132634 = CARTESIAN_POINT('Ctrl Pts',(-30.1712461824057,14.3868080890416,
127.325605825376)) ;
#132635 = CARTESIAN_POINT('Ctrl Pts',(-30.1044933380963,14.2186053771164,
127.097513189475)) ;
#132636 = CARTESIAN_POINT('Ctrl Pts',(-30.0547280039428,13.9916146831158,
126.918804037804)) ;
#132637 = CARTESIAN_POINT('Ctrl Pts',(-30.0268955041398,13.727139474133,126.804607454992)) ;
#132638 = CARTESIAN_POINT('Ctrl Pts',(-30.0231159202939,13.437362164295,126.760227532608)) ;
#132639 = CARTESIAN_POINT('Ctrl Pts',(-30.0443922432487,13.1504054531947,
126.789513820971)) ;
#132640 = CARTESIAN_POINT('Ctrl Pts',(-30.0906616171445,12.8786465021209,
126.89126693415)) ;
#132641 = CARTESIAN_POINT('Ctrl Pts',(-30.157970236125,12.6500332814425,127.055027994723)) ;
#132642 = CARTESIAN_POINT('Ctrl Pts',(-30.2434337782595,12.4743183897028,
127.271533917434)) ;
#132643 = CARTESIAN_POINT('Ctrl Pts',(-30.3417585829433,12.3668547922141,
127.525488336301)) ;
#132644 = CARTESIAN_POINT('Ctrl Pts',(-30.4450821005495,12.335562941567,127.79438563983)) ;
#132645 = CARTESIAN_POINT('Ctrl Pts',(-30.5484944936694,12.3817108072099,
128.063306891139)) ;
#132646 = CARTESIAN_POINT('Ctrl Pts',(-30.6445980415539,12.502839824897,128.310875860644)) ;
#132647 = CARTESIAN_POINT('Ctrl Pts',(-30.7271978616452,12.690351441453,128.518969835721)) ;
#132648 = CARTESIAN_POINT('Ctrl Pts',(-30.7907079505213,12.9285059391321,
128.671549365572)) ;
#132649 = CARTESIAN_POINT('Ctrl Pts',(-30.832295267727,13.2046731907038,128.75974213921)) ;
#132650 = CARTESIAN_POINT('Ctrl Pts',(-30.8487758407748,13.4951333113011,
128.774772845728)) ;
#132651 = CARTESIAN_POINT('Ctrl Pts',(-30.8402346447153,13.779501210584,128.716814376005)) ;
#132652 = CARTESIAN_POINT('Ctrl Pts',(-30.8078637040687,14.0394108332529,
128.589125311067)) ;
#132653 = CARTESIAN_POINT('Ctrl Pts',(-30.7546552751125,14.2552141196343,
128.400557285253)) ;
#132654 = CARTESIAN_POINT('Ctrl Pts',(-30.6851696086428,14.4112842226695,
128.164437543065)) ;
#132655 = CARTESIAN_POINT('Ctrl Pts',(-30.6053419982904,14.49663037618,127.89819080895)) ;
#132656 = CARTESIAN_POINT('Ctrl Pts',(-30.520751800545,14.5049768783044,127.617767628039)) ;
#132657 = CARTESIAN_POINT('Ctrl Pts',(-30.4397470692586,14.4360835729073,
127.348190225217)) ;
#132658 = CARTESIAN_POINT('Ctrl Pts',(-30.3673932451776,14.2946513922982,
127.103676961857)) ;
#132659 = CARTESIAN_POINT('Ctrl Pts',(-30.3101336108046,14.0899140100411,
126.903186984993)) ;
#132660 = CARTESIAN_POINT('Ctrl Pts',(-30.2730059348416,13.8386917046902,
126.761684342598)) ;
#132661 = CARTESIAN_POINT('Ctrl Pts',(-30.2591454609719,13.5555692125345,
126.687892009024)) ;
#132662 = CARTESIAN_POINT('Ctrl Pts',(-30.2703044262027,13.2663901180779,
126.687596604313)) ;
#132663 = CARTESIAN_POINT('Ctrl Pts',(-30.3064563015578,12.9858847333076,
126.760012223785)) ;
#132664 = CARTESIAN_POINT('Ctrl Pts',(-30.3656808780386,12.7375102459871,
126.899927974495)) ;
#132665 = CARTESIAN_POINT('Ctrl Pts',(-30.4446592433479,12.5376376287816,
127.097461701573)) ;
#132666 = CARTESIAN_POINT('Ctrl Pts',(-30.5383897496922,12.4015826977934,
127.338092518212)) ;
#132667 = CARTESIAN_POINT('Ctrl Pts',(-30.6402554773558,12.3390360902595,
127.602664560348)) ;
#132668 = CARTESIAN_POINT('Ctrl Pts',(-30.7445603425615,12.353575403094,127.874253187337)) ;
#132669 = CARTESIAN_POINT('Ctrl Pts',(-30.8445423217259,12.445274073871,128.133104829671)) ;
#132670 = CARTESIAN_POINT('Ctrl Pts',(-30.9331533396269,12.6067971683827,
128.358841764631)) ;
#132671 = CARTESIAN_POINT('Ctrl Pts',(-31.0052235518519,12.8274892534517,
128.536166471027)) ;
#132672 = CARTESIAN_POINT('Ctrl Pts',(-31.0557929024469,13.0891408927057,
128.650910668167)) ;
#132673 = CARTESIAN_POINT('Ctrl Pts',(-31.0826649707566,13.375740122579,128.696283133412)) ;
#132674 = CARTESIAN_POINT('Ctrl Pts',(-31.0842457464183,13.6659116032671,
128.667755109105)) ;
#132675 = CARTESIAN_POINT('Ctrl Pts',(-31.0612969342213,13.9383430672958,
128.567621981036)) ;
#132676 = CARTESIAN_POINT('Ctrl Pts',(-31.0158421470532,14.1747318786697,
128.401589927848)) ;
#132677 = CARTESIAN_POINT('Ctrl Pts',(-30.952741170991,14.3556000224366,128.184334680318)) ;
#132678 = CARTESIAN_POINT('Ctrl Pts',(-30.8757148543573,14.4715471852787,
127.925954832144)) ;
#132679 = CARTESIAN_POINT('Ctrl Pts',(-30.7926989079768,14.5109306884899,
127.650429154449)) ;
#132680 = CARTESIAN_POINT('Ctrl Pts',(-30.7096170404131,14.4734197510009,
127.374712802353)) ;
#132681 = CARTESIAN_POINT('Ctrl Pts',(-30.6324207964218,14.3595613312843,
127.115883659408)) ;
#132682 = CARTESIAN_POINT('Ctrl Pts',(-30.5687431637558,14.179466171533,126.896825275717)) ;
#132683 = CARTESIAN_POINT('Ctrl Pts',(-30.5229949276125,13.9455181185487,
126.730115674649)) ;
#132684 = CARTESIAN_POINT('Ctrl Pts',(-30.4993062024708,13.6723045745694,
126.627634301698)) ;
#132685 = CARTESIAN_POINT('Ctrl Pts',(-30.5003214317798,13.3834915874396,
126.597593551244)) ;
#132686 = CARTESIAN_POINT('Ctrl Pts',(-30.5264493139276,13.0966134068724,
126.640803917263)) ;
#132687 = CARTESIAN_POINT('Ctrl Pts',(-30.5766713219404,12.8330521051259,
126.754396922064)) ;
#132688 = CARTESIAN_POINT('Ctrl Pts',(-30.6483002280116,12.6112324338377,
126.930439181463)) ;
#132689 = CARTESIAN_POINT('Ctrl Pts',(-30.736661695068,12.4482429025448,127.155425447181)) ;
#132690 = CARTESIAN_POINT('Ctrl Pts',(-30.8357315528907,12.3553252392396,
127.411846833704)) ;
#132691 = CARTESIAN_POINT('Ctrl Pts',(-30.9400335857783,12.3382107107946,
127.683413725756)) ;
#132692 = CARTESIAN_POINT('Ctrl Pts',(-31.042636248853,12.3992481458877,127.94994445052)) ;
#132693 = CARTESIAN_POINT('Ctrl Pts',(-31.1362393771601,12.5331204758664,
128.190343537901)) ;
#132694 = CARTESIAN_POINT('Ctrl Pts',(-31.215635139957,12.7309387918669,128.389145202128)) ;
#132695 = CARTESIAN_POINT('Ctrl Pts',(-31.2756357249041,12.9791524410526,
128.53120468286)) ;
#132696 = CARTESIAN_POINT('Ctrl Pts',(-31.312400854353,13.2585790598106,128.605475928875)) ;
#132697 = CARTESIAN_POINT('Ctrl Pts',(-31.3241836080649,13.5499397896395,
128.606744173026)) ;
#132698 = CARTESIAN_POINT('Ctrl Pts',(-31.3110087346716,13.8311712407388,
128.535239748079)) ;
#132699 = CARTESIAN_POINT('Ctrl Pts',(-31.2742363093329,14.0848085651835,
128.394579152518)) ;
#132700 = CARTESIAN_POINT('Ctrl Pts',(-31.2178679894401,14.2892041446737,
128.196968022278)) ;
#132701 = CARTESIAN_POINT('Ctrl Pts',(-31.1457920021485,14.4332159069687,
127.953199131549)) ;
#132702 = CARTESIAN_POINT('Ctrl Pts',(-31.064501704361,14.5042073782218,127.682616508337)) ;
#132703 = CARTESIAN_POINT('Ctrl Pts',(-30.9803569070733,14.4978850554144,
127.403677198383)) ;
#132704 = CARTESIAN_POINT('Ctrl Pts',(-30.9001457048563,14.4145534025925,
127.136236709374)) ;
#132705 = CARTESIAN_POINT('Ctrl Pts',(-30.8302915857101,14.2600830965558,
126.899030948309)) ;
#132706 = CARTESIAN_POINT('Ctrl Pts',(-30.7766783037662,14.0459659620245,
126.70932486434)) ;
#132707 = CARTESIAN_POINT('Ctrl Pts',(-30.7436688177568,13.7875807752627,
126.579828846178)) ;
#132708 = CARTESIAN_POINT('Ctrl Pts',(-30.7344309347098,13.5015008973902,
126.519590640979)) ;
#132709 = CARTESIAN_POINT('Ctrl Pts',(-30.7503570117774,13.2119712102584,
126.533117195425)) ;
#132710 = CARTESIAN_POINT('Ctrl Pts',(-30.7909948356034,12.9363053782512,
126.618694908227)) ;
#132711 = CARTESIAN_POINT('Ctrl Pts',(-30.8544313460082,12.6952736602129,
126.770815078882)) ;
#132712 = CARTESIAN_POINT('Ctrl Pts',(-30.936259477995,12.507125678723,126.976810991267)) ;
#132713 = CARTESIAN_POINT('Ctrl Pts',(-31.0324849838793,12.3837628513247,
127.224594411425)) ;
#132714 = CARTESIAN_POINT('Ctrl Pts',(-31.1350680188049,12.3357954087756,
127.491330342941)) ;
#132715 = CARTESIAN_POINT('Ctrl Pts',(-31.23935127795,12.3652711251859,127.762742575844)) ;
#132716 = CARTESIAN_POINT('Ctrl Pts',(-31.3372466101365,12.4705156806676,
128.015655972246)) ;
#132717 = CARTESIAN_POINT('Ctrl Pts',(-31.4231098978925,12.6439184973371,
128.233370607722)) ;
#132718 = CARTESIAN_POINT('Ctrl Pts',(-31.4913656157794,12.8730354055636,
128.399662361953)) ;
#132719 = CARTESIAN_POINT('Ctrl Pts',(-31.5379531663441,13.1424159445997,
128.502550794473)) ;
#132720 = CARTESIAN_POINT('Ctrl Pts',(-31.5599892196137,13.4306391754528,
128.533873702179)) ;
#132721 = CARTESIAN_POINT('Ctrl Pts',(-31.5568791607716,13.7191539441457,
128.491638388163)) ;
#132722 = CARTESIAN_POINT('Ctrl Pts',(-31.5294551877072,13.9861293896989,
128.378414253767)) ;
#132723 = CARTESIAN_POINT('Ctrl Pts',(-31.4804720297221,14.2128684001206,
128.202207341774)) ;
#132724 = CARTESIAN_POINT('Ctrl Pts',(-31.4139631417804,14.3833347965248,
127.974731570058)) ;
#132725 = CARTESIAN_POINT('Ctrl Pts',(-31.3357239804157,14.4845639099252,
127.713064266216)) ;
#132726 = CARTESIAN_POINT('Ctrl Pts',(-31.2519760904658,14.5099092471542,
127.435310311413)) ;
#132727 = CARTESIAN_POINT('Ctrl Pts',(-31.169269063561,14.4573341215463,127.160540128222)) ;
#132728 = CARTESIAN_POINT('Ctrl Pts',(-31.0944827944426,14.3305258270945,
126.908931141692)) ;
#132729 = CARTESIAN_POINT('Ctrl Pts',(-31.0337818947545,14.1393930806654,
126.698567894651)) ;
#132730 = CARTESIAN_POINT('Ctrl Pts',(-30.991822622221,13.8963012865058,126.542832684996)) ;
#132731 = CARTESIAN_POINT('Ctrl Pts',(-30.9727169093987,13.618527952916,126.453788104164)) ;
#132732 = CARTESIAN_POINT('Ctrl Pts',(-30.9784116943508,13.3290638567204,
126.43746201239)) ;
#132733 = CARTESIAN_POINT('Ctrl Pts',(-31.0092534744897,13.0445549081066,
126.494384804869)) ;
#132734 = CARTESIAN_POINT('Ctrl Pts',(-31.0636975928906,12.7876683953407,
126.620329890945)) ;
#132735 = CARTESIAN_POINT('Ctrl Pts',(-31.1390893626737,12.5753843248543,
126.807286162987)) ;
#132736 = CARTESIAN_POINT('Ctrl Pts',(-31.2294856731981,12.4255194566962,
127.038405016624)) ;
#132737 = CARTESIAN_POINT('Ctrl Pts',(-31.3305520361071,12.3459765628223,
127.300458413669)) ;
#132738 = CARTESIAN_POINT('Ctrl Pts',(-31.434776599086,12.3439073333341,127.571874828474)) ;
#132739 = CARTESIAN_POINT('Ctrl Pts',(-31.5361216061782,12.4188279963137,
127.834788869403)) ;
#132740 = CARTESIAN_POINT('Ctrl Pts',(-31.6280697762185,12.5669347456838,
128.070100154879)) ;
#132741 = CARTESIAN_POINT('Ctrl Pts',(-31.7035334984892,12.7740276750078,
128.257653591068)) ;
#132742 = CARTESIAN_POINT('Ctrl Pts',(-31.759609829367,13.0302839963835,128.388157305165)) ;
#132743 = CARTESIAN_POINT('Ctrl Pts',(-31.7916573927032,13.3133908418281,
128.44867020828)) ;
#132744 = CARTESIAN_POINT('Ctrl Pts',(-31.7986966116337,13.603463644202,128.436213818987)) ;
#132745 = CARTESIAN_POINT('Ctrl Pts',(-31.7809913371395,13.8813033828735,
128.35140974243)) ;
#132746 = CARTESIAN_POINT('Ctrl Pts',(-31.7400851389627,14.1277803353935,
128.198621302036)) ;
#132747 = CARTESIAN_POINT('Ctrl Pts',(-31.6800730695565,14.3222499491186,
127.990196055143)) ;
#132748 = CARTESIAN_POINT('Ctrl Pts',(-31.6061655491007,14.4521801137134,
127.741284607191)) ;
#132749 = CARTESIAN_POINT('Ctrl Pts',(-31.5238300942761,14.5090397013049,
127.467639877269)) ;
#132750 = CARTESIAN_POINT('Ctrl Pts',(-31.4398666707468,14.4879536383768,
127.189213876511)) ;
#132751 = CARTESIAN_POINT('Ctrl Pts',(-31.3611027665607,14.3907169193799,
126.925998091316)) ;
#132752 = CARTESIAN_POINT('Ctrl Pts',(-31.2937040056646,14.2230874926912,
126.695841876849)) ;
#132753 = CARTESIAN_POINT('Ctrl Pts',(-31.2439920013192,14.0008521290395,
126.517762290878)) ;
#132754 = CARTESIAN_POINT('Ctrl Pts',(-31.2150907661555,13.7343152663338,
126.400042595703)) ;
#132755 = CARTESIAN_POINT('Ctrl Pts',(-31.2106083276963,13.4474451530714,
126.353922032443)) ;
#132756 = CARTESIAN_POINT('Ctrl Pts',(-31.2313383311631,13.1575373599845,
126.381288702569)) ;
#132757 = CARTESIAN_POINT('Ctrl Pts',(-31.2764056532061,12.8878586186382,
126.479905180231)) ;
#132758 = CARTESIAN_POINT('Ctrl Pts',(-31.3436059924202,12.6555337160297,
126.643048484565)) ;
#132759 = CARTESIAN_POINT('Ctrl Pts',(-31.4286039772841,12.4784852863875,
126.858237182344)) ;
#132760 = CARTESIAN_POINT('Ctrl Pts',(-31.5266156330296,12.3688435126028,
127.11128245237)) ;
#132761 = CARTESIAN_POINT('Ctrl Pts',(-31.630084559127,12.335379050582,127.380536177025)) ;
#132762 = CARTESIAN_POINT('Ctrl Pts',(-31.7333993373061,12.3794309050292,
127.649233966248)) ;
#132763 = CARTESIAN_POINT('Ctrl Pts',(-31.8295546512421,12.4979553005814,
127.897051153347)) ;
#132764 = CARTESIAN_POINT('Ctrl Pts',(-31.9129345986958,12.6843641512771,
128.107301604166)) ;
#132765 = CARTESIAN_POINT('Ctrl Pts',(-31.9769081760024,12.9208195190715,
128.261300839291)) ;
#132766 = CARTESIAN_POINT('Ctrl Pts',(-32.0192234596835,13.1965599156971,
128.351576775379)) ;
#132767 = CARTESIAN_POINT('Ctrl Pts',(-32.0364080377691,13.4854150034454,
128.36882968244)) ;
#132768 = CARTESIAN_POINT('Ctrl Pts',(-32.0286590942519,13.7715245103546,
128.313041033143)) ;
#132769 = CARTESIAN_POINT('Ctrl Pts',(-31.9967949405779,14.0329603333754,
128.186757372476)) ;
#132770 = CARTESIAN_POINT('Ctrl Pts',(-31.9442598511563,14.2495174070446,
128.000252912401)) ;
#132771 = CARTESIAN_POINT('Ctrl Pts',(-31.8752637456382,14.4077221355952,
127.765584521541)) ;
#132772 = CARTESIAN_POINT('Ctrl Pts',(-31.7949904880439,14.4954974794661,
127.497773147365)) ;
#132773 = CARTESIAN_POINT('Ctrl Pts',(-31.7112118667338,14.5058124227374,
127.220036909701)) ;
#132774 = CARTESIAN_POINT('Ctrl Pts',(-31.6295895835472,14.4390540160987,
126.948477953836)) ;
#132775 = CARTESIAN_POINT('Ctrl Pts',(-31.5567958768622,14.2988995016989,
126.702614005723)) ;
#132776 = CARTESIAN_POINT('Ctrl Pts',(-31.4992152164798,14.0959846822767,
126.501253268444)) ;
#132777 = CARTESIAN_POINT('Ctrl Pts',(-31.4616155663629,13.8467238077785,
126.358483470145)) ;
#132778 = CARTESIAN_POINT('Ctrl Pts',(-31.4469797675735,13.5651499595772,
126.282529118317)) ;
#132779 = CARTESIAN_POINT('Ctrl Pts',(-31.4573898379876,13.2745210705863,
126.279884269193)) ;
#132780 = CARTESIAN_POINT('Ctrl Pts',(-31.4929777781403,12.9930481847516,
126.350603500459)) ;
#132781 = CARTESIAN_POINT('Ctrl Pts',(-31.5514293278227,12.7442685275202,
126.488355718607)) ;
#132782 = CARTESIAN_POINT('Ctrl Pts',(-31.629789771733,12.5428869624623,126.684118709821)) ;
#132783 = CARTESIAN_POINT('Ctrl Pts',(-31.7230911251259,12.4047083280592,
126.923514916853)) ;
#132784 = CARTESIAN_POINT('Ctrl Pts',(-31.8251196709966,12.3396945526809,
127.188456991403)) ;
#132785 = CARTESIAN_POINT('Ctrl Pts',(-31.9293847768492,12.3521469576885,
127.459951466802)) ;
#132786 = CARTESIAN_POINT('Ctrl Pts',(-32.0293584096416,12.441314353945,127.718862688757)) ;
#132787 = CARTESIAN_POINT('Ctrl Pts',(-32.118508034267,12.6011043288198,127.946125196227)) ;
#132788 = CARTESIAN_POINT('Ctrl Pts',(-32.1909463624357,12.8194224397463,
128.124637671274)) ;
#132789 = CARTESIAN_POINT('Ctrl Pts',(-32.2424853469496,13.0811434342732,
128.242065843194)) ;
#132790 = CARTESIAN_POINT('Ctrl Pts',(-32.2700475124695,13.3679217852881,
128.289393931887)) ;
#132791 = CARTESIAN_POINT('Ctrl Pts',(-32.2723234688677,13.6574454003315,
128.262990706036)) ;
#132792 = CARTESIAN_POINT('Ctrl Pts',(-32.2501377563472,13.9304218890574,
128.16512094437)) ;
#132793 = CARTESIAN_POINT('Ctrl Pts',(-32.2052527136117,14.1686008595605,
128.000705406738)) ;
#132794 = CARTESIAN_POINT('Ctrl Pts',(-32.1424368825761,14.3514046814191,
127.78421431945)) ;
#132795 = CARTESIAN_POINT('Ctrl Pts',(-32.0661890017219,14.4688537010489,
127.528311842842)) ;
#132796 = CARTESIAN_POINT('Ctrl Pts',(-31.9829477124764,14.5110084065472,
127.25198980975)) ;
#132797 = CARTESIAN_POINT('Ctrl Pts',(-31.8996523370137,14.4754271659884,
126.975598872173)) ;
#132798 = CARTESIAN_POINT('Ctrl Pts',(-31.8224332847297,14.3641624802179,
126.716820698264)) ;
#132799 = CARTESIAN_POINT('Ctrl Pts',(-31.7580395500746,14.1852632695012,
126.495546204119)) ;
#132800 = CARTESIAN_POINT('Ctrl Pts',(-31.7118161309124,13.9526451401233,
126.327472065972)) ;
#132801 = CARTESIAN_POINT('Ctrl Pts',(-31.6875151171821,13.6818447118076,
126.223384381321)) ;
#132802 = CARTESIAN_POINT('Ctrl Pts',(-31.6876428707132,13.3926206452482,
126.190673672069)) ;
#132803 = CARTESIAN_POINT('Ctrl Pts',(-31.7132303697958,13.1038754923078,
126.232132655585)) ;
#132804 = CARTESIAN_POINT('Ctrl Pts',(-31.7626844305404,12.8403836297391,
126.343597807942)) ;
#132805 = CARTESIAN_POINT('Ctrl Pts',(-31.833493429736,12.6175434576375,126.517332769775)) ;
#132806 = CARTESIAN_POINT('Ctrl Pts',(-31.9215930084005,12.4520178789147,
126.741478574285)) ;
#132807 = CARTESIAN_POINT('Ctrl Pts',(-32.0209307914902,12.3567780608222,
126.998523271918)) ;
#132808 = CARTESIAN_POINT('Ctrl Pts',(-32.1246416504795,12.3376561109864,
127.268538964137)) ;
#132809 = CARTESIAN_POINT('Ctrl Pts',(-32.2275246940126,12.3963494804203,
127.535847716125)) ;
#132810 = CARTESIAN_POINT('Ctrl Pts',(-32.3214673626583,12.5282529228556,
127.777238677115)) ;
#132811 = CARTESIAN_POINT('Ctrl Pts',(-32.4013423719323,12.7243873042916,
127.977442347176)) ;
#132812 = CARTESIAN_POINT('Ctrl Pts',(-32.4619096573449,12.9708923918956,
128.121216797039)) ;
#132813 = CARTESIAN_POINT('Ctrl Pts',(-32.4994416556502,13.2502126197918,
128.197659332614)) ;
#132814 = CARTESIAN_POINT('Ctrl Pts',(-32.5119978982385,13.5400583828972,
128.201358931735)) ;
#132815 = CARTESIAN_POINT('Ctrl Pts',(-32.4994888167825,13.8239338286533,
128.131553230696)) ;
#132816 = CARTESIAN_POINT('Ctrl Pts',(-32.4634273595897,14.0777676729547,
127.99308635593)) ;
#132817 = CARTESIAN_POINT('Ctrl Pts',(-32.4075028614965,14.2841378500946,
127.796711420429)) ;
#132818 = CARTESIAN_POINT('Ctrl Pts',(-32.3359847249591,14.429815657766,127.554661094343)) ;
#132819 = CARTESIAN_POINT('Ctrl Pts',(-32.2546028623038,14.5033259168077,
127.283693381333)) ;
#132820 = CARTESIAN_POINT('Ctrl Pts',(-32.1704924928081,14.499135115111,127.004877771061)) ;
#132821 = CARTESIAN_POINT('Ctrl Pts',(-32.0900191687497,14.4177798325381,
126.736640312097)) ;
#132822 = CARTESIAN_POINT('Ctrl Pts',(-32.0200109297833,14.2657377102023,
126.499094130843)) ;
#132823 = CARTESIAN_POINT('Ctrl Pts',(-31.9656700623202,14.0527574173429,
126.30717910773)) ;
#132824 = CARTESIAN_POINT('Ctrl Pts',(-31.9319934820835,13.7942044324148,
126.175602610685)) ;
#132825 = CARTESIAN_POINT('Ctrl Pts',(-31.922152144827,13.509972220369,126.1137676569)) ;
#132826 = CARTESIAN_POINT('Ctrl Pts',(-31.9373531303038,13.219834764377,126.12511889965)) ;
#132827 = CARTESIAN_POINT('Ctrl Pts',(-31.9773715779164,12.9433154987134,
126.208868906181)) ;
#132828 = CARTESIAN_POINT('Ctrl Pts',(-32.0403631928475,12.7008042356819,
126.359640175799)) ;
#132829 = CARTESIAN_POINT('Ctrl Pts',(-32.1214625671299,12.5118988342583,
126.563632155226)) ;
#132830 = CARTESIAN_POINT('Ctrl Pts',(-32.2168510067031,12.3867144480253,
126.809132213192)) ;
#132831 = CARTESIAN_POINT('Ctrl Pts',(-32.3199033888381,12.3359851161897,
127.077044236849)) ;
#132832 = CARTESIAN_POINT('Ctrl Pts',(-32.4242222709057,12.3634203970633,
127.348571063411)) ;
#132833 = CARTESIAN_POINT('Ctrl Pts',(-32.5223579803355,12.4663876358086,
127.602200216398)) ;
#132834 = CARTESIAN_POINT('Ctrl Pts',(-32.6089883742709,12.6389701182042,
127.82200642748)) ;
#132835 = CARTESIAN_POINT('Ctrl Pts',(-32.6774297887948,12.8657474577828,
127.988998597794)) ;
#132836 = CARTESIAN_POINT('Ctrl Pts',(-32.724805208469,13.1346343436699,128.094136048027)) ;
#132837 = CARTESIAN_POINT('Ctrl Pts',(-32.7399114943369,13.3266512177486,
128.116225545094)) ;
#132838 = CARTESIAN_POINT('Ctrl Pts',(-32.7433109767759,13.4226801736581,
128.115135559137)) ;
#132839 = CARTESIAN_POINT('',(-11.2812798643659,13.1551399285885,133.225361312885)) ;
#132840 = CARTESIAN_POINT('',(-21.9982570673691,12.9778651918053,129.622952131535)) ;
#132841 = CARTESIAN_POINT('Ctrl Pts',(-11.2812798643659,13.1551399285885,
133.225361312885)) ;
#132842 = CARTESIAN_POINT('Ctrl Pts',(-11.2820187647633,13.1489709609094,
133.226788867079)) ;
#132843 = CARTESIAN_POINT('Ctrl Pts',(-11.2940725891313,13.0505878441039,
133.250318667877)) ;
#132844 = CARTESIAN_POINT('Ctrl Pts',(-11.3268196692865,12.8648900473044,
133.323006215356)) ;
#132845 = CARTESIAN_POINT('Ctrl Pts',(-11.3955581347561,12.6378996894465,
133.490786092827)) ;
#132846 = CARTESIAN_POINT('Ctrl Pts',(-11.4818126038911,12.4661938442505,
133.709651137204)) ;
#132847 = CARTESIAN_POINT('Ctrl Pts',(-11.5806418499012,12.3629468779938,
133.965082777503)) ;
#132848 = CARTESIAN_POINT('Ctrl Pts',(-11.6840920756584,12.3360866578135,
134.234357728742)) ;
#132849 = CARTESIAN_POINT('Ctrl Pts',(-11.7874232958009,12.3868467815327,
134.502988211751)) ;
#132850 = CARTESIAN_POINT('Ctrl Pts',(-11.8826517586958,12.5118616193735,
134.748082512994)) ;
#132851 = CARTESIAN_POINT('Ctrl Pts',(-11.9642364503466,12.7022376314793,
134.953268302114)) ;
#132852 = CARTESIAN_POINT('Ctrl Pts',(-12.0268555159077,12.9442211340136,
135.103070944459)) ;
#132853 = CARTESIAN_POINT('Ctrl Pts',(-12.0667868417897,13.2203922331636,
135.186606249474)) ;
#132854 = CARTESIAN_POINT('Ctrl Pts',(-12.0819921567622,13.5109001041669,
135.197934267535)) ;
#132855 = CARTESIAN_POINT('Ctrl Pts',(-12.0718871830781,13.7967277450532,
135.135125417403)) ;
#132856 = CARTESIAN_POINT('Ctrl Pts',(-12.0382787552941,14.0531634695327,
135.003985075531)) ;
#132857 = CARTESIAN_POINT('Ctrl Pts',(-11.984040511163,14.2659161102292,134.812412340654)) ;
#132858 = CARTESIAN_POINT('Ctrl Pts',(-11.9138317313736,14.4182155312585,
134.574200139104)) ;
#132859 = CARTESIAN_POINT('Ctrl Pts',(-11.8331828494072,14.4993926065239,
134.305392211434)) ;
#132860 = CARTESIAN_POINT('Ctrl Pts',(-11.7490444838035,14.5030674016304,
134.026483130585)) ;
#132861 = CARTESIAN_POINT('Ctrl Pts',(-11.6680809986179,14.4296658181567,
133.756898311423)) ;
#132862 = CARTESIAN_POINT('Ctrl Pts',(-11.5965958202758,14.2842405620309,
133.514968656249)) ;
#132863 = CARTESIAN_POINT('Ctrl Pts',(-11.5404239481228,14.0768885755418,
133.31772524141)) ;
#132864 = CARTESIAN_POINT('Ctrl Pts',(-11.5044626643021,13.821937566696,133.179448820527)) ;
#132865 = CARTESIAN_POINT('Ctrl Pts',(-11.492115437901,13.5404397832619,133.110400577556)) ;
#132866 = CARTESIAN_POINT('Ctrl Pts',(-11.5046895368218,13.2491903771815,
133.113990718504)) ;
#132867 = CARTESIAN_POINT('Ctrl Pts',(-11.5423996819585,12.9699188880577,
133.190943520196)) ;
#132868 = CARTESIAN_POINT('Ctrl Pts',(-11.6027127193453,12.7245502986717,
133.33412175314)) ;
#132869 = CARTESIAN_POINT('Ctrl Pts',(-11.6827307770101,12.5279694687298,
133.534676781188)) ;
#132870 = CARTESIAN_POINT('Ctrl Pts',(-11.7767909409935,12.3961377043517,
133.7763823545)) ;
#132871 = CARTESIAN_POINT('Ctrl Pts',(-11.8796482494039,12.3376103677892,
134.043626665423)) ;
#132872 = CARTESIAN_POINT('Ctrl Pts',(-11.9835249356267,12.3569098529355,
134.314074542349)) ;
#132873 = CARTESIAN_POINT('Ctrl Pts',(-12.0830151650733,12.452769019898,134.571498333322)) ;
#132874 = CARTESIAN_POINT('Ctrl Pts',(-12.1707022339469,12.6179593573441,
134.794565234874)) ;
#132875 = CARTESIAN_POINT('Ctrl Pts',(-12.2415306520725,12.8405880377693,
134.968374154773)) ;
#132876 = CARTESIAN_POINT('Ctrl Pts',(-12.2912076318387,13.1065246421439,
135.080214865833)) ;
#132877 = CARTESIAN_POINT('Ctrl Pts',(-12.3163775691246,13.3925179674891,
135.12078307657)) ;
#132878 = CARTESIAN_POINT('Ctrl Pts',(-12.3166058496797,13.6819916651313,
135.088335546118)) ;
#132879 = CARTESIAN_POINT('Ctrl Pts',(-12.2921472081091,13.9537242418059,
134.983669295533)) ;
#132880 = CARTESIAN_POINT('Ctrl Pts',(-12.2457390773696,14.1863734291659,
134.815010882744)) ;
#132881 = CARTESIAN_POINT('Ctrl Pts',(-12.1814800516644,14.3643807985693,
134.59423567404)) ;
#132882 = CARTESIAN_POINT('Ctrl Pts',(-12.1044683457898,14.4754559850244,
134.336147922274)) ;
#132883 = CARTESIAN_POINT('Ctrl Pts',(-12.0208090250937,14.5110246739577,
134.058551574174)) ;
#132884 = CARTESIAN_POINT('Ctrl Pts',(-11.9378612224862,14.4687063588107,
133.783197368949)) ;
#132885 = CARTESIAN_POINT('Ctrl Pts',(-11.8615647632541,14.3514018815055,
133.527145574601)) ;
#132886 = CARTESIAN_POINT('Ctrl Pts',(-11.798502564401,14.1671964752596,133.309749293991)) ;
#132887 = CARTESIAN_POINT('Ctrl Pts',(-11.754049052173,13.9308608041133,133.146872132253)) ;
#132888 = CARTESIAN_POINT('Ctrl Pts',(-11.7316977644638,13.6570089999716,
133.048397750488)) ;
#132889 = CARTESIAN_POINT('Ctrl Pts',(-11.7341180951435,13.3664659574419,
133.022308686926)) ;
#132890 = CARTESIAN_POINT('Ctrl Pts',(-11.761720921654,13.0805681472547,133.069846022257)) ;
#132891 = CARTESIAN_POINT('Ctrl Pts',(-11.8131936002259,12.8190539470386,
133.187112979174)) ;
#132892 = CARTESIAN_POINT('Ctrl Pts',(-11.886092857491,12.5999338423892,133.366806137464)) ;
#132893 = CARTESIAN_POINT('Ctrl Pts',(-11.9747587487869,12.4413957528131,
133.592859241921)) ;
#132894 = CARTESIAN_POINT('Ctrl Pts',(-12.0748052338517,12.3520378265489,
133.85195165464)) ;
#132895 = CARTESIAN_POINT('Ctrl Pts',(-12.1791704719716,12.339734386482,134.123710421306)) ;
#132896 = CARTESIAN_POINT('Ctrl Pts',(-12.2811942198852,12.4049383167358,
134.388634754176)) ;
#132897 = CARTESIAN_POINT('Ctrl Pts',(-12.3743104910804,12.5429634979505,
134.627548525017)) ;
#132898 = CARTESIAN_POINT('Ctrl Pts',(-12.4527350962615,12.7443553986761,
134.823486021638)) ;
#132899 = CARTESIAN_POINT('Ctrl Pts',(-12.5113245953194,12.9943521537239,
134.961502568807)) ;
#132900 = CARTESIAN_POINT('Ctrl Pts',(-12.5466491191103,13.2741647768729,
135.031655728832)) ;
#132901 = CARTESIAN_POINT('Ctrl Pts',(-12.557133530808,13.565720269456,135.029118946566)) ;
#132902 = CARTESIAN_POINT('Ctrl Pts',(-12.5424084976818,13.8474315556546,
134.952884078473)) ;
#132903 = CARTESIAN_POINT('Ctrl Pts',(-12.504658245782,14.0971649669908,134.809596596871)) ;
#132904 = CARTESIAN_POINT('Ctrl Pts',(-12.4468015681524,14.3002122843455,
134.607345660129)) ;
#132905 = CARTESIAN_POINT('Ctrl Pts',(-12.3740820116557,14.4394509674979,
134.361774496034)) ;
#132906 = CARTESIAN_POINT('Ctrl Pts',(-12.2928286579386,14.5058688200503,
134.091445642351)) ;
#132907 = CARTESIAN_POINT('Ctrl Pts',(-12.2085754911848,14.4952594831202,
133.812133112469)) ;
#132908 = CARTESIAN_POINT('Ctrl Pts',(-12.1285286312613,14.4071576912799,
133.54505905862)) ;
#132909 = CARTESIAN_POINT('Ctrl Pts',(-12.0595995840032,14.2488070341169,
133.310594609379)) ;
#132910 = CARTESIAN_POINT('Ctrl Pts',(-12.007204001394,14.032332595662,133.124541926762)) ;
#132911 = CARTESIAN_POINT('Ctrl Pts',(-11.9754518623539,13.7715185673777,
132.998664946929)) ;
#132912 = CARTESIAN_POINT('Ctrl Pts',(-11.9676077024159,13.4849968555095,
132.942553623633)) ;
#132913 = CARTESIAN_POINT('Ctrl Pts',(-11.9852141495617,13.1936954317484,
132.960744777079)) ;
#132914 = CARTESIAN_POINT('Ctrl Pts',(-12.0270155274854,12.9217410981826,
133.049976934939)) ;
#132915 = CARTESIAN_POINT('Ctrl Pts',(-12.0916442917843,12.6826993167214,
133.205531163459)) ;
#132916 = CARTESIAN_POINT('Ctrl Pts',(-12.1748344849184,12.4976839220085,
133.415374259801)) ;
#132917 = CARTESIAN_POINT('Ctrl Pts',(-12.2706003786281,12.3794711428103,
133.662174391645)) ;
#132918 = CARTESIAN_POINT('Ctrl Pts',(-12.3744503899862,12.3351744196322,
133.932269165389)) ;
#132919 = CARTESIAN_POINT('Ctrl Pts',(-12.4782650208009,12.3695012763354,
134.202412750315)) ;
#132920 = CARTESIAN_POINT('Ctrl Pts',(-12.5754721648271,12.4786183736045,
134.453365352351)) ;
#132921 = CARTESIAN_POINT('Ctrl Pts',(-12.6605578265862,12.6556201701116,
134.668788412585)) ;
#132922 = CARTESIAN_POINT('Ctrl Pts',(-12.7278290779799,12.8885376957079,
134.832076052564)) ;
#132923 = CARTESIAN_POINT('Ctrl Pts',(-12.7727942038789,13.1578672277872,
134.93044163856)) ;
#132924 = CARTESIAN_POINT('Ctrl Pts',(-12.7935589960753,13.4488181058444,
134.957796140316)) ;
#132925 = CARTESIAN_POINT('Ctrl Pts',(-12.7888443918457,13.7357351250712,
134.91097260511)) ;
#132926 = CARTESIAN_POINT('Ctrl Pts',(-12.7602605916963,14.0000244154435,
134.794478626913)) ;
#132927 = CARTESIAN_POINT('Ctrl Pts',(-12.7099141607957,14.2248063693443,
134.614145960045)) ;
#132928 = CARTESIAN_POINT('Ctrl Pts',(-12.6428897963242,14.3907221531774,
134.385334239461)) ;
#132929 = CARTESIAN_POINT('Ctrl Pts',(-12.5640447774941,14.4880878052934,
134.121834427977)) ;
#132930 = CARTESIAN_POINT('Ctrl Pts',(-12.4802617689659,14.5090844515927,
133.844015139513)) ;
#132931 = CARTESIAN_POINT('Ctrl Pts',(-12.3974642832698,14.4517331277302,
133.568827359843)) ;
#132932 = CARTESIAN_POINT('Ctrl Pts',(-12.3236763447296,14.3213873494252,
133.320287858352)) ;
#132933 = CARTESIAN_POINT('Ctrl Pts',(-12.2637347152158,14.1266126254878,
133.112060420808)) ;
#132934 = CARTESIAN_POINT('Ctrl Pts',(-12.2229774667805,13.8801113803002,
132.959735466426)) ;
#132935 = CARTESIAN_POINT('Ctrl Pts',(-12.2053838579744,13.6025840232108,
132.875302084043)) ;
#132936 = CARTESIAN_POINT('Ctrl Pts',(-12.2124772397581,13.3122088978665,
132.862974191922)) ;
#132937 = CARTESIAN_POINT('Ctrl Pts',(-12.2448145015933,13.0284665595888,
132.924236901387)) ;
#132938 = CARTESIAN_POINT('Ctrl Pts',(-12.3005599019218,12.7739765033465,
133.053999198988)) ;
#132939 = CARTESIAN_POINT('Ctrl Pts',(-12.3766445028271,12.5655228915478,
133.243117582921)) ;
#132940 = CARTESIAN_POINT('Ctrl Pts',(-12.4681423855166,12.4188418488155,
133.47731500825)) ;
#132941 = CARTESIAN_POINT('Ctrl Pts',(-12.5692422546882,12.3438198182334,
133.739584235759)) ;
#132942 = CARTESIAN_POINT('Ctrl Pts',(-12.6740334889537,12.3461749880073,
134.012474638995)) ;
#132943 = CARTESIAN_POINT('Ctrl Pts',(-12.7747162224539,12.4256199459212,
134.273532924423)) ;
#132944 = CARTESIAN_POINT('Ctrl Pts',(-12.8655945356852,12.5766359900473,
134.505860328425)) ;
#132945 = CARTESIAN_POINT('Ctrl Pts',(-12.9405208029623,12.7882864475543,
134.691614915467)) ;
#132946 = CARTESIAN_POINT('Ctrl Pts',(-12.9949316879518,13.0452019382586,
134.817458837911)) ;
#132947 = CARTESIAN_POINT('Ctrl Pts',(-13.025720643168,13.3293877258915,134.874271333741)) ;
#132948 = CARTESIAN_POINT('Ctrl Pts',(-13.0313457796955,13.6204035856812,
134.857561997613)) ;
#132949 = CARTESIAN_POINT('Ctrl Pts',(-13.0121238177563,13.8971496153171,
134.768280402699)) ;
#132950 = CARTESIAN_POINT('Ctrl Pts',(-12.9702433337836,14.1397539052331,
134.612839445253)) ;
#132951 = CARTESIAN_POINT('Ctrl Pts',(-12.9092683557999,14.3313464702874,
134.401559637406)) ;
#132952 = CARTESIAN_POINT('Ctrl Pts',(-12.8346344667875,14.4574458616527,
134.150487900523)) ;
#132953 = CARTESIAN_POINT('Ctrl Pts',(-12.7520232585293,14.5099723944026,
133.876034599555)) ;
#132954 = CARTESIAN_POINT('Ctrl Pts',(-12.6680149991839,14.4843439695083,
133.597416296755)) ;
#132955 = CARTESIAN_POINT('Ctrl Pts',(-12.5898605639027,14.3827749410654,
133.336012913517)) ;
#132956 = CARTESIAN_POINT('Ctrl Pts',(-12.5235110131134,14.2124739950545,
133.109063094795)) ;
#132957 = CARTESIAN_POINT('Ctrl Pts',(-12.47454385575,13.9855789386979,132.932891873958)) ;
#132958 = CARTESIAN_POINT('Ctrl Pts',(-12.44718714331,13.7185805864342,132.819871229684)) ;
#132959 = CARTESIAN_POINT('Ctrl Pts',(-12.4441083202369,13.4303185636673,
132.777757800251)) ;
#132960 = CARTESIAN_POINT('Ctrl Pts',(-12.4662081675216,13.1417758325219,
132.809228396078)) ;
#132961 = CARTESIAN_POINT('Ctrl Pts',(-12.5128438608682,12.8725286043858,
132.912265477798)) ;
#132962 = CARTESIAN_POINT('Ctrl Pts',(-12.5811355936144,12.6435096258014,
133.078662360882)) ;
#132963 = CARTESIAN_POINT('Ctrl Pts',(-12.6670557983815,12.4701546223289,
133.296533072804)) ;
#132964 = CARTESIAN_POINT('Ctrl Pts',(-12.7650980875458,12.3650501876111,
133.549835459936)) ;
#132965 = CARTESIAN_POINT('Ctrl Pts',(-12.8692895553206,12.3357586674927,
133.821013809302)) ;
#132966 = CARTESIAN_POINT('Ctrl Pts',(-12.9722194636702,12.3843195509594,
134.088641190149)) ;
#132967 = CARTESIAN_POINT('Ctrl Pts',(-13.0679235169665,12.5073666683789,
134.335069106556)) ;
#132968 = CARTESIAN_POINT('Ctrl Pts',(-13.1498474421669,12.6958200369819,
134.541296314724)) ;
#132969 = CARTESIAN_POINT('Ctrl Pts',(-13.2130846476701,12.9363649293222,
134.692916583502)) ;
#132970 = CARTESIAN_POINT('Ctrl Pts',(-13.2537553284003,13.212046231595,134.778583028313)) ;
#132971 = CARTESIAN_POINT('Ctrl Pts',(-13.2696867588976,13.5022481067603,
134.792052779991)) ;
#132972 = CARTESIAN_POINT('Ctrl Pts',(-13.2603291226857,13.7884016128943,
134.731444216182)) ;
#132973 = CARTESIAN_POINT('Ctrl Pts',(-13.2274358441086,14.045945075732,134.602400846472)) ;
#132974 = CARTESIAN_POINT('Ctrl Pts',(-13.1734739345736,14.2610680704969,
134.41149155897)) ;
#132975 = CARTESIAN_POINT('Ctrl Pts',(-13.1038966633744,14.4145624165552,
134.175255364668)) ;
#132976 = CARTESIAN_POINT('Ctrl Pts',(-13.0234728088093,14.4980852125695,
133.907100960487)) ;
#132977 = CARTESIAN_POINT('Ctrl Pts',(-12.939325995419,14.5041312739862,133.628163299805)) ;
#132978 = CARTESIAN_POINT('Ctrl Pts',(-12.8580140805557,14.4326962339747,
133.357486536545)) ;
#132979 = CARTESIAN_POINT('Ctrl Pts',(-12.7862358410937,14.289424830309,133.114743545619)) ;
#132980 = CARTESIAN_POINT('Ctrl Pts',(-12.7294171395877,14.0826507854277,
132.915479459106)) ;
#132981 = CARTESIAN_POINT('Ctrl Pts',(-12.6931113261045,13.8312291814697,
132.77650858526)) ;
#132982 = CARTESIAN_POINT('Ctrl Pts',(-12.6798565616288,13.5479805821752,
132.704527307887)) ;
#132983 = CARTESIAN_POINT('Ctrl Pts',(-12.6918329131031,13.2572981016289,
132.706442366543)) ;
#132984 = CARTESIAN_POINT('Ctrl Pts',(-12.7286154648152,12.9781391944844,
132.780789668285)) ;
#132985 = CARTESIAN_POINT('Ctrl Pts',(-12.788841308569,12.7298471383749,132.923457407859)) ;
#132986 = CARTESIAN_POINT('Ctrl Pts',(-12.8678064119023,12.5331718510569,
133.121190067536)) ;
#132987 = CARTESIAN_POINT('Ctrl Pts',(-12.9619860922532,12.3987050488903,
133.3630746114)) ;
#132988 = CARTESIAN_POINT('Ctrl Pts',(-13.0641173669679,12.3381977133859,
133.628393862531)) ;
#132989 = CARTESIAN_POINT('Ctrl Pts',(-13.1689636586994,12.3556285786372,
133.901368958815)) ;
#132990 = CARTESIAN_POINT('Ctrl Pts',(-13.2676215267395,12.448498640132,134.156721062578)) ;
#132991 = CARTESIAN_POINT('Ctrl Pts',(-13.3562794099848,12.6124651727369,
134.382428532808)) ;
#132992 = CARTESIAN_POINT('Ctrl Pts',(-13.4274024159188,12.8330193864531,
134.55721035227)) ;
#132993 = CARTESIAN_POINT('Ctrl Pts',(-13.4778657839761,13.0981216515098,
134.671314825157)) ;
#132994 = CARTESIAN_POINT('Ctrl Pts',(-13.5037873702561,13.3840423616995,
134.714047923931)) ;
#132995 = CARTESIAN_POINT('Ctrl Pts',(-13.5047230832927,13.6738043197191,
134.683656575562)) ;
#132996 = CARTESIAN_POINT('Ctrl Pts',(-13.4810350619758,13.9458856450603,
134.581307831703)) ;
#132997 = CARTESIAN_POINT('Ctrl Pts',(-13.4350850950003,14.1805609741337,
134.413888828413)) ;
#132998 = CARTESIAN_POINT('Ctrl Pts',(-13.3713435625267,14.3602096703021,
134.19466352274)) ;
#132999 = CARTESIAN_POINT('Ctrl Pts',(-13.2941228668166,14.4737146563849,
133.935766751957)) ;
#133000 = CARTESIAN_POINT('Ctrl Pts',(-13.2111150371913,14.510981736058,133.660304806086)) ;
#133001 = CARTESIAN_POINT('Ctrl Pts',(-13.1279555516473,14.4710234538019,
133.384286573336)) ;
#133002 = CARTESIAN_POINT('Ctrl Pts',(-13.0514607207591,14.3558611755068,
133.127695259553)) ;
#133003 = CARTESIAN_POINT('Ctrl Pts',(-12.987929872837,14.1736059642118,132.908940703681)) ;
#133004 = CARTESIAN_POINT('Ctrl Pts',(-12.9427874558613,13.9381264816024,
132.743987191645)) ;
#133005 = CARTESIAN_POINT('Ctrl Pts',(-12.9198159126567,13.665192099168,132.643720985883)) ;
#133006 = CARTESIAN_POINT('Ctrl Pts',(-12.9214159568252,13.3755914984187,
132.615321479283)) ;
#133007 = CARTESIAN_POINT('Ctrl Pts',(-12.9485033871058,13.0874857506397,
132.661141600498)) ;
#133008 = CARTESIAN_POINT('Ctrl Pts',(-12.9991534842726,12.8264337657975,
132.776172659393)) ;
#133009 = CARTESIAN_POINT('Ctrl Pts',(-13.0712502877118,12.6060974389448,
132.953593799865)) ;
#133010 = CARTESIAN_POINT('Ctrl Pts',(-13.1597261697062,12.4450313389733,
133.179001034814)) ;
#133011 = CARTESIAN_POINT('Ctrl Pts',(-13.2598221399245,12.3534666197661,
133.438152169847)) ;
#133012 = CARTESIAN_POINT('Ctrl Pts',(-13.3638496997786,12.3390029903486,
133.709021457282)) ;
#133013 = CARTESIAN_POINT('Ctrl Pts',(-13.466268319613,12.4020392430349,133.975026492123)) ;
#133014 = CARTESIAN_POINT('Ctrl Pts',(-13.5598211640111,12.5385711173323,
134.215165246668)) ;
#133015 = CARTESIAN_POINT('Ctrl Pts',(-13.6383382505058,12.737337324062,134.411540597844)) ;
#133016 = CARTESIAN_POINT('Ctrl Pts',(-13.6976697861643,12.9861206892308,
134.551707741949)) ;
#133017 = CARTESIAN_POINT('Ctrl Pts',(-13.7337928936498,13.2660910782566,
134.62410596592)) ;
#133018 = CARTESIAN_POINT('Ctrl Pts',(-13.7449404119012,13.5573227840952,
134.623538746113)) ;
#133019 = CARTESIAN_POINT('Ctrl Pts',(-13.731057609949,13.8386952169897,134.549882879065)) ;
#133020 = CARTESIAN_POINT('Ctrl Pts',(-13.6938267710482,14.0906007554108,
134.407982826979)) ;
#133021 = CARTESIAN_POINT('Ctrl Pts',(-13.6366983945426,14.2945039762926,
134.207985282423)) ;
#133022 = CARTESIAN_POINT('Ctrl Pts',(-13.5643971905334,14.4361574187858,
133.963631330981)) ;
#133023 = CARTESIAN_POINT('Ctrl Pts',(-13.4829079562931,14.5051117570611,
133.692450855681)) ;
#133024 = CARTESIAN_POINT('Ctrl Pts',(-13.398865589322,14.496582620466,133.413844416583)) ;
#133025 = CARTESIAN_POINT('Ctrl Pts',(-13.3188758691256,14.4113394819302,
133.147064384826)) ;
#133026 = CARTESIAN_POINT('Ctrl Pts',(-13.2492482094451,14.2546479447355,
132.910444808226)) ;
#133027 = CARTESIAN_POINT('Ctrl Pts',(-13.1961963849046,14.039143877786,132.722400695126)) ;
#133028 = CARTESIAN_POINT('Ctrl Pts',(-13.1638347550569,13.7793416572316,
132.594749383636)) ;
#133029 = CARTESIAN_POINT('Ctrl Pts',(-13.1552775077889,13.4941095874199,
132.536650789137)) ;
#133030 = CARTESIAN_POINT('Ctrl Pts',(-13.1720447629105,13.2026874966814,
132.552397812081)) ;
#133031 = CARTESIAN_POINT('Ctrl Pts',(-13.2133004298939,12.928833346161,132.639904988231)) ;
#133032 = CARTESIAN_POINT('Ctrl Pts',(-13.2774801251183,12.6885083712283,
132.794116581438)) ;
#133033 = CARTESIAN_POINT('Ctrl Pts',(-13.3597053837363,12.5026390795781,
133.001327621254)) ;
#133034 = CARTESIAN_POINT('Ctrl Pts',(-13.455701350823,12.3816810236162,133.248611444686)) ;
#133035 = CARTESIAN_POINT('Ctrl Pts',(-13.5588450701788,12.3354826595071,
133.516837122875)) ;
#133036 = CARTESIAN_POINT('Ctrl Pts',(-13.662986257812,12.3671988660942,133.787859387829)) ;
#133037 = CARTESIAN_POINT('Ctrl Pts',(-13.7608857501055,12.4748749581507,
134.040689706046)) ;
#133038 = CARTESIAN_POINT('Ctrl Pts',(-13.8461189502053,12.6498955190515,
134.256626571108)) ;
#133039 = CARTESIAN_POINT('Ctrl Pts',(-13.9137641762851,12.8801431332148,
134.421162047123)) ;
#133040 = CARTESIAN_POINT('Ctrl Pts',(-13.959688118663,13.1504415297617,134.52210348875)) ;
#133041 = CARTESIAN_POINT('Ctrl Pts',(-13.9810355826832,13.438739202615,134.551438413197)) ;
#133042 = CARTESIAN_POINT('Ctrl Pts',(-13.9771509252308,13.7280473502378,
134.50680820225)) ;
#133043 = CARTESIAN_POINT('Ctrl Pts',(-13.9490883356948,13.9932362064335,
134.391820118097)) ;
#133044 = CARTESIAN_POINT('Ctrl Pts',(-13.899552383743,14.2186783745982,134.213988401194)) ;
#133045 = CARTESIAN_POINT('Ctrl Pts',(-13.8326088799132,14.3872014330787,
133.985246691092)) ;
#133046 = CARTESIAN_POINT('Ctrl Pts',(-13.754354251272,14.486216521528,133.723625961275)) ;
#133047 = CARTESIAN_POINT('Ctrl Pts',(-13.6703274653614,14.5095010567365,
133.444968044136)) ;
#133048 = CARTESIAN_POINT('Ctrl Pts',(-13.587915515568,14.4548476689191,133.171125957688)) ;
#133049 = CARTESIAN_POINT('Ctrl Pts',(-13.5132496102258,14.3259646517619,
132.919798090487)) ;
#133050 = CARTESIAN_POINT('Ctrl Pts',(-13.4528381497739,14.1320240566172,
132.710133322283)) ;
#133051 = CARTESIAN_POINT('Ctrl Pts',(-13.4117984923924,13.8890687487633,
132.557286539592)) ;
#133052 = CARTESIAN_POINT('Ctrl Pts',(-13.3933038950219,13.6109288487181,
132.470050146704)) ;
#133053 = CARTESIAN_POINT('Ctrl Pts',(-13.3996927101153,13.3205780973656,
132.455665139994)) ;
#133054 = CARTESIAN_POINT('Ctrl Pts',(-13.4314451231204,13.0356410236252,
132.515132416829)) ;
#133055 = CARTESIAN_POINT('Ctrl Pts',(-13.4863521726588,12.7811568557338,
132.642583088239)) ;
#133056 = CARTESIAN_POINT('Ctrl Pts',(-13.5618719439237,12.5709851276515,
132.830045482527)) ;
#133057 = CARTESIAN_POINT('Ctrl Pts',(-13.6530001533805,12.4221766619671,
133.063156221214)) ;
#133058 = CARTESIAN_POINT('Ctrl Pts',(-13.7543438242653,12.3447406812541,
133.325997758698)) ;
#133059 = CARTESIAN_POINT('Ctrl Pts',(-13.858979447707,12.3451621602759,133.598484050117)) ;
#133060 = CARTESIAN_POINT('Ctrl Pts',(-13.9595871058779,12.4221617733591,
133.859413033911)) ;
#133061 = CARTESIAN_POINT('Ctrl Pts',(-14.0509368702114,12.5713293574021,
134.093085140404)) ;
#133062 = CARTESIAN_POINT('Ctrl Pts',(-14.1263288360547,12.7811357471148,
134.280239363245)) ;
#133063 = CARTESIAN_POINT('Ctrl Pts',(-14.181464730297,13.037385413305,134.408146154191)) ;
#133064 = CARTESIAN_POINT('Ctrl Pts',(-14.2129289597319,13.3202247802994,
134.46702998844)) ;
#133065 = CARTESIAN_POINT('Ctrl Pts',(-14.2193168783918,13.6126649497902,
134.452393596522)) ;
#133066 = CARTESIAN_POINT('Ctrl Pts',(-14.2008364796894,13.889109539137,134.365400616144)) ;
#133067 = CARTESIAN_POINT('Ctrl Pts',(-14.1595000662705,14.1334576219234,
134.211477497111)) ;
#133068 = CARTESIAN_POINT('Ctrl Pts',(-14.0992466494206,14.3262010857029,
134.002423062281)) ;
#133069 = CARTESIAN_POINT('Ctrl Pts',(-14.0244678789738,14.4552702241494,
133.750713932904)) ;
#133070 = CARTESIAN_POINT('Ctrl Pts',(-13.9418997721999,14.5094659873619,
133.476364746001)) ;
#133071 = CARTESIAN_POINT('Ctrl Pts',(-13.8583861168424,14.48627928254,133.199410244325)) ;
#133072 = CARTESIAN_POINT('Ctrl Pts',(-13.7797353567973,14.3867194330965,
132.936459435104)) ;
#133073 = CARTESIAN_POINT('Ctrl Pts',(-13.7130105219871,14.2183273389604,
132.708437979387)) ;
#133074 = CARTESIAN_POINT('Ctrl Pts',(-13.6633479068396,13.9922441011096,
132.530147180322)) ;
#133075 = CARTESIAN_POINT('Ctrl Pts',(-13.6354328184579,13.7260908863955,
132.415503205816)) ;
#133076 = CARTESIAN_POINT('Ctrl Pts',(-13.6315996421401,13.4392990683917,
132.371317925094)) ;
#133077 = CARTESIAN_POINT('Ctrl Pts',(-13.6531002743803,13.1491383926391,
132.400878674979)) ;
#133078 = CARTESIAN_POINT('Ctrl Pts',(-13.6988895423874,12.880138144259,132.501583429181)) ;
#133079 = CARTESIAN_POINT('Ctrl Pts',(-13.7669016038619,12.6488312040692,
132.66702117208)) ;
#133080 = CARTESIAN_POINT('Ctrl Pts',(-13.8519661020191,12.4746173052797,
132.882564533349)) ;
#133081 = CARTESIAN_POINT('Ctrl Pts',(-13.9499918537797,12.3669410581914,
133.13572242046)) ;
#133082 = CARTESIAN_POINT('Ctrl Pts',(-14.0540803057466,12.3355244467329,
133.406613758036)) ;
#133083 = CARTESIAN_POINT('Ctrl Pts',(-14.1570770496498,12.3818824637266,
133.674448586604)) ;
#133084 = CARTESIAN_POINT('Ctrl Pts',(-14.2529156063067,12.502442440452,133.921340780179)) ;
#133085 = CARTESIAN_POINT('Ctrl Pts',(-14.3357164299663,12.6900860359651,
134.129966525958)) ;
#133086 = CARTESIAN_POINT('Ctrl Pts',(-14.3993556473891,12.9290693621117,
134.282824648329)) ;
#133087 = CARTESIAN_POINT('Ctrl Pts',(-14.4406746427025,13.2033802627449,
134.370454904131)) ;
#133088 = CARTESIAN_POINT('Ctrl Pts',(-14.4573570221151,13.493885424346,134.386064394722)) ;
#133089 = CARTESIAN_POINT('Ctrl Pts',(-14.4487939272164,13.7798208359641,
134.327863613174)) ;
#133090 = CARTESIAN_POINT('Ctrl Pts',(-14.4163591296665,14.0398147256928,
134.199973199807)) ;
#133091 = CARTESIAN_POINT('Ctrl Pts',(-14.3630430477874,14.2555980954836,
134.011057985321)) ;
#133092 = CARTESIAN_POINT('Ctrl Pts',(-14.2938516112464,14.4112165057251,
133.775932908363)) ;
#133093 = CARTESIAN_POINT('Ctrl Pts',(-14.213327419341,14.4969135755094,133.50736843725)) ;
#133094 = CARTESIAN_POINT('Ctrl Pts',(-14.1296189321524,14.5049696810031,
133.229876903082)) ;
#133095 = CARTESIAN_POINT('Ctrl Pts',(-14.0481698596881,14.4360249735447,
132.958821806314)) ;
#133096 = CARTESIAN_POINT('Ctrl Pts',(-13.9759487851369,14.2945754362065,
132.714746600477)) ;
#133097 = CARTESIAN_POINT('Ctrl Pts',(-13.9186392005941,14.0897548858671,
132.514089317548)) ;
#133098 = CARTESIAN_POINT('Ctrl Pts',(-13.8816283734556,13.8387001375239,
132.372961040856)) ;
#133099 = CARTESIAN_POINT('Ctrl Pts',(-13.86765973633,13.5574044598577,132.299056743724)) ;
#133100 = CARTESIAN_POINT('Ctrl Pts',(-13.8789956043886,13.2644130009093,
132.2988381339)) ;
#133101 = CARTESIAN_POINT('Ctrl Pts',(-13.9149994984909,12.9862195730077,
132.371090109727)) ;
#133102 = CARTESIAN_POINT('Ctrl Pts',(-13.9743502243685,12.7371111819008,
132.511275565875)) ;
#133103 = CARTESIAN_POINT('Ctrl Pts',(-14.0530557762854,12.5380203242925,
132.708138925323)) ;
#133104 = CARTESIAN_POINT('Ctrl Pts',(-14.1469276806553,12.4015272632005,
132.949117652525)) ;
#133105 = CARTESIAN_POINT('Ctrl Pts',(-14.2489833656644,12.3389470103484,
133.214189844898)) ;
#133106 = CARTESIAN_POINT('Ctrl Pts',(-14.3533226131928,12.3537864997403,
133.485861761893)) ;
#133107 = CARTESIAN_POINT('Ctrl Pts',(-14.4528614890508,12.4449099176858,
133.743576395913)) ;
#133108 = CARTESIAN_POINT('Ctrl Pts',(-14.5418561425685,12.6072327563546,
133.97027761533)) ;
#133109 = CARTESIAN_POINT('Ctrl Pts',(-14.6133813155202,12.8259751420657,
134.146289595912)) ;
#133110 = CARTESIAN_POINT('Ctrl Pts',(-14.6644626717837,13.0894865209779,
134.262268329824)) ;
#133111 = CARTESIAN_POINT('Ctrl Pts',(-14.6912354788188,13.3763086244584,
134.307339213758)) ;
#133112 = CARTESIAN_POINT('Ctrl Pts',(-14.6927780845657,13.666102426872,134.278737035569)) ;
#133113 = CARTESIAN_POINT('Ctrl Pts',(-14.6699098049705,13.9378774393092,
134.178922193569)) ;
#133114 = CARTESIAN_POINT('Ctrl Pts',(-14.6244200591529,14.174793298913,134.012730262355)) ;
#133115 = CARTESIAN_POINT('Ctrl Pts',(-14.5612019536203,14.355667987911,133.795095051057)) ;
#133116 = CARTESIAN_POINT('Ctrl Pts',(-14.4846906294762,14.4711053294092,
133.538428577137)) ;
#133117 = CARTESIAN_POINT('Ctrl Pts',(-14.4011850462511,14.511170979715,133.261273870169)) ;
#133118 = CARTESIAN_POINT('Ctrl Pts',(-14.3178410780268,14.4729025341711,
132.984673903261)) ;
#133119 = CARTESIAN_POINT('Ctrl Pts',(-14.2414431710577,14.3605014183323,
132.728538157581)) ;
#133120 = CARTESIAN_POINT('Ctrl Pts',(-14.1770966200207,14.1789799497678,
132.507210107387)) ;
#133121 = CARTESIAN_POINT('Ctrl Pts',(-14.1315848885081,13.9453130755044,
132.341277366815)) ;
#133122 = CARTESIAN_POINT('Ctrl Pts',(-14.1079390036142,13.673613297581,132.239086339493)) ;
#133123 = CARTESIAN_POINT('Ctrl Pts',(-14.1087830481224,13.3843416477693,
132.208491884339)) ;
#133124 = CARTESIAN_POINT('Ctrl Pts',(-14.1351400941846,13.0956424787648,
132.252157038047)) ;
#133125 = CARTESIAN_POINT('Ctrl Pts',(-14.1851403795369,12.8335787485534,
132.365283706234)) ;
#133126 = CARTESIAN_POINT('Ctrl Pts',(-14.2566883427613,12.6116522531053,
132.541092961402)) ;
#133127 = CARTESIAN_POINT('Ctrl Pts',(-14.3449178102994,12.4486058050818,
132.765728820733)) ;
#133128 = CARTESIAN_POINT('Ctrl Pts',(-14.4444094609299,12.3551665981467,
133.023238128206)) ;
#133129 = CARTESIAN_POINT('Ctrl Pts',(-14.5487260750023,12.3383111368361,
133.294844327139)) ;
#133130 = CARTESIAN_POINT('Ctrl Pts',(-14.651135777708,12.3991318667188,133.560878201396)) ;
#133131 = CARTESIAN_POINT('Ctrl Pts',(-14.7450247980916,12.5336133546432,
133.801997324254)) ;
#133132 = CARTESIAN_POINT('Ctrl Pts',(-14.8240658891889,12.7304747525644,
133.999922781035)) ;
#133133 = CARTESIAN_POINT('Ctrl Pts',(-14.8843591623108,12.9801493565206,
134.142645016146)) ;
#133134 = CARTESIAN_POINT('Ctrl Pts',(-14.9207776314118,13.2569930870622,
134.216214669517)) ;
#133135 = CARTESIAN_POINT('Ctrl Pts',(-14.9327904526555,13.5493201067258,
134.218039568247)) ;
#133136 = CARTESIAN_POINT('Ctrl Pts',(-14.9195608823309,13.8310609228274,
134.146315593606)) ;
#133137 = CARTESIAN_POINT('Ctrl Pts',(-14.8829071658904,14.0843638099265,
134.006060198745)) ;
#133138 = CARTESIAN_POINT('Ctrl Pts',(-14.8262774665716,14.2896244491401,
133.807537482938)) ;
#133139 = CARTESIAN_POINT('Ctrl Pts',(-14.7544509561564,14.4330063116879,
133.564623744753)) ;
#133140 = CARTESIAN_POINT('Ctrl Pts',(-14.6730981695364,14.5042107415309,
133.293824015626)) ;
#133141 = CARTESIAN_POINT('Ctrl Pts',(-14.5890044461905,14.4979449999679,
133.015056574469)) ;
#133142 = CARTESIAN_POINT('Ctrl Pts',(-14.5085811345525,14.4144601779744,
132.746912885546)) ;
#133143 = CARTESIAN_POINT('Ctrl Pts',(-14.4386966820867,14.2595209902124,
132.509575163383)) ;
#133144 = CARTESIAN_POINT('Ctrl Pts',(-14.3852681727933,14.046214919979,132.32053362023)) ;
#133145 = CARTESIAN_POINT('Ctrl Pts',(-14.3521879692475,13.7868053449528,
132.190703349274)) ;
#133146 = CARTESIAN_POINT('Ctrl Pts',(-14.3429850788203,13.5027357390144,
132.130803960272)) ;
#133147 = CARTESIAN_POINT('Ctrl Pts',(-14.3589256787532,13.2114164567146,
132.144166678592)) ;
#133148 = CARTESIAN_POINT('Ctrl Pts',(-14.3996479591576,12.9359342983456,
132.230005501464)) ;
#133149 = CARTESIAN_POINT('Ctrl Pts',(-14.4630310316759,12.6951562018299,
132.381999972268)) ;
#133150 = CARTESIAN_POINT('Ctrl Pts',(-14.5447779273386,12.5073061272103,
132.587797294127)) ;
#133151 = CARTESIAN_POINT('Ctrl Pts',(-14.6405874915994,12.3841592686752,
132.834495044115)) ;
#133152 = CARTESIAN_POINT('Ctrl Pts',(-14.7436396651289,12.3356200239572,
133.102447533053)) ;
#133153 = CARTESIAN_POINT('Ctrl Pts',(-14.8482334000072,12.3655842279676,
133.374661826652)) ;
#133154 = CARTESIAN_POINT('Ctrl Pts',(-14.9456378863924,12.4702048591763,
133.62631542447)) ;
#133155 = CARTESIAN_POINT('Ctrl Pts',(-15.032031341998,12.6448837976238,133.845354670619)) ;
#133156 = CARTESIAN_POINT('Ctrl Pts',(-15.0997909854076,12.872508423284,134.010430965611)) ;
#133157 = CARTESIAN_POINT('Ctrl Pts',(-15.1466624677231,13.1434988331289,
134.11394299587)) ;
#133158 = CARTESIAN_POINT('Ctrl Pts',(-15.1684830221252,13.4301737780494,
134.144821454034)) ;
#133159 = CARTESIAN_POINT('Ctrl Pts',(-15.1655029363779,13.7187795914099,
134.102960274335)) ;
#133160 = CARTESIAN_POINT('Ctrl Pts',(-15.137871807278,13.9870154433738,133.988964277523)) ;
#133161 = CARTESIAN_POINT('Ctrl Pts',(-15.089103500937,14.2124398345738,133.813561355081)) ;
#133162 = CARTESIAN_POINT('Ctrl Pts',(-15.0226861816082,14.3830654461858,
133.586365342099)) ;
#133163 = CARTESIAN_POINT('Ctrl Pts',(-14.9442977084689,14.4846609541733,
133.324197217531)) ;
#133164 = CARTESIAN_POINT('Ctrl Pts',(-14.8603045751173,14.5097913616969,
133.045629352813)) ;
#133165 = CARTESIAN_POINT('Ctrl Pts',(-14.7781158124174,14.4576093080194,
132.772584210679)) ;
#133166 = CARTESIAN_POINT('Ctrl Pts',(-14.7029379087114,14.3304831317374,
132.519675058584)) ;
#133167 = CARTESIAN_POINT('Ctrl Pts',(-14.6421746060609,14.1386183822934,
132.309056084948)) ;
#133168 = CARTESIAN_POINT('Ctrl Pts',(-14.6004669656827,13.8965846856625,
132.154209706835)) ;
#133169 = CARTESIAN_POINT('Ctrl Pts',(-14.5812880337956,13.6198365630073,
132.065057969682)) ;
#133170 = CARTESIAN_POINT('Ctrl Pts',(-14.5869544254102,13.3288844737818,
132.048478781958)) ;
#133171 = CARTESIAN_POINT('Ctrl Pts',(-14.6178077703533,13.0447399832046,
132.105475686592)) ;
#133172 = CARTESIAN_POINT('Ctrl Pts',(-14.6721136258845,12.7881836368688,
132.231068090543)) ;
#133173 = CARTESIAN_POINT('Ctrl Pts',(-14.7475386699193,12.5755910115287,
132.418091523374)) ;
#133174 = CARTESIAN_POINT('Ctrl Pts',(-14.8378940236856,12.4257574465567,
132.649102005788)) ;
#133175 = CARTESIAN_POINT('Ctrl Pts',(-14.9388209084364,12.3460112405744,
132.910787274949)) ;
#133176 = CARTESIAN_POINT('Ctrl Pts',(-15.0435737078647,12.3439532504127,
133.183578235088)) ;
#133177 = CARTESIAN_POINT('Ctrl Pts',(-15.1446091167616,12.4188218900739,
133.445686307793)) ;
#133178 = CARTESIAN_POINT('Ctrl Pts',(-15.2365998734713,12.5668341062151,
133.681113263233)) ;
#133179 = CARTESIAN_POINT('Ctrl Pts',(-15.3120455807105,12.7739565310488,
133.868616342754)) ;
#133180 = CARTESIAN_POINT('Ctrl Pts',(-15.3679671650309,13.0292275295923,
133.998784482597)) ;
#133181 = CARTESIAN_POINT('Ctrl Pts',(-15.4001513908772,13.3121167714202,
134.059708256056)) ;
#133182 = CARTESIAN_POINT('Ctrl Pts',(-15.407302294284,13.6036711588795,134.047415072482)) ;
#133183 = CARTESIAN_POINT('Ctrl Pts',(-15.3894117903854,13.8822010088686,
133.961971555951)) ;
#133184 = CARTESIAN_POINT('Ctrl Pts',(-15.3488581880954,14.126534024312,133.810499271449)) ;
#133185 = CARTESIAN_POINT('Ctrl Pts',(-15.2890058404676,14.3215277156221,
133.602541497692)) ;
#133186 = CARTESIAN_POINT('Ctrl Pts',(-15.2146261037101,14.4523872469144,
133.352036701433)) ;
#133187 = CARTESIAN_POINT('Ctrl Pts',(-15.132276398967,14.509081269933,133.078352393805)) ;
#133188 = CARTESIAN_POINT('Ctrl Pts',(-15.048156334803,14.4877530584647,132.799404216537)) ;
#133189 = CARTESIAN_POINT('Ctrl Pts',(-14.9697741972722,14.3906972492053,
132.537447195776)) ;
#133190 = CARTESIAN_POINT('Ctrl Pts',(-14.9025432118204,14.2242127265294,
132.307919886886)) ;
#133191 = CARTESIAN_POINT('Ctrl Pts',(-14.8524134830202,14.0000453961231,
132.128331876439)) ;
#133192 = CARTESIAN_POINT('Ctrl Pts',(-14.8236827135926,13.7349941187306,
132.011308130338)) ;
#133193 = CARTESIAN_POINT('Ctrl Pts',(-14.8192110157222,13.4462938086935,
131.964998461715)) ;
#133194 = CARTESIAN_POINT('Ctrl Pts',(-14.8397608257614,13.1586524064852,
131.992109164985)) ;
#133195 = CARTESIAN_POINT('Ctrl Pts',(-14.8852506544382,12.8863235925418,
132.091631205511)) ;
#133196 = CARTESIAN_POINT('Ctrl Pts',(-14.952306886852,12.6553854575325,132.254505839022)) ;
#133197 = CARTESIAN_POINT('Ctrl Pts',(-15.036993538522,12.4787538591612,132.468885463633)) ;
#133198 = CARTESIAN_POINT('Ctrl Pts',(-15.1351325127102,12.3688114822916,
132.722256615459)) ;
#133199 = CARTESIAN_POINT('Ctrl Pts',(-15.2387002100067,12.3354319136936,
132.991765834986)) ;
#133200 = CARTESIAN_POINT('Ctrl Pts',(-15.3419020299315,12.3792576310417,
133.260178529464)) ;
#133201 = CARTESIAN_POINT('Ctrl Pts',(-15.4385746866519,12.4988398999205,
133.509304414363)) ;
#133202 = CARTESIAN_POINT('Ctrl Pts',(-15.5211785051019,12.6835118512005,
133.71760539492)) ;
#133203 = CARTESIAN_POINT('Ctrl Pts',(-15.585614912484,12.9214923912795,133.872725040323)) ;
#133204 = CARTESIAN_POINT('Ctrl Pts',(-15.6276593796861,13.1954916424955,
133.96242929729)) ;
#133205 = CARTESIAN_POINT('Ctrl Pts',(-15.6450448286836,13.4865485670219,
133.980012149667)) ;
#133206 = CARTESIAN_POINT('Ctrl Pts',(-15.6370948847114,13.772471589557,133.923647448758)) ;
#133207 = CARTESIAN_POINT('Ctrl Pts',(-15.6054576941134,14.0322259092952,
133.798239163953)) ;
#133208 = CARTESIAN_POINT('Ctrl Pts',(-15.5528532090993,14.2496185339524,
133.611440842472)) ;
#133209 = CARTESIAN_POINT('Ctrl Pts',(-15.483617346609,14.4079186586772,133.375986031408)) ;
#133210 = CARTESIAN_POINT('Ctrl Pts',(-15.4040148005417,14.495128940057,133.110405781656)) ;
#133211 = CARTESIAN_POINT('Ctrl Pts',(-15.3198980850125,14.5060206783235,
132.831544484233)) ;
#133212 = CARTESIAN_POINT('Ctrl Pts',(-15.2380342056834,14.4388851972431,
132.55918054693)) ;
#133213 = CARTESIAN_POINT('Ctrl Pts',(-15.1654389797841,14.2990479598781,
132.313981427395)) ;
#133214 = CARTESIAN_POINT('Ctrl Pts',(-15.107816605712,14.096277092635,132.112499036057)) ;
#133215 = CARTESIAN_POINT('Ctrl Pts',(-15.0701124492741,13.8463552274942,
131.969338122834)) ;
#133216 = CARTESIAN_POINT('Ctrl Pts',(-15.05554407707,13.5643762793268,131.893541407323)) ;
#133217 = CARTESIAN_POINT('Ctrl Pts',(-15.0659585050918,13.2747380866486,
131.891020251149)) ;
#133218 = CARTESIAN_POINT('Ctrl Pts',(-15.101446630055,12.9934296976024,131.961474427387)) ;
#133219 = CARTESIAN_POINT('Ctrl Pts',(-15.1601039100246,12.7438068041656,
132.099715492444)) ;
#133220 = CARTESIAN_POINT('Ctrl Pts',(-15.2384724882155,12.5426943442427,
132.295520501906)) ;
#133221 = CARTESIAN_POINT('Ctrl Pts',(-15.3316626347415,12.4046936236787,
132.534630966333)) ;
#133222 = CARTESIAN_POINT('Ctrl Pts',(-15.4337983976848,12.3396331759052,
132.799852893319)) ;
#133223 = CARTESIAN_POINT('Ctrl Pts',(-15.5380451833256,12.3522550875064,
133.071297592341)) ;
#133224 = CARTESIAN_POINT('Ctrl Pts',(-15.6378149553019,12.441158614988,133.329684714748)) ;
#133225 = CARTESIAN_POINT('Ctrl Pts',(-15.7271824288003,12.6013769713038,
133.55749869446)) ;
#133226 = CARTESIAN_POINT('Ctrl Pts',(-15.799387164279,12.819071640269,133.735430014399)) ;
#133227 = CARTESIAN_POINT('Ctrl Pts',(-15.8509954325536,13.0807346140254,
133.853055281245)) ;
#133228 = CARTESIAN_POINT('Ctrl Pts',(-15.8785701981475,13.3675408612144,
133.900413861765)) ;
#133229 = CARTESIAN_POINT('Ctrl Pts',(-15.880950069095,13.6570979280699,133.874320504545)) ;
#133230 = CARTESIAN_POINT('Ctrl Pts',(-15.8584614917164,13.9319893911641,
133.775308859387)) ;
#133231 = CARTESIAN_POINT('Ctrl Pts',(-15.8140300794619,14.1676085258846,
133.612576918087)) ;
#133232 = CARTESIAN_POINT('Ctrl Pts',(-15.7508365618172,14.3519029604138,
133.394745430706)) ;
#133233 = CARTESIAN_POINT('Ctrl Pts',(-15.6747542377325,14.4687263868581,
133.139424327783)) ;
#133234 = CARTESIAN_POINT('Ctrl Pts',(-15.5916310901521,14.5110206744739,
132.86348513324)) ;
#133235 = CARTESIAN_POINT('Ctrl Pts',(-15.5082277554707,14.4754839101951,
132.586740900539)) ;
#133236 = CARTESIAN_POINT('Ctrl Pts',(-15.4310148106346,14.3641243881349,
132.327975519891)) ;
#133237 = CARTESIAN_POINT('Ctrl Pts',(-15.366796148105,14.1859981150162,132.10732571318)) ;
#133238 = CARTESIAN_POINT('Ctrl Pts',(-15.3203690301936,13.9527739629267,
131.938549874937)) ;
#133239 = CARTESIAN_POINT('Ctrl Pts',(-15.2960642034895,13.6818171869407,
131.83443758756)) ;
#133240 = CARTESIAN_POINT('Ctrl Pts',(-15.2962284106988,13.3923456599437,
131.801803057666)) ;
#133241 = CARTESIAN_POINT('Ctrl Pts',(-15.3217088635482,13.1044625348289,
131.843052348479)) ;
#133242 = CARTESIAN_POINT('Ctrl Pts',(-15.3712895624886,12.8400820200563,
131.954780479996)) ;
#133243 = CARTESIAN_POINT('Ctrl Pts',(-15.4421215709794,12.6174283224968,
132.128595071256)) ;
#133244 = CARTESIAN_POINT('Ctrl Pts',(-15.5300656767636,12.4521814963559,
132.352341736955)) ;
#133245 = CARTESIAN_POINT('Ctrl Pts',(-15.6293654089259,12.3567835155047,
132.609283754024)) ;
#133246 = CARTESIAN_POINT('Ctrl Pts',(-15.7333497867975,12.3377092271658,
132.880009523703)) ;
#133247 = CARTESIAN_POINT('Ctrl Pts',(-15.8360089773108,12.3962076032604,
133.146742886939)) ;
#133248 = CARTESIAN_POINT('Ctrl Pts',(-15.930453723468,12.5290432373042,133.389409066584)) ;
#133249 = CARTESIAN_POINT('Ctrl Pts',(-16.009869584066,12.7244085230837,133.588441629327)) ;
#133250 = CARTESIAN_POINT('Ctrl Pts',(-16.0704566796156,12.9709500550387,
133.732258312717)) ;
#133251 = CARTESIAN_POINT('Ctrl Pts',(-16.1079755146477,13.2494402817627,
133.808760193825)) ;
#133252 = CARTESIAN_POINT('Ctrl Pts',(-16.1205567949924,13.5418967084717,
133.812230503726)) ;
#133253 = CARTESIAN_POINT('Ctrl Pts',(-16.1080660019669,13.8230883914708,
133.742789063125)) ;
#133254 = CARTESIAN_POINT('Ctrl Pts',(-16.0720612901439,14.0775910910953,
133.604421793909)) ;
#133255 = CARTESIAN_POINT('Ctrl Pts',(-16.016031312662,14.2842118886259,133.407692540579)) ;
#133256 = CARTESIAN_POINT('Ctrl Pts',(-15.9444811188164,14.4299775435325,
133.165534218954)) ;
#133257 = CARTESIAN_POINT('Ctrl Pts',(-15.8629277653847,14.503331032243,132.894001914259)) ;
#133258 = CARTESIAN_POINT('Ctrl Pts',(-15.7793496289803,14.4992417837061,
132.616952244808)) ;
#133259 = CARTESIAN_POINT('Ctrl Pts',(-15.6984734089822,14.4177939822546,
132.347381532007)) ;
#133260 = CARTESIAN_POINT('Ctrl Pts',(-15.6283650852396,14.2650806147523,
132.109470216545)) ;
#133261 = CARTESIAN_POINT('Ctrl Pts',(-15.5743268050137,14.0529681509037,
131.918590385591)) ;
#133262 = CARTESIAN_POINT('Ctrl Pts',(-15.5406403700371,13.7955270319932,
131.787101135372)) ;
#133263 = CARTESIAN_POINT('Ctrl Pts',(-15.5306638256876,13.5095709535078,
131.724666349948)) ;
#133264 = CARTESIAN_POINT('Ctrl Pts',(-15.5460171831695,13.2189036520177,
131.736403340103)) ;
#133265 = CARTESIAN_POINT('Ctrl Pts',(-15.5859137154081,12.9437120966298,
131.819943466577)) ;
#133266 = CARTESIAN_POINT('Ctrl Pts',(-15.6485475179313,12.7018113312773,
131.969792071976)) ;
#133267 = CARTESIAN_POINT('Ctrl Pts',(-15.7301725881226,12.5115374792667,
132.175093619939)) ;
#133268 = CARTESIAN_POINT('Ctrl Pts',(-15.8255194984171,12.3865362509785,
132.420501324227)) ;
#133269 = CARTESIAN_POINT('Ctrl Pts',(-15.9289904176059,12.3360647683775,
132.689500393083)) ;
#133270 = CARTESIAN_POINT('Ctrl Pts',(-16.0322109432962,12.3630945002041,
132.958176956719)) ;
#133271 = CARTESIAN_POINT('Ctrl Pts',(-16.1310535797055,12.4665769548229,
133.213630713827)) ;
#133272 = CARTESIAN_POINT('Ctrl Pts',(-16.2171162898203,12.637873730405,133.432016347732)) ;
#133273 = CARTESIAN_POINT('Ctrl Pts',(-16.2861070614099,12.8661806742055,
133.600365416687)) ;
#133274 = CARTESIAN_POINT('Ctrl Pts',(-16.3331577984964,13.1333277515124,
133.704775971435)) ;
#133275 = CARTESIAN_POINT('Ctrl Pts',(-16.3560616077762,13.4221934836715,
133.738517459493)) ;
#133276 = CARTESIAN_POINT('Ctrl Pts',(-16.3536937500244,13.7107571318464,
133.698487549138)) ;
#133277 = CARTESIAN_POINT('Ctrl Pts',(-16.3267795290435,13.9798563780996,
133.58659147111)) ;
#133278 = CARTESIAN_POINT('Ctrl Pts',(-16.2784408821239,14.2070905580459,
133.412375341533)) ;
#133279 = CARTESIAN_POINT('Ctrl Pts',(-16.2125397227886,14.3790287482914,
133.186748864503)) ;
#133280 = CARTESIAN_POINT('Ctrl Pts',(-16.1346594708171,14.4826462514907,
132.926162382995)) ;
#133281 = CARTESIAN_POINT('Ctrl Pts',(-16.0504302213959,14.5101765749395,
132.646782279628)) ;
#133282 = CARTESIAN_POINT('Ctrl Pts',(-15.9682674268405,14.4602521093363,
132.373878730922)) ;
#133283 = CARTESIAN_POINT('Ctrl Pts',(-15.892694390541,14.3349863303821,132.119771873462)) ;
#133284 = CARTESIAN_POINT('Ctrl Pts',(-15.8317129503708,14.1459036519263,
131.908681279387)) ;
#133285 = CARTESIAN_POINT('Ctrl Pts',(-15.7891216920241,13.9042674567381,
131.751109063095)) ;
#133286 = CARTESIAN_POINT('Ctrl Pts',(-15.7692741641614,13.6274934121279,
131.659929127433)) ;
#133287 = CARTESIAN_POINT('Ctrl Pts',(-15.774240842792,13.3375401227482,131.641402457855)) ;
#133288 = CARTESIAN_POINT('Ctrl Pts',(-15.8042482653973,13.0529656397982,
131.695949415826)) ;
#133289 = CARTESIAN_POINT('Ctrl Pts',(-15.8584516986935,12.793542004979,131.820979830249)) ;
#133290 = CARTESIAN_POINT('Ctrl Pts',(-15.9326864597706,12.5815361452067,
132.004842248444)) ;
#133291 = CARTESIAN_POINT('Ctrl Pts',(-16.0230837910625,12.4287258471182,
132.235797836759)) ;
#133292 = CARTESIAN_POINT('Ctrl Pts',(-16.1240643432101,12.3470719994747,
132.497574210549)) ;
#133293 = CARTESIAN_POINT('Ctrl Pts',(-16.2285925774014,12.3430683223392,
132.769776197563)) ;
#133294 = CARTESIAN_POINT('Ctrl Pts',(-16.3294552263757,12.4155936091128,
133.031491197843)) ;
#133295 = CARTESIAN_POINT('Ctrl Pts',(-16.42158697565,12.5608875783812,133.267432939441)) ;
#133296 = CARTESIAN_POINT('Ctrl Pts',(-16.4979791687381,12.7672957855937,
133.457539227448)) ;
#133297 = CARTESIAN_POINT('Ctrl Pts',(-16.5545469684218,13.0219896288371,
133.589546147221)) ;
#133298 = CARTESIAN_POINT('Ctrl Pts',(-16.5873216769804,13.3035436342973,
133.652289558074)) ;
#133299 = CARTESIAN_POINT('Ctrl Pts',(-16.5952372158022,13.5948422510341,
133.642264450776)) ;
#133300 = CARTESIAN_POINT('Ctrl Pts',(-16.5781262828345,13.8739529691167,
133.559117325056)) ;
#133301 = CARTESIAN_POINT('Ctrl Pts',(-16.5380768677347,14.1203174233417,
133.409012301568)) ;
#133302 = CARTESIAN_POINT('Ctrl Pts',(-16.4787184094645,14.3167168643634,
133.20251930448)) ;
#133303 = CARTESIAN_POINT('Ctrl Pts',(-16.4048795075091,14.4494066861711,
132.953678390524)) ;
#133304 = CARTESIAN_POINT('Ctrl Pts',(-16.3225697948458,14.5084702688582,
132.680063070833)) ;
#133305 = CARTESIAN_POINT('Ctrl Pts',(-16.2386731326133,14.489700746972,132.401879914645)) ;
#133306 = CARTESIAN_POINT('Ctrl Pts',(-16.159666302226,14.3946106074975,132.13794942029)) ;
#133307 = CARTESIAN_POINT('Ctrl Pts',(-16.0919372674924,14.2294635345246,
131.906906848158)) ;
#133308 = CARTESIAN_POINT('Ctrl Pts',(-16.0414142644033,14.0073333887475,
131.726263966149)) ;
#133309 = CARTESIAN_POINT('Ctrl Pts',(-16.0120005571222,13.7435828448799,
131.607279354952)) ;
#133310 = CARTESIAN_POINT('Ctrl Pts',(-16.0067413555039,13.454824745877,131.558621231445)) ;
#133311 = CARTESIAN_POINT('Ctrl Pts',(-16.0266816029947,13.1663898496403,
131.58388276017)) ;
#133312 = CARTESIAN_POINT('Ctrl Pts',(-16.071174096646,12.8948251888563,131.680693404511)) ;
#133313 = CARTESIAN_POINT('Ctrl Pts',(-16.1378143759152,12.6613614393991,
131.842219614895)) ;
#133314 = CARTESIAN_POINT('Ctrl Pts',(-16.2222899580583,12.4827884864443,
132.055914031115)) ;
#133315 = CARTESIAN_POINT('Ctrl Pts',(-16.3195947643377,12.3713198999723,
132.307032186213)) ;
#133316 = CARTESIAN_POINT('Ctrl Pts',(-16.42316155049,12.3351536539427,132.576506572357)) ;
#133317 = CARTESIAN_POINT('Ctrl Pts',(-16.5269587087536,12.3771106003778,
132.846499102918)) ;
#133318 = CARTESIAN_POINT('Ctrl Pts',(-16.6232634802675,12.493746042562,133.094781650953)) ;
#133319 = CARTESIAN_POINT('Ctrl Pts',(-16.7066715515362,12.6767291405437,
133.30534152523)) ;
#133320 = CARTESIAN_POINT('Ctrl Pts',(-16.7719969184263,12.9147362953278,
133.462888792416)) ;
#133321 = CARTESIAN_POINT('Ctrl Pts',(-16.8145117924752,13.1870897175325,
133.554081812245)) ;
#133322 = CARTESIAN_POINT('Ctrl Pts',(-16.832664410647,13.4771402294594,133.573993886311)) ;
#133323 = CARTESIAN_POINT('Ctrl Pts',(-16.8255195547471,13.7642376991577,
133.519905575425)) ;
#133324 = CARTESIAN_POINT('Ctrl Pts',(-16.7943070458963,14.0261140050281,
133.395578546783)) ;
#133325 = CARTESIAN_POINT('Ctrl Pts',(-16.7424882598997,14.2437566095146,
133.211251228587)) ;
#133326 = CARTESIAN_POINT('Ctrl Pts',(-16.6736113908412,14.4043004510961,
132.976804095223)) ;
#133327 = CARTESIAN_POINT('Ctrl Pts',(-16.5942186823598,14.4936451763547,
132.711836822872)) ;
#133328 = CARTESIAN_POINT('Ctrl Pts',(-16.5101466580755,14.5067755223083,
132.433108081231)) ;
#133329 = CARTESIAN_POINT('Ctrl Pts',(-16.4282410882398,14.4421251633059,
132.160681842967)) ;
#133330 = CARTESIAN_POINT('Ctrl Pts',(-16.3551632521983,14.3039891726026,
131.914003956164)) ;
#133331 = CARTESIAN_POINT('Ctrl Pts',(-16.2972497108617,14.1040922169467,
131.711842779145)) ;
#133332 = CARTESIAN_POINT('Ctrl Pts',(-16.2585983326173,13.8535852347893,
131.565668552377)) ;
#133333 = CARTESIAN_POINT('Ctrl Pts',(-16.243420453165,13.5730952435811,131.488208101679)) ;
#133334 = CARTESIAN_POINT('Ctrl Pts',(-16.2531006198612,13.2829861782011,
131.483481649537)) ;
#133335 = CARTESIAN_POINT('Ctrl Pts',(-16.2877661805878,13.0017737284941,
131.551621835108)) ;
#133336 = CARTESIAN_POINT('Ctrl Pts',(-16.3459738367156,12.7500890797144,
131.688431825914)) ;
#133337 = CARTESIAN_POINT('Ctrl Pts',(-16.4238184818004,12.5475577998432,
131.882729415997)) ;
#133338 = CARTESIAN_POINT('Ctrl Pts',(-16.5167586194788,12.4075652478031,
132.121078295711)) ;
#133339 = CARTESIAN_POINT('Ctrl Pts',(-16.6183907518262,12.3405227377109,
132.384938789592)) ;
#133340 = CARTESIAN_POINT('Ctrl Pts',(-16.7229364475564,12.3506975715296,
132.657173213167)) ;
#133341 = CARTESIAN_POINT('Ctrl Pts',(-16.8232859030364,12.438177489278,132.917122022405)) ;
#133342 = CARTESIAN_POINT('Ctrl Pts',(-16.9125712124386,12.5958827964123,
133.1448620791)) ;
#133343 = CARTESIAN_POINT('Ctrl Pts',(-16.9854582743437,12.8123887822574,
133.324729525533)) ;
#133344 = CARTESIAN_POINT('Ctrl Pts',(-17.037709893631,13.0732934241726,133.444215844693)) ;
#133345 = CARTESIAN_POINT('Ctrl Pts',(-17.0659638164382,13.3601444544887,
133.493509177191)) ;
#133346 = CARTESIAN_POINT('Ctrl Pts',(-17.0689675284249,13.6487324697402,
133.469363185352)) ;
#133347 = CARTESIAN_POINT('Ctrl Pts',(-17.0474035047278,13.9231969052117,
133.37321432911)) ;
#133348 = CARTESIAN_POINT('Ctrl Pts',(-17.0033733673897,14.1616648845749,
133.211459633651)) ;
#133349 = CARTESIAN_POINT('Ctrl Pts',(-16.9406158991401,14.3474885130478,
132.994912465869)) ;
#133350 = CARTESIAN_POINT('Ctrl Pts',(-16.864876505793,14.4664584587802,132.740606759249)) ;
#133351 = CARTESIAN_POINT('Ctrl Pts',(-16.7814776117931,14.5109046603937,
132.463712586271)) ;
#133352 = CARTESIAN_POINT('Ctrl Pts',(-16.6983907346783,14.477538406395,132.188050973166)) ;
#133353 = CARTESIAN_POINT('Ctrl Pts',(-16.6207705482251,14.3681997132881,
131.928042842248)) ;
#133354 = CARTESIAN_POINT('Ctrl Pts',(-16.5561356079281,14.19161807787,131.706168442298)) ;
#133355 = CARTESIAN_POINT('Ctrl Pts',(-16.5092308734292,13.9603524956053,
131.536079167786)) ;
#133356 = CARTESIAN_POINT('Ctrl Pts',(-16.4841796106604,13.6895220911817,
131.429699941359)) ;
#133357 = CARTESIAN_POINT('Ctrl Pts',(-16.4836919093705,13.4007319641459,
131.395211960917)) ;
#133358 = CARTESIAN_POINT('Ctrl Pts',(-16.5082964988508,13.1132078283894,
131.433992211526)) ;
#133359 = CARTESIAN_POINT('Ctrl Pts',(-16.5574784700436,12.8466068578935,
131.544388229293)) ;
#133360 = CARTESIAN_POINT('Ctrl Pts',(-16.6273997075169,12.6236984730367,
131.715716955648)) ;
#133361 = CARTESIAN_POINT('Ctrl Pts',(-16.7150468521775,12.4561011970055,
131.938529922164)) ;
#133362 = CARTESIAN_POINT('Ctrl Pts',(-16.8139682824648,12.3585968124196,
132.194412407875)) ;
#133363 = CARTESIAN_POINT('Ctrl Pts',(-16.9182265147246,12.3371246735504,
132.465833558649)) ;
#133364 = CARTESIAN_POINT('Ctrl Pts',(-17.0209026074425,12.3935413485491,
132.732653318412)) ;
#133365 = CARTESIAN_POINT('Ctrl Pts',(-17.1153756443262,12.5236723848828,
132.975519307564)) ;
#133366 = CARTESIAN_POINT('Ctrl Pts',(-17.1956555914022,12.7179304240541,
133.176947444366)) ;
#133367 = CARTESIAN_POINT('Ctrl Pts',(-17.2569924030211,12.9643000603806,
133.322838842009)) ;
#133368 = CARTESIAN_POINT('Ctrl Pts',(-17.2949538933717,13.2410161239663,
133.400773057716)) ;
#133369 = CARTESIAN_POINT('Ctrl Pts',(-17.3083412632257,13.5320326358814,
133.40675253041)) ;
#133370 = CARTESIAN_POINT('Ctrl Pts',(-17.2965889183178,13.8151976332958,
133.339306952295)) ;
#133371 = CARTESIAN_POINT('Ctrl Pts',(-17.2611712342104,14.070965110173,133.202631251777)) ;
#133372 = CARTESIAN_POINT('Ctrl Pts',(-17.2055219190199,14.2795161854134,
133.006946181317)) ;
#133373 = CARTESIAN_POINT('Ctrl Pts',(-17.1344526197165,14.4266233568165,
132.766264881813)) ;
#133374 = CARTESIAN_POINT('Ctrl Pts',(-17.0535835623515,14.5021444966585,
132.496922447555)) ;
#133375 = CARTESIAN_POINT('Ctrl Pts',(-16.9693534559784,14.5004799279669,
132.217713549754)) ;
#133376 = CARTESIAN_POINT('Ctrl Pts',(-16.8885085804287,14.4210758361391,
131.948320350664)) ;
#133377 = CARTESIAN_POINT('Ctrl Pts',(-16.818249196986,14.2711637356508,131.710095463003)) ;
#133378 = CARTESIAN_POINT('Ctrl Pts',(-16.7633840110066,14.0600320259714,
131.516677712646)) ;
#133379 = CARTESIAN_POINT('Ctrl Pts',(-16.729034656478,13.8025046463563,131.383125760343)) ;
#133380 = CARTESIAN_POINT('Ctrl Pts',(-16.7184105236858,13.5194350300881,
131.319077858953)) ;
#133381 = CARTESIAN_POINT('Ctrl Pts',(-16.7329082611137,13.227929848522,131.328230796269)) ;
#133382 = CARTESIAN_POINT('Ctrl Pts',(-16.7721540100418,12.9514279979351,
131.409809044102)) ;
#133383 = CARTESIAN_POINT('Ctrl Pts',(-16.834426980546,12.7076270254922,131.558495828173)) ;
#133384 = CARTESIAN_POINT('Ctrl Pts',(-16.9152315370478,12.5164543914562,
131.761543944961)) ;
#133385 = CARTESIAN_POINT('Ctrl Pts',(-17.0104958015721,12.3891143889345,
132.006622580848)) ;
#133386 = CARTESIAN_POINT('Ctrl Pts',(-17.1132917121907,12.3364756158918,
132.273826383176)) ;
#133387 = CARTESIAN_POINT('Ctrl Pts',(-17.2173332534644,12.3612642231578,
132.54465957405)) ;
#133388 = CARTESIAN_POINT('Ctrl Pts',(-17.3163641429157,12.4629838840005,
132.800676032605)) ;
#133389 = CARTESIAN_POINT('Ctrl Pts',(-17.4026407183266,12.6321971699934,
133.01975282772)) ;
#133390 = CARTESIAN_POINT('Ctrl Pts',(-17.472100457449,12.8584558798932,133.189548524182)) ;
#133391 = CARTESIAN_POINT('Ctrl Pts',(-17.5200564206003,13.1261648647243,
133.296424663186)) ;
#133392 = CARTESIAN_POINT('Ctrl Pts',(-17.5435329958318,13.4141234552309,
133.331916813786)) ;
#133393 = CARTESIAN_POINT('Ctrl Pts',(-17.5418705107985,13.7023852342343,
133.294006470842)) ;
#133394 = CARTESIAN_POINT('Ctrl Pts',(-17.515866367185,13.9714212012371,133.184910655295)) ;
#133395 = CARTESIAN_POINT('Ctrl Pts',(-17.4677121548387,14.202020081249,133.01095053406)) ;
#133396 = CARTESIAN_POINT('Ctrl Pts',(-17.4023716167183,14.3750071736422,
132.787065724901)) ;
#133397 = CARTESIAN_POINT('Ctrl Pts',(-17.3247668097447,14.4806351346196,
132.527282453733)) ;
#133398 = CARTESIAN_POINT('Ctrl Pts',(-17.2410054869792,14.5105855297535,
132.24943004058)) ;
#133399 = CARTESIAN_POINT('Ctrl Pts',(-17.1581501091636,14.4625550657111,
131.974268906069)) ;
#133400 = CARTESIAN_POINT('Ctrl Pts',(-17.0827332780509,14.3400369417443,
131.720826863696)) ;
#133401 = CARTESIAN_POINT('Ctrl Pts',(-17.0209888868574,14.1521957535254,
131.507380128005)) ;
#133402 = CARTESIAN_POINT('Ctrl Pts',(-16.9778207788142,13.9116489154345,
131.348115653949)) ;
#133403 = CARTESIAN_POINT('Ctrl Pts',(-16.9572990580186,13.6358544266559,
131.25499330384)) ;
#133404 = CARTESIAN_POINT('Ctrl Pts',(-16.9615071381463,13.3459427675745,
131.23424300822)) ;
#133405 = CARTESIAN_POINT('Ctrl Pts',(-16.9909211180614,13.0604649745041,
131.286996740778)) ;
#133406 = CARTESIAN_POINT('Ctrl Pts',(-17.0441007990242,12.8015143832803,
131.409241549806)) ;
#133407 = CARTESIAN_POINT('Ctrl Pts',(-17.1180304186239,12.586871423154,131.592073079015)) ;
#133408 = CARTESIAN_POINT('Ctrl Pts',(-17.2080500636742,12.4323032180318,
131.821934768459)) ;
#133409 = CARTESIAN_POINT('Ctrl Pts',(-17.3084611337155,12.348604012381,132.082157360211)) ;
#133410 = CARTESIAN_POINT('Ctrl Pts',(-17.4130111461555,12.3418345254331,
132.3544143668)) ;
#133411 = CARTESIAN_POINT('Ctrl Pts',(-17.5146765749007,12.4127257697425,
132.618266949295)) ;
#133412 = CARTESIAN_POINT('Ctrl Pts',(-17.606721170884,12.5554430365515,132.854114383774)) ;
#133413 = CARTESIAN_POINT('Ctrl Pts',(-17.6839111619126,12.7608029240068,
133.046442139626)) ;
#133414 = CARTESIAN_POINT('Ctrl Pts',(-17.7410331806284,13.0143079229722,
133.180091411217)) ;
#133415 = CARTESIAN_POINT('Ctrl Pts',(-17.7745360164768,13.2953661026702,
133.244952941826)) ;
#133416 = CARTESIAN_POINT('Ctrl Pts',(-17.7831520054483,13.587499191953,133.236886150184)) ;
#133417 = CARTESIAN_POINT('Ctrl Pts',(-17.7666348632763,13.8669338626205,
133.155497022517)) ;
#133418 = CARTESIAN_POINT('Ctrl Pts',(-17.7273863718362,14.1134263503453,
133.007875421063)) ;
#133419 = CARTESIAN_POINT('Ctrl Pts',(-17.6683893078491,14.3121780897716,
132.802342611055)) ;
#133420 = CARTESIAN_POINT('Ctrl Pts',(-17.5946147982464,14.4470050265316,
132.553591742459)) ;
#133421 = CARTESIAN_POINT('Ctrl Pts',(-17.5125911040324,14.5078086325279,
132.280874384855)) ;
#133422 = CARTESIAN_POINT('Ctrl Pts',(-17.4289255794743,14.4913412737729,
132.003473976216)) ;
#133423 = CARTESIAN_POINT('Ctrl Pts',(-17.3497030184291,14.3985299043882,
131.738923406222)) ;
#133424 = CARTESIAN_POINT('Ctrl Pts',(-17.2814947859058,14.2353764928408,
131.506472748856)) ;
#133425 = CARTESIAN_POINT('Ctrl Pts',(-17.2301833982271,14.0132824388172,
131.32333677435)) ;
#133426 = CARTESIAN_POINT('Ctrl Pts',(-17.2003726149901,13.751770584179,131.203370984278)) ;
#133427 = CARTESIAN_POINT('Ctrl Pts',(-17.1942692410409,13.4639004603942,
131.15229798358)) ;
#133428 = CARTESIAN_POINT('Ctrl Pts',(-17.2136563233809,13.1736259559936,
131.175755585428)) ;
#133429 = CARTESIAN_POINT('Ctrl Pts',(-17.2572199771084,12.9029494351804,
131.270058586451)) ;
#133430 = CARTESIAN_POINT('Ctrl Pts',(-17.3234518657098,12.6670694829694,
131.430263375814)) ;
#133431 = CARTESIAN_POINT('Ctrl Pts',(-17.4076950363158,12.4867414535482,
131.643224441991)) ;
#133432 = CARTESIAN_POINT('Ctrl Pts',(-17.5042594533731,12.3736046950475,
131.892333562312)) ;
#133433 = CARTESIAN_POINT('Ctrl Pts',(-17.6083225797878,12.3351061359291,
132.163067552705)) ;
#133434 = CARTESIAN_POINT('Ctrl Pts',(-17.7115102747659,12.3747297412366,
132.431506046747)) ;
#133435 = CARTESIAN_POINT('Ctrl Pts',(-17.80835655534,12.4890530273647,132.681306942846)) ;
#133436 = CARTESIAN_POINT('Ctrl Pts',(-17.8927139370083,12.6718473822343,
132.894413198474)) ;
#133437 = CARTESIAN_POINT('Ctrl Pts',(-17.9581348743092,12.9071471042355,
133.05245843071)) ;
#133438 = CARTESIAN_POINT('Ctrl Pts',(-18.0014489044881,13.1791583633753,
133.145922177929)) ;
#133439 = CARTESIAN_POINT('Ctrl Pts',(-18.020261151911,13.4685703303894,133.16781609884)) ;
#133440 = CARTESIAN_POINT('Ctrl Pts',(-18.0138792132709,13.7556865610863,
133.115998787948)) ;
#133441 = CARTESIAN_POINT('Ctrl Pts',(-17.9834392562243,14.0184520779736,
132.993960277943)) ;
#133442 = CARTESIAN_POINT('Ctrl Pts',(-17.9319093006337,14.2386835545227,
132.810307624848)) ;
#133443 = CARTESIAN_POINT('Ctrl Pts',(-17.8634196060343,14.4009245247973,
132.577005577925)) ;
#133444 = CARTESIAN_POINT('Ctrl Pts',(-17.7839956342627,14.4923209079493,
132.311848278652)) ;
#133445 = CARTESIAN_POINT('Ctrl Pts',(-17.7003715420016,14.5074993821674,
132.034597515729)) ;
#133446 = CARTESIAN_POINT('Ctrl Pts',(-17.6179715693461,14.4446391320812,
131.760580504429)) ;
#133447 = CARTESIAN_POINT('Ctrl Pts',(-17.5449472629492,14.309013886893,131.514230915999)) ;
#133448 = CARTESIAN_POINT('Ctrl Pts',(-17.4863929079662,14.1104149351794,
131.310125649846)) ;
#133449 = CARTESIAN_POINT('Ctrl Pts',(-17.4472233098488,13.8614588559076,
131.162498832848)) ;
#133450 = CARTESIAN_POINT('Ctrl Pts',(-17.4312869960412,13.5819687002437,
131.082859767227)) ;
#133451 = CARTESIAN_POINT('Ctrl Pts',(-17.4402797073093,13.2906279013141,
131.075985151787)) ;
#133452 = CARTESIAN_POINT('Ctrl Pts',(-17.4743143198391,13.009243305788,131.142317233284)) ;
#133453 = CARTESIAN_POINT('Ctrl Pts',(-17.5315517099284,12.7575168112921,
131.276452625469)) ;
#133454 = CARTESIAN_POINT('Ctrl Pts',(-17.6091410096472,12.5525240138587,
131.469879021206)) ;
#133455 = CARTESIAN_POINT('Ctrl Pts',(-17.7014737885802,12.4108770336832,
131.706544893167)) ;
#133456 = CARTESIAN_POINT('Ctrl Pts',(-17.8032831969416,12.3412909140522,
131.97080490142)) ;
#133457 = CARTESIAN_POINT('Ctrl Pts',(-17.9077079735701,12.3493861735078,
132.242732393973)) ;
#133458 = CARTESIAN_POINT('Ctrl Pts',(-18.0080021312736,12.4342727909203,
132.502613425746)) ;
#133459 = CARTESIAN_POINT('Ctrl Pts',(-18.097851259794,12.5900489009072,132.731956223757)) ;
#133460 = CARTESIAN_POINT('Ctrl Pts',(-18.1714811565311,12.8056265995217,
132.913906681068)) ;
#133461 = CARTESIAN_POINT('Ctrl Pts',(-18.2242791522083,13.0653848746049,
133.035014327401)) ;
#133462 = CARTESIAN_POINT('Ctrl Pts',(-18.2532373491338,13.3504851063388,
133.086511791274)) ;
#133463 = CARTESIAN_POINT('Ctrl Pts',(-18.2570176970517,13.6412798147236,
133.064399324168)) ;
#133464 = CARTESIAN_POINT('Ctrl Pts',(-18.2361288879767,13.915548156852,132.970331104728)) ;
#133465 = CARTESIAN_POINT('Ctrl Pts',(-18.1927521468012,14.1552942040558,
132.810491998612)) ;
#133466 = CARTESIAN_POINT('Ctrl Pts',(-18.1304889717146,14.3429101935435,
132.595396822877)) ;
#133467 = CARTESIAN_POINT('Ctrl Pts',(-18.0549535994053,14.4639893047867,
132.341644352442)) ;
#133468 = CARTESIAN_POINT('Ctrl Pts',(-17.9720169774795,14.5107279953385,
132.066239556179)) ;
#133469 = CARTESIAN_POINT('Ctrl Pts',(-17.88839874123,14.4794893752074,131.788842595817)) ;
#133470 = CARTESIAN_POINT('Ctrl Pts',(-17.8108656194136,14.3727211578977,
131.529246532274)) ;
#133471 = CARTESIAN_POINT('Ctrl Pts',(-17.7456151211965,14.1977799584113,
131.305501822006)) ;
#133472 = CARTESIAN_POINT('Ctrl Pts',(-17.6981151394564,13.9680803032242,
131.13369579038)) ;
#133473 = CARTESIAN_POINT('Ctrl Pts',(-17.6723054333923,13.6967826933105,
131.024941140418)) ;
#133474 = CARTESIAN_POINT('Ctrl Pts',(-17.6711447708163,13.4094043760888,
130.98862536116)) ;
#133475 = CARTESIAN_POINT('Ctrl Pts',(-17.6950445630246,13.1212039321583,
131.025303143358)) ;
#133476 = CARTESIAN_POINT('Ctrl Pts',(-17.74333311896,12.8546896237207,131.133221894845)) ;
#133477 = CARTESIAN_POINT('Ctrl Pts',(-17.81282756458,12.6293810356165,131.303196900116)) ;
#133478 = CARTESIAN_POINT('Ctrl Pts',(-17.9005194706817,12.4594635396626,
131.525988684649)) ;
#133479 = CARTESIAN_POINT('Ctrl Pts',(-17.9986989569018,12.3604529302704,
131.779876218196)) ;
#133480 = CARTESIAN_POINT('Ctrl Pts',(-18.1032340963646,12.3366695079855,
132.05199660503)) ;
#133481 = CARTESIAN_POINT('Ctrl Pts',(-18.2056125319901,12.3907630606801,
132.318086056791)) ;
#133482 = CARTESIAN_POINT('Ctrl Pts',(-18.300613364825,12.5187717527639,132.562441868016)) ;
#133483 = CARTESIAN_POINT('Ctrl Pts',(-18.3816465085652,12.7125553045139,
132.765918032423)) ;
#133484 = CARTESIAN_POINT('Ctrl Pts',(-18.4429853099616,12.9551208485313,
132.912159665352)) ;
#133485 = CARTESIAN_POINT('Ctrl Pts',(-18.4820336765163,13.2325620060974,
132.993078593711)) ;
#133486 = CARTESIAN_POINT('Ctrl Pts',(-18.496084383933,13.5243419796884,133.00090515124)) ;
#133487 = CARTESIAN_POINT('Ctrl Pts',(-18.4850639350324,13.8069926528057,
132.935714610325)) ;
#133488 = CARTESIAN_POINT('Ctrl Pts',(-18.4503367662865,14.0639000199269,
132.801056058483)) ;
#133489 = CARTESIAN_POINT('Ctrl Pts',(-18.3952268191814,14.2741558930926,
132.606941700926)) ;
#133490 = CARTESIAN_POINT('Ctrl Pts',(-18.3243680288223,14.4234615625839,
132.366801537788)) ;
#133491 = CARTESIAN_POINT('Ctrl Pts',(-18.2437816042926,14.5011170686614,
132.098327447916)) ;
#133492 = CARTESIAN_POINT('Ctrl Pts',(-18.1592384984199,14.5013614779113,
131.81807310291)) ;
#133493 = CARTESIAN_POINT('Ctrl Pts',(-18.0789307375107,14.4249956630962,
131.550560960519)) ;
#133494 = CARTESIAN_POINT('Ctrl Pts',(-18.0076541118125,14.2760171565871,
131.309082565097)) ;
#133495 = CARTESIAN_POINT('Ctrl Pts',(-17.9524899575172,14.0665442400002,
131.114862544505)) ;
#133496 = CARTESIAN_POINT('Ctrl Pts',(-17.9175014310239,13.8110528410318,
130.979547647309)) ;
#133497 = CARTESIAN_POINT('Ctrl Pts',(-17.9061688391216,13.5262786463887,
130.913174372637)) ;
#133498 = CARTESIAN_POINT('Ctrl Pts',(-17.919877948496,13.2368369901033,130.920277108179)) ;
#133499 = CARTESIAN_POINT('Ctrl Pts',(-17.9586197277239,12.9583255903659,
131.000212959745)) ;
#133500 = CARTESIAN_POINT('Ctrl Pts',(-18.0199083066583,12.7145800096232,
131.146219952724)) ;
#133501 = CARTESIAN_POINT('Ctrl Pts',(-18.1009974511921,12.5201730384604,
131.349794172582)) ;
#133502 = CARTESIAN_POINT('Ctrl Pts',(-18.1949562384929,12.392297716127,131.59141902566)) ;
#133503 = CARTESIAN_POINT('Ctrl Pts',(-18.2981754606917,12.3368042043637,
131.859663996403)) ;
#133504 = CARTESIAN_POINT('Ctrl Pts',(-18.4019398290045,12.3594079574846,
132.129799825424)) ;
#133505 = CARTESIAN_POINT('Ctrl Pts',(-18.5013383418749,12.4588426243277,
132.386856715267)) ;
#133506 = CARTESIAN_POINT('Ctrl Pts',(-18.5881323912535,12.6263832935465,
132.607414342136)) ;
#133507 = CARTESIAN_POINT('Ctrl Pts',(-18.6581587702516,12.8513078071139,
132.778854814353)) ;
#133508 = CARTESIAN_POINT('Ctrl Pts',(-18.7067345904951,13.1175341941134,
132.887608467018)) ;
#133509 = CARTESIAN_POINT('Ctrl Pts',(-18.731003412201,13.4059954970849,132.925314381533)) ;
#133510 = CARTESIAN_POINT('Ctrl Pts',(-18.7300968071152,13.6942419645787,
132.889656262388)) ;
#133511 = CARTESIAN_POINT('Ctrl Pts',(-18.7044541735128,13.9656571359195,
132.781395875164)) ;
#133512 = CARTESIAN_POINT('Ctrl Pts',(-18.6575265026644,14.1945698215837,
132.611470543872)) ;
#133513 = CARTESIAN_POINT('Ctrl Pts',(-18.5922406519204,14.3711224528334,
132.387486886082)) ;
#133514 = CARTESIAN_POINT('Ctrl Pts',(-18.5149037393986,14.4785950091488,
132.128508392993)) ;
#133515 = CARTESIAN_POINT('Ctrl Pts',(-18.4311371510558,14.5108133112394,
131.850601957705)) ;
#133516 = CARTESIAN_POINT('Ctrl Pts',(-18.3483146549276,14.4650394200622,
131.575598992863)) ;
#133517 = CARTESIAN_POINT('Ctrl Pts',(-18.2726066198908,14.3446919400874,
131.321313280288)) ;
#133518 = CARTESIAN_POINT('Ctrl Pts',(-18.2103307361537,14.1586507898245,
131.106307024848)) ;
#133519 = CARTESIAN_POINT('Ctrl Pts',(-18.1664432390162,13.9182142591253,
130.944795156692)) ;
#133520 = CARTESIAN_POINT('Ctrl Pts',(-18.1453636366719,13.6446894301756,
130.850233747273)) ;
#133521 = CARTESIAN_POINT('Ctrl Pts',(-18.1488348343508,13.3538163555555,
130.82719813754)) ;
#133522 = CARTESIAN_POINT('Ctrl Pts',(-18.1774811245967,13.0687529323482,
130.877811758373)) ;
#133523 = CARTESIAN_POINT('Ctrl Pts',(-18.2300437642224,12.8084025711039,
130.998208929724)) ;
#133524 = CARTESIAN_POINT('Ctrl Pts',(-18.3034001053734,12.5923662507696,
131.179384620874)) ;
#133525 = CARTESIAN_POINT('Ctrl Pts',(-18.3931634370597,12.4355966936421,
131.408445657945)) ;
#133526 = CARTESIAN_POINT('Ctrl Pts',(-18.4935575860177,12.3498834173245,
131.668562849344)) ;
#133527 = CARTESIAN_POINT('Ctrl Pts',(-18.5975530541275,12.3409542808635,
131.939369081028)) ;
#133528 = CARTESIAN_POINT('Ctrl Pts',(-18.6994673351223,12.4093757248112,
132.203931136602)) ;
#133529 = CARTESIAN_POINT('Ctrl Pts',(-18.7921201529756,12.5505196315372,
132.441467645947)) ;
#133530 = CARTESIAN_POINT('Ctrl Pts',(-18.8697017731338,12.7541803006072,
132.634971878383)) ;
#133531 = CARTESIAN_POINT('Ctrl Pts',(-18.9273307484839,13.0055267425044,
132.770220733639)) ;
#133532 = CARTESIAN_POINT('Ctrl Pts',(-18.9617100390982,13.2870724884799,
132.83751270461)) ;
#133533 = CARTESIAN_POINT('Ctrl Pts',(-18.9710255677151,13.5781354317469,
132.831615285865)) ;
#133534 = CARTESIAN_POINT('Ctrl Pts',(-18.9553578084607,13.8583662507443,
132.752702523973)) ;
#133535 = CARTESIAN_POINT('Ctrl Pts',(-18.9165383575917,14.1072755060793,
132.606171710367)) ;
#133536 = CARTESIAN_POINT('Ctrl Pts',(-18.8581587772242,14.3069765889331,
132.4025330216)) ;
#133537 = CARTESIAN_POINT('Ctrl Pts',(-18.7850681968336,14.443614067786,132.155907192059)) ;
#133538 = CARTESIAN_POINT('Ctrl Pts',(-18.702941141321,14.5071928082345,131.882773592227)) ;
#133539 = CARTESIAN_POINT('Ctrl Pts',(-18.6190408117616,14.4928945220509,
131.604612881179)) ;
#133540 = CARTESIAN_POINT('Ctrl Pts',(-18.5396187459799,14.4021254936154,
131.339485656911)) ;
#133541 = CARTESIAN_POINT('Ctrl Pts',(-18.4711933901986,14.2413770477371,
131.106496569037)) ;
#133542 = CARTESIAN_POINT('Ctrl Pts',(-18.4192605637911,14.0210258594474,
130.921552581758)) ;
#133543 = CARTESIAN_POINT('Ctrl Pts',(-18.3886405960536,13.7594508415378,
130.799092122936)) ;
#133544 = CARTESIAN_POINT('Ctrl Pts',(-18.381928462571,13.4716753030503,130.746210031867)) ;
#133545 = CARTESIAN_POINT('Ctrl Pts',(-18.4004216312574,13.18278007244,130.767242888151)) ;
#133546 = CARTESIAN_POINT('Ctrl Pts',(-18.4435339670258,12.9097866347109,
130.860039653288)) ;
#133547 = CARTESIAN_POINT('Ctrl Pts',(-18.5088204983959,12.6739761120234,
131.017674750893)) ;
#133548 = CARTESIAN_POINT('Ctrl Pts',(-18.5926770612546,12.4911376353209,
131.229439455072)) ;
#133549 = CARTESIAN_POINT('Ctrl Pts',(-18.6895108158381,12.3755758788311,
131.479159592622)) ;
#133550 = CARTESIAN_POINT('Ctrl Pts',(-18.7928542788589,12.3352662329562,
131.747989657394)) ;
#133551 = CARTESIAN_POINT('Ctrl Pts',(-18.8962659376777,12.3722006143293,
132.017051741353)) ;
#133552 = CARTESIAN_POINT('Ctrl Pts',(-18.9940984306609,12.4858118722087,
132.26946955847)) ;
#133553 = CARTESIAN_POINT('Ctrl Pts',(-19.0779483654093,12.6649628027199,
132.481462828409)) ;
#133554 = CARTESIAN_POINT('Ctrl Pts',(-19.144324386781,12.8995424291904,132.64216747859)) ;
#133555 = CARTESIAN_POINT('Ctrl Pts',(-19.1882893988472,13.1707489990253,
132.73754255469)) ;
#133556 = CARTESIAN_POINT('Ctrl Pts',(-19.2078747746244,13.4602465419289,
132.76165779285)) ;
#133557 = CARTESIAN_POINT('Ctrl Pts',(-19.2021695943243,13.7479094104328,
132.711797460233)) ;
#133558 = CARTESIAN_POINT('Ctrl Pts',(-19.1724541288044,14.0110933638022,
132.591943088721)) ;
#133559 = CARTESIAN_POINT('Ctrl Pts',(-19.1214789970609,14.2330195298938,
132.409891780119)) ;
#133560 = CARTESIAN_POINT('Ctrl Pts',(-19.0533824116154,14.397056415232,132.177734508543)) ;
#133561 = CARTESIAN_POINT('Ctrl Pts',(-18.9744610193818,14.4906410938832,
131.914150162339)) ;
#133562 = CARTESIAN_POINT('Ctrl Pts',(-18.890345578861,14.5080280130628,131.635247249356)) ;
#133563 = CARTESIAN_POINT('Ctrl Pts',(-18.8085392860132,14.4480725424633,
131.363277720596)) ;
#133564 = CARTESIAN_POINT('Ctrl Pts',(-18.7346273925197,14.3139470607326,
131.114108989611)) ;
#133565 = CARTESIAN_POINT('Ctrl Pts',(-18.6756142626322,14.1169437524237,
130.908679443903)) ;
#133566 = CARTESIAN_POINT('Ctrl Pts',(-18.6357563526766,13.8684682048696,
130.758950982595)) ;
#133567 = CARTESIAN_POINT('Ctrl Pts',(-18.6192189361488,13.5907243651,130.677694418299)) ;
#133568 = CARTESIAN_POINT('Ctrl Pts',(-18.6274186795787,13.2994062522709,
130.668497076563)) ;
#133569 = CARTESIAN_POINT('Ctrl Pts',(-18.6607053713449,13.0173302811176,
130.732637587237)) ;
#133570 = CARTESIAN_POINT('Ctrl Pts',(-18.7175745221499,12.7634586998748,
130.865557336184)) ;
#133571 = CARTESIAN_POINT('Ctrl Pts',(-18.7946062779487,12.5574053612187,
131.057405473283)) ;
#133572 = CARTESIAN_POINT('Ctrl Pts',(-18.8863176363417,12.4141338116398,
131.292346024062)) ;
#133573 = CARTESIAN_POINT('Ctrl Pts',(-18.9880396659882,12.342233208706,131.556318246303)) ;
#133574 = CARTESIAN_POINT('Ctrl Pts',(-19.092367557879,12.3479816385131,131.828001920729)) ;
#133575 = CARTESIAN_POINT('Ctrl Pts',(-19.1930265312653,12.4308508598937,
132.088893600864)) ;
#133576 = CARTESIAN_POINT('Ctrl Pts',(-19.2830355733598,12.5841342714032,
132.318802233278)) ;
#133577 = CARTESIAN_POINT('Ctrl Pts',(-19.3575448753726,12.7991564308112,
132.503166321675)) ;
#133578 = CARTESIAN_POINT('Ctrl Pts',(-19.410786935153,13.0569999610756,132.625693509338)) ;
#133579 = CARTESIAN_POINT('Ctrl Pts',(-19.4405356262244,13.3421921034464,
132.679428679679)) ;
#133580 = CARTESIAN_POINT('Ctrl Pts',(-19.4450790880921,13.6321454574867,
132.659662972591)) ;
#133581 = CARTESIAN_POINT('Ctrl Pts',(-19.4247875387373,13.9089725412032,
132.567125349093)) ;
#133582 = CARTESIAN_POINT('Ctrl Pts',(-19.381825668748,14.1498188340954,132.408476398238)) ;
#133583 = CARTESIAN_POINT('Ctrl Pts',(-19.3204518279194,14.3379335225619,
132.196198119276)) ;
#133584 = CARTESIAN_POINT('Ctrl Pts',(-19.2450347897687,14.4615825769609,
131.942693860373)) ;
#133585 = CARTESIAN_POINT('Ctrl Pts',(-19.162267963524,14.5104718339952,131.667809535155)) ;
#133586 = CARTESIAN_POINT('Ctrl Pts',(-19.0783524563333,14.4813917081873,
131.389457000585)) ;
#133587 = CARTESIAN_POINT('Ctrl Pts',(-19.0006162859046,14.3764101476522,
131.129272642533)) ;
#133588 = CARTESIAN_POINT('Ctrl Pts',(-18.9351626104612,14.2041613001764,
130.905077291113)) ;
#133589 = CARTESIAN_POINT('Ctrl Pts',(-18.8868641696125,13.9743839791119,
130.730738018104)) ;
#133590 = CARTESIAN_POINT('Ctrl Pts',(-18.8605695212481,13.7063210401926,
130.620861352139)) ;
#133591 = CARTESIAN_POINT('Ctrl Pts',(-18.8586114405782,13.416701167449,130.581917827711)) ;
#133592 = CARTESIAN_POINT('Ctrl Pts',(-18.8818454285258,13.1291677758352,
130.616763647551)) ;
#133593 = CARTESIAN_POINT('Ctrl Pts',(-18.9294289009308,12.86171027905,130.722620411742)) ;
#133594 = CARTESIAN_POINT('Ctrl Pts',(-18.9984336324713,12.6350478480017,
130.891152728659)) ;
#133595 = CARTESIAN_POINT('Ctrl Pts',(-19.0852684560724,12.4638699665219,
131.111590594525)) ;
#133596 = CARTESIAN_POINT('Ctrl Pts',(-19.1836902605787,12.3621126869917,
131.366013493841)) ;
#133597 = CARTESIAN_POINT('Ctrl Pts',(-19.2880034593845,12.336288293437,131.637540200635)) ;
#133598 = CARTESIAN_POINT('Ctrl Pts',(-19.3907293591919,12.3882079133966,
131.9045787098)) ;
#133599 = CARTESIAN_POINT('Ctrl Pts',(-19.4861202999562,12.5148240028862,
132.150020522081)) ;
#133600 = CARTESIAN_POINT('Ctrl Pts',(-19.566984502277,12.7050812653244,132.353293437429)) ;
#133601 = CARTESIAN_POINT('Ctrl Pts',(-19.6294717703468,12.9482677220772,
132.502618790391)) ;
#133602 = CARTESIAN_POINT('Ctrl Pts',(-19.6689768655333,13.2238578222556,
132.585025535771)) ;
#133603 = CARTESIAN_POINT('Ctrl Pts',(-19.6838357324499,13.5162932448957,
132.595118812429)) ;
#133604 = CARTESIAN_POINT('Ctrl Pts',(-19.6735197937544,13.799165239793,132.532024333921)) ;
#133605 = CARTESIAN_POINT('Ctrl Pts',(-19.6392454600331,14.0580267764743,
132.398557205212)) ;
#133606 = CARTESIAN_POINT('Ctrl Pts',(-19.5848869196862,14.2686028129511,
132.206807442572)) ;
#133607 = CARTESIAN_POINT('Ctrl Pts',(-19.5145008411043,14.4199618502008,
131.968069495771)) ;
#133608 = CARTESIAN_POINT('Ctrl Pts',(-19.4340220268986,14.4998958219189,
131.699871465245)) ;
#133609 = CARTESIAN_POINT('Ctrl Pts',(-19.3495759662661,14.5025664794371,
131.419941342377)) ;
#133610 = CARTESIAN_POINT('Ctrl Pts',(-19.2688627445457,14.4280652825415,
131.151146889785)) ;
#133611 = CARTESIAN_POINT('Ctrl Pts',(-19.197514432747,14.2819177513075,130.909621465088)) ;
#133612 = CARTESIAN_POINT('Ctrl Pts',(-19.1413921728409,14.0723877227319,
130.712339919469)) ;
#133613 = CARTESIAN_POINT('Ctrl Pts',(-19.1060584048045,13.8191595273478,
130.576195818314)) ;
#133614 = CARTESIAN_POINT('Ctrl Pts',(-19.0939136018658,13.5356702848312,
130.507524027747)) ;
#133615 = CARTESIAN_POINT('Ctrl Pts',(-19.1068958007053,13.2451626614465,
130.512392184105)) ;
#133616 = CARTESIAN_POINT('Ctrl Pts',(-19.1449564065195,12.9658959397094,
130.5903314269)) ;
#133617 = CARTESIAN_POINT('Ctrl Pts',(-19.2057189790489,12.720867949973,130.73477557543)) ;
#133618 = CARTESIAN_POINT('Ctrl Pts',(-19.2858400354675,12.5256178596935,
130.935699785553)) ;
#133619 = CARTESIAN_POINT('Ctrl Pts',(-19.3800402811628,12.3947249390078,
131.177818876414)) ;
#133620 = CARTESIAN_POINT('Ctrl Pts',(-19.4831200353959,12.3373274128747,
131.445666380565)) ;
#133621 = CARTESIAN_POINT('Ctrl Pts',(-19.5867485454506,12.3577351376061,
131.715460652154)) ;
#133622 = CARTESIAN_POINT('Ctrl Pts',(-19.6862131801358,12.4546492514378,
131.972779675498)) ;
#133623 = CARTESIAN_POINT('Ctrl Pts',(-19.7738286134021,12.6210676591383,
132.195587853881)) ;
#133624 = CARTESIAN_POINT('Ctrl Pts',(-19.8442902702029,12.8446766854148,
132.368316433847)) ;
#133625 = CARTESIAN_POINT('Ctrl Pts',(-19.8933608798738,13.108808163257,132.478653710118)) ;
#133626 = CARTESIAN_POINT('Ctrl Pts',(-19.9184859283659,13.3979062620311,
132.518747291947)) ;
#133627 = CARTESIAN_POINT('Ctrl Pts',(-19.9181983031023,13.6859097607706,
132.484944374893)) ;
#133628 = CARTESIAN_POINT('Ctrl Pts',(-19.8935840118438,13.9567565280856,
132.379898432991)) ;
#133629 = CARTESIAN_POINT('Ctrl Pts',(-19.8465997978561,14.1899349125241,
132.209373856163)) ;
#133630 = CARTESIAN_POINT('Ctrl Pts',(-19.7823820361551,14.3662692626876,
131.988864508273)) ;
#133631 = CARTESIAN_POINT('Ctrl Pts',(-19.7048377925854,14.4768289979695,
131.729048105592)) ;
#133632 = CARTESIAN_POINT('Ctrl Pts',(-19.621356858463,14.5109207090365,131.452070562692)) ;
#133633 = CARTESIAN_POINT('Ctrl Pts',(-19.5383256537918,14.4673589954117,
131.176412965102)) ;
#133634 = CARTESIAN_POINT('Ctrl Pts',(-19.462343360731,14.3490298117359,130.921339630599)) ;
#133635 = CARTESIAN_POINT('Ctrl Pts',(-19.399598094763,14.1643442573792,130.70492417211)) ;
#133636 = CARTESIAN_POINT('Ctrl Pts',(-19.3553585530389,13.9269540764464,
130.542614298548)) ;
#133637 = CARTESIAN_POINT('Ctrl Pts',(-19.3333939719036,13.6529087066834,
130.44529695513)) ;
#133638 = CARTESIAN_POINT('Ctrl Pts',(-19.3361541913265,13.3625040426011,
130.420224634067)) ;
#133639 = CARTESIAN_POINT('Ctrl Pts',(-19.3641172961552,13.0764917625792,
130.468781137817)) ;
#133640 = CARTESIAN_POINT('Ctrl Pts',(-19.4160399610195,12.8152457852602,
130.587319851219)) ;
#133641 = CARTESIAN_POINT('Ctrl Pts',(-19.4888652574942,12.5977360848388,
130.766942106929)) ;
#133642 = CARTESIAN_POINT('Ctrl Pts',(-19.5781388686584,12.4392301767845,
130.994608862376)) ;
#133643 = CARTESIAN_POINT('Ctrl Pts',(-19.6782931891438,12.3513755992719,
131.254028736787)) ;
#133644 = CARTESIAN_POINT('Ctrl Pts',(-19.7822229405507,12.3399316332142,
131.524661009902)) ;
#133645 = CARTESIAN_POINT('Ctrl Pts',(-19.88504344773,12.4070554351268,131.791616350641)) ;
#133646 = CARTESIAN_POINT('Ctrl Pts',(-19.9771610745846,12.5451369869361,
132.027897931008)) ;
#133647 = CARTESIAN_POINT('Ctrl Pts',(-20.0556173721215,12.7477726868892,
132.223821692675)) ;
#133648 = CARTESIAN_POINT('Ctrl Pts',(-20.1137903255926,12.9979367372735,
132.360683275234)) ;
#133649 = CARTESIAN_POINT('Ctrl Pts',(-20.1489013724765,13.2792370978739,
132.430071631305)) ;
#133650 = CARTESIAN_POINT('Ctrl Pts',(-20.1588787384282,13.5701580555343,
132.426125674529)) ;
#133651 = CARTESIAN_POINT('Ctrl Pts',(-20.143937682242,13.8505377724051,132.349389311992)) ;
#133652 = CARTESIAN_POINT('Ctrl Pts',(-20.1057318059421,14.1007512372239,
132.20463305785)) ;
#133653 = CARTESIAN_POINT('Ctrl Pts',(-20.0478354950526,14.3021715583994,
132.002395149785)) ;
#133654 = CARTESIAN_POINT('Ctrl Pts',(-19.9748500391882,14.4410638226486,
131.755979394128)) ;
#133655 = CARTESIAN_POINT('Ctrl Pts',(-19.892940104349,14.506420576945,131.483512074612)) ;
#133656 = CARTESIAN_POINT('Ctrl Pts',(-19.8092678890523,14.4944296739133,
131.206120710523)) ;
#133657 = CARTESIAN_POINT('Ctrl Pts',(-19.7294350859359,14.4055611915821,
130.939713797808)) ;
#133658 = CARTESIAN_POINT('Ctrl Pts',(-19.66081208133,14.2469875620131,130.706232624641)) ;
#133659 = CARTESIAN_POINT('Ctrl Pts',(-19.6083158027718,14.0284942715184,
130.519673218377)) ;
#133660 = CARTESIAN_POINT('Ctrl Pts',(-19.5769557514165,13.7670074742828,
130.394940588624)) ;
#133661 = CARTESIAN_POINT('Ctrl Pts',(-19.5695668686991,13.4805781215048,
130.340191561689)) ;
#133662 = CARTESIAN_POINT('Ctrl Pts',(-19.5872696261961,13.1913388058783,
130.358899107894)) ;
#133663 = CARTESIAN_POINT('Ctrl Pts',(-19.6297522740938,12.9172330933754,
130.449814911348)) ;
#133664 = CARTESIAN_POINT('Ctrl Pts',(-19.6944389773908,12.6799728703758,
130.60569175476)) ;
#133665 = CARTESIAN_POINT('Ctrl Pts',(-19.7782230780513,12.4949910418975,
130.817115688087)) ;
#133666 = CARTESIAN_POINT('Ctrl Pts',(-19.8739923402946,12.3781840447206,
131.063992159593)) ;
#133667 = CARTESIAN_POINT('Ctrl Pts',(-19.9780674608701,12.3352411023339,
131.33468497079)) ;
#133668 = CARTESIAN_POINT('Ctrl Pts',(-20.0810744379286,12.3701183957634,
131.602725123913)) ;
#133669 = CARTESIAN_POINT('Ctrl Pts',(-20.179252895713,12.4815908370187,131.85612905703)) ;
#133670 = CARTESIAN_POINT('Ctrl Pts',(-20.2634570739637,12.6586744463426,
132.069206441814)) ;
#133671 = CARTESIAN_POINT('Ctrl Pts',(-20.3305901520664,12.8927064505131,
132.232014267973)) ;
#133672 = CARTESIAN_POINT('Ctrl Pts',(-20.3750331233153,13.1615895986342,
132.328969789793)) ;
#133673 = CARTESIAN_POINT('Ctrl Pts',(-20.3954965997089,13.4527337961883,
132.355428882089)) ;
#133674 = CARTESIAN_POINT('Ctrl Pts',(-20.3904573045894,13.7397606263225,
132.307631593907)) ;
#133675 = CARTESIAN_POINT('Ctrl Pts',(-20.3613437715797,14.0044956878458,
132.189457679076)) ;
#133676 = CARTESIAN_POINT('Ctrl Pts',(-20.3110168045734,14.2270717047825,
132.009394785638)) ;
#133677 = CARTESIAN_POINT('Ctrl Pts',(-20.2436381751946,14.3928428531141,
131.779444891534)) ;
#133678 = CARTESIAN_POINT('Ctrl Pts',(-20.164336633125,14.4891679896536,131.51449038135)) ;
#133679 = CARTESIAN_POINT('Ctrl Pts',(-20.0809111882638,14.5086708936273,
131.237865647246)) ;
#133680 = CARTESIAN_POINT('Ctrl Pts',(-19.9983950566067,14.4507091204102,
130.963592375788)) ;
#133681 = CARTESIAN_POINT('Ctrl Pts',(-19.9244190141413,14.318823465338,130.714351089596)) ;
#133682 = CARTESIAN_POINT('Ctrl Pts',(-19.8648700988791,14.1234067424229,
130.507330724768)) ;
#133683 = CARTESIAN_POINT('Ctrl Pts',(-19.8245161746179,13.8772496577341,
130.356293737963)) ;
#133684 = CARTESIAN_POINT('Ctrl Pts',(-19.8070957881005,13.5994498547175,
130.272359938913)) ;
#133685 = CARTESIAN_POINT('Ctrl Pts',(-19.8146864693653,13.3067289539218,
130.261220009531)) ;
#133686 = CARTESIAN_POINT('Ctrl Pts',(-19.8471784531872,13.025513208076,130.323196727465)) ;
#133687 = CARTESIAN_POINT('Ctrl Pts',(-19.9032180692331,12.7708776887036,
130.453754380472)) ;
#133688 = CARTESIAN_POINT('Ctrl Pts',(-19.9797679754465,12.5628412979246,
130.644157296538)) ;
#133689 = CARTESIAN_POINT('Ctrl Pts',(-20.0712997390683,12.4171764122364,
130.878502714501)) ;
#133690 = CARTESIAN_POINT('Ctrl Pts',(-20.173220666744,12.3431378359771,131.142938313351)) ;
#133691 = CARTESIAN_POINT('Ctrl Pts',(-20.2769543623743,12.3467434972734,
131.413078047708)) ;
#133692 = CARTESIAN_POINT('Ctrl Pts',(-20.3779474556413,12.4272274658185,
131.674911921515)) ;
#133693 = CARTESIAN_POINT('Ctrl Pts',(-20.4684824931614,12.5790158149027,
131.906293765199)) ;
#133694 = CARTESIAN_POINT('Ctrl Pts',(-20.5433178346082,12.7916687829571,
132.091724629749)) ;
#133695 = CARTESIAN_POINT('Ctrl Pts',(-20.59747019779,13.0498138992039,132.216737279054)) ;
#133696 = CARTESIAN_POINT('Ctrl Pts',(-20.6277539698486,13.3331756720239,
132.272199599018)) ;
#133697 = CARTESIAN_POINT('Ctrl Pts',(-20.63310319697,13.6238935345468,132.254712776567)) ;
#133698 = CARTESIAN_POINT('Ctrl Pts',(-20.6135004102223,13.9010885274901,
132.164225860573)) ;
#133699 = CARTESIAN_POINT('Ctrl Pts',(-20.5712628793398,14.1432054793993,
132.007719764268)) ;
#133700 = CARTESIAN_POINT('Ctrl Pts',(-20.5099062183509,14.3341070280144,
131.795269476235)) ;
#133701 = CARTESIAN_POINT('Ctrl Pts',(-20.4352339689786,14.4587991787124,
131.544150012527)) ;
#133702 = CARTESIAN_POINT('Ctrl Pts',(-20.3525489079931,14.5101605081857,
131.269477291802)) ;
#133703 = CARTESIAN_POINT('Ctrl Pts',(-20.2687361872864,14.4834097576633,
130.991492371573)) ;
#133704 = CARTESIAN_POINT('Ctrl Pts',(-20.1906756501309,14.380986704451,130.730363509583)) ;
#133705 = CARTESIAN_POINT('Ctrl Pts',(-20.1243569260148,14.2089571607828,
130.503381990289)) ;
#133706 = CARTESIAN_POINT('Ctrl Pts',(-20.0759333865454,13.9828180453883,
130.329004955831)) ;
#133707 = CARTESIAN_POINT('Ctrl Pts',(-20.0486953445985,13.7132629209954,
130.216063933579)) ;
#133708 = CARTESIAN_POINT('Ctrl Pts',(-20.0461136758052,13.42583764063,130.175529664949)) ;
#133709 = CARTESIAN_POINT('Ctrl Pts',(-20.0685766436055,13.1374631065902,
130.208056459246)) ;
#133710 = CARTESIAN_POINT('Ctrl Pts',(-20.1154485813734,12.8691197006536,
130.31184888817)) ;
#133711 = CARTESIAN_POINT('Ctrl Pts',(-20.1842161886027,12.6403113443668,
130.479551228157)) ;
#133712 = CARTESIAN_POINT('Ctrl Pts',(-20.2699974667944,12.468420702256,130.697148821309)) ;
#133713 = CARTESIAN_POINT('Ctrl Pts',(-20.368777345651,12.3638000217504,130.952399609198)) ;
#133714 = CARTESIAN_POINT('Ctrl Pts',(-20.4724837589939,12.3359859144704,
131.22233281641)) ;
#133715 = CARTESIAN_POINT('Ctrl Pts',(-20.5755189014966,12.3855342690204,
131.490214378318)) ;
#133716 = CARTESIAN_POINT('Ctrl Pts',(-20.6710370148352,12.5097023136888,
131.736103980719)) ;
#133717 = CARTESIAN_POINT('Ctrl Pts',(-20.7526999022241,12.6987169895182,
131.941597617443)) ;
#133718 = CARTESIAN_POINT('Ctrl Pts',(-20.8159200282362,12.9413958856346,
132.092978431002)) ;
#133719 = CARTESIAN_POINT('Ctrl Pts',(-20.8560148207953,13.2164083911014,
132.177101494275)) ;
#133720 = CARTESIAN_POINT('Ctrl Pts',(-20.8715568106971,13.5077476116907,
132.18930496735)) ;
#133721 = CARTESIAN_POINT('Ctrl Pts',(-20.8618791478333,13.7917084995172,
132.127994218716)) ;
#133722 = CARTESIAN_POINT('Ctrl Pts',(-20.8285666993428,14.0497089633418,
131.997596945122)) ;
#133723 = CARTESIAN_POINT('Ctrl Pts',(-20.7745879228126,14.2632250030891,
131.806787903495)) ;
#133724 = CARTESIAN_POINT('Ctrl Pts',(-20.7043311974277,14.4168537708596,
131.568328459368)) ;
#133725 = CARTESIAN_POINT('Ctrl Pts',(-20.6239603167272,14.4987598986465,
131.300415425815)) ;
#133726 = CARTESIAN_POINT('Ctrl Pts',(-20.539754785129,14.5035045718472,131.021276419093)) ;
#133727 = CARTESIAN_POINT('Ctrl Pts',(-20.4588117616689,14.4313229997249,
130.751803459987)) ;
#133728 = CARTESIAN_POINT('Ctrl Pts',(-20.3868956375626,14.286096674379,130.508478859911)) ;
#133729 = CARTESIAN_POINT('Ctrl Pts',(-20.3308554449234,14.0806888556304,
130.311826279916)) ;
#133730 = CARTESIAN_POINT('Ctrl Pts',(-20.2944696102375,13.8265805447723,
130.172317712221)) ;
#133731 = CARTESIAN_POINT('Ctrl Pts',(-20.2817095072984,13.5441879409374,
130.101929815543)) ;
#133732 = CARTESIAN_POINT('Ctrl Pts',(-20.2939970046262,13.2530370689606,
130.104694604891)) ;
#133733 = CARTESIAN_POINT('Ctrl Pts',(-20.3312192505214,12.9741114175935,
130.18030810907)) ;
#133734 = CARTESIAN_POINT('Ctrl Pts',(-20.391477731723,12.7272119216586,130.323195480133)) ;
#133735 = CARTESIAN_POINT('Ctrl Pts',(-20.4710215017653,12.5305677659782,
130.522476172394)) ;
#133736 = CARTESIAN_POINT('Ctrl Pts',(-20.5648765077218,12.3976028767503,
130.763584707341)) ;
#133737 = CARTESIAN_POINT('Ctrl Pts',(-20.6677354645716,12.3378877564715,
131.030810858964)) ;
#133738 = CARTESIAN_POINT('Ctrl Pts',(-20.771610142133,12.3561146457162,131.301258410359)) ;
#133739 = CARTESIAN_POINT('Ctrl Pts',(-20.8710140356471,12.4504996091204,
131.558507272223)) ;
#133740 = CARTESIAN_POINT('Ctrl Pts',(-20.9591976245712,12.6151918179393,
131.782920165643)) ;
#133741 = CARTESIAN_POINT('Ctrl Pts',(-21.0301909969835,12.8367627956422,
131.957264907826)) ;
#133742 = CARTESIAN_POINT('Ctrl Pts',(-21.0802720431719,13.102471284239,132.070248175628)) ;
#133743 = CARTESIAN_POINT('Ctrl Pts',(-21.1058128562322,13.388098474674,132.11192368682)) ;
#133744 = CARTESIAN_POINT('Ctrl Pts',(-21.1063578527298,13.6786302634614,
132.08028850925)) ;
#133745 = CARTESIAN_POINT('Ctrl Pts',(-21.0823275663731,13.9495118019851,
131.977027551482)) ;
#133746 = CARTESIAN_POINT('Ctrl Pts',(-21.0362217842379,14.1831630717315,
131.809216673534)) ;
#133747 = CARTESIAN_POINT('Ctrl Pts',(-20.9721884045855,14.3622887251467,
131.589091305906)) ;
#133748 = CARTESIAN_POINT('Ctrl Pts',(-20.8947792880245,14.4748192529362,
131.32962547702)) ;
#133749 = CARTESIAN_POINT('Ctrl Pts',(-20.8116749026299,14.5109473630978,
131.053861074448)) ;
#133750 = CARTESIAN_POINT('Ctrl Pts',(-20.7286272549608,14.46989386631,130.778195045776)) ;
#133751 = CARTESIAN_POINT('Ctrl Pts',(-20.6522431108941,14.3536144736526,
130.521907930923)) ;
#133752 = CARTESIAN_POINT('Ctrl Pts',(-20.5889583813436,14.17062113719,130.303892930056)) ;
#133753 = CARTESIAN_POINT('Ctrl Pts',(-20.5440524129988,13.933736573907,130.13953810035)) ;
#133754 = CARTESIAN_POINT('Ctrl Pts',(-20.5214975045223,13.6617104442443,
130.040649083481)) ;
#133755 = CARTESIAN_POINT('Ctrl Pts',(-20.5235105668905,13.3701432171844,
130.013237741548)) ;
#133756 = CARTESIAN_POINT('Ctrl Pts',(-20.5508607538459,13.0839501475181,
130.0600249237)) ;
#133757 = CARTESIAN_POINT('Ctrl Pts',(-20.6019342296123,12.8226369063403,
130.176200002378)) ;
#133758 = CARTESIAN_POINT('Ctrl Pts',(-20.674162245095,12.6036153158418,130.354083975274)) ;
#133759 = CARTESIAN_POINT('Ctrl Pts',(-20.7628382753172,12.4432239429731,
130.580060592785)) ;
#133760 = CARTESIAN_POINT('Ctrl Pts',(-20.8633579914741,12.3525997513282,
130.840351394468)) ;
#133761 = CARTESIAN_POINT('Ctrl Pts',(-20.9671168641114,12.3393903655815,
131.110528978872)) ;
#133762 = CARTESIAN_POINT('Ctrl Pts',(-21.0694306011919,12.403468098602,131.376231401918)) ;
#133763 = CARTESIAN_POINT('Ctrl Pts',(-21.1627219404933,12.5405072085783,
131.615661785443)) ;
#133764 = CARTESIAN_POINT('Ctrl Pts',(-21.2416127937835,12.7420005519616,
131.812839172161)) ;
#133765 = CARTESIAN_POINT('Ctrl Pts',(-21.3001704333997,12.9900801149227,
131.950949061272)) ;
#133766 = CARTESIAN_POINT('Ctrl Pts',(-21.3360159038547,13.2708158721555,
132.022475029764)) ;
#133767 = CARTESIAN_POINT('Ctrl Pts',(-21.3467250085586,13.5613604134334,
132.020708203514)) ;
#133768 = CARTESIAN_POINT('Ctrl Pts',(-21.332530072888,13.8428560081929,131.946099675255)) ;
#133769 = CARTESIAN_POINT('Ctrl Pts',(-21.2946880005883,14.0951246502648,
131.802259522002)) ;
#133770 = CARTESIAN_POINT('Ctrl Pts',(-21.2376357521135,14.2968154125605,
131.602698948677)) ;
#133771 = CARTESIAN_POINT('Ctrl Pts',(-21.164806246768,14.4382062812648,131.356634806151)) ;
#133772 = CARTESIAN_POINT('Ctrl Pts',(-21.0832408338308,14.5055713938207,
131.085254319312)) ;
#133773 = CARTESIAN_POINT('Ctrl Pts',(-20.9994162423038,14.4957941932041,
130.807360837672)) ;
#133774 = CARTESIAN_POINT('Ctrl Pts',(-20.9195959138854,14.4095662340998,
130.541102349046)) ;
#133775 = CARTESIAN_POINT('Ctrl Pts',(-20.8500186277359,14.2515335127425,
130.304558118666)) ;
#133776 = CARTESIAN_POINT('Ctrl Pts',(-20.7972486154139,14.0347236874785,
130.11728882556)) ;
#133777 = CARTESIAN_POINT('Ctrl Pts',(-20.7653613268004,13.7751700114088,
129.991129528377)) ;
#133778 = CARTESIAN_POINT('Ctrl Pts',(-20.7571817990629,13.489555102194,129.934113768398)) ;
#133779 = CARTESIAN_POINT('Ctrl Pts',(-20.7742556911792,13.1989624545804,
129.950844344899)) ;
#133780 = CARTESIAN_POINT('Ctrl Pts',(-20.8159809707414,12.9245155762064,
130.03960916018)) ;
#133781 = CARTESIAN_POINT('Ctrl Pts',(-20.8805367450398,12.6850932088169,
130.194926855194)) ;
#133782 = CARTESIAN_POINT('Ctrl Pts',(-20.9626356003938,12.5007200500438,
130.401901459438)) ;
#133783 = CARTESIAN_POINT('Ctrl Pts',(-21.0591957946408,12.3802348015134,
130.650687618331)) ;
#133784 = CARTESIAN_POINT('Ctrl Pts',(-21.1622370545661,12.3354177830535,
130.918672003733)) ;
#133785 = CARTESIAN_POINT('Ctrl Pts',(-21.2662887681593,12.3682931650198,
131.189443526458)) ;
#133786 = CARTESIAN_POINT('Ctrl Pts',(-21.3637199956931,12.4764500222757,
131.44102792815)) ;
#133787 = CARTESIAN_POINT('Ctrl Pts',(-21.4490683123423,12.6527561756398,
131.657189302748)) ;
#133788 = CARTESIAN_POINT('Ctrl Pts',(-21.5164968590452,12.8841372675975,
131.821041651181)) ;
#133789 = CARTESIAN_POINT('Ctrl Pts',(-21.5620729321248,13.1550291136418,
131.920951331736)) ;
#133790 = CARTESIAN_POINT('Ctrl Pts',(-21.5829990360394,13.4437302360126,
131.949026741888)) ;
#133791 = CARTESIAN_POINT('Ctrl Pts',(-21.5787261653874,13.7319393007276,
131.903366364301)) ;
#133792 = CARTESIAN_POINT('Ctrl Pts',(-21.5503975227815,13.9965481623833,
131.787623344815)) ;
#133793 = CARTESIAN_POINT('Ctrl Pts',(-21.5005342471165,14.2215298170475,
131.608800269925)) ;
#133794 = CARTESIAN_POINT('Ctrl Pts',(-21.4333938850247,14.3891483272759,
131.379489123203)) ;
#133795 = CARTESIAN_POINT('Ctrl Pts',(-21.3548735774567,14.4871687024338,
131.117033634355)) ;
#133796 = CARTESIAN_POINT('Ctrl Pts',(-21.2709428978837,14.5093408079897,
130.838711318976)) ;
#133797 = CARTESIAN_POINT('Ctrl Pts',(-21.1882422406468,14.4530254583256,
130.563868416307)) ;
#133798 = CARTESIAN_POINT('Ctrl Pts',(-21.1143270880585,14.3240305585518,
130.31499305445)) ;
#133799 = CARTESIAN_POINT('Ctrl Pts',(-21.0539688868397,14.1290979717854,
130.105410602035)) ;
#133800 = CARTESIAN_POINT('Ctrl Pts',(-21.0132069302916,13.8855604155571,
129.953378103653)) ;
#133801 = CARTESIAN_POINT('Ctrl Pts',(-20.9950030451873,13.6058416707122,
129.866845755651)) ;
#133802 = CARTESIAN_POINT('Ctrl Pts',(-21.0018793397198,13.3160021377259,
129.853947611582)) ;
#133803 = CARTESIAN_POINT('Ctrl Pts',(-21.0337293398582,13.0326886676077,
129.913868033499)) ;
#133804 = CARTESIAN_POINT('Ctrl Pts',(-21.0893772116349,12.7766372190837,
130.043216529831)) ;
#133805 = CARTESIAN_POINT('Ctrl Pts',(-21.1653161877122,12.5676698161814,
130.231901557219)) ;
#133806 = CARTESIAN_POINT('Ctrl Pts',(-21.2561790285771,12.4206517790888,
130.464404545457)) ;
#133807 = CARTESIAN_POINT('Ctrl Pts',(-21.3575675366688,12.3443150505119,
130.727387699059)) ;
#133808 = CARTESIAN_POINT('Ctrl Pts',(-21.4618210845223,12.3454567433165,
130.998884337509)) ;
#133809 = CARTESIAN_POINT('Ctrl Pts',(-21.5631430702427,12.4241540146565,
131.261630006307)) ;
#133810 = CARTESIAN_POINT('Ctrl Pts',(-21.6537810155053,12.5736454649868,
131.493407152973)) ;
#133811 = CARTESIAN_POINT('Ctrl Pts',(-21.7290950924145,12.7844244258342,
131.680270904741)) ;
#133812 = CARTESIAN_POINT('Ctrl Pts',(-21.7839298109933,13.041264478038,131.807295952736)) ;
#133813 = CARTESIAN_POINT('Ctrl Pts',(-21.8150448539116,13.3250313838274,
131.865081031141)) ;
#133814 = CARTESIAN_POINT('Ctrl Pts',(-21.8210632536644,13.6156492492809,
131.849571033927)) ;
#133815 = CARTESIAN_POINT('Ctrl Pts',(-21.8022545212773,13.8929002803611,
131.761487721122)) ;
#133816 = CARTESIAN_POINT('Ctrl Pts',(-21.7605924585031,14.1366366428793,
131.606614879296)) ;
#133817 = CARTESIAN_POINT('Ctrl Pts',(-21.6999698317163,14.3287833833703,
131.396421302764)) ;
#133818 = CARTESIAN_POINT('Ctrl Pts',(-21.6253197774301,14.4563288342089,
131.145218098165)) ;
#133819 = CARTESIAN_POINT('Ctrl Pts',(-21.5425945750513,14.5097636463918,
130.870367772935)) ;
#133820 = CARTESIAN_POINT('Ctrl Pts',(-21.4589621479375,14.4852491819093,
130.593003563587)) ;
#133821 = CARTESIAN_POINT('Ctrl Pts',(-21.380714091029,14.385213180382,130.331360934625)) ;
#133822 = CARTESIAN_POINT('Ctrl Pts',(-21.3138290434139,14.2148994362801,
130.102677640231)) ;
#133823 = CARTESIAN_POINT('Ctrl Pts',(-21.264802027938,13.9895605141043,129.92646714371)) ;
#133824 = CARTESIAN_POINT('Ctrl Pts',(-21.2370048320792,13.7226496289756,
129.812102485109)) ;
#133825 = CARTESIAN_POINT('Ctrl Pts',(-21.2336042417307,13.4342098859693,
129.769013814372)) ;
#133826 = CARTESIAN_POINT('Ctrl Pts',(-21.2553236046358,13.1458182759752,
129.799407215841)) ;
#133827 = CARTESIAN_POINT('Ctrl Pts',(-21.3016988392798,12.8759127132536,
129.901648132077)) ;
#133828 = CARTESIAN_POINT('Ctrl Pts',(-21.3694669987003,12.6468868556867,
130.066623481143)) ;
#133829 = CARTESIAN_POINT('Ctrl Pts',(-21.4553373193102,12.4721832296684,
130.284273605613)) ;
#133830 = CARTESIAN_POINT('Ctrl Pts',(-21.5530256217249,12.3661739274481,
130.536616813639)) ;
#133831 = CARTESIAN_POINT('Ctrl Pts',(-21.6575177270796,12.3355863385396,
130.808562220896)) ;
#133832 = CARTESIAN_POINT('Ctrl Pts',(-21.7604456918656,12.3831198658751,
131.076206190241)) ;
#133833 = CARTESIAN_POINT('Ctrl Pts',(-21.8563696469902,12.5053833023315,
131.323242388746)) ;
#133834 = CARTESIAN_POINT('Ctrl Pts',(-21.9382966693068,12.6923270702948,
131.529584453516)) ;
#133835 = CARTESIAN_POINT('Ctrl Pts',(-22.0021645015312,12.9335865705139,
131.682862448256)) ;
#133836 = CARTESIAN_POINT('Ctrl Pts',(-22.0430213128192,13.2085814539572,
131.769129801508)) ;
#133837 = CARTESIAN_POINT('Ctrl Pts',(-22.0592352836556,13.4990557588074,
131.783380739882)) ;
#133838 = CARTESIAN_POINT('Ctrl Pts',(-22.0503004073671,13.7836907462661,
131.724216167399)) ;
#133839 = CARTESIAN_POINT('Ctrl Pts',(-22.0176371901026,14.0427281414566,
131.595717480909)) ;
#133840 = CARTESIAN_POINT('Ctrl Pts',(-21.9641995370827,14.2577309750281,
131.406490661624)) ;
#133841 = CARTESIAN_POINT('Ctrl Pts',(-21.8944782363852,14.4131664617501,
131.169654967239)) ;
#133842 = CARTESIAN_POINT('Ctrl Pts',(-21.8141620072022,14.4973755702956,
130.901832610092)) ;
#133843 = CARTESIAN_POINT('Ctrl Pts',(-21.7303937720881,14.5046724130054,
130.624142862364)) ;
#133844 = CARTESIAN_POINT('Ctrl Pts',(-21.6486693225774,14.4343111747756,
130.352140919931)) ;
#133845 = CARTESIAN_POINT('Ctrl Pts',(-21.5766530687314,14.2913904033354,
130.108640611113)) ;
#133846 = CARTESIAN_POINT('Ctrl Pts',(-21.5199914526865,14.0872940403586,
129.910112364196)) ;
#133847 = CARTESIAN_POINT('Ctrl Pts',(-21.4830382408884,13.8349907742835,
129.769035274606)) ;
#133848 = CARTESIAN_POINT('Ctrl Pts',(-21.4694985396213,13.5522018199285,
129.696252361388)) ;
#133849 = CARTESIAN_POINT('Ctrl Pts',(-21.4810885813508,13.2611771320633,
129.697002826515)) ;
#133850 = CARTESIAN_POINT('Ctrl Pts',(-21.5176805732444,12.9814107201437,
129.770743949859)) ;
#133851 = CARTESIAN_POINT('Ctrl Pts',(-21.5771191123903,12.7341369610279,
129.911345858839)) ;
#133852 = CARTESIAN_POINT('Ctrl Pts',(-21.6563209788842,12.535166216503,130.109544290444)) ;
#133853 = CARTESIAN_POINT('Ctrl Pts',(-21.7502713534583,12.4000170891871,
130.350799701057)) ;
#133854 = CARTESIAN_POINT('Ctrl Pts',(-21.8524815344102,12.3385941106561,
130.616296707476)) ;
#133855 = CARTESIAN_POINT('Ctrl Pts',(-21.9565712501459,12.3545286685026,
130.887315313701)) ;
#133856 = CARTESIAN_POINT('Ctrl Pts',(-22.0562577481496,12.4469846430608,
131.14537139149)) ;
#133857 = CARTESIAN_POINT('Ctrl Pts',(-22.1449360417052,12.6102579412087,
131.371180205731)) ;
#133858 = CARTESIAN_POINT('Ctrl Pts',(-22.2161370464207,12.8296977311719,
131.546256445573)) ;
#133859 = CARTESIAN_POINT('Ctrl Pts',(-22.2667592690025,13.0929763552362,
131.660982603106)) ;
#133860 = CARTESIAN_POINT('Ctrl Pts',(-22.2932535098378,13.3798715107165,
131.705248169509)) ;
#133861 = CARTESIAN_POINT('Ctrl Pts',(-22.2944576782056,13.6705227535771,
131.675549761758)) ;
#133862 = CARTESIAN_POINT('Ctrl Pts',(-22.2711545117995,13.9421700423004,
131.57442408932)) ;
#133863 = CARTESIAN_POINT('Ctrl Pts',(-22.2253820822901,14.1780191011813,
131.407446635602)) ;
#133864 = CARTESIAN_POINT('Ctrl Pts',(-22.1619741826909,14.3579768124892,
131.189272795754)) ;
#133865 = CARTESIAN_POINT('Ctrl Pts',(-22.0850483275451,14.4725057553617,
130.931291857228)) ;
#133866 = CARTESIAN_POINT('Ctrl Pts',(-22.0018889458697,14.5110248787396,
130.655306915796)) ;
#133867 = CARTESIAN_POINT('Ctrl Pts',(-21.9186831269904,14.4721191969269,
130.37915685792)) ;
#133868 = CARTESIAN_POINT('Ctrl Pts',(-21.8419983594231,14.3577454336847,
130.121978165508)) ;
#133869 = CARTESIAN_POINT('Ctrl Pts',(-21.7784559689967,14.1770688666527,
129.90331119887)) ;
#133870 = CARTESIAN_POINT('Ctrl Pts',(-21.7328730623761,13.9416997327419,
129.73698112711)) ;
#133871 = CARTESIAN_POINT('Ctrl Pts',(-21.7095937547817,13.6694104353782,
129.635852457523)) ;
#133872 = CARTESIAN_POINT('Ctrl Pts',(-21.7108544164153,13.3798585935035,
129.60644988842)) ;
#133873 = CARTESIAN_POINT('Ctrl Pts',(-21.7373587408651,13.0927640382574,
129.650717582232)) ;
#133874 = CARTESIAN_POINT('Ctrl Pts',(-21.7879727694938,12.8294542733058,
129.765423278)) ;
#133875 = CARTESIAN_POINT('Ctrl Pts',(-21.8596572059499,12.6090080043084,
129.941724810289)) ;
#133876 = CARTESIAN_POINT('Ctrl Pts',(-21.9481186483126,12.4466659582347,
130.167016290758)) ;
#133877 = CARTESIAN_POINT('Ctrl Pts',(-22.0478029406896,12.3544265354386,
130.425067159699)) ;
#133878 = CARTESIAN_POINT('Ctrl Pts',(-22.1517530143636,12.338485550426,130.695728652991)) ;
#133879 = CARTESIAN_POINT('Ctrl Pts',(-22.2547791723717,12.4009576070215,
130.963329774343)) ;
#133880 = CARTESIAN_POINT('Ctrl Pts',(-22.3479076849026,12.5356622675021,
131.202441690569)) ;
#133881 = CARTESIAN_POINT('Ctrl Pts',(-22.427039674185,12.7342792931547,131.400473047047)) ;
#133882 = CARTESIAN_POINT('Ctrl Pts',(-22.4865817751364,12.9822470405306,
131.541298758196)) ;
#133883 = CARTESIAN_POINT('Ctrl Pts',(-22.5231351067208,13.2626104241267,
131.614868935857)) ;
#133884 = CARTESIAN_POINT('Ctrl Pts',(-22.5345613145019,13.5537330357078,
131.615129217148)) ;
#133885 = CARTESIAN_POINT('Ctrl Pts',(-22.5210072175352,13.8350780443648,
131.542464925158)) ;
#133886 = CARTESIAN_POINT('Ctrl Pts',(-22.4841282635127,14.0872562376869,
131.401629162015)) ;
#133887 = CARTESIAN_POINT('Ctrl Pts',(-22.4271936380161,14.2922552735091,
131.202157542)) ;
#133888 = CARTESIAN_POINT('Ctrl Pts',(-22.3548468095764,14.4349645919609,
130.957589374496)) ;
#133889 = CARTESIAN_POINT('Ctrl Pts',(-22.2738049730186,14.5045540577175,
130.687866104784)) ;
#133890 = CARTESIAN_POINT('Ctrl Pts',(-22.1896316409164,14.4973581396257,
130.408831550043)) ;
#133891 = CARTESIAN_POINT('Ctrl Pts',(-22.1093343470203,14.4126016842873,
130.14105358009)) ;
#133892 = CARTESIAN_POINT('Ctrl Pts',(-22.0399356599868,14.2578370889756,
129.905309744937)) ;
#133893 = CARTESIAN_POINT('Ctrl Pts',(-21.9863765422796,14.0423606370671,
129.715650705837)) ;
#133894 = CARTESIAN_POINT('Ctrl Pts',(-21.9537345461485,13.7833430848993,
129.58722594006)) ;
#133895 = CARTESIAN_POINT('Ctrl Pts',(-21.9448743026681,13.4972454461382,
129.528113894271)) ;
#133896 = CARTESIAN_POINT('Ctrl Pts',(-21.960316850898,13.2225256872019,129.541910774833)) ;
#133897 = CARTESIAN_POINT('Ctrl Pts',(-21.984463817368,13.0520853568101,129.592017243009)) ;
#133898 = CARTESIAN_POINT('Ctrl Pts',(-21.9982570673691,12.9778651918053,
129.622952131535)) ;
#133899 = CARTESIAN_POINT('',(-11.3761033793275,13.1734341962953,133.269779676638)) ;
#133900 = CARTESIAN_POINT('Origin',(-11.3525470049302,13.1551399285885,133.200965310447)) ;
#133901 = CARTESIAN_POINT('',(-11.3289906305328,13.1368456608817,133.132150944256)) ;
#133902 = CARTESIAN_POINT('Origin',(-11.3525470049302,13.1551399285885,133.200965310447)) ;
#133903 = CARTESIAN_POINT('Origin',(-11.3525470049302,13.1551399285885,133.200965310447)) ;
#133904 = CARTESIAN_POINT('',(-22.3151378869403,14.5729486686832,130.548644361977)) ;
#133905 = CARTESIAN_POINT('Ctrl Pts',(-22.3151379480645,14.5729486667267,
130.548644337297)) ;
#133906 = CARTESIAN_POINT('Ctrl Pts',(-22.3011761799316,14.5730368300439,
130.507858330238)) ;
#133907 = CARTESIAN_POINT('Ctrl Pts',(-22.287200210088,14.5706665958407,130.467031058799)) ;
#133908 = CARTESIAN_POINT('Ctrl Pts',(-22.2733078271729,14.5658273790944,
130.42644775387)) ;
#133909 = CARTESIAN_POINT('Ctrl Pts',(-22.2675381995131,14.5638176102188,
130.409593153758)) ;
#133910 = CARTESIAN_POINT('Ctrl Pts',(-22.2617824711753,14.5613818550179,
130.392779157221)) ;
#133911 = CARTESIAN_POINT('Ctrl Pts',(-22.2560476493669,14.5585193175848,
130.376026234156)) ;
#133912 = CARTESIAN_POINT('Ctrl Pts',(-22.2292231059487,14.545129841464,130.297664686553)) ;
#133913 = CARTESIAN_POINT('Ctrl Pts',(-22.2028658648278,14.5224036480338,
130.220668467657)) ;
#133914 = CARTESIAN_POINT('Ctrl Pts',(-22.1776957713426,14.4911112211587,
130.147139851903)) ;
#133915 = CARTESIAN_POINT('Ctrl Pts',(-22.1719521385364,14.4839705162705,
130.130361154999)) ;
#133916 = CARTESIAN_POINT('Ctrl Pts',(-22.166270291937,14.4763839522868,130.113762956894)) ;
#133917 = CARTESIAN_POINT('Ctrl Pts',(-22.1606587249298,14.4683610330769,
130.097370093526)) ;
#133918 = CARTESIAN_POINT('Ctrl Pts',(-22.1355483985991,14.4324605227158,
130.024016224965)) ;
#133919 = CARTESIAN_POINT('Ctrl Pts',(-22.1118463317427,14.3878194900747,
129.954775802407)) ;
#133920 = CARTESIAN_POINT('Ctrl Pts',(-22.0900768461573,14.3354941538269,
129.891181728977)) ;
#133921 = CARTESIAN_POINT('Ctrl Pts',(-22.0856561856623,14.3248686135067,
129.878267881885)) ;
#133922 = CARTESIAN_POINT('Ctrl Pts',(-22.0813151982726,14.3139263466192,
129.865586780601)) ;
#133923 = CARTESIAN_POINT('Ctrl Pts',(-22.0770582501623,14.3026764237554,
129.853151115368)) ;
#133924 = CARTESIAN_POINT('Ctrl Pts',(-22.0575007470533,14.2509914147575,
129.796018504125)) ;
#133925 = CARTESIAN_POINT('Ctrl Pts',(-22.0397191593872,14.1928134151899,
129.744072096327)) ;
#133926 = CARTESIAN_POINT('Ctrl Pts',(-22.0241540809177,14.1296950731463,
129.698603459873)) ;
#133927 = CARTESIAN_POINT('Ctrl Pts',(-22.0196338868241,14.1113651201392,
129.685399089439)) ;
#133928 = CARTESIAN_POINT('Ctrl Pts',(-22.015300592828,14.0926186905485,129.672740752753)) ;
#133929 = CARTESIAN_POINT('Ctrl Pts',(-22.0111649071197,14.0734942173741,
129.660659326894)) ;
#133930 = CARTESIAN_POINT('Ctrl Pts',(-21.9979065378246,14.0121841116736,
129.621928142528)) ;
#133931 = CARTESIAN_POINT('Ctrl Pts',(-21.9866821734794,13.9469968841568,
129.589133277344)) ;
#133932 = CARTESIAN_POINT('Ctrl Pts',(-21.977674302844,13.8791719111513,129.562821710652)) ;
#133933 = CARTESIAN_POINT('Ctrl Pts',(-21.9741790940785,13.8528546548578,
129.552612370148)) ;
#133934 = CARTESIAN_POINT('Ctrl Pts',(-21.9710176873156,13.8261405468838,
129.543378736997)) ;
#133935 = CARTESIAN_POINT('Ctrl Pts',(-21.9682011481905,13.799103138409,129.535150885313)) ;
#133936 = CARTESIAN_POINT('Ctrl Pts',(-21.9656494606323,13.774608176419,129.527696734726)) ;
#133937 = CARTESIAN_POINT('Ctrl Pts',(-21.9633468396246,13.7495103406013,
129.520970042987)) ;
#133938 = CARTESIAN_POINT('Ctrl Pts',(-21.961330695701,13.7240463055939,129.515080342888)) ;
#133939 = CARTESIAN_POINT('Ctrl Pts',(-21.9593134014791,13.6985677422408,
129.509187282458)) ;
#133940 = CARTESIAN_POINT('Ctrl Pts',(-21.9575829900595,13.6727232379291,
129.504132378895)) ;
#133941 = CARTESIAN_POINT('Ctrl Pts',(-21.9561611043169,13.6467675495469,
129.49997876671)) ;
#133942 = CARTESIAN_POINT('Ctrl Pts',(-21.9547385696093,13.6208000146897,
129.495823258767)) ;
#133943 = CARTESIAN_POINT('Ctrl Pts',(-21.953624881802,13.5947219208531,129.492569954795)) ;
#133944 = CARTESIAN_POINT('Ctrl Pts',(-21.9528249799405,13.5687954659883,
129.490233200648)) ;
#133945 = CARTESIAN_POINT('Ctrl Pts',(-21.9521162979408,13.545825633356,129.488162927178)) ;
#133946 = CARTESIAN_POINT('Ctrl Pts',(-21.9516536736589,13.5229752443421,
129.486811359342)) ;
#133947 = CARTESIAN_POINT('Ctrl Pts',(-21.9514293963157,13.5004244329661,
129.486156186226)) ;
#133948 = CARTESIAN_POINT('Ctrl Pts',(-21.9512381070114,13.481190528375,129.485597379848)) ;
#133949 = CARTESIAN_POINT('Ctrl Pts',(-21.9512130944036,13.4613698797395,
129.485523580215)) ;
#133950 = CARTESIAN_POINT('Ctrl Pts',(-21.9513804892,13.4412408608151,129.486012294124)) ;
#133951 = CARTESIAN_POINT('Ctrl Pts',(-21.9515476082074,13.421145005191,129.48650020286)) ;
#133952 = CARTESIAN_POINT('Ctrl Pts',(-21.9519065972143,13.4007422200765,
129.48754900886)) ;
#133953 = CARTESIAN_POINT('Ctrl Pts',(-21.9524666030812,13.3803126577523,
129.489185369577)) ;
#133954 = CARTESIAN_POINT('Ctrl Pts',(-21.9530180572326,13.3601950703844,
129.490796741821)) ;
#133955 = CARTESIAN_POINT('Ctrl Pts',(-21.9537644170884,13.3400519549877,
129.492977752401)) ;
#133956 = CARTESIAN_POINT('Ctrl Pts',(-21.9546975614041,13.3201474123098,
129.49570416507)) ;
#133957 = CARTESIAN_POINT('Ctrl Pts',(-21.9556524119253,13.2997798629067,
129.498493997805)) ;
#133958 = CARTESIAN_POINT('Ctrl Pts',(-21.9568028587807,13.2796626021651,
129.501854897454)) ;
#133959 = CARTESIAN_POINT('Ctrl Pts',(-21.9581222304844,13.2600678710264,
129.505708828523)) ;
#133960 = CARTESIAN_POINT('Ctrl Pts',(-21.9594416021881,13.2404731398877,
129.509562759592)) ;
#133961 = CARTESIAN_POINT('Ctrl Pts',(-21.960929776014,13.2214012994025,129.513909294428)) ;
#133962 = CARTESIAN_POINT('Ctrl Pts',(-21.96254318369,13.2031075416911,129.518622482662)) ;
#133963 = CARTESIAN_POINT('Ctrl Pts',(-21.963701302918,13.1899761100796,129.522005653574)) ;
#133964 = CARTESIAN_POINT('Ctrl Pts',(-21.9649923328492,13.1764783865927,
129.525776897949)) ;
#133965 = CARTESIAN_POINT('Ctrl Pts',(-21.9663999656187,13.1629676618293,
129.529889010867)) ;
#133966 = CARTESIAN_POINT('Ctrl Pts',(-21.9678179998417,13.1493571019527,
129.534031509516)) ;
#133967 = CARTESIAN_POINT('Ctrl Pts',(-21.9693544131974,13.1357338594016,
129.53851997682)) ;
#133968 = CARTESIAN_POINT('Ctrl Pts',(-21.9709759033026,13.1224444824642,
129.543256827227)) ;
#133969 = CARTESIAN_POINT('Ctrl Pts',(-21.9725973934077,13.1091551055269,
129.547993677634)) ;
#133970 = CARTESIAN_POINT('Ctrl Pts',(-21.9743038518766,13.096199960817,129.552978488115)) ;
#133971 = CARTESIAN_POINT('Ctrl Pts',(-21.976045911875,13.0839043074199,129.558067503624)) ;
#133972 = CARTESIAN_POINT('Ctrl Pts',(-21.9773237439476,13.0748852264019,
129.561800387246)) ;
#133973 = CARTESIAN_POINT('Ctrl Pts',(-21.9787131003971,13.065573564542,129.565858984562)) ;
#133974 = CARTESIAN_POINT('Ctrl Pts',(-21.9801662380091,13.056419673348,129.570104049804)) ;
#133975 = CARTESIAN_POINT('Ctrl Pts',(-21.9816281570041,13.0472104647332,
129.574374768186)) ;
#133976 = CARTESIAN_POINT('Ctrl Pts',(-21.9831546331542,13.0381613456531,
129.578833998246)) ;
#133977 = CARTESIAN_POINT('Ctrl Pts',(-21.984681663157,13.0297062023895,129.583294812552)) ;
#133978 = CARTESIAN_POINT('Ctrl Pts',(-21.9848487129258,13.0287812502109,
129.583782804272)) ;
#133979 = CARTESIAN_POINT('Ctrl Pts',(-21.9850157546884,13.0278633792237,
129.584270774027)) ;
#133980 = CARTESIAN_POINT('Ctrl Pts',(-21.9851826941415,13.0269531373025,
129.584758448084)) ;
#133981 = CARTESIAN_POINT('Ctrl Pts',(-21.9863339740107,13.0206757524139,
129.588121639429)) ;
#133982 = CARTESIAN_POINT('Ctrl Pts',(-21.9875828769642,13.0142106156177,
129.591770024712)) ;
#133983 = CARTESIAN_POINT('Ctrl Pts',(-21.9888478967941,13.008138163139,129.595465492)) ;
#133984 = CARTESIAN_POINT('Ctrl Pts',(-21.989454280972,13.0052273478162,129.597236905255)) ;
#133985 = CARTESIAN_POINT('Ctrl Pts',(-21.990064156824,13.0024063418278,129.599018484663)) ;
#133986 = CARTESIAN_POINT('Ctrl Pts',(-21.9906674065461,12.9997366350286,
129.600780735788)) ;
#133987 = CARTESIAN_POINT('Ctrl Pts',(-21.9916964541652,12.9951825418823,
129.603786854577)) ;
#133988 = CARTESIAN_POINT('Ctrl Pts',(-21.9928080155907,12.9906247701674,
129.607034017901)) ;
#133989 = CARTESIAN_POINT('Ctrl Pts',(-21.9938748908751,12.9868577736952,
129.610150641252)) ;
#133990 = CARTESIAN_POINT('Ctrl Pts',(-21.9945019204265,12.984643814723,129.611982359513)) ;
#133991 = CARTESIAN_POINT('Ctrl Pts',(-21.995149121453,12.9825760105869,129.613873003867)) ;
#133992 = CARTESIAN_POINT('Ctrl Pts',(-21.9957649760313,12.9809630503241,
129.615672077092)) ;
#133993 = CARTESIAN_POINT('Ctrl Pts',(-21.996719473855,12.9784631629888,129.618460416319)) ;
#133994 = CARTESIAN_POINT('Ctrl Pts',(-21.997623841344,12.9769886520828,129.621102311744)) ;
#133995 = CARTESIAN_POINT('Ctrl Pts',(-21.9982570673691,12.9778651918053,
129.622952131536)) ;
#133996 = CARTESIAN_POINT('',(-22.3151378869403,14.423223846854,130.548644361977)) ;
#133997 = CARTESIAN_POINT('Ctrl Pts',(-22.3151378869416,14.5729486706397,
130.548644361981)) ;
#133998 = CARTESIAN_POINT('Ctrl Pts',(-22.3536131995393,14.5727057162824,
130.661040871128)) ;
#133999 = CARTESIAN_POINT('Ctrl Pts',(-22.3917725975218,14.5537967295509,
130.772514510611)) ;
#134000 = CARTESIAN_POINT('Ctrl Pts',(-22.4651692698086,14.4793817119497,
130.986925497581)) ;
#134001 = CARTESIAN_POINT('Ctrl Pts',(-22.4997692262472,14.4241005029474,
131.088001071933)) ;
#134002 = CARTESIAN_POINT('Ctrl Pts',(-22.5689108472644,14.2666151380171,
131.289981934841)) ;
#134003 = CARTESIAN_POINT('Ctrl Pts',(-22.6011767967328,14.1573235247065,
131.38423926092)) ;
#134004 = CARTESIAN_POINT('Ctrl Pts',(-22.6488987494123,13.9114366623006,
131.523647638104)) ;
#134005 = CARTESIAN_POINT('Ctrl Pts',(-22.6645996619435,13.7782522629318,
131.569514133756)) ;
#134006 = CARTESIAN_POINT('Ctrl Pts',(-22.6786331937249,13.4898377655437,
131.610509771653)) ;
#134007 = CARTESIAN_POINT('Ctrl Pts',(-22.6736768274188,13.3672753503854,
131.596030921988)) ;
#134008 = CARTESIAN_POINT('Ctrl Pts',(-22.6651145627851,13.2574016528032,
131.571018294663)) ;
#134009 = CARTESIAN_POINT('Ctrl Pts',(-22.6619233775539,13.2306316253481,
131.561696003049)) ;
#134010 = CARTESIAN_POINT('Ctrl Pts',(-22.658869062641,13.2145328967425,131.552773545741)) ;
#134011 = CARTESIAN_POINT('Ctrl Pts',(-22.658166921974,13.2113394407781,131.550722408079)) ;
#134012 = CARTESIAN_POINT('Ctrl Pts',(-22.6572747831006,13.2091027938622,
131.54811623575)) ;
#134013 = CARTESIAN_POINT('Ctrl Pts',(-22.6570602137521,13.2086648958779,
131.547489422314)) ;
#134014 = CARTESIAN_POINT('Ctrl Pts',(-22.6566971522605,13.2082608228121,
131.546428824192)) ;
#134015 = CARTESIAN_POINT('Ctrl Pts',(-22.6565542868357,13.2081743378001,
131.546011476705)) ;
#134016 = CARTESIAN_POINT('Ctrl Pts',(-22.6562872703243,13.2082090859895,
131.545231451236)) ;
#134017 = CARTESIAN_POINT('Ctrl Pts',(-22.656171236643,13.2082979781244,131.54489248633)) ;
#134018 = CARTESIAN_POINT('Ctrl Pts',(-22.6559368182774,13.2086342290079,
131.54420768862)) ;
#134019 = CARTESIAN_POINT('Ctrl Pts',(-22.6558268749173,13.2088894196119,
131.543886515144)) ;
#134020 = CARTESIAN_POINT('Ctrl Pts',(-22.6555685283304,13.2096748296436,
131.543131816805)) ;
#134021 = CARTESIAN_POINT('Ctrl Pts',(-22.6554365161173,13.2102931177128,
131.542746174404)) ;
#134022 = CARTESIAN_POINT('Ctrl Pts',(-22.6550858617799,13.2123135011588,
131.541721820844)) ;
#134023 = CARTESIAN_POINT('Ctrl Pts',(-22.6549030747436,13.2141115604459,
131.541187851828)) ;
#134024 = CARTESIAN_POINT('Ctrl Pts',(-22.6543256425256,13.2215607234665,
131.539501020424)) ;
#134025 = CARTESIAN_POINT('Ctrl Pts',(-22.6541135690987,13.2297469423957,
131.538881498157)) ;
#134026 = CARTESIAN_POINT('Ctrl Pts',(-22.6532410800261,13.2936995343114,
131.536332728065)) ;
#134027 = CARTESIAN_POINT('Ctrl Pts',(-22.6556996367525,13.4112788385444,
131.543514818452)) ;
#134028 = CARTESIAN_POINT('Ctrl Pts',(-22.6382336783187,13.6947112909237,
131.492492159393)) ;
#134029 = CARTESIAN_POINT('Ctrl Pts',(-22.6221628124986,13.8232128942525,
131.445544933384)) ;
#134030 = CARTESIAN_POINT('Ctrl Pts',(-22.5744365803075,14.0563340831041,
131.306124054621)) ;
#134031 = CARTESIAN_POINT('Ctrl Pts',(-22.5435243363485,14.1569964530154,
131.21582125845)) ;
#134032 = CARTESIAN_POINT('Ctrl Pts',(-22.4791435871951,14.2967160993782,
131.027748154618)) ;
#134033 = CARTESIAN_POINT('Ctrl Pts',(-22.4480466097423,14.3443721936477,
130.936905703363)) ;
#134034 = CARTESIAN_POINT('Ctrl Pts',(-22.3828566010413,14.4076338778508,
130.746468539515)) ;
#134035 = CARTESIAN_POINT('Ctrl Pts',(-22.3491318413627,14.4234782772114,
130.647949645059)) ;
#134036 = CARTESIAN_POINT('Ctrl Pts',(-22.3151378869407,14.4232238463042,
130.548644361978)) ;
#134037 = CARTESIAN_POINT('Ctrl Pts',(-21.9982570673691,12.9778651918053,
129.622952131535)) ;
#134038 = CARTESIAN_POINT('Ctrl Pts',(-21.9983740357125,12.9780271046061,
129.623293826836)) ;
#134039 = CARTESIAN_POINT('Ctrl Pts',(-21.9984729623435,12.9782537499198,
129.623582817547)) ;
#134040 = CARTESIAN_POINT('Ctrl Pts',(-21.9986619517152,12.9788663176289,
129.624134905217)) ;
#134041 = CARTESIAN_POINT('Ctrl Pts',(-21.9987422359044,12.9792529318713,
129.624369436452)) ;
#134042 = CARTESIAN_POINT('Ctrl Pts',(-21.9989688888416,12.9806654239707,
129.625031549303)) ;
#134043 = CARTESIAN_POINT('Ctrl Pts',(-21.9990592680355,12.9819390751646,
129.625295570703)) ;
#134044 = CARTESIAN_POINT('Ctrl Pts',(-21.9992344695967,12.9863682734796,
129.625807380551)) ;
#134045 = CARTESIAN_POINT('Ctrl Pts',(-21.9991646228976,12.9906967702327,
129.62560333997)) ;
#134046 = CARTESIAN_POINT('Ctrl Pts',(-21.998493398505,13.0076193276443,129.623642516951)) ;
#134047 = CARTESIAN_POINT('Ctrl Pts',(-21.9973112343386,13.024361696837,129.620189104446)) ;
#134048 = CARTESIAN_POINT('Ctrl Pts',(-21.9922385267737,13.093661183053,129.605370391257)) ;
#134049 = CARTESIAN_POINT('Ctrl Pts',(-21.9869683786663,13.1624395523346,
129.58997490231)) ;
#134050 = CARTESIAN_POINT('Ctrl Pts',(-21.9792387916176,13.3897587207603,
129.567394745249)) ;
#134051 = CARTESIAN_POINT('Ctrl Pts',(-21.9832458177027,13.5079529375974,
129.579100322505)) ;
#134052 = CARTESIAN_POINT('Ctrl Pts',(-21.9990289638202,13.7299217778491,
129.625207044119)) ;
#134053 = CARTESIAN_POINT('Ctrl Pts',(-22.0148314797799,13.8477898854171,
129.671370350136)) ;
#134054 = CARTESIAN_POINT('Ctrl Pts',(-22.0613345650186,14.0688613754809,
129.807218094897)) ;
#134055 = CARTESIAN_POINT('Ctrl Pts',(-22.0926080464121,14.1680229125909,
129.898576160635)) ;
#134056 = CARTESIAN_POINT('Ctrl Pts',(-22.1569266233532,14.3035692712769,
130.08646764308)) ;
#134057 = CARTESIAN_POINT('Ctrl Pts',(-22.1873142259314,14.3485547863788,
130.175237823827)) ;
#134058 = CARTESIAN_POINT('Ctrl Pts',(-22.2505095483839,14.4080651754862,
130.359847984435)) ;
#134059 = CARTESIAN_POINT('Ctrl Pts',(-22.282659459403,14.4229807584986,130.45376633159)) ;
#134060 = CARTESIAN_POINT('Ctrl Pts',(-22.3151378869407,14.4232238463042,
130.548644361978)) ;
#134061 = CARTESIAN_POINT('Ctrl Pts',(-11.2812798643659,13.1551399285885,
133.225361312885)) ;
#134062 = CARTESIAN_POINT('Ctrl Pts',(-11.3048362387632,13.1734341962953,
133.294175679076)) ;
#134063 = CARTESIAN_POINT('Ctrl Pts',(-11.3761033793275,13.1734341962953,
133.269779676638)) ;
#134064 = CARTESIAN_POINT('Ctrl Pts',(-11.4473705198918,13.1734341962953,
133.2453836742)) ;
#134065 = CARTESIAN_POINT('Ctrl Pts',(-11.4238141454945,13.1551399285885,
133.176569308009)) ;
#134066 = CARTESIAN_POINT('Ctrl Pts',(-11.4002577710971,13.1368456608817,
133.107754941818)) ;
#134067 = CARTESIAN_POINT('Ctrl Pts',(-11.3289906305328,13.1368456608817,
133.132150944256)) ;
#134068 = CARTESIAN_POINT('Ctrl Pts',(-11.2577234899685,13.1368456608817,
133.156546946693)) ;
#134069 = CARTESIAN_POINT('Ctrl Pts',(-11.2812798643659,13.1551399285885,
133.225361312885)) ;
#134070 = CARTESIAN_POINT('Ctrl Pts',(-11.2798493008599,13.191264605624,133.215535474837)) ;
#134071 = CARTESIAN_POINT('Ctrl Pts',(-11.3038195704943,13.1991216594078,
133.286995970946)) ;
#134072 = CARTESIAN_POINT('Ctrl Pts',(-11.3749383182286,13.2028260557706,
133.262162005045)) ;
#134073 = CARTESIAN_POINT('Ctrl Pts',(-11.4460570659629,13.2065304521335,
133.237328039145)) ;
#134074 = CARTESIAN_POINT('Ctrl Pts',(-11.4220867963285,13.1986733983497,
133.165867543036)) ;
#134075 = CARTESIAN_POINT('Ctrl Pts',(-11.398116526694,13.1908163445659,133.094407046927)) ;
#134076 = CARTESIAN_POINT('Ctrl Pts',(-11.3269977789597,13.1871119482031,
133.119241012827)) ;
#134077 = CARTESIAN_POINT('Ctrl Pts',(-11.2558790312254,13.1834075518402,
133.144074978727)) ;
#134078 = CARTESIAN_POINT('Ctrl Pts',(-11.2798493008599,13.191264605624,133.215535474837)) ;
#134079 = CARTESIAN_POINT('Ctrl Pts',(-11.27675499221,13.268036520819,133.2128184295)) ;
#134080 = CARTESIAN_POINT('Ctrl Pts',(-11.3016167838991,13.2538025217343,
133.284678753642)) ;
#134081 = CARTESIAN_POINT('Ctrl Pts',(-11.3724255895565,13.2651134066728,
133.260704367766)) ;
#134082 = CARTESIAN_POINT('Ctrl Pts',(-11.4432343952138,13.2764242916113,
133.23672998189)) ;
#134083 = CARTESIAN_POINT('Ctrl Pts',(-11.4183726035248,13.290658290696,133.164869657748)) ;
#134084 = CARTESIAN_POINT('Ctrl Pts',(-11.3935108118358,13.3048922897807,
133.093009333607)) ;
#134085 = CARTESIAN_POINT('Ctrl Pts',(-11.3227020061784,13.2935814048422,
133.116983719482)) ;
#134086 = CARTESIAN_POINT('Ctrl Pts',(-11.251893200521,13.2822705199037,133.140958105358)) ;
#134087 = CARTESIAN_POINT('Ctrl Pts',(-11.27675499221,13.268036520819,133.2128184295)) ;
#134088 = CARTESIAN_POINT('Ctrl Pts',(-11.2723617392628,13.3732912215196,
133.259787303242)) ;
#134089 = CARTESIAN_POINT('Ctrl Pts',(-11.298479063893,13.3290215614615,133.317617538259)) ;
#134090 = CARTESIAN_POINT('Ctrl Pts',(-11.3688780671425,13.3500184403787,
133.299818088917)) ;
#134091 = CARTESIAN_POINT('Ctrl Pts',(-11.439277070392,13.371015319296,133.282018639574)) ;
#134092 = CARTESIAN_POINT('Ctrl Pts',(-11.4131597457618,13.4152849793541,
133.224188404558)) ;
#134093 = CARTESIAN_POINT('Ctrl Pts',(-11.3870424211316,13.4595546394122,
133.166358169541)) ;
#134094 = CARTESIAN_POINT('Ctrl Pts',(-11.3166434178821,13.4385577604949,
133.184157618883)) ;
#134095 = CARTESIAN_POINT('Ctrl Pts',(-11.2462444146326,13.4175608815777,
133.201957068225)) ;
#134096 = CARTESIAN_POINT('Ctrl Pts',(-11.2723617392628,13.3732912215196,
133.259787303242)) ;
#134097 = CARTESIAN_POINT('Ctrl Pts',(-11.2691148403661,13.4471111688333,
133.348383186297)) ;
#134098 = CARTESIAN_POINT('Ctrl Pts',(-11.2961492330365,13.3820520008154,
133.380368710749)) ;
#134099 = CARTESIAN_POINT('Ctrl Pts',(-11.3662774333647,13.409026910249,133.37238538732)) ;
#134100 = CARTESIAN_POINT('Ctrl Pts',(-11.436405633693,13.4360018196825,133.364402063892)) ;
#134101 = CARTESIAN_POINT('Ctrl Pts',(-11.4093712410226,13.5010609877004,
133.33241653944)) ;
#134102 = CARTESIAN_POINT('Ctrl Pts',(-11.3823368483522,13.5661201557183,
133.300431014988)) ;
#134103 = CARTESIAN_POINT('Ctrl Pts',(-11.312208648024,13.5391452462847,133.308414338417)) ;
#134104 = CARTESIAN_POINT('Ctrl Pts',(-11.2420804476957,13.5121703368512,
133.316397661845)) ;
#134105 = CARTESIAN_POINT('Ctrl Pts',(-11.2691148403661,13.4471111688333,
133.348383186297)) ;
#134106 = CARTESIAN_POINT('Ctrl Pts',(-11.26815235584,13.4654248347116,133.423083801914)) ;
#134107 = CARTESIAN_POINT('Ctrl Pts',(-11.295448841143,13.3954694274565,133.433496373216)) ;
#134108 = CARTESIAN_POINT('Ctrl Pts',(-11.3655255940352,13.4231551632892,
133.433144549366)) ;
#134109 = CARTESIAN_POINT('Ctrl Pts',(-11.4356023469274,13.4508408991218,
133.432792725516)) ;
#134110 = CARTESIAN_POINT('Ctrl Pts',(-11.4083058616244,13.5207963063769,
133.422380154214)) ;
#134111 = CARTESIAN_POINT('Ctrl Pts',(-11.3810093763214,13.5907517136319,
133.411967582912)) ;
#134112 = CARTESIAN_POINT('Ctrl Pts',(-11.3109326234292,13.5630659777992,
133.412319406762)) ;
#134113 = CARTESIAN_POINT('Ctrl Pts',(-11.240855870537,13.5353802419666,133.412671230612)) ;
#134114 = CARTESIAN_POINT('Ctrl Pts',(-11.26815235584,13.4654248347116,133.423083801914)) ;
#134115 = CARTESIAN_POINT('Ctrl Pts',(-11.2680244517119,13.4658285122696,
133.460562426083)) ;
#134116 = CARTESIAN_POINT('Ctrl Pts',(-11.2953502173512,13.3959427988304,
133.460195119767)) ;
#134117 = CARTESIAN_POINT('Ctrl Pts',(-11.3654365304336,13.4231193515827,
133.463543154982)) ;
#134118 = CARTESIAN_POINT('Ctrl Pts',(-11.435522843516,13.4502959043349,133.466891190198)) ;
#134119 = CARTESIAN_POINT('Ctrl Pts',(-11.4081970778768,13.5201816177741,
133.467258496514)) ;
#134120 = CARTESIAN_POINT('Ctrl Pts',(-11.3808713122375,13.5900673312133,
133.467625802831)) ;
#134121 = CARTESIAN_POINT('Ctrl Pts',(-11.3107849991551,13.562890778461,133.464277767615)) ;
#134122 = CARTESIAN_POINT('Ctrl Pts',(-11.2406986860726,13.5357142257088,
133.4609297324)) ;
#134123 = CARTESIAN_POINT('Ctrl Pts',(-11.2680244517119,13.4658285122696,
133.460562426083)) ;
#134124 = CARTESIAN_POINT('',(-11.2680244517119,13.4658285122696,133.460562426083)) ;
#134125 = CARTESIAN_POINT('Ctrl Pts',(-11.2812798643659,13.1551399285885,
133.225361312885)) ;
#134126 = CARTESIAN_POINT('Ctrl Pts',(-11.2798493008599,13.191264605624,133.215535474837)) ;
#134127 = CARTESIAN_POINT('Ctrl Pts',(-11.27675499221,13.268036520819,133.2128184295)) ;
#134128 = CARTESIAN_POINT('Ctrl Pts',(-11.2723617392628,13.3732912215196,
133.259787303242)) ;
#134129 = CARTESIAN_POINT('Ctrl Pts',(-11.2691148403661,13.4471111688333,
133.348383186297)) ;
#134130 = CARTESIAN_POINT('Ctrl Pts',(-11.26815235584,13.4654248347116,133.423083801914)) ;
#134131 = CARTESIAN_POINT('Ctrl Pts',(-11.2680244517119,13.4658285122696,
133.460562426083)) ;
#134132 = CARTESIAN_POINT('Origin',(-11.3381107647943,13.4930050650219,133.463910461299)) ;
#134133 = CARTESIAN_POINT('Ctrl Pts',(-11.2680244517119,13.4658285122696,
133.460562426083)) ;
#134134 = CARTESIAN_POINT('Ctrl Pts',(-11.2953502173512,13.3959427988304,
133.460195119767)) ;
#134135 = CARTESIAN_POINT('Ctrl Pts',(-11.3654365304336,13.4231193515827,
133.463543154982)) ;
#134136 = CARTESIAN_POINT('Ctrl Pts',(-11.435522843516,13.4502959043349,133.466891190198)) ;
#134137 = CARTESIAN_POINT('Ctrl Pts',(-11.4081970778768,13.5201816177741,
133.467258496514)) ;
#134138 = CARTESIAN_POINT('Ctrl Pts',(-11.3808713122375,13.5900673312133,
133.467625802831)) ;
#134139 = CARTESIAN_POINT('Ctrl Pts',(-11.3107849991551,13.562890778461,133.464277767615)) ;
#134140 = CARTESIAN_POINT('Ctrl Pts',(-11.2406986860726,13.5357142257088,
133.4609297324)) ;
#134141 = CARTESIAN_POINT('Ctrl Pts',(-11.2680244517119,13.4658285122696,
133.460562426083)) ;
#134142 = CARTESIAN_POINT('Ctrl Pts',(-11.2668676693348,13.4658294080177,
133.842542306898)) ;
#134143 = CARTESIAN_POINT('Ctrl Pts',(-11.294193434974,13.3959436945786,133.842175000581)) ;
#134144 = CARTESIAN_POINT('Ctrl Pts',(-11.3642797480564,13.4231202473308,
133.845523035796)) ;
#134145 = CARTESIAN_POINT('Ctrl Pts',(-11.4343660611389,13.4502968000831,
133.848871071012)) ;
#134146 = CARTESIAN_POINT('Ctrl Pts',(-11.4070402954996,13.5201825135223,
133.849238377328)) ;
#134147 = CARTESIAN_POINT('Ctrl Pts',(-11.3797145298603,13.5900682269615,
133.849605683645)) ;
#134148 = CARTESIAN_POINT('Ctrl Pts',(-11.3096282167779,13.5628916742092,
133.84625764843)) ;
#134149 = CARTESIAN_POINT('Ctrl Pts',(-11.2395419036955,13.5357151214569,
133.842909613214)) ;
#134150 = CARTESIAN_POINT('Ctrl Pts',(-11.2668676693348,13.4658294080177,
133.842542306898)) ;
#134151 = CARTESIAN_POINT('Ctrl Pts',(-11.2657108869576,13.4658303037659,
134.224522187712)) ;
#134152 = CARTESIAN_POINT('Ctrl Pts',(-11.2930366525969,13.3959445903267,
134.224154881395)) ;
#134153 = CARTESIAN_POINT('Ctrl Pts',(-11.3631229656793,13.423121143079,134.227502916611)) ;
#134154 = CARTESIAN_POINT('Ctrl Pts',(-11.4332092787617,13.4502976958313,
134.230850951826)) ;
#134155 = CARTESIAN_POINT('Ctrl Pts',(-11.4058835131224,13.5201834092705,
134.231218258142)) ;
#134156 = CARTESIAN_POINT('Ctrl Pts',(-11.3785577474832,13.5900691227097,
134.231585564459)) ;
#134157 = CARTESIAN_POINT('Ctrl Pts',(-11.3084714344008,13.5628925699574,
134.228237529244)) ;
#134158 = CARTESIAN_POINT('Ctrl Pts',(-11.2383851213183,13.5357160172051,
134.224889494028)) ;
#134159 = CARTESIAN_POINT('Ctrl Pts',(-11.2657108869576,13.4658303037659,
134.224522187712)) ;
#134160 = CARTESIAN_POINT('Ctrl Pts',(-11.2645541045804,13.4658311995141,
134.606502068526)) ;
#134161 = CARTESIAN_POINT('Ctrl Pts',(-11.2918798702197,13.3959454860749,
134.606134762209)) ;
#134162 = CARTESIAN_POINT('Ctrl Pts',(-11.3619661833021,13.4231220388272,
134.609482797425)) ;
#134163 = CARTESIAN_POINT('Ctrl Pts',(-11.4320524963845,13.4502985915795,
134.61283083264)) ;
#134164 = CARTESIAN_POINT('Ctrl Pts',(-11.4047267307453,13.5201843050187,
134.613198138957)) ;
#134165 = CARTESIAN_POINT('Ctrl Pts',(-11.377400965106,13.5900700184578,134.613565445273)) ;
#134166 = CARTESIAN_POINT('Ctrl Pts',(-11.3073146520236,13.5628934657056,
134.610217410058)) ;
#134167 = CARTESIAN_POINT('Ctrl Pts',(-11.2372283389412,13.5357169129533,
134.606869374843)) ;
#134168 = CARTESIAN_POINT('Ctrl Pts',(-11.2645541045804,13.4658311995141,
134.606502068526)) ;
#134169 = CARTESIAN_POINT('',(-11.2645541045804,13.4658311995141,134.606502068526)) ;
#134170 = CARTESIAN_POINT('',(-11.2680244517119,13.4658285122696,133.460562426083)) ;
#134171 = CARTESIAN_POINT('',(-11.3347092035438,13.4180239009611,134.608294431335)) ;
#134172 = CARTESIAN_POINT('Origin',(-11.3346404176629,13.4930077522664,134.609850103741)) ;
#134173 = CARTESIAN_POINT('',(-11.3345717668412,13.5679916035759,134.611405781511)) ;
#134174 = CARTESIAN_POINT('Origin',(-11.3346404176629,13.4930077522664,134.609850103741)) ;
#134175 = CARTESIAN_POINT('Origin',(-11.3346404176629,13.4930077522664,134.609850103741)) ;
#134176 = CARTESIAN_POINT('Ctrl Pts',(-11.2645541045804,13.4658311995141,
134.606502068526)) ;
#134177 = CARTESIAN_POINT('Ctrl Pts',(-11.2918798702197,13.3959454860749,
134.606134762209)) ;
#134178 = CARTESIAN_POINT('Ctrl Pts',(-11.3619661833021,13.4231220388272,
134.609482797425)) ;
#134179 = CARTESIAN_POINT('Ctrl Pts',(-11.4320524963845,13.4502985915795,
134.61283083264)) ;
#134180 = CARTESIAN_POINT('Ctrl Pts',(-11.4047267307453,13.5201843050187,
134.613198138957)) ;
#134181 = CARTESIAN_POINT('Ctrl Pts',(-11.377400965106,13.5900700184578,134.613565445273)) ;
#134182 = CARTESIAN_POINT('Ctrl Pts',(-11.3073146520236,13.5628934657056,
134.610217410058)) ;
#134183 = CARTESIAN_POINT('Ctrl Pts',(-11.2372283389412,13.5357169129533,
134.606869374843)) ;
#134184 = CARTESIAN_POINT('Ctrl Pts',(-11.2645541045804,13.4658311995141,
134.606502068526)) ;
#134185 = CARTESIAN_POINT('Ctrl Pts',(-11.25920483017,13.4658311995141,134.672131214346)) ;
#134186 = CARTESIAN_POINT('Ctrl Pts',(-11.2865612947575,13.3959454860749,
134.6745078611)) ;
#134187 = CARTESIAN_POINT('Ctrl Pts',(-11.3562925573149,13.4231220388272,
134.68489500114)) ;
#134188 = CARTESIAN_POINT('Ctrl Pts',(-11.4260238198722,13.4502985915795,
134.69528214118)) ;
#134189 = CARTESIAN_POINT('Ctrl Pts',(-11.3986673552847,13.5201843050187,
134.692905494426)) ;
#134190 = CARTESIAN_POINT('Ctrl Pts',(-11.3713108906971,13.5900700184579,
134.690528847672)) ;
#134191 = CARTESIAN_POINT('Ctrl Pts',(-11.3015796281398,13.5628934657056,
134.680141707632)) ;
#134192 = CARTESIAN_POINT('Ctrl Pts',(-11.2318483655824,13.5357169129533,
134.669754567592)) ;
#134193 = CARTESIAN_POINT('Ctrl Pts',(-11.25920483017,13.4658311995141,134.672131214346)) ;
#134194 = CARTESIAN_POINT('Ctrl Pts',(-11.2276030587525,13.4658311995141,
134.805074979322)) ;
#134195 = CARTESIAN_POINT('Ctrl Pts',(-11.2541595398934,13.3959454860749,
134.813089440493)) ;
#134196 = CARTESIAN_POINT('Ctrl Pts',(-11.3209495279222,13.4231220388272,
134.837803867739)) ;
#134197 = CARTESIAN_POINT('Ctrl Pts',(-11.3877395159509,13.4502985915795,
134.862518294986)) ;
#134198 = CARTESIAN_POINT('Ctrl Pts',(-11.36118303481,13.5201843050187,134.854503833814)) ;
#134199 = CARTESIAN_POINT('Ctrl Pts',(-11.3346265536691,13.5900700184578,
134.846489372643)) ;
#134200 = CARTESIAN_POINT('Ctrl Pts',(-11.2678365656403,13.5628934657056,
134.821774945397)) ;
#134201 = CARTESIAN_POINT('Ctrl Pts',(-11.2010465776116,13.5357169129533,
134.79706051815)) ;
#134202 = CARTESIAN_POINT('Ctrl Pts',(-11.2276030587525,13.4658311995141,
134.805074979322)) ;
#134203 = CARTESIAN_POINT('Ctrl Pts',(-11.1205249516122,13.4658311995141,
134.982414797281)) ;
#134204 = CARTESIAN_POINT('Ctrl Pts',(-11.1433187808326,13.3959454860749,
134.998198158856)) ;
#134205 = CARTESIAN_POINT('Ctrl Pts',(-11.1992381575979,13.4231220388272,
135.042237953121)) ;
#134206 = CARTESIAN_POINT('Ctrl Pts',(-11.2551575343632,13.4502985915795,
135.086277747385)) ;
#134207 = CARTESIAN_POINT('Ctrl Pts',(-11.2323637051428,13.5201843050187,
135.07049438581)) ;
#134208 = CARTESIAN_POINT('Ctrl Pts',(-11.2095698759223,13.5900700184579,
135.054711024235)) ;
#134209 = CARTESIAN_POINT('Ctrl Pts',(-11.1536504991571,13.5628934657056,
135.01067122997)) ;
#134210 = CARTESIAN_POINT('Ctrl Pts',(-11.0977311223918,13.5357169129533,
134.966631435705)) ;
#134211 = CARTESIAN_POINT('Ctrl Pts',(-11.1205249516122,13.4658311995141,
134.982414797281)) ;
#134212 = CARTESIAN_POINT('Ctrl Pts',(-10.9633031492974,13.4658311995141,
135.117701111297)) ;
#134213 = CARTESIAN_POINT('Ctrl Pts',(-10.9800904444232,13.3959454860749,
135.139700051809)) ;
#134214 = CARTESIAN_POINT('Ctrl Pts',(-11.0196342967342,13.4231220388272,
135.198730933269)) ;
#134215 = CARTESIAN_POINT('Ctrl Pts',(-11.0591781490452,13.4502985915795,
135.257761814729)) ;
#134216 = CARTESIAN_POINT('Ctrl Pts',(-11.0423908539194,13.5201843050187,
135.235762874218)) ;
#134217 = CARTESIAN_POINT('Ctrl Pts',(-11.0256035587936,13.5900700184578,
135.213763933706)) ;
#134218 = CARTESIAN_POINT('Ctrl Pts',(-10.9860597064826,13.5628934657056,
135.154733052246)) ;
#134219 = CARTESIAN_POINT('Ctrl Pts',(-10.9465158541716,13.5357169129533,
135.095702170786)) ;
#134220 = CARTESIAN_POINT('Ctrl Pts',(-10.9633031492974,13.4658311995141,
135.117701111297)) ;
#134221 = CARTESIAN_POINT('Ctrl Pts',(-10.7756218068419,13.4658311995141,
135.197451240537)) ;
#134222 = CARTESIAN_POINT('Ctrl Pts',(-10.7849240119387,13.3959454860749,
135.223477631156)) ;
#134223 = CARTESIAN_POINT('Ctrl Pts',(-10.8046490834956,13.4231220388272,
135.291658096106)) ;
#134224 = CARTESIAN_POINT('Ctrl Pts',(-10.8243741550525,13.4502985915795,
135.359838561057)) ;
#134225 = CARTESIAN_POINT('Ctrl Pts',(-10.8150719499557,13.5201843050187,
135.333812170438)) ;
#134226 = CARTESIAN_POINT('Ctrl Pts',(-10.8057697448589,13.5900700184579,
135.30778577982)) ;
#134227 = CARTESIAN_POINT('Ctrl Pts',(-10.786044673302,13.5628934657056,135.239605314869)) ;
#134228 = CARTESIAN_POINT('Ctrl Pts',(-10.7663196017452,13.5357169129533,
135.171424849918)) ;
#134229 = CARTESIAN_POINT('Ctrl Pts',(-10.7756218068419,13.4658311995141,
135.197451240537)) ;
#134230 = CARTESIAN_POINT('Ctrl Pts',(-10.572784802571,13.4658311995141,135.217973355629)) ;
#134231 = CARTESIAN_POINT('Ctrl Pts',(-10.5737445376646,13.3959454860749,
135.245627319145)) ;
#134232 = CARTESIAN_POINT('Ctrl Pts',(-10.5718329415469,13.4231220388272,
135.3166705477)) ;
#134233 = CARTESIAN_POINT('Ctrl Pts',(-10.5699213454292,13.4502985915795,
135.387713776254)) ;
#134234 = CARTESIAN_POINT('Ctrl Pts',(-10.5689616103356,13.5201843050187,
135.360059812739)) ;
#134235 = CARTESIAN_POINT('Ctrl Pts',(-10.5680018752419,13.5900700184579,
135.332405849223)) ;
#134236 = CARTESIAN_POINT('Ctrl Pts',(-10.5699134713596,13.5628934657056,
135.261362620669)) ;
#134237 = CARTESIAN_POINT('Ctrl Pts',(-10.5718250674773,13.5357169129533,
135.190319392114)) ;
#134238 = CARTESIAN_POINT('Ctrl Pts',(-10.572784802571,13.4658311995141,135.217973355629)) ;
#134239 = CARTESIAN_POINT('Ctrl Pts',(-10.3699582950185,13.4658311995141,
135.175134903948)) ;
#134240 = CARTESIAN_POINT('Ctrl Pts',(-10.362331940556,13.3959454860749,135.201787052399)) ;
#134241 = CARTESIAN_POINT('Ctrl Pts',(-10.3385749628922,13.4231220388272,
135.268914209501)) ;
#134242 = CARTESIAN_POINT('Ctrl Pts',(-10.3148179852285,13.4502985915795,
135.336041366603)) ;
#134243 = CARTESIAN_POINT('Ctrl Pts',(-10.322444339691,13.5201843050187,135.309389218153)) ;
#134244 = CARTESIAN_POINT('Ctrl Pts',(-10.3300706941535,13.5900700184579,
135.282737069703)) ;
#134245 = CARTESIAN_POINT('Ctrl Pts',(-10.3538276718172,13.5628934657056,
135.2156099126)) ;
#134246 = CARTESIAN_POINT('Ctrl Pts',(-10.377584649481,13.5357169129533,135.148482755498)) ;
#134247 = CARTESIAN_POINT('Ctrl Pts',(-10.3699582950185,13.4658311995141,
135.175134903948)) ;
#134248 = CARTESIAN_POINT('Ctrl Pts',(-10.1908705742325,13.4658311995141,
135.071278506368)) ;
#134249 = CARTESIAN_POINT('Ctrl Pts',(-10.1754087005963,13.3959454860749,
135.094305894918)) ;
#134250 = CARTESIAN_POINT('Ctrl Pts',(-10.132144438372,13.4231220388272,135.150910732527)) ;
#134251 = CARTESIAN_POINT('Ctrl Pts',(-10.0888801761478,13.4502985915795,
135.207515570136)) ;
#134252 = CARTESIAN_POINT('Ctrl Pts',(-10.1043420497839,13.5201843050187,
135.184488181586)) ;
#134253 = CARTESIAN_POINT('Ctrl Pts',(-10.11980392342,13.5900700184578,135.161460793036)) ;
#134254 = CARTESIAN_POINT('Ctrl Pts',(-10.1630681856443,13.5628934657056,
135.104855955427)) ;
#134255 = CARTESIAN_POINT('Ctrl Pts',(-10.2063324478686,13.5357169129533,
135.048251117818)) ;
#134256 = CARTESIAN_POINT('Ctrl Pts',(-10.1908705742325,13.4658311995141,
135.071278506368)) ;
#134257 = CARTESIAN_POINT('Ctrl Pts',(-10.0546595912401,13.4658311995141,
134.920519441332)) ;
#134258 = CARTESIAN_POINT('Ctrl Pts',(-10.0329617205844,13.3959454860749,
134.937811672168)) ;
#134259 = CARTESIAN_POINT('Ctrl Pts',(-9.97462287968318,13.4231220388272,
134.978735156726)) ;
#134260 = CARTESIAN_POINT('Ctrl Pts',(-9.91628403878198,13.4502985915795,
135.019658641283)) ;
#134261 = CARTESIAN_POINT('Ctrl Pts',(-9.93798190943768,13.5201843050187,
135.002366410447)) ;
#134262 = CARTESIAN_POINT('Ctrl Pts',(-9.95967978009337,13.5900700184578,
134.985074179611)) ;
#134263 = CARTESIAN_POINT('Ctrl Pts',(-10.0180186209946,13.5628934657056,
134.944150695053)) ;
#134264 = CARTESIAN_POINT('Ctrl Pts',(-10.0763574618958,13.5357169129533,
134.903227210496)) ;
#134265 = CARTESIAN_POINT('Ctrl Pts',(-10.0546595912401,13.4658311995141,
134.920519441332)) ;
#134266 = CARTESIAN_POINT('Ctrl Pts',(-9.96976593511389,13.4658311995141,
134.736076962611)) ;
#134267 = CARTESIAN_POINT('Ctrl Pts',(-9.94383295001097,13.3959454860749,
134.746039923768)) ;
#134268 = CARTESIAN_POINT('Ctrl Pts',(-9.87579920343744,13.4231220388272,
134.767509557221)) ;
#134269 = CARTESIAN_POINT('Ctrl Pts',(-9.8077654568639,13.4502985915795,134.788979190673)) ;
#134270 = CARTESIAN_POINT('Ctrl Pts',(-9.83369844196683,13.5201843050187,
134.779016229516)) ;
#134271 = CARTESIAN_POINT('Ctrl Pts',(-9.85963142706976,13.5900700184578,
134.769053268359)) ;
#134272 = CARTESIAN_POINT('Ctrl Pts',(-9.92766517364329,13.5628934657056,
134.747583634906)) ;
#134273 = CARTESIAN_POINT('Ctrl Pts',(-9.99569892021682,13.5357169129533,
134.726114001454)) ;
#134274 = CARTESIAN_POINT('Ctrl Pts',(-9.96976593511389,13.4658311995141,
134.736076962611)) ;
#134275 = CARTESIAN_POINT('Ctrl Pts',(-9.9450022707828,13.4658311995141,134.530889401624)) ;
#134276 = CARTESIAN_POINT('Ctrl Pts',(-9.91725078023896,13.3959454860749,
134.532432185862)) ;
#134277 = CARTESIAN_POINT('Ctrl Pts',(-9.84588765184722,13.4231220388272,
134.532030726634)) ;
#134278 = CARTESIAN_POINT('Ctrl Pts',(-9.7745245234555,13.4502985915795,134.531629267406)) ;
#134279 = CARTESIAN_POINT('Ctrl Pts',(-9.80227601399935,13.5201843050187,
134.530086483168)) ;
#134280 = CARTESIAN_POINT('Ctrl Pts',(-9.83002750454321,13.5900700184579,
134.52854369893)) ;
#134281 = CARTESIAN_POINT('Ctrl Pts',(-9.90139063293494,13.5628934657056,
134.528945158158)) ;
#134282 = CARTESIAN_POINT('Ctrl Pts',(-9.97275376132666,13.5357169129533,
134.529346617386)) ;
#134283 = CARTESIAN_POINT('Ctrl Pts',(-9.9450022707828,13.4658311995141,134.530889401624)) ;
#134284 = CARTESIAN_POINT('Ctrl Pts',(-9.98579846627996,13.4658311995141,
134.328087474358)) ;
#134285 = CARTESIAN_POINT('Ctrl Pts',(-9.95895961611388,13.3959454860749,
134.321058285225)) ;
#134286 = CARTESIAN_POINT('Ctrl Pts',(-9.89129025850839,13.4231220388272,
134.298825334214)) ;
#134287 = CARTESIAN_POINT('Ctrl Pts',(-9.8236209009029,13.4502985915795,134.276592383203)) ;
#134288 = CARTESIAN_POINT('Ctrl Pts',(-9.85045975106899,13.5201843050187,
134.283621572337)) ;
#134289 = CARTESIAN_POINT('Ctrl Pts',(-9.87729860123505,13.5900700184579,
134.29065076147)) ;
#134290 = CARTESIAN_POINT('Ctrl Pts',(-9.94496795884055,13.5628934657056,
134.312883712481)) ;
#134291 = CARTESIAN_POINT('Ctrl Pts',(-10.012637316446,13.5357169129533,134.335116663492)) ;
#134292 = CARTESIAN_POINT('Ctrl Pts',(-9.98579846627996,13.4658311995141,
134.328087474358)) ;
#134293 = CARTESIAN_POINT('Ctrl Pts',(-10.084932132731,13.4658311995141,134.150331039369)) ;
#134294 = CARTESIAN_POINT('Ctrl Pts',(-10.0615244873061,13.3959454860749,
134.135546052038)) ;
#134295 = CARTESIAN_POINT('Ctrl Pts',(-10.0038742640268,13.4231220388272,
134.093969291127)) ;
#134296 = CARTESIAN_POINT('Ctrl Pts',(-9.94622404074765,13.4502985915795,
134.052392530217)) ;
#134297 = CARTESIAN_POINT('Ctrl Pts',(-9.96963168617264,13.5201843050187,
134.067177517548)) ;
#134298 = CARTESIAN_POINT('Ctrl Pts',(-9.99303933159763,13.5900700184578,
134.08196250488)) ;
#134299 = CARTESIAN_POINT('Ctrl Pts',(-10.0506895548768,13.5628934657056,
134.12353926579)) ;
#134300 = CARTESIAN_POINT('Ctrl Pts',(-10.108339778156,13.5357169129533,134.165116026701)) ;
#134301 = CARTESIAN_POINT('Ctrl Pts',(-10.084932132731,13.4658311995141,134.150331039369)) ;
#134302 = CARTESIAN_POINT('Ctrl Pts',(-10.2325806005316,13.4658311995141,
134.009906610499)) ;
#134303 = CARTESIAN_POINT('Ctrl Pts',(-10.2147622260544,13.3959454860749,
133.98872944415)) ;
#134304 = CARTESIAN_POINT('Ctrl Pts',(-10.1724461134115,13.4231220388272,
133.931643368614)) ;
#134305 = CARTESIAN_POINT('Ctrl Pts',(-10.1301300007686,13.4502985915795,
133.874557293077)) ;
#134306 = CARTESIAN_POINT('Ctrl Pts',(-10.1479483752457,13.5201843050187,
133.895734459426)) ;
#134307 = CARTESIAN_POINT('Ctrl Pts',(-10.1657667497229,13.5900700184578,
133.916911625774)) ;
#134308 = CARTESIAN_POINT('Ctrl Pts',(-10.2080828623658,13.5628934657056,
133.973997701311)) ;
#134309 = CARTESIAN_POINT('Ctrl Pts',(-10.2503989750087,13.5357169129533,
134.031083776847)) ;
#134310 = CARTESIAN_POINT('Ctrl Pts',(-10.2325806005316,13.4658311995141,
134.009906610499)) ;
#134311 = CARTESIAN_POINT('Ctrl Pts',(-10.4193096302539,13.4658311995141,
133.919352405347)) ;
#134312 = CARTESIAN_POINT('Ctrl Pts',(-10.4088951913955,13.3959454860749,
133.893703082496)) ;
#134313 = CARTESIAN_POINT('Ctrl Pts',(-10.3862601761435,13.4231220388272,
133.826314652615)) ;
#134314 = CARTESIAN_POINT('Ctrl Pts',(-10.3636251608916,13.4502985915795,
133.758926222735)) ;
#134315 = CARTESIAN_POINT('Ctrl Pts',(-10.37403959975,13.5201843050187,133.784575545586)) ;
#134316 = CARTESIAN_POINT('Ctrl Pts',(-10.3844540386085,13.5900700184579,
133.810224868437)) ;
#134317 = CARTESIAN_POINT('Ctrl Pts',(-10.4070890538605,13.5628934657056,
133.877613298317)) ;
#134318 = CARTESIAN_POINT('Ctrl Pts',(-10.4297240691124,13.5357169129533,
133.945001728198)) ;
#134319 = CARTESIAN_POINT('Ctrl Pts',(-10.4193096302539,13.4658311995141,
133.919352405347)) ;
#134320 = CARTESIAN_POINT('Ctrl Pts',(-10.6249148927388,13.4658311995141,
133.891382896145)) ;
#134321 = CARTESIAN_POINT('Ctrl Pts',(-10.62292917198,13.3959454860749,133.863786357312)) ;
#134322 = CARTESIAN_POINT('Ctrl Pts',(-10.6222023784514,13.4231220388272,
133.79272927929)) ;
#134323 = CARTESIAN_POINT('Ctrl Pts',(-10.6214755849228,13.4502985915795,
133.721672201269)) ;
#134324 = CARTESIAN_POINT('Ctrl Pts',(-10.6234613056815,13.5201843050187,
133.749268740102)) ;
#134325 = CARTESIAN_POINT('Ctrl Pts',(-10.6254470264403,13.5900700184578,
133.776865278935)) ;
#134326 = CARTESIAN_POINT('Ctrl Pts',(-10.6261738199689,13.5628934657056,
133.847922356956)) ;
#134327 = CARTESIAN_POINT('Ctrl Pts',(-10.6269006134975,13.5357169129533,
133.918979434977)) ;
#134328 = CARTESIAN_POINT('Ctrl Pts',(-10.6249148927388,13.4658311995141,
133.891382896145)) ;
#134329 = CARTESIAN_POINT('Ctrl Pts',(-10.7598002515905,13.4658311995141,
133.915014269252)) ;
#134330 = CARTESIAN_POINT('Ctrl Pts',(-10.763505813003,13.3959454860749,133.887882392195)) ;
#134331 = CARTESIAN_POINT('Ctrl Pts',(-10.7772907287654,13.4231220388272,
133.818909929522)) ;
#134332 = CARTESIAN_POINT('Ctrl Pts',(-10.7910756445278,13.4502985915795,
133.74993746685)) ;
#134333 = CARTESIAN_POINT('Ctrl Pts',(-10.7873700831153,13.5201843050187,
133.777069343907)) ;
#134334 = CARTESIAN_POINT('Ctrl Pts',(-10.7836645217028,13.5900700184578,
133.804201220964)) ;
#134335 = CARTESIAN_POINT('Ctrl Pts',(-10.7698796059404,13.5628934657056,
133.873173683637)) ;
#134336 = CARTESIAN_POINT('Ctrl Pts',(-10.756094690178,13.5357169129533,133.942146146309)) ;
#134337 = CARTESIAN_POINT('Ctrl Pts',(-10.7598002515905,13.4658311995141,
133.915014269252)) ;
#134338 = CARTESIAN_POINT('Ctrl Pts',(-10.8223318974888,13.4658311995141,
133.936074466937)) ;
#134339 = CARTESIAN_POINT('Ctrl Pts',(-10.8287148089814,13.3959454860749,
133.909577338005)) ;
#134340 = CARTESIAN_POINT('Ctrl Pts',(-10.849260688724,13.4231220388272,133.842652384728)) ;
#134341 = CARTESIAN_POINT('Ctrl Pts',(-10.8698065684665,13.4502985915795,
133.77572743145)) ;
#134342 = CARTESIAN_POINT('Ctrl Pts',(-10.8634236569739,13.5201843050187,
133.802224560383)) ;
#134343 = CARTESIAN_POINT('Ctrl Pts',(-10.8570407454813,13.5900700184578,
133.828721689315)) ;
#134344 = CARTESIAN_POINT('Ctrl Pts',(-10.8364948657388,13.5628934657056,
133.895646642592)) ;
#134345 = CARTESIAN_POINT('Ctrl Pts',(-10.8159489859962,13.5357169129533,
133.96257159587)) ;
#134346 = CARTESIAN_POINT('Ctrl Pts',(-10.8223318974888,13.4658311995141,
133.936074466937)) ;
#134347 = CARTESIAN_POINT('Ctrl Pts',(-11.2645541045804,13.4658311995141,
134.606502068526)) ;
#134348 = CARTESIAN_POINT('Ctrl Pts',(-11.25920483017,13.4658311995141,134.672131214346)) ;
#134349 = CARTESIAN_POINT('Ctrl Pts',(-11.2276030587525,13.4658311995141,
134.805074979322)) ;
#134350 = CARTESIAN_POINT('Ctrl Pts',(-11.1205249516122,13.4658311995141,
134.982414797281)) ;
#134351 = CARTESIAN_POINT('Ctrl Pts',(-10.9633031492974,13.4658311995141,
135.117701111297)) ;
#134352 = CARTESIAN_POINT('Ctrl Pts',(-10.7756218068419,13.4658311995141,
135.197451240537)) ;
#134353 = CARTESIAN_POINT('Ctrl Pts',(-10.572784802571,13.4658311995141,135.217973355629)) ;
#134354 = CARTESIAN_POINT('Ctrl Pts',(-10.3699582950185,13.4658311995141,
135.175134903948)) ;
#134355 = CARTESIAN_POINT('Ctrl Pts',(-10.1908705742325,13.4658311995141,
135.071278506368)) ;
#134356 = CARTESIAN_POINT('Ctrl Pts',(-10.0546595912401,13.4658311995141,
134.920519441332)) ;
#134357 = CARTESIAN_POINT('Ctrl Pts',(-9.96976593511389,13.4658311995141,
134.736076962611)) ;
#134358 = CARTESIAN_POINT('Ctrl Pts',(-9.9450022707828,13.4658311995141,134.530889401624)) ;
#134359 = CARTESIAN_POINT('Ctrl Pts',(-9.98579846627996,13.4658311995141,
134.328087474358)) ;
#134360 = CARTESIAN_POINT('Ctrl Pts',(-10.084932132731,13.4658311995141,134.150331039369)) ;
#134361 = CARTESIAN_POINT('Ctrl Pts',(-10.2325806005316,13.4658311995141,
134.009906610499)) ;
#134362 = CARTESIAN_POINT('Ctrl Pts',(-10.4193096302539,13.4658311995141,
133.919352405347)) ;
#134363 = CARTESIAN_POINT('Ctrl Pts',(-10.6249148927388,13.4658311995141,
133.891382896145)) ;
#134364 = CARTESIAN_POINT('Ctrl Pts',(-10.7598002515905,13.4658311995141,
133.915014269252)) ;
#134365 = CARTESIAN_POINT('Ctrl Pts',(-10.8223318974888,13.4658311995141,
133.936074466937)) ;
#134366 = CARTESIAN_POINT('Origin',(-33.7895361580819,13.385947639229,127.22876720957)) ;
#134367 = CARTESIAN_POINT('',(-33.8079438763917,13.4658311995141,127.161214257016)) ;
#134368 = CARTESIAN_POINT('Origin',(-33.7873979966492,13.4930077522664,127.228139210294)) ;
#134369 = CARTESIAN_POINT('Ctrl Pts',(-33.3489959095147,13.1551399285885,
127.871927411069)) ;
#134370 = CARTESIAN_POINT('Ctrl Pts',(-33.3482570091173,13.1489709609094,
127.870499856875)) ;
#134371 = CARTESIAN_POINT('Ctrl Pts',(-33.3362031847492,13.0505878441039,
127.846970056077)) ;
#134372 = CARTESIAN_POINT('Ctrl Pts',(-33.303456104594,12.8648900473044,127.774282508598)) ;
#134373 = CARTESIAN_POINT('Ctrl Pts',(-33.2347176391245,12.6378996894465,
127.606502631126)) ;
#134374 = CARTESIAN_POINT('Ctrl Pts',(-33.1484631699894,12.4661938442505,
127.38763758675)) ;
#134375 = CARTESIAN_POINT('Ctrl Pts',(-33.0496339239794,12.3629468779938,
127.132205946451)) ;
#134376 = CARTESIAN_POINT('Ctrl Pts',(-32.9461836982222,12.3360866578135,
126.862930995212)) ;
#134377 = CARTESIAN_POINT('Ctrl Pts',(-32.8428524780797,12.3868467815327,
126.594300512203)) ;
#134378 = CARTESIAN_POINT('Ctrl Pts',(-32.7476240151848,12.5118616193735,
126.34920621096)) ;
#134379 = CARTESIAN_POINT('Ctrl Pts',(-32.6660393235339,12.7022376314793,
126.14402042184)) ;
#134380 = CARTESIAN_POINT('Ctrl Pts',(-32.6034202579729,12.9442211340136,
125.994217779495)) ;
#134381 = CARTESIAN_POINT('Ctrl Pts',(-32.5634889320909,13.2203922331636,
125.91068247448)) ;
#134382 = CARTESIAN_POINT('Ctrl Pts',(-32.5482836171183,13.5109001041669,
125.899354456419)) ;
#134383 = CARTESIAN_POINT('Ctrl Pts',(-32.5583885908025,13.7967277450532,
125.962163306551)) ;
#134384 = CARTESIAN_POINT('Ctrl Pts',(-32.5919970185865,14.0531634695327,
126.093303648423)) ;
#134385 = CARTESIAN_POINT('Ctrl Pts',(-32.6462352627175,14.2659161102292,
126.2848763833)) ;
#134386 = CARTESIAN_POINT('Ctrl Pts',(-32.7164440425069,14.4182155312585,
126.52308858485)) ;
#134387 = CARTESIAN_POINT('Ctrl Pts',(-32.7970929244734,14.4993926065239,
126.791896512519)) ;
#134388 = CARTESIAN_POINT('Ctrl Pts',(-32.8812312900771,14.5030674016304,
127.070805593369)) ;
#134389 = CARTESIAN_POINT('Ctrl Pts',(-32.9621947752627,14.4296658181567,
127.340390412531)) ;
#134390 = CARTESIAN_POINT('Ctrl Pts',(-33.0336799536047,14.2842405620309,
127.582320067705)) ;
#134391 = CARTESIAN_POINT('Ctrl Pts',(-33.0898518257578,14.0768885755418,
127.779563482544)) ;
#134392 = CARTESIAN_POINT('Ctrl Pts',(-33.1258131095785,13.821937566696,127.917839903426)) ;
#134393 = CARTESIAN_POINT('Ctrl Pts',(-33.1381603359796,13.5404397832619,
127.986888146398)) ;
#134394 = CARTESIAN_POINT('Ctrl Pts',(-33.1255862370588,13.2491903771815,
127.98329800545)) ;
#134395 = CARTESIAN_POINT('Ctrl Pts',(-33.0878760919221,12.9699188880577,
127.906345203758)) ;
#134396 = CARTESIAN_POINT('Ctrl Pts',(-33.0275630545352,12.7245502986717,
127.763166970814)) ;
#134397 = CARTESIAN_POINT('Ctrl Pts',(-32.9475449968705,12.5279694687298,
127.562611942766)) ;
#134398 = CARTESIAN_POINT('Ctrl Pts',(-32.853484832887,12.3961377043517,127.320906369453)) ;
#134399 = CARTESIAN_POINT('Ctrl Pts',(-32.7506275244767,12.3376103677892,
127.053662058531)) ;
#134400 = CARTESIAN_POINT('Ctrl Pts',(-32.6467508382538,12.3569098529355,
126.783214181605)) ;
#134401 = CARTESIAN_POINT('Ctrl Pts',(-32.5472606088073,12.452769019898,126.525790390631)) ;
#134402 = CARTESIAN_POINT('Ctrl Pts',(-32.4595735399336,12.6179593573441,
126.30272348908)) ;
#134403 = CARTESIAN_POINT('Ctrl Pts',(-32.388745121808,12.8405880377693,126.12891456918)) ;
#134404 = CARTESIAN_POINT('Ctrl Pts',(-32.3390681420419,13.1065246421439,
126.017073858121)) ;
#134405 = CARTESIAN_POINT('Ctrl Pts',(-32.313898204756,13.3925179674891,125.976505647384)) ;
#134406 = CARTESIAN_POINT('Ctrl Pts',(-32.3136699242009,13.6819916651313,
126.008953177836)) ;
#134407 = CARTESIAN_POINT('Ctrl Pts',(-32.3381285657715,13.9537242418059,
126.113619428421)) ;
#134408 = CARTESIAN_POINT('Ctrl Pts',(-32.384536696511,14.1863734291659,126.28227784121)) ;
#134409 = CARTESIAN_POINT('Ctrl Pts',(-32.4487957222161,14.3643807985693,
126.503053049914)) ;
#134410 = CARTESIAN_POINT('Ctrl Pts',(-32.5258074280907,14.4754559850244,
126.761140801679)) ;
#134411 = CARTESIAN_POINT('Ctrl Pts',(-32.6094667487868,14.5110246739577,
127.038737149779)) ;
#134412 = CARTESIAN_POINT('Ctrl Pts',(-32.6924145513944,14.4687063588107,
127.314091355005)) ;
#134413 = CARTESIAN_POINT('Ctrl Pts',(-32.7687110106265,14.3514018815055,
127.570143149353)) ;
#134414 = CARTESIAN_POINT('Ctrl Pts',(-32.8317732094795,14.1671964752596,
127.787539429963)) ;
#134415 = CARTESIAN_POINT('Ctrl Pts',(-32.8762267217076,13.9308608041133,
127.950416591701)) ;
#134416 = CARTESIAN_POINT('Ctrl Pts',(-32.8985780094168,13.6570089999716,
128.048890973466)) ;
#134417 = CARTESIAN_POINT('Ctrl Pts',(-32.896157678737,13.3664659574419,128.074980037028)) ;
#134418 = CARTESIAN_POINT('Ctrl Pts',(-32.8685548522265,13.0805681472547,
128.027442701697)) ;
#134419 = CARTESIAN_POINT('Ctrl Pts',(-32.8170821736547,12.8190539470386,
127.91017574478)) ;
#134420 = CARTESIAN_POINT('Ctrl Pts',(-32.7441829163896,12.5999338423892,
127.73048258649)) ;
#134421 = CARTESIAN_POINT('Ctrl Pts',(-32.6555170250936,12.4413957528131,
127.504429482033)) ;
#134422 = CARTESIAN_POINT('Ctrl Pts',(-32.5554705400289,12.3520378265489,
127.245337069314)) ;
#134423 = CARTESIAN_POINT('Ctrl Pts',(-32.4511053019089,12.339734386482,126.973578302647)) ;
#134424 = CARTESIAN_POINT('Ctrl Pts',(-32.3490815539954,12.4049383167358,
126.708653969777)) ;
#134425 = CARTESIAN_POINT('Ctrl Pts',(-32.2559652828001,12.5429634979505,
126.469740198936)) ;
#134426 = CARTESIAN_POINT('Ctrl Pts',(-32.1775406776191,12.7443553986761,
126.273802702315)) ;
#134427 = CARTESIAN_POINT('Ctrl Pts',(-32.1189511785612,12.9943521537239,
126.135786155147)) ;
#134428 = CARTESIAN_POINT('Ctrl Pts',(-32.0836266547703,13.2741647768729,
126.065632995122)) ;
#134429 = CARTESIAN_POINT('Ctrl Pts',(-32.0731422430725,13.565720269456,126.068169777388)) ;
#134430 = CARTESIAN_POINT('Ctrl Pts',(-32.0878672761987,13.8474315556546,
126.144404645481)) ;
#134431 = CARTESIAN_POINT('Ctrl Pts',(-32.1256175280986,14.0971649669908,
126.287692127083)) ;
#134432 = CARTESIAN_POINT('Ctrl Pts',(-32.1834742057281,14.3002122843455,
126.489943063825)) ;
#134433 = CARTESIAN_POINT('Ctrl Pts',(-32.2561937622249,14.4394509674979,
126.73551422792)) ;
#134434 = CARTESIAN_POINT('Ctrl Pts',(-32.3374471159419,14.5058688200503,
127.005843081603)) ;
#134435 = CARTESIAN_POINT('Ctrl Pts',(-32.4217002826958,14.4952594831202,
127.285155611484)) ;
#134436 = CARTESIAN_POINT('Ctrl Pts',(-32.5017471426193,14.4071576912799,
127.552229665334)) ;
#134437 = CARTESIAN_POINT('Ctrl Pts',(-32.5706761898774,14.2488070341169,
127.786694114575)) ;
#134438 = CARTESIAN_POINT('Ctrl Pts',(-32.6230717724866,14.032332595662,127.972746797191)) ;
#134439 = CARTESIAN_POINT('Ctrl Pts',(-32.6548239115267,13.7715185673777,
128.098623777025)) ;
#134440 = CARTESIAN_POINT('Ctrl Pts',(-32.6626680714647,13.4849968555095,
128.154735100321)) ;
#134441 = CARTESIAN_POINT('Ctrl Pts',(-32.6450616243189,13.1936954317484,
128.136543946875)) ;
#134442 = CARTESIAN_POINT('Ctrl Pts',(-32.6032602463952,12.9217410981826,
128.047311789015)) ;
#134443 = CARTESIAN_POINT('Ctrl Pts',(-32.5386314820962,12.6826993167214,
127.891757560495)) ;
#134444 = CARTESIAN_POINT('Ctrl Pts',(-32.4554412889622,12.4976839220085,
127.681914464153)) ;
#134445 = CARTESIAN_POINT('Ctrl Pts',(-32.3596753952525,12.3794711428103,
127.435114332308)) ;
#134446 = CARTESIAN_POINT('Ctrl Pts',(-32.2558253838943,12.3351744196322,
127.165019558565)) ;
#134447 = CARTESIAN_POINT('Ctrl Pts',(-32.1520107530796,12.3695012763354,
126.894875973638)) ;
#134448 = CARTESIAN_POINT('Ctrl Pts',(-32.0548036090535,12.4786183736045,
126.643923371603)) ;
#134449 = CARTESIAN_POINT('Ctrl Pts',(-31.9697179472944,12.6556201701116,
126.428500311369)) ;
#134450 = CARTESIAN_POINT('Ctrl Pts',(-31.9024466959007,12.8885376957079,
126.26521267139)) ;
#134451 = CARTESIAN_POINT('Ctrl Pts',(-31.8574815700017,13.1578672277872,
126.166847085394)) ;
#134452 = CARTESIAN_POINT('Ctrl Pts',(-31.8367167778053,13.4488181058444,
126.139492583638)) ;
#134453 = CARTESIAN_POINT('Ctrl Pts',(-31.8414313820349,13.7357351250712,
126.186316118843)) ;
#134454 = CARTESIAN_POINT('Ctrl Pts',(-31.8700151821842,14.0000244154435,
126.30281009704)) ;
#134455 = CARTESIAN_POINT('Ctrl Pts',(-31.9203616130848,14.2248063693443,
126.483142763909)) ;
#134456 = CARTESIAN_POINT('Ctrl Pts',(-31.9873859775564,14.3907221531774,
126.711954484493)) ;
#134457 = CARTESIAN_POINT('Ctrl Pts',(-32.0662309963865,14.4880878052934,
126.975454295977)) ;
#134458 = CARTESIAN_POINT('Ctrl Pts',(-32.1500140049146,14.5090844515927,
127.253273584441)) ;
#134459 = CARTESIAN_POINT('Ctrl Pts',(-32.2328114906108,14.4517331277302,
127.528461364111)) ;
#134460 = CARTESIAN_POINT('Ctrl Pts',(-32.306599429151,14.3213873494252,127.777000865602)) ;
#134461 = CARTESIAN_POINT('Ctrl Pts',(-32.3665410586647,14.1266126254878,
127.985228303146)) ;
#134462 = CARTESIAN_POINT('Ctrl Pts',(-32.4072983071001,13.8801113803002,
128.137553257528)) ;
#134463 = CARTESIAN_POINT('Ctrl Pts',(-32.4248919159062,13.6025840232108,
128.221986639911)) ;
#134464 = CARTESIAN_POINT('Ctrl Pts',(-32.4177985341224,13.3122088978665,
128.234314532032)) ;
#134465 = CARTESIAN_POINT('Ctrl Pts',(-32.3854612722872,13.0284665595888,
128.173051822567)) ;
#134466 = CARTESIAN_POINT('Ctrl Pts',(-32.3297158719588,12.7739765033465,
128.043289524966)) ;
#134467 = CARTESIAN_POINT('Ctrl Pts',(-32.2536312710535,12.5655228915478,
127.854171141032)) ;
#134468 = CARTESIAN_POINT('Ctrl Pts',(-32.1621333883639,12.4188418488155,
127.619973715704)) ;
#134469 = CARTESIAN_POINT('Ctrl Pts',(-32.0610335191924,12.3438198182334,
127.357704488195)) ;
#134470 = CARTESIAN_POINT('Ctrl Pts',(-31.9562422849269,12.3461749880073,
127.084814084959)) ;
#134471 = CARTESIAN_POINT('Ctrl Pts',(-31.8555595514267,12.4256199459212,
126.823755799531)) ;
#134472 = CARTESIAN_POINT('Ctrl Pts',(-31.7646812381954,12.5766359900473,
126.591428395529)) ;
#134473 = CARTESIAN_POINT('Ctrl Pts',(-31.6897549709183,12.7882864475543,
126.405673808487)) ;
#134474 = CARTESIAN_POINT('Ctrl Pts',(-31.6353440859288,13.0452019382586,
126.279829886042)) ;
#134475 = CARTESIAN_POINT('Ctrl Pts',(-31.6045551307125,13.3293877258915,
126.223017390213)) ;
#134476 = CARTESIAN_POINT('Ctrl Pts',(-31.598929994185,13.6204035856812,126.239726726341)) ;
#134477 = CARTESIAN_POINT('Ctrl Pts',(-31.6181519561243,13.8971496153171,
126.329008321255)) ;
#134478 = CARTESIAN_POINT('Ctrl Pts',(-31.660032440097,14.1397539052331,126.4844492787)) ;
#134479 = CARTESIAN_POINT('Ctrl Pts',(-31.7210074180807,14.3313464702874,
126.695729086547)) ;
#134480 = CARTESIAN_POINT('Ctrl Pts',(-31.7956413070931,14.4574458616527,
126.94680082343)) ;
#134481 = CARTESIAN_POINT('Ctrl Pts',(-31.8782525153513,14.5099723944026,
127.221254124399)) ;
#134482 = CARTESIAN_POINT('Ctrl Pts',(-31.9622607746967,14.4843439695083,
127.499872427198)) ;
#134483 = CARTESIAN_POINT('Ctrl Pts',(-32.0404152099778,14.3827749410654,
127.761275810437)) ;
#134484 = CARTESIAN_POINT('Ctrl Pts',(-32.1067647607671,14.2124739950545,
127.988225629159)) ;
#134485 = CARTESIAN_POINT('Ctrl Pts',(-32.1557319181306,13.9855789386979,
128.164396849995)) ;
#134486 = CARTESIAN_POINT('Ctrl Pts',(-32.1830886305706,13.7185805864342,
128.27741749427)) ;
#134487 = CARTESIAN_POINT('Ctrl Pts',(-32.1861674536437,13.4303185636673,
128.319530923703)) ;
#134488 = CARTESIAN_POINT('Ctrl Pts',(-32.164067606359,13.1417758325219,128.288060327875)) ;
#134489 = CARTESIAN_POINT('Ctrl Pts',(-32.1174319130124,12.8725286043858,
128.185023246156)) ;
#134490 = CARTESIAN_POINT('Ctrl Pts',(-32.0491401802662,12.6435096258014,
128.018626363072)) ;
#134491 = CARTESIAN_POINT('Ctrl Pts',(-31.9632199754991,12.4701546223289,
127.800755651149)) ;
#134492 = CARTESIAN_POINT('Ctrl Pts',(-31.8651776863348,12.3650501876111,
127.547453264018)) ;
#134493 = CARTESIAN_POINT('Ctrl Pts',(-31.7609862185599,12.3357586674927,
127.276274914652)) ;
#134494 = CARTESIAN_POINT('Ctrl Pts',(-31.6580563102104,12.3843195509594,
127.008647533804)) ;
#134495 = CARTESIAN_POINT('Ctrl Pts',(-31.5623522569141,12.5073666683789,
126.762219617398)) ;
#134496 = CARTESIAN_POINT('Ctrl Pts',(-31.4804283317136,12.6958200369819,
126.55599240923)) ;
#134497 = CARTESIAN_POINT('Ctrl Pts',(-31.4171911262104,12.9363649293222,
126.404372140452)) ;
#134498 = CARTESIAN_POINT('Ctrl Pts',(-31.3765204454803,13.212046231595,126.318705695641)) ;
#134499 = CARTESIAN_POINT('Ctrl Pts',(-31.3605890149829,13.5022481067603,
126.305235943963)) ;
#134500 = CARTESIAN_POINT('Ctrl Pts',(-31.3699466511949,13.7884016128943,
126.365844507772)) ;
#134501 = CARTESIAN_POINT('Ctrl Pts',(-31.402839929772,14.045945075732,126.494887877481)) ;
#134502 = CARTESIAN_POINT('Ctrl Pts',(-31.456801839307,14.2610680704969,126.685797164984)) ;
#134503 = CARTESIAN_POINT('Ctrl Pts',(-31.5263791105061,14.4145624165552,
126.922033359285)) ;
#134504 = CARTESIAN_POINT('Ctrl Pts',(-31.6068029650713,14.4980852125695,
127.190187763467)) ;
#134505 = CARTESIAN_POINT('Ctrl Pts',(-31.6909497784616,14.5041312739862,
127.469125424148)) ;
#134506 = CARTESIAN_POINT('Ctrl Pts',(-31.7722616933248,14.4326962339747,
127.739802187408)) ;
#134507 = CARTESIAN_POINT('Ctrl Pts',(-31.8440399327869,14.289424830309,127.982545178335)) ;
#134508 = CARTESIAN_POINT('Ctrl Pts',(-31.9008586342929,14.0826507854277,
128.181809264848)) ;
#134509 = CARTESIAN_POINT('Ctrl Pts',(-31.9371644477761,13.8312291814697,
128.320780138694)) ;
#134510 = CARTESIAN_POINT('Ctrl Pts',(-31.9504192122518,13.5479805821752,
128.392761416066)) ;
#134511 = CARTESIAN_POINT('Ctrl Pts',(-31.9384428607775,13.2572981016289,
128.390846357411)) ;
#134512 = CARTESIAN_POINT('Ctrl Pts',(-31.9016603090654,12.9781391944844,
128.316499055668)) ;
#134513 = CARTESIAN_POINT('Ctrl Pts',(-31.8414344653115,12.7298471383749,
128.173831316095)) ;
#134514 = CARTESIAN_POINT('Ctrl Pts',(-31.7624693619783,12.5331718510569,
127.976098656417)) ;
#134515 = CARTESIAN_POINT('Ctrl Pts',(-31.6682896816273,12.3987050488903,
127.734214112554)) ;
#134516 = CARTESIAN_POINT('Ctrl Pts',(-31.5661584069127,12.3381977133859,
127.468894861423)) ;
#134517 = CARTESIAN_POINT('Ctrl Pts',(-31.4613121151811,12.3556285786372,
127.195919765139)) ;
#134518 = CARTESIAN_POINT('Ctrl Pts',(-31.3626542471411,12.448498640132,126.940567661376)) ;
#134519 = CARTESIAN_POINT('Ctrl Pts',(-31.2739963638957,12.6124651727369,
126.714860191145)) ;
#134520 = CARTESIAN_POINT('Ctrl Pts',(-31.2028733579617,12.8330193864531,
126.540078371683)) ;
#134521 = CARTESIAN_POINT('Ctrl Pts',(-31.1524099899045,13.0981216515098,
126.425973898796)) ;
#134522 = CARTESIAN_POINT('Ctrl Pts',(-31.1264884036244,13.3840423616995,
126.383240800023)) ;
#134523 = CARTESIAN_POINT('Ctrl Pts',(-31.1255526905879,13.6738043197191,
126.413632148392)) ;
#134524 = CARTESIAN_POINT('Ctrl Pts',(-31.1492407119047,13.9458856450603,
126.515980892251)) ;
#134525 = CARTESIAN_POINT('Ctrl Pts',(-31.1951906788803,14.1805609741337,
126.683399895541)) ;
#134526 = CARTESIAN_POINT('Ctrl Pts',(-31.2589322113538,14.3602096703021,
126.902625201214)) ;
#134527 = CARTESIAN_POINT('Ctrl Pts',(-31.336152907064,14.4737146563849,127.161521971997)) ;
#134528 = CARTESIAN_POINT('Ctrl Pts',(-31.4191607366893,14.510981736058,127.436983917868)) ;
#134529 = CARTESIAN_POINT('Ctrl Pts',(-31.5023202222332,14.4710234538019,
127.713002150618)) ;
#134530 = CARTESIAN_POINT('Ctrl Pts',(-31.5788150531214,14.3558611755068,
127.9695934644)) ;
#134531 = CARTESIAN_POINT('Ctrl Pts',(-31.6423459010436,14.1736059642118,
128.188348020273)) ;
#134532 = CARTESIAN_POINT('Ctrl Pts',(-31.6874883180192,13.9381264816024,
128.353301532308)) ;
#134533 = CARTESIAN_POINT('Ctrl Pts',(-31.7104598612239,13.665192099168,128.453567738071)) ;
#134534 = CARTESIAN_POINT('Ctrl Pts',(-31.7088598170554,13.3755914984187,
128.481967244671)) ;
#134535 = CARTESIAN_POINT('Ctrl Pts',(-31.6817723867748,13.0874857506397,
128.436147123456)) ;
#134536 = CARTESIAN_POINT('Ctrl Pts',(-31.6311222896079,12.8264337657975,
128.32111606456)) ;
#134537 = CARTESIAN_POINT('Ctrl Pts',(-31.5590254861687,12.6060974389448,
128.143694924089)) ;
#134538 = CARTESIAN_POINT('Ctrl Pts',(-31.4705496041744,12.4450313389733,
127.91828768914)) ;
#134539 = CARTESIAN_POINT('Ctrl Pts',(-31.3704536339561,12.3534666197661,
127.659136554107)) ;
#134540 = CARTESIAN_POINT('Ctrl Pts',(-31.2664260741019,12.3390029903486,
127.388267266672)) ;
#134541 = CARTESIAN_POINT('Ctrl Pts',(-31.1640074542676,12.4020392430349,
127.122262231831)) ;
#134542 = CARTESIAN_POINT('Ctrl Pts',(-31.0704546098695,12.5385711173323,
126.882123477286)) ;
#134543 = CARTESIAN_POINT('Ctrl Pts',(-30.9919375233747,12.737337324062,126.685748126109)) ;
#134544 = CARTESIAN_POINT('Ctrl Pts',(-30.9326059877163,12.9861206892308,
126.545580982005)) ;
#134545 = CARTESIAN_POINT('Ctrl Pts',(-30.8964828802307,13.2660910782566,
126.473182758033)) ;
#134546 = CARTESIAN_POINT('Ctrl Pts',(-30.8853353619794,13.5573227840952,
126.473749977841)) ;
#134547 = CARTESIAN_POINT('Ctrl Pts',(-30.8992181639316,13.8386952169897,
126.547405844888)) ;
#134548 = CARTESIAN_POINT('Ctrl Pts',(-30.9364490028324,14.0906007554108,
126.689305896974)) ;
#134549 = CARTESIAN_POINT('Ctrl Pts',(-30.993577379338,14.2945039762926,126.889303441531)) ;
#134550 = CARTESIAN_POINT('Ctrl Pts',(-31.0658785833472,14.4361574187858,
127.133657392973)) ;
#134551 = CARTESIAN_POINT('Ctrl Pts',(-31.1473678175875,14.5051117570611,
127.404837868273)) ;
#134552 = CARTESIAN_POINT('Ctrl Pts',(-31.2314101845586,14.496582620466,127.68344430737)) ;
#134553 = CARTESIAN_POINT('Ctrl Pts',(-31.3113999047549,14.4113394819302,
127.950224339128)) ;
#134554 = CARTESIAN_POINT('Ctrl Pts',(-31.3810275644355,14.2546479447355,
128.186843915728)) ;
#134555 = CARTESIAN_POINT('Ctrl Pts',(-31.434079388976,14.039143877786,128.374888028828)) ;
#134556 = CARTESIAN_POINT('Ctrl Pts',(-31.4664410188237,13.7793416572316,
128.502539340318)) ;
#134557 = CARTESIAN_POINT('Ctrl Pts',(-31.4749982660917,13.4941095874199,
128.560637934817)) ;
#134558 = CARTESIAN_POINT('Ctrl Pts',(-31.4582310109701,13.2026874966814,
128.544890911873)) ;
#134559 = CARTESIAN_POINT('Ctrl Pts',(-31.4169753439866,12.928833346161,128.457383735722)) ;
#134560 = CARTESIAN_POINT('Ctrl Pts',(-31.3527956487623,12.6885083712283,
128.303172142516)) ;
#134561 = CARTESIAN_POINT('Ctrl Pts',(-31.2705703901443,12.5026390795781,
128.0959611027)) ;
#134562 = CARTESIAN_POINT('Ctrl Pts',(-31.1745744230575,12.3816810236162,
127.848677279268)) ;
#134563 = CARTESIAN_POINT('Ctrl Pts',(-31.0714307037018,12.3354826595071,
127.580451601079)) ;
#134564 = CARTESIAN_POINT('Ctrl Pts',(-30.9672895160686,12.3671988660942,
127.309429336125)) ;
#134565 = CARTESIAN_POINT('Ctrl Pts',(-30.8693900237751,12.4748749581507,
127.056599017908)) ;
#134566 = CARTESIAN_POINT('Ctrl Pts',(-30.7841568236753,12.6498955190515,
126.840662152846)) ;
#134567 = CARTESIAN_POINT('Ctrl Pts',(-30.7165115975955,12.8801431332148,
126.67612667683)) ;
#134568 = CARTESIAN_POINT('Ctrl Pts',(-30.6705876552176,13.1504415297617,
126.575185235204)) ;
#134569 = CARTESIAN_POINT('Ctrl Pts',(-30.6492401911973,13.438739202615,126.545850310757)) ;
#134570 = CARTESIAN_POINT('Ctrl Pts',(-30.6531248486497,13.7280473502378,
126.590480521703)) ;
#134571 = CARTESIAN_POINT('Ctrl Pts',(-30.6811874381857,13.9932362064335,
126.705468605857)) ;
#134572 = CARTESIAN_POINT('Ctrl Pts',(-30.7307233901376,14.2186783745982,
126.88330032276)) ;
#134573 = CARTESIAN_POINT('Ctrl Pts',(-30.7976668939673,14.3872014330787,
127.112042032862)) ;
#134574 = CARTESIAN_POINT('Ctrl Pts',(-30.8759215226086,14.486216521528,127.373662762679)) ;
#134575 = CARTESIAN_POINT('Ctrl Pts',(-30.9599483085192,14.5095010567365,
127.652320679818)) ;
#134576 = CARTESIAN_POINT('Ctrl Pts',(-31.0423602583126,14.4548476689191,
127.926162766265)) ;
#134577 = CARTESIAN_POINT('Ctrl Pts',(-31.1170261636548,14.3259646517619,
128.177490633467)) ;
#134578 = CARTESIAN_POINT('Ctrl Pts',(-31.1774376241067,14.1320240566172,
128.38715540167)) ;
#134579 = CARTESIAN_POINT('Ctrl Pts',(-31.2184772814882,13.8890687487633,
128.540002184362)) ;
#134580 = CARTESIAN_POINT('Ctrl Pts',(-31.2369718788586,13.6109288487181,
128.62723857725)) ;
#134581 = CARTESIAN_POINT('Ctrl Pts',(-31.2305830637653,13.3205780973656,
128.64162358396)) ;
#134582 = CARTESIAN_POINT('Ctrl Pts',(-31.1988306507602,13.0356410236252,
128.582156307125)) ;
#134583 = CARTESIAN_POINT('Ctrl Pts',(-31.1439236012217,12.7811568557338,
128.454705635715)) ;
#134584 = CARTESIAN_POINT('Ctrl Pts',(-31.0684038299569,12.5709851276515,
128.267243241426)) ;
#134585 = CARTESIAN_POINT('Ctrl Pts',(-30.9772756205,12.4221766619671,128.03413250274)) ;
#134586 = CARTESIAN_POINT('Ctrl Pts',(-30.8759319496152,12.3447406812541,
127.771290965256)) ;
#134587 = CARTESIAN_POINT('Ctrl Pts',(-30.7712963261735,12.3451621602759,
127.498804673837)) ;
#134588 = CARTESIAN_POINT('Ctrl Pts',(-30.6706886680026,12.4221617733591,
127.237875690043)) ;
#134589 = CARTESIAN_POINT('Ctrl Pts',(-30.5793389036692,12.5713293574021,
127.00420358355)) ;
#134590 = CARTESIAN_POINT('Ctrl Pts',(-30.5039469378259,12.7811357471148,
126.817049360709)) ;
#134591 = CARTESIAN_POINT('Ctrl Pts',(-30.4488110435835,13.037385413305,126.689142569762)) ;
#134592 = CARTESIAN_POINT('Ctrl Pts',(-30.4173468141487,13.3202247802994,
126.630258735514)) ;
#134593 = CARTESIAN_POINT('Ctrl Pts',(-30.4109588954888,13.6126649497902,
126.644895127432)) ;
#134594 = CARTESIAN_POINT('Ctrl Pts',(-30.4294392941911,13.889109539137,126.731888107809)) ;
#134595 = CARTESIAN_POINT('Ctrl Pts',(-30.47077570761,14.1334576219234,126.885811226843)) ;
#134596 = CARTESIAN_POINT('Ctrl Pts',(-30.53102912446,14.3262010857029,127.094865661672)) ;
#134597 = CARTESIAN_POINT('Ctrl Pts',(-30.6058078949067,14.4552702241494,
127.346574791049)) ;
#134598 = CARTESIAN_POINT('Ctrl Pts',(-30.6883760016807,14.5094659873619,
127.620923977953)) ;
#134599 = CARTESIAN_POINT('Ctrl Pts',(-30.7718896570381,14.48627928254,127.897878479629)) ;
#134600 = CARTESIAN_POINT('Ctrl Pts',(-30.8505404170833,14.3867194330965,
128.16082928885)) ;
#134601 = CARTESIAN_POINT('Ctrl Pts',(-30.9172652518935,14.2183273389604,
128.388850744567)) ;
#134602 = CARTESIAN_POINT('Ctrl Pts',(-30.966927867041,13.9922441011096,128.567141543632)) ;
#134603 = CARTESIAN_POINT('Ctrl Pts',(-30.9948429554227,13.7260908863955,
128.681785518138)) ;
#134604 = CARTESIAN_POINT('Ctrl Pts',(-30.9986761317404,13.4392990683917,
128.725970798859)) ;
#134605 = CARTESIAN_POINT('Ctrl Pts',(-30.9771754995003,13.1491383926391,
128.696410048975)) ;
#134606 = CARTESIAN_POINT('Ctrl Pts',(-30.9313862314932,12.880138144259,128.595705294773)) ;
#134607 = CARTESIAN_POINT('Ctrl Pts',(-30.8633741700187,12.6488312040692,
128.430267551873)) ;
#134608 = CARTESIAN_POINT('Ctrl Pts',(-30.7783096718615,12.4746173052797,
128.214724190605)) ;
#134609 = CARTESIAN_POINT('Ctrl Pts',(-30.6802839201009,12.3669410581914,
127.961566303494)) ;
#134610 = CARTESIAN_POINT('Ctrl Pts',(-30.5761954681339,12.3355244467329,
127.690674965918)) ;
#134611 = CARTESIAN_POINT('Ctrl Pts',(-30.4731987242308,12.3818824637266,
127.42284013735)) ;
#134612 = CARTESIAN_POINT('Ctrl Pts',(-30.3773601675738,12.502442440452,127.175947943775)) ;
#134613 = CARTESIAN_POINT('Ctrl Pts',(-30.2945593439143,12.6900860359651,
126.967322197996)) ;
#134614 = CARTESIAN_POINT('Ctrl Pts',(-30.2309201264915,12.9290693621117,
126.814464075625)) ;
#134615 = CARTESIAN_POINT('Ctrl Pts',(-30.1896011311781,13.2033802627449,
126.726833819823)) ;
#134616 = CARTESIAN_POINT('Ctrl Pts',(-30.1729187517655,13.493885424346,126.711224329232)) ;
#134617 = CARTESIAN_POINT('Ctrl Pts',(-30.1814818466642,13.7798208359641,
126.769425110779)) ;
#134618 = CARTESIAN_POINT('Ctrl Pts',(-30.2139166442141,14.0398147256928,
126.897315524147)) ;
#134619 = CARTESIAN_POINT('Ctrl Pts',(-30.2672327260932,14.2555980954836,
127.086230738633)) ;
#134620 = CARTESIAN_POINT('Ctrl Pts',(-30.3364241626342,14.4112165057251,
127.321355815591)) ;
#134621 = CARTESIAN_POINT('Ctrl Pts',(-30.4169483545396,14.4969135755094,
127.589920286704)) ;
#134622 = CARTESIAN_POINT('Ctrl Pts',(-30.5006568417281,14.5049696810031,
127.867411820872)) ;
#134623 = CARTESIAN_POINT('Ctrl Pts',(-30.5821059141925,14.4360249735447,
128.13846691764)) ;
#134624 = CARTESIAN_POINT('Ctrl Pts',(-30.6543269887437,14.2945754362065,
128.382542123477)) ;
#134625 = CARTESIAN_POINT('Ctrl Pts',(-30.7116365732865,14.0897548858671,
128.583199406406)) ;
#134626 = CARTESIAN_POINT('Ctrl Pts',(-30.7486474004249,13.8387001375239,
128.724327683098)) ;
#134627 = CARTESIAN_POINT('Ctrl Pts',(-30.7626160375506,13.5574044598577,
128.79823198023)) ;
#134628 = CARTESIAN_POINT('Ctrl Pts',(-30.751280169492,13.2644130009093,128.798450590054)) ;
#134629 = CARTESIAN_POINT('Ctrl Pts',(-30.7152762753897,12.9862195730077,
128.726198614227)) ;
#134630 = CARTESIAN_POINT('Ctrl Pts',(-30.6559255495121,12.7371111819008,
128.586013158079)) ;
#134631 = CARTESIAN_POINT('Ctrl Pts',(-30.5772199975952,12.5380203242925,
128.389149798631)) ;
#134632 = CARTESIAN_POINT('Ctrl Pts',(-30.4833480932253,12.4015272632005,
128.148171071429)) ;
#134633 = CARTESIAN_POINT('Ctrl Pts',(-30.3812924082162,12.3389470103484,
127.883098879055)) ;
#134634 = CARTESIAN_POINT('Ctrl Pts',(-30.2769531606877,12.3537864997403,
127.611426962061)) ;
#134635 = CARTESIAN_POINT('Ctrl Pts',(-30.1774142848297,12.4449099176858,
127.353712328041)) ;
#134636 = CARTESIAN_POINT('Ctrl Pts',(-30.0884196313121,12.6072327563546,
127.127011108624)) ;
#134637 = CARTESIAN_POINT('Ctrl Pts',(-30.0168944583603,12.8259751420657,
126.950999128042)) ;
#134638 = CARTESIAN_POINT('Ctrl Pts',(-29.9658131020968,13.0894865209779,
126.835020394129)) ;
#134639 = CARTESIAN_POINT('Ctrl Pts',(-29.9390402950618,13.3763086244584,
126.789949510195)) ;
#134640 = CARTESIAN_POINT('Ctrl Pts',(-29.9374976893148,13.666102426872,126.818551688385)) ;
#134641 = CARTESIAN_POINT('Ctrl Pts',(-29.9603659689101,13.9378774393092,
126.918366530385)) ;
#134642 = CARTESIAN_POINT('Ctrl Pts',(-30.0058557147277,14.174793298913,127.084558461599)) ;
#134643 = CARTESIAN_POINT('Ctrl Pts',(-30.0690738202602,14.355667987911,127.302193672896)) ;
#134644 = CARTESIAN_POINT('Ctrl Pts',(-30.1455851444044,14.4711053294092,
127.558860146817)) ;
#134645 = CARTESIAN_POINT('Ctrl Pts',(-30.2290907276294,14.511170979715,127.836014853784)) ;
#134646 = CARTESIAN_POINT('Ctrl Pts',(-30.3124346958538,14.4729025341711,
128.112614820692)) ;
#134647 = CARTESIAN_POINT('Ctrl Pts',(-30.3888326028229,14.3605014183323,
128.368750566373)) ;
#134648 = CARTESIAN_POINT('Ctrl Pts',(-30.4531791538599,14.1789799497678,
128.590078616567)) ;
#134649 = CARTESIAN_POINT('Ctrl Pts',(-30.4986908853725,13.9453130755044,
128.756011357139)) ;
#134650 = CARTESIAN_POINT('Ctrl Pts',(-30.5223367702664,13.673613297581,128.858202384461)) ;
#134651 = CARTESIAN_POINT('Ctrl Pts',(-30.5214927257582,13.3843416477693,
128.888796839614)) ;
#134652 = CARTESIAN_POINT('Ctrl Pts',(-30.4951356796959,13.0956424787648,
128.845131685907)) ;
#134653 = CARTESIAN_POINT('Ctrl Pts',(-30.4451353943437,12.8335787485534,
128.73200501772)) ;
#134654 = CARTESIAN_POINT('Ctrl Pts',(-30.3735874311193,12.6116522531053,
128.556195762552)) ;
#134655 = CARTESIAN_POINT('Ctrl Pts',(-30.2853579635812,12.4486058050818,
128.33155990322)) ;
#134656 = CARTESIAN_POINT('Ctrl Pts',(-30.1858663129506,12.3551665981467,
128.074050595748)) ;
#134657 = CARTESIAN_POINT('Ctrl Pts',(-30.0815496988783,12.3383111368361,
127.802444396815)) ;
#134658 = CARTESIAN_POINT('Ctrl Pts',(-29.9791399961725,12.3991318667188,
127.536410522558)) ;
#134659 = CARTESIAN_POINT('Ctrl Pts',(-29.885250975789,12.5336133546432,127.2952913997)) ;
#134660 = CARTESIAN_POINT('Ctrl Pts',(-29.8062098846917,12.7304747525644,
127.097365942919)) ;
#134661 = CARTESIAN_POINT('Ctrl Pts',(-29.7459166115697,12.9801493565206,
126.954643707808)) ;
#134662 = CARTESIAN_POINT('Ctrl Pts',(-29.7094981424688,13.2569930870622,
126.881074054437)) ;
#134663 = CARTESIAN_POINT('Ctrl Pts',(-29.697485321225,13.5493201067258,126.879249155707)) ;
#134664 = CARTESIAN_POINT('Ctrl Pts',(-29.7107148915496,13.8310609228274,
126.950973130347)) ;
#134665 = CARTESIAN_POINT('Ctrl Pts',(-29.7473686079901,14.0843638099265,
127.091228525209)) ;
#134666 = CARTESIAN_POINT('Ctrl Pts',(-29.8039983073089,14.2896244491401,
127.289751241016)) ;
#134667 = CARTESIAN_POINT('Ctrl Pts',(-29.8758248177242,14.4330063116879,
127.5326649792)) ;
#134668 = CARTESIAN_POINT('Ctrl Pts',(-29.9571776043441,14.5042107415309,
127.803464708327)) ;
#134669 = CARTESIAN_POINT('Ctrl Pts',(-30.0412713276901,14.4979449999679,
128.082232149485)) ;
#134670 = CARTESIAN_POINT('Ctrl Pts',(-30.121694639328,14.4144601779744,128.350375838408)) ;
#134671 = CARTESIAN_POINT('Ctrl Pts',(-30.1915790917938,14.2595209902124,
128.587713560571)) ;
#134672 = CARTESIAN_POINT('Ctrl Pts',(-30.2450076010872,14.046214919979,128.776755103724)) ;
#134673 = CARTESIAN_POINT('Ctrl Pts',(-30.2780878046331,13.7868053449528,
128.906585374679)) ;
#134674 = CARTESIAN_POINT('Ctrl Pts',(-30.2872906950602,13.5027357390144,
128.966484763682)) ;
#134675 = CARTESIAN_POINT('Ctrl Pts',(-30.2713500951273,13.2114164567146,
128.953122045362)) ;
#134676 = CARTESIAN_POINT('Ctrl Pts',(-30.230627814723,12.9359342983456,128.86728322249)) ;
#134677 = CARTESIAN_POINT('Ctrl Pts',(-30.1672447422047,12.6951562018299,
128.715288751686)) ;
#134678 = CARTESIAN_POINT('Ctrl Pts',(-30.0854978465419,12.5073061272103,
128.509491429827)) ;
#134679 = CARTESIAN_POINT('Ctrl Pts',(-29.9896882822811,12.3841592686752,
128.262793679839)) ;
#134680 = CARTESIAN_POINT('Ctrl Pts',(-29.8866361087517,12.3356200239572,
127.994841190901)) ;
#134681 = CARTESIAN_POINT('Ctrl Pts',(-29.7820423738734,12.3655842279676,
127.722626897302)) ;
#134682 = CARTESIAN_POINT('Ctrl Pts',(-29.6846378874882,12.4702048591763,
127.470973299483)) ;
#134683 = CARTESIAN_POINT('Ctrl Pts',(-29.5982444318826,12.6448837976238,
127.251934053335)) ;
#134684 = CARTESIAN_POINT('Ctrl Pts',(-29.530484788473,12.872508423284,127.086857758343)) ;
#134685 = CARTESIAN_POINT('Ctrl Pts',(-29.4836133061575,13.1434988331289,
126.983345728084)) ;
#134686 = CARTESIAN_POINT('Ctrl Pts',(-29.4617927517553,13.4301737780494,
126.952467269919)) ;
#134687 = CARTESIAN_POINT('Ctrl Pts',(-29.4647728375027,13.7187795914099,
126.994328449619)) ;
#134688 = CARTESIAN_POINT('Ctrl Pts',(-29.4924039666026,13.9870154433738,
127.108324446431)) ;
#134689 = CARTESIAN_POINT('Ctrl Pts',(-29.5411722729436,14.2124398345738,
127.283727368873)) ;
#134690 = CARTESIAN_POINT('Ctrl Pts',(-29.6075895922723,14.3830654461858,
127.510923381855)) ;
#134691 = CARTESIAN_POINT('Ctrl Pts',(-29.6859780654117,14.4846609541733,
127.773091506423)) ;
#134692 = CARTESIAN_POINT('Ctrl Pts',(-29.7699711987632,14.5097913616969,
128.051659371141)) ;
#134693 = CARTESIAN_POINT('Ctrl Pts',(-29.8521599614632,14.4576093080194,
128.324704513275)) ;
#134694 = CARTESIAN_POINT('Ctrl Pts',(-29.9273378651692,14.3304831317374,
128.57761366537)) ;
#134695 = CARTESIAN_POINT('Ctrl Pts',(-29.9881011678196,14.1386183822934,
128.788232639006)) ;
#134696 = CARTESIAN_POINT('Ctrl Pts',(-30.0298088081978,13.8965846856625,
128.943079017119)) ;
#134697 = CARTESIAN_POINT('Ctrl Pts',(-30.048987740085,13.6198365630073,129.032230754272)) ;
#134698 = CARTESIAN_POINT('Ctrl Pts',(-30.0433213484704,13.3288844737818,
129.048809941996)) ;
#134699 = CARTESIAN_POINT('Ctrl Pts',(-30.0124680035273,13.0447399832046,
128.991813037362)) ;
#134700 = CARTESIAN_POINT('Ctrl Pts',(-29.958162147996,12.7881836368688,128.866220633411)) ;
#134701 = CARTESIAN_POINT('Ctrl Pts',(-29.8827371039613,12.5755910115287,
128.67919720058)) ;
#134702 = CARTESIAN_POINT('Ctrl Pts',(-29.7923817501949,12.4257574465567,
128.448186718166)) ;
#134703 = CARTESIAN_POINT('Ctrl Pts',(-29.6914548654442,12.3460112405744,
128.186501449005)) ;
#134704 = CARTESIAN_POINT('Ctrl Pts',(-29.5867020660159,12.3439532504127,
127.913710488866)) ;
#134705 = CARTESIAN_POINT('Ctrl Pts',(-29.485666657119,12.4188218900739,127.651602416161)) ;
#134706 = CARTESIAN_POINT('Ctrl Pts',(-29.3936759004092,12.5668341062151,
127.416175460721)) ;
#134707 = CARTESIAN_POINT('Ctrl Pts',(-29.3182301931701,12.7739565310488,
127.2286723812)) ;
#134708 = CARTESIAN_POINT('Ctrl Pts',(-29.2623086088496,13.0292275295923,
127.098504241357)) ;
#134709 = CARTESIAN_POINT('Ctrl Pts',(-29.2301243830033,13.3121167714202,
127.037580467898)) ;
#134710 = CARTESIAN_POINT('Ctrl Pts',(-29.2229734795966,13.6036711588795,
127.049873651472)) ;
#134711 = CARTESIAN_POINT('Ctrl Pts',(-29.2408639834952,13.8822010088686,
127.135317168003)) ;
#134712 = CARTESIAN_POINT('Ctrl Pts',(-29.2814175857852,14.126534024312,127.286789452504)) ;
#134713 = CARTESIAN_POINT('Ctrl Pts',(-29.341269933413,14.3215277156221,127.494747226261)) ;
#134714 = CARTESIAN_POINT('Ctrl Pts',(-29.4156496701704,14.4523872469144,
127.745252022521)) ;
#134715 = CARTESIAN_POINT('Ctrl Pts',(-29.4979993749135,14.509081269933,128.018936330148)) ;
#134716 = CARTESIAN_POINT('Ctrl Pts',(-29.5821194390776,14.4877530584647,
128.297884507417)) ;
#134717 = CARTESIAN_POINT('Ctrl Pts',(-29.6605015766084,14.3906972492053,
128.559841528178)) ;
#134718 = CARTESIAN_POINT('Ctrl Pts',(-29.7277325620602,14.2242127265294,
128.789368837068)) ;
#134719 = CARTESIAN_POINT('Ctrl Pts',(-29.7778622908604,14.0000453961231,
128.968956847515)) ;
#134720 = CARTESIAN_POINT('Ctrl Pts',(-29.8065930602879,13.7349941187306,
129.085980593616)) ;
#134721 = CARTESIAN_POINT('Ctrl Pts',(-29.8110647581583,13.4462938086935,
129.132290262238)) ;
#134722 = CARTESIAN_POINT('Ctrl Pts',(-29.7905149481192,13.1586524064852,
129.105179558969)) ;
#134723 = CARTESIAN_POINT('Ctrl Pts',(-29.7450251194424,12.8863235925418,
129.005657518442)) ;
#134724 = CARTESIAN_POINT('Ctrl Pts',(-29.6779688870286,12.6553854575325,
128.842782884932)) ;
#134725 = CARTESIAN_POINT('Ctrl Pts',(-29.5932822353585,12.4787538591612,
128.628403260321)) ;
#134726 = CARTESIAN_POINT('Ctrl Pts',(-29.4951432611704,12.3688114822916,
128.375032108495)) ;
#134727 = CARTESIAN_POINT('Ctrl Pts',(-29.3915755638739,12.3354319136936,
128.105522888968)) ;
#134728 = CARTESIAN_POINT('Ctrl Pts',(-29.2883737439491,12.3792576310417,
127.83711019449)) ;
#134729 = CARTESIAN_POINT('Ctrl Pts',(-29.1917010872287,12.4988398999205,
127.587984309591)) ;
#134730 = CARTESIAN_POINT('Ctrl Pts',(-29.1090972687786,12.6835118512005,
127.379683329034)) ;
#134731 = CARTESIAN_POINT('Ctrl Pts',(-29.0446608613966,12.9214923912795,
127.224563683631)) ;
#134732 = CARTESIAN_POINT('Ctrl Pts',(-29.0026163941945,13.1954916424955,
127.134859426664)) ;
#134733 = CARTESIAN_POINT('Ctrl Pts',(-28.985230945197,13.4865485670219,127.117276574287)) ;
#134734 = CARTESIAN_POINT('Ctrl Pts',(-28.9931808891691,13.772471589557,127.173641275195)) ;
#134735 = CARTESIAN_POINT('Ctrl Pts',(-29.0248180797672,14.0322259092952,
127.299049560001)) ;
#134736 = CARTESIAN_POINT('Ctrl Pts',(-29.0774225647813,14.2496185339524,
127.485847881482)) ;
#134737 = CARTESIAN_POINT('Ctrl Pts',(-29.1466584272716,14.4079186586772,
127.721302692546)) ;
#134738 = CARTESIAN_POINT('Ctrl Pts',(-29.2262609733389,14.495128940057,127.986882942297)) ;
#134739 = CARTESIAN_POINT('Ctrl Pts',(-29.310377688868,14.5060206783235,128.265744239721)) ;
#134740 = CARTESIAN_POINT('Ctrl Pts',(-29.3922415681972,14.4388851972431,
128.538108177024)) ;
#134741 = CARTESIAN_POINT('Ctrl Pts',(-29.4648367940965,14.2990479598781,
128.783307296558)) ;
#134742 = CARTESIAN_POINT('Ctrl Pts',(-29.5224591681686,14.096277092635,128.984789687897)) ;
#134743 = CARTESIAN_POINT('Ctrl Pts',(-29.5601633246064,13.8463552274942,
129.12795060112)) ;
#134744 = CARTESIAN_POINT('Ctrl Pts',(-29.5747316968106,13.5643762793268,
129.203747316631)) ;
#134745 = CARTESIAN_POINT('Ctrl Pts',(-29.5643172687888,13.2747380866486,
129.206268472805)) ;
#134746 = CARTESIAN_POINT('Ctrl Pts',(-29.5288291438255,12.9934296976024,
129.135814296567)) ;
#134747 = CARTESIAN_POINT('Ctrl Pts',(-29.470171863856,12.7438068041656,128.99757323151)) ;
#134748 = CARTESIAN_POINT('Ctrl Pts',(-29.391803285665,12.5426943442427,128.801768222048)) ;
#134749 = CARTESIAN_POINT('Ctrl Pts',(-29.2986131391391,12.4046936236787,
128.56265775762)) ;
#134750 = CARTESIAN_POINT('Ctrl Pts',(-29.1964773761958,12.3396331759052,
128.297435830634)) ;
#134751 = CARTESIAN_POINT('Ctrl Pts',(-29.092230590555,12.3522550875064,128.025991131613)) ;
#134752 = CARTESIAN_POINT('Ctrl Pts',(-28.9924608185787,12.441158614988,127.767604009206)) ;
#134753 = CARTESIAN_POINT('Ctrl Pts',(-28.9030933450802,12.6013769713038,
127.539790029494)) ;
#134754 = CARTESIAN_POINT('Ctrl Pts',(-28.8308886096015,12.819071640269,127.361858709555)) ;
#134755 = CARTESIAN_POINT('Ctrl Pts',(-28.779280341327,13.0807346140254,127.244233442709)) ;
#134756 = CARTESIAN_POINT('Ctrl Pts',(-28.7517055757331,13.3675408612144,
127.196874862189)) ;
#134757 = CARTESIAN_POINT('Ctrl Pts',(-28.7493257047856,13.6570979280699,
127.222968219409)) ;
#134758 = CARTESIAN_POINT('Ctrl Pts',(-28.7718142821641,13.9319893911641,
127.321979864566)) ;
#134759 = CARTESIAN_POINT('Ctrl Pts',(-28.8162456944187,14.1676085258846,
127.484711805867)) ;
#134760 = CARTESIAN_POINT('Ctrl Pts',(-28.8794392120634,14.3519029604138,
127.702543293248)) ;
#134761 = CARTESIAN_POINT('Ctrl Pts',(-28.955521536148,14.4687263868581,127.957864396171)) ;
#134762 = CARTESIAN_POINT('Ctrl Pts',(-29.0386446837284,14.5110206744739,
128.233803590714)) ;
#134763 = CARTESIAN_POINT('Ctrl Pts',(-29.1220480184099,14.4754839101951,
128.510547823415)) ;
#134764 = CARTESIAN_POINT('Ctrl Pts',(-29.1992609632459,14.3641243881349,
128.769313204063)) ;
#134765 = CARTESIAN_POINT('Ctrl Pts',(-29.2634796257756,14.1859981150162,
128.989963010774)) ;
#134766 = CARTESIAN_POINT('Ctrl Pts',(-29.309906743687,13.9527739629267,129.158738849017)) ;
#134767 = CARTESIAN_POINT('Ctrl Pts',(-29.3342115703911,13.6818171869407,
129.262851136394)) ;
#134768 = CARTESIAN_POINT('Ctrl Pts',(-29.3340473631818,13.3923456599437,
129.295485666288)) ;
#134769 = CARTESIAN_POINT('Ctrl Pts',(-29.3085669103323,13.1044625348289,
129.254236375475)) ;
#134770 = CARTESIAN_POINT('Ctrl Pts',(-29.258986211392,12.8400820200563,129.142508243958)) ;
#134771 = CARTESIAN_POINT('Ctrl Pts',(-29.1881542029012,12.6174283224968,
128.968693652698)) ;
#134772 = CARTESIAN_POINT('Ctrl Pts',(-29.1002100971169,12.4521814963559,
128.744946986999)) ;
#134773 = CARTESIAN_POINT('Ctrl Pts',(-29.0009103649547,12.3567835155047,
128.48800496993)) ;
#134774 = CARTESIAN_POINT('Ctrl Pts',(-28.896925987083,12.3377092271658,128.21727920025)) ;
#134775 = CARTESIAN_POINT('Ctrl Pts',(-28.7942667965697,12.3962076032604,
127.950545837014)) ;
#134776 = CARTESIAN_POINT('Ctrl Pts',(-28.6998220504126,12.5290432373042,
127.70787965737)) ;
#134777 = CARTESIAN_POINT('Ctrl Pts',(-28.6204061898145,12.7244085230837,
127.508847094626)) ;
#134778 = CARTESIAN_POINT('Ctrl Pts',(-28.559819094265,12.9709500550387,127.365030411237)) ;
#134779 = CARTESIAN_POINT('Ctrl Pts',(-28.5223002592329,13.2494402817627,
127.288528530129)) ;
#134780 = CARTESIAN_POINT('Ctrl Pts',(-28.5097189788881,13.5418967084717,
127.285058220228)) ;
#134781 = CARTESIAN_POINT('Ctrl Pts',(-28.5222097719137,13.8230883914708,
127.354499660829)) ;
#134782 = CARTESIAN_POINT('Ctrl Pts',(-28.5582144837367,14.0775910910953,
127.492866930045)) ;
#134783 = CARTESIAN_POINT('Ctrl Pts',(-28.6142444612186,14.2842118886259,
127.689596183375)) ;
#134784 = CARTESIAN_POINT('Ctrl Pts',(-28.6857946550641,14.4299775435325,
127.931754504999)) ;
#134785 = CARTESIAN_POINT('Ctrl Pts',(-28.7673480084958,14.503331032243,128.203286809695)) ;
#134786 = CARTESIAN_POINT('Ctrl Pts',(-28.8509261449003,14.4992417837061,
128.480336479146)) ;
#134787 = CARTESIAN_POINT('Ctrl Pts',(-28.9318023648984,14.4177939822546,
128.749907191947)) ;
#134788 = CARTESIAN_POINT('Ctrl Pts',(-29.001910688641,14.2650806147523,128.987818507409)) ;
#134789 = CARTESIAN_POINT('Ctrl Pts',(-29.0559489688668,14.0529681509037,
129.178698338362)) ;
#134790 = CARTESIAN_POINT('Ctrl Pts',(-29.0896354038435,13.7955270319932,
129.310187588582)) ;
#134791 = CARTESIAN_POINT('Ctrl Pts',(-29.099611948193,13.5095709535078,129.372622374006)) ;
#134792 = CARTESIAN_POINT('Ctrl Pts',(-29.0842585907111,13.2189036520177,
129.360885383851)) ;
#134793 = CARTESIAN_POINT('Ctrl Pts',(-29.0443620584725,12.9437120966298,
129.277345257376)) ;
#134794 = CARTESIAN_POINT('Ctrl Pts',(-28.9817282559493,12.7018113312773,
129.127496651977)) ;
#134795 = CARTESIAN_POINT('Ctrl Pts',(-28.900103185758,12.5115374792667,128.922195104015)) ;
#134796 = CARTESIAN_POINT('Ctrl Pts',(-28.8047562754635,12.3865362509785,
128.676787399727)) ;
#134797 = CARTESIAN_POINT('Ctrl Pts',(-28.7012853562746,12.3360647683775,
128.40778833087)) ;
#134798 = CARTESIAN_POINT('Ctrl Pts',(-28.5980648305844,12.3630945002041,
128.139111767235)) ;
#134799 = CARTESIAN_POINT('Ctrl Pts',(-28.4992221941751,12.4665769548229,
127.883658010127)) ;
#134800 = CARTESIAN_POINT('Ctrl Pts',(-28.4131594840602,12.637873730405,127.665272376222)) ;
#134801 = CARTESIAN_POINT('Ctrl Pts',(-28.3441687124707,12.8661806742055,
127.496923307267)) ;
#134802 = CARTESIAN_POINT('Ctrl Pts',(-28.2971179753842,13.1333277515124,
127.392512752519)) ;
#134803 = CARTESIAN_POINT('Ctrl Pts',(-28.2742141661044,13.4221934836715,
127.358771264461)) ;
#134804 = CARTESIAN_POINT('Ctrl Pts',(-28.2765820238562,13.7107571318464,
127.398801174816)) ;
#134805 = CARTESIAN_POINT('Ctrl Pts',(-28.3034962448371,13.9798563780996,
127.510697252844)) ;
#134806 = CARTESIAN_POINT('Ctrl Pts',(-28.3518348917567,14.2070905580459,
127.684913382421)) ;
#134807 = CARTESIAN_POINT('Ctrl Pts',(-28.417736051092,14.3790287482914,127.910539859451)) ;
#134808 = CARTESIAN_POINT('Ctrl Pts',(-28.4956163030634,14.4826462514907,
128.171126340958)) ;
#134809 = CARTESIAN_POINT('Ctrl Pts',(-28.5798455524846,14.5101765749395,
128.450506444325)) ;
#134810 = CARTESIAN_POINT('Ctrl Pts',(-28.66200834704,14.4602521093363,128.723409993032)) ;
#134811 = CARTESIAN_POINT('Ctrl Pts',(-28.7375813833395,14.3349863303821,
128.977516850491)) ;
#134812 = CARTESIAN_POINT('Ctrl Pts',(-28.7985628235098,14.1459036519263,
129.188607444567)) ;
#134813 = CARTESIAN_POINT('Ctrl Pts',(-28.8411540818564,13.9042674567381,
129.346179660859)) ;
#134814 = CARTESIAN_POINT('Ctrl Pts',(-28.8610016097192,13.6274934121279,
129.437359596521)) ;
#134815 = CARTESIAN_POINT('Ctrl Pts',(-28.8560349310886,13.3375401227482,
129.455886266098)) ;
#134816 = CARTESIAN_POINT('Ctrl Pts',(-28.8260275084833,13.0529656397982,
129.401339308127)) ;
#134817 = CARTESIAN_POINT('Ctrl Pts',(-28.7718240751871,12.793542004979,129.276308893705)) ;
#134818 = CARTESIAN_POINT('Ctrl Pts',(-28.69758931411,12.5815361452067,129.09244647551)) ;
#134819 = CARTESIAN_POINT('Ctrl Pts',(-28.607191982818,12.4287258471182,128.861490887195)) ;
#134820 = CARTESIAN_POINT('Ctrl Pts',(-28.5062114306704,12.3470719994747,
128.599714513405)) ;
#134821 = CARTESIAN_POINT('Ctrl Pts',(-28.4016831964791,12.3430683223392,
128.327512526391)) ;
#134822 = CARTESIAN_POINT('Ctrl Pts',(-28.3008205475048,12.4155936091128,
128.065797526111)) ;
#134823 = CARTESIAN_POINT('Ctrl Pts',(-28.2086887982306,12.5608875783812,
127.829855784513)) ;
#134824 = CARTESIAN_POINT('Ctrl Pts',(-28.1322966051425,12.7672957855937,
127.639749496506)) ;
#134825 = CARTESIAN_POINT('Ctrl Pts',(-28.0757288054588,13.0219896288371,
127.507742576733)) ;
#134826 = CARTESIAN_POINT('Ctrl Pts',(-28.0429540969002,13.3035436342973,
127.44499916588)) ;
#134827 = CARTESIAN_POINT('Ctrl Pts',(-28.0350385580784,13.5948422510341,
127.455024273178)) ;
#134828 = CARTESIAN_POINT('Ctrl Pts',(-28.0521494910461,13.8739529691167,
127.538171398898)) ;
#134829 = CARTESIAN_POINT('Ctrl Pts',(-28.0921989061459,14.1203174233417,
127.688276422386)) ;
#134830 = CARTESIAN_POINT('Ctrl Pts',(-28.151557364416,14.3167168643634,127.894769419474)) ;
#134831 = CARTESIAN_POINT('Ctrl Pts',(-28.2253962663715,14.4494066861711,
128.14361033343)) ;
#134832 = CARTESIAN_POINT('Ctrl Pts',(-28.3077059790347,14.5084702688582,
128.41722565312)) ;
#134833 = CARTESIAN_POINT('Ctrl Pts',(-28.3916026412673,14.489700746972,128.695408809309)) ;
#134834 = CARTESIAN_POINT('Ctrl Pts',(-28.4706094716546,14.3946106074975,
128.959339303664)) ;
#134835 = CARTESIAN_POINT('Ctrl Pts',(-28.5383385063881,14.2294635345246,
129.190381875795)) ;
#134836 = CARTESIAN_POINT('Ctrl Pts',(-28.5888615094772,14.0073333887475,
129.371024757805)) ;
#134837 = CARTESIAN_POINT('Ctrl Pts',(-28.6182752167583,13.7435828448799,
129.490009369002)) ;
#134838 = CARTESIAN_POINT('Ctrl Pts',(-28.6235344183767,13.454824745877,129.538667492509)) ;
#134839 = CARTESIAN_POINT('Ctrl Pts',(-28.6035941708859,13.1663898496403,
129.513405963783)) ;
#134840 = CARTESIAN_POINT('Ctrl Pts',(-28.5591016772346,12.8948251888563,
129.416595319443)) ;
#134841 = CARTESIAN_POINT('Ctrl Pts',(-28.4924613979654,12.6613614393991,
129.255069109059)) ;
#134842 = CARTESIAN_POINT('Ctrl Pts',(-28.4079858158223,12.4827884864443,
129.041374692839)) ;
#134843 = CARTESIAN_POINT('Ctrl Pts',(-28.3106810095428,12.3713198999723,
128.790256537741)) ;
#134844 = CARTESIAN_POINT('Ctrl Pts',(-28.2071142233906,12.3351536539427,
128.520782151597)) ;
#134845 = CARTESIAN_POINT('Ctrl Pts',(-28.1033170651269,12.3771106003778,
128.250789621036)) ;
#134846 = CARTESIAN_POINT('Ctrl Pts',(-28.0070122936131,12.493746042562,128.002507073001)) ;
#134847 = CARTESIAN_POINT('Ctrl Pts',(-27.9236042223444,12.6767291405437,
127.791947198724)) ;
#134848 = CARTESIAN_POINT('Ctrl Pts',(-27.8582788554542,12.9147362953278,
127.634399931538)) ;
#134849 = CARTESIAN_POINT('Ctrl Pts',(-27.8157639814054,13.1870897175325,
127.543206911709)) ;
#134850 = CARTESIAN_POINT('Ctrl Pts',(-27.7976113632335,13.4771402294594,
127.523294837643)) ;
#134851 = CARTESIAN_POINT('Ctrl Pts',(-27.8047562191335,13.7642376991577,
127.577383148529)) ;
#134852 = CARTESIAN_POINT('Ctrl Pts',(-27.8359687279842,14.0261140050281,
127.701710177171)) ;
#134853 = CARTESIAN_POINT('Ctrl Pts',(-27.8877875139809,14.2437566095146,
127.886037495367)) ;
#134854 = CARTESIAN_POINT('Ctrl Pts',(-27.9566643830394,14.4043004510961,
128.12048462873)) ;
#134855 = CARTESIAN_POINT('Ctrl Pts',(-28.0360570915207,14.4936451763547,
128.385451901082)) ;
#134856 = CARTESIAN_POINT('Ctrl Pts',(-28.120129115805,14.5067755223083,128.664180642723)) ;
#134857 = CARTESIAN_POINT('Ctrl Pts',(-28.2020346856407,14.4421251633059,
128.936606880987)) ;
#134858 = CARTESIAN_POINT('Ctrl Pts',(-28.2751125216823,14.3039891726026,
129.183284767789)) ;
#134859 = CARTESIAN_POINT('Ctrl Pts',(-28.3330260630189,14.1040922169467,
129.385445944809)) ;
#134860 = CARTESIAN_POINT('Ctrl Pts',(-28.3716774412633,13.8535852347893,
129.531620171577)) ;
#134861 = CARTESIAN_POINT('Ctrl Pts',(-28.3868553207156,13.5730952435811,
129.609080622274)) ;
#134862 = CARTESIAN_POINT('Ctrl Pts',(-28.3771751540194,13.2829861782011,
129.613807074417)) ;
#134863 = CARTESIAN_POINT('Ctrl Pts',(-28.3425095932928,13.0017737284941,
129.545666888846)) ;
#134864 = CARTESIAN_POINT('Ctrl Pts',(-28.284301937165,12.7500890797144,129.408856898039)) ;
#134865 = CARTESIAN_POINT('Ctrl Pts',(-28.2064572920802,12.5475577998432,
129.214559307957)) ;
#134866 = CARTESIAN_POINT('Ctrl Pts',(-28.1135171544018,12.4075652478031,
128.976210428243)) ;
#134867 = CARTESIAN_POINT('Ctrl Pts',(-28.0118850220544,12.3405227377109,
128.712349934362)) ;
#134868 = CARTESIAN_POINT('Ctrl Pts',(-27.9073393263242,12.3506975715296,
128.440115510787)) ;
#134869 = CARTESIAN_POINT('Ctrl Pts',(-27.8069898708441,12.438177489278,128.180166701549)) ;
#134870 = CARTESIAN_POINT('Ctrl Pts',(-27.7177045614419,12.5958827964123,
127.952426644854)) ;
#134871 = CARTESIAN_POINT('Ctrl Pts',(-27.6448174995369,12.8123887822574,
127.772559198421)) ;
#134872 = CARTESIAN_POINT('Ctrl Pts',(-27.5925658802496,13.0732934241726,
127.653072879261)) ;
#134873 = CARTESIAN_POINT('Ctrl Pts',(-27.5643119574423,13.3601444544887,
127.603779546763)) ;
#134874 = CARTESIAN_POINT('Ctrl Pts',(-27.5613082454556,13.6487324697402,
127.627925538602)) ;
#134875 = CARTESIAN_POINT('Ctrl Pts',(-27.5828722691528,13.9231969052117,
127.724074394844)) ;
#134876 = CARTESIAN_POINT('Ctrl Pts',(-27.6269024064909,14.1616648845749,
127.885829090303)) ;
#134877 = CARTESIAN_POINT('Ctrl Pts',(-27.6896598747405,14.3474885130478,
128.102376258084)) ;
#134878 = CARTESIAN_POINT('Ctrl Pts',(-27.7653992680876,14.4664584587802,
128.356681964705)) ;
#134879 = CARTESIAN_POINT('Ctrl Pts',(-27.8487981620875,14.5109046603937,
128.633576137683)) ;
#134880 = CARTESIAN_POINT('Ctrl Pts',(-27.9318850392023,14.477538406395,128.909237750788)) ;
#134881 = CARTESIAN_POINT('Ctrl Pts',(-28.0095052256554,14.3681997132881,
129.169245881706)) ;
#134882 = CARTESIAN_POINT('Ctrl Pts',(-28.0741401659524,14.19161807787,129.391120281656)) ;
#134883 = CARTESIAN_POINT('Ctrl Pts',(-28.1210449004513,13.9603524956053,
129.561209556167)) ;
#134884 = CARTESIAN_POINT('Ctrl Pts',(-28.1460961632202,13.6895220911817,
129.667588782595)) ;
#134885 = CARTESIAN_POINT('Ctrl Pts',(-28.1465838645101,13.4007319641459,
129.702076763037)) ;
#134886 = CARTESIAN_POINT('Ctrl Pts',(-28.1219792750298,13.1132078283894,
129.663296512428)) ;
#134887 = CARTESIAN_POINT('Ctrl Pts',(-28.072797303837,12.8466068578935,129.552900494661)) ;
#134888 = CARTESIAN_POINT('Ctrl Pts',(-28.0028760663637,12.6236984730367,
129.381571768306)) ;
#134889 = CARTESIAN_POINT('Ctrl Pts',(-27.9152289217031,12.4561011970055,
129.15875880179)) ;
#134890 = CARTESIAN_POINT('Ctrl Pts',(-27.8163074914158,12.3585968124196,
128.902876316079)) ;
#134891 = CARTESIAN_POINT('Ctrl Pts',(-27.7120492591559,12.3371246735504,
128.631455165304)) ;
#134892 = CARTESIAN_POINT('Ctrl Pts',(-27.6093731664381,12.3935413485491,
128.364635405542)) ;
#134893 = CARTESIAN_POINT('Ctrl Pts',(-27.5149001295544,12.5236723848828,
128.121769416389)) ;
#134894 = CARTESIAN_POINT('Ctrl Pts',(-27.4346201824783,12.7179304240541,
127.920341279588)) ;
#134895 = CARTESIAN_POINT('Ctrl Pts',(-27.3732833708595,12.9643000603806,
127.774449881944)) ;
#134896 = CARTESIAN_POINT('Ctrl Pts',(-27.3353218805088,13.2410161239663,
127.696515666237)) ;
#134897 = CARTESIAN_POINT('Ctrl Pts',(-27.3219345106549,13.5320326358814,
127.690536193544)) ;
#134898 = CARTESIAN_POINT('Ctrl Pts',(-27.3336868555628,13.8151976332958,
127.757981771659)) ;
#134899 = CARTESIAN_POINT('Ctrl Pts',(-27.3691045396702,14.070965110173,127.894657472177)) ;
#134900 = CARTESIAN_POINT('Ctrl Pts',(-27.4247538548607,14.2795161854134,
128.090342542637)) ;
#134901 = CARTESIAN_POINT('Ctrl Pts',(-27.495823154164,14.4266233568165,128.331023842141)) ;
#134902 = CARTESIAN_POINT('Ctrl Pts',(-27.5766922115291,14.5021444966585,
128.600366276399)) ;
#134903 = CARTESIAN_POINT('Ctrl Pts',(-27.6609223179021,14.5004799279669,
128.8795751742)) ;
#134904 = CARTESIAN_POINT('Ctrl Pts',(-27.7417671934519,14.4210758361391,
129.14896837329)) ;
#134905 = CARTESIAN_POINT('Ctrl Pts',(-27.8120265768946,14.2711637356508,
129.38719326095)) ;
#134906 = CARTESIAN_POINT('Ctrl Pts',(-27.866891762874,14.0600320259714,129.580611011308)) ;
#134907 = CARTESIAN_POINT('Ctrl Pts',(-27.9012411174026,13.8025046463563,
129.714162963611)) ;
#134908 = CARTESIAN_POINT('Ctrl Pts',(-27.9118652501947,13.5194350300881,
129.778210865001)) ;
#134909 = CARTESIAN_POINT('Ctrl Pts',(-27.8973675127668,13.227929848522,129.769057927685)) ;
#134910 = CARTESIAN_POINT('Ctrl Pts',(-27.8581217638387,12.9514279979351,
129.687479679852)) ;
#134911 = CARTESIAN_POINT('Ctrl Pts',(-27.7958487933346,12.7076270254922,
129.538792895781)) ;
#134912 = CARTESIAN_POINT('Ctrl Pts',(-27.7150442368328,12.5164543914562,
129.335744778992)) ;
#134913 = CARTESIAN_POINT('Ctrl Pts',(-27.6197799723084,12.3891143889345,
129.090666143106)) ;
#134914 = CARTESIAN_POINT('Ctrl Pts',(-27.5169840616899,12.3364756158918,
128.823462340777)) ;
#134915 = CARTESIAN_POINT('Ctrl Pts',(-27.4129425204162,12.3612642231578,
128.552629149903)) ;
#134916 = CARTESIAN_POINT('Ctrl Pts',(-27.3139116309648,12.4629838840005,
128.296612691349)) ;
#134917 = CARTESIAN_POINT('Ctrl Pts',(-27.2276350555539,12.6321971699934,
128.077535896234)) ;
#134918 = CARTESIAN_POINT('Ctrl Pts',(-27.1581753164316,12.8584558798932,
127.907740199772)) ;
#134919 = CARTESIAN_POINT('Ctrl Pts',(-27.1102193532803,13.1261648647243,
127.800864060768)) ;
#134920 = CARTESIAN_POINT('Ctrl Pts',(-27.0867427780488,13.4141234552309,
127.765371910168)) ;
#134921 = CARTESIAN_POINT('Ctrl Pts',(-27.088405263082,13.7023852342343,127.803282253112)) ;
#134922 = CARTESIAN_POINT('Ctrl Pts',(-27.1144094066955,13.9714212012371,
127.912378068659)) ;
#134923 = CARTESIAN_POINT('Ctrl Pts',(-27.1625636190418,14.202020081249,128.086338189894)) ;
#134924 = CARTESIAN_POINT('Ctrl Pts',(-27.2279041571622,14.3750071736422,
128.310222999053)) ;
#134925 = CARTESIAN_POINT('Ctrl Pts',(-27.3055089641359,14.4806351346196,
128.570006270221)) ;
#134926 = CARTESIAN_POINT('Ctrl Pts',(-27.3892702869014,14.5105855297535,
128.847858683373)) ;
#134927 = CARTESIAN_POINT('Ctrl Pts',(-27.4721256647169,14.4625550657111,
129.123019817885)) ;
#134928 = CARTESIAN_POINT('Ctrl Pts',(-27.5475424958297,14.3400369417443,
129.376461860258)) ;
#134929 = CARTESIAN_POINT('Ctrl Pts',(-27.6092868870231,14.1521957535254,
129.589908595948)) ;
#134930 = CARTESIAN_POINT('Ctrl Pts',(-27.6524549950664,13.9116489154345,
129.749173070005)) ;
#134931 = CARTESIAN_POINT('Ctrl Pts',(-27.6729767158619,13.6358544266559,
129.842295420114)) ;
#134932 = CARTESIAN_POINT('Ctrl Pts',(-27.6687686357343,13.3459427675745,
129.863045715734)) ;
#134933 = CARTESIAN_POINT('Ctrl Pts',(-27.6393546558192,13.0604649745041,
129.810291983176)) ;
#134934 = CARTESIAN_POINT('Ctrl Pts',(-27.5861749748563,12.8015143832803,
129.688047174148)) ;
#134935 = CARTESIAN_POINT('Ctrl Pts',(-27.5122453552566,12.586871423154,129.505215644939)) ;
#134936 = CARTESIAN_POINT('Ctrl Pts',(-27.4222257102063,12.4323032180318,
129.275353955494)) ;
#134937 = CARTESIAN_POINT('Ctrl Pts',(-27.321814640165,12.348604012381,129.015131363742)) ;
#134938 = CARTESIAN_POINT('Ctrl Pts',(-27.2172646277251,12.3418345254331,
128.742874357153)) ;
#134939 = CARTESIAN_POINT('Ctrl Pts',(-27.1155991989799,12.4127257697425,
128.479021774659)) ;
#134940 = CARTESIAN_POINT('Ctrl Pts',(-27.0235546029965,12.5554430365515,
128.24317434018)) ;
#134941 = CARTESIAN_POINT('Ctrl Pts',(-26.946364611968,12.7608029240068,128.050846584327)) ;
#134942 = CARTESIAN_POINT('Ctrl Pts',(-26.8892425932522,13.0143079229722,
127.917197312737)) ;
#134943 = CARTESIAN_POINT('Ctrl Pts',(-26.8557397574038,13.2953661026702,
127.852335782128)) ;
#134944 = CARTESIAN_POINT('Ctrl Pts',(-26.8471237684322,13.587499191953,127.86040257377)) ;
#134945 = CARTESIAN_POINT('Ctrl Pts',(-26.8636409106043,13.8669338626205,
127.941791701437)) ;
#134946 = CARTESIAN_POINT('Ctrl Pts',(-26.9028894020443,14.1134263503453,
128.089413302891)) ;
#134947 = CARTESIAN_POINT('Ctrl Pts',(-26.9618864660315,14.3121780897716,
128.294946112899)) ;
#134948 = CARTESIAN_POINT('Ctrl Pts',(-27.0356609756341,14.4470050265316,
128.543696981495)) ;
#134949 = CARTESIAN_POINT('Ctrl Pts',(-27.1176846698481,14.5078086325279,
128.816414339099)) ;
#134950 = CARTESIAN_POINT('Ctrl Pts',(-27.2013501944063,14.4913412737729,
129.093814747738)) ;
#134951 = CARTESIAN_POINT('Ctrl Pts',(-27.2805727554514,14.3985299043882,
129.358365317732)) ;
#134952 = CARTESIAN_POINT('Ctrl Pts',(-27.3487809879748,14.2353764928408,
129.590815975098)) ;
#134953 = CARTESIAN_POINT('Ctrl Pts',(-27.4000923756535,14.0132824388172,
129.773951949604)) ;
#134954 = CARTESIAN_POINT('Ctrl Pts',(-27.4299031588905,13.751770584179,129.893917739675)) ;
#134955 = CARTESIAN_POINT('Ctrl Pts',(-27.4360065328396,13.4639004603942,
129.944990740374)) ;
#134956 = CARTESIAN_POINT('Ctrl Pts',(-27.4166194504997,13.1736259559936,
129.921533138526)) ;
#134957 = CARTESIAN_POINT('Ctrl Pts',(-27.3730557967721,12.9029494351804,
129.827230137503)) ;
#134958 = CARTESIAN_POINT('Ctrl Pts',(-27.3068239081708,12.6670694829694,
129.667025348139)) ;
#134959 = CARTESIAN_POINT('Ctrl Pts',(-27.2225807375648,12.4867414535482,
129.454064281963)) ;
#134960 = CARTESIAN_POINT('Ctrl Pts',(-27.1260163205075,12.3736046950475,
129.204955161642)) ;
#134961 = CARTESIAN_POINT('Ctrl Pts',(-27.0219531940928,12.3351061359291,
128.934221171249)) ;
#134962 = CARTESIAN_POINT('Ctrl Pts',(-26.9187654991147,12.3747297412366,
128.665782677207)) ;
#134963 = CARTESIAN_POINT('Ctrl Pts',(-26.8219192185406,12.4890530273647,
128.415981781108)) ;
#134964 = CARTESIAN_POINT('Ctrl Pts',(-26.7375618368722,12.6718473822343,
128.20287552548)) ;
#134965 = CARTESIAN_POINT('Ctrl Pts',(-26.6721408995713,12.9071471042355,
128.044830293244)) ;
#134966 = CARTESIAN_POINT('Ctrl Pts',(-26.6288268693924,13.1791583633753,
127.951366546025)) ;
#134967 = CARTESIAN_POINT('Ctrl Pts',(-26.6100146219695,13.4685703303894,
127.929472625113)) ;
#134968 = CARTESIAN_POINT('Ctrl Pts',(-26.6163965606096,13.7556865610863,
127.981289936006)) ;
#134969 = CARTESIAN_POINT('Ctrl Pts',(-26.6468365176563,14.0184520779736,
128.103328446011)) ;
#134970 = CARTESIAN_POINT('Ctrl Pts',(-26.6983664732469,14.2386835545227,
128.286981099105)) ;
#134971 = CARTESIAN_POINT('Ctrl Pts',(-26.7668561678463,14.4009245247973,
128.520283146029)) ;
#134972 = CARTESIAN_POINT('Ctrl Pts',(-26.8462801396179,14.4923209079493,
128.785440445302)) ;
#134973 = CARTESIAN_POINT('Ctrl Pts',(-26.9299042318789,14.5074993821674,
129.062691208225)) ;
#134974 = CARTESIAN_POINT('Ctrl Pts',(-27.0123042045344,14.4446391320812,
129.336708219525)) ;
#134975 = CARTESIAN_POINT('Ctrl Pts',(-27.0853285109314,14.309013886893,129.583057807955)) ;
#134976 = CARTESIAN_POINT('Ctrl Pts',(-27.1438828659143,14.1104149351794,
129.787163074108)) ;
#134977 = CARTESIAN_POINT('Ctrl Pts',(-27.1830524640317,13.8614588559076,
129.934789891105)) ;
#134978 = CARTESIAN_POINT('Ctrl Pts',(-27.1989887778394,13.5819687002437,
130.014428956727)) ;
#134979 = CARTESIAN_POINT('Ctrl Pts',(-27.1899960665713,13.2906279013141,
130.021303572167)) ;
#134980 = CARTESIAN_POINT('Ctrl Pts',(-27.1559614540415,13.009243305788,129.95497149067)) ;
#134981 = CARTESIAN_POINT('Ctrl Pts',(-27.0987240639522,12.7575168112921,
129.820836098485)) ;
#134982 = CARTESIAN_POINT('Ctrl Pts',(-27.0211347642334,12.5525240138587,
129.627409702748)) ;
#134983 = CARTESIAN_POINT('Ctrl Pts',(-26.9288019853003,12.4108770336832,
129.390743830787)) ;
#134984 = CARTESIAN_POINT('Ctrl Pts',(-26.8269925769389,12.3412909140522,
129.126483822534)) ;
#134985 = CARTESIAN_POINT('Ctrl Pts',(-26.7225678003105,12.3493861735078,
128.854556329981)) ;
#134986 = CARTESIAN_POINT('Ctrl Pts',(-26.6222736426069,12.4342727909203,
128.594675298208)) ;
#134987 = CARTESIAN_POINT('Ctrl Pts',(-26.5324245140866,12.5900489009072,
128.365332500197)) ;
#134988 = CARTESIAN_POINT('Ctrl Pts',(-26.4587946173494,12.8056265995217,
128.183382042886)) ;
#134989 = CARTESIAN_POINT('Ctrl Pts',(-26.4059966216722,13.0653848746049,
128.062274396553)) ;
#134990 = CARTESIAN_POINT('Ctrl Pts',(-26.3770384247468,13.3504851063388,
128.01077693268)) ;
#134991 = CARTESIAN_POINT('Ctrl Pts',(-26.3732580768289,13.6412798147236,
128.032889399786)) ;
#134992 = CARTESIAN_POINT('Ctrl Pts',(-26.3941468859038,13.915548156852,128.126957619226)) ;
#134993 = CARTESIAN_POINT('Ctrl Pts',(-26.4375236270793,14.1552942040558,
128.286796725341)) ;
#134994 = CARTESIAN_POINT('Ctrl Pts',(-26.499786802166,14.3429101935435,128.501891901076)) ;
#134995 = CARTESIAN_POINT('Ctrl Pts',(-26.5753221744753,14.4639893047867,
128.755644371512)) ;
#134996 = CARTESIAN_POINT('Ctrl Pts',(-26.658258796401,14.5107279953385,129.031049167775)) ;
#134997 = CARTESIAN_POINT('Ctrl Pts',(-26.7418770326506,14.4794893752074,
129.308446128137)) ;
#134998 = CARTESIAN_POINT('Ctrl Pts',(-26.819410154467,14.3727211578977,129.56804219168)) ;
#134999 = CARTESIAN_POINT('Ctrl Pts',(-26.884660652684,14.1977799584113,129.791786901947)) ;
#135000 = CARTESIAN_POINT('Ctrl Pts',(-26.9321606344241,13.9680803032242,
129.963592933574)) ;
#135001 = CARTESIAN_POINT('Ctrl Pts',(-26.9579703404882,13.6967826933105,
130.072347583536)) ;
#135002 = CARTESIAN_POINT('Ctrl Pts',(-26.9591310030642,13.4094043760888,
130.108663362794)) ;
#135003 = CARTESIAN_POINT('Ctrl Pts',(-26.935231210856,13.1212039321583,130.071985580596)) ;
#135004 = CARTESIAN_POINT('Ctrl Pts',(-26.8869426549206,12.8546896237207,
129.964066829109)) ;
#135005 = CARTESIAN_POINT('Ctrl Pts',(-26.8174482093006,12.6293810356165,
129.794091823838)) ;
#135006 = CARTESIAN_POINT('Ctrl Pts',(-26.7297563031988,12.4594635396626,
129.571300039305)) ;
#135007 = CARTESIAN_POINT('Ctrl Pts',(-26.6315768169788,12.3604529302704,
129.317412505758)) ;
#135008 = CARTESIAN_POINT('Ctrl Pts',(-26.527041677516,12.3366695079855,129.045292118923)) ;
#135009 = CARTESIAN_POINT('Ctrl Pts',(-26.4246632418904,12.3907630606801,
128.779202667163)) ;
#135010 = CARTESIAN_POINT('Ctrl Pts',(-26.3296624090555,12.5187717527639,
128.534846855937)) ;
#135011 = CARTESIAN_POINT('Ctrl Pts',(-26.2486292653153,12.7125553045139,
128.331370691531)) ;
#135012 = CARTESIAN_POINT('Ctrl Pts',(-26.187290463919,12.9551208485313,128.185129058602)) ;
#135013 = CARTESIAN_POINT('Ctrl Pts',(-26.1482420973643,13.2325620060974,
128.104210130242)) ;
#135014 = CARTESIAN_POINT('Ctrl Pts',(-26.1341913899476,13.5243419796884,
128.096383572714)) ;
#135015 = CARTESIAN_POINT('Ctrl Pts',(-26.1452118388481,13.8069926528057,
128.161574113629)) ;
#135016 = CARTESIAN_POINT('Ctrl Pts',(-26.1799390075941,14.0639000199269,
128.296232665471)) ;
#135017 = CARTESIAN_POINT('Ctrl Pts',(-26.2350489546991,14.2741558930926,
128.490347023028)) ;
#135018 = CARTESIAN_POINT('Ctrl Pts',(-26.3059077450582,14.4234615625839,
128.730487186166)) ;
#135019 = CARTESIAN_POINT('Ctrl Pts',(-26.386494169588,14.5011170686614,128.998961276038)) ;
#135020 = CARTESIAN_POINT('Ctrl Pts',(-26.4710372754606,14.5013614779113,
129.279215621043)) ;
#135021 = CARTESIAN_POINT('Ctrl Pts',(-26.5513450363698,14.4249956630962,
129.546727763435)) ;
#135022 = CARTESIAN_POINT('Ctrl Pts',(-26.6226216620681,14.2760171565871,
129.788206158856)) ;
#135023 = CARTESIAN_POINT('Ctrl Pts',(-26.6777858163634,14.0665442400002,
129.982426179449)) ;
#135024 = CARTESIAN_POINT('Ctrl Pts',(-26.7127743428566,13.8110528410318,
130.117741076645)) ;
#135025 = CARTESIAN_POINT('Ctrl Pts',(-26.7241069347589,13.5262786463887,
130.184114351317)) ;
#135026 = CARTESIAN_POINT('Ctrl Pts',(-26.7103978253846,13.2368369901033,
130.177011615775)) ;
#135027 = CARTESIAN_POINT('Ctrl Pts',(-26.6716560461567,12.9583255903659,
130.097075764209)) ;
#135028 = CARTESIAN_POINT('Ctrl Pts',(-26.6103674672222,12.7145800096232,
129.95106877123)) ;
#135029 = CARTESIAN_POINT('Ctrl Pts',(-26.5292783226885,12.5201730384604,
129.747494551372)) ;
#135030 = CARTESIAN_POINT('Ctrl Pts',(-26.4353195353877,12.392297716127,129.505869698294)) ;
#135031 = CARTESIAN_POINT('Ctrl Pts',(-26.3321003131888,12.3368042043637,
129.23762472755)) ;
#135032 = CARTESIAN_POINT('Ctrl Pts',(-26.2283359448761,12.3594079574846,
128.967488898529)) ;
#135033 = CARTESIAN_POINT('Ctrl Pts',(-26.1289374320057,12.4588426243277,
128.710432008687)) ;
#135034 = CARTESIAN_POINT('Ctrl Pts',(-26.0421433826271,12.6263832935465,
128.489874381818)) ;
#135035 = CARTESIAN_POINT('Ctrl Pts',(-25.9721170036289,12.8513078071139,
128.318433909601)) ;
#135036 = CARTESIAN_POINT('Ctrl Pts',(-25.9235411833855,13.1175341941134,
128.209680256936)) ;
#135037 = CARTESIAN_POINT('Ctrl Pts',(-25.8992723616796,13.4059954970849,
128.171974342421)) ;
#135038 = CARTESIAN_POINT('Ctrl Pts',(-25.9001789667653,13.6942419645787,
128.207632461566)) ;
#135039 = CARTESIAN_POINT('Ctrl Pts',(-25.9258216003677,13.9656571359195,
128.31589284879)) ;
#135040 = CARTESIAN_POINT('Ctrl Pts',(-25.9727492712161,14.1945698215837,
128.485818180082)) ;
#135041 = CARTESIAN_POINT('Ctrl Pts',(-26.0380351219601,14.3711224528334,
128.709801837872)) ;
#135042 = CARTESIAN_POINT('Ctrl Pts',(-26.115372034482,14.4785950091488,128.968780330961)) ;
#135043 = CARTESIAN_POINT('Ctrl Pts',(-26.1991386228248,14.5108133112394,
129.246686766249)) ;
#135044 = CARTESIAN_POINT('Ctrl Pts',(-26.281961118953,14.4650394200622,129.521689731091)) ;
#135045 = CARTESIAN_POINT('Ctrl Pts',(-26.3576691539897,14.3446919400874,
129.775975443665)) ;
#135046 = CARTESIAN_POINT('Ctrl Pts',(-26.4199450377268,14.1586507898245,
129.990981699106)) ;
#135047 = CARTESIAN_POINT('Ctrl Pts',(-26.4638325348643,13.9182142591253,
130.152493567261)) ;
#135048 = CARTESIAN_POINT('Ctrl Pts',(-26.4849121372087,13.6446894301756,
130.247054976681)) ;
#135049 = CARTESIAN_POINT('Ctrl Pts',(-26.4814409395297,13.3538163555555,
130.270090586414)) ;
#135050 = CARTESIAN_POINT('Ctrl Pts',(-26.4527946492839,13.0687529323482,
130.219476965581)) ;
#135051 = CARTESIAN_POINT('Ctrl Pts',(-26.4002320096581,12.8084025711039,
130.099079794229)) ;
#135052 = CARTESIAN_POINT('Ctrl Pts',(-26.3268756685072,12.5923662507696,
129.91790410308)) ;
#135053 = CARTESIAN_POINT('Ctrl Pts',(-26.2371123368209,12.4355966936421,
129.688843066008)) ;
#135054 = CARTESIAN_POINT('Ctrl Pts',(-26.1367181878628,12.3498834173245,
129.42872587461)) ;
#135055 = CARTESIAN_POINT('Ctrl Pts',(-26.032722719753,12.3409542808635,129.157919642926)) ;
#135056 = CARTESIAN_POINT('Ctrl Pts',(-25.9308084387583,12.4093757248112,
128.893357587352)) ;
#135057 = CARTESIAN_POINT('Ctrl Pts',(-25.838155620905,12.5505196315372,128.655821078007)) ;
#135058 = CARTESIAN_POINT('Ctrl Pts',(-25.7605740007468,12.7541803006072,
128.462316845571)) ;
#135059 = CARTESIAN_POINT('Ctrl Pts',(-25.7029450253967,13.0055267425044,
128.327067990315)) ;
#135060 = CARTESIAN_POINT('Ctrl Pts',(-25.6685657347824,13.2870724884799,
128.259776019344)) ;
#135061 = CARTESIAN_POINT('Ctrl Pts',(-25.6592502061655,13.5781354317469,
128.265673438089)) ;
#135062 = CARTESIAN_POINT('Ctrl Pts',(-25.6749179654199,13.8583662507443,
128.344586199981)) ;
#135063 = CARTESIAN_POINT('Ctrl Pts',(-25.7137374162889,14.1072755060793,
128.491117013587)) ;
#135064 = CARTESIAN_POINT('Ctrl Pts',(-25.7721169966564,14.3069765889331,
128.694755702354)) ;
#135065 = CARTESIAN_POINT('Ctrl Pts',(-25.845207577047,14.443614067786,128.941381531894)) ;
#135066 = CARTESIAN_POINT('Ctrl Pts',(-25.9273346325596,14.5071928082345,
129.214515131727)) ;
#135067 = CARTESIAN_POINT('Ctrl Pts',(-26.011234962119,14.4928945220509,129.492675842775)) ;
#135068 = CARTESIAN_POINT('Ctrl Pts',(-26.0906570279007,14.4021254936154,
129.757803067043)) ;
#135069 = CARTESIAN_POINT('Ctrl Pts',(-26.159082383682,14.2413770477371,129.990792154917)) ;
#135070 = CARTESIAN_POINT('Ctrl Pts',(-26.2110152100895,14.0210258594474,
130.175736142196)) ;
#135071 = CARTESIAN_POINT('Ctrl Pts',(-26.241635177827,13.7594508415378,130.298196601018)) ;
#135072 = CARTESIAN_POINT('Ctrl Pts',(-26.2483473113095,13.4716753030503,
130.351078692086)) ;
#135073 = CARTESIAN_POINT('Ctrl Pts',(-26.2298541426232,13.18278007244,130.330045835803)) ;
#135074 = CARTESIAN_POINT('Ctrl Pts',(-26.1867418068547,12.9097866347109,
130.237249070666)) ;
#135075 = CARTESIAN_POINT('Ctrl Pts',(-26.1214552754847,12.6739761120234,
130.079613973061)) ;
#135076 = CARTESIAN_POINT('Ctrl Pts',(-26.037598712626,12.4911376353209,129.867849268882)) ;
#135077 = CARTESIAN_POINT('Ctrl Pts',(-25.9407649580424,12.3755758788311,
129.618129131331)) ;
#135078 = CARTESIAN_POINT('Ctrl Pts',(-25.8374214950217,12.3352662329562,
129.34929906656)) ;
#135079 = CARTESIAN_POINT('Ctrl Pts',(-25.7340098362028,12.3722006143293,
129.0802369826)) ;
#135080 = CARTESIAN_POINT('Ctrl Pts',(-25.6361773432197,12.4858118722087,
128.827819165484)) ;
#135081 = CARTESIAN_POINT('Ctrl Pts',(-25.5523274084712,12.6649628027199,
128.615825895545)) ;
#135082 = CARTESIAN_POINT('Ctrl Pts',(-25.4859513870995,12.8995424291904,
128.455121245363)) ;
#135083 = CARTESIAN_POINT('Ctrl Pts',(-25.4419863750333,13.1707489990253,
128.359746169264)) ;
#135084 = CARTESIAN_POINT('Ctrl Pts',(-25.4224009992562,13.4602465419289,
128.335630931104)) ;
#135085 = CARTESIAN_POINT('Ctrl Pts',(-25.4281061795563,13.7479094104328,
128.385491263721)) ;
#135086 = CARTESIAN_POINT('Ctrl Pts',(-25.4578216450762,14.0110933638022,
128.505345635233)) ;
#135087 = CARTESIAN_POINT('Ctrl Pts',(-25.5087967768197,14.2330195298938,
128.687396943834)) ;
#135088 = CARTESIAN_POINT('Ctrl Pts',(-25.5768933622651,14.397056415232,128.919554215411)) ;
#135089 = CARTESIAN_POINT('Ctrl Pts',(-25.6558147544988,14.4906410938832,
129.183138561615)) ;
#135090 = CARTESIAN_POINT('Ctrl Pts',(-25.7399301950195,14.5080280130628,
129.462041474598)) ;
#135091 = CARTESIAN_POINT('Ctrl Pts',(-25.8217364878674,14.4480725424633,
129.734011003358)) ;
#135092 = CARTESIAN_POINT('Ctrl Pts',(-25.8956483813608,14.3139470607326,
129.983179734343)) ;
#135093 = CARTESIAN_POINT('Ctrl Pts',(-25.9546615112484,14.1169437524237,
130.188609280051)) ;
#135094 = CARTESIAN_POINT('Ctrl Pts',(-25.994519421204,13.8684682048696,130.338337741358)) ;
#135095 = CARTESIAN_POINT('Ctrl Pts',(-26.0110568377318,13.5907243651,130.419594305655)) ;
#135096 = CARTESIAN_POINT('Ctrl Pts',(-26.0028570943019,13.2994062522709,
130.428791647391)) ;
#135097 = CARTESIAN_POINT('Ctrl Pts',(-25.9695704025357,13.0173302811176,
130.364651136717)) ;
#135098 = CARTESIAN_POINT('Ctrl Pts',(-25.9127012517306,12.7634586998748,
130.23173138777)) ;
#135099 = CARTESIAN_POINT('Ctrl Pts',(-25.8356694959319,12.5574053612187,
130.039883250671)) ;
#135100 = CARTESIAN_POINT('Ctrl Pts',(-25.7439581375389,12.4141338116398,
129.804942699892)) ;
#135101 = CARTESIAN_POINT('Ctrl Pts',(-25.6422361078924,12.342233208706,129.540970477651)) ;
#135102 = CARTESIAN_POINT('Ctrl Pts',(-25.5379082160016,12.3479816385131,
129.269286803224)) ;
#135103 = CARTESIAN_POINT('Ctrl Pts',(-25.4372492426153,12.4308508598937,
129.00839512309)) ;
#135104 = CARTESIAN_POINT('Ctrl Pts',(-25.3472402005208,12.5841342714032,
128.778486490676)) ;
#135105 = CARTESIAN_POINT('Ctrl Pts',(-25.272730898508,12.7991564308112,128.594122402279)) ;
#135106 = CARTESIAN_POINT('Ctrl Pts',(-25.2194888387276,13.0569999610756,
128.471595214616)) ;
#135107 = CARTESIAN_POINT('Ctrl Pts',(-25.1897401476562,13.3421921034464,
128.417860044275)) ;
#135108 = CARTESIAN_POINT('Ctrl Pts',(-25.1851966857885,13.6321454574867,
128.437625751363)) ;
#135109 = CARTESIAN_POINT('Ctrl Pts',(-25.2054882351433,13.9089725412032,
128.530163374861)) ;
#135110 = CARTESIAN_POINT('Ctrl Pts',(-25.2484501051326,14.1498188340954,
128.688812325716)) ;
#135111 = CARTESIAN_POINT('Ctrl Pts',(-25.3098239459612,14.3379335225619,
128.901090604678)) ;
#135112 = CARTESIAN_POINT('Ctrl Pts',(-25.3852409841119,14.4615825769609,
129.154594863581)) ;
#135113 = CARTESIAN_POINT('Ctrl Pts',(-25.4680078103566,14.5104718339952,
129.429479188798)) ;
#135114 = CARTESIAN_POINT('Ctrl Pts',(-25.5519233175472,14.4813917081873,
129.707831723369)) ;
#135115 = CARTESIAN_POINT('Ctrl Pts',(-25.6296594879759,14.3764101476522,
129.968016081421)) ;
#135116 = CARTESIAN_POINT('Ctrl Pts',(-25.6951131634194,14.2041613001764,
130.192211432841)) ;
#135117 = CARTESIAN_POINT('Ctrl Pts',(-25.7434116042681,13.9743839791119,
130.36655070585)) ;
#135118 = CARTESIAN_POINT('Ctrl Pts',(-25.7697062526325,13.7063210401926,
130.476427371815)) ;
#135119 = CARTESIAN_POINT('Ctrl Pts',(-25.7716643333024,13.416701167449,130.515370896243)) ;
#135120 = CARTESIAN_POINT('Ctrl Pts',(-25.7484303453548,13.1291677758352,
130.480525076402)) ;
#135121 = CARTESIAN_POINT('Ctrl Pts',(-25.7008468729498,12.86171027905,130.374668312212)) ;
#135122 = CARTESIAN_POINT('Ctrl Pts',(-25.6318421414092,12.6350478480017,
130.206135995294)) ;
#135123 = CARTESIAN_POINT('Ctrl Pts',(-25.5450073178082,12.4638699665219,
129.985698129429)) ;
#135124 = CARTESIAN_POINT('Ctrl Pts',(-25.4465855133018,12.3621126869917,
129.731275230113)) ;
#135125 = CARTESIAN_POINT('Ctrl Pts',(-25.3422723144961,12.336288293437,129.459748523319)) ;
#135126 = CARTESIAN_POINT('Ctrl Pts',(-25.2395464146887,12.3882079133966,
129.192710014154)) ;
#135127 = CARTESIAN_POINT('Ctrl Pts',(-25.1441554739243,12.5148240028862,
128.947268201873)) ;
#135128 = CARTESIAN_POINT('Ctrl Pts',(-25.0632912716036,12.7050812653244,
128.743995286524)) ;
#135129 = CARTESIAN_POINT('Ctrl Pts',(-25.0008040035337,12.9482677220772,
128.594669933562)) ;
#135130 = CARTESIAN_POINT('Ctrl Pts',(-24.9612989083473,13.2238578222556,
128.512263188183)) ;
#135131 = CARTESIAN_POINT('Ctrl Pts',(-24.9464400414306,13.5162932448957,
128.502169911524)) ;
#135132 = CARTESIAN_POINT('Ctrl Pts',(-24.9567559801261,13.799165239793,128.565264390033)) ;
#135133 = CARTESIAN_POINT('Ctrl Pts',(-24.9910303138475,14.0580267764743,
128.698731518742)) ;
#135134 = CARTESIAN_POINT('Ctrl Pts',(-25.0453888541943,14.2686028129511,
128.890481281382)) ;
#135135 = CARTESIAN_POINT('Ctrl Pts',(-25.1157749327763,14.4199618502008,
129.129219228183)) ;
#135136 = CARTESIAN_POINT('Ctrl Pts',(-25.1962537469819,14.4998958219189,
129.397417258709)) ;
#135137 = CARTESIAN_POINT('Ctrl Pts',(-25.2806998076144,14.5025664794371,
129.677347381576)) ;
#135138 = CARTESIAN_POINT('Ctrl Pts',(-25.3614130293349,14.4280652825415,
129.946141834169)) ;
#135139 = CARTESIAN_POINT('Ctrl Pts',(-25.4327613411336,14.2819177513075,
130.187667258866)) ;
#135140 = CARTESIAN_POINT('Ctrl Pts',(-25.4888836010397,14.0723877227319,
130.384948804485)) ;
#135141 = CARTESIAN_POINT('Ctrl Pts',(-25.524217369076,13.8191595273478,130.52109290564)) ;
#135142 = CARTESIAN_POINT('Ctrl Pts',(-25.5363621720147,13.5356702848312,
130.589764696207)) ;
#135143 = CARTESIAN_POINT('Ctrl Pts',(-25.5233799731752,13.2451626614465,
130.584896539849)) ;
#135144 = CARTESIAN_POINT('Ctrl Pts',(-25.4853193673611,12.9658959397094,
130.506957297054)) ;
#135145 = CARTESIAN_POINT('Ctrl Pts',(-25.4245567948317,12.720867949973,130.362513148524)) ;
#135146 = CARTESIAN_POINT('Ctrl Pts',(-25.3444357384131,12.5256178596935,
130.161588938401)) ;
#135147 = CARTESIAN_POINT('Ctrl Pts',(-25.2502354927177,12.3947249390078,
129.91946984754)) ;
#135148 = CARTESIAN_POINT('Ctrl Pts',(-25.1471557384846,12.3373274128747,
129.651622343389)) ;
#135149 = CARTESIAN_POINT('Ctrl Pts',(-25.04352722843,12.3577351376061,129.3818280718)) ;
#135150 = CARTESIAN_POINT('Ctrl Pts',(-24.9440625937448,12.4546492514378,
129.124509048456)) ;
#135151 = CARTESIAN_POINT('Ctrl Pts',(-24.8564471604785,12.6210676591383,
128.901700870073)) ;
#135152 = CARTESIAN_POINT('Ctrl Pts',(-24.7859855036776,12.8446766854148,
128.728972290107)) ;
#135153 = CARTESIAN_POINT('Ctrl Pts',(-24.7369148940067,13.108808163257,128.618635013836)) ;
#135154 = CARTESIAN_POINT('Ctrl Pts',(-24.7117898455147,13.3979062620311,
128.578541432007)) ;
#135155 = CARTESIAN_POINT('Ctrl Pts',(-24.7120774707783,13.6859097607706,
128.612344349061)) ;
#135156 = CARTESIAN_POINT('Ctrl Pts',(-24.7366917620368,13.9567565280856,
128.717390290963)) ;
#135157 = CARTESIAN_POINT('Ctrl Pts',(-24.7836759760245,14.1899349125241,
128.887914867791)) ;
#135158 = CARTESIAN_POINT('Ctrl Pts',(-24.8478937377255,14.3662692626876,
129.10842421568)) ;
#135159 = CARTESIAN_POINT('Ctrl Pts',(-24.9254379812952,14.4768289979695,
129.368240618362)) ;
#135160 = CARTESIAN_POINT('Ctrl Pts',(-25.0089189154175,14.5109207090365,
129.645218161262)) ;
#135161 = CARTESIAN_POINT('Ctrl Pts',(-25.0919501200887,14.4673589954117,
129.920875758852)) ;
#135162 = CARTESIAN_POINT('Ctrl Pts',(-25.1679324131496,14.3490298117359,
130.175949093355)) ;
#135163 = CARTESIAN_POINT('Ctrl Pts',(-25.2306776791176,14.1643442573792,
130.392364551844)) ;
#135164 = CARTESIAN_POINT('Ctrl Pts',(-25.2749172208417,13.9269540764464,
130.554674425406)) ;
#135165 = CARTESIAN_POINT('Ctrl Pts',(-25.296881801977,13.6529087066834,130.651991768824)) ;
#135166 = CARTESIAN_POINT('Ctrl Pts',(-25.294121582554,13.3625040426011,130.677064089887)) ;
#135167 = CARTESIAN_POINT('Ctrl Pts',(-25.2661584777254,13.0764917625792,
130.628507586136)) ;
#135168 = CARTESIAN_POINT('Ctrl Pts',(-25.2142358128611,12.8152457852602,
130.509968872735)) ;
#135169 = CARTESIAN_POINT('Ctrl Pts',(-25.1414105163864,12.5977360848388,
130.330346617025)) ;
#135170 = CARTESIAN_POINT('Ctrl Pts',(-25.0521369052221,12.4392301767845,
130.102679861577)) ;
#135171 = CARTESIAN_POINT('Ctrl Pts',(-24.9519825847367,12.3513755992719,
129.843259987167)) ;
#135172 = CARTESIAN_POINT('Ctrl Pts',(-24.8480528333298,12.3399316332142,
129.572627714051)) ;
#135173 = CARTESIAN_POINT('Ctrl Pts',(-24.7452323261505,12.4070554351268,
129.305672373312)) ;
#135174 = CARTESIAN_POINT('Ctrl Pts',(-24.653114699296,12.5451369869361,129.069390792946)) ;
#135175 = CARTESIAN_POINT('Ctrl Pts',(-24.574658401759,12.7477726868892,128.873467031278)) ;
#135176 = CARTESIAN_POINT('Ctrl Pts',(-24.516485448288,12.9979367372735,128.736605448719)) ;
#135177 = CARTESIAN_POINT('Ctrl Pts',(-24.4813744014041,13.2792370978739,
128.667217092649)) ;
#135178 = CARTESIAN_POINT('Ctrl Pts',(-24.4713970354524,13.5701580555343,
128.671163049425)) ;
#135179 = CARTESIAN_POINT('Ctrl Pts',(-24.4863380916386,13.8505377724051,
128.747899411962)) ;
#135180 = CARTESIAN_POINT('Ctrl Pts',(-24.5245439679385,14.1007512372239,
128.892655666103)) ;
#135181 = CARTESIAN_POINT('Ctrl Pts',(-24.5824402788279,14.3021715583994,
129.094893574169)) ;
#135182 = CARTESIAN_POINT('Ctrl Pts',(-24.6554257346924,14.4410638226486,
129.341309329826)) ;
#135183 = CARTESIAN_POINT('Ctrl Pts',(-24.7373356695316,14.506420576945,129.613776649341)) ;
#135184 = CARTESIAN_POINT('Ctrl Pts',(-24.8210078848283,14.4944296739133,
129.89116801343)) ;
#135185 = CARTESIAN_POINT('Ctrl Pts',(-24.9008406879447,14.4055611915821,
130.157574926146)) ;
#135186 = CARTESIAN_POINT('Ctrl Pts',(-24.9694636925505,14.2469875620131,
130.391056099313)) ;
#135187 = CARTESIAN_POINT('Ctrl Pts',(-25.0219599711088,14.0284942715184,
130.577615505577)) ;
#135188 = CARTESIAN_POINT('Ctrl Pts',(-25.053320022464,13.7670074742828,130.70234813533)) ;
#135189 = CARTESIAN_POINT('Ctrl Pts',(-25.0607089051815,13.4805781215048,
130.757097162265)) ;
#135190 = CARTESIAN_POINT('Ctrl Pts',(-25.0430061476845,13.1913388058783,
130.73838961606)) ;
#135191 = CARTESIAN_POINT('Ctrl Pts',(-25.0005234997867,12.9172330933754,
130.647473812606)) ;
#135192 = CARTESIAN_POINT('Ctrl Pts',(-24.9358367964898,12.6799728703758,
130.491596969194)) ;
#135193 = CARTESIAN_POINT('Ctrl Pts',(-24.8520526958292,12.4949910418975,
130.280173035867)) ;
#135194 = CARTESIAN_POINT('Ctrl Pts',(-24.756283433586,12.3781840447206,130.033296564361)) ;
#135195 = CARTESIAN_POINT('Ctrl Pts',(-24.6522083130104,12.3352411023339,
129.762603753164)) ;
#135196 = CARTESIAN_POINT('Ctrl Pts',(-24.5492013359519,12.3701183957634,
129.494563600041)) ;
#135197 = CARTESIAN_POINT('Ctrl Pts',(-24.4510228781676,12.4815908370187,
129.241159666924)) ;
#135198 = CARTESIAN_POINT('Ctrl Pts',(-24.3668186999168,12.6586744463426,
129.02808228214)) ;
#135199 = CARTESIAN_POINT('Ctrl Pts',(-24.2996856218142,12.8927064505131,
128.86527445598)) ;
#135200 = CARTESIAN_POINT('Ctrl Pts',(-24.2552426505653,13.1615895986342,
128.768318934161)) ;
#135201 = CARTESIAN_POINT('Ctrl Pts',(-24.2347791741716,13.4527337961883,
128.741859841865)) ;
#135202 = CARTESIAN_POINT('Ctrl Pts',(-24.2398184692911,13.7397606263225,
128.789657130047)) ;
#135203 = CARTESIAN_POINT('Ctrl Pts',(-24.2689320023009,14.0044956878458,
128.907831044878)) ;
#135204 = CARTESIAN_POINT('Ctrl Pts',(-24.3192589693072,14.2270717047825,
129.087893938316)) ;
#135205 = CARTESIAN_POINT('Ctrl Pts',(-24.386637598686,14.3928428531141,129.31784383242)) ;
#135206 = CARTESIAN_POINT('Ctrl Pts',(-24.4659391407555,14.4891679896536,
129.582798342604)) ;
#135207 = CARTESIAN_POINT('Ctrl Pts',(-24.5493645856168,14.5086708936273,
129.859423076708)) ;
#135208 = CARTESIAN_POINT('Ctrl Pts',(-24.6318807172738,14.4507091204102,
130.133696348165)) ;
#135209 = CARTESIAN_POINT('Ctrl Pts',(-24.7058567597393,14.318823465338,130.382937634357)) ;
#135210 = CARTESIAN_POINT('Ctrl Pts',(-24.7654056750014,14.1234067424229,
130.589957999186)) ;
#135211 = CARTESIAN_POINT('Ctrl Pts',(-24.8057595992627,13.8772496577341,
130.740994985991)) ;
#135212 = CARTESIAN_POINT('Ctrl Pts',(-24.8231799857801,13.5994498547175,
130.82492878504)) ;
#135213 = CARTESIAN_POINT('Ctrl Pts',(-24.8155893045152,13.3067289539218,
130.836068714423)) ;
#135214 = CARTESIAN_POINT('Ctrl Pts',(-24.7830973206933,13.025513208076,130.774091996489)) ;
#135215 = CARTESIAN_POINT('Ctrl Pts',(-24.7270577046474,12.7708776887036,
130.643534343482)) ;
#135216 = CARTESIAN_POINT('Ctrl Pts',(-24.6505077984341,12.5628412979246,
130.453131427416)) ;
#135217 = CARTESIAN_POINT('Ctrl Pts',(-24.5589760348122,12.4171764122364,
130.218786009453)) ;
#135218 = CARTESIAN_POINT('Ctrl Pts',(-24.4570551071365,12.3431378359771,
129.954350410602)) ;
#135219 = CARTESIAN_POINT('Ctrl Pts',(-24.3533214115063,12.3467434972734,
129.684210676246)) ;
#135220 = CARTESIAN_POINT('Ctrl Pts',(-24.2523283182393,12.4272274658185,
129.422376802438)) ;
#135221 = CARTESIAN_POINT('Ctrl Pts',(-24.1617932807192,12.5790158149027,
129.190994958755)) ;
#135222 = CARTESIAN_POINT('Ctrl Pts',(-24.0869579392724,12.7916687829571,
129.005564094205)) ;
#135223 = CARTESIAN_POINT('Ctrl Pts',(-24.0328055760906,13.0498138992039,
128.8805514449)) ;
#135224 = CARTESIAN_POINT('Ctrl Pts',(-24.002521804032,13.3331756720239,128.825089124936)) ;
#135225 = CARTESIAN_POINT('Ctrl Pts',(-23.9971725769105,13.6238935345468,
128.842575947387)) ;
#135226 = CARTESIAN_POINT('Ctrl Pts',(-24.0167753636582,13.9010885274901,
128.933062863381)) ;
#135227 = CARTESIAN_POINT('Ctrl Pts',(-24.0590128945408,14.1432054793993,
129.089568959686)) ;
#135228 = CARTESIAN_POINT('Ctrl Pts',(-24.1203695555296,14.3341070280144,
129.302019247719)) ;
#135229 = CARTESIAN_POINT('Ctrl Pts',(-24.1950418049019,14.4587991787124,
129.553138711427)) ;
#135230 = CARTESIAN_POINT('Ctrl Pts',(-24.2777268658875,14.5101605081857,
129.827811432152)) ;
#135231 = CARTESIAN_POINT('Ctrl Pts',(-24.3615395865942,14.4834097576633,
130.105796352381)) ;
#135232 = CARTESIAN_POINT('Ctrl Pts',(-24.4396001237497,14.380986704451,130.366925214371)) ;
#135233 = CARTESIAN_POINT('Ctrl Pts',(-24.5059188478657,14.2089571607828,
130.593906733665)) ;
#135234 = CARTESIAN_POINT('Ctrl Pts',(-24.5543423873352,13.9828180453883,
130.768283768123)) ;
#135235 = CARTESIAN_POINT('Ctrl Pts',(-24.5815804292821,13.7132629209954,
130.881224790375)) ;
#135236 = CARTESIAN_POINT('Ctrl Pts',(-24.5841620980753,13.42583764063,130.921759059005)) ;
#135237 = CARTESIAN_POINT('Ctrl Pts',(-24.5616991302751,13.1374631065902,
130.889232264708)) ;
#135238 = CARTESIAN_POINT('Ctrl Pts',(-24.5148271925072,12.8691197006536,
130.785439835784)) ;
#135239 = CARTESIAN_POINT('Ctrl Pts',(-24.4460595852779,12.6403113443668,
130.617737495797)) ;
#135240 = CARTESIAN_POINT('Ctrl Pts',(-24.3602783070861,12.468420702256,130.400139902644)) ;
#135241 = CARTESIAN_POINT('Ctrl Pts',(-24.2614984282295,12.3638000217504,
130.144889114756)) ;
#135242 = CARTESIAN_POINT('Ctrl Pts',(-24.1577920148866,12.3359859144704,
129.874955907544)) ;
#135243 = CARTESIAN_POINT('Ctrl Pts',(-24.054756872384,12.3855342690204,129.607074345636)) ;
#135244 = CARTESIAN_POINT('Ctrl Pts',(-23.9592387590454,12.5097023136888,
129.361184743235)) ;
#135245 = CARTESIAN_POINT('Ctrl Pts',(-23.8775758716564,12.6987169895182,
129.155691106511)) ;
#135246 = CARTESIAN_POINT('Ctrl Pts',(-23.8143557456443,12.9413958856346,
129.004310292951)) ;
#135247 = CARTESIAN_POINT('Ctrl Pts',(-23.7742609530853,13.2164083911014,
128.920187229679)) ;
#135248 = CARTESIAN_POINT('Ctrl Pts',(-23.7587189631835,13.5077476116907,
128.907983756604)) ;
#135249 = CARTESIAN_POINT('Ctrl Pts',(-23.7683966260473,13.7917084995172,
128.969294505237)) ;
#135250 = CARTESIAN_POINT('Ctrl Pts',(-23.8017090745378,14.0497089633418,
129.099691778832)) ;
#135251 = CARTESIAN_POINT('Ctrl Pts',(-23.855687851068,14.2632250030891,129.290500820459)) ;
#135252 = CARTESIAN_POINT('Ctrl Pts',(-23.9259445764529,14.4168537708596,
129.528960264585)) ;
#135253 = CARTESIAN_POINT('Ctrl Pts',(-24.0063154571533,14.4987598986465,
129.796873298139)) ;
#135254 = CARTESIAN_POINT('Ctrl Pts',(-24.0905209887515,14.5035045718472,
130.07601230486)) ;
#135255 = CARTESIAN_POINT('Ctrl Pts',(-24.1714640122117,14.4313229997249,
130.345485263966)) ;
#135256 = CARTESIAN_POINT('Ctrl Pts',(-24.243380136318,14.286096674379,130.588809864043)) ;
#135257 = CARTESIAN_POINT('Ctrl Pts',(-24.2994203289572,14.0806888556304,
130.785462444038)) ;
#135258 = CARTESIAN_POINT('Ctrl Pts',(-24.3358061636431,13.8265805447723,
130.924971011733)) ;
#135259 = CARTESIAN_POINT('Ctrl Pts',(-24.3485662665821,13.5441879409374,
130.995358908411)) ;
#135260 = CARTESIAN_POINT('Ctrl Pts',(-24.3362787692544,13.2530370689606,
130.992594119063)) ;
#135261 = CARTESIAN_POINT('Ctrl Pts',(-24.2990565233592,12.9741114175935,
130.916980614884)) ;
#135262 = CARTESIAN_POINT('Ctrl Pts',(-24.2387980421576,12.7272119216586,
130.774093243821)) ;
#135263 = CARTESIAN_POINT('Ctrl Pts',(-24.1592542721153,12.5305677659782,
130.57481255156)) ;
#135264 = CARTESIAN_POINT('Ctrl Pts',(-24.0653992661587,12.3976028767503,
130.333704016612)) ;
#135265 = CARTESIAN_POINT('Ctrl Pts',(-23.9625403093089,12.3378877564715,
130.06647786499)) ;
#135266 = CARTESIAN_POINT('Ctrl Pts',(-23.8586656317476,12.3561146457162,
129.796030313594)) ;
#135267 = CARTESIAN_POINT('Ctrl Pts',(-23.7592617382335,12.4504996091204,
129.538781451731)) ;
#135268 = CARTESIAN_POINT('Ctrl Pts',(-23.6710781493093,12.6151918179393,
129.314368558311)) ;
#135269 = CARTESIAN_POINT('Ctrl Pts',(-23.6000847768971,12.8367627956422,
129.140023816127)) ;
#135270 = CARTESIAN_POINT('Ctrl Pts',(-23.5500037307086,13.102471284239,129.027040548326)) ;
#135271 = CARTESIAN_POINT('Ctrl Pts',(-23.5244629176484,13.388098474674,128.985365037134)) ;
#135272 = CARTESIAN_POINT('Ctrl Pts',(-23.5239179211507,13.6786302634614,
129.017000214703)) ;
#135273 = CARTESIAN_POINT('Ctrl Pts',(-23.5479482075075,13.9495118019851,
129.120261172471)) ;
#135274 = CARTESIAN_POINT('Ctrl Pts',(-23.5940539896427,14.1831630717315,
129.28807205042)) ;
#135275 = CARTESIAN_POINT('Ctrl Pts',(-23.658087369295,14.3622887251467,129.508197418047)) ;
#135276 = CARTESIAN_POINT('Ctrl Pts',(-23.7354964858561,14.4748192529362,
129.767663246934)) ;
#135277 = CARTESIAN_POINT('Ctrl Pts',(-23.8186008712506,14.5109473630978,
130.043427649505)) ;
#135278 = CARTESIAN_POINT('Ctrl Pts',(-23.9016485189198,14.46989386631,130.319093678178)) ;
#135279 = CARTESIAN_POINT('Ctrl Pts',(-23.9780326629865,14.3536144736526,
130.57538079303)) ;
#135280 = CARTESIAN_POINT('Ctrl Pts',(-24.041317392537,14.17062113719,130.793395793898)) ;
#135281 = CARTESIAN_POINT('Ctrl Pts',(-24.0862233608817,13.933736573907,130.957750623604)) ;
#135282 = CARTESIAN_POINT('Ctrl Pts',(-24.1087782693582,13.6617104442443,
131.056639640472)) ;
#135283 = CARTESIAN_POINT('Ctrl Pts',(-24.1067652069901,13.3701432171844,
131.084050982405)) ;
#135284 = CARTESIAN_POINT('Ctrl Pts',(-24.0794150200347,13.0839501475181,
131.037263800254)) ;
#135285 = CARTESIAN_POINT('Ctrl Pts',(-24.0283415442683,12.8226369063403,
130.921088721576)) ;
#135286 = CARTESIAN_POINT('Ctrl Pts',(-23.9561135287856,12.6036153158418,
130.74320474868)) ;
#135287 = CARTESIAN_POINT('Ctrl Pts',(-23.8674374985634,12.4432239429731,
130.517228131168)) ;
#135288 = CARTESIAN_POINT('Ctrl Pts',(-23.7669177824065,12.3525997513282,
130.256937329486)) ;
#135289 = CARTESIAN_POINT('Ctrl Pts',(-23.6631589097691,12.3393903655815,
129.986759745082)) ;
#135290 = CARTESIAN_POINT('Ctrl Pts',(-23.5608451726887,12.403468098602,129.721057322036)) ;
#135291 = CARTESIAN_POINT('Ctrl Pts',(-23.4675538333872,12.5405072085783,
129.481626938511)) ;
#135292 = CARTESIAN_POINT('Ctrl Pts',(-23.388662980097,12.7420005519616,129.284449551793)) ;
#135293 = CARTESIAN_POINT('Ctrl Pts',(-23.3301053404809,12.9900801149227,
129.146339662681)) ;
#135294 = CARTESIAN_POINT('Ctrl Pts',(-23.2942598700259,13.2708158721555,
129.07481369419)) ;
#135295 = CARTESIAN_POINT('Ctrl Pts',(-23.2835507653219,13.5613604134334,
129.07658052044)) ;
#135296 = CARTESIAN_POINT('Ctrl Pts',(-23.2977457009926,13.8428560081929,
129.151189048699)) ;
#135297 = CARTESIAN_POINT('Ctrl Pts',(-23.3355877732922,14.0951246502648,
129.295029201952)) ;
#135298 = CARTESIAN_POINT('Ctrl Pts',(-23.392640021767,14.2968154125605,129.494589775277)) ;
#135299 = CARTESIAN_POINT('Ctrl Pts',(-23.4654695271126,14.4382062812648,
129.740653917803)) ;
#135300 = CARTESIAN_POINT('Ctrl Pts',(-23.5470349400498,14.5055713938207,
130.012034404642)) ;
#135301 = CARTESIAN_POINT('Ctrl Pts',(-23.6308595315768,14.4957941932041,
130.289927886282)) ;
#135302 = CARTESIAN_POINT('Ctrl Pts',(-23.7106798599952,14.4095662340998,
130.556186374908)) ;
#135303 = CARTESIAN_POINT('Ctrl Pts',(-23.7802571461447,14.2515335127425,
130.792730605287)) ;
#135304 = CARTESIAN_POINT('Ctrl Pts',(-23.8330271584667,14.0347236874785,
130.979999898394)) ;
#135305 = CARTESIAN_POINT('Ctrl Pts',(-23.8649144470802,13.7751700114088,
131.106159195577)) ;
#135306 = CARTESIAN_POINT('Ctrl Pts',(-23.8730939748177,13.489555102194,131.163174955555)) ;
#135307 = CARTESIAN_POINT('Ctrl Pts',(-23.8560200827014,13.1989624545804,
131.146444379055)) ;
#135308 = CARTESIAN_POINT('Ctrl Pts',(-23.8142948031392,12.9245155762064,
131.057679563774)) ;
#135309 = CARTESIAN_POINT('Ctrl Pts',(-23.7497390288408,12.6850932088169,
130.90236186876)) ;
#135310 = CARTESIAN_POINT('Ctrl Pts',(-23.6676401734867,12.5007200500438,
130.695387264516)) ;
#135311 = CARTESIAN_POINT('Ctrl Pts',(-23.5710799792398,12.3802348015134,
130.446601105623)) ;
#135312 = CARTESIAN_POINT('Ctrl Pts',(-23.4680387193144,12.3354177830535,
130.178616720221)) ;
#135313 = CARTESIAN_POINT('Ctrl Pts',(-23.3639870057212,12.3682931650198,
129.907845197495)) ;
#135314 = CARTESIAN_POINT('Ctrl Pts',(-23.2665557781875,12.4764500222757,
129.656260795804)) ;
#135315 = CARTESIAN_POINT('Ctrl Pts',(-23.1812074615382,12.6527561756398,
129.440099421206)) ;
#135316 = CARTESIAN_POINT('Ctrl Pts',(-23.1137789148354,12.8841372675975,
129.276247072773)) ;
#135317 = CARTESIAN_POINT('Ctrl Pts',(-23.0682028417558,13.1550291136418,
129.176337392218)) ;
#135318 = CARTESIAN_POINT('Ctrl Pts',(-23.0472767378411,13.4437302360126,
129.148261982065)) ;
#135319 = CARTESIAN_POINT('Ctrl Pts',(-23.0515496084932,13.7319393007276,
129.193922359653)) ;
#135320 = CARTESIAN_POINT('Ctrl Pts',(-23.079878251099,13.9965481623833,129.309665379139)) ;
#135321 = CARTESIAN_POINT('Ctrl Pts',(-23.129741526764,14.2215298170475,129.488488454029)) ;
#135322 = CARTESIAN_POINT('Ctrl Pts',(-23.1968818888558,14.3891483272759,
129.717799600751)) ;
#135323 = CARTESIAN_POINT('Ctrl Pts',(-23.2754021964238,14.4871687024338,
129.980255089599)) ;
#135324 = CARTESIAN_POINT('Ctrl Pts',(-23.3593328759968,14.5093408079897,
130.258577404978)) ;
#135325 = CARTESIAN_POINT('Ctrl Pts',(-23.4420335332337,14.4530254583256,
130.533420307647)) ;
#135326 = CARTESIAN_POINT('Ctrl Pts',(-23.5159486858221,14.3240305585518,
130.782295669503)) ;
#135327 = CARTESIAN_POINT('Ctrl Pts',(-23.5763068870408,14.1290979717854,
130.991878121919)) ;
#135328 = CARTESIAN_POINT('Ctrl Pts',(-23.617068843589,13.8855604155571,131.143910620301)) ;
#135329 = CARTESIAN_POINT('Ctrl Pts',(-23.6352727286933,13.6058416707122,
131.230442968303)) ;
#135330 = CARTESIAN_POINT('Ctrl Pts',(-23.6283964341607,13.3160021377259,
131.243341112372)) ;
#135331 = CARTESIAN_POINT('Ctrl Pts',(-23.5965464340223,13.0326886676077,
131.183420690455)) ;
#135332 = CARTESIAN_POINT('Ctrl Pts',(-23.5408985622457,12.7766372190837,
131.054072194123)) ;
#135333 = CARTESIAN_POINT('Ctrl Pts',(-23.4649595861684,12.5676698161814,
130.865387166735)) ;
#135334 = CARTESIAN_POINT('Ctrl Pts',(-23.3740967453034,12.4206517790888,
130.632884178497)) ;
#135335 = CARTESIAN_POINT('Ctrl Pts',(-23.2727082372118,12.3443150505119,
130.369901024895)) ;
#135336 = CARTESIAN_POINT('Ctrl Pts',(-23.1684546893583,12.3454567433165,
130.098404386445)) ;
#135337 = CARTESIAN_POINT('Ctrl Pts',(-23.0671327036379,12.4241540146565,
129.835658717647)) ;
#135338 = CARTESIAN_POINT('Ctrl Pts',(-22.9764947583752,12.5736454649868,
129.60388157098)) ;
#135339 = CARTESIAN_POINT('Ctrl Pts',(-22.9011806814661,12.7844244258342,
129.417017819213)) ;
#135340 = CARTESIAN_POINT('Ctrl Pts',(-22.8463459628872,13.041264478038,129.289992771218)) ;
#135341 = CARTESIAN_POINT('Ctrl Pts',(-22.815230919969,13.3250313838274,129.232207692813)) ;
#135342 = CARTESIAN_POINT('Ctrl Pts',(-22.8092125202162,13.6156492492809,
129.247717690027)) ;
#135343 = CARTESIAN_POINT('Ctrl Pts',(-22.8280212526032,13.8929002803611,
129.335801002832)) ;
#135344 = CARTESIAN_POINT('Ctrl Pts',(-22.8696833153775,14.1366366428793,
129.490673844657)) ;
#135345 = CARTESIAN_POINT('Ctrl Pts',(-22.9303059421642,14.3287833833703,
129.70086742119)) ;
#135346 = CARTESIAN_POINT('Ctrl Pts',(-23.0049559964505,14.4563288342089,
129.952070625789)) ;
#135347 = CARTESIAN_POINT('Ctrl Pts',(-23.0876811988293,14.5097636463918,
130.226920951019)) ;
#135348 = CARTESIAN_POINT('Ctrl Pts',(-23.171313625943,14.4852491819093,130.504285160366)) ;
#135349 = CARTESIAN_POINT('Ctrl Pts',(-23.2495616828516,14.385213180382,130.765927789329)) ;
#135350 = CARTESIAN_POINT('Ctrl Pts',(-23.3164467304666,14.2148994362801,
130.994611083723)) ;
#135351 = CARTESIAN_POINT('Ctrl Pts',(-23.3654737459425,13.9895605141043,
131.170821580244)) ;
#135352 = CARTESIAN_POINT('Ctrl Pts',(-23.3932709418014,13.7226496289756,
131.285186238845)) ;
#135353 = CARTESIAN_POINT('Ctrl Pts',(-23.3966715321499,13.4342098859693,
131.328274909581)) ;
#135354 = CARTESIAN_POINT('Ctrl Pts',(-23.3749521692447,13.1458182759752,
131.297881508113)) ;
#135355 = CARTESIAN_POINT('Ctrl Pts',(-23.3285769346008,12.8759127132536,
131.195640591877)) ;
#135356 = CARTESIAN_POINT('Ctrl Pts',(-23.2608087751802,12.6468868556867,
131.030665242811)) ;
#135357 = CARTESIAN_POINT('Ctrl Pts',(-23.1749384545703,12.4721832296684,
130.81301511834)) ;
#135358 = CARTESIAN_POINT('Ctrl Pts',(-23.0772501521557,12.3661739274481,
130.560671910315)) ;
#135359 = CARTESIAN_POINT('Ctrl Pts',(-22.972758046801,12.3355863385396,130.288726503058)) ;
#135360 = CARTESIAN_POINT('Ctrl Pts',(-22.8698300820149,12.3831198658751,
130.021082533712)) ;
#135361 = CARTESIAN_POINT('Ctrl Pts',(-22.7739061268904,12.5053833023315,
129.774046335208)) ;
#135362 = CARTESIAN_POINT('Ctrl Pts',(-22.6919791045737,12.6923270702948,
129.567704270438)) ;
#135363 = CARTESIAN_POINT('Ctrl Pts',(-22.6281112723494,12.9335865705139,
129.414426275698)) ;
#135364 = CARTESIAN_POINT('Ctrl Pts',(-22.5872544610613,13.2085814539572,
129.328158922446)) ;
#135365 = CARTESIAN_POINT('Ctrl Pts',(-22.5710404902249,13.4990557588074,
129.313907984072)) ;
#135366 = CARTESIAN_POINT('Ctrl Pts',(-22.5799753665134,13.7836907462661,
129.373072556554)) ;
#135367 = CARTESIAN_POINT('Ctrl Pts',(-22.612638583778,14.0427281414566,129.501571243045)) ;
#135368 = CARTESIAN_POINT('Ctrl Pts',(-22.6660762367978,14.2577309750281,
129.69079806233)) ;
#135369 = CARTESIAN_POINT('Ctrl Pts',(-22.7357975374954,14.4131664617501,
129.927633756715)) ;
#135370 = CARTESIAN_POINT('Ctrl Pts',(-22.8161137666784,14.4973755702956,
130.195456113862)) ;
#135371 = CARTESIAN_POINT('Ctrl Pts',(-22.8998820017925,14.5046724130054,
130.47314586159)) ;
#135372 = CARTESIAN_POINT('Ctrl Pts',(-22.9816064513032,14.4343111747756,
130.745147804022)) ;
#135373 = CARTESIAN_POINT('Ctrl Pts',(-23.0536227051492,14.2913904033354,
130.98864811284)) ;
#135374 = CARTESIAN_POINT('Ctrl Pts',(-23.1102843211941,14.0872940403586,
131.187176359758)) ;
#135375 = CARTESIAN_POINT('Ctrl Pts',(-23.1472375329922,13.8349907742835,
131.328253449348)) ;
#135376 = CARTESIAN_POINT('Ctrl Pts',(-23.1607772342592,13.5522018199285,
131.401036362566)) ;
#135377 = CARTESIAN_POINT('Ctrl Pts',(-23.1491871925298,13.2611771320633,
131.400285897439)) ;
#135378 = CARTESIAN_POINT('Ctrl Pts',(-23.1125952006362,12.9814107201437,
131.326544774095)) ;
#135379 = CARTESIAN_POINT('Ctrl Pts',(-23.0531566614903,12.7341369610279,
131.185942865115)) ;
#135380 = CARTESIAN_POINT('Ctrl Pts',(-22.9739547949964,12.535166216503,130.98774443351)) ;
#135381 = CARTESIAN_POINT('Ctrl Pts',(-22.8800044204222,12.4000170891871,
130.746489022896)) ;
#135382 = CARTESIAN_POINT('Ctrl Pts',(-22.7777942394703,12.3385941106561,
130.480992016477)) ;
#135383 = CARTESIAN_POINT('Ctrl Pts',(-22.6737045237347,12.3545286685026,
130.209973410253)) ;
#135384 = CARTESIAN_POINT('Ctrl Pts',(-22.574018025731,12.4469846430608,129.951917332464)) ;
#135385 = CARTESIAN_POINT('Ctrl Pts',(-22.4853397321754,12.6102579412087,
129.726108518223)) ;
#135386 = CARTESIAN_POINT('Ctrl Pts',(-22.4141387274598,12.8296977311719,
129.551032278381)) ;
#135387 = CARTESIAN_POINT('Ctrl Pts',(-22.3635165048781,13.0929763552362,
129.436306120848)) ;
#135388 = CARTESIAN_POINT('Ctrl Pts',(-22.3370222640428,13.3798715107165,
129.392040554444)) ;
#135389 = CARTESIAN_POINT('Ctrl Pts',(-22.3358180956749,13.6705227535771,
129.421738962196)) ;
#135390 = CARTESIAN_POINT('Ctrl Pts',(-22.359121262081,13.9421700423004,129.522864634634)) ;
#135391 = CARTESIAN_POINT('Ctrl Pts',(-22.4048936915904,14.1780191011813,
129.689842088352)) ;
#135392 = CARTESIAN_POINT('Ctrl Pts',(-22.4683015911897,14.3579768124892,
129.908015928199)) ;
#135393 = CARTESIAN_POINT('Ctrl Pts',(-22.5452274463354,14.4725057553617,
130.165996866725)) ;
#135394 = CARTESIAN_POINT('Ctrl Pts',(-22.6283868280108,14.5110248787396,
130.441981808158)) ;
#135395 = CARTESIAN_POINT('Ctrl Pts',(-22.7115926468901,14.4721191969269,
130.718131866034)) ;
#135396 = CARTESIAN_POINT('Ctrl Pts',(-22.7882774144574,14.3577454336847,
130.975310558445)) ;
#135397 = CARTESIAN_POINT('Ctrl Pts',(-22.8518198048839,14.1770688666527,
131.193977525084)) ;
#135398 = CARTESIAN_POINT('Ctrl Pts',(-22.8974027115045,13.9416997327419,
131.360307596844)) ;
#135399 = CARTESIAN_POINT('Ctrl Pts',(-22.9206820190988,13.6694104353782,
131.461436266431)) ;
#135400 = CARTESIAN_POINT('Ctrl Pts',(-22.9194213574652,13.3798585935035,
131.490838835533)) ;
#135401 = CARTESIAN_POINT('Ctrl Pts',(-22.8929170330155,13.0927640382574,
131.446571141722)) ;
#135402 = CARTESIAN_POINT('Ctrl Pts',(-22.8423030043868,12.8294542733058,
131.331865445954)) ;
#135403 = CARTESIAN_POINT('Ctrl Pts',(-22.7706185679307,12.6090080043084,
131.155563913664)) ;
#135404 = CARTESIAN_POINT('Ctrl Pts',(-22.6821571255679,12.4466659582347,
130.930272433196)) ;
#135405 = CARTESIAN_POINT('Ctrl Pts',(-22.5824728331909,12.3544265354386,
130.672221564255)) ;
#135406 = CARTESIAN_POINT('Ctrl Pts',(-22.478522759517,12.338485550426,130.401560070963)) ;
#135407 = CARTESIAN_POINT('Ctrl Pts',(-22.3754966015088,12.4009576070215,
130.133958949611)) ;
#135408 = CARTESIAN_POINT('Ctrl Pts',(-22.2823680889779,12.5356622675021,
129.894847033385)) ;
#135409 = CARTESIAN_POINT('Ctrl Pts',(-22.2032360996956,12.7342792931547,
129.696815676907)) ;
#135410 = CARTESIAN_POINT('Ctrl Pts',(-22.1436939987442,12.9822470405306,
129.555989965758)) ;
#135411 = CARTESIAN_POINT('Ctrl Pts',(-22.1071406671597,13.2626104241267,
129.482419788097)) ;
#135412 = CARTESIAN_POINT('Ctrl Pts',(-22.0957144593787,13.5537330357078,
129.482159506806)) ;
#135413 = CARTESIAN_POINT('Ctrl Pts',(-22.1092685563454,13.8350780443648,
129.554823798795)) ;
#135414 = CARTESIAN_POINT('Ctrl Pts',(-22.1461475103679,14.0872562376869,
129.695659561939)) ;
#135415 = CARTESIAN_POINT('Ctrl Pts',(-22.2030821358645,14.2922552735091,
129.895131181954)) ;
#135416 = CARTESIAN_POINT('Ctrl Pts',(-22.2754289643042,14.4349645919609,
130.139699349458)) ;
#135417 = CARTESIAN_POINT('Ctrl Pts',(-22.3564708008619,14.5045540577175,
130.40942261917)) ;
#135418 = CARTESIAN_POINT('Ctrl Pts',(-22.4406441329642,14.4973581396257,
130.688457173911)) ;
#135419 = CARTESIAN_POINT('Ctrl Pts',(-22.5209414268602,14.4126016842873,
130.956235143864)) ;
#135420 = CARTESIAN_POINT('Ctrl Pts',(-22.5903401138937,14.2578370889756,
131.191978979017)) ;
#135421 = CARTESIAN_POINT('Ctrl Pts',(-22.643899231601,14.0423606370671,131.381638018117)) ;
#135422 = CARTESIAN_POINT('Ctrl Pts',(-22.676541227732,13.7833430848993,131.510062783894)) ;
#135423 = CARTESIAN_POINT('Ctrl Pts',(-22.6854014712124,13.4972454461382,
131.569174829683)) ;
#135424 = CARTESIAN_POINT('Ctrl Pts',(-22.6691263169549,13.2077137971034,
131.554634071507)) ;
#135425 = CARTESIAN_POINT('Ctrl Pts',(-22.6279874269016,12.9318531124,131.467669892297)) ;
#135426 = CARTESIAN_POINT('Ctrl Pts',(-22.5644211603477,12.6922552108513,
131.31506619976)) ;
#135427 = CARTESIAN_POINT('Ctrl Pts',(-22.4822337913331,12.504666487009,131.108074794862)) ;
#135428 = CARTESIAN_POINT('Ctrl Pts',(-22.3859455591042,12.3825157199122,
130.860070359518)) ;
#135429 = CARTESIAN_POINT('Ctrl Pts',(-22.283236535859,12.3357140444497,130.592990061673)) ;
#135430 = CARTESIAN_POINT('Ctrl Pts',(-22.1793293005588,12.3660679541908,
130.322564167356)) ;
#135431 = CARTESIAN_POINT('Ctrl Pts',(-22.0811143599576,12.4727573812884,
130.068868334442)) ;
#135432 = CARTESIAN_POINT('Ctrl Pts',(-21.995572717209,12.6471452986828,129.852067795218)) ;
#135433 = CARTESIAN_POINT('Ctrl Pts',(-21.9277324469771,12.8766362181276,
129.686942307119)) ;
#135434 = CARTESIAN_POINT('Ctrl Pts',(-21.88149427899,13.1457609561308,129.584999326918)) ;
#135435 = CARTESIAN_POINT('Ctrl Pts',(-21.8597035864534,13.436208516762,129.554631981768)) ;
#135436 = CARTESIAN_POINT('Ctrl Pts',(-21.8632848179525,13.7232902020091,
129.598101610311)) ;
#135437 = CARTESIAN_POINT('Ctrl Pts',(-21.8909607988816,13.9896012284326,
129.712029646671)) ;
#135438 = CARTESIAN_POINT('Ctrl Pts',(-21.9403194385609,14.2159296230216,
129.889382772798)) ;
#135439 = CARTESIAN_POINT('Ctrl Pts',(-22.0069084874016,14.3851342144556,
130.117025681466)) ;
#135440 = CARTESIAN_POINT('Ctrl Pts',(-22.0853055168022,14.4854516976048,
130.379173666988)) ;
#135441 = CARTESIAN_POINT('Ctrl Pts',(-22.1690106808166,14.5096986607512,
130.656773596937)) ;
#135442 = CARTESIAN_POINT('Ctrl Pts',(-22.2516547688815,14.4561737731647,
130.931357792915)) ;
#135443 = CARTESIAN_POINT('Ctrl Pts',(-22.3263675110369,14.3282785458503,
131.182786371531)) ;
#135444 = CARTESIAN_POINT('Ctrl Pts',(-22.3868479785871,14.1363003864466,
131.392508931439)) ;
#135445 = CARTESIAN_POINT('Ctrl Pts',(-22.4284860760948,13.8924839857025,
131.547317007501)) ;
#135446 = CARTESIAN_POINT('Ctrl Pts',(-22.44725520974,13.6154602436594,131.6352536123)) ;
#135447 = CARTESIAN_POINT('Ctrl Pts',(-22.4412045671012,13.3244466531158,
131.650714430567)) ;
#135448 = CARTESIAN_POINT('Ctrl Pts',(-22.4100202102661,13.0407282159145,
131.592726094803)) ;
#135449 = CARTESIAN_POINT('Ctrl Pts',(-22.3552546417009,12.7843965627726,
131.465846020052)) ;
#135450 = CARTESIAN_POINT('Ctrl Pts',(-22.2799328403175,12.5734338880589,
131.27897230653)) ;
#135451 = CARTESIAN_POINT('Ctrl Pts',(-22.1888584470267,12.4236459559127,
131.046058924602)) ;
#135452 = CARTESIAN_POINT('Ctrl Pts',(-22.0881362776665,12.3455712635568,
130.784862015627)) ;
#135453 = CARTESIAN_POINT('Ctrl Pts',(-21.9835492566618,12.3443023671055,
130.512500328341)) ;
#135454 = CARTESIAN_POINT('Ctrl Pts',(-21.8821100407858,12.420933178294,130.249388866071)) ;
#135455 = CARTESIAN_POINT('Ctrl Pts',(-21.7910702729597,12.5684896870098,
130.016446821888)) ;
#135456 = CARTESIAN_POINT('Ctrl Pts',(-21.7150620477299,12.7783872300958,
129.827643163685)) ;
#135457 = CARTESIAN_POINT('Ctrl Pts',(-21.6597355302853,13.0341435528073,
129.699158062916)) ;
#135458 = CARTESIAN_POINT('Ctrl Pts',(-21.6280379920894,13.3161552682329,
129.639527649233)) ;
#135459 = CARTESIAN_POINT('Ctrl Pts',(-21.6212166338096,13.6077102167408,
129.65278753406)) ;
#135460 = CARTESIAN_POINT('Ctrl Pts',(-21.6394813968357,13.8863966863271,
129.739379830896)) ;
#135461 = CARTESIAN_POINT('Ctrl Pts',(-21.6805482499846,14.1306963082603,
129.892451481926)) ;
#135462 = CARTESIAN_POINT('Ctrl Pts',(-21.7404897132441,14.3238933046915,
130.100547666824)) ;
#135463 = CARTESIAN_POINT('Ctrl Pts',(-21.8147710462659,14.4535137780173,
130.350663609957)) ;
#135464 = CARTESIAN_POINT('Ctrl Pts',(-21.8973774190617,14.5094099168095,
130.625175022534)) ;
#135465 = CARTESIAN_POINT('Ctrl Pts',(-21.9815416990517,14.4867701673882,
130.904282937535)) ;
#135466 = CARTESIAN_POINT('Ctrl Pts',(-22.0595736035611,14.3890643828725,
131.165115307558)) ;
#135467 = CARTESIAN_POINT('Ctrl Pts',(-22.1268562117523,14.2211869107964,
131.394908944864)) ;
#135468 = CARTESIAN_POINT('Ctrl Pts',(-22.1766796342833,13.9958858020985,
131.573633433779)) ;
#135469 = CARTESIAN_POINT('Ctrl Pts',(-22.2049451389284,13.7314793548645,
131.689162299244)) ;
#135470 = CARTESIAN_POINT('Ctrl Pts',(-22.2091882562906,13.4423639400344,
131.734833540967)) ;
#135471 = CARTESIAN_POINT('Ctrl Pts',(-22.187986226038,13.1530743203904,131.706032228928)) ;
#135472 = CARTESIAN_POINT('Ctrl Pts',(-22.1426951060036,12.8842566111771,
131.60670589681)) ;
#135473 = CARTESIAN_POINT('Ctrl Pts',(-22.0749780240027,12.6519995362001,
131.442148263088)) ;
#135474 = CARTESIAN_POINT('Ctrl Pts',(-21.9900041425516,12.4766942436469,
131.226917109559)) ;
#135475 = CARTESIAN_POINT('Ctrl Pts',(-21.8923871793902,12.3681120678918,
130.974864846892)) ;
#135476 = CARTESIAN_POINT('Ctrl Pts',(-21.787890239755,12.3353450096833,130.70292564467)) ;
#135477 = CARTESIAN_POINT('Ctrl Pts',(-21.6847703934588,12.3808789292608,
130.434751982444)) ;
#135478 = CARTESIAN_POINT('Ctrl Pts',(-21.5888638247786,12.5006496739186,
130.187651595634)) ;
#135479 = CARTESIAN_POINT('Ctrl Pts',(-21.5062882918341,12.6862348924807,
129.979488344586)) ;
#135480 = CARTESIAN_POINT('Ctrl Pts',(-21.4420352783819,12.9253055289241,
129.824962379676)) ;
#135481 = CARTESIAN_POINT('Ctrl Pts',(-21.4003702869002,13.1996774467986,
129.7363633676)) ;
#135482 = CARTESIAN_POINT('Ctrl Pts',(-21.3833560025974,13.4900583198245,
129.719780265193)) ;
#135483 = CARTESIAN_POINT('Ctrl Pts',(-21.3916055296796,13.7765694769724,
129.777104936438)) ;
#135484 = CARTESIAN_POINT('Ctrl Pts',(-21.4238225675142,14.036835662277,129.904358363752)) ;
#135485 = CARTESIAN_POINT('Ctrl Pts',(-21.4764867420294,14.2522894974628,
130.091167062838)) ;
#135486 = CARTESIAN_POINT('Ctrl Pts',(-21.5461349346789,14.410142650821,130.327932770345)) ;
#135487 = CARTESIAN_POINT('Ctrl Pts',(-21.6258533196047,14.4959011359271,
130.593837523055)) ;
#135488 = CARTESIAN_POINT('Ctrl Pts',(-21.7097706486653,14.5055615596735,
130.872034708298)) ;
#135489 = CARTESIAN_POINT('Ctrl Pts',(-21.7915115159255,14.4373879166647,
131.144023400965)) ;
#135490 = CARTESIAN_POINT('Ctrl Pts',(-21.8638380594977,14.2968056087925,
131.388393161352)) ;
#135491 = CARTESIAN_POINT('Ctrl Pts',(-21.9212551892473,14.0934340145334,
131.589268391717)) ;
#135492 = CARTESIAN_POINT('Ctrl Pts',(-21.9586969314941,13.8423638114029,
131.731737544598)) ;
#135493 = CARTESIAN_POINT('Ctrl Pts',(-21.9729463381941,13.5615577206812,
131.806433890657)) ;
#135494 = CARTESIAN_POINT('Ctrl Pts',(-21.9620894874447,13.2694348944804,
131.807950532534)) ;
#135495 = CARTESIAN_POINT('Ctrl Pts',(-21.9263140164209,12.9897647818979,
131.73650343455)) ;
#135496 = CARTESIAN_POINT('Ctrl Pts',(-21.8673223314263,12.7403852471457,
131.597325259585)) ;
#135497 = CARTESIAN_POINT('Ctrl Pts',(-21.7886865523693,12.5401778472151,
131.400734212814)) ;
#135498 = CARTESIAN_POINT('Ctrl Pts',(-21.6953778525397,12.4032538731495,
131.161259541037)) ;
#135499 = CARTESIAN_POINT('Ctrl Pts',(-21.5932072064287,12.3392654765734,
130.895922348931)) ;
#135500 = CARTESIAN_POINT('Ctrl Pts',(-21.4887973419696,12.3529795705707,
130.624055509138)) ;
#135501 = CARTESIAN_POINT('Ctrl Pts',(-21.3889895957889,12.44341496887,130.365620015526)) ;
#135502 = CARTESIAN_POINT('Ctrl Pts',(-21.3002278613015,12.6038142404483,
130.13942068693)) ;
#135503 = CARTESIAN_POINT('Ctrl Pts',(-21.2279512253468,12.8232746698558,
129.96143747852)) ;
#135504 = CARTESIAN_POINT('Ctrl Pts',(-21.1769064226059,13.0848674095602,
129.845368695489)) ;
#135505 = CARTESIAN_POINT('Ctrl Pts',(-21.149658170467,13.3712340427374,129.798893618011)) ;
#135506 = CARTESIAN_POINT('Ctrl Pts',(-21.1476946959762,13.6620670155129,
129.826365855313)) ;
#135507 = CARTESIAN_POINT('Ctrl Pts',(-21.1703666330339,13.9347879219274,
129.92569032549)) ;
#135508 = CARTESIAN_POINT('Ctrl Pts',(-21.2152993770454,14.1711547034761,
130.090075797328)) ;
#135509 = CARTESIAN_POINT('Ctrl Pts',(-21.2785796529392,14.3538985958079,
130.308060225528)) ;
#135510 = CARTESIAN_POINT('Ctrl Pts',(-21.3548663994536,14.4699515410886,
130.564015298951)) ;
#135511 = CARTESIAN_POINT('Ctrl Pts',(-21.4380889896721,14.511011729743,130.840261217569)) ;
#135512 = CARTESIAN_POINT('Ctrl Pts',(-21.5213196238039,14.4745400421894,
131.116445883889)) ;
#135513 = CARTESIAN_POINT('Ctrl Pts',(-21.5987228795245,14.3614974996119,
131.37591886424)) ;
#135514 = CARTESIAN_POINT('Ctrl Pts',(-21.6624280158677,14.1829580277845,
131.594943503888)) ;
#135515 = CARTESIAN_POINT('Ctrl Pts',(-21.7085901232024,13.9492404929465,
131.762934960253)) ;
#135516 = CARTESIAN_POINT('Ctrl Pts',(-21.7325457579653,13.6775800982586,
131.866060493852)) ;
#135517 = CARTESIAN_POINT('Ctrl Pts',(-21.7320824211323,13.3886494635436,
131.897743516193)) ;
#135518 = CARTESIAN_POINT('Ctrl Pts',(-21.7060357693068,13.0993478015478,
131.855033735375)) ;
#135519 = CARTESIAN_POINT('Ctrl Pts',(-21.6563720516456,12.8369458310676,
131.74287352401)) ;
#135520 = CARTESIAN_POINT('Ctrl Pts',(-21.5849505607058,12.6140529768099,
131.567486815159)) ;
#135521 = CARTESIAN_POINT('Ctrl Pts',(-21.4972346922135,12.4507323341902,
131.344230579028)) ;
#135522 = CARTESIAN_POINT('Ctrl Pts',(-21.3977816403119,12.3558899306528,
131.086868664739)) ;
#135523 = CARTESIAN_POINT('Ctrl Pts',(-21.2931236526698,12.3380969081111,
130.814378116707)) ;
#135524 = CARTESIAN_POINT('Ctrl Pts',(-21.1912351475806,12.3976016694818,
130.549680132567)) ;
#135525 = CARTESIAN_POINT('Ctrl Pts',(-21.0970918464179,12.530583824708,130.307814407326)) ;
#135526 = CARTESIAN_POINT('Ctrl Pts',(-21.0173249384038,12.7283490506027,
130.108013541003)) ;
#135527 = CARTESIAN_POINT('Ctrl Pts',(-20.9573893511929,12.9742771227128,
129.965922835233)) ;
#135528 = CARTESIAN_POINT('Ctrl Pts',(-20.9200880297606,13.2539376227601,
129.890167219948)) ;
#135529 = CARTESIAN_POINT('Ctrl Pts',(-20.907889243952,13.5450903335013,129.887655062896)) ;
#135530 = CARTESIAN_POINT('Ctrl Pts',(-20.920784302057,13.8275787514848,129.958467916581)) ;
#135531 = CARTESIAN_POINT('Ctrl Pts',(-20.9569782930972,14.080619519853,130.097260030665)) ;
#135532 = CARTESIAN_POINT('Ctrl Pts',(-21.0136849887986,14.2877392133105,
130.296196899106)) ;
#135533 = CARTESIAN_POINT('Ctrl Pts',(-21.0849841102122,14.431213841156,130.537392435781)) ;
#135534 = CARTESIAN_POINT('Ctrl Pts',(-21.1665056814218,14.5038738166411,
130.808799012005)) ;
#135535 = CARTESIAN_POINT('Ctrl Pts',(-21.2505166479721,14.4984557576167,
131.087288159437)) ;
#135536 = CARTESIAN_POINT('Ctrl Pts',(-21.3308085825838,14.4164646825051,
131.354946228948)) ;
#135537 = CARTESIAN_POINT('Ctrl Pts',(-21.4010755566249,14.2622140461571,
131.593482336718)) ;
#135538 = CARTESIAN_POINT('Ctrl Pts',(-21.4547420541191,14.0497489487789,
131.7832014722)) ;
#135539 = CARTESIAN_POINT('Ctrl Pts',(-21.4881853748102,13.7905258352839,
131.91413728601)) ;
#135540 = CARTESIAN_POINT('Ctrl Pts',(-21.4977462696728,13.506486494377,131.975100243164)) ;
#135541 = CARTESIAN_POINT('Ctrl Pts',(-21.4819835887124,13.2142515667239,
131.96236180773)) ;
#135542 = CARTESIAN_POINT('Ctrl Pts',(-21.4419223606185,12.9406232851689,
131.878185903014)) ;
#135543 = CARTESIAN_POINT('Ctrl Pts',(-21.3786934156362,12.6982138740687,
131.726763051586)) ;
#135544 = CARTESIAN_POINT('Ctrl Pts',(-21.2972126241658,12.5096112048297,
131.521723412285)) ;
#135545 = CARTESIAN_POINT('Ctrl Pts',(-21.2011850848722,12.3850648620669,
131.274514023005)) ;
#135546 = CARTESIAN_POINT('Ctrl Pts',(-21.0984907761846,12.3359713268051,
131.007507556083)) ;
#135547 = CARTESIAN_POINT('Ctrl Pts',(-20.9944877940312,12.3641515700291,
130.736812488399)) ;
#135548 = CARTESIAN_POINT('Ctrl Pts',(-20.8961804382662,12.4683944776065,
130.482779938443)) ;
#135549 = CARTESIAN_POINT('Ctrl Pts',(-20.8099546373725,12.6414744910879,
130.264081389746)) ;
#135550 = CARTESIAN_POINT('Ctrl Pts',(-20.7415876002801,12.8692739707259,
130.097372977444)) ;
#135551 = CARTESIAN_POINT('Ctrl Pts',(-20.6945289877427,13.1394382839076,
129.993253900407)) ;
#135552 = CARTESIAN_POINT('Ctrl Pts',(-20.672298328365,13.4257125423889,129.961149556797)) ;
#135553 = CARTESIAN_POINT('Ctrl Pts',(-20.6750007501078,13.7153678926771,
130.002310555712)) ;
#135554 = CARTESIAN_POINT('Ctrl Pts',(-20.7020667565521,13.9823826092166,
130.114434508231)) ;
#135555 = CARTESIAN_POINT('Ctrl Pts',(-20.7509060316579,14.210351268189,130.290309073817)) ;
#135556 = CARTESIAN_POINT('Ctrl Pts',(-20.8169604036749,14.3810373513132,
130.516327937223)) ;
#135557 = CARTESIAN_POINT('Ctrl Pts',(-20.8950665489886,14.4835203874639,
130.777619160747)) ;
#135558 = CARTESIAN_POINT('Ctrl Pts',(-20.9787343216663,14.5102051470099,
131.055116750985)) ;
#135559 = CARTESIAN_POINT('Ctrl Pts',(-21.0618484768981,14.4584272467564,
131.331220006128)) ;
#135560 = CARTESIAN_POINT('Ctrl Pts',(-21.1364526301434,14.3332271538461,
131.582140708526)) ;
#135561 = CARTESIAN_POINT('Ctrl Pts',(-21.1976622623504,14.1422679027751,
131.794126036847)) ;
#135562 = CARTESIAN_POINT('Ctrl Pts',(-21.23975721544,13.9003526545792,131.950166196499)) ;
#135563 = CARTESIAN_POINT('Ctrl Pts',(-21.2592791168289,13.6237176044633,
132.040346931511)) ;
#135564 = CARTESIAN_POINT('Ctrl Pts',(-21.2539545891703,13.3329588361478,
132.057910063551)) ;
#135565 = CARTESIAN_POINT('Ctrl Pts',(-21.2234510913761,13.0482791472687,
132.00196258976)) ;
#135566 = CARTESIAN_POINT('Ctrl Pts',(-21.1691539099102,12.7905984211716,
131.876506766355)) ;
#135567 = CARTESIAN_POINT('Ctrl Pts',(-21.0947340593749,12.5792074314873,
131.692098693563)) ;
#135568 = CARTESIAN_POINT('Ctrl Pts',(-21.0040480835755,12.4271420328258,
131.460337471105)) ;
#135569 = CARTESIAN_POINT('Ctrl Pts',(-20.9032486407606,12.3466854620337,
131.199002527252)) ;
#135570 = CARTESIAN_POINT('Ctrl Pts',(-20.7987770579087,12.3433384451733,
130.926945640301)) ;
#135571 = CARTESIAN_POINT('Ctrl Pts',(-20.6974847568586,12.417256873973,130.664144724903)) ;
#135572 = CARTESIAN_POINT('Ctrl Pts',(-20.6057021506296,12.5633304568432,
130.429162568903)) ;
#135573 = CARTESIAN_POINT('Ctrl Pts',(-20.5294560018403,12.7708593905581,
130.239538039818)) ;
#135574 = CARTESIAN_POINT('Ctrl Pts',(-20.4733463103174,13.025326349885,130.108769986711)) ;
#135575 = CARTESIAN_POINT('Ctrl Pts',(-20.4407772110818,13.3082178025067,
130.046756066484)) ;
#135576 = CARTESIAN_POINT('Ctrl Pts',(-20.4333100328866,13.5990344955289,
130.058039052296)) ;
#135577 = CARTESIAN_POINT('Ctrl Pts',(-20.4506880067864,13.8774216043795,
130.141913702905)) ;
#135578 = CARTESIAN_POINT('Ctrl Pts',(-20.4911818153333,14.1239848990119,
130.293425636597)) ;
#135579 = CARTESIAN_POINT('Ctrl Pts',(-20.5507855806424,14.3192776170792,
130.500609692184)) ;
#135580 = CARTESIAN_POINT('Ctrl Pts',(-20.6247405377758,14.4507732360595,
130.749766053951)) ;
#135581 = CARTESIAN_POINT('Ctrl Pts',(-20.7069579624013,14.5087792678555,
131.023045402965)) ;
#135582 = CARTESIAN_POINT('Ctrl Pts',(-20.7911628034135,14.4887238336712,
131.302264434157)) ;
#135583 = CARTESIAN_POINT('Ctrl Pts',(-20.8697693366433,14.3928285084541,
131.564906273796)) ;
#135584 = CARTESIAN_POINT('Ctrl Pts',(-20.9374577677181,14.2263682040696,
131.795916170133)) ;
#135585 = CARTESIAN_POINT('Ctrl Pts',(-20.9876137387477,14.0038696460673,
131.975425509327)) ;
#135586 = CARTESIAN_POINT('Ctrl Pts',(-21.0167121922335,13.7389372008462,
132.093575454873)) ;
#135587 = CARTESIAN_POINT('Ctrl Pts',(-21.021624803058,13.4518073715824,132.141010517718)) ;
#135588 = CARTESIAN_POINT('Ctrl Pts',(-21.001265184062,13.1616327439453,132.114737089628)) ;
#135589 = CARTESIAN_POINT('Ctrl Pts',(-20.9563235153239,12.8906304372966,
132.016607385205)) ;
#135590 = CARTESIAN_POINT('Ctrl Pts',(-20.8895478488704,12.6585325321797,
131.854601473478)) ;
#135591 = CARTESIAN_POINT('Ctrl Pts',(-20.8050290649649,12.4808578746759,
131.640730446969)) ;
#135592 = CARTESIAN_POINT('Ctrl Pts',(-20.706854482996,12.369794968941,131.387313297938)) ;
#135593 = CARTESIAN_POINT('Ctrl Pts',(-20.6035841518815,12.3353140243209,
131.118587941619)) ;
#135594 = CARTESIAN_POINT('Ctrl Pts',(-20.4999425243112,12.3783402005982,
130.849020652898)) ;
#135595 = CARTESIAN_POINT('Ctrl Pts',(-20.4037610912831,12.4961137906607,
130.601107675479)) ;
#135596 = CARTESIAN_POINT('Ctrl Pts',(-20.3206161817449,12.6800956082709,
130.391318319672)) ;
#135597 = CARTESIAN_POINT('Ctrl Pts',(-20.2557578107062,12.9180877152906,
130.235043956869)) ;
#135598 = CARTESIAN_POINT('Ctrl Pts',(-20.2134909793572,13.1911275173993,
130.144619104063)) ;
#135599 = CARTESIAN_POINT('Ctrl Pts',(-20.1956945315034,13.4815072415882,
130.125770538085)) ;
#135600 = CARTESIAN_POINT('Ctrl Pts',(-20.2032544219231,13.7684314308885,
130.181084199128)) ;
#135601 = CARTESIAN_POINT('Ctrl Pts',(-20.2346242895992,14.029076308477,130.305758033525)) ;
#135602 = CARTESIAN_POINT('Ctrl Pts',(-20.2871102678795,14.2473093926041,
130.492262967075)) ;
#135603 = CARTESIAN_POINT('Ctrl Pts',(-20.3557014691764,14.4057091519906,
130.725627737145)) ;
#135604 = CARTESIAN_POINT('Ctrl Pts',(-20.4356832288713,14.4946178708306,
130.992528144001)) ;
#135605 = CARTESIAN_POINT('Ctrl Pts',(-20.5195606513706,14.5063975208026,
131.270592829057)) ;
#135606 = CARTESIAN_POINT('Ctrl Pts',(-20.601669735203,14.4401278585609,131.543748083559)) ;
#135607 = CARTESIAN_POINT('Ctrl Pts',(-20.6740334559909,14.3020001323071,
131.788087967881)) ;
#135608 = CARTESIAN_POINT('Ctrl Pts',(-20.7320052756849,14.100380875427,131.990589852135)) ;
#135609 = CARTESIAN_POINT('Ctrl Pts',(-20.7701334334659,13.8504602239821,
132.135070902885)) ;
#135610 = CARTESIAN_POINT('Ctrl Pts',(-20.7851220054825,13.5690360496352,
132.212066464694)) ;
#135611 = CARTESIAN_POINT('Ctrl Pts',(-20.7749067351906,13.277347744237,132.215406858043)) ;
#135612 = CARTESIAN_POINT('Ctrl Pts',(-20.739950771466,12.9978265767653,132.146263744771)) ;
#135613 = CARTESIAN_POINT('Ctrl Pts',(-20.6815482067024,12.747023860199,132.008839074771)) ;
#135614 = CARTESIAN_POINT('Ctrl Pts',(-20.6035221230103,12.5453431667421,
131.813989900865)) ;
#135615 = CARTESIAN_POINT('Ctrl Pts',(-20.5104128505178,12.4062333259034,
131.575152883014)) ;
#135616 = CARTESIAN_POINT('Ctrl Pts',(-20.4087091658857,12.3400677949455,
131.311081123435)) ;
#135617 = CARTESIAN_POINT('Ctrl Pts',(-20.303791085454,12.3515722965719,131.037884994155)) ;
#135618 = CARTESIAN_POINT('Ctrl Pts',(-20.2041191745575,12.4396025465946,
130.779723997866)) ;
#135619 = CARTESIAN_POINT('Ctrl Pts',(-20.1147712529316,12.5983879462257,
130.551883797315)) ;
#135620 = CARTESIAN_POINT('Ctrl Pts',(-20.0421585923302,12.8155081778463,
130.372801469089)) ;
#135621 = CARTESIAN_POINT('Ctrl Pts',(-19.9900861703505,13.0777480891852,
130.253944896754)) ;
#135622 = CARTESIAN_POINT('Ctrl Pts',(-19.9622906553043,13.3640007134148,
130.205892912972)) ;
#135623 = CARTESIAN_POINT('Ctrl Pts',(-19.9596040305283,13.6530970190172,
130.231033720601)) ;
#135624 = CARTESIAN_POINT('Ctrl Pts',(-19.9815947583038,13.9274410550996,
130.328465672942)) ;
#135625 = CARTESIAN_POINT('Ctrl Pts',(-20.0259169621657,14.1649405448642,
130.491043143204)) ;
#135626 = CARTESIAN_POINT('Ctrl Pts',(-20.0889049637749,14.3499176915205,
130.708260928926)) ;
#135627 = CARTESIAN_POINT('Ctrl Pts',(-20.1649263048442,14.4676736740884,
130.963435819328)) ;
#135628 = CARTESIAN_POINT('Ctrl Pts',(-20.247688472556,14.5109849198275,131.238193829716)) ;
#135629 = CARTESIAN_POINT('Ctrl Pts',(-20.331483197017,14.4763368011369,131.516227084564)) ;
#135630 = CARTESIAN_POINT('Ctrl Pts',(-20.4085145537121,14.3664425274482,
131.774319022009)) ;
#135631 = CARTESIAN_POINT('Ctrl Pts',(-20.4732700628347,14.1882602546085,
131.996710354005)) ;
#135632 = CARTESIAN_POINT('Ctrl Pts',(-20.5197600667737,13.9563928712726,
132.165546655575)) ;
#135633 = CARTESIAN_POINT('Ctrl Pts',(-20.544429934519,13.6856075071528,132.270760904427)) ;
#135634 = CARTESIAN_POINT('Ctrl Pts',(-20.5446218153691,13.3967978155194,
132.304370094684)) ;
#135635 = CARTESIAN_POINT('Ctrl Pts',(-20.5194831662747,13.1083772147109,
132.264162983921)) ;
#135636 = CARTESIAN_POINT('Ctrl Pts',(-20.4702619913672,12.8436201216384,
132.15346806604)) ;
#135637 = CARTESIAN_POINT('Ctrl Pts',(-20.3994698940617,12.6197329650473,
131.979865314557)) ;
#135638 = CARTESIAN_POINT('Ctrl Pts',(-20.3120006020497,12.4541610182818,
131.75739537006)) ;
#135639 = CARTESIAN_POINT('Ctrl Pts',(-20.2125860830344,12.3575181073951,
131.500199627294)) ;
#135640 = CARTESIAN_POINT('Ctrl Pts',(-20.1088815096965,12.337407534574,131.230203979974)) ;
#135641 = CARTESIAN_POINT('Ctrl Pts',(-20.0060146641454,12.3950240477661,
130.962919259217)) ;
#135642 = CARTESIAN_POINT('Ctrl Pts',(-19.9119864658295,12.5255974682326,
130.721236187127)) ;
#135643 = CARTESIAN_POINT('Ctrl Pts',(-19.8314897395286,12.7221236513144,
130.519397456966)) ;
#135644 = CARTESIAN_POINT('Ctrl Pts',(-19.7710089279874,12.966643820031,130.375676004731)) ;
#135645 = CARTESIAN_POINT('Ctrl Pts',(-19.732928013481,13.2467842966359,130.297774420096)) ;
#135646 = CARTESIAN_POINT('Ctrl Pts',(-19.7201400299444,13.5364084867458,
130.293371523372)) ;
#135647 = CARTESIAN_POINT('Ctrl Pts',(-19.7322324408918,13.819301352246,130.361818332685)) ;
#135648 = CARTESIAN_POINT('Ctrl Pts',(-19.7678249009645,14.0737430594077,
130.498891515294)) ;
#135649 = CARTESIAN_POINT('Ctrl Pts',(-19.8239107737393,14.2823383256047,
130.695974069195)) ;
#135650 = CARTESIAN_POINT('Ctrl Pts',(-19.8950604586474,14.4280819786068,
130.936830915041)) ;
#135651 = CARTESIAN_POINT('Ctrl Pts',(-19.9759986631136,14.5027907188546,
131.20637093887)) ;
#135652 = CARTESIAN_POINT('Ctrl Pts',(-20.0606762821136,14.4996009182714,
131.487070199978)) ;
#135653 = CARTESIAN_POINT('Ctrl Pts',(-20.1407098011001,14.4198435135005,
131.753794032065)) ;
#135654 = CARTESIAN_POINT('Ctrl Pts',(-20.2112630859601,14.2682255575811,
131.993092362855)) ;
#135655 = CARTESIAN_POINT('Ctrl Pts',(-20.2656775957736,14.0566692320112,
132.185107721384)) ;
#135656 = CARTESIAN_POINT('Ctrl Pts',(-20.2997748055791,13.7984046917339,
132.317960439349)) ;
#135657 = CARTESIAN_POINT('Ctrl Pts',(-20.3099989318143,13.5146255183712,
132.38088711118)) ;
#135658 = CARTESIAN_POINT('Ctrl Pts',(-20.2951296394703,13.22379017507,132.370580468596)) ;
#135659 = CARTESIAN_POINT('Ctrl Pts',(-20.2555701663945,12.9476430099182,
132.288081447981)) ;
#135660 = CARTESIAN_POINT('Ctrl Pts',(-20.1928769291611,12.7041858709694,
132.138213583783)) ;
#135661 = CARTESIAN_POINT('Ctrl Pts',(-20.1120002752265,12.5142908380612,
131.934883468866)) ;
#135662 = CARTESIAN_POINT('Ctrl Pts',(-20.0165096996154,12.3877724329813,
131.689173717466)) ;
#135663 = CARTESIAN_POINT('Ctrl Pts',(-19.913478604829,12.3361912043238,131.421332336646)) ;
#135664 = CARTESIAN_POINT('Ctrl Pts',(-19.8094708653727,12.3624798224069,
131.150606824843)) ;
#135665 = CARTESIAN_POINT('Ctrl Pts',(-19.7113062006748,12.4640688022784,
130.896852899496)) ;
#135666 = CARTESIAN_POINT('Ctrl Pts',(-19.6243191332476,12.6358046245907,
130.676044087363)) ;
#135667 = CARTESIAN_POINT('Ctrl Pts',(-19.5555745074161,12.862048858162,130.508185639822)) ;
#135668 = CARTESIAN_POINT('Ctrl Pts',(-19.5079382213539,13.1294243703739,
130.402168639634)) ;
#135669 = CARTESIAN_POINT('Ctrl Pts',(-19.4847311841948,13.419127554444,130.367646107838)) ;
#135670 = CARTESIAN_POINT('Ctrl Pts',(-19.486760537507,13.7060585256719,130.406486755971)) ;
#135671 = CARTESIAN_POINT('Ctrl Pts',(-19.5132448910941,13.9758635071568,
130.517143788552)) ;
#135672 = CARTESIAN_POINT('Ctrl Pts',(-19.561461527867,14.2044690811379,130.691105042514)) ;
#135673 = CARTESIAN_POINT('Ctrl Pts',(-19.6271525262166,14.3772046466544,
130.916107336043)) ;
#135674 = CARTESIAN_POINT('Ctrl Pts',(-19.7049913038784,14.4817041640368,
131.17660395042)) ;
#135675 = CARTESIAN_POINT('Ctrl Pts',(-19.7886768197028,14.5103977605507,
131.454191387136)) ;
#135676 = CARTESIAN_POINT('Ctrl Pts',(-19.8713625246764,14.461387716176,131.728812616932)) ;
#135677 = CARTESIAN_POINT('Ctrl Pts',(-19.9466960883751,14.3378670523305,
131.982034797292)) ;
#135678 = CARTESIAN_POINT('Ctrl Pts',(-20.0083045176645,14.1487649480966,
132.195144873615)) ;
#135679 = CARTESIAN_POINT('Ctrl Pts',(-20.0510942154457,13.9077124472436,
132.35327591803)) ;
#135680 = CARTESIAN_POINT('Ctrl Pts',(-20.0712746305926,13.6318349091011,
132.445369268278)) ;
#135681 = CARTESIAN_POINT('Ctrl Pts',(-20.0666628175852,13.3411961915081,
132.465016541542)) ;
#135682 = CARTESIAN_POINT('Ctrl Pts',(-20.0369065317575,13.0563347009616,
132.411215549619)) ;
#135683 = CARTESIAN_POINT('Ctrl Pts',(-19.9832697572704,12.7976622253545,
132.287685663652)) ;
#135684 = CARTESIAN_POINT('Ctrl Pts',(-19.909474160919,12.584625305209,132.105083184337)) ;
#135685 = CARTESIAN_POINT('Ctrl Pts',(-19.8184221729735,12.429833286881,131.872506784025)) ;
#135686 = CARTESIAN_POINT('Ctrl Pts',(-19.7187303437125,12.3481748757021,
131.614098966012)) ;
#135687 = CARTESIAN_POINT('Ctrl Pts',(-19.6138632113487,12.3422836205948,
131.341022208364)) ;
#135688 = CARTESIAN_POINT('Ctrl Pts',(-19.5124594677726,12.414162317258,131.077872115915)) ;
#135689 = CARTESIAN_POINT('Ctrl Pts',(-19.420212188348,12.55849168118,130.841573794732)) ;
#135690 = CARTESIAN_POINT('Ctrl Pts',(-19.3435324232807,12.7644624942609,
130.65066449742)) ;
#135691 = CARTESIAN_POINT('Ctrl Pts',(-19.2868798087134,13.0174115077838,
130.518256914751)) ;
#135692 = CARTESIAN_POINT('Ctrl Pts',(-19.2535766304538,13.2998964348547,
130.454116409847)) ;
#135693 = CARTESIAN_POINT('Ctrl Pts',(-19.2453729976278,13.5908799629275,
130.463258994527)) ;
#135694 = CARTESIAN_POINT('Ctrl Pts',(-19.2621513468008,13.8706960081611,
130.545479006086)) ;
#135695 = CARTESIAN_POINT('Ctrl Pts',(-19.3020872042403,14.1180202656557,
130.695329004107)) ;
#135696 = CARTESIAN_POINT('Ctrl Pts',(-19.3610103361281,14.3143765894564,
130.900421785235)) ;
#135697 = CARTESIAN_POINT('Ctrl Pts',(-19.434812974818,14.4481660809184,131.149213001408)) ;
#135698 = CARTESIAN_POINT('Ctrl Pts',(-19.5166794707772,14.5080838606745,
131.421381896559)) ;
#135699 = CARTESIAN_POINT('Ctrl Pts',(-19.6008596180551,14.4905518531177,
131.700498217892)) ;
#135700 = CARTESIAN_POINT('Ctrl Pts',(-19.679959110775,14.3964092296967,131.964690313878)) ;
#135701 = CARTESIAN_POINT('Ctrl Pts',(-19.7478273039877,14.232304987228,132.196115316038)) ;
#135702 = CARTESIAN_POINT('Ctrl Pts',(-19.7986192880396,14.0113006854444,
132.37749892765)) ;
#135703 = CARTESIAN_POINT('Ctrl Pts',(-19.8284139029138,13.7469853282518,
132.497724021509)) ;
#135704 = CARTESIAN_POINT('Ctrl Pts',(-19.8340820683678,13.4601451324146,
132.547372256783)) ;
#135705 = CARTESIAN_POINT('Ctrl Pts',(-19.8142531422841,13.1687003200991,
132.522778212001)) ;
#135706 = CARTESIAN_POINT('Ctrl Pts',(-19.7703730343976,12.8989650919222,
132.427483609972)) ;
#135707 = CARTESIAN_POINT('Ctrl Pts',(-19.7036589079187,12.6635916504989,
132.265932090456)) ;
#135708 = CARTESIAN_POINT('Ctrl Pts',(-19.6199118535932,12.485239800862,132.054155238019)) ;
#135709 = CARTESIAN_POINT('Ctrl Pts',(-19.5219805853211,12.3719259500599,
131.801473410491)) ;
#135710 = CARTESIAN_POINT('Ctrl Pts',(-19.4189379680128,12.3351771032852,
131.53336398971)) ;
#135711 = CARTESIAN_POINT('Ctrl Pts',(-19.3148770024859,12.3762351050997,
131.26268009039)) ;
#135712 = CARTESIAN_POINT('Ctrl Pts',(-19.2189066435572,12.4911992435135,
131.01519951472)) ;
#135713 = CARTESIAN_POINT('Ctrl Pts',(-19.1347439547889,12.6745749260732,
130.802658266804)) ;
#135714 = CARTESIAN_POINT('Ctrl Pts',(-19.0695712650756,12.9105841176317,
130.64534787781)) ;
#135715 = CARTESIAN_POINT('Ctrl Pts',(-19.026516615279,13.1834575472762,130.552699546602)) ;
#135716 = CARTESIAN_POINT('Ctrl Pts',(-19.0081217007437,13.4728172007292,
130.532007746554)) ;
#135717 = CARTESIAN_POINT('Ctrl Pts',(-19.0147866964172,13.7593252111675,
130.584597145698)) ;
#135718 = CARTESIAN_POINT('Ctrl Pts',(-19.0457740324292,14.0229111380707,
130.708413150787)) ;
#135719 = CARTESIAN_POINT('Ctrl Pts',(-19.0973111190571,14.2409568530166,
130.891883602161)) ;
#135720 = CARTESIAN_POINT('Ctrl Pts',(-19.165926552844,14.4024702596202,131.125549278518)) ;
#135721 = CARTESIAN_POINT('Ctrl Pts',(-19.2454507888212,14.4930252918819,
131.390998297428)) ;
#135722 = CARTESIAN_POINT('Ctrl Pts',(-19.3293410740711,14.5071138077779,
131.669126207063)) ;
#135723 = CARTESIAN_POINT('Ctrl Pts',(-19.4112821511384,14.4434722304718,
131.941650206842)) ;
#135724 = CARTESIAN_POINT('Ctrl Pts',(-19.4842739640058,14.3072991508372,
132.187922760495)) ;
#135725 = CARTESIAN_POINT('Ctrl Pts',(-19.5429829781195,14.1061281755834,
132.392741540416)) ;
#135726 = CARTESIAN_POINT('Ctrl Pts',(-19.5814898983426,13.8584458365122,
132.538171297678)) ;
#135727 = CARTESIAN_POINT('Ctrl Pts',(-19.5972452937213,13.5782527615593,
132.617345758941)) ;
#135728 = CARTESIAN_POINT('Ctrl Pts',(-19.587821553024,13.2862405830432,132.623036030091)) ;
#135729 = CARTESIAN_POINT('Ctrl Pts',(-19.5535345414538,13.0054673407222,
132.55591759128)) ;
#135730 = CARTESIAN_POINT('Ctrl Pts',(-19.4954706738399,12.7527978446706,
132.419600001604)) ;
#135731 = CARTESIAN_POINT('Ctrl Pts',(-19.4183727349997,12.5507722085017,
132.227270319449)) ;
#135732 = CARTESIAN_POINT('Ctrl Pts',(-19.3255707730553,12.4092693590586,
131.989364894937)) ;
#135733 = CARTESIAN_POINT('Ctrl Pts',(-19.2238321783356,12.3409406073707,
131.725254513543)) ;
#135734 = CARTESIAN_POINT('Ctrl Pts',(-19.119236753858,12.3499819194409,131.452886617979)) ;
#135735 = CARTESIAN_POINT('Ctrl Pts',(-19.0188367516298,12.4363532158425,
131.192772449436)) ;
#135736 = CARTESIAN_POINT('Ctrl Pts',(-18.9295447538629,12.5925663631045,
130.964931579883)) ;
#135737 = CARTESIAN_POINT('Ctrl Pts',(-18.85618070133,12.8085170384963,130.783729205798)) ;
#135738 = CARTESIAN_POINT('Ctrl Pts',(-18.8035406576781,13.0694866152918,
130.663175810496)) ;
#135739 = CARTESIAN_POINT('Ctrl Pts',(-18.774944483164,13.3550371201656,130.612758020313)) ;
#135740 = CARTESIAN_POINT('Ctrl Pts',(-18.7715872372659,13.6462143005165,
130.636161963138)) ;
#135741 = CARTESIAN_POINT('Ctrl Pts',(-18.7928313609646,13.9195287631536,
130.73120381732)) ;
#135742 = CARTESIAN_POINT('Ctrl Pts',(-18.8365269344384,14.1586150899391,
130.891977988719)) ;
#135743 = CARTESIAN_POINT('Ctrl Pts',(-18.8989146423201,14.3449689837057,
131.10737481057)) ;
#135744 = CARTESIAN_POINT('Ctrl Pts',(-18.9745793166611,14.465239738532,131.36150472704)) ;
#135745 = CARTESIAN_POINT('Ctrl Pts',(-19.0578793507872,14.5107689866746,
131.638093119859)) ;
#135746 = CARTESIAN_POINT('Ctrl Pts',(-19.1409583613005,14.4787461978325,
131.913707901465)) ;
#135747 = CARTESIAN_POINT('Ctrl Pts',(-19.2189706552468,14.3700644324197,
132.17497387013)) ;
#135748 = CARTESIAN_POINT('Ctrl Pts',(-19.2836848317943,14.1946408166751,
132.397013538057)) ;
#135749 = CARTESIAN_POINT('Ctrl Pts',(-19.3309065027156,13.963907732595,132.568053904224)) ;
#135750 = CARTESIAN_POINT('Ctrl Pts',(-19.3562835215805,13.6940409321305,
132.675319682935)) ;
#135751 = CARTESIAN_POINT('Ctrl Pts',(-19.3571223286895,13.4043243937501,
132.710955989412)) ;
#135752 = CARTESIAN_POINT('Ctrl Pts',(-19.3329129352278,13.1175424358185,
132.673226068229)) ;
#135753 = CARTESIAN_POINT('Ctrl Pts',(-19.284075134649,12.8501254079525,132.563869228407)) ;
#135754 = CARTESIAN_POINT('Ctrl Pts',(-19.2141838640519,12.6260375389968,
132.392718948333)) ;
#135755 = CARTESIAN_POINT('Ctrl Pts',(-19.1270338823226,12.4581545252769,
132.171242119684)) ;
#135756 = CARTESIAN_POINT('Ctrl Pts',(-19.0280972219191,12.3594525497003,
131.915366042047)) ;
#135757 = CARTESIAN_POINT('Ctrl Pts',(-18.9241027514417,12.3367944069397,
131.644635976731)) ;
#135758 = CARTESIAN_POINT('Ctrl Pts',(-18.8208265565642,12.3925085409291,
131.376240849143)) ;
#135759 = CARTESIAN_POINT('Ctrl Pts',(-18.7265133411892,12.5213898755188,
131.133731510503)) ;
#135760 = CARTESIAN_POINT('Ctrl Pts',(-18.6457952560714,12.7155724021421,
130.931131518529)) ;
#135761 = CARTESIAN_POINT('Ctrl Pts',(-18.5846065804363,12.9595220676015,
130.785423050799)) ;
#135762 = CARTESIAN_POINT('Ctrl Pts',(-18.546066469657,13.2367788940881,130.70592009773)) ;
#135763 = CARTESIAN_POINT('Ctrl Pts',(-18.5323213213029,13.5277643625836,
130.698889739784)) ;
#135764 = CARTESIAN_POINT('Ctrl Pts',(-18.543793348028,13.8120453761231,130.765623615628)) ;
#135765 = CARTESIAN_POINT('Ctrl Pts',(-18.5788549474306,14.0676654739834,
130.901176319765)) ;
#135766 = CARTESIAN_POINT('Ctrl Pts',(-18.6343035780449,14.2771419928287,
131.096308854122)) ;
#135767 = CARTESIAN_POINT('Ctrl Pts',(-18.7050835708224,14.425031880978,131.336092927187)) ;
#135768 = CARTESIAN_POINT('Ctrl Pts',(-18.7861994089251,14.5017260060049,
131.60629231186)) ;
#135769 = CARTESIAN_POINT('Ctrl Pts',(-18.8699095303306,14.5010099059246,
131.883776032442)) ;
#135770 = CARTESIAN_POINT('Ctrl Pts',(-18.950862117856,14.4231233705973,132.153475808602)) ;
#135771 = CARTESIAN_POINT('Ctrl Pts',(-19.0216063325537,14.2735700722065,
132.393250548626)) ;
#135772 = CARTESIAN_POINT('Ctrl Pts',(-19.0766525736922,14.0631260843178,
132.587185321685)) ;
#135773 = CARTESIAN_POINT('Ctrl Pts',(-19.1112752517511,13.8068513237717,
132.721449739404)) ;
#135774 = CARTESIAN_POINT('Ctrl Pts',(-19.1222768851844,13.5229068768556,
132.786731908381)) ;
#135775 = CARTESIAN_POINT('Ctrl Pts',(-19.1081388609896,13.2323185296325,
132.778518604924)) ;
#135776 = CARTESIAN_POINT('Ctrl Pts',(-19.0692979350921,12.955462422634,132.698120669452)) ;
#135777 = CARTESIAN_POINT('Ctrl Pts',(-19.0072938758856,12.7108337306576,
132.550242420851)) ;
#135778 = CARTESIAN_POINT('Ctrl Pts',(-18.9267369862212,12.5189036902296,
132.347912261719)) ;
#135779 = CARTESIAN_POINT('Ctrl Pts',(-18.8318784493428,12.3906586207823,
132.103941582259)) ;
#135780 = CARTESIAN_POINT('Ctrl Pts',(-18.7288363533557,12.3366531336248,
131.836123081131)) ;
#135781 = CARTESIAN_POINT('Ctrl Pts',(-18.624925410328,12.360297772879,131.565617456112)) ;
#135782 = CARTESIAN_POINT('Ctrl Pts',(-18.5256578035359,12.4609988515391,
131.308947306111)) ;
#135783 = CARTESIAN_POINT('Ctrl Pts',(-18.4392051331275,12.6291274638668,
131.089332236554)) ;
#135784 = CARTESIAN_POINT('Ctrl Pts',(-18.3692689876453,12.8555169755094,
130.918257614385)) ;
#135785 = CARTESIAN_POINT('Ctrl Pts',(-18.3212190683975,13.1215885522129,
130.810953330662)) ;
#135786 = CARTESIAN_POINT('Ctrl Pts',(-18.2972960902934,13.4096083938423,
130.774191778671)) ;
#135787 = CARTESIAN_POINT('Ctrl Pts',(-18.2985416991129,13.698212942693,130.810897551179)) ;
#135788 = CARTESIAN_POINT('Ctrl Pts',(-18.3244750392328,13.9691452295141,
130.91998909622)) ;
#135789 = CARTESIAN_POINT('Ctrl Pts',(-18.3719691340465,14.1982918407705,
131.091726472608)) ;
#135790 = CARTESIAN_POINT('Ctrl Pts',(-18.437100638801,14.3728095621698,131.315054734931)) ;
#135791 = CARTESIAN_POINT('Ctrl Pts',(-18.5147502122421,14.479662285758,131.575038501861)) ;
#135792 = CARTESIAN_POINT('Ctrl Pts',(-18.5984271700058,14.5107460879228,
131.852624565577)) ;
#135793 = CARTESIAN_POINT('Ctrl Pts',(-18.6814592251425,14.4636147982726,
132.128355723987)) ;
#135794 = CARTESIAN_POINT('Ctrl Pts',(-18.7567611079911,14.3427084720644,
132.38133252825)) ;
#135795 = CARTESIAN_POINT('Ctrl Pts',(-18.8191499212685,14.1545214106307,
132.596878690056)) ;
#135796 = CARTESIAN_POINT('Ctrl Pts',(-18.8624161383915,13.914665784431,132.756380600079)) ;
#135797 = CARTESIAN_POINT('Ctrl Pts',(-18.8832226690577,13.6405172708492,
132.850185928448)) ;
#135798 = CARTESIAN_POINT('Ctrl Pts',(-18.879379985006,13.3501102818962,132.872073497633)) ;
#135799 = CARTESIAN_POINT('Ctrl Pts',(-18.8504830366193,13.0651843315454,
132.820727303234)) ;
#135800 = CARTESIAN_POINT('Ctrl Pts',(-18.7972049191449,12.80388772374,132.698441638351)) ;
#135801 = CARTESIAN_POINT('Ctrl Pts',(-18.723938579695,12.5899465270377,132.517340764542)) ;
#135802 = CARTESIAN_POINT('Ctrl Pts',(-18.6339631078438,12.4339563210189,
132.28768165985)) ;
#135803 = CARTESIAN_POINT('Ctrl Pts',(-18.533655418016,12.3491846989202,132.027754670765)) ;
#135804 = CARTESIAN_POINT('Ctrl Pts',(-18.4287414629348,12.3415474281895,
131.754556958259)) ;
#135805 = CARTESIAN_POINT('Ctrl Pts',(-18.3275546121177,12.4110292201394,
131.491915929484)) ;
#135806 = CARTESIAN_POINT('Ctrl Pts',(-18.2349169164515,12.5533605448057,
131.254484931781)) ;
#135807 = CARTESIAN_POINT('Ctrl Pts',(-18.1578099509812,12.7574391512257,
131.062286140571)) ;
#135808 = CARTESIAN_POINT('Ctrl Pts',(-18.1003696787992,13.0095817126533,
130.92762938283)) ;
#135809 = CARTESIAN_POINT('Ctrl Pts',(-18.0663253206741,13.2928226801242,
130.861470362866)) ;
#135810 = CARTESIAN_POINT('Ctrl Pts',(-18.0574821752941,13.5820119966617,
130.868533156755)) ;
#135811 = CARTESIAN_POINT('Ctrl Pts',(-18.0735684910089,13.8633229249982,
130.948835515899)) ;
#135812 = CARTESIAN_POINT('Ctrl Pts',(-18.1128079244624,14.1112602779132,
131.096570682687)) ;
#135813 = CARTESIAN_POINT('Ctrl Pts',(-18.1713264366975,14.3095521754014,
131.300538449874)) ;
#135814 = CARTESIAN_POINT('Ctrl Pts',(-18.2445253330056,14.4451057235358,
131.547453993518)) ;
#135815 = CARTESIAN_POINT('Ctrl Pts',(-18.3269176211252,14.5076745769451,
131.821434215678)) ;
#135816 = CARTESIAN_POINT('Ctrl Pts',(-18.4109135921778,14.4918702514085,
132.09992274832)) ;
#135817 = CARTESIAN_POINT('Ctrl Pts',(-18.4899530140776,14.4001695900989,
132.363825830347)) ;
#135818 = CARTESIAN_POINT('Ctrl Pts',(-18.5581972721776,14.238339270588,132.596306467926)) ;
#135819 = CARTESIAN_POINT('Ctrl Pts',(-18.6097312244741,14.0178457541506,
132.77999745246)) ;
#135820 = CARTESIAN_POINT('Ctrl Pts',(-18.6401448193709,13.7549024704848,
132.901969265826)) ;
#135821 = CARTESIAN_POINT('Ctrl Pts',(-18.6463850313128,13.4669383655623,
132.953465269722)) ;
#135822 = CARTESIAN_POINT('Ctrl Pts',(-18.6276503009215,13.1792878389568,
132.931593942622)) ;
#135823 = CARTESIAN_POINT('Ctrl Pts',(-18.5840179153444,12.9054935275296,
132.837423835677)) ;
#135824 = CARTESIAN_POINT('Ctrl Pts',(-18.5184918875895,12.6708451835732,
132.679031311941)) ;
#135825 = CARTESIAN_POINT('Ctrl Pts',(-18.4344363065144,12.4890109361581,
132.466673752346)) ;
#135826 = CARTESIAN_POINT('Ctrl Pts',(-18.3378254602386,12.3747427440592,
132.217485900113)) ;
#135827 = CARTESIAN_POINT('Ctrl Pts',(-18.2341291109171,12.335118127865,131.947725095572)) ;
#135828 = CARTESIAN_POINT('Ctrl Pts',(-18.1304829793124,12.3735357257966,
131.678071654494)) ;
#135829 = CARTESIAN_POINT('Ctrl Pts',(-18.0332195672274,12.4876827050984,
131.427169660191)) ;
#135830 = CARTESIAN_POINT('Ctrl Pts',(-17.9493134502573,12.668143871092,131.215113064817)) ;
#135831 = CARTESIAN_POINT('Ctrl Pts',(-17.8833190355393,12.9033827829949,
131.055504217813)) ;
#135832 = CARTESIAN_POINT('Ctrl Pts',(-17.8397509602161,13.1743601664502,
130.961218011576)) ;
#135833 = CARTESIAN_POINT('Ctrl Pts',(-17.8204668396867,13.4644840041335,
130.938043352746)) ;
#135834 = CARTESIAN_POINT('Ctrl Pts',(-17.8265350254978,13.7518155739233,
130.988946607329)) ;
#135835 = CARTESIAN_POINT('Ctrl Pts',(-17.8566012791567,14.0147480425275,
131.109855058721)) ;
#135836 = CARTESIAN_POINT('Ctrl Pts',(-17.90786398017,14.2359322469135,131.292745615315)) ;
#135837 = CARTESIAN_POINT('Ctrl Pts',(-17.9762298617494,14.3990328419962,
131.525712867481)) ;
#135838 = CARTESIAN_POINT('Ctrl Pts',(-18.055065638864,14.4913721211862,131.788962667964)) ;
#135839 = CARTESIAN_POINT('Ctrl Pts',(-18.1393991985355,14.5077030613306,
132.068583449212)) ;
#135840 = CARTESIAN_POINT('Ctrl Pts',(-18.2210461373333,14.4466726935246,
132.340051735665)) ;
#135841 = CARTESIAN_POINT('Ctrl Pts',(-18.2950035387414,14.3110620977678,
132.589454770925)) ;
#135842 = CARTESIAN_POINT('Ctrl Pts',(-18.3535868279914,14.1132680684101,
132.793577578567)) ;
#135843 = CARTESIAN_POINT('Ctrl Pts',(-18.393011856418,13.8656264960883,132.941870264204)) ;
#135844 = CARTESIAN_POINT('Ctrl Pts',(-18.4093627200831,13.5853317318957,
133.022849013586)) ;
#135845 = CARTESIAN_POINT('Ctrl Pts',(-18.4005900814448,13.2939513094312,
133.030374526169)) ;
#135846 = CARTESIAN_POINT('Ctrl Pts',(-18.3670959101891,13.0136081090702,
132.965460512865)) ;
#135847 = CARTESIAN_POINT('Ctrl Pts',(-18.3099441323283,12.7604084565328,
132.831704484875)) ;
#135848 = CARTESIAN_POINT('Ctrl Pts',(-18.2330287799136,12.5556140537718,
132.640069906698)) ;
#135849 = CARTESIAN_POINT('Ctrl Pts',(-18.1403993250708,12.412162783817,132.402717407191)) ;
#135850 = CARTESIAN_POINT('Ctrl Pts',(-18.039122761627,12.3419224833159,132.139862058296)) ;
#135851 = CARTESIAN_POINT('Ctrl Pts',(-17.9346214328855,12.3485705631489,
131.867734666129)) ;
#135852 = CARTESIAN_POINT('Ctrl Pts',(-17.8340398826189,12.4325162173742,
131.60707108893)) ;
#135853 = CARTESIAN_POINT('Ctrl Pts',(-17.7440580525167,12.5872706018155,
131.377320640071)) ;
#135854 = CARTESIAN_POINT('Ctrl Pts',(-17.6702459325862,12.8016741765326,
131.1947873473)) ;
#135855 = CARTESIAN_POINT('Ctrl Pts',(-17.6170393754709,13.0608926757193,
131.072495055625)) ;
#135856 = CARTESIAN_POINT('Ctrl Pts',(-17.5876611427528,13.3463627388947,
131.019840506949)) ;
#135857 = CARTESIAN_POINT('Ctrl Pts',(-17.5835099051843,13.6367413735624,
131.040812586735)) ;
#135858 = CARTESIAN_POINT('Ctrl Pts',(-17.6040712549613,13.912123441329,131.134008457263)) ;
#135859 = CARTESIAN_POINT('Ctrl Pts',(-17.6473147092117,14.1528033236638,
131.293522210415)) ;
#135860 = CARTESIAN_POINT('Ctrl Pts',(-17.7090710684674,14.3402810134416,
131.506980670982)) ;
#135861 = CARTESIAN_POINT('Ctrl Pts',(-17.784324421975,14.4626257099404,131.759874983544)) ;
#135862 = CARTESIAN_POINT('Ctrl Pts',(-17.8676273435361,14.5106364099982,
132.036519206507)) ;
#135863 = CARTESIAN_POINT('Ctrl Pts',(-17.9509431998974,14.4805445966973,
132.31289642704)) ;
#135864 = CARTESIAN_POINT('Ctrl Pts',(-18.0287637016259,14.3748126779467,
132.57339232087)) ;
#135865 = CARTESIAN_POINT('Ctrl Pts',(-18.0942745357637,14.2005693776624,
132.797921352006)) ;
#135866 = CARTESIAN_POINT('Ctrl Pts',(-18.1420291731984,13.9714224956824,
132.970479780879)) ;
#135867 = CARTESIAN_POINT('Ctrl Pts',(-18.1681061343277,13.7016038456452,
133.07989078727)) ;
#135868 = CARTESIAN_POINT('Ctrl Pts',(-18.1697184694213,13.4137877720204,
133.117594113432)) ;
#135869 = CARTESIAN_POINT('Ctrl Pts',(-18.1460719924332,13.1249621059971,
133.081716204354)) ;
#135870 = CARTESIAN_POINT('Ctrl Pts',(-18.098349112227,12.858759801946,132.975335138158)) ;
#135871 = CARTESIAN_POINT('Ctrl Pts',(-18.0285125557916,12.6311849064932,
132.804627705542)) ;
#135872 = CARTESIAN_POINT('Ctrl Pts',(-17.9419067380147,12.4620614418067,
132.584665021202)) ;
#135873 = CARTESIAN_POINT('Ctrl Pts',(-17.8431161137062,12.3611529243014,
132.329254527925)) ;
#135874 = CARTESIAN_POINT('Ctrl Pts',(-17.7394163400758,12.336402737043,132.059308529178)) ;
#135875 = CARTESIAN_POINT('Ctrl Pts',(-17.636008023939,12.3896954767389,131.790522379684)) ;
#135876 = CARTESIAN_POINT('Ctrl Pts',(-17.5411529235148,12.5169545730866,
131.54651181945)) ;
#135877 = CARTESIAN_POINT('Ctrl Pts',(-17.4601656512396,12.7090014500136,
131.343041028757)) ;
#135878 = CARTESIAN_POINT('Ctrl Pts',(-17.3982954159609,12.9518209129291,
131.195365244849)) ;
#135879 = CARTESIAN_POINT('Ctrl Pts',(-17.3590590475251,13.2283911259786,
131.113826328101)) ;
#135880 = CARTESIAN_POINT('Ctrl Pts',(-17.3445909288019,13.5192444476926,
131.104682525303)) ;
#135881 = CARTESIAN_POINT('Ctrl Pts',(-17.3552759397806,13.8035929406365,
131.169057687742)) ;
#135882 = CARTESIAN_POINT('Ctrl Pts',(-17.3897650651813,14.0607675161601,
131.30300701978)) ;
#135883 = CARTESIAN_POINT('Ctrl Pts',(-17.4443353177419,14.2709776513911,
131.49540177985)) ;
#135884 = CARTESIAN_POINT('Ctrl Pts',(-17.5152284115638,14.4220258151157,
131.735762483094)) ;
#135885 = CARTESIAN_POINT('Ctrl Pts',(-17.5958972727999,14.5004899933202,
132.004539334194)) ;
#135886 = CARTESIAN_POINT('Ctrl Pts',(-17.6797407048686,14.5020985766214,
132.282472815977)) ;
#135887 = CARTESIAN_POINT('Ctrl Pts',(-17.7606887259789,14.426667623352,132.552070316538)) ;
#135888 = CARTESIAN_POINT('Ctrl Pts',(-17.8320641853255,14.2786158189735,
132.79380669298)) ;
#135889 = CARTESIAN_POINT('Ctrl Pts',(-17.8875765378756,14.0697690186074,
132.989079973035)) ;
#135890 = CARTESIAN_POINT('Ctrl Pts',(-17.922834488677,13.8142976320865,133.125231432651)) ;
#135891 = CARTESIAN_POINT('Ctrl Pts',(-17.9345112522901,13.5318062075926,
133.19237603013)) ;
#135892 = CARTESIAN_POINT('Ctrl Pts',(-17.9211404368569,13.2403761874523,
133.186487415733)) ;
#135893 = CARTESIAN_POINT('Ctrl Pts',(-17.8827207165006,12.9618561593774,
133.107451653599)) ;
#135894 = CARTESIAN_POINT('Ctrl Pts',(-17.821581417852,12.7173263730279,132.96193349821)) ;
#135895 = CARTESIAN_POINT('Ctrl Pts',(-17.7413926221805,12.5233446886838,
132.760735766704)) ;
#135896 = CARTESIAN_POINT('Ctrl Pts',(-17.6467746618759,12.3931312315505,
132.517486220828)) ;
#135897 = CARTESIAN_POINT('Ctrl Pts',(-17.5437035922363,12.337075246258,132.249632321582)) ;
#135898 = CARTESIAN_POINT('Ctrl Pts',(-17.4401454160532,12.3586764449227,
131.98003227223)) ;
#135899 = CARTESIAN_POINT('Ctrl Pts',(-17.3410665934673,12.4563696314589,
131.723751639427)) ;
#135900 = CARTESIAN_POINT('Ctrl Pts',(-17.2536320179894,12.6234424170359,
131.50146332499)) ;
#135901 = CARTESIAN_POINT('Ctrl Pts',(-17.1832036195686,12.8484690314232,
131.32893954711)) ;
#135902 = CARTESIAN_POINT('Ctrl Pts',(-17.1344653483001,13.1134860607375,
131.219613229379)) ;
#135903 = CARTESIAN_POINT('Ctrl Pts',(-17.1097906021278,13.402425050447,131.180795951585)) ;
#135904 = CARTESIAN_POINT('Ctrl Pts',(-17.1104146704051,13.6901681944769,
131.215561704661)) ;
#135905 = CARTESIAN_POINT('Ctrl Pts',(-17.1355551568111,13.9614083380647,
131.322263958797)) ;
#135906 = CARTESIAN_POINT('Ctrl Pts',(-17.1825349214449,14.1924050674132,
131.492558721692)) ;
#135907 = CARTESIAN_POINT('Ctrl Pts',(-17.247284144374,14.3688010159201,131.714792207733)) ;
#135908 = CARTESIAN_POINT('Ctrl Pts',(-17.3247083783915,14.4776662097744,
131.974131076165)) ;
#135909 = CARTESIAN_POINT('Ctrl Pts',(-17.4080456851403,14.5108828480259,
132.250624200494)) ;
#135910 = CARTESIAN_POINT('Ctrl Pts',(-17.4912091781135,14.4662997711349,
132.526737050679)) ;
#135911 = CARTESIAN_POINT('Ctrl Pts',(-17.5670722488366,14.3468724358185,
132.781476724685)) ;
#135912 = CARTESIAN_POINT('Ctrl Pts',(-17.6295496572066,14.161614932188,132.997074962764)) ;
#135913 = CARTESIAN_POINT('Ctrl Pts',(-17.6736158962945,13.9230022753498,
133.158962448849)) ;
#135914 = CARTESIAN_POINT('Ctrl Pts',(-17.6951931588153,13.6485314062169,
133.25514650467)) ;
#135915 = CARTESIAN_POINT('Ctrl Pts',(-17.6920615738823,13.3583011743042,
133.279105884718)) ;
#135916 = CARTESIAN_POINT('Ctrl Pts',(-17.6637579865309,13.072504270402,133.229551323447)) ;
#135917 = CARTESIAN_POINT('Ctrl Pts',(-17.6114584214845,12.8117566735177,
133.109923707737)) ;
#135918 = CARTESIAN_POINT('Ctrl Pts',(-17.5386760935971,12.5955171582893,
132.930311398659)) ;
#135919 = CARTESIAN_POINT('Ctrl Pts',(-17.4485485923782,12.4369580568928,
132.700390646819)) ;
#135920 = CARTESIAN_POINT('Ctrl Pts',(-17.3489049682672,12.3507869630092,
132.442246375848)) ;
#135921 = CARTESIAN_POINT('Ctrl Pts',(-17.2444930320388,12.3404899643528,
132.170365644373)) ;
#135922 = CARTESIAN_POINT('Ctrl Pts',(-17.1426216271441,12.4078494476239,
131.905884901552)) ;
#135923 = CARTESIAN_POINT('Ctrl Pts',(-17.0495668256941,12.5483871977687,
131.667259067528)) ;
#135924 = CARTESIAN_POINT('Ctrl Pts',(-16.971814498006,12.7513533086917,131.473242742698)) ;
#135925 = CARTESIAN_POINT('Ctrl Pts',(-16.9139622836365,13.001941318222,131.337310415625)) ;
#135926 = CARTESIAN_POINT('Ctrl Pts',(-16.8792750897038,13.2828868274063,
131.269082634896)) ;
#135927 = CARTESIAN_POINT('Ctrl Pts',(-16.8695679518648,13.5743278631276,
131.273876133887)) ;
#135928 = CARTESIAN_POINT('Ctrl Pts',(-16.8850187674673,13.8554587804339,
131.352236081223)) ;
#135929 = CARTESIAN_POINT('Ctrl Pts',(-16.9233899892215,14.103739100914,131.497307260457)) ;
#135930 = CARTESIAN_POINT('Ctrl Pts',(-16.9815525794946,14.3046990175591,
131.70035759611)) ;
#135931 = CARTESIAN_POINT('Ctrl Pts',(-17.0547401043487,14.4424188711516,
131.947366060444)) ;
#135932 = CARTESIAN_POINT('Ctrl Pts',(-17.1362824190426,14.5067209234145,
132.218584626412)) ;
#135933 = CARTESIAN_POINT('Ctrl Pts',(-17.2205230150152,14.4936392684735,
132.497872334383)) ;
#135934 = CARTESIAN_POINT('Ctrl Pts',(-17.2999675507863,14.404006740505,132.76301963)) ;
#135935 = CARTESIAN_POINT('Ctrl Pts',(-17.3687938432936,14.2433942656814,
132.99730827925)) ;
#135936 = CARTESIAN_POINT('Ctrl Pts',(-17.4206621252372,14.0252993056693,
133.181832423558)) ;
#135937 = CARTESIAN_POINT('Ctrl Pts',(-17.4518062177166,13.7626963119846,
133.306025850587)) ;
#135938 = CARTESIAN_POINT('Ctrl Pts',(-17.4588018749284,13.4766513624265,
133.3595520989)) ;
#135939 = CARTESIAN_POINT('Ctrl Pts',(-17.4407196010973,13.1866966293381,
133.339828540076)) ;
#135940 = CARTESIAN_POINT('Ctrl Pts',(-17.3976621744542,12.9123106961637,
133.247325290375)) ;
#135941 = CARTESIAN_POINT('Ctrl Pts',(-17.3328316521718,12.6769408805555,
133.090898057899)) ;
#135942 = CARTESIAN_POINT('Ctrl Pts',(-17.2494627622651,12.4935889535621,
132.880470073151)) ;
#135943 = CARTESIAN_POINT('Ctrl Pts',(-17.152618226233,12.3766908568814,132.630777552473)) ;
#135944 = CARTESIAN_POINT('Ctrl Pts',(-17.049231423334,12.3352383862452,132.361846606225)) ;
#135945 = CARTESIAN_POINT('Ctrl Pts',(-16.9457336891591,12.3713736006973,
132.092556286143)) ;
#135946 = CARTESIAN_POINT('Ctrl Pts',(-16.8484161060952,12.4827590293817,
131.841396897906)) ;
#135947 = CARTESIAN_POINT('Ctrl Pts',(-16.7634777794498,12.6627224306716,
131.626558702344)) ;
#135948 = CARTESIAN_POINT('Ctrl Pts',(-16.6972681323854,12.8955397849013,
131.466150815898)) ;
#135949 = CARTESIAN_POINT('Ctrl Pts',(-16.652840547036,13.1663558963296,131.369445368094)) ;
#135950 = CARTESIAN_POINT('Ctrl Pts',(-16.6328908225603,13.4563321062043,
131.344330530745)) ;
#135951 = CARTESIAN_POINT('Ctrl Pts',(-16.6382111416064,13.74354179735,131.392991362756)) ;
#135952 = CARTESIAN_POINT('Ctrl Pts',(-16.6676592322395,14.007863745204,131.512146621969)) ;
#135953 = CARTESIAN_POINT('Ctrl Pts',(-16.7182928746253,14.2299792391956,
131.693135937676)) ;
#135954 = CARTESIAN_POINT('Ctrl Pts',(-16.7859878307255,14.3948659481182,
131.924049786769)) ;
#135955 = CARTESIAN_POINT('Ctrl Pts',(-16.8651153132331,14.4898740802148,
132.188374983265)) ;
#135956 = CARTESIAN_POINT('Ctrl Pts',(-16.9488778829896,14.5084149248409,
132.466110688147)) ;
#135957 = CARTESIAN_POINT('Ctrl Pts',(-17.0311885247318,14.4492459338564,
132.739733964955)) ;
#135958 = CARTESIAN_POINT('Ctrl Pts',(-17.104950151554,14.316609488643,132.988318108268)) ;
#135959 = CARTESIAN_POINT('Ctrl Pts',(-17.1643724443007,14.1198900556279,
133.195042593654)) ;
#135960 = CARTESIAN_POINT('Ctrl Pts',(-17.2043618345605,13.8734079349303,
133.344971495627)) ;
#135961 = CARTESIAN_POINT('Ctrl Pts',(-17.2214102827416,13.5947694158123,
133.42787905469)) ;
#135962 = CARTESIAN_POINT('Ctrl Pts',(-17.2135302438731,13.3033325180628,
133.438020470237)) ;
#135963 = CARTESIAN_POINT('Ctrl Pts',(-17.1805025277542,13.0207084742087,
133.374676701685)) ;
#135964 = CARTESIAN_POINT('Ctrl Pts',(-17.124234300538,12.767628690545,133.243341451459)) ;
#135965 = CARTESIAN_POINT('Ctrl Pts',(-17.0476257592213,12.5604751539345,
133.052712263167)) ;
#135966 = CARTESIAN_POINT('Ctrl Pts',(-16.9553890051503,12.4152916729436,
132.816483612565)) ;
#135967 = CARTESIAN_POINT('Ctrl Pts',(-16.8542709676215,12.3428120631862,
132.554100291461)) ;
#135968 = CARTESIAN_POINT('Ctrl Pts',(-16.7494730831066,12.3473797413046,
132.281194465277)) ;
#135969 = CARTESIAN_POINT('Ctrl Pts',(-16.6487943422117,12.4294695368143,
132.020223589768)) ;
#135970 = CARTESIAN_POINT('Ctrl Pts',(-16.5588158738871,12.5816148375682,
131.790339248201)) ;
#135971 = CARTESIAN_POINT('Ctrl Pts',(-16.4842129576639,12.7949907280796,
131.605591372129)) ;
#135972 = CARTESIAN_POINT('Ctrl Pts',(-16.4302842435271,13.054101177031,131.481287531456)) ;
#135973 = CARTESIAN_POINT('Ctrl Pts',(-16.4003618883851,13.3386274126212,
131.426981031138)) ;
#135974 = CARTESIAN_POINT('Ctrl Pts',(-16.3954982522069,13.6281884734652,
131.445764473398)) ;
#135975 = CARTESIAN_POINT('Ctrl Pts',(-16.4153244875857,13.9042249218154,
131.536802751734)) ;
#135976 = CARTESIAN_POINT('Ctrl Pts',(-16.4579192874622,14.1463903457502,
131.694429834647)) ;
#135977 = CARTESIAN_POINT('Ctrl Pts',(-16.519604946235,14.3364819716926,131.907871784003)) ;
#135978 = CARTESIAN_POINT('Ctrl Pts',(-16.5941877045133,14.4598817702337,
132.158628290576)) ;
#135979 = CARTESIAN_POINT('Ctrl Pts',(-16.6772180078865,14.5104486170863,
132.434425087988)) ;
#135980 = CARTESIAN_POINT('Ctrl Pts',(-16.7610712369098,14.4822486369166,
132.712559593312)) ;
#135981 = CARTESIAN_POINT('Ctrl Pts',(-16.8386672352436,14.3791733041028,
132.97219580738)) ;
#135982 = CARTESIAN_POINT('Ctrl Pts',(-16.9049174530084,14.2063740303146,
133.199006100538)) ;
#135983 = CARTESIAN_POINT('Ctrl Pts',(-16.9532362150924,13.9777765864427,
133.373293310572)) ;
#135984 = CARTESIAN_POINT('Ctrl Pts',(-16.9798528341138,13.7109259499415,
133.484028399788)) ;
#135985 = CARTESIAN_POINT('Ctrl Pts',(-16.9822174695309,13.4211174151953,
133.524197897855)) ;
#135986 = CARTESIAN_POINT('Ctrl Pts',(-16.9593603734184,13.1336909339448,
133.490426214311)) ;
#135987 = CARTESIAN_POINT('Ctrl Pts',(-16.9122699848515,12.8658812639418,
133.385975367206)) ;
#135988 = CARTESIAN_POINT('Ctrl Pts',(-16.8429275372481,12.6367690190525,
133.216731683706)) ;
#135989 = CARTESIAN_POINT('Ctrl Pts',(-16.7566414738858,12.4658337897599,
132.997733929609)) ;
#135990 = CARTESIAN_POINT('Ctrl Pts',(-16.6584445847538,12.3631245211514,
132.743942914283)) ;
#135991 = CARTESIAN_POINT('Ctrl Pts',(-16.5545911413088,12.3360466241608,
132.473621289443)) ;
#135992 = CARTESIAN_POINT('Ctrl Pts',(-16.4514231221753,12.3868688002356,
132.205414356226)) ;
#135993 = CARTESIAN_POINT('Ctrl Pts',(-16.3561369237034,12.5119418325269,
131.960173693308)) ;
#135994 = CARTESIAN_POINT('Ctrl Pts',(-16.2746048987367,12.7021783709845,
131.755117298832)) ;
#135995 = CARTESIAN_POINT('Ctrl Pts',(-16.2118058427217,12.9449353770794,
131.604890369302)) ;
#135996 = CARTESIAN_POINT('Ctrl Pts',(-16.1719673653937,13.2214383784226,
131.521650682401)) ;
#135997 = CARTESIAN_POINT('Ctrl Pts',(-16.1568634879724,13.5108147708277,
131.510491075186)) ;
#135998 = CARTESIAN_POINT('Ctrl Pts',(-16.1669300007681,13.7968084175674,
131.573203022695)) ;
#135999 = CARTESIAN_POINT('Ctrl Pts',(-16.2006569741179,14.0536576083437,
131.704754764011)) ;
#136000 = CARTESIAN_POINT('Ctrl Pts',(-16.254784608073,14.2659120564335,131.895928413579)) ;
#136001 = CARTESIAN_POINT('Ctrl Pts',(-16.3251935914364,14.4185012516542,
132.134813692496)) ;
#136002 = CARTESIAN_POINT('Ctrl Pts',(-16.4055493007845,14.4992712221482,
132.402638758212)) ;
#136003 = CARTESIAN_POINT('Ctrl Pts',(-16.4897480826034,14.5031360116066,
132.681750239267)) ;
#136004 = CARTESIAN_POINT('Ctrl Pts',(-16.5707620204115,14.4296202074177,
132.951505237183)) ;
#136005 = CARTESIAN_POINT('Ctrl Pts',(-16.6421991335516,14.2844131247839,
133.193261917155)) ;
#136006 = CARTESIAN_POINT('Ctrl Pts',(-16.6984700341114,14.0764755685082,
133.390876378768)) ;
#136007 = CARTESIAN_POINT('Ctrl Pts',(-16.7342912161991,13.8227947339683,
133.528581938243)) ;
#136008 = CARTESIAN_POINT('Ctrl Pts',(-16.7467556388197,13.5398702989391,
133.59814585037)) ;
#136009 = CARTESIAN_POINT('Ctrl Pts',(-16.7340724183047,13.2487717783427,
133.594219576124)) ;
#136010 = CARTESIAN_POINT('Ctrl Pts',(-16.6965212883533,12.9703362151756,
133.517627433161)) ;
#136011 = CARTESIAN_POINT('Ctrl Pts',(-16.6359937287517,12.7241092781338,
133.373940651091)) ;
#136012 = CARTESIAN_POINT('Ctrl Pts',(-16.5560795871543,12.5279171433205,
133.173632261453)) ;
#136013 = CARTESIAN_POINT('Ctrl Pts',(-16.4618411443677,12.3959938665945,
132.931466168076)) ;
#136014 = CARTESIAN_POINT('Ctrl Pts',(-16.3593827732272,12.3376260980812,
132.665255360874)) ;
#136015 = CARTESIAN_POINT('Ctrl Pts',(-16.2550385035652,12.3570497794023,
132.393594158916)) ;
#136016 = CARTESIAN_POINT('Ctrl Pts',(-16.1560569930776,12.4525559733436,
132.137489642659)) ;
#136017 = CARTESIAN_POINT('Ctrl Pts',(-16.0682112092327,12.6176036105847,
131.9139932347)) ;
#136018 = CARTESIAN_POINT('Ctrl Pts',(-15.9972052369213,12.8410947019102,
131.739774174027)) ;
#136019 = CARTESIAN_POINT('Ctrl Pts',(-15.9477710009751,13.1055203518464,
131.628457545108)) ;
#136020 = CARTESIAN_POINT('Ctrl Pts',(-15.9223966595682,13.3928980327512,
131.587457525944)) ;
#136021 = CARTESIAN_POINT('Ctrl Pts',(-15.9222756880834,13.6824543649216,
131.620230232659)) ;
#136022 = CARTESIAN_POINT('Ctrl Pts',(-15.9466295677973,13.9532692757644,
131.724475741057)) ;
#136023 = CARTESIAN_POINT('Ctrl Pts',(-15.9930649492766,14.1862511235797,
131.893256545959)) ;
#136024 = CARTESIAN_POINT('Ctrl Pts',(-16.0572774469947,14.3643962082537,
132.113884233036)) ;
#136025 = CARTESIAN_POINT('Ctrl Pts',(-16.1348869305229,14.4759024807437,
132.373959659061)) ;
#136026 = CARTESIAN_POINT('Ctrl Pts',(-16.2178601983213,14.5109062464403,
132.649271579231)) ;
#136027 = CARTESIAN_POINT('Ctrl Pts',(-16.3010573982548,14.4687351628052,
132.925452283273)) ;
#136028 = CARTESIAN_POINT('Ctrl Pts',(-16.3772524895357,14.351243796897,133.18118301111)) ;
#136029 = CARTESIAN_POINT('Ctrl Pts',(-16.4401554780105,14.1681343550178,
133.397975738382)) ;
#136030 = CARTESIAN_POINT('Ctrl Pts',(-16.4850310227968,13.9291093552066,
133.562448350169)) ;
#136031 = CARTESIAN_POINT('Ctrl Pts',(-16.5070926720565,13.6572015399983,
133.659816803159)) ;
#136032 = CARTESIAN_POINT('Ctrl Pts',(-16.5046943032788,13.3659146668707,
133.686064790888)) ;
#136033 = CARTESIAN_POINT('Ctrl Pts',(-16.4771547092974,13.0809591455927,
133.638599282157)) ;
#136034 = CARTESIAN_POINT('Ctrl Pts',(-16.4256137570119,12.8188859308948,
133.521201214271)) ;
#136035 = CARTESIAN_POINT('Ctrl Pts',(-16.3527339561376,12.5999510440463,
133.341543109138)) ;
#136036 = CARTESIAN_POINT('Ctrl Pts',(-16.2641281336111,12.4414984825018,
133.115647334815)) ;
#136037 = CARTESIAN_POINT('Ctrl Pts',(-16.1641430091743,12.3520343108791,
132.85671610708)) ;
#136038 = CARTESIAN_POINT('Ctrl Pts',(-16.0594698293865,12.3398054622105,
132.584157469235)) ;
#136039 = CARTESIAN_POINT('Ctrl Pts',(-15.9577980199829,12.4047865271677,
132.320144279598)) ;
#136040 = CARTESIAN_POINT('Ctrl Pts',(-15.8643756324851,12.5431933869583,
132.080444267518)) ;
#136041 = CARTESIAN_POINT('Ctrl Pts',(-15.7860699178347,12.7444965603529,
131.884816381687)) ;
#136042 = CARTESIAN_POINT('Ctrl Pts',(-15.7274833077799,12.9945025224571,
131.746812479205)) ;
#136043 = CARTESIAN_POINT('Ctrl Pts',(-15.6921182047523,13.2745329094811,
131.676561655677)) ;
#136044 = CARTESIAN_POINT('Ctrl Pts',(-15.6817523163213,13.5670626370277,
131.679561862218)) ;
#136045 = CARTESIAN_POINT('Ctrl Pts',(-15.6963153264075,13.8462370772247,
131.755016293096)) ;
#136046 = CARTESIAN_POINT('Ctrl Pts',(-15.7342967830937,14.0979241250953,
131.899230741437)) ;
#136047 = CARTESIAN_POINT('Ctrl Pts',(-15.7919436686276,14.2997383418867,
132.100703473067)) ;
#136048 = CARTESIAN_POINT('Ctrl Pts',(-15.8645031781154,14.4393312193764,
132.345773094754)) ;
#136049 = CARTESIAN_POINT('Ctrl Pts',(-15.9465184391645,14.5060643569228,
132.618629039297)) ;
#136050 = CARTESIAN_POINT('Ctrl Pts',(-16.0301677623958,14.4951758782706,
132.895935895831)) ;
#136051 = CARTESIAN_POINT('Ctrl Pts',(-16.1102104627669,14.4072623281432,
133.163000755797)) ;
#136052 = CARTESIAN_POINT('Ctrl Pts',(-16.1790779676799,14.2495039694875,
133.397213921694)) ;
#136053 = CARTESIAN_POINT('Ctrl Pts',(-16.2319003919638,14.0308221258824,
133.584830620202)) ;
#136054 = CARTESIAN_POINT('Ctrl Pts',(-16.2633270017823,13.7719100664948,
133.709489495124)) ;
#136055 = CARTESIAN_POINT('Ctrl Pts',(-16.2711876727272,13.4847456450531,
133.765738112161)) ;
#136056 = CARTESIAN_POINT('Ctrl Pts',(-16.253847194686,13.1955425031336,133.748069200693)) ;
#136057 = CARTESIAN_POINT('Ctrl Pts',(-16.2115198754741,12.9200552968874,
133.65773228028)) ;
#136058 = CARTESIAN_POINT('Ctrl Pts',(-16.147222084084,12.6831184385928,133.502892140705)) ;
#136059 = CARTESIAN_POINT('Ctrl Pts',(-16.064282599147,12.4980281206389,133.293729089209)) ;
#136060 = CARTESIAN_POINT('Ctrl Pts',(-15.9679392810076,12.3791543430107,
133.045434009803)) ;
#136061 = CARTESIAN_POINT('Ctrl Pts',(-15.8643595558364,12.3353503717386,
132.776040083288)) ;
#136062 = CARTESIAN_POINT('Ctrl Pts',(-15.7608810145636,12.3691099621928,
132.506761731086)) ;
#136063 = CARTESIAN_POINT('Ctrl Pts',(-15.6627255542582,12.4795856785055,
132.253375320536)) ;
#136064 = CARTESIAN_POINT('Ctrl Pts',(-15.5784730291827,12.6553361009926,
132.040088792181)) ;
#136065 = CARTESIAN_POINT('Ctrl Pts',(-15.5110293575352,12.8882259217544,
131.876334600156)) ;
#136066 = CARTESIAN_POINT('Ctrl Pts',(-15.4660114239873,13.1581921393272,
131.777882402057)) ;
#136067 = CARTESIAN_POINT('Ctrl Pts',(-15.4453153424862,13.4482190387101,
131.750625899504)) ;
#136068 = CARTESIAN_POINT('Ctrl Pts',(-15.4499239120655,13.7352663202425,
131.797145410483)) ;
#136069 = CARTESIAN_POINT('Ctrl Pts',(-15.4786708796544,14.0004787425337,
131.914245491789)) ;
#136070 = CARTESIAN_POINT('Ctrl Pts',(-15.528718936817,14.2242401467777,132.093531049238)) ;
#136071 = CARTESIAN_POINT('Ctrl Pts',(-15.5963327554751,14.391486003047,132.324353743837)) ;
#136072 = CARTESIAN_POINT('Ctrl Pts',(-15.6747831211035,14.4880341837757,
132.586510244365)) ;
#136073 = CARTESIAN_POINT('Ctrl Pts',(-15.7588156763009,14.5089767222778,
132.865167334381)) ;
#136074 = CARTESIAN_POINT('Ctrl Pts',(-15.8410228376495,14.4520807364783,
133.138385805997)) ;
#136075 = CARTESIAN_POINT('Ctrl Pts',(-15.9152233944989,14.3213934969356,
133.388297276998)) ;
#136076 = CARTESIAN_POINT('Ctrl Pts',(-15.9751021978438,14.126427628205,133.596336490836)) ;
#136077 = CARTESIAN_POINT('Ctrl Pts',(-16.0157883783172,13.8807880817665,
133.748352793927)) ;
#136078 = CARTESIAN_POINT('Ctrl Pts',(-16.0334719367804,13.6022566506269,
133.833171646611)) ;
#136079 = CARTESIAN_POINT('Ctrl Pts',(-16.0263427101219,13.3123739575692,
133.845337187169)) ;
#136080 = CARTESIAN_POINT('Ctrl Pts',(-15.9941097511416,13.0290004002489,
133.784332603085)) ;
#136081 = CARTESIAN_POINT('Ctrl Pts',(-15.9383247563886,12.7741270713226,
133.65449670321)) ;
#136082 = CARTESIAN_POINT('Ctrl Pts',(-15.8622768484471,12.5657352250487,
133.465472847607)) ;
#136083 = CARTESIAN_POINT('Ctrl Pts',(-15.7707760397584,12.4188762117679,
133.231275457079)) ;
#136084 = CARTESIAN_POINT('Ctrl Pts',(-15.6694610724198,12.3438128452305,
132.968446766761)) ;
#136085 = CARTESIAN_POINT('Ctrl Pts',(-15.5650490222749,12.3461025205116,
132.696542230689)) ;
#136086 = CARTESIAN_POINT('Ctrl Pts',(-15.4641117267899,12.4255735874937,
132.43482095437)) ;
#136087 = CARTESIAN_POINT('Ctrl Pts',(-15.3733010936375,12.5765456735502,
132.202668192957)) ;
#136088 = CARTESIAN_POINT('Ctrl Pts',(-15.2984189865204,12.7879286592572,
132.017014437685)) ;
#136089 = CARTESIAN_POINT('Ctrl Pts',(-15.243943520018,13.0448054046113,131.89098628761)) ;
#136090 = CARTESIAN_POINT('Ctrl Pts',(-15.2130872375626,13.329756321322,131.834065836623)) ;
#136091 = CARTESIAN_POINT('Ctrl Pts',(-15.207498078425,13.6201107178654,131.850804210703)) ;
#136092 = CARTESIAN_POINT('Ctrl Pts',(-15.226664565684,13.8967554382586,131.93990903969)) ;
#136093 = CARTESIAN_POINT('Ctrl Pts',(-15.2685096670752,14.1394983367384,
132.095250212473)) ;
#136094 = CARTESIAN_POINT('Ctrl Pts',(-15.3296325471033,14.3315001569242,
132.307040763849)) ;
#136095 = CARTESIAN_POINT('Ctrl Pts',(-15.4041948784221,14.4575222943013,
132.557868425866)) ;
#136096 = CARTESIAN_POINT('Ctrl Pts',(-15.4871845489021,14.5099977938908,
132.833577267545)) ;
#136097 = CARTESIAN_POINT('Ctrl Pts',(-15.5706474715052,14.4843800867397,
133.110384973781)) ;
#136098 = CARTESIAN_POINT('Ctrl Pts',(-15.6489358172198,14.3828781461486,
133.372231534079)) ;
#136099 = CARTESIAN_POINT('Ctrl Pts',(-15.7152215321923,14.212816168216,133.598953578525)) ;
#136100 = CARTESIAN_POINT('Ctrl Pts',(-15.7643324415315,13.9854781681749,
133.775621838138)) ;
#136101 = CARTESIAN_POINT('Ctrl Pts',(-15.7916807767753,13.7179644909653,
133.888670251454)) ;
#136102 = CARTESIAN_POINT('Ctrl Pts',(-15.7946921387686,13.4301920376034,
133.930530607513)) ;
#136103 = CARTESIAN_POINT('Ctrl Pts',(-15.7726967990617,13.1421055633853,
133.899307008492)) ;
#136104 = CARTESIAN_POINT('Ctrl Pts',(-15.725756949418,12.87150128464,133.795559990037)) ;
#136105 = CARTESIAN_POINT('Ctrl Pts',(-15.6577073073503,12.6436097991943,
133.629723531333)) ;
#136106 = CARTESIAN_POINT('Ctrl Pts',(-15.5716152896333,12.4698498437503,
133.411423269474)) ;
#136107 = CARTESIAN_POINT('Ctrl Pts',(-15.4736825799438,12.3651221856613,
133.158394352247)) ;
#136108 = CARTESIAN_POINT('Ctrl Pts',(-15.3697907387214,12.335692224637,132.887997751447)) ;
#136109 = CARTESIAN_POINT('Ctrl Pts',(-15.2664401785828,12.3844432071478,
132.619277578795)) ;
#136110 = CARTESIAN_POINT('Ctrl Pts',(-15.1710399074463,12.5072147901112,
132.373635971455)) ;
#136111 = CARTESIAN_POINT('Ctrl Pts',(-15.0889535850671,12.6957550150873,
132.166979770339)) ;
#136112 = CARTESIAN_POINT('Ctrl Pts',(-15.0255721551039,12.9372999479051,
132.01505517321)) ;
#136113 = CARTESIAN_POINT('Ctrl Pts',(-14.9850575690906,13.2121499543988,
131.929735608954)) ;
#136114 = CARTESIAN_POINT('Ctrl Pts',(-14.9691714974783,13.5032465104466,
131.91650779929)) ;
#136115 = CARTESIAN_POINT('Ctrl Pts',(-14.9783938577685,13.7871080328991,
131.976440567623)) ;
#136116 = CARTESIAN_POINT('Ctrl Pts',(-15.0115648784408,14.0469104745439,
132.106594492085)) ;
#136117 = CARTESIAN_POINT('Ctrl Pts',(-15.0651801887707,14.2605649124229,
132.296255586953)) ;
#136118 = CARTESIAN_POINT('Ctrl Pts',(-15.1354050179275,14.4153649488043,
132.534693807358)) ;
#136119 = CARTESIAN_POINT('Ctrl Pts',(-15.2152370606947,14.4978582783663,
132.800850624746)) ;
#136120 = CARTESIAN_POINT('Ctrl Pts',(-15.2994258322498,14.5041773990225,
133.079939121836)) ;
#136121 = CARTESIAN_POINT('Ctrl Pts',(-15.3806609287712,14.4329779197685,
133.350346880059)) ;
#136122 = CARTESIAN_POINT('Ctrl Pts',(-15.4527495072584,14.2890422314917,
133.594146581102)) ;
#136123 = CARTESIAN_POINT('Ctrl Pts',(-15.5093788401438,14.082779433517,133.79275764401)) ;
#136124 = CARTESIAN_POINT('Ctrl Pts',(-15.545753191267,13.8309337098099,133.931989144067)) ;
#136125 = CARTESIAN_POINT('Ctrl Pts',(-15.5589571408963,13.5483120187831,
134.003745938923)) ;
#136126 = CARTESIAN_POINT('Ctrl Pts',(-15.5470459162325,13.2574777531019,
134.002035659956)) ;
#136127 = CARTESIAN_POINT('Ctrl Pts',(-15.510131605999,12.9779697529959,133.92735890912)) ;
#136128 = CARTESIAN_POINT('Ctrl Pts',(-15.4504417667573,12.7311580251373,
133.786020643798)) ;
#136129 = CARTESIAN_POINT('Ctrl Pts',(-15.3706607271275,12.5323980592304,
133.586256423076)) ;
#136130 = CARTESIAN_POINT('Ctrl Pts',(-15.2770803375685,12.3989897288854,
133.345890363007)) ;
#136131 = CARTESIAN_POINT('Ctrl Pts',(-15.1745710010167,12.3382487603058,
133.079602207309)) ;
#136132 = CARTESIAN_POINT('Ctrl Pts',(-15.0705359722807,12.3552058083452,
132.808726876001)) ;
#136133 = CARTESIAN_POINT('Ctrl Pts',(-14.9706606470321,12.4490680703867,
132.550225448555)) ;
#136134 = CARTESIAN_POINT('Ctrl Pts',(-14.8824522342596,12.612854304799,132.325691498574)) ;
#136135 = CARTESIAN_POINT('Ctrl Pts',(-14.8113527265263,12.8333918295054,
132.150980279395)) ;
#136136 = CARTESIAN_POINT('Ctrl Pts',(-14.7610563805274,13.0975419155814,
132.037242671929)) ;
#136137 = CARTESIAN_POINT('Ctrl Pts',(-14.7349932181902,13.3843701567211,
131.99420597981)) ;
#136138 = CARTESIAN_POINT('Ctrl Pts',(-14.7341460984049,13.6749248626015,
132.024944556395)) ;
#136139 = CARTESIAN_POINT('Ctrl Pts',(-14.7579228982456,13.9463602578246,
132.127499501483)) ;
#136140 = CARTESIAN_POINT('Ctrl Pts',(-14.8035289837161,14.1798324379302,
132.293714438332)) ;
#136141 = CARTESIAN_POINT('Ctrl Pts',(-14.8677079251816,14.3606302769089,
132.514446261517)) ;
#136142 = CARTESIAN_POINT('Ctrl Pts',(-14.9443462637881,14.4733618864566,
132.771384751192)) ;
#136143 = CARTESIAN_POINT('Ctrl Pts',(-15.0280034573494,14.5110756600993,
133.049012799316)) ;
#136144 = CARTESIAN_POINT('Ctrl Pts',(-15.1108313580727,14.4709889009811,
133.323927299789)) ;
#136145 = CARTESIAN_POINT('Ctrl Pts',(-15.1874906865422,14.3556941984043,
133.581070483478)) ;
#136146 = CARTESIAN_POINT('Ctrl Pts',(-15.2510153385486,14.1731666486328,
133.79982111375)) ;
#136147 = CARTESIAN_POINT('Ctrl Pts',(-15.2960503606692,13.9378584167298,
133.964426013949)) ;
#136148 = CARTESIAN_POINT('Ctrl Pts',(-15.3190310826371,13.6656355311939,
134.064636189014)) ;
#136149 = CARTESIAN_POINT('Ctrl Pts',(-15.3173445451022,13.3744563081115,
134.092966610367)) ;
#136150 = CARTESIAN_POINT('Ctrl Pts',(-15.2904580609234,13.0885611803192,
134.047472889722)) ;
#136151 = CARTESIAN_POINT('Ctrl Pts',(-15.2396747814133,12.8263306498725,
133.932194970172)) ;
#136152 = CARTESIAN_POINT('Ctrl Pts',(-15.1677163389787,12.6063807769631,
133.755109558956)) ;
#136153 = CARTESIAN_POINT('Ctrl Pts',(-15.0788943634793,12.4447492933123,
133.528822932428)) ;
#136154 = CARTESIAN_POINT('Ctrl Pts',(-14.9791253222199,12.3535025882306,
133.270511156007)) ;
#136155 = CARTESIAN_POINT('Ctrl Pts',(-14.8746674650902,12.3391045054194,
132.998527191728)) ;
#136156 = CARTESIAN_POINT('Ctrl Pts',(-14.7728141849366,12.4018104241151,
132.733985657383)) ;
#136157 = CARTESIAN_POINT('Ctrl Pts',(-14.6787517401919,12.5389586489687,
132.49253663729)) ;
#136158 = CARTESIAN_POINT('Ctrl Pts',(-14.6003862698118,12.7377764458565,
132.296567507347)) ;
#136159 = CARTESIAN_POINT('Ctrl Pts',(-14.5411439660413,12.9863019722805,
132.156626084833)) ;
#136160 = CARTESIAN_POINT('Ctrl Pts',(-14.5050286674343,13.2660338630659,
132.084222246459)) ;
#136161 = CARTESIAN_POINT('Ctrl Pts',(-14.4938897468974,13.5582232268191,
132.08492344046)) ;
#136162 = CARTESIAN_POINT('Ctrl Pts',(-14.507818431321,13.8387404070693,132.158622706454)) ;
#136163 = CARTESIAN_POINT('Ctrl Pts',(-14.5449327754259,14.0904925183414,
132.300141702221)) ;
#136164 = CARTESIAN_POINT('Ctrl Pts',(-14.6025167026814,14.2955136011611,
132.501693163721)) ;
#136165 = CARTESIAN_POINT('Ctrl Pts',(-14.6743979140284,14.4360006812449,
132.744601960421)) ;
#136166 = CARTESIAN_POINT('Ctrl Pts',(-14.7560190059001,14.5051702931602,
133.016232266989)) ;
#136167 = CARTESIAN_POINT('Ctrl Pts',(-14.8399788108669,14.4966323764384,
133.29455720462)) ;
#136168 = CARTESIAN_POINT('Ctrl Pts',(-14.92026343514,14.4108291399258,133.562335509995)) ;
#136169 = CARTESIAN_POINT('Ctrl Pts',(-14.9895377292265,14.2547209501546,
133.797763255438)) ;
#136170 = CARTESIAN_POINT('Ctrl Pts',(-15.0426869064103,14.0388606089928,
133.986156454842)) ;
#136171 = CARTESIAN_POINT('Ctrl Pts',(-15.0750262925721,13.779405578044,134.113692915164)) ;
#136172 = CARTESIAN_POINT('Ctrl Pts',(-15.0835065338818,13.4926641580088,
134.171741504609)) ;
#136173 = CARTESIAN_POINT('Ctrl Pts',(-15.0668941196817,13.2038302112353,
134.156144137311)) ;
#136174 = CARTESIAN_POINT('Ctrl Pts',(-15.0254043328273,12.9280759931688,
134.068184900734)) ;
#136175 = CARTESIAN_POINT('Ctrl Pts',(-14.9614251335503,12.6887447492448,
133.914424357805)) ;
#136176 = CARTESIAN_POINT('Ctrl Pts',(-14.8789170489459,12.5022966343227,
133.706505074034)) ;
#136177 = CARTESIAN_POINT('Ctrl Pts',(-14.7832955283864,12.381763978882,133.460180040676)) ;
#136178 = CARTESIAN_POINT('Ctrl Pts',(-14.6794737714671,12.3354318114705,
133.190193795545)) ;
#136179 = CARTESIAN_POINT('Ctrl Pts',(-14.5760954726489,12.3672035513488,
132.921157086038)) ;
#136180 = CARTESIAN_POINT('Ctrl Pts',(-14.4781651153176,12.474426481286,132.668233520948)) ;
#136181 = CARTESIAN_POINT('Ctrl Pts',(-14.3924892268079,12.6503068829769,
132.451164645272)) ;
#136182 = CARTESIAN_POINT('Ctrl Pts',(-14.3248849840194,12.8812481424524,
132.28680518042)) ;
#136183 = CARTESIAN_POINT('Ctrl Pts',(-14.2792429233544,13.1494231082653,
132.186430077652)) ;
#136184 = CARTESIAN_POINT('Ctrl Pts',(-14.2577333010081,13.4405328283774,
132.156949660664)) ;
#136185 = CARTESIAN_POINT('Ctrl Pts',(-14.2616812486159,13.7272524095848,
132.201463654968)) ;
#136186 = CARTESIAN_POINT('Ctrl Pts',(-14.2897398061011,13.9933197786215,
132.316545259697)) ;
#136187 = CARTESIAN_POINT('Ctrl Pts',(-14.3391869583318,14.2183989061991,
132.494053529779)) ;
#136188 = CARTESIAN_POINT('Ctrl Pts',(-14.4064273444875,14.3876287517767,
132.723811096672)) ;
#136189 = CARTESIAN_POINT('Ctrl Pts',(-14.4845242454382,14.4861870970875,
132.984890006035)) ;
#136190 = CARTESIAN_POINT('Ctrl Pts',(-14.5685621236943,14.5095212297327,
133.263587921165)) ;
#136191 = CARTESIAN_POINT('Ctrl Pts',(-14.6509971062007,14.4547287275128,
133.537507814222)) ;
#136192 = CARTESIAN_POINT('Ctrl Pts',(-14.7254748058222,14.3261105544631,
133.788208742009)) ;
#136193 = CARTESIAN_POINT('Ctrl Pts',(-14.7858563786915,14.1327425032557,
133.997729271496)) ;
#136194 = CARTESIAN_POINT('Ctrl Pts',(-14.8271232484926,13.8885306001009,
134.151412460096)) ;
#136195 = CARTESIAN_POINT('Ctrl Pts',(-14.8454990345243,13.6107524410049,
134.23824836838)) ;
#136196 = CARTESIAN_POINT('Ctrl Pts',(-14.8391902936134,13.3210542583331,
134.252793238962)) ;
#136197 = CARTESIAN_POINT('Ctrl Pts',(-14.8073003870615,13.0351251235983,
134.193044709195)) ;
#136198 = CARTESIAN_POINT('Ctrl Pts',(-14.7526013452373,12.7816150209491,
134.066072694138)) ;
#136199 = CARTESIAN_POINT('Ctrl Pts',(-14.6768446022253,12.5706518061014,
133.878035031889)) ;
#136200 = CARTESIAN_POINT('Ctrl Pts',(-14.5857344899984,12.422091900903,133.644955346922)) ;
#136201 = CARTESIAN_POINT('Ctrl Pts',(-14.4844870236026,12.3448083833829,
133.382365111388)) ;
#136202 = CARTESIAN_POINT('Ctrl Pts',(-14.3801271179856,12.3450375607664,
133.110594842367)) ;
#136203 = CARTESIAN_POINT('Ctrl Pts',(-14.2791586916205,12.4222140372622,
132.848729115977)) ;
#136204 = CARTESIAN_POINT('Ctrl Pts',(-14.1879207671711,12.5713072693593,
132.615345977553)) ;
#136205 = CARTESIAN_POINT('Ctrl Pts',(-14.1124789413141,12.7812068465324,
132.428068113172)) ;
#136206 = CARTESIAN_POINT('Ctrl Pts',(-14.0572435650617,13.0378486801572,
132.299917089332)) ;
#136207 = CARTESIAN_POINT('Ctrl Pts',(-14.0258214639467,13.3220972424203,
132.241311719484)) ;
#136208 = CARTESIAN_POINT('Ctrl Pts',(-14.0195168117333,13.6116477161832,
132.255856984885)) ;
#136209 = CARTESIAN_POINT('Ctrl Pts',(-14.0380429091883,13.8896343949454,
132.343170883447)) ;
#136210 = CARTESIAN_POINT('Ctrl Pts',(-14.0792096341859,14.1329048293709,
132.496445041414)) ;
#136211 = CARTESIAN_POINT('Ctrl Pts',(-14.139739650008,14.3266157424045,132.706473107546)) ;
#136212 = CARTESIAN_POINT('Ctrl Pts',(-14.2142389199618,14.4550271923226,
132.957226742653)) ;
#136213 = CARTESIAN_POINT('Ctrl Pts',(-14.2968257149156,14.5094869156272,
133.231648652557)) ;
#136214 = CARTESIAN_POINT('Ctrl Pts',(-14.3803943332945,14.4863255111229,
133.508781433968)) ;
#136215 = CARTESIAN_POINT('Ctrl Pts',(-14.4590295914748,14.3868080890416,
133.771682898577)) ;
#136216 = CARTESIAN_POINT('Ctrl Pts',(-14.5257824357843,14.2186053771164,
133.999775534479)) ;
#136217 = CARTESIAN_POINT('Ctrl Pts',(-14.5755477699378,13.9916146831158,
134.17848468615)) ;
#136218 = CARTESIAN_POINT('Ctrl Pts',(-14.6033802697407,13.727139474133,134.292681268961)) ;
#136219 = CARTESIAN_POINT('Ctrl Pts',(-14.6071598535866,13.437362164295,134.337061191346)) ;
#136220 = CARTESIAN_POINT('Ctrl Pts',(-14.5858835306319,13.1504054531947,
134.307774902983)) ;
#136221 = CARTESIAN_POINT('Ctrl Pts',(-14.5396141567361,12.8786465021209,
134.206021789804)) ;
#136222 = CARTESIAN_POINT('Ctrl Pts',(-14.4723055377556,12.6500332814425,
134.042260729231)) ;
#136223 = CARTESIAN_POINT('Ctrl Pts',(-14.386841995621,12.4743183897028,133.825754806519)) ;
#136224 = CARTESIAN_POINT('Ctrl Pts',(-14.2885171909372,12.3668547922141,
133.571800387653)) ;
#136225 = CARTESIAN_POINT('Ctrl Pts',(-14.1851936733311,12.335562941567,133.302903084124)) ;
#136226 = CARTESIAN_POINT('Ctrl Pts',(-14.0817812802112,12.3817108072099,
133.033981832815)) ;
#136227 = CARTESIAN_POINT('Ctrl Pts',(-13.9856777323266,12.502839824897,132.78641286331)) ;
#136228 = CARTESIAN_POINT('Ctrl Pts',(-13.9030779122353,12.690351441453,132.578318888232)) ;
#136229 = CARTESIAN_POINT('Ctrl Pts',(-13.8395678233593,12.9285059391321,
132.425739358382)) ;
#136230 = CARTESIAN_POINT('Ctrl Pts',(-13.7979805061536,13.2046731907038,
132.337546584743)) ;
#136231 = CARTESIAN_POINT('Ctrl Pts',(-13.7814999331058,13.4951333113011,
132.322515878226)) ;
#136232 = CARTESIAN_POINT('Ctrl Pts',(-13.7900411291653,13.779501210584,132.380474347949)) ;
#136233 = CARTESIAN_POINT('Ctrl Pts',(-13.8224120698119,14.0394108332529,
132.508163412887)) ;
#136234 = CARTESIAN_POINT('Ctrl Pts',(-13.8756204987681,14.2552141196343,
132.696731438701)) ;
#136235 = CARTESIAN_POINT('Ctrl Pts',(-13.9451061652378,14.4112842226695,
132.932851180889)) ;
#136236 = CARTESIAN_POINT('Ctrl Pts',(-14.0249337755901,14.49663037618,133.199097915004)) ;
#136237 = CARTESIAN_POINT('Ctrl Pts',(-14.1095239733355,14.5049768783044,
133.479521095915)) ;
#136238 = CARTESIAN_POINT('Ctrl Pts',(-14.190528704622,14.4360835729073,133.749098498737)) ;
#136239 = CARTESIAN_POINT('Ctrl Pts',(-14.262882528703,14.2946513922982,133.993611762097)) ;
#136240 = CARTESIAN_POINT('Ctrl Pts',(-14.320142163076,14.0899140100411,134.194101738961)) ;
#136241 = CARTESIAN_POINT('Ctrl Pts',(-14.3572698390389,13.8386917046902,
134.335604381356)) ;
#136242 = CARTESIAN_POINT('Ctrl Pts',(-14.3711303129086,13.5555692125345,
134.40939671493)) ;
#136243 = CARTESIAN_POINT('Ctrl Pts',(-14.3599713476779,13.2663901180779,
134.409692119641)) ;
#136244 = CARTESIAN_POINT('Ctrl Pts',(-14.3238194723227,12.9858847333076,
134.337276500168)) ;
#136245 = CARTESIAN_POINT('Ctrl Pts',(-14.2645948958419,12.7375102459871,
134.197360749458)) ;
#136246 = CARTESIAN_POINT('Ctrl Pts',(-14.1856165305326,12.5376376287816,
133.99982702238)) ;
#136247 = CARTESIAN_POINT('Ctrl Pts',(-14.0918860241884,12.4015826977934,
133.759196205742)) ;
#136248 = CARTESIAN_POINT('Ctrl Pts',(-13.9900202965247,12.3390360902595,
133.494624163606)) ;
#136249 = CARTESIAN_POINT('Ctrl Pts',(-13.885715431319,12.353575403094,133.223035536617)) ;
#136250 = CARTESIAN_POINT('Ctrl Pts',(-13.7857334521546,12.445274073871,132.964183894283)) ;
#136251 = CARTESIAN_POINT('Ctrl Pts',(-13.6971224342536,12.6067971683827,
132.738446959323)) ;
#136252 = CARTESIAN_POINT('Ctrl Pts',(-13.6250522220287,12.8274892534517,
132.561122252927)) ;
#136253 = CARTESIAN_POINT('Ctrl Pts',(-13.5744828714336,13.0891408927057,
132.446378055787)) ;
#136254 = CARTESIAN_POINT('Ctrl Pts',(-13.547610803124,13.375740122579,132.401005590542)) ;
#136255 = CARTESIAN_POINT('Ctrl Pts',(-13.5460300274622,13.6659116032671,
132.429533614848)) ;
#136256 = CARTESIAN_POINT('Ctrl Pts',(-13.5689788396593,13.9383430672958,
132.529666742918)) ;
#136257 = CARTESIAN_POINT('Ctrl Pts',(-13.6144336268274,14.1747318786697,
132.695698796106)) ;
#136258 = CARTESIAN_POINT('Ctrl Pts',(-13.6775346028895,14.3556000224366,
132.912954043635)) ;
#136259 = CARTESIAN_POINT('Ctrl Pts',(-13.7545609195232,14.4715471852787,
133.171333891809)) ;
#136260 = CARTESIAN_POINT('Ctrl Pts',(-13.8375768659038,14.5109306884899,
133.446859569505)) ;
#136261 = CARTESIAN_POINT('Ctrl Pts',(-13.9206587334674,14.4734197510009,
133.722575921601)) ;
#136262 = CARTESIAN_POINT('Ctrl Pts',(-13.9978549774587,14.3595613312843,
133.981405064546)) ;
#136263 = CARTESIAN_POINT('Ctrl Pts',(-14.0615326101247,14.179466171533,134.200463448237)) ;
#136264 = CARTESIAN_POINT('Ctrl Pts',(-14.1072808462681,13.9455181185487,
134.367173049305)) ;
#136265 = CARTESIAN_POINT('Ctrl Pts',(-14.1309695714097,13.6723045745694,
134.469654422256)) ;
#136266 = CARTESIAN_POINT('Ctrl Pts',(-14.1299543421008,13.3834915874396,
134.49969517271)) ;
#136267 = CARTESIAN_POINT('Ctrl Pts',(-14.103826459953,13.0966134068724,134.456484806691)) ;
#136268 = CARTESIAN_POINT('Ctrl Pts',(-14.0536044519402,12.8330521051259,
134.342891801889)) ;
#136269 = CARTESIAN_POINT('Ctrl Pts',(-13.9819755458689,12.6112324338377,
134.166849542491)) ;
#136270 = CARTESIAN_POINT('Ctrl Pts',(-13.8936140788126,12.4482429025448,
133.941863276773)) ;
#136271 = CARTESIAN_POINT('Ctrl Pts',(-13.7945442209898,12.3553252392396,
133.68544189025)) ;
#136272 = CARTESIAN_POINT('Ctrl Pts',(-13.6902421881023,12.3382107107946,
133.413874998198)) ;
#136273 = CARTESIAN_POINT('Ctrl Pts',(-13.5876395250276,12.3992481458877,
133.147344273434)) ;
#136274 = CARTESIAN_POINT('Ctrl Pts',(-13.4940363967205,12.5331204758664,
132.906945186053)) ;
#136275 = CARTESIAN_POINT('Ctrl Pts',(-13.4146406339235,12.7309387918669,
132.708143521826)) ;
#136276 = CARTESIAN_POINT('Ctrl Pts',(-13.3546400489765,12.9791524410526,
132.566084041094)) ;
#136277 = CARTESIAN_POINT('Ctrl Pts',(-13.3178749195276,13.2585790598106,
132.491812795079)) ;
#136278 = CARTESIAN_POINT('Ctrl Pts',(-13.3060921658157,13.5499397896395,
132.490544550928)) ;
#136279 = CARTESIAN_POINT('Ctrl Pts',(-13.319267039209,13.8311712407388,132.562048975874)) ;
#136280 = CARTESIAN_POINT('Ctrl Pts',(-13.3560394645477,14.0848085651835,
132.702709571436)) ;
#136281 = CARTESIAN_POINT('Ctrl Pts',(-13.4124077844404,14.2892041446737,
132.900320701676)) ;
#136282 = CARTESIAN_POINT('Ctrl Pts',(-13.4844837717321,14.4332159069687,
133.144089592404)) ;
#136283 = CARTESIAN_POINT('Ctrl Pts',(-13.5657740695195,14.5042073782218,
133.414672215616)) ;
#136284 = CARTESIAN_POINT('Ctrl Pts',(-13.6499188668072,14.4978850554144,
133.693611525571)) ;
#136285 = CARTESIAN_POINT('Ctrl Pts',(-13.7301300690243,14.4145534025925,
133.96105201458)) ;
#136286 = CARTESIAN_POINT('Ctrl Pts',(-13.7999841881705,14.2600830965558,
134.198257775645)) ;
#136287 = CARTESIAN_POINT('Ctrl Pts',(-13.8535974701144,14.0459659620245,
134.387963859614)) ;
#136288 = CARTESIAN_POINT('Ctrl Pts',(-13.8866069561238,13.7875807752627,
134.517459877776)) ;
#136289 = CARTESIAN_POINT('Ctrl Pts',(-13.8958448391708,13.5015008973902,
134.577698082975)) ;
#136290 = CARTESIAN_POINT('Ctrl Pts',(-13.8799187621032,13.2119712102584,
134.564171528529)) ;
#136291 = CARTESIAN_POINT('Ctrl Pts',(-13.8392809382772,12.9363053782512,
134.478593815727)) ;
#136292 = CARTESIAN_POINT('Ctrl Pts',(-13.7758444278724,12.6952736602129,
134.326473645072)) ;
#136293 = CARTESIAN_POINT('Ctrl Pts',(-13.6940162958856,12.507125678723,134.120477732686)) ;
#136294 = CARTESIAN_POINT('Ctrl Pts',(-13.5977907900013,12.3837628513247,
133.872694312529)) ;
#136295 = CARTESIAN_POINT('Ctrl Pts',(-13.4952077550757,12.3357954087756,
133.605958381013)) ;
#136296 = CARTESIAN_POINT('Ctrl Pts',(-13.3909244959306,12.3652711251859,
133.33454614811)) ;
#136297 = CARTESIAN_POINT('Ctrl Pts',(-13.2930291637441,12.4705156806676,
133.081632751708)) ;
#136298 = CARTESIAN_POINT('Ctrl Pts',(-13.2071658759881,12.6439184973371,
132.863918116231)) ;
#136299 = CARTESIAN_POINT('Ctrl Pts',(-13.1389101581012,12.8730354055636,
132.697626362)) ;
#136300 = CARTESIAN_POINT('Ctrl Pts',(-13.0923226075365,13.1424159445997,
132.594737929481)) ;
#136301 = CARTESIAN_POINT('Ctrl Pts',(-13.0702865542668,13.4306391754528,
132.563415021775)) ;
#136302 = CARTESIAN_POINT('Ctrl Pts',(-13.0733966131089,13.7191539441457,
132.605650335791)) ;
#136303 = CARTESIAN_POINT('Ctrl Pts',(-13.1008205861734,13.9861293896989,
132.718874470187)) ;
#136304 = CARTESIAN_POINT('Ctrl Pts',(-13.1498037441585,14.2128684001206,
132.89508138218)) ;
#136305 = CARTESIAN_POINT('Ctrl Pts',(-13.2163126321001,14.3833347965248,
133.122557153896)) ;
#136306 = CARTESIAN_POINT('Ctrl Pts',(-13.2945517934649,14.4845639099252,
133.384224457738)) ;
#136307 = CARTESIAN_POINT('Ctrl Pts',(-13.3782996834148,14.5099092471542,
133.66197841254)) ;
#136308 = CARTESIAN_POINT('Ctrl Pts',(-13.4610067103196,14.4573341215463,
133.936748595732)) ;
#136309 = CARTESIAN_POINT('Ctrl Pts',(-13.535792979438,14.3305258270945,134.188357582262)) ;
#136310 = CARTESIAN_POINT('Ctrl Pts',(-13.5964938791261,14.1393930806654,
134.398720829303)) ;
#136311 = CARTESIAN_POINT('Ctrl Pts',(-13.6384531516596,13.8963012865058,
134.554456038958)) ;
#136312 = CARTESIAN_POINT('Ctrl Pts',(-13.6575588644819,13.618527952916,134.64350061979)) ;
#136313 = CARTESIAN_POINT('Ctrl Pts',(-13.6518640795297,13.3290638567204,
134.659826711564)) ;
#136314 = CARTESIAN_POINT('Ctrl Pts',(-13.6210222993908,13.0445549081066,
134.602903919085)) ;
#136315 = CARTESIAN_POINT('Ctrl Pts',(-13.5665781809899,12.7876683953407,
134.476958833009)) ;
#136316 = CARTESIAN_POINT('Ctrl Pts',(-13.4911864112069,12.5753843248543,
134.290002560966)) ;
#136317 = CARTESIAN_POINT('Ctrl Pts',(-13.4007901006825,12.4255194566962,
134.05888370733)) ;
#136318 = CARTESIAN_POINT('Ctrl Pts',(-13.2997237377735,12.3459765628223,
133.796830310285)) ;
#136319 = CARTESIAN_POINT('Ctrl Pts',(-13.1954991747945,12.3439073333341,
133.52541389548)) ;
#136320 = CARTESIAN_POINT('Ctrl Pts',(-13.0941541677024,12.4188279963137,
133.262499854551)) ;
#136321 = CARTESIAN_POINT('Ctrl Pts',(-13.002205997662,12.5669347456838,133.027188569075)) ;
#136322 = CARTESIAN_POINT('Ctrl Pts',(-12.9267422753913,12.7740276750078,
132.839635132885)) ;
#136323 = CARTESIAN_POINT('Ctrl Pts',(-12.8706659445136,13.0302839963835,
132.709131418789)) ;
#136324 = CARTESIAN_POINT('Ctrl Pts',(-12.8386183811773,13.3133908418281,
132.648618515674)) ;
#136325 = CARTESIAN_POINT('Ctrl Pts',(-12.8315791622469,13.603463644202,132.661074904967)) ;
#136326 = CARTESIAN_POINT('Ctrl Pts',(-12.8492844367411,13.8813033828735,
132.745878981524)) ;
#136327 = CARTESIAN_POINT('Ctrl Pts',(-12.8901906349179,14.1277803353935,
132.898667421918)) ;
#136328 = CARTESIAN_POINT('Ctrl Pts',(-12.9502027043241,14.3222499491186,
133.107092668811)) ;
#136329 = CARTESIAN_POINT('Ctrl Pts',(-13.0241102247799,14.4521801137134,
133.356004116762)) ;
#136330 = CARTESIAN_POINT('Ctrl Pts',(-13.1064456796044,14.5090397013049,
133.629648846685)) ;
#136331 = CARTESIAN_POINT('Ctrl Pts',(-13.1904091031337,14.4879536383768,
133.908074847443)) ;
#136332 = CARTESIAN_POINT('Ctrl Pts',(-13.2691730073198,14.3907169193799,
134.171290632638)) ;
#136333 = CARTESIAN_POINT('Ctrl Pts',(-13.3365717682159,14.2230874926912,
134.401446847104)) ;
#136334 = CARTESIAN_POINT('Ctrl Pts',(-13.3862837725614,14.0008521290395,
134.579526433076)) ;
#136335 = CARTESIAN_POINT('Ctrl Pts',(-13.4151850077251,13.7343152663338,
134.697246128251)) ;
#136336 = CARTESIAN_POINT('Ctrl Pts',(-13.4196674461843,13.4474451530714,
134.74336669151)) ;
#136337 = CARTESIAN_POINT('Ctrl Pts',(-13.3989374427175,13.1575373599845,
134.716000021385)) ;
#136338 = CARTESIAN_POINT('Ctrl Pts',(-13.3538701206744,12.8878586186382,
134.617383543723)) ;
#136339 = CARTESIAN_POINT('Ctrl Pts',(-13.2866697814604,12.6555337160297,
134.454240239388)) ;
#136340 = CARTESIAN_POINT('Ctrl Pts',(-13.2016717965965,12.4784852863875,
134.239051541609)) ;
#136341 = CARTESIAN_POINT('Ctrl Pts',(-13.103660140851,12.3688435126028,133.986006271584)) ;
#136342 = CARTESIAN_POINT('Ctrl Pts',(-13.0001912147535,12.335379050582,133.716752546929)) ;
#136343 = CARTESIAN_POINT('Ctrl Pts',(-12.8968764365744,12.3794309050292,
133.448054757706)) ;
#136344 = CARTESIAN_POINT('Ctrl Pts',(-12.8007211226384,12.4979553005814,
133.200237570607)) ;
#136345 = CARTESIAN_POINT('Ctrl Pts',(-12.7173411751848,12.6843641512771,
132.989987119788)) ;
#136346 = CARTESIAN_POINT('Ctrl Pts',(-12.6533675978781,12.9208195190715,
132.835987884663)) ;
#136347 = CARTESIAN_POINT('Ctrl Pts',(-12.6110523141971,13.1965599156971,
132.745711948575)) ;
#136348 = CARTESIAN_POINT('Ctrl Pts',(-12.5938677361115,13.4854150034454,
132.728459041513)) ;
#136349 = CARTESIAN_POINT('Ctrl Pts',(-12.6016166796287,13.7715245103546,
132.784247690811)) ;
#136350 = CARTESIAN_POINT('Ctrl Pts',(-12.6334808333027,14.0329603333754,
132.910531351478)) ;
#136351 = CARTESIAN_POINT('Ctrl Pts',(-12.6860159227242,14.2495174070446,
133.097035811552)) ;
#136352 = CARTESIAN_POINT('Ctrl Pts',(-12.7550120282424,14.4077221355952,
133.331704202413)) ;
#136353 = CARTESIAN_POINT('Ctrl Pts',(-12.8352852858367,14.4954974794661,
133.599515576589)) ;
#136354 = CARTESIAN_POINT('Ctrl Pts',(-12.9190639071468,14.5058124227374,
133.877251814252)) ;
#136355 = CARTESIAN_POINT('Ctrl Pts',(-13.0006861903333,14.4390540160987,
134.148810770118)) ;
#136356 = CARTESIAN_POINT('Ctrl Pts',(-13.0734798970183,14.2988995016989,
134.394674718231)) ;
#136357 = CARTESIAN_POINT('Ctrl Pts',(-13.1310605574008,14.0959846822767,
134.59603545551)) ;
#136358 = CARTESIAN_POINT('Ctrl Pts',(-13.1686602075177,13.8467238077785,
134.738805253809)) ;
#136359 = CARTESIAN_POINT('Ctrl Pts',(-13.1832960063071,13.5651499595772,
134.814759605636)) ;
#136360 = CARTESIAN_POINT('Ctrl Pts',(-13.1728859358929,13.2745210705863,
134.817404454761)) ;
#136361 = CARTESIAN_POINT('Ctrl Pts',(-13.1372979957402,12.9930481847516,
134.746685223495)) ;
#136362 = CARTESIAN_POINT('Ctrl Pts',(-13.0788464460579,12.7442685275202,
134.608933005347)) ;
#136363 = CARTESIAN_POINT('Ctrl Pts',(-13.0004860021476,12.5428869624623,
134.413170014133)) ;
#136364 = CARTESIAN_POINT('Ctrl Pts',(-12.9071846487547,12.4047083280592,
134.173773807101)) ;
#136365 = CARTESIAN_POINT('Ctrl Pts',(-12.8051561028839,12.3396945526809,
133.90883173255)) ;
#136366 = CARTESIAN_POINT('Ctrl Pts',(-12.7008909970313,12.3521469576885,
133.637337257152)) ;
#136367 = CARTESIAN_POINT('Ctrl Pts',(-12.6009173642389,12.441314353945,133.378426035197)) ;
#136368 = CARTESIAN_POINT('Ctrl Pts',(-12.5117677396135,12.6011043288198,
133.151163527727)) ;
#136369 = CARTESIAN_POINT('Ctrl Pts',(-12.4393294114449,12.8194224397463,
132.97265105268)) ;
#136370 = CARTESIAN_POINT('Ctrl Pts',(-12.387790426931,13.0811434342732,132.85522288076)) ;
#136371 = CARTESIAN_POINT('Ctrl Pts',(-12.360228261411,13.3679217852881,132.807894792067)) ;
#136372 = CARTESIAN_POINT('Ctrl Pts',(-12.3579523050129,13.6574454003315,
132.834298017918)) ;
#136373 = CARTESIAN_POINT('Ctrl Pts',(-12.3801380175334,13.9304218890574,
132.932167779584)) ;
#136374 = CARTESIAN_POINT('Ctrl Pts',(-12.4250230602689,14.1686008595605,
133.096583317216)) ;
#136375 = CARTESIAN_POINT('Ctrl Pts',(-12.4878388913045,14.3514046814191,
133.313074404504)) ;
#136376 = CARTESIAN_POINT('Ctrl Pts',(-12.5640867721586,14.4688537010489,
133.568976881112)) ;
#136377 = CARTESIAN_POINT('Ctrl Pts',(-12.6473280614042,14.5110084065472,
133.845298914204)) ;
#136378 = CARTESIAN_POINT('Ctrl Pts',(-12.7306234368668,14.4754271659884,
134.121689851781)) ;
#136379 = CARTESIAN_POINT('Ctrl Pts',(-12.8078424891508,14.3641624802179,
134.38046802569)) ;
#136380 = CARTESIAN_POINT('Ctrl Pts',(-12.8722362238059,14.1852632695012,
134.601742519835)) ;
#136381 = CARTESIAN_POINT('Ctrl Pts',(-12.9184596429682,13.9526451401233,
134.769816657982)) ;
#136382 = CARTESIAN_POINT('Ctrl Pts',(-12.9427606566985,13.6818447118076,
134.873904342633)) ;
#136383 = CARTESIAN_POINT('Ctrl Pts',(-12.9426329031674,13.3926206452482,
134.906615051885)) ;
#136384 = CARTESIAN_POINT('Ctrl Pts',(-12.9170454040847,13.1038754923078,
134.865156068369)) ;
#136385 = CARTESIAN_POINT('Ctrl Pts',(-12.8675913433402,12.8403836297391,
134.753690916011)) ;
#136386 = CARTESIAN_POINT('Ctrl Pts',(-12.7967823441445,12.6175434576375,
134.579955954179)) ;
#136387 = CARTESIAN_POINT('Ctrl Pts',(-12.70868276548,12.4520178789147,134.355810149669)) ;
#136388 = CARTESIAN_POINT('Ctrl Pts',(-12.6093449823904,12.3567780608222,
134.098765452035)) ;
#136389 = CARTESIAN_POINT('Ctrl Pts',(-12.5056341234011,12.3376561109864,
133.828749759816)) ;
#136390 = CARTESIAN_POINT('Ctrl Pts',(-12.402751079868,12.3963494804203,133.561441007829)) ;
#136391 = CARTESIAN_POINT('Ctrl Pts',(-12.3088084112223,12.5282529228556,
133.320050046839)) ;
#136392 = CARTESIAN_POINT('Ctrl Pts',(-12.2289334019483,12.7243873042916,
133.119846376778)) ;
#136393 = CARTESIAN_POINT('Ctrl Pts',(-12.1683661165357,12.9708923918956,
132.976071926915)) ;
#136394 = CARTESIAN_POINT('Ctrl Pts',(-12.1308341182304,13.2502126197918,
132.899629391339)) ;
#136395 = CARTESIAN_POINT('Ctrl Pts',(-12.1182778756421,13.5400583828972,
132.895929792219)) ;
#136396 = CARTESIAN_POINT('Ctrl Pts',(-12.1307869570981,13.8239338286533,
132.965735493257)) ;
#136397 = CARTESIAN_POINT('Ctrl Pts',(-12.1668484142908,14.0777676729547,
133.104202368024)) ;
#136398 = CARTESIAN_POINT('Ctrl Pts',(-12.222772912384,14.2841378500946,133.300577303525)) ;
#136399 = CARTESIAN_POINT('Ctrl Pts',(-12.2942910489215,14.429815657766,133.542627629611)) ;
#136400 = CARTESIAN_POINT('Ctrl Pts',(-12.3756729115768,14.5033259168077,
133.813595342621)) ;
#136401 = CARTESIAN_POINT('Ctrl Pts',(-12.4597832810724,14.499135115111,134.092410952893)) ;
#136402 = CARTESIAN_POINT('Ctrl Pts',(-12.5402566051309,14.4177798325381,
134.360648411857)) ;
#136403 = CARTESIAN_POINT('Ctrl Pts',(-12.6102648440973,14.2657377102023,
134.59819459311)) ;
#136404 = CARTESIAN_POINT('Ctrl Pts',(-12.6646057115603,14.0527574173429,
134.790109616224)) ;
#136405 = CARTESIAN_POINT('Ctrl Pts',(-12.6982822917971,13.7942044324148,
134.921686113269)) ;
#136406 = CARTESIAN_POINT('Ctrl Pts',(-12.7081236290535,13.509972220369,134.983521067054)) ;
#136407 = CARTESIAN_POINT('Ctrl Pts',(-12.6929226435767,13.219834764377,134.972169824304)) ;
#136408 = CARTESIAN_POINT('Ctrl Pts',(-12.6529041959642,12.9433154987134,
134.888419817773)) ;
#136409 = CARTESIAN_POINT('Ctrl Pts',(-12.5899125810331,12.7008042356819,
134.737648548155)) ;
#136410 = CARTESIAN_POINT('Ctrl Pts',(-12.5088132067507,12.5118988342583,
134.533656568728)) ;
#136411 = CARTESIAN_POINT('Ctrl Pts',(-12.4134247671775,12.3867144480253,
134.288156510762)) ;
#136412 = CARTESIAN_POINT('Ctrl Pts',(-12.3103723850424,12.3359851161897,
134.020244487105)) ;
#136413 = CARTESIAN_POINT('Ctrl Pts',(-12.2060535029749,12.3634203970633,
133.748717660543)) ;
#136414 = CARTESIAN_POINT('Ctrl Pts',(-12.1079177935451,12.4663876358086,
133.495088507556)) ;
#136415 = CARTESIAN_POINT('Ctrl Pts',(-12.0212873996097,12.6389701182042,
133.275282296474)) ;
#136416 = CARTESIAN_POINT('Ctrl Pts',(-11.9528459850857,12.8657474577828,
133.108290126159)) ;
#136417 = CARTESIAN_POINT('Ctrl Pts',(-11.9054705654115,13.1346343436699,
133.003152675926)) ;
#136418 = CARTESIAN_POINT('Ctrl Pts',(-11.8903642795437,13.3266512177486,
132.98106317886)) ;
#136419 = CARTESIAN_POINT('Ctrl Pts',(-11.8869647971046,13.4226801736581,
132.982153164817)) ;
#136420 = CARTESIAN_POINT('Ctrl Pts',(-33.3254395351173,13.1734341962953,
127.803113044878)) ;
#136421 = CARTESIAN_POINT('Ctrl Pts',(-33.3247359866207,13.1676985117492,
127.801788763031)) ;
#136422 = CARTESIAN_POINT('Ctrl Pts',(-33.3132623631218,13.0762045259503,
127.779953878293)) ;
#136423 = CARTESIAN_POINT('Ctrl Pts',(-33.282285149324,12.9034782773047,127.712436580561)) ;
#136424 = CARTESIAN_POINT('Ctrl Pts',(-33.2176093851333,12.6923998391673,
127.556524920366)) ;
#136425 = CARTESIAN_POINT('Ctrl Pts',(-33.1366442117355,12.5327609209973,
127.353111300579)) ;
#136426 = CARTESIAN_POINT('Ctrl Pts',(-33.0439865108413,12.4368205813749,
127.115708366726)) ;
#136427 = CARTESIAN_POINT('Ctrl Pts',(-32.9470466339548,12.4119420222618,
126.865451857032)) ;
#136428 = CARTESIAN_POINT('Ctrl Pts',(-32.8502205148306,12.4592681303251,
126.615824485106)) ;
#136429 = CARTESIAN_POINT('Ctrl Pts',(-32.7609435571221,12.5756589901857,
126.388116095926)) ;
#136430 = CARTESIAN_POINT('Ctrl Pts',(-32.6843652232408,12.7528353501054,
126.197555194626)) ;
#136431 = CARTESIAN_POINT('Ctrl Pts',(-32.6254359841591,12.9779970726337,
126.058531505893)) ;
#136432 = CARTESIAN_POINT('Ctrl Pts',(-32.5876159994447,13.2349353323575,
125.981163983675)) ;
#136433 = CARTESIAN_POINT('Ctrl Pts',(-32.5727992859682,13.5051817925228,
125.970971172671)) ;
#136434 = CARTESIAN_POINT('Ctrl Pts',(-32.5815223767738,13.7710455478253,
126.029743179252)) ;
#136435 = CARTESIAN_POINT('Ctrl Pts',(-32.6121127150153,14.0095405119009,
126.15206688756)) ;
#136436 = CARTESIAN_POINT('Ctrl Pts',(-32.6618848688714,14.207375982779,126.330592997822)) ;
#136437 = CARTESIAN_POINT('Ctrl Pts',(-32.7265064202986,14.3489569036635,
126.552483435506)) ;
#136438 = CARTESIAN_POINT('Ctrl Pts',(-32.8008290640631,14.4243647348289,
126.802810757179)) ;
#136439 = CARTESIAN_POINT('Ctrl Pts',(-32.8783902118096,14.4276726167065,
127.062506054467)) ;
#136440 = CARTESIAN_POINT('Ctrl Pts',(-32.9529895057271,14.3592846174027,
127.313499396792)) ;
#136441 = CARTESIAN_POINT('Ctrl Pts',(-33.0187620925496,14.2239083327593,
127.538741069416)) ;
#136442 = CARTESIAN_POINT('Ctrl Pts',(-33.0702809219999,14.0309432296264,
127.722391722539)) ;
#136443 = CARTESIAN_POINT('Ctrl Pts',(-33.1029915194089,13.793723337017,127.851172033353)) ;
#136444 = CARTESIAN_POINT('Ctrl Pts',(-33.1137372251236,13.531837086658,127.915541813163)) ;
#136445 = CARTESIAN_POINT('Ctrl Pts',(-33.1012954087164,13.2609089527483,
127.912338104309)) ;
#136446 = CARTESIAN_POINT('Ctrl Pts',(-33.0654710758441,13.0011532245151,
127.840894256415)) ;
#136447 = CARTESIAN_POINT('Ctrl Pts',(-33.0086291360852,12.7729628061281,
127.707856012819)) ;
#136448 = CARTESIAN_POINT('Ctrl Pts',(-32.9334589590993,12.5901802135074,
127.521462919618)) ;
#136449 = CARTESIAN_POINT('Ctrl Pts',(-32.8452372911632,12.4676468179757,
127.296813129222)) ;
#136450 = CARTESIAN_POINT('Ctrl Pts',(-32.74883806695,12.4133145081089,127.048434581224)) ;
#136451 = CARTESIAN_POINT('Ctrl Pts',(-32.651505357267,12.4313808819739,126.797103381314)) ;
#136452 = CARTESIAN_POINT('Ctrl Pts',(-32.5582583386558,12.520660304575,126.557917651661)) ;
#136453 = CARTESIAN_POINT('Ctrl Pts',(-32.4760025184329,12.6744195620442,
126.350716856275)) ;
#136454 = CARTESIAN_POINT('Ctrl Pts',(-32.4094362840527,12.8815892822748,
126.189358896427)) ;
#136455 = CARTESIAN_POINT('Ctrl Pts',(-32.3625474664159,13.1290193057785,
126.085663140554)) ;
#136456 = CARTESIAN_POINT('Ctrl Pts',(-32.3384651461866,13.3950772223713,
126.048272145446)) ;
#136457 = CARTESIAN_POINT('Ctrl Pts',(-32.3375813691581,13.66434219871,126.078804798388)) ;
#136458 = CARTESIAN_POINT('Ctrl Pts',(-32.3596574822361,13.9170737503532,
126.176511056621)) ;
#136459 = CARTESIAN_POINT('Ctrl Pts',(-32.4021492792394,14.1334228182709,
126.333728828426)) ;
#136460 = CARTESIAN_POINT('Ctrl Pts',(-32.4612401199057,14.2989215662944,
126.539406409158)) ;
#136461 = CARTESIAN_POINT('Ctrl Pts',(-32.5321839761624,14.4021434485844,
126.779768376024)) ;
#136462 = CARTESIAN_POINT('Ctrl Pts',(-32.6093004013496,14.4351203020035,
127.038251205167)) ;
#136463 = CARTESIAN_POINT('Ctrl Pts',(-32.685749140631,14.3956460292368,127.294619936752)) ;
#136464 = CARTESIAN_POINT('Ctrl Pts',(-32.7559987732593,14.2864256382767,
127.533007359851)) ;
#136465 = CARTESIAN_POINT('Ctrl Pts',(-32.8139294455932,14.1149876156061,
127.735413101504)) ;
#136466 = CARTESIAN_POINT('Ctrl Pts',(-32.8545469809948,13.8950778859157,
127.887084365748)) ;
#136467 = CARTESIAN_POINT('Ctrl Pts',(-32.8745963697914,13.6402949383964,
127.97883429511)) ;
#136468 = CARTESIAN_POINT('Ctrl Pts',(-32.8716009144099,13.3700135586503,
128.003243267968)) ;
#136469 = CARTESIAN_POINT('Ctrl Pts',(-32.8451817708658,13.1040821018971,
127.959163781802)) ;
#136470 = CARTESIAN_POINT('Ctrl Pts',(-32.7965610116962,12.8608604058745,
127.850228031512)) ;
#136471 = CARTESIAN_POINT('Ctrl Pts',(-32.7280100000708,12.6570995861258,
127.683237242378)) ;
#136472 = CARTESIAN_POINT('Ctrl Pts',(-32.6448060717616,12.5097126273575,
127.473139968475)) ;
#136473 = CARTESIAN_POINT('Ctrl Pts',(-32.5510193789591,12.4266925864004,
127.23233405547)) ;
#136474 = CARTESIAN_POINT('Ctrl Pts',(-32.4532256004834,12.4153566077392,
126.979772250946)) ;
#136475 = CARTESIAN_POINT('Ctrl Pts',(-32.3576194837689,12.4761183331586,
126.73359550688)) ;
#136476 = CARTESIAN_POINT('Ctrl Pts',(-32.2703085357419,12.6046109786899,
126.511640612033)) ;
#136477 = CARTESIAN_POINT('Ctrl Pts',(-32.1966708395862,12.792032892229,126.32968693581)) ;
#136478 = CARTESIAN_POINT('Ctrl Pts',(-32.141491025989,13.0246459231079,126.201630976747)) ;
#136479 = CARTESIAN_POINT('Ctrl Pts',(-32.1079590635852,13.2849675496699,
126.136714360042)) ;
#136480 = CARTESIAN_POINT('Ctrl Pts',(-32.0975331597763,13.5561838423073,
126.139422059227)) ;
#136481 = CARTESIAN_POINT('Ctrl Pts',(-32.1105557909978,13.8182129454441,
126.210683763545)) ;
#136482 = CARTESIAN_POINT('Ctrl Pts',(-32.1449979162491,14.0504673994418,
126.344307337019)) ;
#136483 = CARTESIAN_POINT('Ctrl Pts',(-32.1981332617765,14.2392687956967,
126.532766020785)) ;
#136484 = CARTESIAN_POINT('Ctrl Pts',(-32.2650887614462,14.3686948710642,
126.761498858709)) ;
#136485 = CARTESIAN_POINT('Ctrl Pts',(-32.3399771946658,14.4303698610576,
127.013234105376)) ;
#136486 = CARTESIAN_POINT('Ctrl Pts',(-32.4176418524857,14.4203874495029,
127.273299867643)) ;
#136487 = CARTESIAN_POINT('Ctrl Pts',(-32.4913827908126,14.3383234433453,
127.521952665853)) ;
#136488 = CARTESIAN_POINT('Ctrl Pts',(-32.5547753616378,14.1909247439309,
127.740243611178)) ;
#136489 = CARTESIAN_POINT('Ctrl Pts',(-32.6027829052078,13.9894772519221,
127.913477677594)) ;
#136490 = CARTESIAN_POINT('Ctrl Pts',(-32.6315787822835,13.7468083909025,
128.030718638725)) ;
#136491 = CARTESIAN_POINT('Ctrl Pts',(-32.6381297055454,13.4802543553281,
128.083052077669)) ;
#136492 = CARTESIAN_POINT('Ctrl Pts',(-32.621004032577,13.2092851257182,128.066265392245)) ;
#136493 = CARTESIAN_POINT('Ctrl Pts',(-32.5813816261219,12.956342695595,127.983398583339)) ;
#136494 = CARTESIAN_POINT('Ctrl Pts',(-32.5205209542112,12.7340443035837,
127.838851944066)) ;
#136495 = CARTESIAN_POINT('Ctrl Pts',(-32.4424022518424,12.5620254475304,
127.643824006467)) ;
#136496 = CARTESIAN_POINT('Ctrl Pts',(-32.3525984203938,12.45216345603,127.414440626927)) ;
#136497 = CARTESIAN_POINT('Ctrl Pts',(-32.2552772387971,12.4110698281944,
127.163418282472)) ;
#136498 = CARTESIAN_POINT('Ctrl Pts',(-32.1580021613722,12.4431134785041,
126.912378453322)) ;
#136499 = CARTESIAN_POINT('Ctrl Pts',(-32.0668852322613,12.544720783163,126.679216971146)) ;
#136500 = CARTESIAN_POINT('Ctrl Pts',(-31.9870500616397,12.7094608170751,
126.479131976701)) ;
#136501 = CARTESIAN_POINT('Ctrl Pts',(-31.9237909814612,12.9261933498066,
126.32756494422)) ;
#136502 = CARTESIAN_POINT('Ctrl Pts',(-31.8812909269055,13.1767718308822,
126.236400480011)) ;
#136503 = CARTESIAN_POINT('Ctrl Pts',(-31.861298454265,13.4474343048381,126.211302126729)) ;
#136504 = CARTESIAN_POINT('Ctrl Pts',(-31.8650124128939,13.7143157453809,
126.255202512803)) ;
#136505 = CARTESIAN_POINT('Ctrl Pts',(-31.8909286602407,13.9601208806252,
126.363903867448)) ;
#136506 = CARTESIAN_POINT('Ctrl Pts',(-31.9370786723428,14.1691500146303,
126.531977690957)) ;
#136507 = CARTESIAN_POINT('Ctrl Pts',(-31.9987411279638,14.3234012813758,
126.74512586519)) ;
#136508 = CARTESIAN_POINT('Ctrl Pts',(-32.0713879414062,14.4138714388817,
126.990519088113)) ;
#136509 = CARTESIAN_POINT('Ctrl Pts',(-32.1486213371649,14.433295070235,127.249205234635)) ;
#136510 = CARTESIAN_POINT('Ctrl Pts',(-32.2249233067821,14.3798377067091,
127.505417902984)) ;
#136511 = CARTESIAN_POINT('Ctrl Pts',(-32.292842495317,14.2584887860387,127.736813241794)) ;
#136512 = CARTESIAN_POINT('Ctrl Pts',(-32.3478706736015,14.0772215251275,
127.930687195659)) ;
#136513 = CARTESIAN_POINT('Ctrl Pts',(-32.385043591268,13.847858128252,128.072541376849)) ;
#136514 = CARTESIAN_POINT('Ctrl Pts',(-32.4006697912098,13.5896600373134,
128.151227440308)) ;
#136515 = CARTESIAN_POINT('Ctrl Pts',(-32.3933293828918,13.3195390353182,
128.162833702852)) ;
#136516 = CARTESIAN_POINT('Ctrl Pts',(-32.362503604888,13.0556171631187,128.105986435172)) ;
#136517 = CARTESIAN_POINT('Ctrl Pts',(-32.3099087281082,12.8189344364704,
127.985427645554)) ;
#136518 = CARTESIAN_POINT('Ctrl Pts',(-32.2383978311714,12.6251004110513,
127.809670253998)) ;
#136519 = CARTESIAN_POINT('Ctrl Pts',(-32.1525576056768,12.4887479855771,
127.592000333581)) ;
#136520 = CARTESIAN_POINT('Ctrl Pts',(-32.0577945487542,12.419067054962,127.348242601568)) ;
#136521 = CARTESIAN_POINT('Ctrl Pts',(-31.9596036759549,12.4213699638912,
127.094633590444)) ;
#136522 = CARTESIAN_POINT('Ctrl Pts',(-31.8652480188587,12.4953802031986,
126.852058359587)) ;
#136523 = CARTESIAN_POINT('Ctrl Pts',(-31.7800198291274,12.6359571478174,
126.636236452674)) ;
#136524 = CARTESIAN_POINT('Ctrl Pts',(-31.7096390960426,12.8329196540899,
126.463760566805)) ;
#136525 = CARTESIAN_POINT('Ctrl Pts',(-31.6583487363999,13.0719648930025,
126.347032519857)) ;
#136526 = CARTESIAN_POINT('Ctrl Pts',(-31.6290353321278,13.3363496355774,
126.294530496598)) ;
#136527 = CARTESIAN_POINT('Ctrl Pts',(-31.6231309158897,13.6070576006529,
126.310423983356)) ;
#136528 = CARTESIAN_POINT('Ctrl Pts',(-31.6403386798103,13.8644611285128,
126.393821576157)) ;
#136529 = CARTESIAN_POINT('Ctrl Pts',(-31.6786205812712,14.0900772537897,
126.53875012761)) ;
#136530 = CARTESIAN_POINT('Ctrl Pts',(-31.7346571079609,14.2682172289019,
126.735603420313)) ;
#136531 = CARTESIAN_POINT('Ctrl Pts',(-31.803393598769,14.3854165946879,126.969447305855)) ;
#136532 = CARTESIAN_POINT('Ctrl Pts',(-31.8795398028215,14.4341663213204,
127.225014629057)) ;
#136533 = CARTESIAN_POINT('Ctrl Pts',(-31.9569737821743,14.4102121337139,
127.484427730781)) ;
#136534 = CARTESIAN_POINT('Ctrl Pts',(-32.0289551185517,14.3156229192553,
127.727797868407)) ;
#136535 = CARTESIAN_POINT('Ctrl Pts',(-32.0899457704392,14.1571117362938,
127.939092933894)) ;
#136536 = CARTESIAN_POINT('Ctrl Pts',(-32.1347596628421,13.9459764077607,
128.103131375364)) ;
#136537 = CARTESIAN_POINT('Ctrl Pts',(-32.1594663640903,13.6975622322246,
128.208410639942)) ;
#136538 = CARTESIAN_POINT('Ctrl Pts',(-32.1615862487737,13.4293974985453,
128.247722758148)) ;
#136539 = CARTESIAN_POINT('Ctrl Pts',(-32.140285070969,13.1610019357677,128.218585285993)) ;
#136540 = CARTESIAN_POINT('Ctrl Pts',(-32.0961603941235,12.9105848440385,
128.12288354399)) ;
#136541 = CARTESIAN_POINT('Ctrl Pts',(-32.0318978199246,12.6976134711112,
127.968256892856)) ;
#136542 = CARTESIAN_POINT('Ctrl Pts',(-31.9512431314668,12.5364422844779,
127.765768139102)) ;
#136543 = CARTESIAN_POINT('Ctrl Pts',(-31.8593208623527,12.4387732297296,
127.530343940325)) ;
#136544 = CARTESIAN_POINT('Ctrl Pts',(-31.7616857575535,12.4116342438892,
127.278318451746)) ;
#136545 = CARTESIAN_POINT('Ctrl Pts',(-31.6652363599927,12.4569142353896,
127.029622347502)) ;
#136546 = CARTESIAN_POINT('Ctrl Pts',(-31.5755156798081,12.5714751747461,
126.800673437744)) ;
#136547 = CARTESIAN_POINT('Ctrl Pts',(-31.4986226921134,12.7468632873084,
126.609142921284)) ;
#136548 = CARTESIAN_POINT('Ctrl Pts',(-31.4391185557765,12.9706872458922,
126.468427929382)) ;
#136549 = CARTESIAN_POINT('Ctrl Pts',(-31.4006101144724,13.2271704836993,
126.389077954558)) ;
#136550 = CARTESIAN_POINT('Ctrl Pts',(-31.3851182967717,13.4971329274745,
126.376892427359)) ;
#136551 = CARTESIAN_POINT('Ctrl Pts',(-31.3931465053214,13.7633005024016,
126.433617383089)) ;
#136552 = CARTESIAN_POINT('Ctrl Pts',(-31.4230717823098,14.002826770648,126.553990439311)) ;
#136553 = CARTESIAN_POINT('Ctrl Pts',(-31.4725840354185,14.2028677119568,
126.731901109757)) ;
#136554 = CARTESIAN_POINT('Ctrl Pts',(-31.5366209577425,14.3455611134847,
126.951952487503)) ;
#136555 = CARTESIAN_POINT('Ctrl Pts',(-31.6107344089728,14.4231516282667,
127.201672543475)) ;
#136556 = CARTESIAN_POINT('Ctrl Pts',(-31.6883036036575,14.4286657485207,
127.461395249587)) ;
#136557 = CARTESIAN_POINT('Ctrl Pts',(-31.7632257320844,14.3621070241951,
127.713405765765)) ;
#136558 = CARTESIAN_POINT('Ctrl Pts',(-31.8292721612924,14.2287344049999,
127.939404631142)) ;
#136559 = CARTESIAN_POINT('Ctrl Pts',(-31.8813900908942,14.0363062184854,
128.124936526363)) ;
#136560 = CARTESIAN_POINT('Ctrl Pts',(-31.9144283378458,13.8023698285734,
128.254361978838)) ;
#136561 = CARTESIAN_POINT('Ctrl Pts',(-31.9260122072278,13.538853365046,128.321462132145)) ;
#136562 = CARTESIAN_POINT('Ctrl Pts',(-31.914128124353,13.2684519615159,128.319816614393)) ;
#136563 = CARTESIAN_POINT('Ctrl Pts',(-31.8791690447666,13.0087998067706,
128.250796154468)) ;
#136564 = CARTESIAN_POINT('Ctrl Pts',(-31.8224023910236,12.7778891535909,
128.118233618976)) ;
#136565 = CARTESIAN_POINT('Ctrl Pts',(-31.7482172105361,12.5950174463895,
127.934464371389)) ;
#136566 = CARTESIAN_POINT('Ctrl Pts',(-31.6598803438761,12.4700325386615,
127.709648223425)) ;
#136567 = CARTESIAN_POINT('Ctrl Pts',(-31.5641604318378,12.4138573770184,
127.463058249321)) ;
#136568 = CARTESIAN_POINT('Ctrl Pts',(-31.4659188821753,12.4301864135647,
127.209377342197)) ;
#136569 = CARTESIAN_POINT('Ctrl Pts',(-31.3734534378068,12.5166843884807,
126.972114937016)) ;
#136570 = CARTESIAN_POINT('Ctrl Pts',(-31.2902901080974,12.6693064636983,
126.762458503211)) ;
#136571 = CARTESIAN_POINT('Ctrl Pts',(-31.2234519388235,12.8745470940793,
126.600193818904)) ;
#136572 = CARTESIAN_POINT('Ctrl Pts',(-31.1758307675459,13.1212023426986,
126.494392150649)) ;
#136573 = CARTESIAN_POINT('Ctrl Pts',(-31.1510486370885,13.3871938876445,
126.454987702193)) ;
#136574 = CARTESIAN_POINT('Ctrl Pts',(-31.1495067038997,13.6567281593303,
126.483608122168)) ;
#136575 = CARTESIAN_POINT('Ctrl Pts',(-31.1708676258371,13.9097854189498,
126.579158796714)) ;
#136576 = CARTESIAN_POINT('Ctrl Pts',(-31.2129315448557,14.1280196349839,
126.73522563179)) ;
#136577 = CARTESIAN_POINT('Ctrl Pts',(-31.2715422679824,14.2950456009744,
126.939462493752)) ;
#136578 = CARTESIAN_POINT('Ctrl Pts',(-31.3426766589583,14.4005267641298,
127.180579567432)) ;
#136579 = CARTESIAN_POINT('Ctrl Pts',(-31.4191922825314,14.4350836720727,
127.437076071627)) ;
#136580 = CARTESIAN_POINT('Ctrl Pts',(-31.4958370560869,14.3978038966436,
127.694063116912)) ;
#136581 = CARTESIAN_POINT('Ctrl Pts',(-31.5662721684202,14.290575680997,127.932952398699)) ;
#136582 = CARTESIAN_POINT('Ctrl Pts',(-31.6246390663626,14.12095115065,128.136621698187)) ;
#136583 = CARTESIAN_POINT('Ctrl Pts',(-31.6658960174295,13.9018371946246,
128.290224742107)) ;
#136584 = CARTESIAN_POINT('Ctrl Pts',(-31.6865228260498,13.6479071600813,
128.383641361219)) ;
#136585 = CARTESIAN_POINT('Ctrl Pts',(-31.6842923198617,13.3785018299636,
128.410199122277)) ;
#136586 = CARTESIAN_POINT('Ctrl Pts',(-31.6583478216367,13.1105161592094,
128.36771780606)) ;
#136587 = CARTESIAN_POINT('Ctrl Pts',(-31.6104959175347,12.8677237069018,
128.260861005059)) ;
#136588 = CARTESIAN_POINT('Ctrl Pts',(-31.5426928619191,12.6628308000804,
128.095983031294)) ;
#136589 = CARTESIAN_POINT('Ctrl Pts',(-31.4596635073516,12.5130918940735,
127.886486535544)) ;
#136590 = CARTESIAN_POINT('Ctrl Pts',(-31.3658287353506,12.4280189169956,
127.645626007363)) ;
#136591 = CARTESIAN_POINT('Ctrl Pts',(-31.2683509695454,12.4146728594404,
127.393890391169)) ;
#136592 = CARTESIAN_POINT('Ctrl Pts',(-31.1723757083,12.4734182584077,127.146708101578)) ;
#136593 = CARTESIAN_POINT('Ctrl Pts',(-31.0846573530238,12.6005220023049,
126.923613424427)) ;
#136594 = CARTESIAN_POINT('Ctrl Pts',(-31.0109368887495,12.7855010880113,
126.741250268444)) ;
#136595 = CARTESIAN_POINT('Ctrl Pts',(-30.955066181992,13.0169859630547,126.611193115861)) ;
#136596 = CARTESIAN_POINT('Ctrl Pts',(-30.9207893580841,13.2774552371681,
126.544188371834)) ;
#136597 = CARTESIAN_POINT('Ctrl Pts',(-30.9097471402995,13.5483710343065,
126.545063201967)) ;
#136598 = CARTESIAN_POINT('Ctrl Pts',(-30.9219886293322,13.810085890561,126.613924362208)) ;
#136599 = CARTESIAN_POINT('Ctrl Pts',(-30.9559449844738,14.0443619160834,
126.746258785875)) ;
#136600 = CARTESIAN_POINT('Ctrl Pts',(-31.008405506402,14.2339605947032,126.932620299341)) ;
#136601 = CARTESIAN_POINT('Ctrl Pts',(-31.0749719859752,14.3656339160498,
127.160221612215)) ;
#136602 = CARTESIAN_POINT('Ctrl Pts',(-31.1500767570186,14.429668532247,127.41275139113)) ;
#136603 = CARTESIAN_POINT('Ctrl Pts',(-31.2275475074464,14.4216217933316,
127.672160409701)) ;
#136604 = CARTESIAN_POINT('Ctrl Pts',(-31.3012384048704,14.3422174614337,
127.920539923313)) ;
#136605 = CARTESIAN_POINT('Ctrl Pts',(-31.3652787531755,14.1963613484393,
128.140837493756)) ;
#136606 = CARTESIAN_POINT('Ctrl Pts',(-31.4138953869596,13.9958156934089,
128.315925248088)) ;
#136607 = CARTESIAN_POINT('Ctrl Pts',(-31.4432585655663,13.7540872313105,
128.43481729489)) ;
#136608 = CARTESIAN_POINT('Ctrl Pts',(-31.450475087272,13.4887318703653,128.488999277485)) ;
#136609 = CARTESIAN_POINT('Ctrl Pts',(-31.43413020577,13.217649057413,128.474486119166)) ;
#136610 = CARTESIAN_POINT('Ctrl Pts',(-31.3950123680558,12.9629384688392,
128.39322410481)) ;
#136611 = CARTESIAN_POINT('Ctrl Pts',(-31.3345685415584,12.7394456661168,
128.249925967071)) ;
#136612 = CARTESIAN_POINT('Ctrl Pts',(-31.2573511672677,12.5666312709512,
128.057344274841)) ;
#136613 = CARTESIAN_POINT('Ctrl Pts',(-31.1673288730419,12.4542159420662,
127.827511121374)) ;
#136614 = CARTESIAN_POINT('Ctrl Pts',(-31.070668381057,12.4113528372628,127.57822465589)) ;
#136615 = CARTESIAN_POINT('Ctrl Pts',(-30.9730874968929,12.4409689748371,
127.326366763197)) ;
#136616 = CARTESIAN_POINT('Ctrl Pts',(-30.8813233211208,12.5412370844769,
127.091459318539)) ;
#136617 = CARTESIAN_POINT('Ctrl Pts',(-30.8013523482404,12.7041353062448,
126.890894803477)) ;
#136618 = CARTESIAN_POINT('Ctrl Pts',(-30.7377485662174,12.9183855377871,
126.738165448688)) ;
#136619 = CARTESIAN_POINT('Ctrl Pts',(-30.6943522476391,13.1698655592683,
126.644607861054)) ;
#136620 = CARTESIAN_POINT('Ctrl Pts',(-30.673823555151,13.4380609708233,126.617664783583)) ;
#136621 = CARTESIAN_POINT('Ctrl Pts',(-30.676760958467,13.7071666218626,126.659527815916)) ;
#136622 = CARTESIAN_POINT('Ctrl Pts',(-30.7021921592017,13.9538087956849,
126.766828921088)) ;
#136623 = CARTESIAN_POINT('Ctrl Pts',(-30.7475911892574,14.1634526907068,
126.932575600775)) ;
#136624 = CARTESIAN_POINT('Ctrl Pts',(-30.8091751138635,14.3201289730171,
127.145660569958)) ;
#136625 = CARTESIAN_POINT('Ctrl Pts',(-30.8812761696098,14.4121340863402,
127.389305094501)) ;
#136626 = CARTESIAN_POINT('Ctrl Pts',(-30.958733820161,14.4336855953277,127.648772839054)) ;
#136627 = CARTESIAN_POINT('Ctrl Pts',(-31.0346820701722,14.3827386084068,
127.90373275799)) ;
#136628 = CARTESIAN_POINT('Ctrl Pts',(-31.1034133500512,14.2627494800209,
128.137724022921)) ;
#136629 = CARTESIAN_POINT('Ctrl Pts',(-31.1588772991111,14.0822577525838,
128.332935808731)) ;
#136630 = CARTESIAN_POINT('Ctrl Pts',(-31.1963198264823,13.8561932154224,
128.475274428315)) ;
#136631 = CARTESIAN_POINT('Ctrl Pts',(-31.2127805251386,13.5974242945969,
128.556569267893)) ;
#136632 = CARTESIAN_POINT('Ctrl Pts',(-31.2060956554007,13.3273252607923,
128.570089421003)) ;
#136633 = CARTESIAN_POINT('Ctrl Pts',(-31.175812020864,13.0622912163539,128.514912832323)) ;
#136634 = CARTESIAN_POINT('Ctrl Pts',(-31.1240000905166,12.8256130939751,
128.396503818187)) ;
#136635 = CARTESIAN_POINT('Ctrl Pts',(-31.053014393086,12.6301799024571,128.222286646203)) ;
#136636 = CARTESIAN_POINT('Ctrl Pts',(-30.967517721781,12.4918476681471,128.005627111809)) ;
#136637 = CARTESIAN_POINT('Ctrl Pts',(-30.8725245502937,12.4199209913987,
127.761337053555)) ;
#136638 = CARTESIAN_POINT('Ctrl Pts',(-30.7744792943277,12.4204245912294,
127.50810295915)) ;
#136639 = CARTESIAN_POINT('Ctrl Pts',(-30.6801950959887,12.4921595921641,
127.265646464946)) ;
#136640 = CARTESIAN_POINT('Ctrl Pts',(-30.5945273226143,12.6310172827489,
127.048572948748)) ;
#136641 = CARTESIAN_POINT('Ctrl Pts',(-30.5237138912385,12.8262646896106,
126.87479382954)) ;
#136642 = CARTESIAN_POINT('Ctrl Pts',(-30.4717477142723,13.0646913803179,
126.756146616642)) ;
#136643 = CARTESIAN_POINT('Ctrl Pts',(-30.4418079793539,13.3278244086872,
126.701716231981)) ;
#136644 = CARTESIAN_POINT('Ctrl Pts',(-30.4351907633276,13.5998585157466,
126.715682786109)) ;
#136645 = CARTESIAN_POINT('Ctrl Pts',(-30.4517112140757,13.8569826798842,
126.79695024305)) ;
#136646 = CARTESIAN_POINT('Ctrl Pts',(-30.4894856805257,14.0842218842957,
126.940467978151)) ;
#136647 = CARTESIAN_POINT('Ctrl Pts',(-30.5448536574112,14.2634335835668,
127.135250757845)) ;
#136648 = CARTESIAN_POINT('Ctrl Pts',(-30.61372079861,14.3833954654661,127.369690463296)) ;
#136649 = CARTESIAN_POINT('Ctrl Pts',(-30.6898267170265,14.4336980433791,
127.62516189827)) ;
#136650 = CARTESIAN_POINT('Ctrl Pts',(-30.7668057003665,14.4120157811793,
127.88302690415)) ;
#136651 = CARTESIAN_POINT('Ctrl Pts',(-30.8392469707509,14.3192946840505,
128.127838160812)) ;
#136652 = CARTESIAN_POINT('Ctrl Pts',(-30.900587536692,14.1625583197416,128.340130750955)) ;
#136653 = CARTESIAN_POINT('Ctrl Pts',(-30.9460465529525,13.9521768872698,
128.506141732049)) ;
#136654 = CARTESIAN_POINT('Ctrl Pts',(-30.9712728779103,13.7045477483084,
128.612931121415)) ;
#136655 = CARTESIAN_POINT('Ctrl Pts',(-30.9740973294734,13.4377490370904,
128.65416965186)) ;
#136656 = CARTESIAN_POINT('Ctrl Pts',(-30.9533497435813,13.1678476255433,
128.626808748527)) ;
#136657 = CARTESIAN_POINT('Ctrl Pts',(-30.9100151336481,12.9176590110113,
128.533274696295)) ;
#136658 = CARTESIAN_POINT('Ctrl Pts',(-30.8460093946488,12.7025601678247,
128.379540475209)) ;
#136659 = CARTESIAN_POINT('Ctrl Pts',(-30.7661541649053,12.5405894739356,
128.179214757253)) ;
#136660 = CARTESIAN_POINT('Ctrl Pts',(-30.6742450321208,12.4405287609816,
127.943925123088)) ;
#136661 = CARTESIAN_POINT('Ctrl Pts',(-30.5767059002742,12.4114132286229,
127.69216607229)) ;
#136662 = CARTESIAN_POINT('Ctrl Pts',(-30.4801944320936,12.454644377757,127.443276439968)) ;
#136663 = CARTESIAN_POINT('Ctrl Pts',(-30.3903499727896,12.5668919625006,
127.213894581398)) ;
#136664 = CARTESIAN_POINT('Ctrl Pts',(-30.3126378072182,12.7415275985948,
127.020134144309)) ;
#136665 = CARTESIAN_POINT('Ctrl Pts',(-30.2527609211518,12.9638992642169,
126.878266781381)) ;
#136666 = CARTESIAN_POINT('Ctrl Pts',(-30.2136507437356,13.2191082193463,
126.797089063546)) ;
#136667 = CARTESIAN_POINT('Ctrl Pts',(-30.1974592284486,13.4893534284064,
126.782913516033)) ;
#136668 = CARTESIAN_POINT('Ctrl Pts',(-30.2047500779676,13.7553188201862,
126.837397733995)) ;
#136669 = CARTESIAN_POINT('Ctrl Pts',(-30.2342451153367,13.9971251061997,
126.956700334414)) ;
#136670 = CARTESIAN_POINT('Ctrl Pts',(-30.2831588596257,14.1977811038748,
127.132755162612)) ;
#136671 = CARTESIAN_POINT('Ctrl Pts',(-30.346836697301,14.342451043168,127.351773566812)) ;
#136672 = CARTESIAN_POINT('Ctrl Pts',(-30.421041235796,14.4220642715211,127.601876667778)) ;
#136673 = CARTESIAN_POINT('Ctrl Pts',(-30.4982063681556,14.4294491071756,
127.860253341172)) ;
#136674 = CARTESIAN_POINT('Ctrl Pts',(-30.5732568669214,14.3652072705711,
128.112616520929)) ;
#136675 = CARTESIAN_POINT('Ctrl Pts',(-30.639714705362,14.2335292315096,128.339855798)) ;
#136676 = CARTESIAN_POINT('Ctrl Pts',(-30.6922904669337,14.0429180682628,
128.526684338748)) ;
#136677 = CARTESIAN_POINT('Ctrl Pts',(-30.7259826319712,13.809322141679,128.658117930451)) ;
#136678 = CARTESIAN_POINT('Ctrl Pts',(-30.7382344074887,13.5476219044277,
128.727006823205)) ;
#136679 = CARTESIAN_POINT('Ctrl Pts',(-30.7269403534024,13.2750712862456,
128.727347582682)) ;
#136680 = CARTESIAN_POINT('Ctrl Pts',(-30.6927096810356,13.0163165161328,
128.660275654036)) ;
#136681 = CARTESIAN_POINT('Ctrl Pts',(-30.6367586931873,12.7846452326426,
128.530021727058)) ;
#136682 = CARTESIAN_POINT('Ctrl Pts',(-30.5628122994071,12.5995256932136,
128.347061120519)) ;
#136683 = CARTESIAN_POINT('Ctrl Pts',(-30.4747613342132,12.4726551815389,
128.123086887986)) ;
#136684 = CARTESIAN_POINT('Ctrl Pts',(-30.3791108848396,12.4145513483266,
127.876726073933)) ;
#136685 = CARTESIAN_POINT('Ctrl Pts',(-30.2813444524036,12.428469046116,127.624255078957)) ;
#136686 = CARTESIAN_POINT('Ctrl Pts',(-30.1880546184578,12.5133431382162,
127.384795540324)) ;
#136687 = CARTESIAN_POINT('Ctrl Pts',(-30.1045779411166,12.664436679697,127.174213781019)) ;
#136688 = CARTESIAN_POINT('Ctrl Pts',(-30.0373665693582,12.8679925136389,
127.010803548602)) ;
#136689 = CARTESIAN_POINT('Ctrl Pts',(-29.9891717630807,13.1131689974074,
126.903257186694)) ;
#136690 = CARTESIAN_POINT('Ctrl Pts',(-29.9635947628022,13.3800002481821,
126.861679569015)) ;
#136691 = CARTESIAN_POINT('Ctrl Pts',(-29.9614886970203,13.6495651471469,
126.888635732367)) ;
#136692 = CARTESIAN_POINT('Ctrl Pts',(-29.9820901647901,13.9023388794203,
126.981828620855)) ;
#136693 = CARTESIAN_POINT('Ctrl Pts',(-30.0237239088706,14.122657772282,127.136756156811)) ;
#136694 = CARTESIAN_POINT('Ctrl Pts',(-30.0818493827078,14.2908247523975,
127.339514451375)) ;
#136695 = CARTESIAN_POINT('Ctrl Pts',(-30.1523278927941,14.3981040608109,
127.578557488567)) ;
#136696 = CARTESIAN_POINT('Ctrl Pts',(-30.2293017778159,14.435262692703,127.836631386951)) ;
#136697 = CARTESIAN_POINT('Ctrl Pts',(-30.3061172612986,14.3995540237045,
128.094159932593)) ;
#136698 = CARTESIAN_POINT('Ctrl Pts',(-30.37646616318,14.2948938625941,128.332624943181)) ;
#136699 = CARTESIAN_POINT('Ctrl Pts',(-30.4355875307391,14.1259509671256,
128.538688857853)) ;
#136700 = CARTESIAN_POINT('Ctrl Pts',(-30.4771902665087,13.908522649266,128.693202393505)) ;
#136701 = CARTESIAN_POINT('Ctrl Pts',(-30.4984453367561,13.6557404743469,
128.788409222222)) ;
#136702 = CARTESIAN_POINT('Ctrl Pts',(-30.4969183209716,13.3866405652258,
128.817008538499)) ;
#136703 = CARTESIAN_POINT('Ctrl Pts',(-30.4716526944361,13.1181024502092,
128.776531708148)) ;
#136704 = CARTESIAN_POINT('Ctrl Pts',(-30.4244050237175,12.8743683126388,
128.671446151271)) ;
#136705 = CARTESIAN_POINT('Ctrl Pts',(-30.3571122022536,12.667995764075,128.508067284342)) ;
#136706 = CARTESIAN_POINT('Ctrl Pts',(-30.2743107927955,12.5164144284275,
128.299288210376)) ;
#136707 = CARTESIAN_POINT('Ctrl Pts',(-30.181040701032,12.4295970392297,128.059953712799)) ;
#136708 = CARTESIAN_POINT('Ctrl Pts',(-30.0832914972491,12.4140261285354,
127.80753264675)) ;
#136709 = CARTESIAN_POINT('Ctrl Pts',(-29.9873254871061,12.4707103016775,
127.560322493363)) ;
#136710 = CARTESIAN_POINT('Ctrl Pts',(-29.8992941244822,12.5959067650868,
127.336315129567)) ;
#136711 = CARTESIAN_POINT('Ctrl Pts',(-29.8250863434499,12.7791141929297,
127.152509042809)) ;
#136712 = CARTESIAN_POINT('Ctrl Pts',(-29.7683155464233,13.0114292224114,
127.020076886844)) ;
#136713 = CARTESIAN_POINT('Ctrl Pts',(-29.7337701163823,13.2689898399713,
126.951978873228)) ;
#136714 = CARTESIAN_POINT('Ctrl Pts',(-29.7219200549302,13.5409256282928,
126.950629438591)) ;
#136715 = CARTESIAN_POINT('Ctrl Pts',(-29.733554311949,13.8029839862651,127.017693083378)) ;
#136716 = CARTESIAN_POINT('Ctrl Pts',(-29.7669729925105,14.038560788847,127.14849808743)) ;
#136717 = CARTESIAN_POINT('Ctrl Pts',(-29.8189700914752,14.2294230403712,
127.333487758985)) ;
#136718 = CARTESIAN_POINT('Ctrl Pts',(-29.8850962736987,14.3627051094246,
127.559749339054)) ;
#136719 = CARTESIAN_POINT('Ctrl Pts',(-29.9600740109055,14.4288334049426,
127.811925871913)) ;
#136720 = CARTESIAN_POINT('Ctrl Pts',(-30.0375926178455,14.4228924634038,
128.071485668505)) ;
#136721 = CARTESIAN_POINT('Ctrl Pts',(-30.1116851063149,14.3451234718206,
128.321135357699)) ;
#136722 = CARTESIAN_POINT('Ctrl Pts',(-30.1759653031879,14.2008973362482,
128.542101575168)) ;
#136723 = CARTESIAN_POINT('Ctrl Pts',(-30.2249348888654,14.0023960855746,
128.718117429598)) ;
#136724 = CARTESIAN_POINT('Ctrl Pts',(-30.2549649553424,13.7610318696562,
128.839037447966)) ;
#136725 = CARTESIAN_POINT('Ctrl Pts',(-30.2627841057998,13.4967570532622,
128.894894568641)) ;
#136726 = CARTESIAN_POINT('Ctrl Pts',(-30.2472089094513,13.2257686273763,
128.882599290474)) ;
#136727 = CARTESIAN_POINT('Ctrl Pts',(-30.2085846766644,12.9695426801037,
128.802889416745)) ;
#136728 = CARTESIAN_POINT('Ctrl Pts',(-30.1488841254311,12.7456272140063,
128.661652559478)) ;
#136729 = CARTESIAN_POINT('Ctrl Pts',(-30.072111052342,12.5709695556374,128.470385081871)) ;
#136730 = CARTESIAN_POINT('Ctrl Pts',(-29.9822608788723,12.4565179199043,
128.241096280183)) ;
#136731 = CARTESIAN_POINT('Ctrl Pts',(-29.8856850056017,12.4114773768948,
127.992062768051)) ;
#136732 = CARTESIAN_POINT('Ctrl Pts',(-29.7876800986946,12.4394645441859,
127.739096174326)) ;
#136733 = CARTESIAN_POINT('Ctrl Pts',(-29.6963815648897,12.5368906975998,
127.505279670265)) ;
#136734 = CARTESIAN_POINT('Ctrl Pts',(-29.6153252716396,12.6994727132711,
127.301831679422)) ;
#136735 = CARTESIAN_POINT('Ctrl Pts',(-29.5516191180179,12.911284387256,127.148596694426)) ;
#136736 = CARTESIAN_POINT('Ctrl Pts',(-29.5073375465469,13.1634090150243,
127.052650475059)) ;
#136737 = CARTESIAN_POINT('Ctrl Pts',(-29.4863722183674,13.43009560959,127.024270357643)) ;
#136738 = CARTESIAN_POINT('Ctrl Pts',(-29.4884710007012,13.6985487058695,
127.063557018195)) ;
#136739 = CARTESIAN_POINT('Ctrl Pts',(-29.5134955024387,13.9480246666546,
127.169938370698)) ;
#136740 = CARTESIAN_POINT('Ctrl Pts',(-29.5581845038541,14.1576527817006,
127.333424570295)) ;
#136741 = CARTESIAN_POINT('Ctrl Pts',(-29.6192793503669,14.3162850148807,
127.545072239958)) ;
#136742 = CARTESIAN_POINT('Ctrl Pts',(-29.6915017728377,14.4106899860489,
127.789227708375)) ;
#136743 = CARTESIAN_POINT('Ctrl Pts',(-29.7689280820927,14.4339585124651,
128.048612152318)) ;
#136744 = CARTESIAN_POINT('Ctrl Pts',(-29.8446720420226,14.3853107733964,
128.302830330113)) ;
#136745 = CARTESIAN_POINT('Ctrl Pts',(-29.9138779062533,14.2669554463922,
128.538293583746)) ;
#136746 = CARTESIAN_POINT('Ctrl Pts',(-29.9696709434551,14.0883946272744,
128.734393104411)) ;
#136747 = CARTESIAN_POINT('Ctrl Pts',(-30.0077339518895,13.8631868173472,
128.878592553755)) ;
#136748 = CARTESIAN_POINT('Ctrl Pts',(-30.0248332499743,13.6057121370264,
128.961669133376)) ;
#136749 = CARTESIAN_POINT('Ctrl Pts',(-30.0188186236366,13.3350529276947,
128.977231035736)) ;
#136750 = CARTESIAN_POINT('Ctrl Pts',(-29.9893748969538,13.070755438595,128.924351996727)) ;
#136751 = CARTESIAN_POINT('Ctrl Pts',(-29.9381198967641,12.8321487482004,
128.80767194367)) ;
#136752 = CARTESIAN_POINT('Ctrl Pts',(-29.8672185952709,12.6344630496442,
128.633863552684)) ;
#136753 = CARTESIAN_POINT('Ctrl Pts',(-29.7824442419727,12.4951762287069,
128.419156640686)) ;
#136754 = CARTESIAN_POINT('Ctrl Pts',(-29.6878398932175,12.4210996304978,
128.175941162278)) ;
#136755 = CARTESIAN_POINT('Ctrl Pts',(-29.5896845117349,12.4192964067175,
127.922422995401)) ;
#136756 = CARTESIAN_POINT('Ctrl Pts',(-29.4950005569696,12.4890491878224,
127.678869190978)) ;
#136757 = CARTESIAN_POINT('Ctrl Pts',(-29.4087337325941,12.6268326334366,
127.460163347604)) ;
#136758 = CARTESIAN_POINT('Ctrl Pts',(-29.3378740489248,12.819583008208,127.286057249325)) ;
#136759 = CARTESIAN_POINT('Ctrl Pts',(-29.2851760043964,13.0571001381562,
127.165305917233)) ;
#136760 = CARTESIAN_POINT('Ctrl Pts',(-29.2545650359893,13.3202804831109,
127.108978042676)) ;
#136761 = CARTESIAN_POINT('Ctrl Pts',(-29.2472402862376,13.5914915741981,
127.120763375443)) ;
#136762 = CARTESIAN_POINT('Ctrl Pts',(-29.2632084846412,13.8505565623955,
127.200591332072)) ;
#136763 = CARTESIAN_POINT('Ctrl Pts',(-29.3002581970792,14.0777828680815,
127.341827832713)) ;
#136764 = CARTESIAN_POINT('Ctrl Pts',(-29.3552517763385,14.2590885920228,
127.535591866083)) ;
#136765 = CARTESIAN_POINT('Ctrl Pts',(-29.4237488183174,14.3807166711332,
127.768911763596)) ;
#136766 = CARTESIAN_POINT('Ctrl Pts',(-29.4996525428167,14.433343609964,128.023765667449)) ;
#136767 = CARTESIAN_POINT('Ctrl Pts',(-29.5771911863462,14.4133893696398,
128.283487783955)) ;
#136768 = CARTESIAN_POINT('Ctrl Pts',(-29.6493874448515,14.322997838196,128.527374224998)) ;
#136769 = CARTESIAN_POINT('Ctrl Pts',(-29.7111985626371,14.1680350352392,
128.741068674878)) ;
#136770 = CARTESIAN_POINT('Ctrl Pts',(-29.7570938139527,13.9594348156913,
128.90828666285)) ;
#136771 = CARTESIAN_POINT('Ctrl Pts',(-29.7830790443061,13.7128291975183,
129.017289967226)) ;
#136772 = CARTESIAN_POINT('Ctrl Pts',(-29.786491574937,13.4442543437845,129.060505529858)) ;
#136773 = CARTESIAN_POINT('Ctrl Pts',(-29.7666355649697,13.1766944137287,
129.03542159918)) ;
#136774 = CARTESIAN_POINT('Ctrl Pts',(-29.7235723363899,12.9234094680339,
128.942988295954)) ;
#136775 = CARTESIAN_POINT('Ctrl Pts',(-29.6604602934402,12.7086523131788,
128.791635677424)) ;
#136776 = CARTESIAN_POINT('Ctrl Pts',(-29.5809549544293,12.5444332770708,
128.592392030058)) ;
#136777 = CARTESIAN_POINT('Ctrl Pts',(-29.4889378675449,12.442265427868,128.356904521378)) ;
#136778 = CARTESIAN_POINT('Ctrl Pts',(-29.3918859003814,12.4113238221151,
128.106429463482)) ;
#136779 = CARTESIAN_POINT('Ctrl Pts',(-29.2951830663714,12.4521999804418,
127.857002016351)) ;
#136780 = CARTESIAN_POINT('Ctrl Pts',(-29.2045584488125,12.5635389839908,
127.625544044653)) ;
#136781 = CARTESIAN_POINT('Ctrl Pts',(-29.1270346002203,12.7354102486573,
127.432082992235)) ;
#136782 = CARTESIAN_POINT('Ctrl Pts',(-29.0664146932763,12.9568497903179,
127.288112348408)) ;
#136783 = CARTESIAN_POINT('Ctrl Pts',(-29.026628696439,13.2117694204113,127.205005677321)) ;
#136784 = CARTESIAN_POINT('Ctrl Pts',(-29.009781511419,13.4825284434545,127.188995235441)) ;
#136785 = CARTESIAN_POINT('Ctrl Pts',(-29.0165029066214,13.7484828360667,
127.24177102206)) ;
#136786 = CARTESIAN_POINT('Ctrl Pts',(-29.0452591215666,13.990067054495,127.358763219007)) ;
#136787 = CARTESIAN_POINT('Ctrl Pts',(-29.0935118085886,14.1922208547519,
127.532848793653)) ;
#136788 = CARTESIAN_POINT('Ctrl Pts',(-29.1572269990264,14.3393855053723,
127.752176269274)) ;
#136789 = CARTESIAN_POINT('Ctrl Pts',(-29.2305804306216,14.42040771759,127.999501211694)) ;
#136790 = CARTESIAN_POINT('Ctrl Pts',(-29.3081218951313,14.4304302239803,
128.259154471138)) ;
#136791 = CARTESIAN_POINT('Ctrl Pts',(-29.3835564511664,14.3678711876826,
128.512736663744)) ;
#136792 = CARTESIAN_POINT('Ctrl Pts',(-29.4503619230929,14.2376928211799,
128.741022388839)) ;
#136793 = CARTESIAN_POINT('Ctrl Pts',(-29.5032308391101,14.0489884118596,
128.928618678733)) ;
#136794 = CARTESIAN_POINT('Ctrl Pts',(-29.5375680722681,13.8164457415788,
129.061943923346)) ;
#136795 = CARTESIAN_POINT('Ctrl Pts',(-29.5503747746567,13.5541090228178,
129.132594337899)) ;
#136796 = CARTESIAN_POINT('Ctrl Pts',(-29.5399467581774,13.2846773793449,
129.135075798619)) ;
#136797 = CARTESIAN_POINT('Ctrl Pts',(-29.5061893697733,13.0230236388571,
129.069677559174)) ;
#136798 = CARTESIAN_POINT('Ctrl Pts',(-29.4508852278089,12.7908728134741,
128.941231892332)) ;
#136799 = CARTESIAN_POINT('Ctrl Pts',(-29.3772505067172,12.6038718896903,
128.75925572478)) ;
#136800 = CARTESIAN_POINT('Ctrl Pts',(-29.2898362457015,12.4755978547321,
128.537018141377)) ;
#136801 = CARTESIAN_POINT('Ctrl Pts',(-29.194109143763,12.4151865518673,128.290517599109)) ;
#136802 = CARTESIAN_POINT('Ctrl Pts',(-29.0964293211591,12.4270410419496,
128.038256726691)) ;
#136803 = CARTESIAN_POINT('Ctrl Pts',(-29.0029243016515,12.5098502218198,
127.798170594329)) ;
#136804 = CARTESIAN_POINT('Ctrl Pts',(-28.9191009602141,12.6589865553575,
127.586552482933)) ;
#136805 = CARTESIAN_POINT('Ctrl Pts',(-28.8512558271298,12.8615686437882,
127.421356708522)) ;
#136806 = CARTESIAN_POINT('Ctrl Pts',(-28.8025728823475,13.1050265779988,
127.31227708127)) ;
#136807 = CARTESIAN_POINT('Ctrl Pts',(-28.7762486857145,13.3718443264194,
127.268571741822)) ;
#136808 = CARTESIAN_POINT('Ctrl Pts',(-28.7733651472645,13.6411903783996,
127.293193753917)) ;
#136809 = CARTESIAN_POINT('Ctrl Pts',(-28.7936073014881,13.896863473321,127.385643006294)) ;
#136810 = CARTESIAN_POINT('Ctrl Pts',(-28.8342644907742,14.1159779541294,
127.537349449591)) ;
#136811 = CARTESIAN_POINT('Ctrl Pts',(-28.8923618748685,14.287325692981,127.74029379046)) ;
#136812 = CARTESIAN_POINT('Ctrl Pts',(-28.9624436618844,14.3958947357892,
127.978085746243)) ;
#136813 = CARTESIAN_POINT('Ctrl Pts',(-29.0390644308761,14.435126510394,128.23502978254)) ;
#136814 = CARTESIAN_POINT('Ctrl Pts',(-29.1159362844718,14.4019578679091,
128.492693840916)) ;
#136815 = CARTESIAN_POINT('Ctrl Pts',(-29.1870377918795,14.298265208763,128.73360610522)) ;
#136816 = CARTESIAN_POINT('Ctrl Pts',(-29.2460470592508,14.1324802055206,
128.939037898302)) ;
#136817 = CARTESIAN_POINT('Ctrl Pts',(-29.288497423552,13.915462828794,129.096196593093)) ;
#136818 = CARTESIAN_POINT('Ctrl Pts',(-29.3103654608126,13.663371252365,129.193190377412)) ;
#136819 = CARTESIAN_POINT('Ctrl Pts',(-29.3094695407686,13.3940849584222,
129.223687381527)) ;
#136820 = CARTESIAN_POINT('Ctrl Pts',(-29.2850224789087,13.1263052968225,
129.185456897491)) ;
#136821 = CARTESIAN_POINT('Ctrl Pts',(-29.2381611448435,12.8804158989885,
129.08167274597)) ;
#136822 = CARTESIAN_POINT('Ctrl Pts',(-29.1715363437508,12.6733663230833,
128.92014851409)) ;
#136823 = CARTESIAN_POINT('Ctrl Pts',(-29.0889990041124,12.5197379443073,
128.712196434406)) ;
#136824 = CARTESIAN_POINT('Ctrl Pts',(-28.9959071355212,12.4310982287018,
128.473389219666)) ;
#136825 = CARTESIAN_POINT('Ctrl Pts',(-28.8984687306233,12.413462824637,128.221785958842)) ;
#136826 = CARTESIAN_POINT('Ctrl Pts',(-28.8022697790058,12.4679867146693,
127.973924652651)) ;
#136827 = CARTESIAN_POINT('Ctrl Pts',(-28.7137196227215,12.5916525071464,
127.748478120459)) ;
#136828 = CARTESIAN_POINT('Ctrl Pts',(-28.639163277288,12.773468390421,127.563641479719)) ;
#136829 = CARTESIAN_POINT('Ctrl Pts',(-28.5821237966997,13.0028687582652,
127.43018831272)) ;
#136830 = CARTESIAN_POINT('Ctrl Pts',(-28.5465487884164,13.2619623581497,
127.359364860779)) ;
#136831 = CARTESIAN_POINT('Ctrl Pts',(-28.534169523219,13.5340191309755,127.35648469017)) ;
#136832 = CARTESIAN_POINT('Ctrl Pts',(-28.5451189938016,13.7955674320649,
127.421423522418)) ;
#136833 = CARTESIAN_POINT('Ctrl Pts',(-28.5779338052964,14.0322612851413,
127.550472253615)) ;
#136834 = CARTESIAN_POINT('Ctrl Pts',(-28.6293739615442,14.22438976877,127.733793431735)) ;
#136835 = CARTESIAN_POINT('Ctrl Pts',(-28.6952422477354,14.3598900784348,
127.959353406453)) ;
#136836 = CARTESIAN_POINT('Ctrl Pts',(-28.7704037460775,14.4280176148554,
128.212213421062)) ;
#136837 = CARTESIAN_POINT('Ctrl Pts',(-28.8474474420826,14.4241023882727,
128.47017427123)) ;
#136838 = CARTESIAN_POINT('Ctrl Pts',(-28.9219593848284,14.3482280503466,
128.721153256107)) ;
#136839 = CARTESIAN_POINT('Ctrl Pts',(-28.9864498905584,14.206072490763,128.942653447451)) ;
#136840 = CARTESIAN_POINT('Ctrl Pts',(-29.035985750403,14.008680924911,129.120380524179)) ;
#136841 = CARTESIAN_POINT('Ctrl Pts',(-29.0665824887295,13.7691472453329,
129.242843957834)) ;
#136842 = CARTESIAN_POINT('Ctrl Pts',(-29.0751153015166,13.5031161765621,
129.301061223738)) ;
#136843 = CARTESIAN_POINT('Ctrl Pts',(-29.0600884173673,13.2327334709729,
129.290277948207)) ;
#136844 = CARTESIAN_POINT('Ctrl Pts',(-29.0222348119566,12.9767767271815,
129.212705748521)) ;
#136845 = CARTESIAN_POINT('Ctrl Pts',(-28.9632320010006,12.7518157779669,
129.073464224787)) ;
#136846 = CARTESIAN_POINT('Ctrl Pts',(-28.8865689011726,12.5749030821108,
128.882657897678)) ;
#136847 = CARTESIAN_POINT('Ctrl Pts',(-28.7971500754483,12.4587258790909,
128.654567687979)) ;
#136848 = CARTESIAN_POINT('Ctrl Pts',(-28.7001805984422,12.4118884075951,
128.40456104214)) ;
#136849 = CARTESIAN_POINT('Ctrl Pts',(-28.6034625867503,12.4371447896242,
128.154880032499)) ;
#136850 = CARTESIAN_POINT('Ctrl Pts',(-28.5108176103101,12.5335140110472,
127.917531270634)) ;
#136851 = CARTESIAN_POINT('Ctrl Pts',(-28.4300750917707,12.6929505579163,
127.714687315915)) ;
#136852 = CARTESIAN_POINT('Ctrl Pts',(-28.3652170696654,12.9053983605441,
127.558411095435)) ;
#136853 = CARTESIAN_POINT('Ctrl Pts',(-28.320776308873,13.1539498809503,127.461624968063)) ;
#136854 = CARTESIAN_POINT('Ctrl Pts',(-28.298797481994,13.4226750852024,127.430585596952)) ;
#136855 = CARTESIAN_POINT('Ctrl Pts',(-28.3003278552427,13.6910891488428,
127.468168994763)) ;
#136856 = CARTESIAN_POINT('Ctrl Pts',(-28.3246858188287,13.9413684449187,
127.57259757245)) ;
#136857 = CARTESIAN_POINT('Ctrl Pts',(-28.3689739237031,14.1526799175884,
127.734981003135)) ;
#136858 = CARTESIAN_POINT('Ctrl Pts',(-28.4295901071815,14.3125333365339,
127.945168675357)) ;
#136859 = CARTESIAN_POINT('Ctrl Pts',(-28.5013420399729,14.4088194545048,
128.187852724351)) ;
#136860 = CARTESIAN_POINT('Ctrl Pts',(-28.5789855165237,14.4343198922647,
128.447994052582)) ;
#136861 = CARTESIAN_POINT('Ctrl Pts',(-28.6547069342175,14.3877722216923,
128.702080644945)) ;
#136862 = CARTESIAN_POINT('Ctrl Pts',(-28.7242795531825,14.2711471229662,
128.938658704747)) ;
#136863 = CARTESIAN_POINT('Ctrl Pts',(-28.7802793365346,14.0951743050547,
129.135196568692)) ;
#136864 = CARTESIAN_POINT('Ctrl Pts',(-28.819161267005,13.870335406886,129.281932862346)) ;
#136865 = CARTESIAN_POINT('Ctrl Pts',(-28.8368809389887,13.6128359937758,
129.366896771082)) ;
#136866 = CARTESIAN_POINT('Ctrl Pts',(-28.8315194560845,13.3431053830175,
129.384270113394)) ;
#136867 = CARTESIAN_POINT('Ctrl Pts',(-28.8028631485192,13.0784070527184,
129.333670117737)) ;
#136868 = CARTESIAN_POINT('Ctrl Pts',(-28.7516974964307,12.8371326222925,
129.217513861175)) ;
#136869 = CARTESIAN_POINT('Ctrl Pts',(-28.6819104589447,12.6399916348322,
129.04664441349)) ;
#136870 = CARTESIAN_POINT('Ctrl Pts',(-28.5970929224664,12.4979353055065,
128.83198887352)) ;
#136871 = CARTESIAN_POINT('Ctrl Pts',(-28.5024370244011,12.4220838760127,
128.588688477948)) ;
#136872 = CARTESIAN_POINT('Ctrl Pts',(-28.4044917843163,12.4184701174221,
128.335717148348)) ;
#136873 = CARTESIAN_POINT('Ctrl Pts',(-28.3099706653344,12.4860424298892,
128.092527425312)) ;
#136874 = CARTESIAN_POINT('Ctrl Pts',(-28.223574515994,12.6212969688775,127.873340879876)) ;
#136875 = CARTESIAN_POINT('Ctrl Pts',(-28.1518306616533,12.8133838986541,
127.69681361212)) ;
#136876 = CARTESIAN_POINT('Ctrl Pts',(-28.0985302457413,13.0503648242526,
127.574351579876)) ;
#136877 = CARTESIAN_POINT('Ctrl Pts',(-28.0673717372715,13.3123036510868,
127.516329514673)) ;
#136878 = CARTESIAN_POINT('Ctrl Pts',(-28.0593362748271,13.583277796962,127.526004293595)) ;
#136879 = CARTESIAN_POINT('Ctrl Pts',(-28.074579667337,13.8428842825667,127.603695842468)) ;
#136880 = CARTESIAN_POINT('Ctrl Pts',(-28.1111583249458,14.0720012464851,
127.743661870436)) ;
#136881 = CARTESIAN_POINT('Ctrl Pts',(-28.1656930951673,14.2546155052048,
127.936063605963)) ;
#136882 = CARTESIAN_POINT('Ctrl Pts',(-28.2336890692285,14.3779471220683,
128.167835790675)) ;
#136883 = CARTESIAN_POINT('Ctrl Pts',(-28.3095549362229,14.43277854508,128.422626942245)) ;
#136884 = CARTESIAN_POINT('Ctrl Pts',(-28.3868885672699,14.415204860474,128.681637758062)) ;
#136885 = CARTESIAN_POINT('Ctrl Pts',(-28.4596630946583,14.3266409888288,
128.927362056089)) ;
#136886 = CARTESIAN_POINT('Ctrl Pts',(-28.5219364510198,14.1729215219676,
129.142467156732)) ;
#136887 = CARTESIAN_POINT('Ctrl Pts',(-28.5681998414333,13.9662155734193,
129.310666589753)) ;
#136888 = CARTESIAN_POINT('Ctrl Pts',(-28.5948212406952,13.7208187019913,
129.421494134839)) ;
#136889 = CARTESIAN_POINT('Ctrl Pts',(-28.5989652050376,13.4521886901424,
129.466894357061)) ;
#136890 = CARTESIAN_POINT('Ctrl Pts',(-28.5796745440176,13.1838897555981,
129.443530441394)) ;
#136891 = CARTESIAN_POINT('Ctrl Pts',(-28.5375432029936,12.9313138708941,
129.353617345095)) ;
#136892 = CARTESIAN_POINT('Ctrl Pts',(-28.4748147134164,12.7142071151624,
129.203518501486)) ;
#136893 = CARTESIAN_POINT('Ctrl Pts',(-28.3955037882874,12.548182284736,129.004911407026)) ;
#136894 = CARTESIAN_POINT('Ctrl Pts',(-28.3042662810769,12.4445945488069,
128.771517428537)) ;
#136895 = CARTESIAN_POINT('Ctrl Pts',(-28.2072142920676,12.4110615295413,
128.521074478556)) ;
#136896 = CARTESIAN_POINT('Ctrl Pts',(-28.109954279377,12.4502003407784,128.270178669755)) ;
#136897 = CARTESIAN_POINT('Ctrl Pts',(-28.0196765282693,12.558798155004,128.039502633665)) ;
#136898 = CARTESIAN_POINT('Ctrl Pts',(-27.9414026174185,12.7290992906361,
127.843940992415)) ;
#136899 = CARTESIAN_POINT('Ctrl Pts',(-27.8799523087916,12.9505642772134,
127.697713789602)) ;
#136900 = CARTESIAN_POINT('Ctrl Pts',(-27.8397310330826,13.2039533601212,
127.613220973736)) ;
#136901 = CARTESIAN_POINT('Ctrl Pts',(-27.8221719989325,13.4737768024146,
127.59504291459)) ;
#136902 = CARTESIAN_POINT('Ctrl Pts',(-27.828142978279,13.7408243075777,127.645702023097)) ;
#136903 = CARTESIAN_POINT('Ctrl Pts',(-27.8565009523758,13.984382806197,127.761690204667)) ;
#136904 = CARTESIAN_POINT('Ctrl Pts',(-27.904026451956,14.1867700036955,127.933475703758)) ;
#136905 = CARTESIAN_POINT('Ctrl Pts',(-27.9674069988023,14.3360222992997,
128.151866633947)) ;
#136906 = CARTESIAN_POINT('Ctrl Pts',(-28.0405654232842,14.419030482185,128.398621922666)) ;
#136907 = CARTESIAN_POINT('Ctrl Pts',(-28.1180655766905,14.4311357445316,
128.658152500593)) ;
#136908 = CARTESIAN_POINT('Ctrl Pts',(-28.1935404493141,14.3708888244175,
128.91179298057)) ;
#136909 = CARTESIAN_POINT('Ctrl Pts',(-28.2607936473277,14.242292745065,129.141455567403)) ;
#136910 = CARTESIAN_POINT('Ctrl Pts',(-28.3139374658551,14.0562620175223,
129.329683129342)) ;
#136911 = CARTESIAN_POINT('Ctrl Pts',(-28.3491506733618,13.8231737937943,
129.465813554896)) ;
#136912 = CARTESIAN_POINT('Ctrl Pts',(-28.3625271445841,13.5622217788933,
129.538011618253)) ;
#136913 = CARTESIAN_POINT('Ctrl Pts',(-28.3527809549952,13.2923511462151,
129.542545200143)) ;
#136914 = CARTESIAN_POINT('Ctrl Pts',(-28.3197908030112,13.0307857162003,
129.479299324232)) ;
#136915 = CARTESIAN_POINT('Ctrl Pts',(-28.2649022282346,12.7967159869363,
129.352185243173)) ;
#136916 = CARTESIAN_POINT('Ctrl Pts',(-28.1917552814469,12.6083943270826,
129.171610865605)) ;
#136917 = CARTESIAN_POINT('Ctrl Pts',(-28.1045726910697,12.4782667432663,
128.950081296167)) ;
#136918 = CARTESIAN_POINT('Ctrl Pts',(-28.0093162223049,12.4160107733854,
128.704845792822)) ;
#136919 = CARTESIAN_POINT('Ctrl Pts',(-27.9113561678863,12.425588900326,128.451849759996)) ;
#136920 = CARTESIAN_POINT('Ctrl Pts',(-27.8173088069426,12.5070742961233,
128.210311026811)) ;
#136921 = CARTESIAN_POINT('Ctrl Pts',(-27.7335650904484,12.6538727227807,
127.998759420859)) ;
#136922 = CARTESIAN_POINT('Ctrl Pts',(-27.6650837722555,12.8553498973186,
127.831762310882)) ;
#136923 = CARTESIAN_POINT('Ctrl Pts',(-27.615801809689,13.0981033261267,127.720951140335)) ;
#136924 = CARTESIAN_POINT('Ctrl Pts',(-27.58884476403,13.3649637765944,127.675446327313)) ;
#136925 = CARTESIAN_POINT('Ctrl Pts',(-27.5853834682543,13.6334093866667,
127.698255596654)) ;
#136926 = CARTESIAN_POINT('Ctrl Pts',(-27.6047690706477,13.8886868084012,
127.78804071139)) ;
#136927 = CARTESIAN_POINT('Ctrl Pts',(-27.6450492586127,14.1104518117265,
127.938840818448)) ;
#136928 = CARTESIAN_POINT('Ctrl Pts',(-27.7027415775045,14.2832226170572,
128.140591352709)) ;
#136929 = CARTESIAN_POINT('Ctrl Pts',(-27.7725050879397,14.3937886197238,
128.377439933488)) ;
#136930 = CARTESIAN_POINT('Ctrl Pts',(-27.8493794925505,14.4350213819736,
128.635274356798)) ;
#136931 = CARTESIAN_POINT('Ctrl Pts',(-27.9259608175934,14.4038716569565,
128.891931541062)) ;
#136932 = CARTESIAN_POINT('Ctrl Pts',(-27.9974403274595,14.3020574397598,
129.134001140412)) ;
#136933 = CARTESIAN_POINT('Ctrl Pts',(-28.0568366490592,14.1377082667359,
129.340572157127)) ;
#136934 = CARTESIAN_POINT('Ctrl Pts',(-28.0997330529527,13.922512079821,129.498952043521)) ;
#136935 = CARTESIAN_POINT('Ctrl Pts',(-28.1222933683625,13.6705375109782,
129.598054557402)) ;
#136936 = CARTESIAN_POINT('Ctrl Pts',(-28.1220048988863,13.4018845306058,
129.630275138781)) ;
#136937 = CARTESIAN_POINT('Ctrl Pts',(-28.0983744340301,13.1344381767143,
129.594340562343)) ;
#136938 = CARTESIAN_POINT('Ctrl Pts',(-28.05188015388,12.8864833216457,129.491795996965)) ;
#136939 = CARTESIAN_POINT('Ctrl Pts',(-27.9861062755655,12.6791960458196,
129.332582797579)) ;
#136940 = CARTESIAN_POINT('Ctrl Pts',(-27.9038435542885,12.5233811558849,
129.125499147987)) ;
#136941 = CARTESIAN_POINT('Ctrl Pts',(-27.8111043969776,12.4327816680599,
128.887676707755)) ;
#136942 = CARTESIAN_POINT('Ctrl Pts',(-27.7134087891038,12.412915954978,128.635426708969)) ;
#136943 = CARTESIAN_POINT('Ctrl Pts',(-27.6171947184772,12.4655032606852,
128.387484215435)) ;
#136944 = CARTESIAN_POINT('Ctrl Pts',(-27.528620482135,12.5866528980437,128.161850174214)) ;
#136945 = CARTESIAN_POINT('Ctrl Pts',(-27.4532574084139,12.7674395130523,
127.974785517744)) ;
#136946 = CARTESIAN_POINT('Ctrl Pts',(-27.3955179677537,12.996680662144,127.839402986817)) ;
#136947 = CARTESIAN_POINT('Ctrl Pts',(-27.3595338870752,13.2541240952596,
127.767245304833)) ;
#136948 = CARTESIAN_POINT('Ctrl Pts',(-27.3464077619685,13.5248420441081,
127.762028996665)) ;
#136949 = CARTESIAN_POINT('Ctrl Pts',(-27.356666975349,13.7882270430707,127.825112744732)) ;
#136950 = CARTESIAN_POINT('Ctrl Pts',(-27.3889352588637,14.026098281457,127.952588217587)) ;
#136951 = CARTESIAN_POINT('Ctrl Pts',(-27.4400200252131,14.220023125983,128.134939040121)) ;
#136952 = CARTESIAN_POINT('Ctrl Pts',(-27.5054425779506,14.3567721922805,
128.359124707489)) ;
#136953 = CARTESIAN_POINT('Ctrl Pts',(-27.5799717340147,14.4269174319569,
128.609946622311)) ;
#136954 = CARTESIAN_POINT('Ctrl Pts',(-27.6576169156365,14.4252573107259,
128.869919222744)) ;
#136955 = CARTESIAN_POINT('Ctrl Pts',(-27.7321017988657,14.3512845156984,
129.120733211293)) ;
#136956 = CARTESIAN_POINT('Ctrl Pts',(-27.7967359453251,14.2117350890935,
129.342525302038)) ;
#136957 = CARTESIAN_POINT('Ctrl Pts',(-27.8470386906761,14.0152549017169,
129.52261496323)) ;
#136958 = CARTESIAN_POINT('Ctrl Pts',(-27.8782495117232,13.7756400409677,
129.646998433737)) ;
#136959 = CARTESIAN_POINT('Ctrl Pts',(-27.8873911313969,13.512293601297,129.706715524423)) ;
#136960 = CARTESIAN_POINT('Ctrl Pts',(-27.8731583548882,13.24113011058,129.698336607786)) ;
#136961 = CARTESIAN_POINT('Ctrl Pts',(-27.8359087024829,12.9839533998787,
129.622589483103)) ;
#136962 = CARTESIAN_POINT('Ctrl Pts',(-27.7772389969083,12.757224045122,129.484428783906)) ;
#136963 = CARTESIAN_POINT('Ctrl Pts',(-27.7013420867903,12.5794741736853,
129.295717193307)) ;
#136964 = CARTESIAN_POINT('Ctrl Pts',(-27.61199789567,12.4611210903509,129.067932649301)) ;
#136965 = CARTESIAN_POINT('Ctrl Pts',(-27.5156597037437,12.4122668276836,
128.819593542146)) ;
#136966 = CARTESIAN_POINT('Ctrl Pts',(-27.4181724680739,12.4354395008957,
128.567907202221)) ;
#136967 = CARTESIAN_POINT('Ctrl Pts',(-27.325352341727,12.5301694700227,128.330034016627)) ;
#136968 = CARTESIAN_POINT('Ctrl Pts',(-27.2444119944152,12.6876686468163,
128.126545747607)) ;
#136969 = CARTESIAN_POINT('Ctrl Pts',(-27.1791191129236,12.8982124507683,
127.968922538508)) ;
#136970 = CARTESIAN_POINT('Ctrl Pts',(-27.1338326861557,13.1472879171854,
127.869844817616)) ;
#136971 = CARTESIAN_POINT('Ctrl Pts',(-27.1113227512545,13.4151706330379,
127.837176477762)) ;
#136972 = CARTESIAN_POINT('Ctrl Pts',(-27.1121984761234,13.6833052761831,
127.872788487339)) ;
#136973 = CARTESIAN_POINT('Ctrl Pts',(-27.1357131249715,13.9335262221531,
127.97461183381)) ;
#136974 = CARTESIAN_POINT('Ctrl Pts',(-27.1798239658889,14.1479664879784,
128.136760203425)) ;
#136975 = CARTESIAN_POINT('Ctrl Pts',(-27.2399210422133,14.3087959148104,
128.345327481302)) ;
#136976 = CARTESIAN_POINT('Ctrl Pts',(-27.3114169111032,14.4069520206095,
128.58726493726)) ;
#136977 = CARTESIAN_POINT('Ctrl Pts',(-27.38862876507,14.4347039368911,128.845984629067)) ;
#136978 = CARTESIAN_POINT('Ctrl Pts',(-27.4649895003704,14.3899170830749,
129.10217320422)) ;
#136979 = CARTESIAN_POINT('Ctrl Pts',(-27.5344215210273,14.2758481997907,
129.338132040779)) ;
#136980 = CARTESIAN_POINT('Ctrl Pts',(-27.5911283659314,14.1010294693846,
129.536862778471)) ;
#136981 = CARTESIAN_POINT('Ctrl Pts',(-27.6305468417763,13.8772034754541,
129.685173590359)) ;
#136982 = CARTESIAN_POINT('Ctrl Pts',(-27.6488943694278,13.6206147826081,
129.771944550201)) ;
#136983 = CARTESIAN_POINT('Ctrl Pts',(-27.6442384536181,13.3509222115741,
129.791386599852)) ;
#136984 = CARTESIAN_POINT('Ctrl Pts',(-27.616132866257,13.0853829719641,129.742455025968)) ;
#136985 = CARTESIAN_POINT('Ctrl Pts',(-27.5659241263139,12.8445476848772,
129.628889117042)) ;
#136986 = CARTESIAN_POINT('Ctrl Pts',(-27.4964177152632,12.644952930344,129.458978943419)) ;
#136987 = CARTESIAN_POINT('Ctrl Pts',(-27.4119515874544,12.5012606918104,
129.245340538602)) ;
#136988 = CARTESIAN_POINT('Ctrl Pts',(-27.3178276586184,12.4235056732711,
129.003484340073)) ;
#136989 = CARTESIAN_POINT('Ctrl Pts',(-27.2198616603803,12.417318606479,128.750460970837)) ;
#136990 = CARTESIAN_POINT('Ctrl Pts',(-27.1245890090358,12.4833714427519,
128.505283372717)) ;
#136991 = CARTESIAN_POINT('Ctrl Pts',(-27.0382770555464,12.6162285125256,
128.286182494922)) ;
#136992 = CARTESIAN_POINT('Ctrl Pts',(-26.9657884587366,12.8073409623945,
128.107588748283)) ;
#136993 = CARTESIAN_POINT('Ctrl Pts',(-26.91197273339,13.0432164497969,127.983598029365)) ;
#136994 = CARTESIAN_POINT('Ctrl Pts',(-26.8801365095611,13.3046948495717,
127.923605110898)) ;
#136995 = CARTESIAN_POINT('Ctrl Pts',(-26.8714475726995,13.5764462618644,
127.931458802618)) ;
#136996 = CARTESIAN_POINT('Ctrl Pts',(-26.8861390506494,13.8363549423102,
128.007514684919)) ;
#136997 = CARTESIAN_POINT('Ctrl Pts',(-26.9219756410579,14.0655921172455,
128.14516922602)) ;
#136998 = CARTESIAN_POINT('Ctrl Pts',(-26.9761724713165,14.2503953829721,
128.3366792907)) ;
#136999 = CARTESIAN_POINT('Ctrl Pts',(-27.0441067566407,14.3757153759899,
128.568369328025)) ;
#137000 = CARTESIAN_POINT('Ctrl Pts',(-27.119708134456,14.4321659861442,128.822325410149)) ;
#137001 = CARTESIAN_POINT('Ctrl Pts',(-27.1968293833805,14.4167343147861,
129.08060826829)) ;
#137002 = CARTESIAN_POINT('Ctrl Pts',(-27.2698051782105,14.3302900075088,
129.326910391088)) ;
#137003 = CARTESIAN_POINT('Ctrl Pts',(-27.3325244628476,14.1784243814557,
129.543326387964)) ;
#137004 = CARTESIAN_POINT('Ctrl Pts',(-27.3795172134242,13.971750794682,129.713846487644)) ;
#137005 = CARTESIAN_POINT('Ctrl Pts',(-27.4065121003142,13.7284357059757,
129.825586303865)) ;
#137006 = CARTESIAN_POINT('Ctrl Pts',(-27.411442494474,13.4606302027768,129.873232722216)) ;
#137007 = CARTESIAN_POINT('Ctrl Pts',(-27.3926620627969,13.190619216966,129.851547306682)) ;
#137008 = CARTESIAN_POINT('Ctrl Pts',(-27.3513990743719,12.9388679934988,
129.763965154305)) ;
#137009 = CARTESIAN_POINT('Ctrl Pts',(-27.2890472382881,12.7195132188822,
129.615095019132)) ;
#137010 = CARTESIAN_POINT('Ctrl Pts',(-27.2099509779105,12.5518557366653,
129.417169431718)) ;
#137011 = CARTESIAN_POINT('Ctrl Pts',(-27.1194048865831,12.4467157565619,
129.185641424037)) ;
#137012 = CARTESIAN_POINT('Ctrl Pts',(-27.0218870634375,12.4110145774925,
128.934027986269)) ;
#137013 = CARTESIAN_POINT('Ctrl Pts',(-26.9251985270549,12.4479828352211,
128.684575244082)) ;
#137014 = CARTESIAN_POINT('Ctrl Pts',(-26.8344156748515,12.5544308126574,
128.452487217202)) ;
#137015 = CARTESIAN_POINT('Ctrl Pts',(-26.7552540847317,12.7245572127077,
128.254559235342)) ;
#137016 = CARTESIAN_POINT('Ctrl Pts',(-26.6937193015478,12.9435039801677,
128.107866481436)) ;
#137017 = CARTESIAN_POINT('Ctrl Pts',(-26.6527533456264,13.1965754196772,
128.021262076669)) ;
#137018 = CARTESIAN_POINT('Ctrl Pts',(-26.6345818546693,13.4658054148295,
128.001239973814)) ;
#137019 = CARTESIAN_POINT('Ctrl Pts',(-26.6398440618961,13.7328709435355,
128.049786254539)) ;
#137020 = CARTESIAN_POINT('Ctrl Pts',(-26.6674841230862,13.9772572574738,
128.163645532069)) ;
#137021 = CARTESIAN_POINT('Ctrl Pts',(-26.7147375930126,14.1820528886268,
128.33480544544)) ;
#137022 = CARTESIAN_POINT('Ctrl Pts',(-26.7777583985121,14.3328843450188,
128.552131428521)) ;
#137023 = CARTESIAN_POINT('Ctrl Pts',(-26.8509440034052,14.4178010956835,
128.799064816972)) ;
#137024 = CARTESIAN_POINT('Ctrl Pts',(-26.9280312466132,14.4318123970992,
129.057219724161)) ;
#137025 = CARTESIAN_POINT('Ctrl Pts',(-27.0039631337358,14.3732303174577,
129.312341756014)) ;
#137026 = CARTESIAN_POINT('Ctrl Pts',(-27.0711704740135,14.246970367672,129.541698456142)) ;
#137027 = CARTESIAN_POINT('Ctrl Pts',(-27.1249090976529,14.0621465768449,
129.731735704159)) ;
#137028 = CARTESIAN_POINT('Ctrl Pts',(-27.1606059412427,13.8305008090445,
129.869217691575)) ;
#137029 = CARTESIAN_POINT('Ctrl Pts',(-27.1746889753248,13.5704782336575,
129.943442839551)) ;
#137030 = CARTESIAN_POINT('Ctrl Pts',(-27.1655792705688,13.2994607453498,
129.949975686195)) ;
#137031 = CARTESIAN_POINT('Ctrl Pts',(-27.133176892415,13.0377344275702,129.888411790656)) ;
#137032 = CARTESIAN_POINT('Ctrl Pts',(-27.0791944720116,12.8036246677019,
129.763785021152)) ;
#137033 = CARTESIAN_POINT('Ctrl Pts',(-27.0062821178587,12.6130123925856,
129.58402121372)) ;
#137034 = CARTESIAN_POINT('Ctrl Pts',(-26.9196663424445,12.4813447985494,
129.364056212953)) ;
#137035 = CARTESIAN_POINT('Ctrl Pts',(-26.8242420692028,12.4167223946536,
129.118448864076)) ;
#137036 = CARTESIAN_POINT('Ctrl Pts',(-26.7263952125267,12.4243655838416,
128.865737206127)) ;
#137037 = CARTESIAN_POINT('Ctrl Pts',(-26.6324009307372,12.5034382504578,
128.624259769196)) ;
#137038 = CARTESIAN_POINT('Ctrl Pts',(-26.5481314271763,12.6484425830615,
128.411216523542)) ;
#137039 = CARTESIAN_POINT('Ctrl Pts',(-26.4789570120788,12.8490571219356,
128.242281700259)) ;
#137040 = CARTESIAN_POINT('Ctrl Pts',(-26.4291671135027,13.0907448949446,
128.129961496988)) ;
#137041 = CARTESIAN_POINT('Ctrl Pts',(-26.4015577929671,13.3559777711551,
128.082404456019)) ;
#137042 = CARTESIAN_POINT('Ctrl Pts',(-26.3973692775735,13.6264772467065,
128.103324558719)) ;
#137043 = CARTESIAN_POINT('Ctrl Pts',(-26.4161290926396,13.8815733250424,
128.191173426764)) ;
#137044 = CARTESIAN_POINT('Ctrl Pts',(-26.4558018566002,14.1045282295606,
128.340192241249)) ;
#137045 = CARTESIAN_POINT('Ctrl Pts',(-26.5130348991941,14.2789670310199,
128.540593076948)) ;
#137046 = CARTESIAN_POINT('Ctrl Pts',(-26.5826080859745,14.3914951662386,
128.776928435221)) ;
#137047 = CARTESIAN_POINT('Ctrl Pts',(-26.6590559552618,14.4348607606962,
129.033377878272)) ;
#137048 = CARTESIAN_POINT('Ctrl Pts',(-26.7361279143954,14.4056890546892,
129.291651441273)) ;
#137049 = CARTESIAN_POINT('Ctrl Pts',(-26.807530292351,14.3062653173801,129.533337989376)) ;
#137050 = CARTESIAN_POINT('Ctrl Pts',(-26.8674978374188,14.1434405254574,
129.741649803858)) ;
#137051 = CARTESIAN_POINT('Ctrl Pts',(-26.9109484293722,13.9296996080406,
129.901626502744)) ;
#137052 = CARTESIAN_POINT('Ctrl Pts',(-26.9342104512912,13.6772902050266,
130.002938697121)) ;
#137053 = CARTESIAN_POINT('Ctrl Pts',(-26.9345509523393,13.4099497148623,
130.036858568768)) ;
#137054 = CARTESIAN_POINT('Ctrl Pts',(-26.911574948467,13.1418739584321,130.002879415227)) ;
#137055 = CARTESIAN_POINT('Ctrl Pts',(-26.8659145129542,12.8939990940818,
129.90263809472)) ;
#137056 = CARTESIAN_POINT('Ctrl Pts',(-26.8005350813149,12.6844791174551,
129.744684127644)) ;
#137057 = CARTESIAN_POINT('Ctrl Pts',(-26.7182272801976,12.5265062887792,
129.537620729892)) ;
#137058 = CARTESIAN_POINT('Ctrl Pts',(-26.6261818479671,12.4345049990361,
129.301652381516)) ;
#137059 = CARTESIAN_POINT('Ctrl Pts',(-26.5282261254205,12.4124896095147,
129.04875220205)) ;
#137060 = CARTESIAN_POINT('Ctrl Pts',(-26.4322917120542,12.4629154785975,
128.801487434298)) ;
#137061 = CARTESIAN_POINT('Ctrl Pts',(-26.3432251854872,12.5820912201831,
128.574467292554)) ;
#137062 = CARTESIAN_POINT('Ctrl Pts',(-26.2671581421373,12.7624371254393,
128.385498413564)) ;
#137063 = CARTESIAN_POINT('Ctrl Pts',(-26.2094237671192,12.9881391647597,
128.249786258131)) ;
#137064 = CARTESIAN_POINT('Ctrl Pts',(-26.1724245557909,13.2462582186001,
128.174853451086)) ;
#137065 = CARTESIAN_POINT('Ctrl Pts',(-26.1586794395876,13.5176870879671,
128.167919605747)) ;
#137066 = CARTESIAN_POINT('Ctrl Pts',(-26.1682601316726,13.7805943652363,
128.228904238184)) ;
#137067 = CARTESIAN_POINT('Ctrl Pts',(-26.1998860836901,14.0195268693382,
128.35450332008)) ;
#137068 = CARTESIAN_POINT('Ctrl Pts',(-26.2504691063118,14.2150384579935,
128.535393340333)) ;
#137069 = CARTESIAN_POINT('Ctrl Pts',(-26.3156944845117,14.3538332405852,
128.759076824619)) ;
#137070 = CARTESIAN_POINT('Ctrl Pts',(-26.3899618416788,14.4259646788893,
129.009091256447)) ;
#137071 = CARTESIAN_POINT('Ctrl Pts',(-26.4678956866111,14.4260802935488,
129.270038211653)) ;
#137072 = CARTESIAN_POINT('Ctrl Pts',(-26.5418878654518,14.3549351031628,
129.519100877499)) ;
#137073 = CARTESIAN_POINT('Ctrl Pts',(-26.6074625898789,14.2162529727103,
129.743922519442)) ;
#137074 = CARTESIAN_POINT('Ctrl Pts',(-26.6580452321054,14.0213157651239,
129.924758738153)) ;
#137075 = CARTESIAN_POINT('Ctrl Pts',(-26.6898532286372,13.7835943457729,
130.050782470753)) ;
#137076 = CARTESIAN_POINT('Ctrl Pts',(-26.6996483276662,13.5186609566866,
130.112664324409)) ;
#137077 = CARTESIAN_POINT('Ctrl Pts',(-26.6861549241806,13.2494163240999,
130.106191722595)) ;
#137078 = CARTESIAN_POINT('Ctrl Pts',(-26.6493702443734,12.9903692068144,
130.031973073397)) ;
#137079 = CARTESIAN_POINT('Ctrl Pts',(-26.591620486111,12.7636901200826,129.896303906618)) ;
#137080 = CARTESIAN_POINT('Ctrl Pts',(-26.5154518565401,12.5829314316244,
129.707103805501)) ;
#137081 = CARTESIAN_POINT('Ctrl Pts',(-26.4273296697944,12.4640788592141,
129.482529198083)) ;
#137082 = CARTESIAN_POINT('Ctrl Pts',(-26.3305930618283,12.4125693600516,
129.233221648972)) ;
#137083 = CARTESIAN_POINT('Ctrl Pts',(-26.2333657019323,12.433709410136,128.982182141248)) ;
#137084 = CARTESIAN_POINT('Ctrl Pts',(-26.1402024934681,12.5263145122891,
128.743340215982)) ;
#137085 = CARTESIAN_POINT('Ctrl Pts',(-26.0587798870192,12.682258725893,128.538473987008)) ;
#137086 = CARTESIAN_POINT('Ctrl Pts',(-25.9929595121332,12.8915625393506,
128.379320359343)) ;
#137087 = CARTESIAN_POINT('Ctrl Pts',(-25.9470977802172,13.1392602988437,
128.278495272757)) ;
#137088 = CARTESIAN_POINT('Ctrl Pts',(-25.923848945908,13.4076118605944,128.243769009844)) ;
#137089 = CARTESIAN_POINT('Ctrl Pts',(-25.9240227025973,13.6757335665798,
128.277286286111)) ;
#137090 = CARTESIAN_POINT('Ctrl Pts',(-25.9471968230485,13.9281677275871,
128.378335497117)) ;
#137091 = CARTESIAN_POINT('Ctrl Pts',(-25.9901765099646,14.1410411517753,
128.536727728813)) ;
#137092 = CARTESIAN_POINT('Ctrl Pts',(-26.0502174839161,14.305185990512,128.745389721773)) ;
#137093 = CARTESIAN_POINT('Ctrl Pts',(-26.1214648073103,14.4050577723151,
128.98657892307)) ;
#137094 = CARTESIAN_POINT('Ctrl Pts',(-26.1986808777145,14.4349188595374,
129.24534957222)) ;
#137095 = CARTESIAN_POINT('Ctrl Pts',(-26.2750125302576,14.3922309403959,
129.501391075404)) ;
#137096 = CARTESIAN_POINT('Ctrl Pts',(-26.3447157195158,14.2801808361509,
129.738135053733)) ;
#137097 = CARTESIAN_POINT('Ctrl Pts',(-26.4019169360842,14.1070360328529,
129.938316871328)) ;
#137098 = CARTESIAN_POINT('Ctrl Pts',(-26.442001427727,13.8833119932821,130.088719159854)) ;
#137099 = CARTESIAN_POINT('Ctrl Pts',(-26.4608722515451,13.6288342780485,
130.176828146041)) ;
#137100 = CARTESIAN_POINT('Ctrl Pts',(-26.4568988722014,13.3582466690145,
130.198396750865)) ;
#137101 = CARTESIAN_POINT('Ctrl Pts',(-26.4295097212651,13.0930922580285,
130.151455564506)) ;
#137102 = CARTESIAN_POINT('Ctrl Pts',(-26.3798739225849,12.8509541830077,
130.03960846532)) ;
#137103 = CARTESIAN_POINT('Ctrl Pts',(-26.3109011279355,12.6500625833759,
129.871238266472)) ;
#137104 = CARTESIAN_POINT('Ctrl Pts',(-26.2266721288439,12.504322047528,129.658344470603)) ;
#137105 = CARTESIAN_POINT('Ctrl Pts',(-26.1325625349995,12.4246931678785,
129.41658611775)) ;
#137106 = CARTESIAN_POINT('Ctrl Pts',(-26.0351158553051,12.416496187653,129.164910619629)) ;
#137107 = CARTESIAN_POINT('Ctrl Pts',(-25.9396110218934,12.4802513742885,
128.919072246389)) ;
#137108 = CARTESIAN_POINT('Ctrl Pts',(-25.852731120451,12.6116452281821,128.698399944407)) ;
#137109 = CARTESIAN_POINT('Ctrl Pts',(-25.7798786336614,12.8011771463769,
128.518710754517)) ;
#137110 = CARTESIAN_POINT('Ctrl Pts',(-25.7255934891361,13.0350449035092,
128.393230108689)) ;
#137111 = CARTESIAN_POINT('Ctrl Pts',(-25.6929390835032,13.2969779492496,
128.330976980489)) ;
#137112 = CARTESIAN_POINT('Ctrl Pts',(-25.6836018345808,13.5677345965553,
128.336810948533)) ;
#137113 = CARTESIAN_POINT('Ctrl Pts',(-25.6975030410831,13.8283851031189,
128.410563145185)) ;
#137114 = CARTESIAN_POINT('Ctrl Pts',(-25.7329373000182,14.0598713577401,
128.547204922732)) ;
#137115 = CARTESIAN_POINT('Ctrl Pts',(-25.7865616994345,14.2455587170749,
128.736952477156)) ;
#137116 = CARTESIAN_POINT('Ctrl Pts',(-25.8538626621655,14.3725641249717,
128.966665310634)) ;
#137117 = CARTESIAN_POINT('Ctrl Pts',(-25.9295581721334,14.4315964655583,
129.221010674223)) ;
#137118 = CARTESIAN_POINT('Ctrl Pts',(-26.006896602782,14.4181824327013,129.480002352547)) ;
#137119 = CARTESIAN_POINT('Ctrl Pts',(-26.0800584448921,14.3336378405054,
129.726841816837)) ;
#137120 = CARTESIAN_POINT('Ctrl Pts',(-26.1429821311044,14.1840091545094,
129.943759080814)) ;
#137121 = CARTESIAN_POINT('Ctrl Pts',(-26.1905534207569,13.9789558731559,
130.115961872093)) ;
#137122 = CARTESIAN_POINT('Ctrl Pts',(-26.2182982510239,13.7355808052625,
130.230023298186)) ;
#137123 = CARTESIAN_POINT('Ctrl Pts',(-26.2237942797622,13.4678622499821,
130.279352827581)) ;
#137124 = CARTESIAN_POINT('Ctrl Pts',(-26.2058494672465,13.1991328428123,
130.259921864044)) ;
#137125 = CARTESIAN_POINT('Ctrl Pts',(-26.1650019081548,12.9452257319575,
130.173741107483)) ;
#137126 = CARTESIAN_POINT('Ctrl Pts',(-26.1035333591206,12.7259341486132,
130.027259340735)) ;
#137127 = CARTESIAN_POINT('Ctrl Pts',(-26.0247947651335,12.5559411201038,
129.830445570047)) ;
#137128 = CARTESIAN_POINT('Ctrl Pts',(-25.9339940341689,12.4485460987932,
129.598349481578)) ;
#137129 = CARTESIAN_POINT('Ctrl Pts',(-25.8371492819582,12.4111599413339,
129.348503860636)) ;
#137130 = CARTESIAN_POINT('Ctrl Pts',(-25.7402515382401,12.4456278255399,
129.098470636215)) ;
#137131 = CARTESIAN_POINT('Ctrl Pts',(-25.6485459840358,12.5514145660075,
128.863951218949)) ;
#137132 = CARTESIAN_POINT('Ctrl Pts',(-25.5698638699777,12.7181519497096,
128.667054512607)) ;
#137133 = CARTESIAN_POINT('Ctrl Pts',(-25.5074380429627,12.9364297066312,
128.517889419159)) ;
#137134 = CARTESIAN_POINT('Ctrl Pts',(-25.4658667658109,13.1887531775189,
128.42950707232)) ;
#137135 = CARTESIAN_POINT('Ctrl Pts',(-25.4469754063975,13.4580633206524,
128.407419238398)) ;
#137136 = CARTESIAN_POINT('Ctrl Pts',(-25.451607744199,13.7256377650323,128.454145515707)) ;
#137137 = CARTESIAN_POINT('Ctrl Pts',(-25.478575349501,13.9704139197111,128.565972664552)) ;
#137138 = CARTESIAN_POINT('Ctrl Pts',(-25.5253124387396,14.1767864101741,
128.735643536007)) ;
#137139 = CARTESIAN_POINT('Ctrl Pts',(-25.5879676204535,14.3292888333563,
128.951905035728)) ;
#137140 = CARTESIAN_POINT('Ctrl Pts',(-25.6606881108518,14.4162418922063,
129.197374916368)) ;
#137141 = CARTESIAN_POINT('Ctrl Pts',(-25.7382280461626,14.4323070636622,
129.457069048766)) ;
#137142 = CARTESIAN_POINT('Ctrl Pts',(-25.8136145906716,14.3764282690484,
129.710284803776)) ;
#137143 = CARTESIAN_POINT('Ctrl Pts',(-25.8816430048817,14.2515625943371,
129.942266343958)) ;
#137144 = CARTESIAN_POINT('Ctrl Pts',(-25.9358089722647,14.0682229013696,
130.133536052826)) ;
#137145 = CARTESIAN_POINT('Ctrl Pts',(-25.9721443127368,13.8370234728167,
130.27297416193)) ;
#137146 = CARTESIAN_POINT('Ctrl Pts',(-25.9867897769764,13.5786250860868,
130.348703835847)) ;
#137147 = CARTESIAN_POINT('Ctrl Pts',(-25.9784177256828,13.3076278419877,
130.357397820919)) ;
#137148 = CARTESIAN_POINT('Ctrl Pts',(-25.946711000963,13.0452574114126,130.29787280956)) ;
#137149 = CARTESIAN_POINT('Ctrl Pts',(-25.8930679516197,12.809151348438,130.17437735159)) ;
#137150 = CARTESIAN_POINT('Ctrl Pts',(-25.820675289845,12.6175516783773,129.996081228465)) ;
#137151 = CARTESIAN_POINT('Ctrl Pts',(-25.7346394044431,12.4843718423873,
129.777720227258)) ;
#137152 = CARTESIAN_POINT('Ctrl Pts',(-25.6392954299083,12.417595884224,129.532379981805)) ;
#137153 = CARTESIAN_POINT('Ctrl Pts',(-25.5415392329717,12.4230554793737,
129.2798939571)) ;
#137154 = CARTESIAN_POINT('Ctrl Pts',(-25.44720407137,12.5002516157562,129.037475794767)) ;
#137155 = CARTESIAN_POINT('Ctrl Pts',(-25.3627875475538,12.6429370956148,
128.823904379455)) ;
#137156 = CARTESIAN_POINT('Ctrl Pts',(-25.2927915452869,12.8430358914049,
128.652724826988)) ;
#137157 = CARTESIAN_POINT('Ctrl Pts',(-25.2425908671118,13.0829430235275,
128.539082315147)) ;
#137158 = CARTESIAN_POINT('Ctrl Pts',(-25.2142446030042,13.3482625175679,
128.489444003025)) ;
#137159 = CARTESIAN_POINT('Ctrl Pts',(-25.2093485809571,13.6179804749313,
128.508179789217)) ;
#137160 = CARTESIAN_POINT('Ctrl Pts',(-25.2275485580834,13.8754577443227,
128.59460738022)) ;
#137161 = CARTESIAN_POINT('Ctrl Pts',(-25.2668351056179,14.0994367889634,
128.742519747541)) ;
#137162 = CARTESIAN_POINT('Ctrl Pts',(-25.3232457097912,14.2743408092093,
128.94029910677)) ;
#137163 = CARTESIAN_POINT('Ctrl Pts',(-25.3927071649368,14.3892596649761,
129.176405541247)) ;
#137164 = CARTESIAN_POINT('Ctrl Pts',(-25.4689980053617,14.4346258039945,
129.432371808498)) ;
#137165 = CARTESIAN_POINT('Ctrl Pts',(-25.5463449745986,14.4074612367265,
129.691535915979)) ;
#137166 = CARTESIAN_POINT('Ctrl Pts',(-25.617936621825,14.3096987873791,129.93377050553)) ;
#137167 = CARTESIAN_POINT('Ctrl Pts',(-25.6780966245885,14.1493774053066,
130.142501646616)) ;
#137168 = CARTESIAN_POINT('Ctrl Pts',(-25.7222855141894,13.9355628673905,
130.304835839477)) ;
#137169 = CARTESIAN_POINT('Ctrl Pts',(-25.7460052192223,13.6861606086544,
130.407190418653)) ;
#137170 = CARTESIAN_POINT('Ctrl Pts',(-25.7470805202155,13.4167352141788,
130.443555111418)) ;
#137171 = CARTESIAN_POINT('Ctrl Pts',(-25.7247262193035,13.1492793403457,
130.411279088771)) ;
#137172 = CARTESIAN_POINT('Ctrl Pts',(-25.6797214030516,12.9005268822979,
130.312955257449)) ;
#137173 = CARTESIAN_POINT('Ctrl Pts',(-25.6147970669545,12.6897474327515,
130.15634284889)) ;
#137174 = CARTESIAN_POINT('Ctrl Pts',(-25.5332896147307,12.5306016381553,
129.951467636062)) ;
#137175 = CARTESIAN_POINT('Ctrl Pts',(-25.4410148555985,12.4360458908817,
129.71500187315)) ;
#137176 = CARTESIAN_POINT('Ctrl Pts',(-25.3432666007832,12.412131814103,129.462653094517)) ;
#137177 = CARTESIAN_POINT('Ctrl Pts',(-25.247007374808,12.4605357915181,129.214505440553)) ;
#137178 = CARTESIAN_POINT('Ctrl Pts',(-25.1575767032805,12.5784164167772,
128.986475142405)) ;
#137179 = CARTESIAN_POINT('Ctrl Pts',(-25.0816726489816,12.75548162504,128.797692124086)) ;
#137180 = CARTESIAN_POINT('Ctrl Pts',(-25.0228641768447,12.9817623745855,
128.659113501594)) ;
#137181 = CARTESIAN_POINT('Ctrl Pts',(-24.9854431235873,13.2381597682889,
128.58279479078)) ;
#137182 = CARTESIAN_POINT('Ctrl Pts',(-24.9709442140284,13.5101991451629,
128.573753044088)) ;
#137183 = CARTESIAN_POINT('Ctrl Pts',(-24.9798702789117,13.7733130624052,
128.632787335484)) ;
#137184 = CARTESIAN_POINT('Ctrl Pts',(-25.0110723397697,14.0140640637462,
128.757279546855)) ;
#137185 = CARTESIAN_POINT('Ctrl Pts',(-25.0609598922125,14.2098744225724,
128.935968377652)) ;
#137186 = CARTESIAN_POINT('Ctrl Pts',(-25.1257461413825,14.3505801926375,
129.158347749617)) ;
#137187 = CARTESIAN_POINT('Ctrl Pts',(-25.1999128259953,14.4248316495575,
129.408106389125)) ;
#137188 = CARTESIAN_POINT('Ctrl Pts',(-25.2777575377082,14.4272048200234,
129.668752235258)) ;
#137189 = CARTESIAN_POINT('Ctrl Pts',(-25.3521251101368,14.3577939953671,
129.919009377019)) ;
#137190 = CARTESIAN_POINT('Ctrl Pts',(-25.4177703520866,14.2217458175161,
130.143874634482)) ;
#137191 = CARTESIAN_POINT('Ctrl Pts',(-25.4692388352905,14.0267542055663,
130.327561274206)) ;
#137192 = CARTESIAN_POINT('Ctrl Pts',(-25.5013721592421,13.7911380978429,
130.454356036342)) ;
#137193 = CARTESIAN_POINT('Ctrl Pts',(-25.511924687266,13.5273991680406,130.518376373105)) ;
#137194 = CARTESIAN_POINT('Ctrl Pts',(-25.4991050868109,13.2571617641776,
130.51398320948)) ;
#137195 = CARTESIAN_POINT('Ctrl Pts',(-25.4629538937068,12.9974109548792,
130.441621863609)) ;
#137196 = CARTESIAN_POINT('Ctrl Pts',(-25.4056927623469,12.7695380249157,
130.307406345911)) ;
#137197 = CARTESIAN_POINT('Ctrl Pts',(-25.33042840628,12.5879937236174,130.120669835219)) ;
#137198 = CARTESIAN_POINT('Ctrl Pts',(-25.2420766509654,12.4663339906868,
129.895635723357)) ;
#137199 = CARTESIAN_POINT('Ctrl Pts',(-25.1454696806416,12.41305303315,129.64669692387)) ;
#137200 = CARTESIAN_POINT('Ctrl Pts',(-25.048369544625,12.4321501041493,129.395973750274)) ;
#137201 = CARTESIAN_POINT('Ctrl Pts',(-24.9551458762365,12.522410787778,129.156886231369)) ;
#137202 = CARTESIAN_POINT('Ctrl Pts',(-24.8729558359052,12.677312203341,128.949927053074)) ;
#137203 = CARTESIAN_POINT('Ctrl Pts',(-24.8067307250646,12.8853931735732,
128.789574538439)) ;
#137204 = CARTESIAN_POINT('Ctrl Pts',(-24.7604114391819,13.1311434381669,
128.687274602819)) ;
#137205 = CARTESIAN_POINT('Ctrl Pts',(-24.7363638964199,13.4000886870271,
128.650328698818)) ;
#137206 = CARTESIAN_POINT('Ctrl Pts',(-24.7359629848961,13.667985481151,128.682120218875)) ;
#137207 = CARTESIAN_POINT('Ctrl Pts',(-24.7581853104846,13.9198929118074,
128.780178599926)) ;
#137208 = CARTESIAN_POINT('Ctrl Pts',(-24.801208903198,14.13673316727,128.939133160208)) ;
#137209 = CARTESIAN_POINT('Ctrl Pts',(-24.8602641638815,14.300676131018,129.144561484622)) ;
#137210 = CARTESIAN_POINT('Ctrl Pts',(-24.9316995313073,14.4034182516523,
129.386532253094)) ;
#137211 = CARTESIAN_POINT('Ctrl Pts',(-25.008652081806,14.4350219439221,129.644438670051)) ;
#137212 = CARTESIAN_POINT('Ctrl Pts',(-25.085177028276,14.3943912099649,129.901089775853)) ;
#137213 = CARTESIAN_POINT('Ctrl Pts',(-25.1551357368836,14.2842181242634,
130.138566635532)) ;
#137214 = CARTESIAN_POINT('Ctrl Pts',(-25.2127728109964,14.11233380319,130.340059721754)) ;
#137215 = CARTESIAN_POINT('Ctrl Pts',(-25.2531900001201,13.8914433444145,
130.491203497753)) ;
#137216 = CARTESIAN_POINT('Ctrl Pts',(-25.2728802791194,13.6364806192018,
130.581877006212)) ;
#137217 = CARTESIAN_POINT('Ctrl Pts',(-25.2695691902487,13.3663281974235,
130.60534009255)) ;
#137218 = CARTESIAN_POINT('Ctrl Pts',(-25.2428141688484,13.1002905199636,
130.560312718125)) ;
#137219 = CARTESIAN_POINT('Ctrl Pts',(-25.1937738940479,12.8573187097229,
130.450194224165)) ;
#137220 = CARTESIAN_POINT('Ctrl Pts',(-25.1252949558094,12.6550559201632,
130.28326882404)) ;
#137221 = CARTESIAN_POINT('Ctrl Pts',(-25.041522175675,12.5076995201524,130.071671442903)) ;
#137222 = CARTESIAN_POINT('Ctrl Pts',(-24.9476355648718,12.4260782231414,
129.830561197084)) ;
#137223 = CARTESIAN_POINT('Ctrl Pts',(-24.8502501407946,12.4155414284777,
129.579046625511)) ;
#137224 = CARTESIAN_POINT('Ctrl Pts',(-24.7538966162756,12.4780902528913,
129.330983042156)) ;
#137225 = CARTESIAN_POINT('Ctrl Pts',(-24.6675208764697,12.6066343285888,
129.111475024232)) ;
#137226 = CARTESIAN_POINT('Ctrl Pts',(-24.5938515785469,12.7952135376049,
128.9295353476)) ;
#137227 = CARTESIAN_POINT('Ctrl Pts',(-24.5390606686421,13.0279818005268,
128.802553603919)) ;
#137228 = CARTESIAN_POINT('Ctrl Pts',(-24.5057245134978,13.2896873731217,
128.73835017349)) ;
#137229 = CARTESIAN_POINT('Ctrl Pts',(-24.4957718456139,13.5603127148141,
128.742368279822)) ;
#137230 = CARTESIAN_POINT('Ctrl Pts',(-24.5089980783373,13.8211026709328,
128.814095191955)) ;
#137231 = CARTESIAN_POINT('Ctrl Pts',(-24.5438612527322,14.0538031496825,
128.949086534568)) ;
#137232 = CARTESIAN_POINT('Ctrl Pts',(-24.5970360172465,14.2410907162982,
129.137531563715)) ;
#137233 = CARTESIAN_POINT('Ctrl Pts',(-24.6642374142229,14.3701940931664,
129.367050561935)) ;
#137234 = CARTESIAN_POINT('Ctrl Pts',(-24.7397318651878,14.4308809460844,
129.62077656555)) ;
#137235 = CARTESIAN_POINT('Ctrl Pts',(-24.8168605982929,14.4196139003572,
129.879052696967)) ;
#137236 = CARTESIAN_POINT('Ctrl Pts',(-24.8904031542241,14.336836882695,130.127084143124)) ;
#137237 = CARTESIAN_POINT('Ctrl Pts',(-24.9535128568133,14.1892311561633,
130.344459510931)) ;
#137238 = CARTESIAN_POINT('Ctrl Pts',(-25.001609263022,13.9859053785223,130.518165732824)) ;
#137239 = CARTESIAN_POINT('Ctrl Pts',(-25.0300402506867,13.7426112517957,
130.634341797192)) ;
#137240 = CARTESIAN_POINT('Ctrl Pts',(-25.0361683447046,13.4761438814329,
130.685407728846)) ;
#137241 = CARTESIAN_POINT('Ctrl Pts',(-25.0189583644701,13.2070931774866,
130.668139714786)) ;
#137242 = CARTESIAN_POINT('Ctrl Pts',(-24.97869544815,12.9521503928351,130.583708331341)) ;
#137243 = CARTESIAN_POINT('Ctrl Pts',(-24.9177844273565,12.7315094289201,
130.438861249866)) ;
#137244 = CARTESIAN_POINT('Ctrl Pts',(-24.8391101053067,12.55952255891,130.242364324163)) ;
#137245 = CARTESIAN_POINT('Ctrl Pts',(-24.7493048000512,12.4509681348577,
130.012910139936)) ;
#137246 = CARTESIAN_POINT('Ctrl Pts',(-24.6517732733907,12.4111337654698,
129.761332887985)) ;
#137247 = CARTESIAN_POINT('Ctrl Pts',(-24.5552548880009,12.4436883987287,
129.512247618014)) ;
#137248 = CARTESIAN_POINT('Ctrl Pts',(-24.4632268332124,12.5474867410868,
129.276810629961)) ;
#137249 = CARTESIAN_POINT('Ctrl Pts',(-24.3842162437121,12.7123018104689,
129.078905084089)) ;
#137250 = CARTESIAN_POINT('Ctrl Pts',(-24.3210840647397,12.930070804837,128.927784936673)) ;
#137251 = CARTESIAN_POINT('Ctrl Pts',(-24.2790719777108,13.1802337484168,
128.837930667053)) ;
#137252 = CARTESIAN_POINT('Ctrl Pts',(-24.2593594113849,13.4510759105696,
128.813665180465)) ;
#137253 = CARTESIAN_POINT('Ctrl Pts',(-24.2633748242578,13.7180592820174,
128.858471439146)) ;
#137254 = CARTESIAN_POINT('Ctrl Pts',(-24.2897810253052,13.9642785857624,
128.968736525003)) ;
#137255 = CARTESIAN_POINT('Ctrl Pts',(-24.3359172579478,14.1712561448263,
129.136557180843)) ;
#137256 = CARTESIAN_POINT('Ctrl Pts',(-24.3979070515482,14.3253724982605,
129.350764867934)) ;
#137257 = CARTESIAN_POINT('Ctrl Pts',(-24.4709758873292,14.4148742496936,
129.597512003327)) ;
#137258 = CARTESIAN_POINT('Ctrl Pts',(-24.5478797311828,14.4329087927554,
129.855085425243)) ;
#137259 = CARTESIAN_POINT('Ctrl Pts',(-24.6239219034766,14.3788838662948,
130.110446558237)) ;
#137260 = CARTESIAN_POINT('Ctrl Pts',(-24.692012674099,14.2561020385484,130.342495417094)) ;
#137261 = CARTESIAN_POINT('Ctrl Pts',(-24.7466767208365,14.0742378905462,
130.535245795861)) ;
#137262 = CARTESIAN_POINT('Ctrl Pts',(-24.7834767939557,13.8451951074059,
130.675901048507)) ;
#137263 = CARTESIAN_POINT('Ctrl Pts',(-24.7989416578835,13.5867436924812,
130.754122251571)) ;
#137264 = CARTESIAN_POINT('Ctrl Pts',(-24.7911326203798,13.3144406104729,
130.764624304837)) ;
#137265 = CARTESIAN_POINT('Ctrl Pts',(-24.760168773577,13.0528697153062,130.707111677067)) ;
#137266 = CARTESIAN_POINT('Ctrl Pts',(-24.7072987550556,12.8160519673843,
130.585813252149)) ;
#137267 = CARTESIAN_POINT('Ctrl Pts',(-24.6353533732366,12.6226066577663,
130.408861363044)) ;
#137268 = CARTESIAN_POINT('Ctrl Pts',(-24.5494827855599,12.4871997727771,
130.1910537292)) ;
#137269 = CARTESIAN_POINT('Ctrl Pts',(-24.4539509697658,12.4184347906441,
129.945282406851)) ;
#137270 = CARTESIAN_POINT('Ctrl Pts',(-24.3567514327947,12.421900095689,129.694230668796)) ;
#137271 = CARTESIAN_POINT('Ctrl Pts',(-24.2621043582377,12.4968773890891,
129.450935185036)) ;
#137272 = CARTESIAN_POINT('Ctrl Pts',(-24.1771968895545,12.6381725134135,
129.235992950347)) ;
#137273 = CARTESIAN_POINT('Ctrl Pts',(-24.1068996585392,12.8360676034159,
129.063819100228)) ;
#137274 = CARTESIAN_POINT('Ctrl Pts',(-24.0558483744943,13.0762564614049,
128.947865518948)) ;
#137275 = CARTESIAN_POINT('Ctrl Pts',(-24.0270075658694,13.3398739353009,
128.896618474856)) ;
#137276 = CARTESIAN_POINT('Ctrl Pts',(-24.0213604180131,13.6103042607725,
128.913234992603)) ;
#137277 = CARTESIAN_POINT('Ctrl Pts',(-24.0389205379422,13.8681248638129,
128.997754741653)) ;
#137278 = CARTESIAN_POINT('Ctrl Pts',(-24.0775340449391,14.0932870641316,
129.14367411103)) ;
#137279 = CARTESIAN_POINT('Ctrl Pts',(-24.1339243216249,14.2707836154913,
129.341616284265)) ;
#137280 = CARTESIAN_POINT('Ctrl Pts',(-24.2026976504377,14.3866738270234,
129.575503449419)) ;
#137281 = CARTESIAN_POINT('Ctrl Pts',(-24.2789122688586,14.4343395634598,
129.831274305498)) ;
#137282 = CARTESIAN_POINT('Ctrl Pts',(-24.3561654891957,14.4093417232231,
130.090097199801)) ;
#137283 = CARTESIAN_POINT('Ctrl Pts',(-24.4280593379148,14.3139583409208,
130.333211542835)) ;
#137284 = CARTESIAN_POINT('Ctrl Pts',(-24.4890184297721,14.1538396198972,
130.544536166567)) ;
#137285 = CARTESIAN_POINT('Ctrl Pts',(-24.5333312219411,13.9434082159672,
130.706904626891)) ;
#137286 = CARTESIAN_POINT('Ctrl Pts',(-24.5579214950625,13.6926166151685,
130.812110819993)) ;
#137287 = CARTESIAN_POINT('Ctrl Pts',(-24.5595818848025,13.4252309496683,
130.849953790189)) ;
#137288 = CARTESIAN_POINT('Ctrl Pts',(-24.5379430220355,13.1569924841194,
130.81983442348)) ;
#137289 = CARTESIAN_POINT('Ctrl Pts',(-24.4936001603481,12.907415746913,130.723430091029)) ;
#137290 = CARTESIAN_POINT('Ctrl Pts',(-24.4288932095814,12.6946405642384,
130.567589996659)) ;
#137291 = CARTESIAN_POINT('Ctrl Pts',(-24.3483707094481,12.5348309351463,
130.365354677471)) ;
#137292 = CARTESIAN_POINT('Ctrl Pts',(-24.2557580076912,12.4376124732534,
130.128119836039)) ;
#137293 = CARTESIAN_POINT('Ctrl Pts',(-24.158577834541,12.411847051202,129.877251493057)) ;
#137294 = CARTESIAN_POINT('Ctrl Pts',(-24.0620294843223,12.4580456459642,
129.628319557637)) ;
#137295 = CARTESIAN_POINT('Ctrl Pts',(-23.9724819407128,12.5736491008617,
129.399871559833)) ;
#137296 = CARTESIAN_POINT('Ctrl Pts',(-23.8958324246764,12.7495591345061,
129.209023299466)) ;
#137297 = CARTESIAN_POINT('Ctrl Pts',(-23.8363403529087,12.9753683217391,
129.06853311284)) ;
#137298 = CARTESIAN_POINT('Ctrl Pts',(-23.7983705149086,13.2312289198464,
128.990617600681)) ;
#137299 = CARTESIAN_POINT('Ctrl Pts',(-23.7832383935185,13.5022490913223,
128.979611461187)) ;
#137300 = CARTESIAN_POINT('Ctrl Pts',(-23.7915690414023,13.7663766429706,
129.036987224607)) ;
#137301 = CARTESIAN_POINT('Ctrl Pts',(-23.8218816093751,14.0063275981214,
129.158621057965)) ;
#137302 = CARTESIAN_POINT('Ctrl Pts',(-23.8714125707789,14.2048735685629,
129.336436861487)) ;
#137303 = CARTESIAN_POINT('Ctrl Pts',(-23.9360766035452,14.3476911545505,
129.558558579197)) ;
#137304 = CARTESIAN_POINT('Ctrl Pts',(-24.0101424431012,14.4237776141336,
129.808052928934)) ;
#137305 = CARTESIAN_POINT('Ctrl Pts',(-24.0877654886693,14.4280807917519,
130.067962762365)) ;
#137306 = CARTESIAN_POINT('Ctrl Pts',(-24.1623469987095,14.360827921304,130.318852067325)) ;
#137307 = CARTESIAN_POINT('Ctrl Pts',(-24.2285176630201,14.2256361349193,
130.545392667963)) ;
#137308 = CARTESIAN_POINT('Ctrl Pts',(-24.2799186020434,14.0344801252662,
130.728492767782)) ;
#137309 = CARTESIAN_POINT('Ctrl Pts',(-24.3130244781345,13.7980437562362,
130.858419713646)) ;
#137310 = CARTESIAN_POINT('Ctrl Pts',(-24.3241513604221,13.53532438393,130.924036543225)) ;
#137311 = CARTESIAN_POINT('Ctrl Pts',(-24.3119764531114,13.2644875678434,
130.921600659002)) ;
#137312 = CARTESIAN_POINT('Ctrl Pts',(-24.276607917817,13.0050530170807,130.851402331197)) ;
#137313 = CARTESIAN_POINT('Ctrl Pts',(-24.2198137245786,12.775438141039,130.718635056671)) ;
#137314 = CARTESIAN_POINT('Ctrl Pts',(-24.1450871500959,12.5925960963687,
130.533426659931)) ;
#137315 = CARTESIAN_POINT('Ctrl Pts',(-24.0570562303304,12.4690082469491,
130.309331812912)) ;
#137316 = CARTESIAN_POINT('Ctrl Pts',(-23.9606548006948,12.4135709185057,
130.060969797119)) ;
#137317 = CARTESIAN_POINT('Ctrl Pts',(-23.8633239205352,12.4306394810107,
129.809638399428)) ;
#137318 = CARTESIAN_POINT('Ctrl Pts',(-23.7701586445981,12.5185474861746,
129.570614180752)) ;
#137319 = CARTESIAN_POINT('Ctrl Pts',(-23.6874386169935,12.6718439913262,
129.362161787323)) ;
#137320 = CARTESIAN_POINT('Ctrl Pts',(-23.6207199401336,12.8780301439606,
129.200304555462)) ;
#137321 = CARTESIAN_POINT('Ctrl Pts',(-23.5734544100946,13.1252485962165,
129.095546151147)) ;
#137322 = CARTESIAN_POINT('Ctrl Pts',(-23.5490275882913,13.3909665400584,
129.057124901564)) ;
#137323 = CARTESIAN_POINT('Ctrl Pts',(-23.5478469452304,13.6612160877443,
129.086903188456)) ;
#137324 = CARTESIAN_POINT('Ctrl Pts',(-23.5695278793464,13.9131568788034,
129.183301070422)) ;
#137325 = CARTESIAN_POINT('Ctrl Pts',(-23.6117378779522,14.1304384080089,
129.339731339965)) ;
#137326 = CARTESIAN_POINT('Ctrl Pts',(-23.670618868599,14.2969775137474,129.544805224008)) ;
#137327 = CARTESIAN_POINT('Ctrl Pts',(-23.7419278031084,14.4015522183562,
129.786450816467)) ;
#137328 = CARTESIAN_POINT('Ctrl Pts',(-23.8185327256045,14.4350500547512,
130.04322857818)) ;
#137329 = CARTESIAN_POINT('Ctrl Pts',(-23.895073988246,14.396751965708,130.29988774461)) ;
#137330 = CARTESIAN_POINT('Ctrl Pts',(-23.9654056990637,14.2884849239284,
130.538494109741)) ;
#137331 = CARTESIAN_POINT('Ctrl Pts',(-24.0235441195686,14.1181741044495,
130.74147538802)) ;
#137332 = CARTESIAN_POINT('Ctrl Pts',(-24.064579062323,13.8977533675812,130.894521933553)) ;
#137333 = CARTESIAN_POINT('Ctrl Pts',(-24.0848219240481,13.6446685040666,
130.986656853548)) ;
#137334 = CARTESIAN_POINT('Ctrl Pts',(-24.0822023369396,13.3734340849695,
131.012296376983)) ;
#137335 = CARTESIAN_POINT('Ctrl Pts',(-24.0560179172839,13.1072277425428,
130.968914707618)) ;
#137336 = CARTESIAN_POINT('Ctrl Pts',(-24.0077701366724,12.8641926256241,
130.860994227657)) ;
#137337 = CARTESIAN_POINT('Ctrl Pts',(-23.9398468464116,12.6605228267135,
130.695685489353)) ;
#137338 = CARTESIAN_POINT('Ctrl Pts',(-23.8566310215138,12.5114117943071,
130.485659567777)) ;
#137339 = CARTESIAN_POINT('Ctrl Pts',(-23.7623999995309,12.4272142366947,
130.24373969586)) ;
#137340 = CARTESIAN_POINT('Ctrl Pts',(-23.6651743173675,12.4150347895705,
129.99264727931)) ;
#137341 = CARTESIAN_POINT('Ctrl Pts',(-23.5692968163676,12.4747490693336,
129.745746794804)) ;
#137342 = CARTESIAN_POINT('Ctrl Pts',(-23.4818229937488,12.6023244974168,
129.523310907728)) ;
#137343 = CARTESIAN_POINT('Ctrl Pts',(-23.407748924182,12.7898413054048,129.340204613242)) ;
#137344 = CARTESIAN_POINT('Ctrl Pts',(-23.3526025051574,13.0206705904154,
129.212059796763)) ;
#137345 = CARTESIAN_POINT('Ctrl Pts',(-23.3185827971363,13.2818516686094,
129.145867360566)) ;
#137346 = CARTESIAN_POINT('Ctrl Pts',(-23.3079501436408,13.5521276503918,
129.147857520888)) ;
#137347 = CARTESIAN_POINT('Ctrl Pts',(-23.320481206199,13.8139567141273,129.217605438094)) ;
#137348 = CARTESIAN_POINT('Ctrl Pts',(-23.3550030243452,14.048569772894,129.351746255589)) ;
#137349 = CARTESIAN_POINT('Ctrl Pts',(-23.407397020995,14.236110064849,129.537698849994)) ;
#137350 = CARTESIAN_POINT('Ctrl Pts',(-23.4744514414992,14.3675383495349,
129.766892450617)) ;
#137351 = CARTESIAN_POINT('Ctrl Pts',(-23.5496273539776,14.4300942129039,
130.019607525919)) ;
#137352 = CARTESIAN_POINT('Ctrl Pts',(-23.6268969486743,14.4208865440108,
130.27835213759)) ;
#137353 = CARTESIAN_POINT('Ctrl Pts',(-23.7004306698474,14.3405661595428,
130.526245792846)) ;
#137354 = CARTESIAN_POINT('Ctrl Pts',(-23.7644224178413,14.1934623353678,
130.746473197132)) ;
#137355 = CARTESIAN_POINT('Ctrl Pts',(-23.8127756419206,13.9917022900947,
130.920839890071)) ;
#137356 = CARTESIAN_POINT('Ctrl Pts',(-23.8416998117934,13.7502057571416,
131.038343138081)) ;
#137357 = CARTESIAN_POINT('Ctrl Pts',(-23.8485644464668,13.4844948245858,
131.091517749686)) ;
#137358 = CARTESIAN_POINT('Ctrl Pts',(-23.8319362934437,13.2141841608485,
131.076089294491)) ;
#137359 = CARTESIAN_POINT('Ctrl Pts',(-23.7923791092109,12.9589228600533,
130.99365805615)) ;
#137360 = CARTESIAN_POINT('Ctrl Pts',(-23.7315857819428,12.7362703078518,
130.849331458812)) ;
#137361 = CARTESIAN_POINT('Ctrl Pts',(-23.654489045961,12.5648475135275,130.656969361176)) ;
#137362 = CARTESIAN_POINT('Ctrl Pts',(-23.5639389610065,12.452872637983,130.425740312664)) ;
#137363 = CARTESIAN_POINT('Ctrl Pts',(-23.4673752556237,12.411294196787,130.176678568121)) ;
#137364 = CARTESIAN_POINT('Ctrl Pts',(-23.3698780425036,12.4419882066381,
129.92505446556)) ;
#137365 = CARTESIAN_POINT('Ctrl Pts',(-23.2785520721008,12.5427027858175,
129.691305126012)) ;
#137366 = CARTESIAN_POINT('Ctrl Pts',(-23.1984718637741,12.706796402249,129.490533281651)) ;
#137367 = CARTESIAN_POINT('Ctrl Pts',(-23.135068634506,12.9221001593752,129.338439944309)) ;
#137368 = CARTESIAN_POINT('Ctrl Pts',(-23.0919954586335,13.1741319900526,
129.245841884835)) ;
#137369 = CARTESIAN_POINT('Ctrl Pts',(-23.0718580306747,13.4427023276839,
129.220070404539)) ;
#137370 = CARTESIAN_POINT('Ctrl Pts',(-23.0751585689848,13.7107857008536,
129.26289034347)) ;
#137371 = CARTESIAN_POINT('Ctrl Pts',(-23.1008376347237,13.9568883020333,
129.370893251844)) ;
#137372 = CARTESIAN_POINT('Ctrl Pts',(-23.1465403344726,14.1661036589884,
129.537562189888)) ;
#137373 = CARTESIAN_POINT('Ctrl Pts',(-23.2083074256075,14.3219384877272,
129.75117659853)) ;
#137374 = CARTESIAN_POINT('Ctrl Pts',(-23.2806542878813,14.4130180667709,
129.995597829584)) ;
#137375 = CARTESIAN_POINT('Ctrl Pts',(-23.3580236308951,14.4335349377785,
130.254752754733)) ;
#137376 = CARTESIAN_POINT('Ctrl Pts',(-23.4342369440473,14.3810414591398,
130.510644418635)) ;
#137377 = CARTESIAN_POINT('Ctrl Pts',(-23.5022753810008,14.2609491563611,
130.742352348115)) ;
#137378 = CARTESIAN_POINT('Ctrl Pts',(-23.5576881153806,14.0795345145358,
130.937487790807)) ;
#137379 = CARTESIAN_POINT('Ctrl Pts',(-23.5948722936596,13.8529285433275,
131.079068657613)) ;
#137380 = CARTESIAN_POINT('Ctrl Pts',(-23.6110592381906,13.5926909018936,
131.159708991485)) ;
#137381 = CARTESIAN_POINT('Ctrl Pts',(-23.6039222248104,13.3230679904021,
131.171845507133)) ;
#137382 = CARTESIAN_POINT('Ctrl Pts',(-23.5735515673625,13.0595446516906,
131.116246634271)) ;
#137383 = CARTESIAN_POINT('Ctrl Pts',(-23.5210444853348,12.821409078981,130.996073210915)) ;
#137384 = CARTESIAN_POINT('Ctrl Pts',(-23.4496688403902,12.6270968771254,
130.820718874116)) ;
#137385 = CARTESIAN_POINT('Ctrl Pts',(-23.3644228508194,12.4904302575877,
130.604624186015)) ;
#137386 = CARTESIAN_POINT('Ctrl Pts',(-23.2693883176564,12.4195264376518,
130.360202664601)) ;
#137387 = CARTESIAN_POINT('Ctrl Pts',(-23.1717013390917,12.4206997747971,
130.107888702409)) ;
#137388 = CARTESIAN_POINT('Ctrl Pts',(-23.07674697722,12.4940150849619,129.863744537933)) ;
#137389 = CARTESIAN_POINT('Ctrl Pts',(-22.9917454792659,12.6331733496192,
129.648432936584)) ;
#137390 = CARTESIAN_POINT('Ctrl Pts',(-22.9210033107914,12.8293255236082,
129.47492493208)) ;
#137391 = CARTESIAN_POINT('Ctrl Pts',(-22.8693173983923,13.0683011169746,
129.357098375333)) ;
#137392 = CARTESIAN_POINT('Ctrl Pts',(-22.8397009911573,13.3322965961088,
129.303691206083)) ;
#137393 = CARTESIAN_POINT('Ctrl Pts',(-22.8334317380967,13.6026348428664,
129.318468394913)) ;
#137394 = CARTESIAN_POINT('Ctrl Pts',(-22.8502549510441,13.8605087628932,
129.400751483274)) ;
#137395 = CARTESIAN_POINT('Ctrl Pts',(-22.8883323200656,14.0871783650871,
129.545152491834)) ;
#137396 = CARTESIAN_POINT('Ctrl Pts',(-22.9440423731906,14.2658343770077,
129.74099514858)) ;
#137397 = CARTESIAN_POINT('Ctrl Pts',(-23.0127923157115,14.3843789391541,
129.974962574827)) ;
#137398 = CARTESIAN_POINT('Ctrl Pts',(-23.0890433292092,14.4339734241572,
130.230900091451)) ;
#137399 = CARTESIAN_POINT('Ctrl Pts',(-23.1661312317174,14.4110559361857,
130.489146023008)) ;
#137400 = CARTESIAN_POINT('Ctrl Pts',(-23.2382006324762,14.3178925144465,
130.732739172181)) ;
#137401 = CARTESIAN_POINT('Ctrl Pts',(-23.2996857722997,14.1593686690055,
130.945647915619)) ;
#137402 = CARTESIAN_POINT('Ctrl Pts',(-23.3445584705906,13.9496805388889,
131.109722558938)) ;
#137403 = CARTESIAN_POINT('Ctrl Pts',(-23.3696736527837,13.7013470012748,
131.216252350218)) ;
#137404 = CARTESIAN_POINT('Ctrl Pts',(-23.3720920163119,13.4330164706509,
131.256471678111)) ;
#137405 = CARTESIAN_POINT('Ctrl Pts',(-23.3511454215899,13.1647607659068,
131.228335735827)) ;
#137406 = CARTESIAN_POINT('Ctrl Pts',(-23.3072621176942,12.9137311953691,
131.133374404822)) ;
#137407 = CARTESIAN_POINT('Ctrl Pts',(-23.2434888033612,12.7007529765594,
130.980069049084)) ;
#137408 = CARTESIAN_POINT('Ctrl Pts',(-23.1628787911392,12.5383275950027,
130.777785669083)) ;
#137409 = CARTESIAN_POINT('Ctrl Pts',(-23.0712872888514,12.4398166155699,
130.543252817928)) ;
#137410 = CARTESIAN_POINT('Ctrl Pts',(-22.9733700901106,12.4114725014285,
130.290514442298)) ;
#137411 = CARTESIAN_POINT('Ctrl Pts',(-22.8769228839034,12.4557968837197,
130.041802473424)) ;
#137412 = CARTESIAN_POINT('Ctrl Pts',(-22.7869968694901,12.5696290703402,
129.812287837357)) ;
#137413 = CARTESIAN_POINT('Ctrl Pts',(-22.7101031050184,12.7436129145437,
129.620649242638)) ;
#137414 = CARTESIAN_POINT('Ctrl Pts',(-22.6500085106509,12.9681021997866,
129.478393868049)) ;
#137415 = CARTESIAN_POINT('Ctrl Pts',(-22.6113280612937,13.2239470656193,
129.398484240347)) ;
#137416 = CARTESIAN_POINT('Ctrl Pts',(-22.5955724991583,13.4941632022952,
129.385572434223)) ;
#137417 = CARTESIAN_POINT('Ctrl Pts',(-22.6032116810304,13.7589185594046,
129.440951942343)) ;
#137418 = CARTESIAN_POINT('Ctrl Pts',(-22.6329203868012,13.999834830615,129.560819723437)) ;
#137419 = CARTESIAN_POINT('Ctrl Pts',(-22.6819480888645,14.1997645777198,
129.737163915801)) ;
#137420 = CARTESIAN_POINT('Ctrl Pts',(-22.7461154267965,14.3442636718176,
129.957775023844)) ;
#137421 = CARTESIAN_POINT('Ctrl Pts',(-22.8201291984854,14.4224928178984,
130.207186244669)) ;
#137422 = CARTESIAN_POINT('Ctrl Pts',(-22.8973493324398,14.429171124512,130.465747266348)) ;
#137423 = CARTESIAN_POINT('Ctrl Pts',(-22.9726528467362,14.3636109202534,
130.718991967903)) ;
#137424 = CARTESIAN_POINT('Ctrl Pts',(-23.0389194410672,14.2305642022342,
130.945696008778)) ;
#137425 = CARTESIAN_POINT('Ctrl Pts',(-23.0908974390234,14.0406276478755,
131.130542175203)) ;
#137426 = CARTESIAN_POINT('Ctrl Pts',(-23.1245333358198,13.8058700767644,
131.261928515044)) ;
#137427 = CARTESIAN_POINT('Ctrl Pts',(-23.1363830164337,13.5427809263485,
131.329774433396)) ;
#137428 = CARTESIAN_POINT('Ctrl Pts',(-23.1248575359644,13.2720606343581,
131.329212568738)) ;
#137429 = CARTESIAN_POINT('Ctrl Pts',(-23.0900746108795,13.0118430008048,
131.26075620549)) ;
#137430 = CARTESIAN_POINT('Ctrl Pts',(-23.0340455584365,12.7818788914411,
131.13011430412)) ;
#137431 = CARTESIAN_POINT('Ctrl Pts',(-22.9596349753376,12.5968717145733,
130.945912471778)) ;
#137432 = CARTESIAN_POINT('Ctrl Pts',(-22.8715122077198,12.471251749294,130.721681034181)) ;
#137433 = CARTESIAN_POINT('Ctrl Pts',(-22.7757176314075,12.4142248024153,
130.474925696683)) ;
#137434 = CARTESIAN_POINT('Ctrl Pts',(-22.6781851317645,12.4291610280905,
130.22306244369)) ;
#137435 = CARTESIAN_POINT('Ctrl Pts',(-22.5847562522808,12.5152749264354,
129.983286515838)) ;
#137436 = CARTESIAN_POINT('Ctrl Pts',(-22.5015747269694,12.6672522037425,
129.773535207759)) ;
#137437 = CARTESIAN_POINT('Ctrl Pts',(-22.4346652666614,12.8714563204239,
129.610995698154)) ;
#137438 = CARTESIAN_POINT('Ctrl Pts',(-22.3868994473045,13.1164156174602,
129.504613845988)) ;
#137439 = CARTESIAN_POINT('Ctrl Pts',(-22.3615817594558,13.3833143441499,
129.463785300508)) ;
#137440 = CARTESIAN_POINT('Ctrl Pts',(-22.3597882823452,13.6536761481919,
129.49176218256)) ;
#137441 = CARTESIAN_POINT('Ctrl Pts',(-22.3807933273105,13.9063303510439,
129.58617443786)) ;
#137442 = CARTESIAN_POINT('Ctrl Pts',(-22.4226906447706,14.125656517117,129.741831670047)) ;
#137443 = CARTESIAN_POINT('Ctrl Pts',(-22.480992797728,14.2929703980627,129.945090280937)) ;
#137444 = CARTESIAN_POINT('Ctrl Pts',(-22.5518543733382,14.3994043116304,
130.185355863779)) ;
#137445 = CARTESIAN_POINT('Ctrl Pts',(-22.6285093988248,14.4351253202173,
130.442339869809)) ;
#137446 = CARTESIAN_POINT('Ctrl Pts',(-22.7051973850955,14.3988243960317,
130.699449624082)) ;
#137447 = CARTESIAN_POINT('Ctrl Pts',(-22.7758084986371,14.2923293352694,
130.938885575333)) ;
#137448 = CARTESIAN_POINT('Ctrl Pts',(-22.8341888942695,14.1241731264117,
131.142472997224)) ;
#137449 = CARTESIAN_POINT('Ctrl Pts',(-22.8758535864009,13.9051614113411,
131.297356933649)) ;
#137450 = CARTESIAN_POINT('Ctrl Pts',(-22.8967675053112,13.6518311651615,
131.391575680539)) ;
#137451 = CARTESIAN_POINT('Ctrl Pts',(-22.8948524255514,13.3824709073359,
131.419066522015)) ;
#137452 = CARTESIAN_POINT('Ctrl Pts',(-22.8694536911301,13.1154253755206,
131.378028547348)) ;
#137453 = CARTESIAN_POINT('Ctrl Pts',(-22.8216303727267,12.870532700791,131.271475250091)) ;
#137454 = CARTESIAN_POINT('Ctrl Pts',(-22.7542127450307,12.6655371324335,
131.107638188433)) ;
#137455 = CARTESIAN_POINT('Ctrl Pts',(-22.6711951167249,12.5146112693424,
130.898249520681)) ;
#137456 = CARTESIAN_POINT('Ctrl Pts',(-22.5777454584632,12.4289102076434,
130.658411657876)) ;
#137457 = CARTESIAN_POINT('Ctrl Pts',(-22.4803400259961,12.4141896647539,
130.406868783015)) ;
#137458 = CARTESIAN_POINT('Ctrl Pts',(-22.3837956818218,12.4724108271044,
130.158202744766)) ;
#137459 = CARTESIAN_POINT('Ctrl Pts',(-22.2964764439714,12.5978141623982,
129.936061247941)) ;
#137460 = CARTESIAN_POINT('Ctrl Pts',(-22.222180894914,12.7826551138703,129.752158405497)) ;
#137461 = CARTESIAN_POINT('Ctrl Pts',(-22.1661151196085,13.013381389437,129.621487955934)) ;
#137462 = CARTESIAN_POINT('Ctrl Pts',(-22.1314362662289,13.2742167666549,
129.553393622124)) ;
#137463 = CARTESIAN_POINT('Ctrl Pts',(-22.1201350356918,13.5450313802589,
129.553498432196)) ;
#137464 = CARTESIAN_POINT('Ctrl Pts',(-22.1320713682587,13.8067210995316,
129.621436808792)) ;
#137465 = CARTESIAN_POINT('Ctrl Pts',(-22.1657011419629,14.0412512155271,
129.752780861513)) ;
#137466 = CARTESIAN_POINT('Ctrl Pts',(-22.2179806871803,14.2318696546287,
129.938653767515)) ;
#137467 = CARTESIAN_POINT('Ctrl Pts',(-22.2845880318834,14.3645252689238,
130.16645539328)) ;
#137468 = CARTESIAN_POINT('Ctrl Pts',(-22.3592798328537,14.4291513639763,
130.417628538692)) ;
#137469 = CARTESIAN_POINT('Ctrl Pts',(-22.436871642398,14.4223448397237,130.677436734826)) ;
#137470 = CARTESIAN_POINT('Ctrl Pts',(-22.510846648584,14.3433928726762,130.926745639385)) ;
#137471 = CARTESIAN_POINT('Ctrl Pts',(-22.57467863088,14.1993298116068,131.146227665756)) ;
#137472 = CARTESIAN_POINT('Ctrl Pts',(-22.6237644035119,13.9988091287191,
131.322818887298)) ;
#137473 = CARTESIAN_POINT('Ctrl Pts',(-22.6533894867198,13.7578102679721,
131.442430456946)) ;
#137474 = CARTESIAN_POINT('Ctrl Pts',(-22.6608850427505,13.491649195449,131.497555891874)) ;
#137475 = CARTESIAN_POINT('Ctrl Pts',(-22.64500311771,13.2223244098795,131.484163859812)) ;
#137476 = CARTESIAN_POINT('Ctrl Pts',(-22.6059893392227,12.96574693319,131.403407690678)) ;
#137477 = CARTESIAN_POINT('Ctrl Pts',(-22.5461201352489,12.7429297081588,
131.261604090611)) ;
#137478 = CARTESIAN_POINT('Ctrl Pts',(-22.4689354238792,12.5685157395234,
131.069226764808)) ;
#137479 = CARTESIAN_POINT('Ctrl Pts',(-22.3786382574204,12.4549912739037,
130.83872380872)) ;
#137480 = CARTESIAN_POINT('Ctrl Pts',(-22.2823846413124,12.4115665134561,
130.590501453343)) ;
#137481 = CARTESIAN_POINT('Ctrl Pts',(-22.185022978805,12.439915366976,130.339196899106)) ;
#137482 = CARTESIAN_POINT('Ctrl Pts',(-22.0929640431126,12.5392662703676,
130.103484375993)) ;
#137483 = CARTESIAN_POINT('Ctrl Pts',(-22.0127053078525,12.7015765318143,
129.902116599291)) ;
#137484 = CARTESIAN_POINT('Ctrl Pts',(-21.9489204298559,12.9151235355211,
129.748837978728)) ;
#137485 = CARTESIAN_POINT('Ctrl Pts',(-21.9052335765829,13.1655123701317,
129.65434805994)) ;
#137486 = CARTESIAN_POINT('Ctrl Pts',(-21.8842873311341,13.435707308921,129.626447566814)) ;
#137487 = CARTESIAN_POINT('Ctrl Pts',(-21.8869481330479,13.7027427336547,
129.667228378349)) ;
#137488 = CARTESIAN_POINT('Ctrl Pts',(-21.9120183916717,13.9504288164231,
129.773544414319)) ;
#137489 = CARTESIAN_POINT('Ctrl Pts',(-21.9572517363974,14.1608970885181,
129.938846468588)) ;
#137490 = CARTESIAN_POINT('Ctrl Pts',(-22.018507368848,14.3182076506529,130.150909064873)) ;
#137491 = CARTESIAN_POINT('Ctrl Pts',(-22.0907386237567,14.4114239636762,
130.395045201029)) ;
#137492 = CARTESIAN_POINT('Ctrl Pts',(-22.1678997175522,14.43387114395,130.653528180286)) ;
#137493 = CARTESIAN_POINT('Ctrl Pts',(-22.2440626405903,14.3839736485786,
130.909179188166)) ;
#137494 = CARTESIAN_POINT('Ctrl Pts',(-22.3128383560668,14.2649034164715,
131.143264149934)) ;
#137495 = CARTESIAN_POINT('Ctrl Pts',(-22.368369781886,14.0862373803975,131.338529256948)) ;
#137496 = CARTESIAN_POINT('Ctrl Pts',(-22.4063643713204,13.8593710344565,
131.482693687338)) ;
#137497 = CARTESIAN_POINT('Ctrl Pts',(-22.423082781093,13.6016402973256,131.564639588124)) ;
#137498 = CARTESIAN_POINT('Ctrl Pts',(-22.416710563554,13.3309242141033,131.579161001393)) ;
#137499 = CARTESIAN_POINT('Ctrl Pts',(-22.3869594339498,13.0670234319289,
131.525359499281)) ;
#137500 = CARTESIAN_POINT('Ctrl Pts',(-22.3352755509082,12.828626261272,131.407481838502)) ;
#137501 = CARTESIAN_POINT('Ctrl Pts',(-22.2644737257156,12.6324569777035,
131.233812164351)) ;
#137502 = CARTESIAN_POINT('Ctrl Pts',(-22.179026147261,12.4932134027072,131.017336188657)) ;
#137503 = CARTESIAN_POINT('Ctrl Pts',(-22.0846147994345,12.4206918298189,
130.774574849433)) ;
#137504 = CARTESIAN_POINT('Ctrl Pts',(-21.9866149275365,12.4196226590599,
130.521455957442)) ;
#137505 = CARTESIAN_POINT('Ctrl Pts',(-21.8915517263097,12.4910154498675,
130.276970511203)) ;
#137506 = CARTESIAN_POINT('Ctrl Pts',(-21.8061759252374,12.6283739089441,
130.060574403858)) ;
#137507 = CARTESIAN_POINT('Ctrl Pts',(-21.734785916595,12.8237068444054,129.885261771197)) ;
#137508 = CARTESIAN_POINT('Ctrl Pts',(-21.6826427874687,13.0616748025397,
129.766076185179)) ;
#137509 = CARTESIAN_POINT('Ctrl Pts',(-21.6524872755057,13.3240381252934,
129.710950435826)) ;
#137510 = CARTESIAN_POINT('Ctrl Pts',(-21.6454690535715,13.5952492770895,
129.723635230244)) ;
#137511 = CARTESIAN_POINT('Ctrl Pts',(-21.6617842864879,13.8544594163448,
129.804532436936)) ;
#137512 = CARTESIAN_POINT('Ctrl Pts',(-21.6993093477804,14.081653901287,129.947257582405)) ;
#137513 = CARTESIAN_POINT('Ctrl Pts',(-21.7543881862704,14.2612879476329,
130.141148761343)) ;
#137514 = CARTESIAN_POINT('Ctrl Pts',(-21.8227956619766,14.38176341734,130.374105622269)) ;
#137515 = CARTESIAN_POINT('Ctrl Pts',(-21.8989363667567,14.4336477337376,
130.629729117928)) ;
#137516 = CARTESIAN_POINT('Ctrl Pts',(-21.9765152606609,14.4124734002023,
130.889599388047)) ;
#137517 = CARTESIAN_POINT('Ctrl Pts',(-22.0483877837567,14.3214777532126,
131.132438584826)) ;
#137518 = CARTESIAN_POINT('Ctrl Pts',(-22.1102442273107,14.1652192668134,
131.34638096803)) ;
#137519 = CARTESIAN_POINT('Ctrl Pts',(-22.1558537131498,13.9555650448247,
131.512795439526)) ;
#137520 = CARTESIAN_POINT('Ctrl Pts',(-22.1814091769848,13.7095599731385,
131.620407563)) ;
#137521 = CARTESIAN_POINT('Ctrl Pts',(-22.1846084318414,13.4405995134717,
131.66302940788)) ;
#137522 = CARTESIAN_POINT('Ctrl Pts',(-22.1641410813746,13.1715077445613,
131.63637428883)) ;
#137523 = CARTESIAN_POINT('Ctrl Pts',(-22.1212713726189,12.9214880531583,
131.54412153606)) ;
#137524 = CARTESIAN_POINT('Ctrl Pts',(-22.0575394234642,12.7055052901806,
131.391205523699)) ;
#137525 = CARTESIAN_POINT('Ctrl Pts',(-21.9777673697123,12.542519660956,131.191170277208)) ;
#137526 = CARTESIAN_POINT('Ctrl Pts',(-21.8862402490834,12.4416160246637,
130.956908046475)) ;
#137527 = CARTESIAN_POINT('Ctrl Pts',(-21.7883180011064,12.4112449651492,
130.704175247965)) ;
#137528 = CARTESIAN_POINT('Ctrl Pts',(-21.6916915206646,12.4537097184138,
130.45497041539)) ;
#137529 = CARTESIAN_POINT('Ctrl Pts',(-21.6017839340474,12.5652232692769,
130.225394633114)) ;
#137530 = CARTESIAN_POINT('Ctrl Pts',(-21.5242852905658,12.7379440024603,
130.032062311546)) ;
#137531 = CARTESIAN_POINT('Ctrl Pts',(-21.4638348212917,12.9603974208925,
129.888644578289)) ;
#137532 = CARTESIAN_POINT('Ctrl Pts',(-21.4244019077111,13.2156634379738,
129.806566052762)) ;
#137533 = CARTESIAN_POINT('Ctrl Pts',(-21.4079017130301,13.4857933225146,
129.791484741217)) ;
#137534 = CARTESIAN_POINT('Ctrl Pts',(-21.4149000703604,13.7522945834018,
129.845154416319)) ;
#137535 = CARTESIAN_POINT('Ctrl Pts',(-21.4441925744404,13.9943543864371,
129.96386451108)) ;
#137536 = CARTESIAN_POINT('Ctrl Pts',(-21.4925040843012,14.1947045665703,
130.137957931616)) ;
#137537 = CARTESIAN_POINT('Ctrl Pts',(-21.5566005957734,14.341452901732,130.358505717863)) ;
#137538 = CARTESIAN_POINT('Ctrl Pts',(-21.6300619513567,14.4211242912775,
130.606132041837)) ;
#137539 = CARTESIAN_POINT('Ctrl Pts',(-21.7074195269614,14.4300014441918,
130.865166461581)) ;
#137540 = CARTESIAN_POINT('Ctrl Pts',(-21.782739862899,14.3664766103849,131.118399093227)) ;
#137541 = CARTESIAN_POINT('Ctrl Pts',(-21.8492962143774,14.2356053057405,
131.345912604585)) ;
#137542 = CARTESIAN_POINT('Ctrl Pts',(-21.9019742543641,14.0463421699273,
131.532943707079)) ;
#137543 = CARTESIAN_POINT('Ctrl Pts',(-21.9360655876364,13.8127313116574,
131.665625433991)) ;
#137544 = CARTESIAN_POINT('Ctrl Pts',(-21.9485792452769,13.5514862656321,
131.735251200451)) ;
#137545 = CARTESIAN_POINT('Ctrl Pts',(-21.9377331317714,13.2797432937496,
131.736799208666)) ;
#137546 = CARTESIAN_POINT('Ctrl Pts',(-21.9037118572088,13.0196142656872,
131.670476580031)) ;
#137547 = CARTESIAN_POINT('Ctrl Pts',(-21.848095759366,12.7876902930479,131.541159383157)) ;
#137548 = CARTESIAN_POINT('Ctrl Pts',(-21.774212667836,12.601531820227,131.358452186942)) ;
#137549 = CARTESIAN_POINT('Ctrl Pts',(-21.6866886351043,12.4742597851615,
131.135876049528)) ;
#137550 = CARTESIAN_POINT('Ctrl Pts',(-21.5909295194249,12.4148459828286,
130.889268624499)) ;
#137551 = CARTESIAN_POINT('Ctrl Pts',(-21.4930969827498,12.4277167902933,
130.63661588948)) ;
#137552 = CARTESIAN_POINT('Ctrl Pts',(-21.3995555315845,12.5119511239392,
130.396485892115)) ;
#137553 = CARTESIAN_POINT('Ctrl Pts',(-21.3162990844251,12.6612550507726,
130.186368956131)) ;
#137554 = CARTESIAN_POINT('Ctrl Pts',(-21.2483839343844,12.8654797343675,
130.021126795539)) ;
#137555 = CARTESIAN_POINT('Ctrl Pts',(-21.2002270894872,13.1088715380583,
129.913494497197)) ;
#137556 = CARTESIAN_POINT('Ctrl Pts',(-21.1742080824271,13.3752798477322,
129.870610368109)) ;
#137557 = CARTESIAN_POINT('Ctrl Pts',(-21.1717085434086,13.6458119714847,
129.89651662008)) ;
#137558 = CARTESIAN_POINT('Ctrl Pts',(-21.1921257233827,13.8994657965604,
129.989254351832)) ;
#137559 = CARTESIAN_POINT('Ctrl Pts',(-21.233245209048,14.1192748903921,130.142500293083)) ;
#137560 = CARTESIAN_POINT('Ctrl Pts',(-21.2914251747259,14.289180306213,130.345585373604)) ;
#137561 = CARTESIAN_POINT('Ctrl Pts',(-21.3616961232879,14.3970324953059,
130.583966718822)) ;
#137562 = CARTESIAN_POINT('Ctrl Pts',(-21.4384087866577,14.4351164743851,
130.841195428719)) ;
#137563 = CARTESIAN_POINT('Ctrl Pts',(-21.5151210055013,14.4010787676098,
131.098338089324)) ;
#137564 = CARTESIAN_POINT('Ctrl Pts',(-21.5863960251658,14.2958209234975,
131.339908880083)) ;
#137565 = CARTESIAN_POINT('Ctrl Pts',(-21.6449304989321,14.1296521766069,
131.543828654143)) ;
#137566 = CARTESIAN_POINT('Ctrl Pts',(-21.6871346231113,13.9121761436852,
131.700257800473)) ;
#137567 = CARTESIAN_POINT('Ctrl Pts',(-21.7086771478897,13.659430364987,131.796334004922)) ;
#137568 = CARTESIAN_POINT('Ctrl Pts',(-21.7075047728149,13.3906473352246,
131.825945739935)) ;
#137569 = CARTESIAN_POINT('Ctrl Pts',(-21.6825267550966,13.12154860475,131.786357720267)) ;
#137570 = CARTESIAN_POINT('Ctrl Pts',(-21.6355924854869,12.8774995309081,
131.682170944537)) ;
#137571 = CARTESIAN_POINT('Ctrl Pts',(-21.5684160783297,12.6702279872938,
131.519185241917)) ;
#137572 = CARTESIAN_POINT('Ctrl Pts',(-21.4860950112321,12.5183910771853,
131.311688639648)) ;
#137573 = CARTESIAN_POINT('Ctrl Pts',(-21.3928599529137,12.4302683284587,
131.072491120113)) ;
#137574 = CARTESIAN_POINT('Ctrl Pts',(-21.2947906658205,12.4138255810916,
130.819247899391)) ;
#137575 = CARTESIAN_POINT('Ctrl Pts',(-21.1993133837603,12.469284941687,130.5732787841)) ;
#137576 = CARTESIAN_POINT('Ctrl Pts',(-21.111045383612,12.5930867722267,130.348576358499)) ;
#137577 = CARTESIAN_POINT('Ctrl Pts',(-21.0361572295438,12.7771358580158,
130.163027615693)) ;
#137578 = CARTESIAN_POINT('Ctrl Pts',(-20.9797275916326,13.0059648630076,
130.031178709991)) ;
#137579 = CARTESIAN_POINT('Ctrl Pts',(-20.9443527411009,13.266147051347,129.961050822874)) ;
#137580 = CARTESIAN_POINT('Ctrl Pts',(-20.9323325930837,13.536990507266,129.959060513734)) ;
#137581 = CARTESIAN_POINT('Ctrl Pts',(-20.9436543105165,13.7997447814263,
130.025277225395)) ;
#137582 = CARTESIAN_POINT('Ctrl Pts',(-20.9766477952397,14.0350782594662,
130.154719818596)) ;
#137583 = CARTESIAN_POINT('Ctrl Pts',(-21.0287127379786,14.2276700254763,
130.3400969056)) ;
#137584 = CARTESIAN_POINT('Ctrl Pts',(-21.0943520323041,14.3610390583721,
130.564758598525)) ;
#137585 = CARTESIAN_POINT('Ctrl Pts',(-21.1694845733918,14.4285213443226,
130.817501137148)) ;
#137586 = CARTESIAN_POINT('Ctrl Pts',(-21.2469270728871,14.4233691665642,
131.076802064509)) ;
#137587 = CARTESIAN_POINT('Ctrl Pts',(-21.320899695783,14.3469901017567,131.325999762253)) ;
#137588 = CARTESIAN_POINT('Ctrl Pts',(-21.3855341560455,14.2034040422047,
131.548081815734)) ;
#137589 = CARTESIAN_POINT('Ctrl Pts',(-21.4347256418351,14.0056848767319,
131.724728264946)) ;
#137590 = CARTESIAN_POINT('Ctrl Pts',(-21.465092607587,13.7644936141034,131.846677236872)) ;
#137591 = CARTESIAN_POINT('Ctrl Pts',(-21.4732444413167,13.5002464496988,
131.903523955919)) ;
#137592 = CARTESIAN_POINT('Ctrl Pts',(-21.4578324144306,13.2284058869682,
131.891809873456)) ;
#137593 = CARTESIAN_POINT('Ctrl Pts',(-21.4198290919617,12.9739038042497,
131.813645652512)) ;
#137594 = CARTESIAN_POINT('Ctrl Pts',(-21.3602690958964,12.748470453343,131.672940766185)) ;
#137595 = CARTESIAN_POINT('Ctrl Pts',(-21.2837438582424,12.5731123494061,
131.482377603287)) ;
#137596 = CARTESIAN_POINT('Ctrl Pts',(-21.1936880421902,12.4573590885892,
131.252613188665)) ;
#137597 = CARTESIAN_POINT('Ctrl Pts',(-21.0974470732546,12.4118025442917,
131.004458624852)) ;
#137598 = CARTESIAN_POINT('Ctrl Pts',(-20.9999957475628,12.4381298230363,
130.752902669264)) ;
#137599 = CARTESIAN_POINT('Ctrl Pts',(-20.9078518526991,12.5352056579817,
130.516875210043)) ;
#137600 = CARTESIAN_POINT('Ctrl Pts',(-20.8269544230574,12.6963006078304,
130.313742235523)) ;
#137601 = CARTESIAN_POINT('Ctrl Pts',(-20.7626803376973,12.9082756117234,
130.15899041196)) ;
#137602 = CARTESIAN_POINT('Ctrl Pts',(-20.7182259000088,13.1596325354774,
130.062478814741)) ;
#137603 = CARTESIAN_POINT('Ctrl Pts',(-20.6968797595826,13.4259468867853,
130.032958383663)) ;
#137604 = CARTESIAN_POINT('Ctrl Pts',(-20.6987180598139,13.6953761022081,
130.071595056294)) ;
#137605 = CARTESIAN_POINT('Ctrl Pts',(-20.7232215568337,13.9437170228922,
130.176233244644)) ;
#137606 = CARTESIAN_POINT('Ctrl Pts',(-20.767971164486,14.1557110770192,130.340160815693)) ;
#137607 = CARTESIAN_POINT('Ctrl Pts',(-20.8287309225785,14.3144000142637,
130.550712718952)) ;
#137608 = CARTESIAN_POINT('Ctrl Pts',(-20.9006919276648,14.4096307818779,
130.794052371241)) ;
#137609 = CARTESIAN_POINT('Ctrl Pts',(-20.9778182880555,14.4343455417677,
131.052440775311)) ;
#137610 = CARTESIAN_POINT('Ctrl Pts',(-21.0544154691547,14.3860725443644,
131.309506234514)) ;
#137611 = CARTESIAN_POINT('Ctrl Pts',(-21.1230945083084,14.2695097476577,
131.543118119901)) ;
#137612 = CARTESIAN_POINT('Ctrl Pts',(-21.179301480217,14.0917908235827,131.740489361359)) ;
#137613 = CARTESIAN_POINT('Ctrl Pts',(-21.2177234690881,13.8666927964708,
131.885799826201)) ;
#137614 = CARTESIAN_POINT('Ctrl Pts',(-21.2351412575897,13.6093229660632,
131.969833893824)) ;
#137615 = CARTESIAN_POINT('Ctrl Pts',(-21.2294450096949,13.3388432839998,
131.986311133137)) ;
#137616 = CARTESIAN_POINT('Ctrl Pts',(-21.2003261125768,13.0740475195294,
131.934408442014)) ;
#137617 = CARTESIAN_POINT('Ctrl Pts',(-21.1490766645565,12.8343947236294,
131.817855849607)) ;
#137618 = CARTESIAN_POINT('Ctrl Pts',(-21.079117586523,12.6378260096104,131.646478866635)) ;
#137619 = CARTESIAN_POINT('Ctrl Pts',(-20.9940307650976,12.496463053358,131.431074246898)) ;
#137620 = CARTESIAN_POINT('Ctrl Pts',(-20.8995453725939,12.4217254212934,
131.188184304878)) ;
#137621 = CARTESIAN_POINT('Ctrl Pts',(-20.8016533511348,12.4187226067802,
130.935348047491)) ;
#137622 = CARTESIAN_POINT('Ctrl Pts',(-20.7067290384026,12.4875916105364,
130.691149701073)) ;
#137623 = CARTESIAN_POINT('Ctrl Pts',(-20.6206591273952,12.6235711646796,
130.472855830561)) ;
#137624 = CARTESIAN_POINT('Ctrl Pts',(-20.5490501305615,12.8167006668533,
130.296777642181)) ;
#137625 = CARTESIAN_POINT('Ctrl Pts',(-20.496178051986,13.0534699877681,130.175467508203)) ;
#137626 = CARTESIAN_POINT('Ctrl Pts',(-20.4652082763484,13.316652871898,130.118125632978)) ;
#137627 = CARTESIAN_POINT('Ctrl Pts',(-20.4575910264854,13.5871780619914,
130.128970220053)) ;
#137628 = CARTESIAN_POINT('Ctrl Pts',(-20.4730839064674,13.8461109459276,
130.207338015546)) ;
#137629 = CARTESIAN_POINT('Ctrl Pts',(-20.5100737122391,14.0754122507699,
130.348613835523)) ;
#137630 = CARTESIAN_POINT('Ctrl Pts',(-20.5648370930962,14.2569964936062,
130.541657854969)) ;
#137631 = CARTESIAN_POINT('Ctrl Pts',(-20.6329413594287,14.3792169088182,
130.773722810003)) ;
#137632 = CARTESIAN_POINT('Ctrl Pts',(-20.7087226220765,14.4330645733332,
131.028200436973)) ;
#137633 = CARTESIAN_POINT('Ctrl Pts',(-20.7863398371565,14.4142942248449,
131.288175280098)) ;
#137634 = CARTESIAN_POINT('Ctrl Pts',(-20.8587443892862,14.3249818846189,
131.532699501629)) ;
#137635 = CARTESIAN_POINT('Ctrl Pts',(-20.9209779259209,14.170040968278,131.747774216565)) ;
#137636 = CARTESIAN_POINT('Ctrl Pts',(-20.9669011427084,13.9629929132432,
131.914918567305)) ;
#137637 = CARTESIAN_POINT('Ctrl Pts',(-20.9932272956991,13.716497262182,132.024969893988)) ;
#137638 = CARTESIAN_POINT('Ctrl Pts',(-20.9970536036366,13.4493823964161,
132.069231580467)) ;
#137639 = CARTESIAN_POINT('Ctrl Pts',(-20.9773681367216,13.1794660173532,
132.044927528063)) ;
#137640 = CARTESIAN_POINT('Ctrl Pts',(-20.9348193274938,12.9274139550297,
131.953787995804)) ;
#137641 = CARTESIAN_POINT('Ctrl Pts',(-20.8719669700059,12.7115777182511,
131.803243101651)) ;
#137642 = CARTESIAN_POINT('Ctrl Pts',(-20.7926171746203,12.5463884321844,
131.604472050351)) ;
#137643 = CARTESIAN_POINT('Ctrl Pts',(-20.7005656856551,12.4431786925169,
131.36894206665)) ;
#137644 = CARTESIAN_POINT('Ctrl Pts',(-20.6037919880621,12.4112124579401,
131.119195085756)) ;
#137645 = CARTESIAN_POINT('Ctrl Pts',(-20.5066772839954,12.4513454594276,
130.868694657424)) ;
#137646 = CARTESIAN_POINT('Ctrl Pts',(-20.4165141092168,12.5610016830577,
130.638362595368)) ;
#137647 = CARTESIAN_POINT('Ctrl Pts',(-20.3384849755394,12.7322315169158,
130.443517766448)) ;
#137648 = CARTESIAN_POINT('Ctrl Pts',(-20.2774709313571,12.953682166373,130.2984736935)) ;
#137649 = CARTESIAN_POINT('Ctrl Pts',(-20.2374795071584,13.207709520667,130.214695903395)) ;
#137650 = CARTESIAN_POINT('Ctrl Pts',(-20.2202513164256,13.477838949959,130.19750736579)) ;
#137651 = CARTESIAN_POINT('Ctrl Pts',(-20.2266080907571,13.7447249701473,
130.249306408078)) ;
#137652 = CARTESIAN_POINT('Ctrl Pts',(-20.2551147268125,13.9871378811425,
130.365615989591)) ;
#137653 = CARTESIAN_POINT('Ctrl Pts',(-20.3032561348622,14.1900736221216,
130.539429290487)) ;
#137654 = CARTESIAN_POINT('Ctrl Pts',(-20.366375984174,14.3373317370972,130.756810802034)) ;
#137655 = CARTESIAN_POINT('Ctrl Pts',(-20.4400778737823,14.4199335161434,
131.005366056279)) ;
#137656 = CARTESIAN_POINT('Ctrl Pts',(-20.517398884963,14.4307824011819,131.264277739086)) ;
#137657 = CARTESIAN_POINT('Ctrl Pts',(-20.593060063551,14.3690285687369,131.518596966109)) ;
#137658 = CARTESIAN_POINT('Ctrl Pts',(-20.6596542407766,14.240441055026,131.746082495927)) ;
#137659 = CARTESIAN_POINT('Ctrl Pts',(-20.7128484353568,14.0528077050883,
131.934627680386)) ;
#137660 = CARTESIAN_POINT('Ctrl Pts',(-20.7475784142269,13.8202656328653,
132.069181756592)) ;
#137661 = CARTESIAN_POINT('Ctrl Pts',(-20.7607767450837,13.5584446016604,
132.140947553018)) ;
#137662 = CARTESIAN_POINT('Ctrl Pts',(-20.7505287005013,13.2871051677591,
132.144192204044)) ;
#137663 = CARTESIAN_POINT('Ctrl Pts',(-20.7172718444425,13.0271137580964,
132.080012631234)) ;
#137664 = CARTESIAN_POINT('Ctrl Pts',(-20.662202991394,12.7938648791111,131.952326610137)) ;
#137665 = CARTESIAN_POINT('Ctrl Pts',(-20.5888877956183,12.6063348860961,
131.771239179103)) ;
#137666 = CARTESIAN_POINT('Ctrl Pts',(-20.5015478328552,12.4770288288764,
131.549255832687)) ;
#137667 = CARTESIAN_POINT('Ctrl Pts',(-20.4062249604456,12.4155889254397,
131.303824104185)) ;
#137668 = CARTESIAN_POINT('Ctrl Pts',(-20.3079159542625,12.4264045620756,
131.049934819456)) ;
#137669 = CARTESIAN_POINT('Ctrl Pts',(-20.2145031376508,12.5084012335638,
130.810058284156)) ;
#137670 = CARTESIAN_POINT('Ctrl Pts',(-20.1306995642403,12.6562045204938,
130.598414583344)) ;
#137671 = CARTESIAN_POINT('Ctrl Pts',(-20.0624739819763,12.8582527624523,
130.432148065107)) ;
#137672 = CARTESIAN_POINT('Ctrl Pts',(-20.0133566463447,13.1022479915201,
130.321924077519)) ;
#137673 = CARTESIAN_POINT('Ctrl Pts',(-19.9868280658771,13.3685510945704,
130.277573143074)) ;
#137674 = CARTESIAN_POINT('Ctrl Pts',(-19.9836603277551,13.6374690116671,
130.301308492192)) ;
#137675 = CARTESIAN_POINT('Ctrl Pts',(-20.0034420277648,13.8926337185126,
130.392287293504)) ;
#137676 = CARTESIAN_POINT('Ctrl Pts',(-20.0439943690178,14.1134973759114,
130.543852003553)) ;
#137677 = CARTESIAN_POINT('Ctrl Pts',(-20.1019010050305,14.2854804463777,
130.746225783846)) ;
#137678 = CARTESIAN_POINT('Ctrl Pts',(-20.1719255332864,14.3949169663802,
130.983882406649)) ;
#137679 = CARTESIAN_POINT('Ctrl Pts',(-20.248213487577,14.4350950477778,131.239727536652)) ;
#137680 = CARTESIAN_POINT('Ctrl Pts',(-20.3254463492532,14.4027523557503,
131.498591864264)) ;
#137681 = CARTESIAN_POINT('Ctrl Pts',(-20.396382333849,14.3004224268776,131.738877616431)) ;
#137682 = CARTESIAN_POINT('Ctrl Pts',(-20.45588703209,14.1345848166218,131.945929948589)) ;
#137683 = CARTESIAN_POINT('Ctrl Pts',(-20.4983986905152,13.9188292644318,
132.103144456355)) ;
#137684 = CARTESIAN_POINT('Ctrl Pts',(-20.5206054593495,13.6668968300226,
132.201163345285)) ;
#137685 = CARTESIAN_POINT('Ctrl Pts',(-20.5200422127212,13.3982258229591,
132.232566609447)) ;
#137686 = CARTESIAN_POINT('Ctrl Pts',(-20.4959120705654,13.1299460140076,
132.195305612606)) ;
#137687 = CARTESIAN_POINT('Ctrl Pts',(-20.4493854866592,12.883706046321,132.092482303726)) ;
#137688 = CARTESIAN_POINT('Ctrl Pts',(-20.3827956444432,12.6755091493533,
131.931155444613)) ;
#137689 = CARTESIAN_POINT('Ctrl Pts',(-20.3007023283114,12.5215778727762,
131.724390139687)) ;
#137690 = CARTESIAN_POINT('Ctrl Pts',(-20.2075018171708,12.4317802296238,
131.485347148361)) ;
#137691 = CARTESIAN_POINT('Ctrl Pts',(-20.1103254681884,12.4131805085562,
131.234422161529)) ;
#137692 = CARTESIAN_POINT('Ctrl Pts',(-20.0139320775133,12.4668842419267,
130.986048105159)) ;
#137693 = CARTESIAN_POINT('Ctrl Pts',(-19.9257741902488,12.5884449970434,
130.76151375573)) ;
#137694 = CARTESIAN_POINT('Ctrl Pts',(-19.8502049393805,12.7713420307832,
130.574069477332)) ;
#137695 = CARTESIAN_POINT('Ctrl Pts',(-19.793268697052,12.9988617172705,130.44070264408)) ;
#137696 = CARTESIAN_POINT('Ctrl Pts',(-19.757165794996,13.2594912156624,130.368579354002)) ;
#137697 = CARTESIAN_POINT('Ctrl Pts',(-19.7446008853565,13.528913215532,130.364828114744)) ;
#137698 = CARTESIAN_POINT('Ctrl Pts',(-19.7551763127313,13.7920446626032,
130.428843415922)) ;
#137699 = CARTESIAN_POINT('Ctrl Pts',(-19.7876094727285,14.0286822474636,
130.556687451896)) ;
#137700 = CARTESIAN_POINT('Ctrl Pts',(-19.8390978347557,14.2226476411148,
130.740339467478)) ;
#137701 = CARTESIAN_POINT('Ctrl Pts',(-19.9045962847081,14.3581279629795,
130.964687569436)) ;
#137702 = CARTESIAN_POINT('Ctrl Pts',(-19.9791897742387,14.4275172103506,
131.215693011947)) ;
#137703 = CARTESIAN_POINT('Ctrl Pts',(-20.0572472309711,14.4244373538993,
131.477053037658)) ;
#137704 = CARTESIAN_POINT('Ctrl Pts',(-20.1309835390558,14.3501368659966,
131.72538106024)) ;
#137705 = CARTESIAN_POINT('Ctrl Pts',(-20.1958863249354,14.2089998659338,
131.948172797202)) ;
#137706 = CARTESIAN_POINT('Ctrl Pts',(-20.2457715176204,14.0121252002097,
132.126956829028)) ;
#137707 = CARTESIAN_POINT('Ctrl Pts',(-20.2767468394311,13.771824837408,132.250689691059)) ;
#137708 = CARTESIAN_POINT('Ctrl Pts',(-20.2855151937684,13.5078187869416,
132.309363670343)) ;
#137709 = CARTESIAN_POINT('Ctrl Pts',(-20.2709382772913,13.2372790594901,
132.29991113471)) ;
#137710 = CARTESIAN_POINT('Ctrl Pts',(-20.2333968985353,12.9804327969093,
132.223307498601)) ;
#137711 = CARTESIAN_POINT('Ctrl Pts',(-20.1743352916517,12.7540239326364,
132.084048582146)) ;
#137712 = CARTESIAN_POINT('Ctrl Pts',(-20.0983730228796,12.5774627760268,
131.895074679153)) ;
#137713 = CARTESIAN_POINT('Ctrl Pts',(-20.0088178169133,12.4598743078943,
131.666703703983)) ;
#137714 = CARTESIAN_POINT('Ctrl Pts',(-19.9122599860254,12.4120040784052,
131.41777242998)) ;
#137715 = CARTESIAN_POINT('Ctrl Pts',(-19.8148042629863,12.4365719244432,
131.166187081806)) ;
#137716 = CARTESIAN_POINT('Ctrl Pts',(-19.7227956012826,12.5311793554758,
130.930416460681)) ;
#137717 = CARTESIAN_POINT('Ctrl Pts',(-19.6411874345405,12.6910252858477,
130.725320832536)) ;
#137718 = CARTESIAN_POINT('Ctrl Pts',(-19.5765629416592,12.9015545976397,
130.569498377236)) ;
#137719 = CARTESIAN_POINT('Ctrl Pts',(-19.5315753841879,13.1503193803916,
130.471219010104)) ;
#137720 = CARTESIAN_POINT('Ctrl Pts',(-19.5093124096303,13.4198238208766,
130.439454333555)) ;
#137721 = CARTESIAN_POINT('Ctrl Pts',(-19.5105321036796,13.6867201897118,
130.475929754006)) ;
#137722 = CARTESIAN_POINT('Ctrl Pts',(-19.5344899978628,13.9376559886512,
130.579206334042)) ;
#137723 = CARTESIAN_POINT('Ctrl Pts',(-19.5786625804763,14.15024285779,130.741353841934)) ;
#137724 = CARTESIAN_POINT('Ctrl Pts',(-19.6390835815084,14.3108380618515,
130.95096108692)) ;
#137725 = CARTESIAN_POINT('Ctrl Pts',(-19.710796343946,14.4079445273837,131.193561999246)) ;
#137726 = CARTESIAN_POINT('Ctrl Pts',(-19.7879385451593,14.4345276708083,
131.452034692613)) ;
#137727 = CARTESIAN_POINT('Ctrl Pts',(-19.8641423507794,14.3888298887491,
131.707720589177)) ;
#137728 = CARTESIAN_POINT('Ctrl Pts',(-19.9334963492316,14.2738285073071,
131.943474886351)) ;
#137729 = CARTESIAN_POINT('Ctrl Pts',(-19.9900753188983,14.0978368978208,
132.141892587942)) ;
#137730 = CARTESIAN_POINT('Ctrl Pts',(-20.029142353165,13.873540820756,132.289148752814)) ;
#137731 = CARTESIAN_POINT('Ctrl Pts',(-20.0471730607309,13.6168751421622,
132.374962241574)) ;
#137732 = CARTESIAN_POINT('Ctrl Pts',(-20.0421398303126,13.3465065043273,
132.39337844358)) ;
#137733 = CARTESIAN_POINT('Ctrl Pts',(-20.0137168616045,13.0815409163059,
132.343472421558)) ;
#137734 = CARTESIAN_POINT('Ctrl Pts',(-19.9630818029184,12.8409648020749,
132.228711336927)) ;
#137735 = CARTESIAN_POINT('Ctrl Pts',(-19.8937037272603,12.6428641094173,
132.059013597505)) ;
#137736 = CARTESIAN_POINT('Ctrl Pts',(-19.8082706443675,12.4989647241715,
131.842851496796)) ;
#137737 = CARTESIAN_POINT('Ctrl Pts',(-19.7148222298413,12.423107716889,131.602682335525)) ;
#137738 = CARTESIAN_POINT('Ctrl Pts',(-19.6165590013728,12.4177381354183,
131.34889731826)) ;
#137739 = CARTESIAN_POINT('Ctrl Pts',(-19.5215312608125,12.4847094665518,
131.104373207812)) ;
#137740 = CARTESIAN_POINT('Ctrl Pts',(-19.4350279161659,12.6190666936061,
130.884854431054)) ;
#137741 = CARTESIAN_POINT('Ctrl Pts',(-19.3630156634519,12.8107470171755,
130.707580165133)) ;
#137742 = CARTESIAN_POINT('Ctrl Pts',(-19.3096393875782,13.046104708988,130.584743629659)) ;
#137743 = CARTESIAN_POINT('Ctrl Pts',(-19.2779861809298,13.3089102809665,
130.525423125906)) ;
#137744 = CARTESIAN_POINT('Ctrl Pts',(-19.2696835204742,13.5795916473862,
130.534276424891)) ;
#137745 = CARTESIAN_POINT('Ctrl Pts',(-19.2846166337307,13.8398547760041,
130.611106017032)) ;
#137746 = CARTESIAN_POINT('Ctrl Pts',(-19.3210881365978,14.0698648400938,
130.750835724147)) ;
#137747 = CARTESIAN_POINT('Ctrl Pts',(-19.3752206498596,14.2524395531566,
130.941933848175)) ;
#137748 = CARTESIAN_POINT('Ctrl Pts',(-19.443181843827,14.3767942781604,131.173660667841)) ;
#137749 = CARTESIAN_POINT('Ctrl Pts',(-19.5186387491627,14.4324209526977,
131.42710546284)) ;
#137750 = CARTESIAN_POINT('Ctrl Pts',(-19.5962340512703,14.4159981333991,
131.686985719429)) ;
#137751 = CARTESIAN_POINT('Ctrl Pts',(-19.6690951170259,14.3283155565982,
131.93295372937)) ;
#137752 = CARTESIAN_POINT('Ctrl Pts',(-19.731498600517,14.1755659528296,132.148414877089)) ;
#137753 = CARTESIAN_POINT('Ctrl Pts',(-19.7780133273736,13.9699068567355,
132.317303495422)) ;
#137754 = CARTESIAN_POINT('Ctrl Pts',(-19.8049862544587,13.7239840394015,
132.42928569716)) ;
#137755 = CARTESIAN_POINT('Ctrl Pts',(-19.809515235663,13.4571373132025,132.475606075713)) ;
#137756 = CARTESIAN_POINT('Ctrl Pts',(-19.7903204177427,13.1860385292999,
132.45286442784)) ;
#137757 = CARTESIAN_POINT('Ctrl Pts',(-19.7487646879107,12.9351633483058,
132.364359945624)) ;
#137758 = CARTESIAN_POINT('Ctrl Pts',(-19.6859631867643,12.7162804285951,
132.21423823404)) ;
#137759 = CARTESIAN_POINT('Ctrl Pts',(-19.6073342675828,12.5504602957499,
132.017412800741)) ;
#137760 = CARTESIAN_POINT('Ctrl Pts',(-19.5155082129029,12.445157177056,131.782565908142)) ;
#137761 = CARTESIAN_POINT('Ctrl Pts',(-19.4189472179032,12.4110818139133,
131.533391011119)) ;
#137762 = CARTESIAN_POINT('Ctrl Pts',(-19.3214401093541,12.4493848627241,
131.281852651979)) ;
#137763 = CARTESIAN_POINT('Ctrl Pts',(-19.2314769431166,12.5564279113244,
131.051920666311)) ;
#137764 = CARTESIAN_POINT('Ctrl Pts',(-19.1524965061616,12.7270948639173,
130.85451813902)) ;
#137765 = CARTESIAN_POINT('Ctrl Pts',(-19.0911924448804,12.9467013244188,
130.708509031209)) ;
#137766 = CARTESIAN_POINT('Ctrl Pts',(-19.0504665817876,13.2005745310841,
130.622663698416)) ;
#137767 = CARTESIAN_POINT('Ctrl Pts',(-19.0326836209356,13.4697555759231,
130.603759575917)) ;
#137768 = CARTESIAN_POINT('Ctrl Pts',(-19.0382102244379,13.7362551955502,
130.653023431916)) ;
#137769 = CARTESIAN_POINT('Ctrl Pts',(-19.0663557867909,13.9814041489959,
130.76853786842)) ;
#137770 = CARTESIAN_POINT('Ctrl Pts',(-19.1136199928099,14.1841666435664,
130.939526111425)) ;
#137771 = CARTESIAN_POINT('Ctrl Pts',(-19.1767577967624,14.3343211623714,
131.15719018996)) ;
#137772 = CARTESIAN_POINT('Ctrl Pts',(-19.2500366332053,14.418455096693,131.404394753815)) ;
#137773 = CARTESIAN_POINT('Ctrl Pts',(-19.3273692986292,14.4314520041057,
131.663366130815)) ;
#137774 = CARTESIAN_POINT('Ctrl Pts',(-19.4028774363666,14.3721435581282,
131.917097822485)) ;
#137775 = CARTESIAN_POINT('Ctrl Pts',(-19.4700541032919,14.2453739060394,
132.146382805055)) ;
#137776 = CARTESIAN_POINT('Ctrl Pts',(-19.5239307336061,14.0581567741166,
132.337084920621)) ;
#137777 = CARTESIAN_POINT('Ctrl Pts',(-19.5590167477845,13.8276969055429,
132.472521311396)) ;
#137778 = CARTESIAN_POINT('Ctrl Pts',(-19.5729299943671,13.5670204809412,
132.54631437139)) ;
#137779 = CARTESIAN_POINT('Ctrl Pts',(-19.5634175629659,13.2953787817414,
132.551745553635)) ;
#137780 = CARTESIAN_POINT('Ctrl Pts',(-19.5307814551787,13.0342215951602,
132.489449839042)) ;
#137781 = CARTESIAN_POINT('Ctrl Pts',(-19.4760249872077,12.7992353621788,
132.362794033766)) ;
#137782 = CARTESIAN_POINT('Ctrl Pts',(-19.4035773877406,12.6113833751158,
132.184049216232)) ;
#137783 = CARTESIAN_POINT('Ctrl Pts',(-19.3165223036231,12.4798504311987,
131.962931933643)) ;
#137784 = CARTESIAN_POINT('Ctrl Pts',(-19.2211653039383,12.4163978737343,
131.717463870116)) ;
#137785 = CARTESIAN_POINT('Ctrl Pts',(-19.1231585738506,12.4249214769568,
131.464343284139)) ;
#137786 = CARTESIAN_POINT('Ctrl Pts',(-19.0290644089191,12.5053755581291,
131.222650125226)) ;
#137787 = CARTESIAN_POINT('Ctrl Pts',(-18.945316002603,12.6507858524343,131.011003544665)) ;
#137788 = CARTESIAN_POINT('Ctrl Pts',(-18.8763895924228,12.8517470379754,
130.84276469136)) ;
#137789 = CARTESIAN_POINT('Ctrl Pts',(-18.8267448309181,13.0945613893121,
130.730961303292)) ;
#137790 = CARTESIAN_POINT('Ctrl Pts',(-18.7994718959822,13.3602125815229,
130.684409044151)) ;
#137791 = CARTESIAN_POINT('Ctrl Pts',(-18.7956758360037,13.6310671509035,
130.706531095789)) ;
#137792 = CARTESIAN_POINT('Ctrl Pts',(-18.8147674164781,13.8852753501133,
130.79528480511)) ;
#137793 = CARTESIAN_POINT('Ctrl Pts',(-18.8547365620153,14.1076160518456,
130.945173100413)) ;
#137794 = CARTESIAN_POINT('Ctrl Pts',(-18.9120865572062,14.2808806548592,
131.145853438459)) ;
#137795 = CARTESIAN_POINT('Ctrl Pts',(-18.9817798655855,14.3926567066995,
131.382539424301)) ;
#137796 = CARTESIAN_POINT('Ctrl Pts',(-19.0585628808164,14.4348969494453,
131.640089890739)) ;
#137797 = CARTESIAN_POINT('Ctrl Pts',(-19.1351376242844,14.4049966963277,
131.896703997414)) ;
#137798 = CARTESIAN_POINT('Ctrl Pts',(-19.2069795117691,14.303792887026,132.139944585753)) ;
#137799 = CARTESIAN_POINT('Ctrl Pts',(-19.2664511487555,14.1405203843961,
132.346669416583)) ;
#137800 = CARTESIAN_POINT('Ctrl Pts',(-19.3096417752548,13.925819103477,132.505934041616)) ;
#137801 = CARTESIAN_POINT('Ctrl Pts',(-19.3325065328025,13.6747404913737,
132.605860844122)) ;
#137802 = CARTESIAN_POINT('Ctrl Pts',(-19.332541849949,13.4052256729127,132.639149944979)) ;
#137803 = CARTESIAN_POINT('Ctrl Pts',(-19.3092812735878,13.1384692552609,
132.604191768055)) ;
#137804 = CARTESIAN_POINT('Ctrl Pts',(-19.2631063121014,12.8897551675282,
132.502613781544)) ;
#137805 = CARTESIAN_POINT('Ctrl Pts',(-19.1973582392372,12.6813708112152,
132.343566871807)) ;
#137806 = CARTESIAN_POINT('Ctrl Pts',(-19.1155604461688,12.5252896551219,
132.137725194002)) ;
#137807 = CARTESIAN_POINT('Ctrl Pts',(-19.0228059236477,12.4335762169434,
131.899908767192)) ;
#137808 = CARTESIAN_POINT('Ctrl Pts',(-18.925357266948,12.4126069646067,131.64830074567)) ;
#137809 = CARTESIAN_POINT('Ctrl Pts',(-18.8285810937,12.4645413585742,131.398893890923)) ;
#137810 = CARTESIAN_POINT('Ctrl Pts',(-18.740157757668,12.5845282308657,131.173590439064)) ;
#137811 = CARTESIAN_POINT('Ctrl Pts',(-18.6643847827615,12.7652450506007,
130.985436414686)) ;
#137812 = CARTESIAN_POINT('Ctrl Pts',(-18.6067882108563,12.9922346613826,
130.850221426745)) ;
#137813 = CARTESIAN_POINT('Ctrl Pts',(-18.5702632954388,13.250181771579,130.776605389314)) ;
#137814 = CARTESIAN_POINT('Ctrl Pts',(-18.5568044283898,13.5208712081626,
130.770411334257)) ;
#137815 = CARTESIAN_POINT('Ctrl Pts',(-18.5668006964617,13.7852947823376,
130.832834130771)) ;
#137816 = CARTESIAN_POINT('Ctrl Pts',(-18.5987394298108,14.0230293048616,
130.959264121613)) ;
#137817 = CARTESIAN_POINT('Ctrl Pts',(-18.6496368762035,14.2178153725244,
131.141101449601)) ;
#137818 = CARTESIAN_POINT('Ctrl Pts',(-18.7147914630156,14.3552930120595,
131.364452232031)) ;
#137819 = CARTESIAN_POINT('Ctrl Pts',(-18.7895474760606,14.4265292407486,
131.616072894725)) ;
#137820 = CARTESIAN_POINT('Ctrl Pts',(-18.8667133662151,14.4257522410885,
131.874439194348)) ;
#137821 = CARTESIAN_POINT('Ctrl Pts',(-18.9412988303887,14.3531912390316,
132.125538928334)) ;
#137822 = CARTESIAN_POINT('Ctrl Pts',(-19.006381267232,14.2139749778386,132.348774125945)) ;
#137823 = CARTESIAN_POINT('Ctrl Pts',(-19.0568528029414,14.0181343967752,
132.529344981123)) ;
#137824 = CARTESIAN_POINT('Ctrl Pts',(-19.0883199089333,13.7796846047307,
132.654391142837)) ;
#137825 = CARTESIAN_POINT('Ctrl Pts',(-19.0978098271686,13.5155236952114,
132.715257194164)) ;
#137826 = CARTESIAN_POINT('Ctrl Pts',(-19.0839141888874,13.2452127497976,
132.707751963834)) ;
#137827 = CARTESIAN_POINT('Ctrl Pts',(-19.0470411501845,12.9877059092876,
132.633102744637)) ;
#137828 = CARTESIAN_POINT('Ctrl Pts',(-18.9886209994034,12.7602061146998,
132.49569403547)) ;
#137829 = CARTESIAN_POINT('Ctrl Pts',(-18.912954495156,12.5817513014504,132.307649978698)) ;
#137830 = CARTESIAN_POINT('Ctrl Pts',(-18.823989235305,12.4625557645347,132.080895111837)) ;
#137831 = CARTESIAN_POINT('Ctrl Pts',(-18.7274195905187,12.4124303731174,
131.831984343437)) ;
#137832 = CARTESIAN_POINT('Ctrl Pts',(-18.6300548105444,12.4345388042572,
131.580601782827)) ;
#137833 = CARTESIAN_POINT('Ctrl Pts',(-18.5370135094554,12.5283216388457,
131.342120309818)) ;
#137834 = CARTESIAN_POINT('Ctrl Pts',(-18.4559097133117,12.6848122289345,
131.138130709134)) ;
#137835 = CARTESIAN_POINT('Ctrl Pts',(-18.3901713005438,12.8954782844364,
130.979318768591)) ;
#137836 = CARTESIAN_POINT('Ctrl Pts',(-18.3448005512406,13.1430312169486,
130.879841045138)) ;
#137837 = CARTESIAN_POINT('Ctrl Pts',(-18.3218747041718,13.4109716006735,
130.845992375282)) ;
#137838 = CARTESIAN_POINT('Ctrl Pts',(-18.3223625152694,13.6794257001286,
130.880484421356)) ;
#137839 = CARTESIAN_POINT('Ctrl Pts',(-18.3458072065772,13.9314101129575,
130.982305968587)) ;
#137840 = CARTESIAN_POINT('Ctrl Pts',(-18.3893102806117,14.1445006499188,
131.1423845234)) ;
#137841 = CARTESIAN_POINT('Ctrl Pts',(-18.4492119247963,14.30675364297,131.350434987214)) ;
#137842 = CARTESIAN_POINT('Ctrl Pts',(-18.5207480281994,14.4060487021468,
131.592559699906)) ;
#137843 = CARTESIAN_POINT('Ctrl Pts',(-18.5978819309036,14.4348548844435,
131.851031778509)) ;
#137844 = CARTESIAN_POINT('Ctrl Pts',(-18.674405910123,14.3909041683382,132.107751135057)) ;
#137845 = CARTESIAN_POINT('Ctrl Pts',(-18.7437339428587,14.2783347545864,
132.343276751579)) ;
#137846 = CARTESIAN_POINT('Ctrl Pts',(-18.8010355018281,14.1031935593991,
132.54396170515)) ;
#137847 = CARTESIAN_POINT('Ctrl Pts',(-18.8405463694835,13.8800104934357,
132.692493251368)) ;
#137848 = CARTESIAN_POINT('Ctrl Pts',(-18.859162215355,13.6249527950758,132.779899013047)) ;
#137849 = CARTESIAN_POINT('Ctrl Pts',(-18.8548446588266,13.3547990721566,
132.800399354658)) ;
#137850 = CARTESIAN_POINT('Ctrl Pts',(-18.827222338478,13.0897727529312,132.752776683914)) ;
#137851 = CARTESIAN_POINT('Ctrl Pts',(-18.776916467683,12.8467550013015,132.639173733262)) ;
#137852 = CARTESIAN_POINT('Ctrl Pts',(-18.7080316497001,12.6478124741987,
132.470872436135)) ;
#137853 = CARTESIAN_POINT('Ctrl Pts',(-18.6236048883295,12.5027972402551,
132.257422574238)) ;
#137854 = CARTESIAN_POINT('Ctrl Pts',(-18.5295771589345,12.4240443790735,
132.015841001444)) ;
#137855 = CARTESIAN_POINT('Ctrl Pts',(-18.4312698393036,12.4170503512975,
131.761943008889)) ;
#137856 = CARTESIAN_POINT('Ctrl Pts',(-18.3364462745014,12.4817913528845,
131.517890812399)) ;
#137857 = CARTESIAN_POINT('Ctrl Pts',(-18.2495792781442,12.6142900077789,
131.297317545331)) ;
#137858 = CARTESIAN_POINT('Ctrl Pts',(-18.1771702037882,12.8042102941726,
131.118842529841)) ;
#137859 = CARTESIAN_POINT('Ctrl Pts',(-18.1230598700679,13.0388185676317,
130.993913398293)) ;
#137860 = CARTESIAN_POINT('Ctrl Pts',(-18.0907140204209,13.302328429414,130.932716168419)) ;
#137861 = CARTESIAN_POINT('Ctrl Pts',(-18.0818206414082,13.5713413202646,
130.939632216682)) ;
#137862 = CARTESIAN_POINT('Ctrl Pts',(-18.0961078605723,13.8329961698972,
131.014678941615)) ;
#137863 = CARTESIAN_POINT('Ctrl Pts',(-18.1319332307441,14.0635775985236,
131.152440731558)) ;
#137864 = CARTESIAN_POINT('Ctrl Pts',(-18.1856883445983,14.2479536598407,
131.342493359132)) ;
#137865 = CARTESIAN_POINT('Ctrl Pts',(-18.2530905010094,14.3739504234545,
131.572475100791)) ;
#137866 = CARTESIAN_POINT('Ctrl Pts',(-18.3290310806664,14.4320428147267,
131.827608185542)) ;
#137867 = CARTESIAN_POINT('Ctrl Pts',(-18.4064572253342,14.4172275166343,
132.086904527241)) ;
#137868 = CARTESIAN_POINT('Ctrl Pts',(-18.4792652025405,14.3318167265824,
132.332603920243)) ;
#137869 = CARTESIAN_POINT('Ctrl Pts',(-18.5420198013597,14.1811818661954,
132.549047819145)) ;
#137870 = CARTESIAN_POINT('Ctrl Pts',(-18.5892218579538,13.9759968010836,
132.720084196974)) ;
#137871 = CARTESIAN_POINT('Ctrl Pts',(-18.6167720804193,13.7313492742168,
132.833691346408)) ;
#137872 = CARTESIAN_POINT('Ctrl Pts',(-18.6218292587465,13.4634561374574,
132.881731398093)) ;
#137873 = CARTESIAN_POINT('Ctrl Pts',(-18.6036627628578,13.1958849564785,
132.861520033549)) ;
#137874 = CARTESIAN_POINT('Ctrl Pts',(-18.5623283084843,12.9412337113468,
132.774062788288)) ;
#137875 = CARTESIAN_POINT('Ctrl Pts',(-18.5006384449743,12.7230235201935,
132.626876709527)) ;
#137876 = CARTESIAN_POINT('Ctrl Pts',(-18.4217152103521,12.5539648159992,
132.4295120841)) ;
#137877 = CARTESIAN_POINT('Ctrl Pts',(-18.3311245557592,12.4477725871464,
132.19791079546)) ;
#137878 = CARTESIAN_POINT('Ctrl Pts',(-18.2339496661273,12.4110238125286,
131.947200890198)) ;
#137879 = CARTESIAN_POINT('Ctrl Pts',(-18.1368321085862,12.4468710259381,
131.696619131312)) ;
#137880 = CARTESIAN_POINT('Ctrl Pts',(-18.0456588191261,12.5531554017273,
131.463507987167)) ;
#137881 = CARTESIAN_POINT('Ctrl Pts',(-17.9669224096408,12.7211113672027,
131.26655346719)) ;
#137882 = CARTESIAN_POINT('Ctrl Pts',(-17.9048518984378,12.9400020306265,
131.118407374436)) ;
#137883 = CARTESIAN_POINT('Ctrl Pts',(-17.863651253699,13.1921120605742,131.031037055592)) ;
#137884 = CARTESIAN_POINT('Ctrl Pts',(-17.8450388569388,13.4620045410206,
131.009824678449)) ;
#137885 = CARTESIAN_POINT('Ctrl Pts',(-17.8500091814281,13.7292706250682,
131.057520791156)) ;
#137886 = CARTESIAN_POINT('Ctrl Pts',(-17.877302446402,13.9738125834417,131.170328613009)) ;
#137887 = CARTESIAN_POINT('Ctrl Pts',(-17.9243069985026,14.1794946936577,
131.340779996349)) ;
#137888 = CARTESIAN_POINT('Ctrl Pts',(-17.9872121330728,14.3311259021016,
131.557794969855)) ;
#137889 = CARTESIAN_POINT('Ctrl Pts',(-18.0598546631151,14.4169205484559,
131.802952666368)) ;
#137890 = CARTESIAN_POINT('Ctrl Pts',(-18.1375957078681,14.4320030369242,
132.063314977191)) ;
#137891 = CARTESIAN_POINT('Ctrl Pts',(-18.2128346595683,14.3751243958677,
132.316063847586)) ;
#137892 = CARTESIAN_POINT('Ctrl Pts',(-18.2809030990878,14.2488768695212,
132.548263675906)) ;
#137893 = CARTESIAN_POINT('Ctrl Pts',(-18.3346701612726,14.0648019477406,
132.738317017284)) ;
#137894 = CARTESIAN_POINT('Ctrl Pts',(-18.3706065108531,13.8343789431172,
132.876418354214)) ;
#137895 = CARTESIAN_POINT('Ctrl Pts',(-18.3850723877934,13.5736072409061,
132.951890561446)) ;
#137896 = CARTESIAN_POINT('Ctrl Pts',(-18.3761672531653,13.3025526358433,
132.959029018342)) ;
#137897 = CARTESIAN_POINT('Ctrl Pts',(-18.3442712548047,13.0417946956511,
132.898783688445)) ;
#137898 = CARTESIAN_POINT('Ctrl Pts',(-18.2903655411103,12.8063141545274,
132.774510267761)) ;
#137899 = CARTESIAN_POINT('Ctrl Pts',(-18.2180840269614,12.6158857625783,
132.596412350114)) ;
#137900 = CARTESIAN_POINT('Ctrl Pts',(-18.1311881459215,12.4825397359329,
132.375809127955)) ;
#137901 = CARTESIAN_POINT('Ctrl Pts',(-18.0362627850358,12.4173081349344,
132.131507312481)) ;
#137902 = CARTESIAN_POINT('Ctrl Pts',(-17.9383440031491,12.4236049843711,
131.878609271307)) ;
#137903 = CARTESIAN_POINT('Ctrl Pts',(-17.8440809897297,12.5018025571804,
131.636403802442)) ;
#137904 = CARTESIAN_POINT('Ctrl Pts',(-17.7596883142505,12.6458565227928,
131.422980744586)) ;
#137905 = CARTESIAN_POINT('Ctrl Pts',(-17.6903452885415,12.8453790155913,
131.25350285176)) ;
#137906 = CARTESIAN_POINT('Ctrl Pts',(-17.6401750273876,13.0865651955858,
131.140080379431)) ;
#137907 = CARTESIAN_POINT('Ctrl Pts',(-17.6121734948375,13.3521426916341,
131.091447534242)) ;
#137908 = CARTESIAN_POINT('Ctrl Pts',(-17.6076411176606,13.6222556634887,
131.11130620512)) ;
#137909 = CARTESIAN_POINT('Ctrl Pts',(-17.6260946648748,13.8783882532463,
131.198344630055)) ;
#137910 = CARTESIAN_POINT('Ctrl Pts',(-17.6656422043345,14.1022120327878,
131.347061644052)) ;
#137911 = CARTESIAN_POINT('Ctrl Pts',(-17.7224071623684,14.2765229338953,
131.545938908787)) ;
#137912 = CARTESIAN_POINT('Ctrl Pts',(-17.7917189747294,14.3902286899454,
131.781476416858)) ;
#137913 = CARTESIAN_POINT('Ctrl Pts',(-17.868504117299,14.4347769429382,132.03908049303)) ;
#137914 = CARTESIAN_POINT('Ctrl Pts',(-17.945297953661,14.4066722645431,132.296405177608)) ;
#137915 = CARTESIAN_POINT('Ctrl Pts',(-18.0169665014956,14.3082119147666,
132.538929595933)) ;
#137916 = CARTESIAN_POINT('Ctrl Pts',(-18.0771757737706,14.1460357865502,
132.747971370351)) ;
#137917 = CARTESIAN_POINT('Ctrl Pts',(-18.1208631205668,13.9328084550501,
132.908648173399)) ;
#137918 = CARTESIAN_POINT('Ctrl Pts',(-18.1443765191894,13.6817741223337,
133.01057033936)) ;
#137919 = CARTESIAN_POINT('Ctrl Pts',(-18.1451355362661,13.4140262375942,
133.045780899098)) ;
#137920 = CARTESIAN_POINT('Ctrl Pts',(-18.1223937690385,13.1453688529206,
133.012545885146)) ;
#137921 = CARTESIAN_POINT('Ctrl Pts',(-18.0772619681856,12.8977836855868,
132.913734043249)) ;
#137922 = CARTESIAN_POINT('Ctrl Pts',(-18.0115583762481,12.6861562793818,
132.75510008698)) ;
#137923 = CARTESIAN_POINT('Ctrl Pts',(-17.9302682655273,12.5289208756677,
132.550665981142)) ;
#137924 = CARTESIAN_POINT('Ctrl Pts',(-17.8376485738812,12.4351549245617,
132.313282405298)) ;
#137925 = CARTESIAN_POINT('Ctrl Pts',(-17.7404755119573,12.4122393500749,
132.06240264819)) ;
#137926 = CARTESIAN_POINT('Ctrl Pts',(-17.6435763564324,12.4619213661245,
131.812631468907)) ;
#137927 = CARTESIAN_POINT('Ctrl Pts',(-17.5546470358377,12.5803996271663,
131.5859316702)) ;
#137928 = CARTESIAN_POINT('Ctrl Pts',(-17.4786252319612,12.7591298548141,
131.39696631873)) ;
#137929 = CARTESIAN_POINT('Ctrl Pts',(-17.4203939792657,12.9850686452271,
131.259920960058)) ;
#137930 = CARTESIAN_POINT('Ctrl Pts',(-17.3832212801289,13.2423776276029,
131.184410564057)) ;
#137931 = CARTESIAN_POINT('Ctrl Pts',(-17.3690898070798,13.5129448157843,
131.176250191703)) ;
#137932 = CARTESIAN_POINT('Ctrl Pts',(-17.3783551205516,13.77743197275,131.236478044151)) ;
#137933 = CARTESIAN_POINT('Ctrl Pts',(-17.409759931989,14.0166133244865,131.361417283664)) ;
#137934 = CARTESIAN_POINT('Ctrl Pts',(-17.4598438655703,14.2120829890599,
131.540706325791)) ;
#137935 = CARTESIAN_POINT('Ctrl Pts',(-17.5250988063294,14.3524988741423,
131.764596500736)) ;
#137936 = CARTESIAN_POINT('Ctrl Pts',(-17.5994416441049,14.4253825551606,
132.014893373193)) ;
#137937 = CARTESIAN_POINT('Ctrl Pts',(-17.6767305680226,14.4267683079455,
132.273679412469)) ;
#137938 = CARTESIAN_POINT('Ctrl Pts',(-17.7513139884147,14.3564920605334,
132.524684240105)) ;
#137939 = CARTESIAN_POINT('Ctrl Pts',(-17.8169814369023,14.2186720033249,
132.749746015345)) ;
#137940 = CARTESIAN_POINT('Ctrl Pts',(-17.8678873517568,14.024316870989,132.931562679198)) ;
#137941 = CARTESIAN_POINT('Ctrl Pts',(-17.8999449624512,13.7866137007774,
133.058365103571)) ;
#137942 = CARTESIAN_POINT('Ctrl Pts',(-17.9100655439473,13.5238037993467,
133.120963683801)) ;
#137943 = CARTESIAN_POINT('Ctrl Pts',(-17.8968818080034,13.2527086934904,
133.115621577909)) ;
#137944 = CARTESIAN_POINT('Ctrl Pts',(-17.8603976095492,12.9936531386933,
133.042239984524)) ;
#137945 = CARTESIAN_POINT('Ctrl Pts',(-17.8027854988235,12.7662442453604,
132.907025673019)) ;
#137946 = CARTESIAN_POINT('Ctrl Pts',(-17.727459915204,12.5858801794281,132.720034663329)) ;
#137947 = CARTESIAN_POINT('Ctrl Pts',(-17.6387177576524,12.4648530906934,
132.493949883096)) ;
#137948 = CARTESIAN_POINT('Ctrl Pts',(-17.5421197700846,12.4128201898405,
132.245005559525)) ;
#137949 = CARTESIAN_POINT('Ctrl Pts',(-17.4450854922055,12.4330274008567,
131.994463533369)) ;
#137950 = CARTESIAN_POINT('Ctrl Pts',(-17.3522227610111,12.5240123078526,
131.756341738845)) ;
#137951 = CARTESIAN_POINT('Ctrl Pts',(-17.2702012517368,12.6795221093343,
131.549866414866)) ;
#137952 = CARTESIAN_POINT('Ctrl Pts',(-17.2040049855668,12.8889213981569,
131.389705808723)) ;
#137953 = CARTESIAN_POINT('Ctrl Pts',(-17.1579940844833,13.1354946974878,
131.288346856863)) ;
#137954 = CARTESIAN_POINT('Ctrl Pts',(-17.1343661691126,13.4042911387148,
131.252587647338)) ;
#137955 = CARTESIAN_POINT('Ctrl Pts',(-17.1342785297306,13.6719452303359,
131.285274315191)) ;
#137956 = CARTESIAN_POINT('Ctrl Pts',(-17.1569876367207,13.9242175359662,
131.384873870538)) ;
#137957 = CARTESIAN_POINT('Ctrl Pts',(-17.200011377229,14.1390288765416,131.543612046333)) ;
#137958 = CARTESIAN_POINT('Ctrl Pts',(-17.2595571651154,14.3030286155002,
131.750644929818)) ;
#137959 = CARTESIAN_POINT('Ctrl Pts',(-17.3308835517988,14.4041953321141,
131.992170382071)) ;
#137960 = CARTESIAN_POINT('Ctrl Pts',(-17.407703870412,14.4349854776255,132.249625669667)) ;
#137961 = CARTESIAN_POINT('Ctrl Pts',(-17.4843503152303,14.3934046912769,
132.506700507749)) ;
#137962 = CARTESIAN_POINT('Ctrl Pts',(-17.5541977602429,14.2822103213118,
132.743866956498)) ;
#137963 = CARTESIAN_POINT('Ctrl Pts',(-17.611586421142,14.1097942547729,132.944599624469)) ;
#137964 = CARTESIAN_POINT('Ctrl Pts',(-17.6518405058853,13.8877667397205,
133.095350804758)) ;
#137965 = CARTESIAN_POINT('Ctrl Pts',(-17.6711705177654,13.6324084843775,
133.18497005015)) ;
#137966 = CARTESIAN_POINT('Ctrl Pts',(-17.667514600264,13.362418602374,133.207397716684)) ;
#137967 = CARTESIAN_POINT('Ctrl Pts',(-17.6404429322753,13.0965815355502,
133.161441915775)) ;
#137968 = CARTESIAN_POINT('Ctrl Pts',(-17.5910518071046,12.8540736750208,
133.050310617862)) ;
#137969 = CARTESIAN_POINT('Ctrl Pts',(-17.5226154463243,12.6529924848678,
132.883394021802)) ;
#137970 = CARTESIAN_POINT('Ctrl Pts',(-17.4380430797127,12.5055874669249,
132.669701279278)) ;
#137971 = CARTESIAN_POINT('Ctrl Pts',(-17.3446363922236,12.4255318802945,
132.429776740736)) ;
#137972 = CARTESIAN_POINT('Ctrl Pts',(-17.2467990552435,12.4160627421656,
132.17710214303)) ;
#137973 = CARTESIAN_POINT('Ctrl Pts',(-17.1513349333761,12.4788298708389,
131.931338759304)) ;
#137974 = CARTESIAN_POINT('Ctrl Pts',(-17.0640791511962,12.6096602147663,
131.709653385946)) ;
#137975 = CARTESIAN_POINT('Ctrl Pts',(-16.9910680476231,12.7985461290531,
131.529487423907)) ;
#137976 = CARTESIAN_POINT('Ctrl Pts',(-16.9365757845701,13.0317085131987,
131.403370398451)) ;
#137977 = CARTESIAN_POINT('Ctrl Pts',(-16.9036356126022,13.2930834714085,
131.340246128436)) ;
#137978 = CARTESIAN_POINT('Ctrl Pts',(-16.8939332084059,13.5641923615561,
131.345053455658)) ;
#137979 = CARTESIAN_POINT('Ctrl Pts',(-16.9076309665478,13.825680563738,131.418292261047)) ;
#137980 = CARTESIAN_POINT('Ctrl Pts',(-16.9426513295678,14.0565822354865,
131.553574700513)) ;
#137981 = CARTESIAN_POINT('Ctrl Pts',(-16.9960730462588,14.2434410576494,
131.742775697406)) ;
#137982 = CARTESIAN_POINT('Ctrl Pts',(-17.063462231909,14.3714533294417,131.972845687759)) ;
#137983 = CARTESIAN_POINT('Ctrl Pts',(-17.1386182416936,14.4311593636965,
132.225408177244)) ;
#137984 = CARTESIAN_POINT('Ctrl Pts',(-17.2162705777589,14.4188767520017,
132.485449845098)) ;
#137985 = CARTESIAN_POINT('Ctrl Pts',(-17.289454458351,14.3353894135925,132.732308120181)) ;
#137986 = CARTESIAN_POINT('Ctrl Pts',(-17.3527484313346,14.1858866633471,
132.950435408973)) ;
#137987 = CARTESIAN_POINT('Ctrl Pts',(-17.4002649162093,13.9829323617686,
133.12224680942)) ;
#137988 = CARTESIAN_POINT('Ctrl Pts',(-17.4284928876731,13.7386002363464,
133.237921480042)) ;
#137989 = CARTESIAN_POINT('Ctrl Pts',(-17.4342568106554,13.4724911093289,
133.28784950881)) ;
#137990 = CARTESIAN_POINT('Ctrl Pts',(-17.4166917401806,13.2027754915033,
133.269636837191)) ;
#137991 = CARTESIAN_POINT('Ctrl Pts',(-17.3758922241434,12.9475729624172,
133.183729538493)) ;
#137992 = CARTESIAN_POINT('Ctrl Pts',(-17.3148505174348,12.7286906957619,
133.038370433074)) ;
#137993 = CARTESIAN_POINT('Ctrl Pts',(-17.2365672672713,12.5582194265839,
132.842798939928)) ;
#137994 = CARTESIAN_POINT('Ctrl Pts',(-17.145755018373,12.449581474798,132.610728316885)) ;
#137995 = CARTESIAN_POINT('Ctrl Pts',(-17.048869231413,12.4111325027633,132.360788548371)) ;
#137996 = CARTESIAN_POINT('Ctrl Pts',(-16.9518907589334,12.4448573237376,
132.110542706646)) ;
#137997 = CARTESIAN_POINT('Ctrl Pts',(-16.8606690827077,12.5485736287012,
131.877191065832)) ;
#137998 = CARTESIAN_POINT('Ctrl Pts',(-16.7809677960658,12.7160675413709,
131.677651641686)) ;
#137999 = CARTESIAN_POINT('Ctrl Pts',(-16.7187005371509,12.9327061605047,
131.528760508014)) ;
#138000 = CARTESIAN_POINT('Ctrl Pts',(-16.6766985699532,13.1846668295447,
131.439140928805)) ;
#138001 = CARTESIAN_POINT('Ctrl Pts',(-16.6574670017428,13.454422434914,131.416124014694)) ;
#138002 = CARTESIAN_POINT('Ctrl Pts',(-16.661742910167,13.7215757053134,131.461733848406)) ;
#138003 = CARTESIAN_POINT('Ctrl Pts',(-16.6884601779481,13.9674105502267,
131.572911655568)) ;
#138004 = CARTESIAN_POINT('Ctrl Pts',(-16.7348809932181,14.1739595025082,
131.741594194927)) ;
#138005 = CARTESIAN_POINT('Ctrl Pts',(-16.7971641277775,14.3272528691842,
131.95669868954)) ;
#138006 = CARTESIAN_POINT('Ctrl Pts',(-16.8700735166993,14.4155297813334,
132.202859198817)) ;
#138007 = CARTESIAN_POINT('Ctrl Pts',(-16.9472882019751,14.4326688958934,
132.461466810552)) ;
#138008 = CARTESIAN_POINT('Ctrl Pts',(-17.0231401686984,14.3775211091171,
132.716222598503)) ;
#138009 = CARTESIAN_POINT('Ctrl Pts',(-17.0910320528626,14.2540409956265,
132.947659679326)) ;
#138010 = CARTESIAN_POINT('Ctrl Pts',(-17.1455765747362,14.0709649077151,
133.140134912755)) ;
#138011 = CARTESIAN_POINT('Ctrl Pts',(-17.1820383867769,13.8416200756966,
133.279758830705)) ;
#138012 = CARTESIAN_POINT('Ctrl Pts',(-17.1971558117406,13.5823886653328,
133.357025362899)) ;
#138013 = CARTESIAN_POINT('Ctrl Pts',(-17.1890809730824,13.3112805522026,
133.366597716942)) ;
#138014 = CARTESIAN_POINT('Ctrl Pts',(-17.1576142662405,13.0483998972253,
133.307814067063)) ;
#138015 = CARTESIAN_POINT('Ctrl Pts',(-17.1045340611823,12.8130299251434,
133.18579186815)) ;
#138016 = CARTESIAN_POINT('Ctrl Pts',(-17.0325353932624,12.6204061484624,
133.008629332675)) ;
#138017 = CARTESIAN_POINT('Ctrl Pts',(-16.9460051642248,12.4854479729451,
132.789070942826)) ;
#138018 = CARTESIAN_POINT('Ctrl Pts',(-16.8512268174505,12.4181326854097,
132.545207526116)) ;
#138019 = CARTESIAN_POINT('Ctrl Pts',(-16.7530299629711,12.4224942327925,
132.291585045142)) ;
#138020 = CARTESIAN_POINT('Ctrl Pts',(-16.6586767662889,12.4989652676932,
132.049092748305)) ;
#138021 = CARTESIAN_POINT('Ctrl Pts',(-16.5742899308655,12.6405918868476,
131.835543037408)) ;
#138022 = CARTESIAN_POINT('Ctrl Pts',(-16.5042089716432,12.8391592679731,
131.66400498736)) ;
#138023 = CARTESIAN_POINT('Ctrl Pts',(-16.4533647225878,13.0802458850777,
131.548711680705)) ;
#138024 = CARTESIAN_POINT('Ctrl Pts',(-16.4248581823331,13.3449461423443,
131.498541148238)) ;
#138025 = CARTESIAN_POINT('Ctrl Pts',(-16.4196652563147,13.6142996015355,
131.516362648374)) ;
#138026 = CARTESIAN_POINT('Ctrl Pts',(-16.4374352642044,13.871042063758,131.601394145467)) ;
#138027 = CARTESIAN_POINT('Ctrl Pts',(-16.4763794639753,14.0962487888297,
131.748356865339)) ;
#138028 = CARTESIAN_POINT('Ctrl Pts',(-16.5330749843241,14.2729913868137,
131.947221307867)) ;
#138029 = CARTESIAN_POINT('Ctrl Pts',(-16.6017670425338,14.3876795373717,
132.180769530083)) ;
#138030 = CARTESIAN_POINT('Ctrl Pts',(-16.6783001681769,14.4346057861214,
132.437586362415)) ;
#138031 = CARTESIAN_POINT('Ctrl Pts',(-16.7555901343856,14.4082599511792,
132.696547850718)) ;
#138032 = CARTESIAN_POINT('Ctrl Pts',(-16.8270546879802,14.3122705937861,
132.938272501908)) ;
#138033 = CARTESIAN_POINT('Ctrl Pts',(-16.8879493008856,14.1514361884325,
133.149437664589)) ;
#138034 = CARTESIAN_POINT('Ctrl Pts',(-16.9321596596727,13.938718878438,133.311723147941)) ;
#138035 = CARTESIAN_POINT('Ctrl Pts',(-16.9561807399697,13.6904434101565,
133.414875985821)) ;
#138036 = CARTESIAN_POINT('Ctrl Pts',(-16.9576332584604,13.4208420564826,
133.452380950427)) ;
#138037 = CARTESIAN_POINT('Ctrl Pts',(-16.9356300496651,13.1534853885067,
133.421103696326)) ;
#138038 = CARTESIAN_POINT('Ctrl Pts',(-16.8910845324162,12.9044050301422,
133.324087087722)) ;
#138039 = CARTESIAN_POINT('Ctrl Pts',(-16.8258399516658,12.6913476051149,
133.166814351142)) ;
#138040 = CARTESIAN_POINT('Ctrl Pts',(-16.7448464344601,12.5324269089272,
132.963277516479)) ;
#138041 = CARTESIAN_POINT('Ctrl Pts',(-16.6527813349133,12.4369854999087,
132.727399071395)) ;
#138042 = CARTESIAN_POINT('Ctrl Pts',(-16.5554635744337,12.4119049756276,
132.476169895595)) ;
#138043 = CARTESIAN_POINT('Ctrl Pts',(-16.4587903747933,12.4592885776231,
132.226936038438)) ;
#138044 = CARTESIAN_POINT('Ctrl Pts',(-16.369459226937,12.5757336581161,131.999091644708)) ;
#138045 = CARTESIAN_POINT('Ctrl Pts',(-16.2929303792811,12.7527802479952,
131.808650847101)) ;
#138046 = CARTESIAN_POINT('Ctrl Pts',(-16.233831620826,12.9786617700214,131.669233459945)) ;
#138047 = CARTESIAN_POINT('Ctrl Pts',(-16.1960975343855,13.2359087639226,
131.592141252244)) ;
#138048 = CARTESIAN_POINT('Ctrl Pts',(-16.1813777949376,13.5051025506678,
131.582103812986)) ;
#138049 = CARTESIAN_POINT('Ctrl Pts',(-16.1900648118431,13.7711208061555,
131.640785889966)) ;
#138050 = CARTESIAN_POINT('Ctrl Pts',(-16.2207641246595,14.0100002848338,
131.763493038331)) ;
#138051 = CARTESIAN_POINT('Ctrl Pts',(-16.270434947496,14.2073723791963,131.941647170154)) ;
#138052 = CARTESIAN_POINT('Ctrl Pts',(-16.3352409404344,14.3492225893051,
132.164164640069)) ;
#138053 = CARTESIAN_POINT('Ctrl Pts',(-16.409293471862,14.4242519725476,132.413576464951)) ;
#138054 = CARTESIAN_POINT('Ctrl Pts',(-16.4869103046887,14.4277364692307,
132.673460341557)) ;
#138055 = CARTESIAN_POINT('Ctrl Pts',(-16.5615560359961,14.3592420521561,
132.924612133088)) ;
#138056 = CARTESIAN_POINT('Ctrl Pts',(-16.6272846105789,14.2240687585133,
133.149692670284)) ;
#138057 = CARTESIAN_POINT('Ctrl Pts',(-16.6788937432045,14.030558632252,133.333688881493)) ;
#138058 = CARTESIAN_POINT('Ctrl Pts',(-16.711477566971,13.7945207204753,133.461937265753)) ;
#138059 = CARTESIAN_POINT('Ctrl Pts',(-16.7223284172129,13.5313068874669,
133.52678750857)) ;
#138060 = CARTESIAN_POINT('Ctrl Pts',(-16.7097854403445,13.2605193044374,
133.523270922987)) ;
#138061 = CARTESIAN_POINT('Ctrl Pts',(-16.6741113532666,13.0015411948259,
133.452162116115)) ;
#138062 = CARTESIAN_POINT('Ctrl Pts',(-16.6170671904399,12.7725524549383,
133.318651252456)) ;
#138063 = CARTESIAN_POINT('Ctrl Pts',(-16.5419949518571,12.5901314518039,
133.132487335332)) ;
#138064 = CARTESIAN_POINT('Ctrl Pts',(-16.4536061361104,12.4675131593939,
132.907409541441)) ;
#138065 = CARTESIAN_POINT('Ctrl Pts',(-16.3575808899583,12.4133289167984,
132.659991584727)) ;
#138066 = CARTESIAN_POINT('Ctrl Pts',(-16.2598099681386,12.4315113355368,
132.407532861116)) ;
#138067 = CARTESIAN_POINT('Ctrl Pts',(-16.1670397257563,12.5204618518985,
132.16957309303)) ;
#138068 = CARTESIAN_POINT('Ctrl Pts',(-16.0846355190378,12.6740885345687,
131.961972963439)) ;
#138069 = CARTESIAN_POINT('Ctrl Pts',(-16.0179019249324,12.8820605395618,
131.800234643535)) ;
#138070 = CARTESIAN_POINT('Ctrl Pts',(-15.9712426615901,13.1280848840325,
131.697024439696)) ;
#138071 = CARTESIAN_POINT('Ctrl Pts',(-15.9469668397302,13.3954305340358,
131.659233485228)) ;
#138072 = CARTESIAN_POINT('Ctrl Pts',(-15.9461825995179,13.6647721177767,
131.690068609628)) ;
#138073 = CARTESIAN_POINT('Ctrl Pts',(-15.9681635891478,13.9166503659834,
131.787382281983)) ;
#138074 = CARTESIAN_POINT('Ctrl Pts',(-16.0106798137103,14.1333087838378,
131.944714198646)) ;
#138075 = CARTESIAN_POINT('Ctrl Pts',(-16.0697275923172,14.2989356853765,
132.150254382635)) ;
#138076 = CARTESIAN_POINT('Ctrl Pts',(-16.1412221891328,14.4025578150193,
132.392466616012)) ;
#138077 = CARTESIAN_POINT('Ctrl Pts',(-16.2177066260317,14.4350103975139,
132.648822954175)) ;
#138078 = CARTESIAN_POINT('Ctrl Pts',(-16.2943852287552,14.3956728087921,
132.905961120951)) ;
#138079 = CARTESIAN_POINT('Ctrl Pts',(-16.3645411469182,14.2862787628231,
133.144049835379)) ;
#138080 = CARTESIAN_POINT('Ctrl Pts',(-16.4223268601029,14.1158603656016,
133.345893655305)) ;
#138081 = CARTESIAN_POINT('Ctrl Pts',(-16.4633288681658,13.8934485615438,
133.499050647192)) ;
#138082 = CARTESIAN_POINT('Ctrl Pts',(-16.4831146759898,13.6404741720686,
133.589770768568)) ;
#138083 = CARTESIAN_POINT('Ctrl Pts',(-16.4801375304379,13.3695007769354,
133.61432799691)) ;
#138084 = CARTESIAN_POINT('Ctrl Pts',(-16.4537797381838,13.1044457745781,
133.57031484177)) ;
#138085 = CARTESIAN_POINT('Ctrl Pts',(-16.4050939273146,12.8607040814897,
133.461257392851)) ;
#138086 = CARTESIAN_POINT('Ctrl Pts',(-16.3365614867353,12.6571155232214,
133.294299070555)) ;
#138087 = CARTESIAN_POINT('Ctrl Pts',(-16.2534138250762,12.5098080882698,
133.0843480198)) ;
#138088 = CARTESIAN_POINT('Ctrl Pts',(-16.1596845798564,12.4266891682411,
132.843691860747)) ;
#138089 = CARTESIAN_POINT('Ctrl Pts',(-16.0616021737357,12.4154229677179,
132.590386606377)) ;
#138090 = CARTESIAN_POINT('Ctrl Pts',(-15.966325957389,12.4759770344289,132.345056626352)) ;
#138091 = CARTESIAN_POINT('Ctrl Pts',(-15.8787279504542,12.6048251808736,
132.12237116192)) ;
#138092 = CARTESIAN_POINT('Ctrl Pts',(-15.8052016738303,12.7921644823966,
131.940705271743)) ;
#138093 = CARTESIAN_POINT('Ctrl Pts',(-15.7500244795214,13.0247861234327,
131.812661169464)) ;
#138094 = CARTESIAN_POINT('Ctrl Pts',(-15.7164543667027,13.2853104299406,
131.747653984486)) ;
#138095 = CARTESIAN_POINT('Ctrl Pts',(-15.7061363872041,13.5574329936333,
131.750794145615)) ;
#138096 = CARTESIAN_POINT('Ctrl Pts',(-15.7190145282048,13.8171020410684,
131.821326630695)) ;
#138097 = CARTESIAN_POINT('Ctrl Pts',(-15.7536666697236,14.0511737874882,
131.955815273683)) ;
#138098 = CARTESIAN_POINT('Ctrl Pts',(-15.8066102077267,14.2388281318634,
132.143548289998)) ;
#138099 = CARTESIAN_POINT('Ctrl Pts',(-15.8734175812164,14.3685838894511,
132.371814409385)) ;
#138100 = CARTESIAN_POINT('Ctrl Pts',(-15.9490084927082,14.4305511388163,
132.625903139036)) ;
#138101 = CARTESIAN_POINT('Ctrl Pts',(-16.0261164552073,14.4203097552105,
132.884100960231)) ;
#138102 = CARTESIAN_POINT('Ctrl Pts',(-16.0998534732104,14.3384208536168,
133.132745263409)) ;
#138103 = CARTESIAN_POINT('Ctrl Pts',(-16.1631903784252,14.191573241038,133.350802092867)) ;
#138104 = CARTESIAN_POINT('Ctrl Pts',(-16.2115879549403,13.9880715785311,
133.525492647251)) ;
#138105 = CARTESIAN_POINT('Ctrl Pts',(-16.2400869176167,13.7471726162761,
133.641599094846)) ;
#138106 = CARTESIAN_POINT('Ctrl Pts',(-16.246651218704,13.4800206998336,133.694060674702)) ;
#138107 = CARTESIAN_POINT('Ctrl Pts',(-16.229778657571,13.2110031222513,133.677758671742)) ;
#138108 = CARTESIAN_POINT('Ctrl Pts',(-16.1896573660202,12.9547749456752,
133.593866138619)) ;
#138109 = CARTESIAN_POINT('Ctrl Pts',(-16.1291102530169,12.7344342581801,
133.449982717363)) ;
#138110 = CARTESIAN_POINT('Ctrl Pts',(-16.0512258609112,12.5623453815543,
133.255586921922)) ;
#138111 = CARTESIAN_POINT('Ctrl Pts',(-15.9608808173794,12.4518692126569,
133.024814380634)) ;
#138112 = CARTESIAN_POINT('Ctrl Pts',(-15.8638130263969,12.4112334904619,
132.774443526975)) ;
#138113 = CARTESIAN_POINT('Ctrl Pts',(-15.7668529272895,12.442749147545,132.5242072591)) ;
#138114 = CARTESIAN_POINT('Ctrl Pts',(-15.6748471126679,12.5456206803201,
132.288785581323)) ;
#138115 = CARTESIAN_POINT('Ctrl Pts',(-15.5957928836906,12.7091960284291,
132.090684643297)) ;
#138116 = CARTESIAN_POINT('Ctrl Pts',(-15.532372609487,12.9259029795746,131.938683853535)) ;
#138117 = CARTESIAN_POINT('Ctrl Pts',(-15.4898220287173,13.1770736190436,
131.847439441881)) ;
#138118 = CARTESIAN_POINT('Ctrl Pts',(-15.4698955138865,13.446876823357,131.822431045904)) ;
#138119 = CARTESIAN_POINT('Ctrl Pts',(-15.473510723152,13.7138795618443,131.86604868999)) ;
#138120 = CARTESIAN_POINT('Ctrl Pts',(-15.4995760707828,13.9605431609207,
131.975315053857)) ;
#138121 = CARTESIAN_POINT('Ctrl Pts',(-15.5454521788285,14.1686235242906,
132.142413250352)) ;
#138122 = CARTESIAN_POINT('Ctrl Pts',(-15.6076569312687,14.324111246448,132.35743463947)) ;
#138123 = CARTESIAN_POINT('Ctrl Pts',(-15.6799406277305,14.4138215674339,
132.60157667707)) ;
#138124 = CARTESIAN_POINT('Ctrl Pts',(-15.7574038518846,14.433194510591,132.861043022859)) ;
#138125 = CARTESIAN_POINT('Ctrl Pts',(-15.8331619537095,14.3801615030747,
133.115422095018)) ;
#138126 = CARTESIAN_POINT('Ctrl Pts',(-15.9014613999127,14.2584943373808,
133.348094869365)) ;
#138127 = CARTESIAN_POINT('Ctrl Pts',(-15.9564312114714,14.0770492595335,
133.541793626735)) ;
#138128 = CARTESIAN_POINT('Ctrl Pts',(-15.9935402622882,13.8484876221982,
133.683360192996)) ;
#138129 = CARTESIAN_POINT('Ctrl Pts',(-16.009247390655,13.5893551833119,133.762405373348)) ;
#138130 = CARTESIAN_POINT('Ctrl Pts',(-16.0018749025918,13.3196923685202,
133.773860283275)) ;
#138131 = CARTESIAN_POINT('Ctrl Pts',(-15.9711471832523,13.0561135108425,
133.717252900059)) ;
#138132 = CARTESIAN_POINT('Ctrl Pts',(-15.9185145007849,12.8190742431854,
133.596625733539)) ;
#138133 = CARTESIAN_POINT('Ctrl Pts',(-15.8470380014776,12.6252976951711,
133.420956165043)) ;
#138134 = CARTESIAN_POINT('Ctrl Pts',(-15.7611948347474,12.4887797495905,
133.203286234919)) ;
#138135 = CARTESIAN_POINT('Ctrl Pts',(-15.6662301653529,12.4190606643947,
132.959008435366)) ;
#138136 = CARTESIAN_POINT('Ctrl Pts',(-15.5683946837629,12.4213023126393,
132.706315786054)) ;
#138137 = CARTESIAN_POINT('Ctrl Pts',(-15.4738004702747,12.4953371872364,
132.463124320861)) ;
#138138 = CARTESIAN_POINT('Ctrl Pts',(-15.388635753643,12.6358732180601,132.247464766846)) ;
#138139 = CARTESIAN_POINT('Ctrl Pts',(-15.3182966935884,12.8325868641011,
132.075082447187)) ;
#138140 = CARTESIAN_POINT('Ctrl Pts',(-15.2669461693639,13.0715961519443,
131.958183075629)) ;
#138141 = CARTESIAN_POINT('Ctrl Pts',(-15.2375683477149,13.3366927750057,
131.905581597702)) ;
#138142 = CARTESIAN_POINT('Ctrl Pts',(-15.2316989598249,13.606785296831,131.921501350001)) ;
#138143 = CARTESIAN_POINT('Ctrl Pts',(-15.2488554240905,13.8640946124835,
132.004734373222)) ;
#138144 = CARTESIAN_POINT('Ctrl Pts',(-15.2871043553366,14.0898396891215,
132.149570187172)) ;
#138145 = CARTESIAN_POINT('Ctrl Pts',(-15.3432768304583,14.2683601358406,
132.346899303774)) ;
#138146 = CARTESIAN_POINT('Ctrl Pts',(-15.4119474860211,14.3854877046267,
132.58051583122)) ;
#138147 = CARTESIAN_POINT('Ctrl Pts',(-15.4884424926978,14.4341894572121,
132.837252051673)) ;
#138148 = CARTESIAN_POINT('Ctrl Pts',(-15.5653738474254,14.4102459921106,
133.094979330122)) ;
#138149 = CARTESIAN_POINT('Ctrl Pts',(-15.6374786298125,14.3157190634071,
133.33876207548)) ;
#138150 = CARTESIAN_POINT('Ctrl Pts',(-15.6984108184879,14.1574303068782,
133.549845061473)) ;
#138151 = CARTESIAN_POINT('Ctrl Pts',(-15.7433567069142,13.9458829151207,
133.714346199498)) ;
#138152 = CARTESIAN_POINT('Ctrl Pts',(-15.7680544461719,13.6969896292084,
133.819651524776)) ;
#138153 = CARTESIAN_POINT('Ctrl Pts',(-15.7701128925175,13.4292803760991,
133.858728163607)) ;
#138154 = CARTESIAN_POINT('Ctrl Pts',(-15.7489102637766,13.161309101516,133.829820281867)) ;
#138155 = CARTESIAN_POINT('Ctrl Pts',(-15.7044987762573,12.9096301866455,
133.733459274238)) ;
#138156 = CARTESIAN_POINT('Ctrl Pts',(-15.6404646327747,12.6977069175332,
133.579353143141)) ;
#138157 = CARTESIAN_POINT('Ctrl Pts',(-15.559648556402,12.5361591830993,133.376465293707)) ;
#138158 = CARTESIAN_POINT('Ctrl Pts',(-15.4678292234998,12.4388403169488,
133.141295158116)) ;
#138159 = CARTESIAN_POINT('Ctrl Pts',(-15.3704747732284,12.4115721832676,
132.889995995841)) ;
#138160 = CARTESIAN_POINT('Ctrl Pts',(-15.2736312055909,12.457029405049,132.640284459813)) ;
#138161 = CARTESIAN_POINT('Ctrl Pts',(-15.184195197508,12.5713337324556,132.412066033633)) ;
#138162 = CARTESIAN_POINT('Ctrl Pts',(-15.1071501777741,12.7468028195077,
132.220136803515)) ;
#138163 = CARTESIAN_POINT('Ctrl Pts',(-15.047509486281,12.9715572514285,132.079139887293)) ;
#138164 = CARTESIAN_POINT('Ctrl Pts',(-15.0091484797696,13.2272670730613,
132.000111495129)) ;
#138165 = CARTESIAN_POINT('Ctrl Pts',(-14.9936966441721,13.4980618104753,
131.988152202933)) ;
#138166 = CARTESIAN_POINT('Ctrl Pts',(-15.001604720738,13.7620973804226,132.044245602663)) ;
#138167 = CARTESIAN_POINT('Ctrl Pts',(-15.0317823075058,14.0037248374368,
132.165654919109)) ;
#138168 = CARTESIAN_POINT('Ctrl Pts',(-15.0809769621606,14.2023999767799,
132.342402115779)) ;
#138169 = CARTESIAN_POINT('Ctrl Pts',(-15.1456099214344,14.3463072474208,
132.564505013179)) ;
#138170 = CARTESIAN_POINT('Ctrl Pts',(-15.2191783755769,14.422940695718,132.812364240475)) ;
#138171 = CARTESIAN_POINT('Ctrl Pts',(-15.2967860408574,14.4287087327574,
133.072227594889)) ;
#138172 = CARTESIAN_POINT('Ctrl Pts',(-15.3716376729965,14.3623692114808,
133.323987574419)) ;
#138173 = CARTESIAN_POINT('Ctrl Pts',(-15.4379695538221,14.2283780368313,
133.550970447247)) ;
#138174 = CARTESIAN_POINT('Ctrl Pts',(-15.4899134645702,14.0364257268117,
133.735894159578)) ;
#138175 = CARTESIAN_POINT('Ctrl Pts',(-15.5230141171127,13.8020945875402,
133.865562324939)) ;
#138176 = CARTESIAN_POINT('Ctrl Pts',(-15.5345523813327,13.5391614868317,
133.932453214591)) ;
#138177 = CARTESIAN_POINT('Ctrl Pts',(-15.5227285394594,13.2686187848472,
133.930998203796)) ;
#138178 = CARTESIAN_POINT('Ctrl Pts',(-15.4876456278164,13.0086420125285,
133.861671450079)) ;
#138179 = CARTESIAN_POINT('Ctrl Pts',(-15.4313828702978,12.7791081292504,
133.730344592057)) ;
#138180 = CARTESIAN_POINT('Ctrl Pts',(-15.3564307908051,12.5942977815412,
133.544687034302)) ;
#138181 = CARTESIAN_POINT('Ctrl Pts',(-15.2686565651916,12.470297081659,133.321282306556)) ;
#138182 = CARTESIAN_POINT('Ctrl Pts',(-15.1725820175887,12.4139049910115,
133.073791862213)) ;
#138183 = CARTESIAN_POINT('Ctrl Pts',(-15.0751009055877,12.4297924178913,
132.822062245848)) ;
#138184 = CARTESIAN_POINT('Ctrl Pts',(-14.9814943161782,12.5172147153485,
132.581873444977)) ;
#138185 = CARTESIAN_POINT('Ctrl Pts',(-14.8987521018085,12.6696685432672,
132.373307698593)) ;
#138186 = CARTESIAN_POINT('Ctrl Pts',(-14.8319357526133,12.8748935660195,
132.211108712332)) ;
#138187 = CARTESIAN_POINT('Ctrl Pts',(-14.7844724177792,13.1206629009233,
132.105647075877)) ;
#138188 = CARTESIAN_POINT('Ctrl Pts',(-14.7595563487713,13.3874986726008,
132.06596134526)) ;
#138189 = CARTESIAN_POINT('Ctrl Pts',(-14.758095005719,13.6577700342002,132.094905614256)) ;
#138190 = CARTESIAN_POINT('Ctrl Pts',(-14.7795395109122,13.9102263509794,
132.190647313271)) ;
#138191 = CARTESIAN_POINT('Ctrl Pts',(-14.8212877176841,14.1273421319092,
132.345592371695)) ;
#138192 = CARTESIAN_POINT('Ctrl Pts',(-14.8803004027794,14.2954362033895,
132.5512322011)) ;
#138193 = CARTESIAN_POINT('Ctrl Pts',(-14.9508986266852,14.4001990487277,
132.790525926894)) ;
#138194 = CARTESIAN_POINT('Ctrl Pts',(-15.0280123654046,14.4351706370755,
133.049038822137)) ;
#138195 = CARTESIAN_POINT('Ctrl Pts',(-15.1043517226695,14.3977719552174,
133.304998580299)) ;
#138196 = CARTESIAN_POINT('Ctrl Pts',(-15.1749382989597,14.2904204351337,
133.544401657337)) ;
#138197 = CARTESIAN_POINT('Ctrl Pts',(-15.2332991479685,14.1205426319521,
133.748067460587)) ;
#138198 = CARTESIAN_POINT('Ctrl Pts',(-15.2744570161202,13.9015880459834,
133.901346174034)) ;
#138199 = CARTESIAN_POINT('Ctrl Pts',(-15.2950942480665,13.6483197880018,
133.994710398155)) ;
#138200 = CARTESIAN_POINT('Ctrl Pts',(-15.2927791762567,13.3774460440173,
134.021204705381)) ;
#138201 = CARTESIAN_POINT('Ctrl Pts',(-15.2670274488561,13.1115164567619,
133.979025907644)) ;
#138202 = CARTESIAN_POINT('Ctrl Pts',(-15.2190484647999,12.8676277943346,
133.871940072646)) ;
#138203 = CARTESIAN_POINT('Ctrl Pts',(-15.151375622549,12.6630942095761,133.70737402675)) ;
#138204 = CARTESIAN_POINT('Ctrl Pts',(-15.0680214022309,12.5128296966432,
133.497060151253)) ;
#138205 = CARTESIAN_POINT('Ctrl Pts',(-14.9744932694045,12.42805223675,133.256979709909)) ;
#138206 = CARTESIAN_POINT('Ctrl Pts',(-14.8766121383161,12.4147676661353,
133.004208092286)) ;
#138207 = CARTESIAN_POINT('Ctrl Pts',(-14.7811668098369,12.4732051898518,
132.75838587031)) ;
#138208 = CARTESIAN_POINT('Ctrl Pts',(-14.6929706084526,12.6008829742714,
132.534073690074)) ;
#138209 = CARTESIAN_POINT('Ctrl Pts',(-14.6193920014731,12.7859099614939,
132.352088247255)) ;
#138210 = CARTESIAN_POINT('Ctrl Pts',(-14.5636050471311,13.0171549052487,
132.222240809291)) ;
#138211 = CARTESIAN_POINT('Ctrl Pts',(-14.5293360875052,13.277402309204,132.155230612714)) ;
#138212 = CARTESIAN_POINT('Ctrl Pts',(-14.5182996919213,13.5492090907174,
132.156231309037)) ;
#138213 = CARTESIAN_POINT('Ctrl Pts',(-14.5305857227298,13.8101281640257,
132.225131951709)) ;
#138214 = CARTESIAN_POINT('Ctrl Pts',(-14.5644345612442,14.0442615498891,
132.35711154665)) ;
#138215 = CARTESIAN_POINT('Ctrl Pts',(-14.6173143320161,14.2348996277818,
132.54492092966)) ;
#138216 = CARTESIAN_POINT('Ctrl Pts',(-14.6834945620548,14.365488247491,132.771175660337)) ;
#138217 = CARTESIAN_POINT('Ctrl Pts',(-14.7587206634414,14.429722906614,133.024124517551)) ;
#138218 = CARTESIAN_POINT('Ctrl Pts',(-14.8361154517203,14.4216680373145,
133.283271314569)) ;
#138219 = CARTESIAN_POINT('Ctrl Pts',(-14.9100777170694,14.3417421595957,
133.532580346532)) ;
#138220 = CARTESIAN_POINT('Ctrl Pts',(-14.9737927629375,14.1964292169101,
133.751768065663)) ;
#138221 = CARTESIAN_POINT('Ctrl Pts',(-15.0224985277877,13.9955519637573,
133.927180888922)) ;
#138222 = CARTESIAN_POINT('Ctrl Pts',(-15.0518421016778,13.7541465447125,
134.045965793673)) ;
#138223 = CARTESIAN_POINT('Ctrl Pts',(-15.058983051814,13.4873871522708,134.100101961475)) ;
#138224 = CARTESIAN_POINT('Ctrl Pts',(-15.0427889947955,13.2187119669683,
134.085726725674)) ;
#138225 = CARTESIAN_POINT('Ctrl Pts',(-15.0034481865866,12.9622340924051,
134.004045221197)) ;
#138226 = CARTESIAN_POINT('Ctrl Pts',(-14.9431938775443,12.7396655368573,
133.861166062646)) ;
#138227 = CARTESIAN_POINT('Ctrl Pts',(-14.8657108599282,12.5663130362906,
133.667926321551)) ;
#138228 = CARTESIAN_POINT('Ctrl Pts',(-14.7760398095514,12.4542929852172,
133.438984177008)) ;
#138229 = CARTESIAN_POINT('Ctrl Pts',(-14.678743994539,12.4113060985389,133.188061925005)) ;
#138230 = CARTESIAN_POINT('Ctrl Pts',(-14.5818778745094,12.440972973662,132.938049002869)) ;
#138231 = CARTESIAN_POINT('Ctrl Pts',(-14.4900849893319,12.5408195803972,
132.703054608506)) ;
#138232 = CARTESIAN_POINT('Ctrl Pts',(-14.4096989960112,12.7045177215447,
132.501438908251)) ;
#138233 = CARTESIAN_POINT('Ctrl Pts',(-14.346132189806,12.9194126862855,132.348873857722)) ;
#138234 = CARTESIAN_POINT('Ctrl Pts',(-14.3030031795231,13.1689179469772,
132.255840036165)) ;
#138235 = CARTESIAN_POINT('Ctrl Pts',(-14.2823169602156,13.4397285772897,
132.228764995968)) ;
#138236 = CARTESIAN_POINT('Ctrl Pts',(-14.2853193282304,13.7064270482981,
132.270516703463)) ;
#138237 = CARTESIAN_POINT('Ctrl Pts',(-14.3107446190627,13.9538862841149,
132.377905843498)) ;
#138238 = CARTESIAN_POINT('Ctrl Pts',(-14.3560623753014,14.1631927449857,
132.543351061516)) ;
#138239 = CARTESIAN_POINT('Ctrl Pts',(-14.4179193623701,14.3205261030357,
132.757382303374)) ;
#138240 = CARTESIAN_POINT('Ctrl Pts',(-14.4898754019086,14.4121066368491,
133.00052214106)) ;
#138241 = CARTESIAN_POINT('Ctrl Pts',(-14.5673432317612,14.4337042758691,
133.260027216362)) ;
#138242 = CARTESIAN_POINT('Ctrl Pts',(-14.6433126851901,14.3826278342729,
133.515059598052)) ;
#138243 = CARTESIAN_POINT('Ctrl Pts',(-14.711870574383,14.2628852897391,133.748467202197)) ;
#138244 = CARTESIAN_POINT('Ctrl Pts',(-14.767308001138,14.0829262304897,133.943544580163)) ;
#138245 = CARTESIAN_POINT('Ctrl Pts',(-14.804958064437,13.8556922728628,134.08666212542)) ;
#138246 = CARTESIAN_POINT('Ctrl Pts',(-14.821309401496,13.5972599907668,134.167584085587)) ;
#138247 = CARTESIAN_POINT('Ctrl Pts',(-14.8147006723657,13.3277680057125,
134.181252611574)) ;
#138248 = CARTESIAN_POINT('Ctrl Pts',(-14.7842864021737,13.0618110658261,
134.125814803658)) ;
#138249 = CARTESIAN_POINT('Ctrl Pts',(-14.7326708515057,12.8260390349159,
134.007850477343)) ;
#138250 = CARTESIAN_POINT('Ctrl Pts',(-14.6614620611927,12.6298697180506,
133.833098581207)) ;
#138251 = CARTESIAN_POINT('Ctrl Pts',(-14.575982707112,12.4917687928696,133.616467821938)) ;
#138252 = CARTESIAN_POINT('Ctrl Pts',(-14.4810796906638,12.4199839443985,
133.372411393608)) ;
#138253 = CARTESIAN_POINT('Ctrl Pts',(-14.383292851168,12.4203084099031,133.119842779795)) ;
#138254 = CARTESIAN_POINT('Ctrl Pts',(-14.2886705183159,12.4922084263286,
132.876515661936)) ;
#138255 = CARTESIAN_POINT('Ctrl Pts',(-14.203107613883,12.6309968831691,132.659710749856)) ;
#138256 = CARTESIAN_POINT('Ctrl Pts',(-14.1322473538398,12.8263310850707,
132.485816844473)) ;
#138257 = CARTESIAN_POINT('Ctrl Pts',(-14.0801877023912,13.0651227719104,
132.366942948258)) ;
#138258 = CARTESIAN_POINT('Ctrl Pts',(-14.0502840451506,13.3295667495973,
132.312773352509)) ;
#138259 = CARTESIAN_POINT('Ctrl Pts',(-14.0437510939769,13.5989123639349,
132.326651696683)) ;
#138260 = CARTESIAN_POINT('Ctrl Pts',(-14.0603102617504,13.8574710596154,
132.408219676378)) ;
#138261 = CARTESIAN_POINT('Ctrl Pts',(-14.0979300090043,14.0837078972677,
132.551132179434)) ;
#138262 = CARTESIAN_POINT('Ctrl Pts',(-14.1535518862661,14.2638191910291,
132.746822281892)) ;
#138263 = CARTESIAN_POINT('Ctrl Pts',(-14.2221618886066,14.3831695722174,
132.980371817265)) ;
#138264 = CARTESIAN_POINT('Ctrl Pts',(-14.2982848293422,14.4337176680091,
133.235911108826)) ;
#138265 = CARTESIAN_POINT('Ctrl Pts',(-14.3753145515019,14.4120588735212,
133.493942054439)) ;
#138266 = CARTESIAN_POINT('Ctrl Pts',(-14.4477414803192,14.3193773095664,
133.738707356022)) ;
#138267 = CARTESIAN_POINT('Ctrl Pts',(-14.5091083465657,14.1628171058123,
133.951066133343)) ;
#138268 = CARTESIAN_POINT('Ctrl Pts',(-14.5546602501446,13.9515916314902,
134.117466746109)) ;
#138269 = CARTESIAN_POINT('Ctrl Pts',(-14.5798144029916,13.705523326728,134.223839172995)) ;
#138270 = CARTESIAN_POINT('Ctrl Pts',(-14.5825811444736,13.4359481915904,
134.265260316511)) ;
#138271 = CARTESIAN_POINT('Ctrl Pts',(-14.5620507546937,13.169026252587,134.238153095214)) ;
#138272 = CARTESIAN_POINT('Ctrl Pts',(-14.5182618166179,12.916272819337,134.143645987583)) ;
#138273 = CARTESIAN_POINT('Ctrl Pts',(-14.4549186809599,12.7036779649805,
133.99146914691)) ;
#138274 = CARTESIAN_POINT('Ctrl Pts',(-14.374687848165,12.5403117624792,133.790249344614)) ;
#138275 = CARTESIAN_POINT('Ctrl Pts',(-14.2824989348909,12.4404489594076,
133.554219478518)) ;
#138276 = CARTESIAN_POINT('Ctrl Pts',(-14.1856763731449,12.4114485635984,
133.304313177069)) ;
#138277 = CARTESIAN_POINT('Ctrl Pts',(-14.0887755516816,12.4544846359496,
133.054413939327)) ;
#138278 = CARTESIAN_POINT('Ctrl Pts',(-13.998682567479,12.5672617568272,132.824403407284)) ;
#138279 = CARTESIAN_POINT('Ctrl Pts',(-13.9211585063749,12.7417744672769,
132.631137059237)) ;
#138280 = CARTESIAN_POINT('Ctrl Pts',(-13.8614037350289,12.9633750466865,
132.489527799616)) ;
#138281 = CARTESIAN_POINT('Ctrl Pts',(-13.8220394457413,13.2203111282886,
132.40782907511)) ;
#138282 = CARTESIAN_POINT('Ctrl Pts',(-13.8060358886469,13.4905143177326,
132.394191857521)) ;
#138283 = CARTESIAN_POINT('Ctrl Pts',(-13.8133099943821,13.755021596538,132.448448822965)) ;
#138284 = CARTESIAN_POINT('Ctrl Pts',(-13.8427459453627,13.9967495673617,
132.567564010889)) ;
#138285 = CARTESIAN_POINT('Ctrl Pts',(-13.8915602482871,14.1974242169902,
132.743295638543)) ;
#138286 = CARTESIAN_POINT('Ctrl Pts',(-13.9555090185762,14.3425139654286,
132.963240650371)) ;
#138287 = CARTESIAN_POINT('Ctrl Pts',(-14.0290714695679,14.4218015795288,
133.21118520583)) ;
#138288 = CARTESIAN_POINT('Ctrl Pts',(-14.1070493874014,14.4294553596466,
133.472292177633)) ;
#138289 = CARTESIAN_POINT('Ctrl Pts',(-14.181690309578,14.3652618643662,133.723279219976)) ;
#138290 = CARTESIAN_POINT('Ctrl Pts',(-14.2482705789536,14.2335997278837,
133.950926411238)) ;
#138291 = CARTESIAN_POINT('Ctrl Pts',(-14.3008003166485,14.043065952539,134.137599115662)) ;
#138292 = CARTESIAN_POINT('Ctrl Pts',(-14.334600453399,13.8093139342674,134.269381140691)) ;
#138293 = CARTESIAN_POINT('Ctrl Pts',(-14.3467469914,13.5459140316558,134.338166616757)) ;
#138294 = CARTESIAN_POINT('Ctrl Pts',(-14.3356273569063,13.2769104618193,
134.338576916924)) ;
#138295 = CARTESIAN_POINT('Ctrl Pts',(-14.3012529645766,13.0160047166174,
134.271353792998)) ;
#138296 = CARTESIAN_POINT('Ctrl Pts',(-14.2454215258121,12.7850162006338,
134.141350290204)) ;
#138297 = CARTESIAN_POINT('Ctrl Pts',(-14.1712185020009,12.5991696538989,
133.957766591908)) ;
#138298 = CARTESIAN_POINT('Ctrl Pts',(-14.083300535675,12.4727066988936,133.734115733787)) ;
#138299 = CARTESIAN_POINT('Ctrl Pts',(-13.9878279907723,12.4146340125785,
133.488219860348)) ;
#138300 = CARTESIAN_POINT('Ctrl Pts',(-13.8900938776437,12.4282724622725,
133.235826128764)) ;
#138301 = CARTESIAN_POINT('Ctrl Pts',(-13.7963885477012,12.5136821957653,
132.995310230063)) ;
#138302 = CARTESIAN_POINT('Ctrl Pts',(-13.7132720195936,12.6640313593757,
132.785624145284)) ;
#138303 = CARTESIAN_POINT('Ctrl Pts',(-13.645547905693,12.8694014058608,132.620995535521)) ;
#138304 = CARTESIAN_POINT('Ctrl Pts',(-13.5978347475723,13.1128473164404,
132.514595028059)) ;
#138305 = CARTESIAN_POINT('Ctrl Pts',(-13.5721656264375,13.3794713552814,
132.472736688106)) ;
#138306 = CARTESIAN_POINT('Ctrl Pts',(-13.5700232955001,13.6493875459495,
132.499624261885)) ;
#138307 = CARTESIAN_POINT('Ctrl Pts',(-13.5906979487209,13.9027716733404,
132.593113973492)) ;
#138308 = CARTESIAN_POINT('Ctrl Pts',(-13.6323003089401,14.1226003916879,
132.747892074304)) ;
#138309 = CARTESIAN_POINT('Ctrl Pts',(-13.6903176396252,14.2907614910249,
132.950296656493)) ;
#138310 = CARTESIAN_POINT('Ctrl Pts',(-13.76127060048,14.3985142710539,133.190934634915)) ;
#138311 = CARTESIAN_POINT('Ctrl Pts',(-13.8377932896785,14.4350393250775,
133.447491800336)) ;
#138312 = CARTESIAN_POINT('Ctrl Pts',(-13.9143676794725,14.400035592365,133.704198098061)) ;
#138313 = CARTESIAN_POINT('Ctrl Pts',(-13.9854510810604,14.2940192580209,
133.945170020293)) ;
#138314 = CARTESIAN_POINT('Ctrl Pts',(-14.0439573923053,14.1264036829356,
134.149121613712)) ;
#138315 = CARTESIAN_POINT('Ctrl Pts',(-14.0857782181044,13.9087136150407,
134.304358215958)) ;
#138316 = CARTESIAN_POINT('Ctrl Pts',(-14.1070694486661,13.6545233565068,
134.399835876429)) ;
#138317 = CARTESIAN_POINT('Ctrl Pts',(-14.1053844366646,13.3858501360358,
134.427920015331)) ;
#138318 = CARTESIAN_POINT('Ctrl Pts',(-14.0803367946603,13.11900556216,134.387865314787)) ;
#138319 = CARTESIAN_POINT('Ctrl Pts',(-14.0328788178783,12.8738785752154,
134.282346772143)) ;
#138320 = CARTESIAN_POINT('Ctrl Pts',(-13.9655106265573,12.6676054071639,
134.118751181152)) ;
#138321 = CARTESIAN_POINT('Ctrl Pts',(-13.8825856552335,12.516077131837,133.909646349396)) ;
#138322 = CARTESIAN_POINT('Ctrl Pts',(-13.7897110779122,12.4297444851197,
133.671323006778)) ;
#138323 = CARTESIAN_POINT('Ctrl Pts',(-13.6919754716078,12.4139325771417,
133.418938373948)) ;
#138324 = CARTESIAN_POINT('Ctrl Pts',(-13.5958285338883,12.4708186129552,
133.171266520997)) ;
#138325 = CARTESIAN_POINT('Ctrl Pts',(-13.5080655357658,12.5954480986012,
132.94792799004)) ;
#138326 = CARTESIAN_POINT('Ctrl Pts',(-13.4335244933812,12.7795462403225,
132.763308241075)) ;
#138327 = CARTESIAN_POINT('Ctrl Pts',(-13.3770299436409,13.0105017874409,
132.631490811353)) ;
#138328 = CARTESIAN_POINT('Ctrl Pts',(-13.3421556868852,13.2704658553687,
132.562743301802)) ;
#138329 = CARTESIAN_POINT('Ctrl Pts',(-13.3305220477458,13.5415024018121,
132.561910660489)) ;
#138330 = CARTESIAN_POINT('Ctrl Pts',(-13.3421066509126,13.8030869084645,
132.628769487748)) ;
#138331 = CARTESIAN_POINT('Ctrl Pts',(-13.3756345993665,14.0389746831751,
132.759952112845)) ;
#138332 = CARTESIAN_POINT('Ctrl Pts',(-13.4273915726418,14.2290323686529,
132.944092286592)) ;
#138333 = CARTESIAN_POINT('Ctrl Pts',(-13.4937472681949,14.3629000991712,
133.17115070044)) ;
#138334 = CARTESIAN_POINT('Ctrl Pts',(-13.5686675780257,14.4288302625026,
133.423124913234)) ;
#138335 = CARTESIAN_POINT('Ctrl Pts',(-13.6462332083306,14.422836536164,133.682844745829)) ;
#138336 = CARTESIAN_POINT('Ctrl Pts',(-13.7201301396068,14.3452102750607,
133.931839588516)) ;
#138337 = CARTESIAN_POINT('Ctrl Pts',(-13.7843830850645,14.2014203774082,
134.152682847936)) ;
#138338 = CARTESIAN_POINT('Ctrl Pts',(-13.8335217961475,14.002164262405,134.329317533484)) ;
#138339 = CARTESIAN_POINT('Ctrl Pts',(-13.8634889037809,13.7617532002817,
134.449925964223)) ;
#138340 = CARTESIAN_POINT('Ctrl Pts',(-13.8713352949717,13.4956080912223,
134.506099255839)) ;
#138341 = CARTESIAN_POINT('Ctrl Pts',(-13.8557782269919,13.2262846444733,
134.493650674134)) ;
#138342 = CARTESIAN_POINT('Ctrl Pts',(-13.8172322300386,12.9698877409975,
134.414183738046)) ;
#138343 = CARTESIAN_POINT('Ctrl Pts',(-13.7574812944028,12.7457364397051,
134.272830100964)) ;
#138344 = CARTESIAN_POINT('Ctrl Pts',(-13.6806317994049,12.5708017682082,
134.081378097011)) ;
#138345 = CARTESIAN_POINT('Ctrl Pts',(-13.5903919715778,12.456149717707,133.851080417193)) ;
#138346 = CARTESIAN_POINT('Ctrl Pts',(-13.4942558602785,12.4116404870963,
133.603177645582)) ;
#138347 = CARTESIAN_POINT('Ctrl Pts',(-13.3965419126512,12.4391729305521,
133.350956099842)) ;
#138348 = CARTESIAN_POINT('Ctrl Pts',(-13.3047832313469,12.5371797605548,
133.115969475029)) ;
#138349 = CARTESIAN_POINT('Ctrl Pts',(-13.224224637073,12.6985743465351,132.913751244712)) ;
#138350 = CARTESIAN_POINT('Ctrl Pts',(-13.1600523063441,12.9117741381151,
132.75938813857)) ;
#138351 = CARTESIAN_POINT('Ctrl Pts',(-13.1160389583248,13.1624013185224,
132.664019628854)) ;
#138352 = CARTESIAN_POINT('Ctrl Pts',(-13.0948693964311,13.430527916598,132.635227970366)) ;
#138353 = CARTESIAN_POINT('Ctrl Pts',(-13.0970891229502,13.6988963503242,
132.674862389402)) ;
#138354 = CARTESIAN_POINT('Ctrl Pts',(-13.1219243680964,13.9472005331235,
132.780524168488)) ;
#138355 = CARTESIAN_POINT('Ctrl Pts',(-13.1668095584822,14.1580510542122,
132.944759839031)) ;
#138356 = CARTESIAN_POINT('Ctrl Pts',(-13.2279893075256,14.3165352263592,
133.156667794039)) ;
#138357 = CARTESIAN_POINT('Ctrl Pts',(-13.300074213206,14.4105996600904,133.400356897989)) ;
#138358 = CARTESIAN_POINT('Ctrl Pts',(-13.3772745227853,14.4340684661328,
133.65898364802)) ;
#138359 = CARTESIAN_POINT('Ctrl Pts',(-13.4534960317781,14.3850544028617,
133.914807927191)) ;
#138360 = CARTESIAN_POINT('Ctrl Pts',(-13.5223409843892,14.2669952592305,
134.149060765162)) ;
#138361 = CARTESIAN_POINT('Ctrl Pts',(-13.5780776236805,14.08911548236,134.344922101581)) ;
#138362 = CARTESIAN_POINT('Ctrl Pts',(-13.6163713098489,13.8629229464963,
134.489949169064)) ;
#138363 = CARTESIAN_POINT('Ctrl Pts',(-13.6334000812586,13.604494449949,134.572926457528)) ;
#138364 = CARTESIAN_POINT('Ctrl Pts',(-13.6273628390361,13.3352196406284,
134.588252141428)) ;
#138365 = CARTESIAN_POINT('Ctrl Pts',(-13.5979289468704,13.0705830393377,
134.535442159946)) ;
#138366 = CARTESIAN_POINT('Ctrl Pts',(-13.5465441539597,12.8316693122143,
134.418434168296)) ;
#138367 = CARTESIAN_POINT('Ctrl Pts',(-13.4756744662724,12.6342706901117,
134.244688087508)) ;
#138368 = CARTESIAN_POINT('Ctrl Pts',(-13.3908617467319,12.4949548455415,
134.029880371869)) ;
#138369 = CARTESIAN_POINT('Ctrl Pts',(-13.2961267998515,12.421067631229,133.786322706496)) ;
#138370 = CARTESIAN_POINT('Ctrl Pts',(-13.1984664907621,12.4192534681359,
133.53408220403)) ;
#138371 = CARTESIAN_POINT('Ctrl Pts',(-13.1034923930835,12.4890550596445,
133.28977926538)) ;
#138372 = CARTESIAN_POINT('Ctrl Pts',(-13.017265404549,12.6269264793826,133.071181056084)) ;
#138373 = CARTESIAN_POINT('Ctrl Pts',(-12.9463889263436,12.8196494832229,
132.897028166528)) ;
#138374 = CARTESIAN_POINT('Ctrl Pts',(-12.8935445665423,13.0580835296679,
132.775965890197)) ;
#138375 = CARTESIAN_POINT('Ctrl Pts',(-12.8630605529485,13.321466149626,132.720020527257)) ;
#138376 = CARTESIAN_POINT('Ctrl Pts',(-12.8558430268871,13.5912986837364,
132.731956034601)) ;
#138377 = CARTESIAN_POINT('Ctrl Pts',(-12.8716409242927,13.8497218506693,
132.811188161045)) ;
#138378 = CARTESIAN_POINT('Ctrl Pts',(-12.9090128451689,14.0789422009193,
132.953652047894)) ;
#138379 = CARTESIAN_POINT('Ctrl Pts',(-12.9641549217213,14.2597600748466,
133.147850764733)) ;
#138380 = CARTESIAN_POINT('Ctrl Pts',(-13.0322170994182,14.3805241466999,
133.379686428977)) ;
#138381 = CARTESIAN_POINT('Ctrl Pts',(-13.1081075369044,14.4333051039602,
133.634503568026)) ;
#138382 = CARTESIAN_POINT('Ctrl Pts',(-13.1855018681886,14.4135763254968,
133.893739522478)) ;
#138383 = CARTESIAN_POINT('Ctrl Pts',(-13.2580501555575,14.3230160042054,
134.138797856071)) ;
#138384 = CARTESIAN_POINT('Ctrl Pts',(-13.3200141919047,14.1669880886898,
134.353077810686)) ;
#138385 = CARTESIAN_POINT('Ctrl Pts',(-13.3655273041903,13.9601855279978,
134.518891328518)) ;
#138386 = CARTESIAN_POINT('Ctrl Pts',(-13.39166667475,13.7121979850729,134.628542890827)) ;
#138387 = CARTESIAN_POINT('Ctrl Pts',(-13.3950941590884,13.44532544281,134.671581655692)) ;
#138388 = CARTESIAN_POINT('Ctrl Pts',(-13.3750645278574,13.1756579344581,
134.646260957203)) ;
#138389 = CARTESIAN_POINT('Ctrl Pts',(-13.3324016363677,12.9248371120238,
134.554668453737)) ;
#138390 = CARTESIAN_POINT('Ctrl Pts',(-13.2691521870421,12.7087904185415,
134.403066738095)) ;
#138391 = CARTESIAN_POINT('Ctrl Pts',(-13.189355166933,12.5441839960965,134.203071426488)) ;
#138392 = CARTESIAN_POINT('Ctrl Pts',(-13.0974574702678,12.4422953635853,
133.967886639172)) ;
#138393 = CARTESIAN_POINT('Ctrl Pts',(-13.0004980461265,12.4112745925655,
133.717648882006)) ;
#138394 = CARTESIAN_POINT('Ctrl Pts',(-12.9036891883039,12.4523611217467,
133.467956597446)) ;
#138395 = CARTESIAN_POINT('Ctrl Pts',(-12.8135499305002,12.5627156193445,
133.237713892736)) ;
#138396 = CARTESIAN_POINT('Ctrl Pts',(-12.7352975800842,12.736203215032,133.04244250152)) ;
#138397 = CARTESIAN_POINT('Ctrl Pts',(-12.6751129170403,12.9562236735918,
132.899511681536)) ;
#138398 = CARTESIAN_POINT('Ctrl Pts',(-12.6350705235841,13.212763202245,132.81587545549)) ;
#138399 = CARTESIAN_POINT('Ctrl Pts',(-12.618415408845,13.4814739437606,132.800169250016)) ;
#138400 = CARTESIAN_POINT('Ctrl Pts',(-12.624949611358,13.747602021364,132.852409321137)) ;
#138401 = CARTESIAN_POINT('Ctrl Pts',(-12.6539126495085,13.9907502143909,
132.970218060048)) ;
#138402 = CARTESIAN_POINT('Ctrl Pts',(-12.7021026429137,14.192126827699,133.144029351541)) ;
#138403 = CARTESIAN_POINT('Ctrl Pts',(-12.765596611934,14.3392030081547,133.362624554204)) ;
#138404 = CARTESIAN_POINT('Ctrl Pts',(-12.8395683339224,14.420750007367,133.612027485091)) ;
#138405 = CARTESIAN_POINT('Ctrl Pts',(-12.9167981216665,14.4302362672735,
133.870632857131)) ;
#138406 = CARTESIAN_POINT('Ctrl Pts',(-12.992010059953,14.3680283061645,134.123465509195)) ;
#138407 = CARTESIAN_POINT('Ctrl Pts',(-13.0589983401631,14.237554410734,134.352370279363)) ;
#138408 = CARTESIAN_POINT('Ctrl Pts',(-13.1118284099058,14.0487160493496,
134.539853291678)) ;
#138409 = CARTESIAN_POINT('Ctrl Pts',(-13.146070298649,13.8167884864147,134.672814185713)) ;
#138410 = CARTESIAN_POINT('Ctrl Pts',(-13.158940600161,13.5548285940714,134.743611055561)) ;
#138411 = CARTESIAN_POINT('Ctrl Pts',(-13.1485141240606,13.2844751401064,
134.74620797937)) ;
#138412 = CARTESIAN_POINT('Ctrl Pts',(-13.1146632560627,13.0226684871857,
134.680563192847)) ;
#138413 = CARTESIAN_POINT('Ctrl Pts',(-13.0595530042838,12.7913020649599,
134.552571784859)) ;
#138414 = CARTESIAN_POINT('Ctrl Pts',(-12.9859254140349,12.6040508049077,
134.370634704252)) ;
#138415 = CARTESIAN_POINT('Ctrl Pts',(-12.8984068250737,12.4756114262356,
134.148131473393)) ;
#138416 = CARTESIAN_POINT('Ctrl Pts',(-12.8027801955588,12.4152434956171,
133.901891080666)) ;
#138417 = CARTESIAN_POINT('Ctrl Pts',(-12.7050832331602,12.4269403592131,
133.649583880182)) ;
#138418 = CARTESIAN_POINT('Ctrl Pts',(-12.6113870773195,12.5099952735333,
133.409010819848)) ;
#138419 = CARTESIAN_POINT('Ctrl Pts',(-12.5277681815658,12.6587328614396,
133.19790502644)) ;
#138420 = CARTESIAN_POINT('Ctrl Pts',(-12.4597036669732,12.8618951640278,
133.03216961154)) ;
#138421 = CARTESIAN_POINT('Ctrl Pts',(-12.4110853088982,13.1054069389763,
132.923273357885)) ;
#138422 = CARTESIAN_POINT('Ctrl Pts',(-12.3847729703008,13.3721986649784,
132.879596342574)) ;
#138423 = CARTESIAN_POINT('Ctrl Pts',(-12.3819859406308,13.6415133850086,
132.904506589099)) ;
#138424 = CARTESIAN_POINT('Ctrl Pts',(-12.4019516425332,13.8954057097587,
132.995891115908)) ;
#138425 = CARTESIAN_POINT('Ctrl Pts',(-12.4430233781849,14.1169004603375,
133.149166980611)) ;
#138426 = CARTESIAN_POINT('Ctrl Pts',(-12.5007743421724,14.286862322143,133.350862259024)) ;
#138427 = CARTESIAN_POINT('Ctrl Pts',(-12.5710080643675,14.3960130352986,
133.589195796255)) ;
#138428 = CARTESIAN_POINT('Ctrl Pts',(-12.6477378354541,14.435114922765,133.846495972005)) ;
#138429 = CARTESIAN_POINT('Ctrl Pts',(-12.7245100764212,14.4019052021935,
134.103831117832)) ;
#138430 = CARTESIAN_POINT('Ctrl Pts',(-12.7956173758933,14.2983009170395,
134.344755254071)) ;
#138431 = CARTESIAN_POINT('Ctrl Pts',(-12.8547869888769,14.1317969214597,
134.550768714552)) ;
#138432 = CARTESIAN_POINT('Ctrl Pts',(-12.8970503379981,13.915343377283,134.707274446338)) ;
#138433 = CARTESIAN_POINT('Ctrl Pts',(-12.9189151717186,13.6633971798664,
134.804245408245)) ;
#138434 = CARTESIAN_POINT('Ctrl Pts',(-12.9180538654643,13.3943409624926,
134.83481321692)) ;
#138435 = CARTESIAN_POINT('Ctrl Pts',(-12.8935049395089,13.1257595222001,
134.796388178548)) ;
#138436 = CARTESIAN_POINT('Ctrl Pts',(-12.846763798285,12.880696500419,134.692848177627)) ;
#138437 = CARTESIAN_POINT('Ctrl Pts',(-12.7801601096525,12.6734734022958,
134.531398034018)) ;
#138438 = CARTESIAN_POINT('Ctrl Pts',(-12.697476922483,12.5195858406816,134.323074933688)) ;
#138439 = CARTESIAN_POINT('Ctrl Pts',(-12.6043494730584,12.4310932858069,
134.084172254176)) ;
#138440 = CARTESIAN_POINT('Ctrl Pts',(-12.5071674014279,12.4134132661188,
133.833228867129)) ;
#138441 = CARTESIAN_POINT('Ctrl Pts',(-12.4107585325106,12.468118840117,133.584832882078)) ;
#138442 = CARTESIAN_POINT('Ctrl Pts',(-12.322679446483,12.5909169061166,133.360570988226)) ;
#138443 = CARTESIAN_POINT('Ctrl Pts',(-12.2476924053518,12.773448841542,133.174646358778)) ;
#138444 = CARTESIAN_POINT('Ctrl Pts',(-12.1906716921723,13.0028153371377,
133.041232379228)) ;
#138445 = CARTESIAN_POINT('Ctrl Pts',(-12.1550824724469,13.2626811935882,
132.970465210837)) ;
#138446 = CARTESIAN_POINT('Ctrl Pts',(-12.1427326514074,13.5323090949329,
132.967368623297)) ;
#138447 = CARTESIAN_POINT('Ctrl Pts',(-12.1536928653571,13.7963542441069,
133.032649674846)) ;
#138448 = CARTESIAN_POINT('Ctrl Pts',(-12.186561825762,14.0324257207359,133.161790426664)) ;
#138449 = CARTESIAN_POINT('Ctrl Pts',(-12.237904814768,14.2243211070582,133.344781568927)) ;
#138450 = CARTESIAN_POINT('Ctrl Pts',(-12.3037435818566,14.3597396565784,
133.570240962877)) ;
#138451 = CARTESIAN_POINT('Ctrl Pts',(-12.3787469038738,14.4280132025405,
133.822575280817)) ;
#138452 = CARTESIAN_POINT('Ctrl Pts',(-12.4562812799884,14.424002708898,134.082180684632)) ;
#138453 = CARTESIAN_POINT('Ctrl Pts',(-12.5304216950177,14.3482149181964,
134.331918050498)) ;
#138454 = CARTESIAN_POINT('Ctrl Pts',(-12.5948207053285,14.2066839719766,
134.553078199398)) ;
#138455 = CARTESIAN_POINT('Ctrl Pts',(-12.6446347356738,14.0084845387879,
134.731769140596)) ;
#138456 = CARTESIAN_POINT('Ctrl Pts',(-12.675219666801,13.7679164068615,134.854314117452)) ;
#138457 = CARTESIAN_POINT('Ctrl Pts',(-12.6836312574652,13.5034894092934,
134.911972405466)) ;
#138458 = CARTESIAN_POINT('Ctrl Pts',(-12.6687474515576,13.2335994760701,
134.901547727802)) ;
#138459 = CARTESIAN_POINT('Ctrl Pts',(-12.6307771287539,12.9764076821957,
134.823780832756)) ;
#138460 = CARTESIAN_POINT('Ctrl Pts',(-12.5714387747411,12.7508792714819,
134.683681699463)) ;
#138461 = CARTESIAN_POINT('Ctrl Pts',(-12.495269711498,12.5752390770026,134.494092455625)) ;
#138462 = CARTESIAN_POINT('Ctrl Pts',(-12.4058116411776,12.4588915032614,
134.265916566441)) ;
#138463 = CARTESIAN_POINT('Ctrl Pts',(-12.3092343034192,12.4118138319928,
134.016919850756)) ;
#138464 = CARTESIAN_POINT('Ctrl Pts',(-12.2114871975486,12.4374481797596,
133.764590911581)) ;
#138465 = CARTESIAN_POINT('Ctrl Pts',(-12.1195045200242,12.5333386342992,
133.528936382898)) ;
#138466 = CARTESIAN_POINT('Ctrl Pts',(-12.0382298417102,12.693967439573,133.324775627438)) ;
#138467 = CARTESIAN_POINT('Ctrl Pts',(-11.9738864832373,12.9050030598073,
133.169754954227)) ;
#138468 = CARTESIAN_POINT('Ctrl Pts',(-11.9291410370529,13.1551457617761,
133.072300353404)) ;
#138469 = CARTESIAN_POINT('Ctrl Pts',(-11.9146402414172,13.3338156180663,
133.051979646352)) ;
#138470 = CARTESIAN_POINT('Ctrl Pts',(-11.9112544450943,13.4231220139207,
133.053109614684)) ;
#138471 = CARTESIAN_POINT('Ctrl Pts',(-33.254172394553,13.1734341962953,127.827509047315)) ;
#138472 = CARTESIAN_POINT('Ctrl Pts',(-33.2534688468502,13.1676985193225,
127.826184767787)) ;
#138473 = CARTESIAN_POINT('Ctrl Pts',(-33.2419952032343,13.0762043638356,
127.804349824282)) ;
#138474 = CARTESIAN_POINT('Ctrl Pts',(-33.211018017341,12.9034783486566,127.736832608067)) ;
#138475 = CARTESIAN_POINT('Ctrl Pts',(-33.1463422411098,12.6923998158235,
127.580920912699)) ;
#138476 = CARTESIAN_POINT('Ctrl Pts',(-33.065377068761,12.5327609203509,127.377507295976)) ;
#138477 = CARTESIAN_POINT('Ctrl Pts',(-32.9727193640174,12.4368205750072,
127.140104350878)) ;
#138478 = CARTESIAN_POINT('Ctrl Pts',(-32.8757794851729,12.4119420230158,
126.889847835464)) ;
#138479 = CARTESIAN_POINT('Ctrl Pts',(-32.7789533634292,12.4592681400663,
126.640220455885)) ;
#138480 = CARTESIAN_POINT('Ctrl Pts',(-32.6896764047084,12.5756590132109,
126.412512063749)) ;
#138481 = CARTESIAN_POINT('Ctrl Pts',(-32.6130980713007,12.7528353886377,
126.221951163832)) ;
#138482 = CARTESIAN_POINT('Ctrl Pts',(-32.5541688347234,12.9779971268721,
126.082927482414)) ;
#138483 = CARTESIAN_POINT('Ctrl Pts',(-32.516348854518,13.2349353999384,126.005559973369)) ;
#138484 = CARTESIAN_POINT('Ctrl Pts',(-32.5015321471705,13.505181868833,125.99536718027)) ;
#138485 = CARTESIAN_POINT('Ctrl Pts',(-32.510255245493,13.7710456278858,126.054139208809)) ;
#138486 = CARTESIAN_POINT('Ctrl Pts',(-32.5408455912521,14.0095405856191,
126.176462939078)) ;
#138487 = CARTESIAN_POINT('Ctrl Pts',(-32.590617752256,14.2073760437107,126.354989070221)) ;
#138488 = CARTESIAN_POINT('Ctrl Pts',(-32.6552393094493,14.348956944597,126.576879524749)) ;
#138489 = CARTESIAN_POINT('Ctrl Pts',(-32.7295619569501,14.4243647503837,
126.827206857336)) ;
#138490 = CARTESIAN_POINT('Ctrl Pts',(-32.8071231055973,14.4276726038888,
127.086902157256)) ;
#138491 = CARTESIAN_POINT('Ctrl Pts',(-32.8817223975628,14.359284576391,127.337895493878)) ;
#138492 = CARTESIAN_POINT('Ctrl Pts',(-32.9474949797647,14.2239082664501,
127.563137153005)) ;
#138493 = CARTESIAN_POINT('Ctrl Pts',(-32.999013802318,14.0309431435162,127.74678778598)) ;
#138494 = CARTESIAN_POINT('Ctrl Pts',(-33.0317243912484,13.7937232390813,
127.875568072026)) ;
#138495 = CARTESIAN_POINT('Ctrl Pts',(-33.0424700880379,13.531836984712,127.939937825762)) ;
#138496 = CARTESIAN_POINT('Ctrl Pts',(-33.0300282628962,13.2609088557136,
127.936734091393)) ;
#138497 = CARTESIAN_POINT('Ctrl Pts',(-32.994203922637,13.0011531405438,127.865290221919)) ;
#138498 = CARTESIAN_POINT('Ctrl Pts',(-32.9373619772109,12.7729627395585,
127.732251961769)) ;
#138499 = CARTESIAN_POINT('Ctrl Pts',(-32.8621917971211,12.590180168645,127.545858859501)) ;
#138500 = CARTESIAN_POINT('Ctrl Pts',(-32.7739701282575,12.4676467946536,
127.321209066395)) ;
#138501 = CARTESIAN_POINT('Ctrl Pts',(-32.6775709057836,12.4133145045735,
127.072830523477)) ;
#138502 = CARTESIAN_POINT('Ctrl Pts',(-32.5802381988428,12.4313808939379,
126.821499331578)) ;
#138503 = CARTESIAN_POINT('Ctrl Pts',(-32.4869911846938,12.5206603265203,
126.58231361496)) ;
#138504 = CARTESIAN_POINT('Ctrl Pts',(-32.4047353688031,12.6744195884329,
126.37511283223)) ;
#138505 = CARTESIAN_POINT('Ctrl Pts',(-32.338169138496,12.8815893082003,126.21375488428)) ;
#138506 = CARTESIAN_POINT('Ctrl Pts',(-32.2912803241275,13.1290193256912,
126.110059137956)) ;
#138507 = CARTESIAN_POINT('Ctrl Pts',(-32.267198005655,13.3950772370959,126.072668147979)) ;
#138508 = CARTESIAN_POINT('Ctrl Pts',(-32.2663142294123,13.664342206485,126.103200803217)) ;
#138509 = CARTESIAN_POINT('Ctrl Pts',(-32.2883903421483,13.9170737521182,
126.200907060451)) ;
#138510 = CARTESIAN_POINT('Ctrl Pts',(-32.3308821384472,14.1334228172292,
126.358124830198)) ;
#138511 = CARTESIAN_POINT('Ctrl Pts',(-32.3899729784829,14.2989215646412,
126.563802409089)) ;
#138512 = CARTESIAN_POINT('Ctrl Pts',(-32.4609168345964,14.402143447902,126.804164375536)) ;
#138513 = CARTESIAN_POINT('Ctrl Pts',(-32.5380332606012,14.4351203022994,
127.062647207067)) ;
#138514 = CARTESIAN_POINT('Ctrl Pts',(-32.6144820010754,14.3956460287634,
127.319015942137)) ;
#138515 = CARTESIAN_POINT('Ctrl Pts',(-32.6847316352454,14.2864256341772,
127.557403369739)) ;
#138516 = CARTESIAN_POINT('Ctrl Pts',(-32.7426623087253,14.1149876043022,
127.75980911474)) ;
#138517 = CARTESIAN_POINT('Ctrl Pts',(-32.7832798440404,13.8950778661998,
127.911480378731)) ;
#138518 = CARTESIAN_POINT('Ctrl Pts',(-32.8033292316642,13.6402949079638,
128.003230304667)) ;
#138519 = CARTESIAN_POINT('Ctrl Pts',(-32.8003337734113,13.3700135183461,
128.027639269137)) ;
#138520 = CARTESIAN_POINT('Ctrl Pts',(-32.773914625545,13.1040820554216,127.983559770344)) ;
#138521 = CARTESIAN_POINT('Ctrl Pts',(-32.7252938610734,12.8608603578453,
127.874624004567)) ;
#138522 = CARTESIAN_POINT('Ctrl Pts',(-32.6567428432369,12.6570995418072,
127.707633197288)) ;
#138523 = CARTESIAN_POINT('Ctrl Pts',(-32.5735389098173,12.5097125952048,
127.497535908456)) ;
#138524 = CARTESIAN_POINT('Ctrl Pts',(-32.4797522125056,12.4266925714705,
127.256729982278)) ;
#138525 = CARTESIAN_POINT('Ctrl Pts',(-32.3819584315157,12.4153566152999,
127.00416817041)) ;
#138526 = CARTESIAN_POINT('Ctrl Pts',(-32.2863523147031,12.4761183658278,
126.757991426057)) ;
#138527 = CARTESIAN_POINT('Ctrl Pts',(-32.1990413692234,12.604611036471,126.536036538651)) ;
#138528 = CARTESIAN_POINT('Ctrl Pts',(-32.1254036781347,12.7920329725734,
126.35408287723)) ;
#138529 = CARTESIAN_POINT('Ctrl Pts',(-32.0702238718563,13.0246460204259,
126.226026939548)) ;
#138530 = CARTESIAN_POINT('Ctrl Pts',(-32.0366919182254,13.2849676562724,
126.161110348471)) ;
#138531 = CARTESIAN_POINT('Ctrl Pts',(-32.026266023829,13.5561839498762,126.163818075152)) ;
#138532 = CARTESIAN_POINT('Ctrl Pts',(-32.0392886640995,13.8182130447303,
126.235079805905)) ;
#138533 = CARTESIAN_POINT('Ctrl Pts',(-32.0737307971117,14.0504674828932,
126.36870340205)) ;
#138534 = CARTESIAN_POINT('Ctrl Pts',(-32.1268661482956,14.2392688566164,
126.55716210234)) ;
#138535 = CARTESIAN_POINT('Ctrl Pts',(-32.1938216509952,14.3686949061628,
126.785894949115)) ;
#138536 = CARTESIAN_POINT('Ctrl Pts',(-32.2687100849035,14.4303698699092,
127.037630197794)) ;
#138537 = CARTESIAN_POINT('Ctrl Pts',(-32.3463747404381,14.4203874335836,
127.297695953386)) ;
#138538 = CARTESIAN_POINT('Ctrl Pts',(-32.4201156741376,14.3383234077631,
127.546348738078)) ;
#138539 = CARTESIAN_POINT('Ctrl Pts',(-32.4835082392893,14.1909246948651,
127.764639666828)) ;
#138540 = CARTESIAN_POINT('Ctrl Pts',(-32.5315157767965,13.9894771952072,
127.937873715533)) ;
#138541 = CARTESIAN_POINT('Ctrl Pts',(-32.5603116476677,13.746808334038,128.05511465854)) ;
#138542 = CARTESIAN_POINT('Ctrl Pts',(-32.5668625656013,13.4802543050363,
128.107448081919)) ;
#138543 = CARTESIAN_POINT('Ctrl Pts',(-32.5497368890375,13.2092850864011,
128.090661385991)) ;
#138544 = CARTESIAN_POINT('Ctrl Pts',(-32.510114480248,12.9563426654799,128.007794570266)) ;
#138545 = CARTESIAN_POINT('Ctrl Pts',(-32.4492538079865,12.7340442860679,
127.863247929968)) ;
#138546 = CARTESIAN_POINT('Ctrl Pts',(-32.3711351066077,12.5620254392794,
127.668219995262)) ;
#138547 = CARTESIAN_POINT('Ctrl Pts',(-32.281331276348,12.4521634534599,127.438836619194)) ;
#138548 = CARTESIAN_POINT('Ctrl Pts',(-32.1840100969233,12.411069828673,127.187814281084)) ;
#138549 = CARTESIAN_POINT('Ctrl Pts',(-32.0867350208807,12.4431134787165,
126.936774455973)) ;
#138550 = CARTESIAN_POINT('Ctrl Pts',(-31.9956180924333,12.544720782059,126.703612975735)) ;
#138551 = CARTESIAN_POINT('Ctrl Pts',(-31.9157829218615,12.7094608145556,
126.503527981435)) ;
#138552 = CARTESIAN_POINT('Ctrl Pts',(-31.8525238410862,12.9261933483464,
126.351960947211)) ;
#138553 = CARTESIAN_POINT('Ctrl Pts',(-31.8100237861107,13.176771832056,126.260796481775)) ;
#138554 = CARTESIAN_POINT('Ctrl Pts',(-31.7900313135677,13.4474343122789,
126.235698128778)) ;
#138555 = CARTESIAN_POINT('Ctrl Pts',(-31.7937452734304,13.7143157583518,
126.279598518457)) ;
#138556 = CARTESIAN_POINT('Ctrl Pts',(-31.8196615228194,13.9601208974721,
126.388299879067)) ;
#138557 = CARTESIAN_POINT('Ctrl Pts',(-31.865811538458,14.1691500345588,126.556373712908)) ;
#138558 = CARTESIAN_POINT('Ctrl Pts',(-31.9274739976856,14.3234012984993,
126.769521897676)) ;
#138559 = CARTESIAN_POINT('Ctrl Pts',(-32.0001208151247,14.4138714488527,
127.014915132275)) ;
#138560 = CARTESIAN_POINT('Ctrl Pts',(-32.0773542138778,14.4332950677581,
127.273601287544)) ;
#138561 = CARTESIAN_POINT('Ctrl Pts',(-32.1536561858525,14.3798376866145,
127.529813962779)) ;
#138562 = CARTESIAN_POINT('Ctrl Pts',(-32.2215753737412,14.2584887466458,
127.761209299702)) ;
#138563 = CARTESIAN_POINT('Ctrl Pts',(-32.2766035496271,14.0772214658074,
127.95508324656)) ;
#138564 = CARTESIAN_POINT('Ctrl Pts',(-32.3137764626411,13.8478580499734,
128.096937414159)) ;
#138565 = CARTESIAN_POINT('Ctrl Pts',(-32.329402655682,13.5896599466639,128.175623457458)) ;
#138566 = CARTESIAN_POINT('Ctrl Pts',(-32.3220622392593,13.3195389388511,
128.187229696327)) ;
#138567 = CARTESIAN_POINT('Ctrl Pts',(-32.2912364524646,13.0556170681804,
128.130382402966)) ;
#138568 = CARTESIAN_POINT('Ctrl Pts',(-32.2386415673211,12.818934352168,128.009823588916)) ;
#138569 = CARTESIAN_POINT('Ctrl Pts',(-32.1671306632537,12.6251003449816,
127.834066176529)) ;
#138570 = CARTESIAN_POINT('Ctrl Pts',(-32.0812904327446,12.4887479439426,
127.616396241464)) ;
#138571 = CARTESIAN_POINT('Ctrl Pts',(-31.9865273733683,12.4190670413713,
127.372638502282)) ;
#138572 = CARTESIAN_POINT('Ctrl Pts',(-31.8883365010758,12.4213699793115,
127.119029492639)) ;
#138573 = CARTESIAN_POINT('Ctrl Pts',(-31.7939808471855,12.4953802453317,
126.876454271148)) ;
#138574 = CARTESIAN_POINT('Ctrl Pts',(-31.7087526630847,12.6359572118525,
126.660632380682)) ;
#138575 = CARTESIAN_POINT('Ctrl Pts',(-31.638371937277,12.8329197331058,126.488156516072)) ;
#138576 = CARTESIAN_POINT('Ctrl Pts',(-31.587081585685,13.0719649791817,126.371428492643)) ;
#138577 = CARTESIAN_POINT('Ctrl Pts',(-31.5577681893857,13.3363497207088,
126.318926492673)) ;
#138578 = CARTESIAN_POINT('Ctrl Pts',(-31.5518637801405,13.6070576774105,
126.33481999986)) ;
#138579 = CARTESIAN_POINT('Ctrl Pts',(-31.5690715493904,13.8644611915849,
126.418217608229)) ;
#138580 = CARTESIAN_POINT('Ctrl Pts',(-31.6073534542258,14.0900773002825,
126.56314616954)) ;
#138581 = CARTESIAN_POINT('Ctrl Pts',(-31.6633899820247,14.2682172577694,
126.759999465483)) ;
#138582 = CARTESIAN_POINT('Ctrl Pts',(-31.7321264723496,14.385416608164,126.993843349614)) ;
#138583 = CARTESIAN_POINT('Ctrl Pts',(-31.8082726742393,14.4341663222017,
127.249410666497)) ;
#138584 = CARTESIAN_POINT('Ctrl Pts',(-31.8857066502997,14.4102121268538,
127.508823758604)) ;
#138585 = CARTESIAN_POINT('Ctrl Pts',(-31.957687983606,14.3156229092393,127.752193887258)) ;
#138586 = CARTESIAN_POINT('Ctrl Pts',(-32.0186786327333,14.157111727064,127.963488944682)) ;
#138587 = CARTESIAN_POINT('Ctrl Pts',(-32.0634925232266,13.9459764019392,
128.127527380573)) ;
#138588 = CARTESIAN_POINT('Ctrl Pts',(-32.0881992235517,13.6975622305703,
128.232806642455)) ;
#138589 = CARTESIAN_POINT('Ctrl Pts',(-32.0903191081306,13.4293975003276,
128.272118760355)) ;
#138590 = CARTESIAN_POINT('Ctrl Pts',(-32.0690179306767,13.1610019390536,
128.242981289226)) ;
#138591 = CARTESIAN_POINT('Ctrl Pts',(-32.0248932540369,12.910584846224,128.147279547823)) ;
#138592 = CARTESIAN_POINT('Ctrl Pts',(-31.960630679398,12.6976134707592,127.992652895403)) ;
#138593 = CARTESIAN_POINT('Ctrl Pts',(-31.8799759896631,12.536442281865,127.790164137919)) ;
#138594 = CARTESIAN_POINT('Ctrl Pts',(-31.788053718589,12.4387732267397,127.554739933416)) ;
#138595 = CARTESIAN_POINT('Ctrl Pts',(-31.6904186112103,12.4116342438423,
127.302714437302)) ;
#138596 = CARTESIAN_POINT('Ctrl Pts',(-31.5939692116319,12.4569142421678,
127.054018327164)) ;
#138597 = CARTESIAN_POINT('Ctrl Pts',(-31.5042485299717,12.5714751922183,
126.825069413096)) ;
#138598 = CARTESIAN_POINT('Ctrl Pts',(-31.4273555423138,12.7468633179545,
126.633538896743)) ;
#138599 = CARTESIAN_POINT('Ctrl Pts',(-31.367851407675,12.9706872906827,126.492823909801)) ;
#138600 = CARTESIAN_POINT('Ctrl Pts',(-31.3293429699657,13.2271705417113,
126.413473945479)) ;
#138601 = CARTESIAN_POINT('Ctrl Pts',(-31.3138511575412,13.4971329945125,
126.401288433693)) ;
#138602 = CARTESIAN_POINT('Ctrl Pts',(-31.3218793728741,13.7633005745665,
126.458013409239)) ;
#138603 = CARTESIAN_POINT('Ctrl Pts',(-31.3518046568443,14.0028268383939,
126.578386485857)) ;
#138604 = CARTESIAN_POINT('Ctrl Pts',(-31.4013169171817,14.2028677697453,
126.756297177419)) ;
#138605 = CARTESIAN_POINT('Ctrl Pts',(-31.4653538450798,14.3455611528234,
126.976348571448)) ;
#138606 = CARTESIAN_POINT('Ctrl Pts',(-31.5394673004167,14.4231516441217,
127.226068639417)) ;
#138607 = CARTESIAN_POINT('Ctrl Pts',(-31.6170364965111,14.428665737009,127.485791349647)) ;
#138608 = CARTESIAN_POINT('Ctrl Pts',(-31.6919586235444,14.3621069846461,
127.737801861754)) ;
#138609 = CARTESIAN_POINT('Ctrl Pts',(-31.7580050485926,14.2287343396627,
127.963800714979)) ;
#138610 = CARTESIAN_POINT('Ctrl Pts',(-31.8101229715983,14.0363061322534,
128.149332590931)) ;
#138611 = CARTESIAN_POINT('Ctrl Pts',(-31.8431612103325,13.8023697285695,
128.2787580194)) ;
#138612 = CARTESIAN_POINT('Ctrl Pts',(-31.8547450705058,13.5388532599518,
128.345858145807)) ;
#138613 = CARTESIAN_POINT('Ctrl Pts',(-31.842860978612,13.2684518599204,128.344212601708)) ;
#138614 = CARTESIAN_POINT('Ctrl Pts',(-31.8079018909361,13.0087997166185,
128.275192118151)) ;
#138615 = CARTESIAN_POINT('Ctrl Pts',(-31.751135231145,12.7778890822412,128.142629564991)) ;
#138616 = CARTESIAN_POINT('Ctrl Pts',(-31.67695004648,12.5950173960976,127.958860305201)) ;
#138617 = CARTESIAN_POINT('Ctrl Pts',(-31.5886131786522,12.4700325121189,
127.734044153826)) ;
#138618 = CARTESIAN_POINT('Ctrl Pts',(-31.4928932673828,12.4138573722268,
127.487454181968)) ;
#138619 = CARTESIAN_POINT('Ctrl Pts',(-31.3946517212827,12.4301864266095,
127.23377328525)) ;
#138620 = CARTESIAN_POINT('Ctrl Pts',(-31.302186280418,12.5166844150512,126.996510890305)) ;
#138621 = CARTESIAN_POINT('Ctrl Pts',(-31.2190229561058,12.6693064963876,
126.786854472266)) ;
#138622 = CARTESIAN_POINT('Ctrl Pts',(-31.1521847913265,12.8745471287187,
126.62458980109)) ;
#138623 = CARTESIAN_POINT('Ctrl Pts',(-31.1045636243091,13.1212023718215,
126.51878814528)) ;
#138624 = CARTESIAN_POINT('Ctrl Pts',(-31.0797814964469,13.3871939110425,
126.479383704405)) ;
#138625 = CARTESIAN_POINT('Ctrl Pts',(-31.0782395647314,13.6567281745513,
126.508004128684)) ;
#138626 = CARTESIAN_POINT('Ctrl Pts',(-31.0996004868119,13.9097854264049,
126.603554803648)) ;
#138627 = CARTESIAN_POINT('Ctrl Pts',(-31.1416644050721,14.1280196368697,
126.759621636509)) ;
#138628 = CARTESIAN_POINT('Ctrl Pts',(-31.2002751272883,14.2950456004005,
126.96385849581)) ;
#138629 = CARTESIAN_POINT('Ctrl Pts',(-31.2714095173753,14.4005267631623,
127.204975566894)) ;
#138630 = CARTESIAN_POINT('Ctrl Pts',(-31.3479251409683,14.4350836721885,
127.461472071147)) ;
#138631 = CARTESIAN_POINT('Ctrl Pts',(-31.4245699151336,14.397803897227,127.718459118213)) ;
#138632 = CARTESIAN_POINT('Ctrl Pts',(-31.4950050286166,14.2905756800978,
127.957348403359)) ;
#138633 = CARTESIAN_POINT('Ctrl Pts',(-31.5533719277229,14.1209511451637,
128.161017706247)) ;
#138634 = CARTESIAN_POINT('Ctrl Pts',(-31.5946288792335,13.9018371823522,
128.314620751464)) ;
#138635 = CARTESIAN_POINT('Ctrl Pts',(-31.6152556872759,13.6479071387663,
128.408037368887)) ;
#138636 = CARTESIAN_POINT('Ctrl Pts',(-31.6130251791501,13.378501800303,128.434595124285)) ;
#138637 = CARTESIAN_POINT('Ctrl Pts',(-31.5870806772977,13.1105161208594,
128.392113797471)) ;
#138638 = CARTESIAN_POINT('Ctrl Pts',(-31.5392287688349,12.8677236673919,
128.285256983731)) ;
#138639 = CARTESIAN_POINT('Ctrl Pts',(-31.4714257078563,12.662830762423,128.120378994299)) ;
#138640 = CARTESIAN_POINT('Ctrl Pts',(-31.3883963482576,12.513091865374,127.910882483852)) ;
#138641 = CARTESIAN_POINT('Ctrl Pts',(-31.2945615714775,12.4280189029097,
127.670021941709)) ;
#138642 = CARTESIAN_POINT('Ctrl Pts',(-31.1970838031679,12.4146728655739,
127.418286318199)) ;
#138643 = CARTESIAN_POINT('Ctrl Pts',(-31.1011085411165,12.473418288016,127.171104026254)) ;
#138644 = CARTESIAN_POINT('Ctrl Pts',(-31.0133901877585,12.6005220564223,
126.948009354706)) ;
#138645 = CARTESIAN_POINT('Ctrl Pts',(-30.9396697281207,12.7855011637684,
126.765646212268)) ;
#138646 = CARTESIAN_POINT('Ctrl Pts',(-30.8837990280299,13.0169860566136,
126.63558907916)) ;
#138647 = CARTESIAN_POINT('Ctrl Pts',(-30.849522212533,13.2774553414867,126.568584359704)) ;
#138648 = CARTESIAN_POINT('Ctrl Pts',(-30.8384800040019,13.5483711409958,
126.569459216869)) ;
#138649 = CARTESIAN_POINT('Ctrl Pts',(-30.8507215021823,13.8100859907312,
126.638320403832)) ;
#138650 = CARTESIAN_POINT('Ctrl Pts',(-30.8846778654308,14.0443620014337,
126.770654851182)) ;
#138651 = CARTESIAN_POINT('Ctrl Pts',(-30.9371383935864,14.2339606584883,
126.95701638284)) ;
#138652 = CARTESIAN_POINT('Ctrl Pts',(-31.0037048768907,14.3656339537851,
127.184617706613)) ;
#138653 = CARTESIAN_POINT('Ctrl Pts',(-31.0788096488771,14.4296685423803,
127.437147488283)) ;
#138654 = CARTESIAN_POINT('Ctrl Pts',(-31.1562803975842,14.4216217772437,
127.696556501827)) ;
#138655 = CARTESIAN_POINT('Ctrl Pts',(-31.2299712909159,14.3422174229119,
127.944936003485)) ;
#138656 = CARTESIAN_POINT('Ctrl Pts',(-31.294011633153,14.1963612940614,128.165233556202)) ;
#138657 = CARTESIAN_POINT('Ctrl Pts',(-31.342628260302,13.9958156297376,128.340321291151)) ;
#138658 = CARTESIAN_POINT('Ctrl Pts',(-31.3719914321145,13.7540871657713,
128.459213318105)) ;
#138659 = CARTESIAN_POINT('Ctrl Pts',(-31.379207947723,13.4887318093835,128.513395282888)) ;
#138660 = CARTESIAN_POINT('Ctrl Pts',(-31.3628630615942,13.2176490073036,
128.498882111054)) ;
#138661 = CARTESIAN_POINT('Ctrl Pts',(-31.32374522082,12.9629384302475,128.417620087759)) ;
#138662 = CARTESIAN_POINT('Ctrl Pts',(-31.2633013934625,12.739445641898,128.274321947507)) ;
#138663 = CARTESIAN_POINT('Ctrl Pts',(-31.1860840193193,12.5666312573546,
128.081740255708)) ;
#138664 = CARTESIAN_POINT('Ctrl Pts',(-31.0960617266757,12.4542159373709,
127.851907106863)) ;
#138665 = CARTESIAN_POINT('Ctrl Pts',(-30.9994012366927,12.4113528375642,
127.602620647228)) ;
#138666 = CARTESIAN_POINT('Ctrl Pts',(-30.9018203547689,12.4409689765868,
127.350762761079)) ;
#138667 = CARTESIAN_POINT('Ctrl Pts',(-30.8100561805039,12.5412370849313,
127.115855320823)) ;
#138668 = CARTESIAN_POINT('Ctrl Pts',(-30.7300852082415,12.7041353047709,
126.915290807566)) ;
#138669 = CARTESIAN_POINT('Ctrl Pts',(-30.6664814262111,12.9183855347654,
126.762561452756)) ;
#138670 = CARTESIAN_POINT('Ctrl Pts',(-30.6230851071898,13.1698655571926,
126.669003863828)) ;
#138671 = CARTESIAN_POINT('Ctrl Pts',(-30.6025564144617,13.4380609714907,
126.642060785656)) ;
#138672 = CARTESIAN_POINT('Ctrl Pts',(-30.6054938183217,13.7071666281258,
126.683923819577)) ;
#138673 = CARTESIAN_POINT('Ctrl Pts',(-30.630925020495,13.95380880599,126.791224928952)) ;
#138674 = CARTESIAN_POINT('Ctrl Pts',(-30.6763240529893,14.1634527040787,
126.956971615764)) ;
#138675 = CARTESIAN_POINT('Ctrl Pts',(-30.737907981033,14.3201289862677,127.170056594989)) ;
#138676 = CARTESIAN_POINT('Ctrl Pts',(-30.8100090399554,14.4121340944115,
127.413701128809)) ;
#138677 = CARTESIAN_POINT('Ctrl Pts',(-30.8874666938385,14.4336855937072,
127.673168883096)) ;
#138678 = CARTESIAN_POINT('Ctrl Pts',(-30.9634149457897,14.3827385924792,
127.928128807699)) ;
#138679 = CARTESIAN_POINT('Ctrl Pts',(-31.0321462262809,14.2627494461532,
128.162120074418)) ;
#138680 = CARTESIAN_POINT('Ctrl Pts',(-31.0876101736151,14.0822576993362,
128.357331855187)) ;
#138681 = CARTESIAN_POINT('Ctrl Pts',(-31.1250526967628,13.856193146146,128.499670462433)) ;
#138682 = CARTESIAN_POINT('Ctrl Pts',(-31.1415133894991,13.5974242111817,
128.580965284718)) ;
#138683 = CARTESIAN_POINT('Ctrl Pts',(-31.1348285122354,13.3273251704849,
128.594485415842)) ;
#138684 = CARTESIAN_POINT('Ctrl Pts',(-31.1045448692166,13.062291125414,128.539308802384)) ;
#138685 = CARTESIAN_POINT('Ctrl Pts',(-31.0527329307778,12.8256130125541,
128.420899764611)) ;
#138686 = CARTESIAN_POINT('Ctrl Pts',(-30.98174722609,12.6301798373562,128.246682571427)) ;
#138687 = CARTESIAN_POINT('Ctrl Pts',(-30.8962505494071,12.4918476261695,
128.030023021322)) ;
#138688 = CARTESIAN_POINT('Ctrl Pts',(-30.8012573749623,12.4199209769537,
127.785732954429)) ;
#138689 = CARTESIAN_POINT('Ctrl Pts',(-30.703212119019,12.4204246059211,127.53249886009)) ;
#138690 = CARTESIAN_POINT('Ctrl Pts',(-30.6089279234257,12.492159634428,127.290042373906)) ;
#138691 = CARTESIAN_POINT('Ctrl Pts',(-30.5232601554124,12.6310173484571,
127.072968873371)) ;
#138692 = CARTESIAN_POINT('Ctrl Pts',(-30.4524467312471,12.8262647723397,
126.899189775226)) ;
#138693 = CARTESIAN_POINT('Ctrl Pts',(-30.4004805626087,13.0646914718589,
126.780542586656)) ;
#138694 = CARTESIAN_POINT('Ctrl Pts',(-30.3705408361266,13.3278245014775,
126.72611222664)) ;
#138695 = CARTESIAN_POINT('Ctrl Pts',(-30.3639236278037,13.5998586000628,
126.740078803271)) ;
#138696 = CARTESIAN_POINT('Ctrl Pts',(-30.3804440847528,13.8569827516154,
126.821346278327)) ;
#138697 = CARTESIAN_POINT('Ctrl Pts',(-30.4182185553018,14.0842219381739,
126.964864025402)) ;
#138698 = CARTESIAN_POINT('Ctrl Pts',(-30.4735865343095,14.2634336188574,
127.159646811296)) ;
#138699 = CARTESIAN_POINT('Ctrl Pts',(-30.5424536748966,14.3833954818559,
127.39408651496)) ;
#138700 = CARTESIAN_POINT('Ctrl Pts',(-30.6185595912135,14.433698045123,127.6495579438)) ;
#138701 = CARTESIAN_POINT('Ctrl Pts',(-30.6955385718699,14.412015772317,127.90742294184)) ;
#138702 = CARTESIAN_POINT('Ctrl Pts',(-30.7679798384188,14.319294669833,128.152234187299)) ;
#138703 = CARTESIAN_POINT('Ctrl Pts',(-30.829320400999,14.16255830471,128.364526767623)) ;
#138704 = CARTESIAN_POINT('Ctrl Pts',(-30.8747794144243,13.9521768757504,
128.530537740434)) ;
#138705 = CARTESIAN_POINT('Ctrl Pts',(-30.9000057378481,13.7045477413862,
128.637327125319)) ;
#138706 = CARTESIAN_POINT('Ctrl Pts',(-30.9028301887914,13.4377490344594,
128.678565653954)) ;
#138707 = CARTESIAN_POINT('Ctrl Pts',(-30.8820826030584,13.1678476271901,
128.651204751086)) ;
#138708 = CARTESIAN_POINT('Ctrl Pts',(-30.8387479936137,12.917659013908,128.55767070028)) ;
#138709 = CARTESIAN_POINT('Ctrl Pts',(-30.7747422547336,12.7025601696351,
128.403936479543)) ;
#138710 = CARTESIAN_POINT('Ctrl Pts',(-30.6948870245618,12.5405894739967,
128.203610760336)) ;
#138711 = CARTESIAN_POINT('Ctrl Pts',(-30.6029778904066,12.4405287595892,
127.968321122167)) ;
#138712 = CARTESIAN_POINT('Ctrl Pts',(-30.5054387564785,12.4114132283242,
127.716562065288)) ;
#138713 = CARTESIAN_POINT('Ctrl Pts',(-30.4089272864758,12.4546443819082,
127.467672427643)) ;
#138714 = CARTESIAN_POINT('Ctrl Pts',(-30.3190828257142,12.5668919742526,
127.238290564815)) ;
#138715 = CARTESIAN_POINT('Ctrl Pts',(-30.241370659299,12.7415276223377,127.044530125261)) ;
#138716 = CARTESIAN_POINT('Ctrl Pts',(-30.1814937744117,12.963899300171,126.902662765778)) ;
#138717 = CARTESIAN_POINT('Ctrl Pts',(-30.1423835997439,13.2191082670462,
126.821485055972)) ;
#138718 = CARTESIAN_POINT('Ctrl Pts',(-30.1261920888456,13.4893534858843,
126.807309521278)) ;
#138719 = CARTESIAN_POINT('Ctrl Pts',(-30.1334829442477,13.7553188833262,
126.861793756427)) ;
#138720 = CARTESIAN_POINT('Ctrl Pts',(-30.1629779883077,13.9971251681561,
126.981096376392)) ;
#138721 = CARTESIAN_POINT('Ctrl Pts',(-30.2118917393662,14.1977811573069,
127.157151224366)) ;
#138722 = CARTESIAN_POINT('Ctrl Pts',(-30.2755695825853,14.3424510805747,
127.37616964476)) ;
#138723 = CARTESIAN_POINT('Ctrl Pts',(-30.3497741256928,14.4220642873528,
127.6262727592)) ;
#138724 = CARTESIAN_POINT('Ctrl Pts',(-30.4269392595461,14.429449097017,127.884649436958)) ;
#138725 = CARTESIAN_POINT('Ctrl Pts',(-30.5019897574921,14.3652072331767,
128.137012614321)) ;
#138726 = CARTESIAN_POINT('Ctrl Pts',(-30.5684475923327,14.2335291681656,
128.364251880874)) ;
#138727 = CARTESIAN_POINT('Ctrl Pts',(-30.6210233478071,14.0429179829767,
128.551080403811)) ;
#138728 = CARTESIAN_POINT('Ctrl Pts',(-30.6547155048059,13.8093220415122,
128.682513972031)) ;
#138729 = CARTESIAN_POINT('Ctrl Pts',(-30.6669672711903,13.5476217971459,
128.751402838105)) ;
#138730 = CARTESIAN_POINT('Ctrl Pts',(-30.655673207762,13.2750711815888,128.751743570291)) ;
#138731 = CARTESIAN_POINT('Ctrl Pts',(-30.6214425269047,13.0163164213971,
128.684671616842)) ;
#138732 = CARTESIAN_POINT('Ctrl Pts',(-30.5654915322016,12.7846451556795,
128.554417669839)) ;
#138733 = CARTESIAN_POINT('Ctrl Pts',(-30.4915451337098,12.5995256384001,
128.371457049536)) ;
#138734 = CARTESIAN_POINT('Ctrl Pts',(-30.4034941667108,12.4726551517152,
128.14748281173)) ;
#138735 = CARTESIAN_POINT('Ctrl Pts',(-30.3078437177502,12.4145513421249,
127.901121998884)) ;
#138736 = CARTESIAN_POINT('Ctrl Pts',(-30.210077288083,12.4284690605263,127.648651011996)) ;
#138737 = CARTESIAN_POINT('Ctrl Pts',(-30.1167874583968,12.5133431684666,
127.409191485807)) ;
#138738 = CARTESIAN_POINT('Ctrl Pts',(-30.0333107867574,12.6644367182662,
127.198609743159)) ;
#138739 = CARTESIAN_POINT('Ctrl Pts',(-29.9660994199644,12.8679925564765,
127.035199525246)) ;
#138740 = CARTESIAN_POINT('Ctrl Pts',(-29.9179046187407,13.1131690365504,
126.927653178102)) ;
#138741 = CARTESIAN_POINT('Ctrl Pts',(-29.8923276220366,13.3800002802051,
126.886075570865)) ;
#138742 = CARTESIAN_POINT('Ctrl Pts',(-29.890221558393,13.6495651704166,126.913031740464)) ;
#138743 = CARTESIAN_POINT('Ctrl Pts',(-29.9108230270758,13.9023388943094,
127.006224631618)) ;
#138744 = CARTESIAN_POINT('Ctrl Pts',(-29.9524567704631,14.1226577783971,
127.161152165549)) ;
#138745 = CARTESIAN_POINT('Ctrl Pts',(-30.0105822434621,14.2908247544057,
127.363910457664)) ;
#138746 = CARTESIAN_POINT('Ctrl Pts',(-30.0810607522141,14.3981040604,127.602953490958)) ;
#138747 = CARTESIAN_POINT('Ctrl Pts',(-30.1580346362768,14.4352626925802,
127.861027386541)) ;
#138748 = CARTESIAN_POINT('Ctrl Pts',(-30.2348501197493,14.3995540245642,
128.118555932153)) ;
#138749 = CARTESIAN_POINT('Ctrl Pts',(-30.3051990221144,14.2948938638273,
128.357020944154)) ;
#138750 = CARTESIAN_POINT('Ctrl Pts',(-30.3643203908641,14.125950965529,128.563084862304)) ;
#138751 = CARTESIAN_POINT('Ctrl Pts',(-30.4059231271862,13.9085226432365,
128.717598399571)) ;
#138752 = CARTESIAN_POINT('Ctrl Pts',(-30.4271781973549,13.655740461518,128.812805228058)) ;
#138753 = CARTESIAN_POINT('Ctrl Pts',(-30.425651180432,13.3866405451627,128.841404541009)) ;
#138754 = CARTESIAN_POINT('Ctrl Pts',(-30.400385551166,13.1181024213027,128.800927702681)) ;
#138755 = CARTESIAN_POINT('Ctrl Pts',(-30.3531378768886,12.8743682814219,
128.695842135408)) ;
#138756 = CARTESIAN_POINT('Ctrl Pts',(-30.2858450507144,12.6679957327003,
128.532463254719)) ;
#138757 = CARTESIAN_POINT('Ctrl Pts',(-30.2030436364601,12.5164144034558,
128.323684166742)) ;
#138758 = CARTESIAN_POINT('Ctrl Pts',(-30.1097735403851,12.4295970264179,
128.08434965657)) ;
#138759 = CARTESIAN_POINT('Ctrl Pts',(-30.0120243335714,12.4140261333183,
127.831928581667)) ;
#138760 = CARTESIAN_POINT('Ctrl Pts',(-29.9160583223097,12.4707103278581,
127.584718425012)) ;
#138761 = CARTESIAN_POINT('Ctrl Pts',(-29.8280269609598,12.5959068144279,
127.360711064938)) ;
#138762 = CARTESIAN_POINT('Ctrl Pts',(-29.7538191838626,12.7791142632462,
127.176904989675)) ;
#138763 = CARTESIAN_POINT('Ctrl Pts',(-29.6970483927431,13.0114293123004,
127.044472850966)) ;
#138764 = CARTESIAN_POINT('Ctrl Pts',(-29.6625029707419,13.2689899400059,
126.976374860837)) ;
#138765 = CARTESIAN_POINT('Ctrl Pts',(-29.6506529182366,13.5409257328685,
126.975025452337)) ;
#138766 = CARTESIAN_POINT('Ctrl Pts',(-29.6622871843877,13.8029840857302,
127.0420891238)) ;
#138767 = CARTESIAN_POINT('Ctrl Pts',(-29.6957058732804,14.0385608749257,
127.17289415219)) ;
#138768 = CARTESIAN_POINT('Ctrl Pts',(-29.7477029788471,14.2294231057281,
127.357883843032)) ;
#138769 = CARTESIAN_POINT('Ctrl Pts',(-29.8138291653475,14.3627051490732,
127.584145435595)) ;
#138770 = CARTESIAN_POINT('Ctrl Pts',(-29.8888069040326,14.428833416405,127.836321972772)) ;
#138771 = CARTESIAN_POINT('Ctrl Pts',(-29.9663255096702,14.4228924472986,
128.095881765559)) ;
#138772 = CARTESIAN_POINT('Ctrl Pts',(-30.0404179941072,14.3451234315922,
128.345531442974)) ;
#138773 = CARTESIAN_POINT('Ctrl Pts',(-30.1046981850006,14.2008972781255,
128.566497642975)) ;
#138774 = CARTESIAN_POINT('Ctrl Pts',(-30.1536677639362,14.0023960154245,
128.742513477709)) ;
#138775 = CARTESIAN_POINT('Ctrl Pts',(-30.1836978229632,13.761031796391,128.863433474315)) ;
#138776 = CARTESIAN_POINT('Ctrl Pts',(-30.1915169666826,13.4967569826491,
128.919290575306)) ;
#138777 = CARTESIAN_POINT('Ctrl Pts',(-30.1759417647318,13.2257685669237,
128.906995280774)) ;
#138778 = CARTESIAN_POINT('Ctrl Pts',(-30.1373175281481,12.9695426329055,
128.827285395953)) ;
#138779 = CARTESIAN_POINT('Ctrl Pts',(-30.0776169751352,12.7456271817385,
128.686048533487)) ;
#138780 = CARTESIAN_POINT('Ctrl Pts',(-30.0008439016691,12.5709695365104,
128.494781054778)) ;
#138781 = CARTESIAN_POINT('Ctrl Pts',(-29.9109937297079,12.4565179124428,
128.265492257497)) ;
#138782 = CARTESIAN_POINT('Ctrl Pts',(-29.8144178586128,12.411477377022,128.016458751721)) ;
#138783 = CARTESIAN_POINT('Ctrl Pts',(-29.7164129546977,12.4394645473503,
127.763492166737)) ;
#138784 = CARTESIAN_POINT('Ctrl Pts',(-29.625114422541,12.5368907011572,127.52967566749)) ;
#138785 = CARTESIAN_POINT('Ctrl Pts',(-29.5440581310289,12.6994727139768,
127.326227681724)) ;
#138786 = CARTESIAN_POINT('Ctrl Pts',(-29.4803519777916,12.9112843857967,
127.172992697851)) ;
#138787 = CARTESIAN_POINT('Ctrl Pts',(-29.4360704062874,13.1634090116609,
127.077046478387)) ;
#138788 = CARTESIAN_POINT('Ctrl Pts',(-29.4151050777489,13.4300956070728,
127.048666359922)) ;
#138789 = CARTESIAN_POINT('Ctrl Pts',(-29.4172038600174,13.698548706025,127.087953020284)) ;
#138790 = CARTESIAN_POINT('Ctrl Pts',(-29.4422283626999,13.948024671753,127.194334375548)) ;
#138791 = CARTESIAN_POINT('Ctrl Pts',(-29.4869173656092,14.1576527891806,
127.357820579509)) ;
#138792 = CARTESIAN_POINT('Ctrl Pts',(-29.54801221472,14.3162850237807,127.569468256761)) ;
#138793 = CARTESIAN_POINT('Ctrl Pts',(-29.6202346404057,14.4106899925297,
127.813623734569)) ;
#138794 = CARTESIAN_POINT('Ctrl Pts',(-29.6976609528792,14.4339585114454,
128.073008187915)) ;
#138795 = CARTESIAN_POINT('Ctrl Pts',(-29.7734049144381,14.3853107611265,
128.327226370468)) ;
#138796 = CARTESIAN_POINT('Ctrl Pts',(-29.8426107800081,14.2669554182004,
128.562689628014)) ;
#138797 = CARTESIAN_POINT('Ctrl Pts',(-29.8984038160143,14.0883945818005,
128.758789145186)) ;
#138798 = CARTESIAN_POINT('Ctrl Pts',(-29.9364668210969,13.8631867563802,
128.902988584739)) ;
#138799 = CARTESIAN_POINT('Ctrl Pts',(-29.9535661140654,13.6057120624757,
128.986065149413)) ;
#138800 = CARTESIAN_POINT('Ctrl Pts',(-29.9475514809259,13.3350528446723,
129.001627031904)) ;
#138801 = CARTESIAN_POINT('Ctrl Pts',(-29.9181077464122,13.0707553542234,
128.948747970018)) ;
#138802 = CARTESIAN_POINT('Ctrl Pts',(-29.8668527383469,12.8321486706852,
128.832067893954)) ;
#138803 = CARTESIAN_POINT('Ctrl Pts',(-29.7959514293353,12.634462986152,128.658259481005)) ;
#138804 = CARTESIAN_POINT('Ctrl Pts',(-29.7111770706639,12.4951761871636,
128.443552553311)) ;
#138805 = CARTESIAN_POINT('Ctrl Pts',(-29.6165727185072,12.4210996152358,
128.200337064967)) ;
#138806 = CARTESIAN_POINT('Ctrl Pts',(-29.5184173364358,12.4192964203799,
127.946818896369)) ;
#138807 = CARTESIAN_POINT('Ctrl Pts',(-29.4237333839853,12.4890492296412,
127.703265098707)) ;
#138808 = CARTESIAN_POINT('Ctrl Pts',(-29.3374665646916,12.6268326997912,
127.48455927018)) ;
#138809 = CARTESIAN_POINT('Ctrl Pts',(-29.2666068879605,12.8195830933143,
127.310453192169)) ;
#138810 = CARTESIAN_POINT('Ctrl Pts',(-29.2139088518931,13.0571002340723,
127.189701884794)) ;
#138811 = CARTESIAN_POINT('Ctrl Pts',(-29.1832978923029,13.3202805814274,
127.133374035993)) ;
#138812 = CARTESIAN_POINT('Ctrl Pts',(-29.1759731508813,13.5914916661993,
127.145159393094)) ;
#138813 = CARTESIAN_POINT('Ctrl Pts',(-29.1919413561174,13.850556640903,127.224987369683)) ;
#138814 = CARTESIAN_POINT('Ctrl Pts',(-29.2289910736229,14.0777829295082,
127.366223885127)) ;
#138815 = CARTESIAN_POINT('Ctrl Pts',(-29.2839846556262,14.2590886329476,
127.559987926514)) ;
#138816 = CARTESIAN_POINT('Ctrl Pts',(-29.3524816976542,14.3807166913486,
127.79330782417)) ;
#138817 = CARTESIAN_POINT('Ctrl Pts',(-29.4283854204452,14.433343612586,128.048161723033)) ;
#138818 = CARTESIAN_POINT('Ctrl Pts',(-29.5059240605093,14.4133893592863,
128.307883829415)) ;
#138819 = CARTESIAN_POINT('Ctrl Pts',(-29.5781203155356,14.3229978195751,
128.551770260296)) ;
#138820 = CARTESIAN_POINT('Ctrl Pts',(-29.6399314292429,14.1680350137977,
128.765464698261)) ;
#138821 = CARTESIAN_POINT('Ctrl Pts',(-29.685826677058,13.9594347962821,128.932682676008)) ;
#138822 = CARTESIAN_POINT('Ctrl Pts',(-29.7118119049308,13.7128291828127,
129.041685973137)) ;
#138823 = CARTESIAN_POINT('Ctrl Pts',(-29.7152244342629,13.4442543360426,
129.084901531975)) ;
#138824 = CARTESIAN_POINT('Ctrl Pts',(-29.6953684239956,13.1766944104108,
129.059817600421)) ;
#138825 = CARTESIAN_POINT('Ctrl Pts',(-29.6523051959867,12.9234094695572,
128.967384298863)) ;
#138826 = CARTESIAN_POINT('Ctrl Pts',(-29.5891931535503,12.7086523153548,
128.816031681833)) ;
#138827 = CARTESIAN_POINT('Ctrl Pts',(-29.5096878148105,12.5444332786266,
128.616788035257)) ;
#138828 = CARTESIAN_POINT('Ctrl Pts',(-29.4176707271872,12.4422654276919,
128.381300524419)) ;
#138829 = CARTESIAN_POINT('Ctrl Pts',(-29.3206187587525,12.4113238218205,
128.13082546281)) ;
#138830 = CARTESIAN_POINT('Ctrl Pts',(-29.2239159231989,12.4521999821779,
127.881398011169)) ;
#138831 = CARTESIAN_POINT('Ctrl Pts',(-29.1332913036832,12.5635389919688,
127.649940033755)) ;
#138832 = CARTESIAN_POINT('Ctrl Pts',(-29.0557674545012,12.7354102649258,
127.456478979614)) ;
#138833 = CARTESIAN_POINT('Ctrl Pts',(-28.9951475479058,12.9568498172893,
127.312508336806)) ;
#138834 = CARTESIAN_POINT('Ctrl Pts',(-28.9553615529616,13.2117694586679,
127.229401671249)) ;
#138835 = CARTESIAN_POINT('Ctrl Pts',(-28.9385143715075,13.4825284922973,
127.213391239786)) ;
#138836 = CARTESIAN_POINT('Ctrl Pts',(-28.9452357718578,13.7484828909248,
127.266167041443)) ;
#138837 = CARTESIAN_POINT('Ctrl Pts',(-28.973991992575,13.9900671084782,127.383159255252)) ;
#138838 = CARTESIAN_POINT('Ctrl Pts',(-29.0222446858003,14.1922209027102,
127.557244848018)) ;
#138839 = CARTESIAN_POINT('Ctrl Pts',(-29.0859598821377,14.3393855403521,
127.776572340874)) ;
#138840 = CARTESIAN_POINT('Ctrl Pts',(-29.1593133178373,14.4204077329138,
128.023897295284)) ;
#138841 = CARTESIAN_POINT('Ctrl Pts',(-29.23685478466,14.4304302154213,128.283550561485)) ;
#138842 = CARTESIAN_POINT('Ctrl Pts',(-29.312289340566,14.367871152587,128.537132753714)) ;
#138843 = CARTESIAN_POINT('Ctrl Pts',(-29.3790948094322,14.2376927603017,
128.765418469869)) ;
#138844 = CARTESIAN_POINT('Ctrl Pts',(-29.4319637198198,14.0489883287211,
128.953014743318)) ;
#138845 = CARTESIAN_POINT('Ctrl Pts',(-29.4663009452838,13.8164456424353,
129.086339965454)) ;
#138846 = CARTESIAN_POINT('Ctrl Pts',(-29.4791076386463,13.5541089152985,
129.156990353639)) ;
#138847 = CARTESIAN_POINT('Ctrl Pts',(-29.4686796127963,13.2846772722545,
129.159471786986)) ;
#138848 = CARTESIAN_POINT('Ctrl Pts',(-29.4349222155091,13.0230235410346,
129.094073521591)) ;
#138849 = CARTESIAN_POINT('Ctrl Pts',(-29.3796180661493,12.790872732509,128.965627833144)) ;
#138850 = CARTESIAN_POINT('Ctrl Pts',(-29.3059833398163,12.603871831162,128.783651650281)) ;
#138851 = CARTESIAN_POINT('Ctrl Pts',(-29.2185690761389,12.4755978216217,
128.561414059103)) ;
#138852 = CARTESIAN_POINT('Ctrl Pts',(-29.122841974274,12.4151865443115,128.31491351705)) ;
#138853 = CARTESIAN_POINT('Ctrl Pts',(-29.0251621540499,12.4270410572104,
128.062652651585)) ;
#138854 = CARTESIAN_POINT('Ctrl Pts',(-28.9316571387812,12.5098502555296,
127.822566531605)) ;
#138855 = CARTESIAN_POINT('Ctrl Pts',(-28.847833803276,12.6589866002263,127.610948437538)) ;
#138856 = CARTESIAN_POINT('Ctrl Pts',(-28.7799886758662,12.8615686944882,
127.445752679704)) ;
#138857 = CARTESIAN_POINT('Ctrl Pts',(-28.7313057367753,13.1050266274507,
127.336673069078)) ;
#138858 = CARTESIAN_POINT('Ctrl Pts',(-28.7049815446916,13.3718443687466,
127.292967742919)) ;
#138859 = CARTESIAN_POINT('Ctrl Pts',(-28.7020980093711,13.6411904118671,
127.317589764157)) ;
#138860 = CARTESIAN_POINT('Ctrl Pts',(-28.7223401648118,13.8968634944342,
127.41003902009)) ;
#138861 = CARTESIAN_POINT('Ctrl Pts',(-28.7629973543961,14.1159779670334,
127.561745464258)) ;
#138862 = CARTESIAN_POINT('Ctrl Pts',(-28.8210947372898,14.287325697854,127.764689801619)) ;
#138863 = CARTESIAN_POINT('Ctrl Pts',(-28.8911765229029,14.3958947367542,
128.002481753305)) ;
#138864 = CARTESIAN_POINT('Ctrl Pts',(-28.9677972904603,14.4351265100489,
128.259425785411)) ;
#138865 = CARTESIAN_POINT('Ctrl Pts',(-29.0446691431128,14.401957868372,128.517089841033)) ;
#138866 = CARTESIAN_POINT('Ctrl Pts',(-29.1157706503648,14.2982652104899,
128.758002104881)) ;
#138867 = CARTESIAN_POINT('Ctrl Pts',(-29.174779918269,14.132480207139,128.96343389952)) ;
#138868 = CARTESIAN_POINT('Ctrl Pts',(-29.2172302832933,13.915462827869,129.120592596423)) ;
#138869 = CARTESIAN_POINT('Ctrl Pts',(-29.2390983208705,13.6633712465324,
129.217586381667)) ;
#138870 = CARTESIAN_POINT('Ctrl Pts',(-29.2382024002942,13.3940849462189,
129.248083384228)) ;
#138871 = CARTESIAN_POINT('Ctrl Pts',(-29.2137553366703,13.1263052775463,
129.209852895038)) ;
#138872 = CARTESIAN_POINT('Ctrl Pts',(-29.1668939996439,12.8804158751522,
129.106068734867)) ;
#138873 = CARTESIAN_POINT('Ctrl Pts',(-29.1002691947144,12.6733662983206,
128.944544491779)) ;
#138874 = CARTESIAN_POINT('Ctrl Pts',(-29.0177318506309,12.5197379232373,
128.736592399109)) ;
#138875 = CARTESIAN_POINT('Ctrl Pts',(-28.9246399778716,12.4310982173194,
128.497785172193)) ;
#138876 = CARTESIAN_POINT('Ctrl Pts',(-28.8272015701286,12.4134628281618,
128.246181903058)) ;
#138877 = CARTESIAN_POINT('Ctrl Pts',(-28.7310026168688,12.4679867371616,
127.998320592069)) ;
#138878 = CARTESIAN_POINT('Ctrl Pts',(-28.6424524610437,12.5916525516401,
127.772874061218)) ;
#138879 = CARTESIAN_POINT('Ctrl Pts',(-28.5678961190025,12.7734684549556,
127.588037430388)) ;
#138880 = CARTESIAN_POINT('Ctrl Pts',(-28.5108566436919,13.0028688411228,
127.454584278807)) ;
#138881 = CARTESIAN_POINT('Ctrl Pts',(-28.475281642713,13.2619624535534,127.383760848204)) ;
#138882 = CARTESIAN_POINT('Ctrl Pts',(-28.4629023861597,13.5340192322936,
127.380880702846)) ;
#138883 = CARTESIAN_POINT('Ctrl Pts',(-28.4738518656341,13.7955675293532,
127.44581956107)) ;
#138884 = CARTESIAN_POINT('Ctrl Pts',(-28.5066666855688,14.0322613707932,
127.574868316922)) ;
#138885 = CARTESIAN_POINT('Ctrl Pts',(-28.5581068487113,14.224389834904,127.758189515183)) ;
#138886 = CARTESIAN_POINT('Ctrl Pts',(-28.623975139686,14.3598901194567,127.983749503875)) ;
#138887 = CARTESIAN_POINT('Ctrl Pts',(-28.6991366399092,14.4280176273918,
128.236609523979)) ;
#138888 = CARTESIAN_POINT('Ctrl Pts',(-28.7761803352426,14.4241023725172,
128.494570372186)) ;
#138889 = CARTESIAN_POINT('Ctrl Pts',(-28.8506922742166,14.3482280088461,
128.745549346044)) ;
#138890 = CARTESIAN_POINT('Ctrl Pts',(-28.91518277418,14.2060724290961,128.967049520542)) ;
#138891 = CARTESIAN_POINT('Ctrl Pts',(-28.9647186270019,14.0086808494732,
129.144776576755)) ;
#138892 = CARTESIAN_POINT('Ctrl Pts',(-28.995315357535,13.7691471639152,129.267239987643)) ;
#138893 = CARTESIAN_POINT('Ctrl Pts',(-29.003848162705,13.5031160987729,129.325457231296)) ;
#138894 = CARTESIAN_POINT('Ctrl Pts',(-28.9888212723258,13.2327334020777,
129.314673937566)) ;
#138895 = CARTESIAN_POINT('Ctrl Pts',(-28.9509676621617,12.9767766707072,
129.237101723994)) ;
#138896 = CARTESIAN_POINT('Ctrl Pts',(-28.891964848477,12.7518157375075,129.097860192288)) ;
#138897 = CARTESIAN_POINT('Ctrl Pts',(-28.8153017480323,12.5749030577416,
128.907053863378)) ;
#138898 = CARTESIAN_POINT('Ctrl Pts',(-28.7258829233603,12.458725868686,128.678963656753)) ;
#138899 = CARTESIAN_POINT('Ctrl Pts',(-28.6289134490532,12.4118884071783,
128.428957018799)) ;
#138900 = CARTESIAN_POINT('Ctrl Pts',(-28.5321954393679,12.4371447951342,
128.179276015019)) ;
#138901 = CARTESIAN_POINT('Ctrl Pts',(-28.4395504661701,12.5335140178268,
127.941927262626)) ;
#138902 = CARTESIAN_POINT('Ctrl Pts',(-28.358807949602,12.6929505633227,127.739083313665)) ;
#138903 = CARTESIAN_POINT('Ctrl Pts',(-28.2939499289173,12.9053983623053,
127.582807097336)) ;
#138904 = CARTESIAN_POINT('Ctrl Pts',(-28.2495091684995,13.1539498796381,
127.486020971058)) ;
#138905 = CARTESIAN_POINT('Ctrl Pts',(-28.2275303414602,13.4226750818637,
127.454981599478)) ;
#138906 = CARTESIAN_POINT('Ctrl Pts',(-28.2290607143686,13.6910891460654,
127.492564996296)) ;
#138907 = CARTESIAN_POINT('Ctrl Pts',(-28.2534186782273,13.9413684453662,
127.59699357478)) ;
#138908 = CARTESIAN_POINT('Ctrl Pts',(-28.2977067840336,14.1526799208371,
127.759377008187)) ;
#138909 = CARTESIAN_POINT('Ctrl Pts',(-28.3583229693319,14.3125333416555,
127.969564685725)) ;
#138910 = CARTESIAN_POINT('Ctrl Pts',(-28.430074904473,14.4088194589569,128.212248741583)) ;
#138911 = CARTESIAN_POINT('Ctrl Pts',(-28.507718384322,14.4343198918705,128.472390079449)) ;
#138912 = CARTESIAN_POINT('Ctrl Pts',(-28.5834398035334,14.3877722127897,
128.726476676245)) ;
#138913 = CARTESIAN_POINT('Ctrl Pts',(-28.6530124243077,14.2711471004472,
128.963054741333)) ;
#138914 = CARTESIAN_POINT('Ctrl Pts',(-28.7090122067586,14.0951742684999,
129.159592602646)) ;
#138915 = CARTESIAN_POINT('Ctrl Pts',(-28.7478941350473,13.870335354891,129.306328889926)) ;
#138916 = CARTESIAN_POINT('Ctrl Pts',(-28.7656138027504,13.612835927565,129.391292786156)) ;
#138917 = CARTESIAN_POINT('Ctrl Pts',(-28.760252313802,13.3431053086278,129.408666110812)) ;
#138918 = CARTESIAN_POINT('Ctrl Pts',(-28.7315959991371,13.0784069754049,
129.358066094416)) ;
#138919 = CARTESIAN_POINT('Ctrl Pts',(-28.6804303391378,12.8371325485697,
129.241909814744)) ;
#138920 = CARTESIAN_POINT('Ctrl Pts',(-28.6106432947035,12.6399915744991,
129.071040346761)) ;
#138921 = CARTESIAN_POINT('Ctrl Pts',(-28.5258257524472,12.4979352646964,
128.856384789912)) ;
#138922 = CARTESIAN_POINT('Ctrl Pts',(-28.4311698505634,12.4220838603556,
128.613084383185)) ;
#138923 = CARTESIAN_POINT('Ctrl Pts',(-28.3332246094965,12.4184701300548,
128.360113050716)) ;
#138924 = CARTESIAN_POINT('Ctrl Pts',(-28.2387034924304,12.4860424705287,
128.116923333277)) ;
#138925 = CARTESIAN_POINT('Ctrl Pts',(-28.1523073475974,12.6212970350437,
127.897736801008)) ;
#138926 = CARTESIAN_POINT('Ctrl Pts',(-28.0805635000624,12.8133839848722,
127.721209553133)) ;
#138927 = CARTESIAN_POINT('Ctrl Pts',(-28.0272630926043,13.050364922785,127.598747545585)) ;
#138928 = CARTESIAN_POINT('Ctrl Pts',(-27.9961045931269,13.3123037538977,
127.540725506652)) ;
#138929 = CARTESIAN_POINT('Ctrl Pts',(-27.988069139493,13.5832778951352,127.550400311311)) ;
#138930 = CARTESIAN_POINT('Ctrl Pts',(-28.0033125395844,13.8428843681781,
127.628091882332)) ;
#138931 = CARTESIAN_POINT('Ctrl Pts',(-28.0398912028952,14.0720013140808,
127.768057926957)) ;
#138932 = CARTESIAN_POINT('Ctrl Pts',(-28.0944259765686,14.2546155515289,
127.960459672568)) ;
#138933 = CARTESIAN_POINT('Ctrl Pts',(-28.1624219515475,14.3779471461467,
128.192231859961)) ;
#138934 = CARTESIAN_POINT('Ctrl Pts',(-28.2382878170761,14.4327785489293,
128.447023007249)) ;
#138935 = CARTESIAN_POINT('Ctrl Pts',(-28.3156214450991,14.4152048482771,
128.706033814232)) ;
#138936 = CARTESIAN_POINT('Ctrl Pts',(-28.3883959682431,14.3266409658442,
128.95175809986)) ;
#138937 = CARTESIAN_POINT('Ctrl Pts',(-28.4506693198691,14.1729214945641,
129.16686318667)) ;
#138938 = CARTESIAN_POINT('Ctrl Pts',(-28.4969327062817,13.9662155459552,
129.335062608003)) ;
#138939 = CARTESIAN_POINT('Ctrl Pts',(-28.5235541022144,13.7208186783693,
129.445890143364)) ;
#138940 = CARTESIAN_POINT('Ctrl Pts',(-28.5276980643996,13.4521886748155,
129.491290359284)) ;
#138941 = CARTESIAN_POINT('Ctrl Pts',(-28.5084074025572,13.1838897462868,
129.467926441214)) ;
#138942 = CARTESIAN_POINT('Ctrl Pts',(-28.4662760617063,12.9313138678917,
129.378013345421)) ;
#138943 = CARTESIAN_POINT('Ctrl Pts',(-28.4035475729084,12.7142071157524,
129.227914504089)) ;
#138944 = CARTESIAN_POINT('Ctrl Pts',(-28.3242366485113,12.5481822862925,
129.029307411766)) ;
#138945 = CARTESIAN_POINT('Ctrl Pts',(-28.2329991415399,12.4445945495957,
128.795913433975)) ;
#138946 = CARTESIAN_POINT('Ctrl Pts',(-28.1359471520329,12.4110615292549,
128.54547048254)) ;
#138947 = CARTESIAN_POINT('Ctrl Pts',(-28.0386871379967,12.4502003410622,
128.294574669809)) ;
#138948 = CARTESIAN_POINT('Ctrl Pts',(-27.9484093855994,12.5587981584367,
128.063898629952)) ;
#138949 = CARTESIAN_POINT('Ctrl Pts',(-27.8701354737038,12.7290992999271,
127.86833698565)) ;
#138950 = CARTESIAN_POINT('Ctrl Pts',(-27.8086851646448,12.9505642966122,
127.722109781574)) ;
#138951 = CARTESIAN_POINT('Ctrl Pts',(-27.7684638902634,13.2039533885785,
127.637616969587)) ;
#138952 = CARTESIAN_POINT('Ctrl Pts',(-27.7509048587101,13.4737768400672,
127.619438918027)) ;
#138953 = CARTESIAN_POINT('Ctrl Pts',(-27.7568758422641,13.7408243528461,
127.670098038824)) ;
#138954 = CARTESIAN_POINT('Ctrl Pts',(-27.7852338217469,13.9843828533781,
127.786086236129)) ;
#138955 = CARTESIAN_POINT('Ctrl Pts',(-27.8327593266423,14.1867700455966,
127.957871750746)) ;
#138956 = CARTESIAN_POINT('Ctrl Pts',(-27.896139879253,14.3360223311849,128.176262697775)) ;
#138957 = CARTESIAN_POINT('Ctrl Pts',(-27.9692983079035,14.4190304968155,
128.423017998671)) ;
#138958 = CARTESIAN_POINT('Ctrl Pts',(-28.0467984639361,14.4311357374112,
128.682548584271)) ;
#138959 = CARTESIAN_POINT('Ctrl Pts',(-28.1222733369049,14.3708887924222,
128.936189065257)) ;
#138960 = CARTESIAN_POINT('Ctrl Pts',(-28.1895265325835,14.2422926877059,
129.165851645267)) ;
#138961 = CARTESIAN_POINT('Ctrl Pts',(-28.2426703459913,14.0562619383273,
129.354079192252)) ;
#138962 = CARTESIAN_POINT('Ctrl Pts',(-28.2778835463942,13.8231736969123,
129.490209597053)) ;
#138963 = CARTESIAN_POINT('Ctrl Pts',(-28.2912600088371,13.5622216724448,
129.562407634763)) ;
#138964 = CARTESIAN_POINT('Ctrl Pts',(-28.2815138099123,13.2923510388066,
129.56694118938)) ;
#138965 = CARTESIAN_POINT('Ctrl Pts',(-28.2485236488303,13.0307856163929,
129.503695286891)) ;
#138966 = CARTESIAN_POINT('Ctrl Pts',(-28.1936350662213,12.7967159031727,
129.376581182953)) ;
#138967 = CARTESIAN_POINT('Ctrl Pts',(-28.1204881136384,12.6083942654361,
129.196006788455)) ;
#138968 = CARTESIAN_POINT('Ctrl Pts',(-28.033305520065,12.4782667075604,128.97447720968)) ;
#138969 = CARTESIAN_POINT('Ctrl Pts',(-27.9380490506444,12.4160107642981,
128.72924170442)) ;
#138970 = CARTESIAN_POINT('Ctrl Pts',(-27.840088998415,12.425588916255,128.476245677989)) ;
#138971 = CARTESIAN_POINT('Ctrl Pts',(-27.7460416419619,12.5070743322311,
128.234706957922)) ;
#138972 = CARTESIAN_POINT('Ctrl Pts',(-27.6622979311355,12.6538727730597,
128.023155368527)) ;
#138973 = CARTESIAN_POINT('Ctrl Pts',(-27.5938166192311,12.8553499552797,
127.85615827692)) ;
#138974 = CARTESIAN_POINT('Ctrl Pts',(-27.5445346630511,13.098103384175,127.74534712503)) ;
#138975 = CARTESIAN_POINT('Ctrl Pts',(-27.5175776227433,13.3649638276871,
127.69984232764)) ;
#138976 = CARTESIAN_POINT('Ctrl Pts',(-27.5141163308945,13.6334094300958,
127.722651608453)) ;
#138977 = CARTESIAN_POINT('Ctrl Pts',(-27.5335019356169,13.8886868396263,
127.812436729992)) ;
#138978 = CARTESIAN_POINT('Ctrl Pts',(-27.5737821241816,14.1104518310445,
127.963236838802)) ;
#138979 = CARTESIAN_POINT('Ctrl Pts',(-27.6314744421073,14.2832226261628,
128.164987370241)) ;
#138980 = CARTESIAN_POINT('Ctrl Pts',(-27.7012379510992,14.3937886224781,
128.401835946804)) ;
#138981 = CARTESIAN_POINT('Ctrl Pts',(-27.7781123535692,14.4350213815805,
128.65967036386)) ;
#138982 = CARTESIAN_POINT('Ctrl Pts',(-27.8546936773711,14.4038716563582,
128.916327544499)) ;
#138983 = CARTESIAN_POINT('Ctrl Pts',(-27.9261731861543,14.302057440806,129.158397140685)) ;
#138984 = CARTESIAN_POINT('Ctrl Pts',(-27.9855695077338,14.1377082691097,
129.364968157342)) ;
#138985 = CARTESIAN_POINT('Ctrl Pts',(-28.0284659120487,13.9225120820519,
129.523348044967)) ;
#138986 = CARTESIAN_POINT('Ctrl Pts',(-28.0510262279841,13.6705375102117,
129.622450560383)) ;
#138987 = CARTESIAN_POINT('Ctrl Pts',(-28.0507377584204,13.401884525291,129.654671141506)) ;
#138988 = CARTESIAN_POINT('Ctrl Pts',(-28.027107292662,13.1344381659713,129.618736562433)) ;
#138989 = CARTESIAN_POINT('Ctrl Pts',(-27.9806130101491,12.8864833048174,
129.516191990152)) ;
#138990 = CARTESIAN_POINT('Ctrl Pts',(-27.9148391290743,12.6791960280418,
129.356978782703)) ;
#138991 = CARTESIAN_POINT('Ctrl Pts',(-27.8325764038185,12.5233811391943,
129.149895121488)) ;
#138992 = CARTESIAN_POINT('Ctrl Pts',(-27.7398372427668,12.4327816584244,
128.912072670328)) ;
#138993 = CARTESIAN_POINT('Ctrl Pts',(-27.6421416316699,12.4129159573699,
128.659822662127)) ;
#138994 = CARTESIAN_POINT('Ctrl Pts',(-27.5459275592162,12.4655032796393,
128.411880163255)) ;
#138995 = CARTESIAN_POINT('Ctrl Pts',(-27.4573533230035,12.5866529362795,
128.186246122412)) ;
#138996 = CARTESIAN_POINT('Ctrl Pts',(-27.3819902516143,12.7674395708452,
127.999181472755)) ;
#138997 = CARTESIAN_POINT('Ctrl Pts',(-27.3242508154076,12.9966807390071,
127.863798954836)) ;
#138998 = CARTESIAN_POINT('Ctrl Pts',(-27.2882667414954,13.2541241840609,
127.79164129262)) ;
#138999 = CARTESIAN_POINT('Ctrl Pts',(-27.2751406243702,13.5248421394856,
127.786425007767)) ;
#139000 = CARTESIAN_POINT('Ctrl Pts',(-27.2853998464079,13.7882271369091,
127.849508781125)) ;
#139001 = CARTESIAN_POINT('Ctrl Pts',(-27.3176681383781,14.0260983655197,
127.97698427868)) ;
#139002 = CARTESIAN_POINT('Ctrl Pts',(-27.3687529118647,14.2200231919602,
128.159335122063)) ;
#139003 = CARTESIAN_POINT('Ctrl Pts',(-27.4341754696823,14.356772234067,128.383520804271)) ;
#139004 = CARTESIAN_POINT('Ctrl Pts',(-27.5087046282768,14.4269174457709,
128.634342726485)) ;
#139005 = CARTESIAN_POINT('Ctrl Pts',(-27.5863498095606,14.4252572954794,
128.894315325931)) ;
#139006 = CARTESIAN_POINT('Ctrl Pts',(-27.6608346895068,14.3512844735739,
129.14512930489)) ;
#139007 = CARTESIAN_POINT('Ctrl Pts',(-27.7254688305769,14.2117350246389,
129.366921379891)) ;
#139008 = CARTESIAN_POINT('Ctrl Pts',(-27.7757715686293,14.0152548216542,
129.547011019762)) ;
#139009 = CARTESIAN_POINT('Ctrl Pts',(-27.8069823814624,13.7756399540023,
129.671394466275)) ;
#139010 = CARTESIAN_POINT('Ctrl Pts',(-27.8161239931437,13.5122935142519,
129.731111533612)) ;
#139011 = CARTESIAN_POINT('Ctrl Pts',(-27.8018912094678,13.241130032097,129.722732596038)) ;
#139012 = CARTESIAN_POINT('Ctrl Pts',(-27.7646415514717,12.9839533345939,
129.646985455023)) ;
#139013 = CARTESIAN_POINT('Ctrl Pts',(-27.705971842593,12.7572239976212,129.508824746173)) ;
#139014 = CARTESIAN_POINT('Ctrl Pts',(-27.6300749308619,12.5794741431288,
129.320113150862)) ;
#139015 = CARTESIAN_POINT('Ctrl Pts',(-27.5407307406086,12.4611210765961,
129.092328609389)) ;
#139016 = CARTESIAN_POINT('Ctrl Pts',(-27.4443925507261,12.4122668265322,
128.843989508204)) ;
#139017 = CARTESIAN_POINT('Ctrl Pts',(-27.3469053180412,12.4354395083141,
128.592303176999)) ;
#139018 = CARTESIAN_POINT('Ctrl Pts',(-27.2540851953818,12.5301694803305,
128.354430002177)) ;
#139019 = CARTESIAN_POINT('Ctrl Pts',(-27.1731448505004,12.6876686572945,
128.150941740257)) ;
#139020 = CARTESIAN_POINT('Ctrl Pts',(-27.1078519711564,12.8982124580512,
127.993318537432)) ;
#139021 = CARTESIAN_POINT('Ctrl Pts',(-27.062565545524,13.1472879194742,127.894240819857)) ;
#139022 = CARTESIAN_POINT('Ctrl Pts',(-27.0400556107669,13.4151706318018,
127.861572480424)) ;
#139023 = CARTESIAN_POINT('Ctrl Pts',(-27.0409313353343,13.6833052731468,
127.89718448912)) ;
#139024 = CARTESIAN_POINT('Ctrl Pts',(-27.0644459838438,13.9335262194554,
127.999007834601)) ;
#139025 = CARTESIAN_POINT('Ctrl Pts',(-27.1085568252031,14.1479664880633,
128.161156205508)) ;
#139026 = CARTESIAN_POINT('Ctrl Pts',(-27.1686539025929,14.3087959168501,
128.369723486497)) ;
#139027 = CARTESIAN_POINT('Ctrl Pts',(-27.2401497732243,14.4069520231813,
128.611660947542)) ;
#139028 = CARTESIAN_POINT('Ctrl Pts',(-27.3173616295847,14.4347039370495,
128.870380646342)) ;
#139029 = CARTESIAN_POINT('Ctrl Pts',(-27.3937223670572,14.3899170768859,
129.12656922784)) ;
#139030 = CARTESIAN_POINT('Ctrl Pts',(-27.463154389175,14.2758481834518,129.362528068667)) ;
#139031 = CARTESIAN_POINT('Ctrl Pts',(-27.5198612341215,14.1010294405417,
129.561258806483)) ;
#139032 = CARTESIAN_POINT('Ctrl Pts',(-27.5592797085226,13.8772034323747,
129.709569614153)) ;
#139033 = CARTESIAN_POINT('Ctrl Pts',(-27.5776272327468,13.6206147260663,
129.796340563983)) ;
#139034 = CARTESIAN_POINT('Ctrl Pts',(-27.5729713117708,13.3509221462812,
129.815782598542)) ;
#139035 = CARTESIAN_POINT('Ctrl Pts',(-27.544865717924,13.0853829020601,129.766851005711)) ;
#139036 = CARTESIAN_POINT('Ctrl Pts',(-27.494656970879,12.8445476179022,129.653285076039)) ;
#139037 = CARTESIAN_POINT('Ctrl Pts',(-27.42515055289,12.6449528736105,129.483374882147)) ;
#139038 = CARTESIAN_POINT('Ctrl Pts',(-27.3406844192613,12.501260652652,129.269736460329)) ;
#139039 = CARTESIAN_POINT('Ctrl Pts',(-27.2465604864716,12.423505657414,129.02788025025)) ;
#139040 = CARTESIAN_POINT('Ctrl Pts',(-27.1485944866452,12.4173186176401,
128.774856876374)) ;
#139041 = CARTESIAN_POINT('Ctrl Pts',(-27.0533218365845,12.4833714818954,
128.529679282004)) ;
#139042 = CARTESIAN_POINT('Ctrl Pts',(-26.9670098871684,12.6162285773946,
128.310578416108)) ;
#139043 = CARTESIAN_POINT('Ctrl Pts',(-26.8945212967897,12.8073410485065,
128.131984688256)) ;
#139044 = CARTESIAN_POINT('Ctrl Pts',(-26.8407055797364,13.0432165498209,
128.007993993565)) ;
#139045 = CARTESIAN_POINT('Ctrl Pts',(-26.8088693650207,13.3046949553566,
127.94800110172)) ;
#139046 = CARTESIAN_POINT('Ctrl Pts',(-26.8001804373194,13.5764463640802,
127.9558548202)) ;
#139047 = CARTESIAN_POINT('Ctrl Pts',(-26.8148719233268,13.8363550328947,
128.031910726039)) ;
#139048 = CARTESIAN_POINT('Ctrl Pts',(-26.8507085202357,14.0655921907836,
128.169565286129)) ;
#139049 = CARTESIAN_POINT('Ctrl Pts',(-26.9049053545545,14.2503954340108,
128.36107536267)) ;
#139050 = CARTESIAN_POINT('Ctrl Pts',(-26.9728396411132,14.3757154030236,
128.592765403602)) ;
#139051 = CARTESIAN_POINT('Ctrl Pts',(-27.048441018008,14.4321659912553,128.846721483037)) ;
#139052 = CARTESIAN_POINT('Ctrl Pts',(-27.1255622643999,14.4167343012476,
129.10500433378)) ;
#139053 = CARTESIAN_POINT('Ctrl Pts',(-27.198538054879,14.3302899803119,129.351306443868)) ;
#139054 = CARTESIAN_POINT('Ctrl Pts',(-27.2612573342443,14.1784243472653,
129.567722425343)) ;
#139055 = CARTESIAN_POINT('Ctrl Pts',(-27.3082500797653,13.9717507603948,
129.738242510254)) ;
#139056 = CARTESIAN_POINT('Ctrl Pts',(-27.3352449628971,13.7284356730931,
129.849982315497)) ;
#139057 = CARTESIAN_POINT('Ctrl Pts',(-27.3401753539222,13.4606301780327,
129.897628724691)) ;
#139058 = CARTESIAN_POINT('Ctrl Pts',(-27.3213949208222,13.1906192009326,
129.875943304999)) ;
#139059 = CARTESIAN_POINT('Ctrl Pts',(-27.2801319319356,12.9388679840775,
129.788361151274)) ;
#139060 = CARTESIAN_POINT('Ctrl Pts',(-27.2177800966894,12.7195132163599,
129.639491018548)) ;
#139061 = CARTESIAN_POINT('Ctrl Pts',(-27.1386838373461,12.5518557369755,
129.441565434155)) ;
#139062 = CARTESIAN_POINT('Ctrl Pts',(-27.0481377468026,12.4467157573859,
129.210037428764)) ;
#139063 = CARTESIAN_POINT('Ctrl Pts',(-26.950619923967,12.4110145774445,128.958423991903)) ;
#139064 = CARTESIAN_POINT('Ctrl Pts',(-26.8539313870607,12.4479828345384,
128.708971248185)) ;
#139065 = CARTESIAN_POINT('Ctrl Pts',(-26.7631485338844,12.5544308128886,
128.476883218463)) ;
#139066 = CARTESIAN_POINT('Ctrl Pts',(-26.6839869423467,12.7245572177545,
128.278955232461)) ;
#139067 = CARTESIAN_POINT('Ctrl Pts',(-26.622452158733,12.9435039918997,128.1322624773)) ;
#139068 = CARTESIAN_POINT('Ctrl Pts',(-26.5814862033874,13.1965754394182,
128.045658074214)) ;
#139069 = CARTESIAN_POINT('Ctrl Pts',(-26.5633147142469,13.465805442607,128.025635976667)) ;
#139070 = CARTESIAN_POINT('Ctrl Pts',(-26.5685769247246,13.7328709787398,
128.074182266888)) ;
#139071 = CARTESIAN_POINT('Ctrl Pts',(-26.5962169903584,13.9772572958127,
128.188041557399)) ;
#139072 = CARTESIAN_POINT('Ctrl Pts',(-26.6434704653874,14.1820529249742,
128.359201485676)) ;
#139073 = CARTESIAN_POINT('Ctrl Pts',(-26.7064912763497,14.3328843736513,
128.576527484716)) ;
#139074 = CARTESIAN_POINT('Ctrl Pts',(-26.779676885671,14.417801109475,128.823460886102)) ;
#139075 = CARTESIAN_POINT('Ctrl Pts',(-26.8567641312626,14.4318123913692,
129.081615800254)) ;
#139076 = CARTESIAN_POINT('Ctrl Pts',(-26.932696019571,14.373230288219,129.336737835572)) ;
#139077 = CARTESIAN_POINT('Ctrl Pts',(-26.9999033577708,14.2469703146016,
129.56609452963)) ;
#139078 = CARTESIAN_POINT('Ctrl Pts',(-27.0536419770243,14.062146501963,129.756131764833)) ;
#139079 = CARTESIAN_POINT('Ctrl Pts',(-27.089338814048,13.8305007160398,129.893613733069)) ;
#139080 = CARTESIAN_POINT('Ctrl Pts',(-27.1034218397827,13.5704781299009,
129.967838856659)) ;
#139081 = CARTESIAN_POINT('Ctrl Pts',(-27.0943121258094,13.299460638904,129.974371676377)) ;
#139082 = CARTESIAN_POINT('Ctrl Pts',(-27.061909738513,13.0377343274411,129.91280775413)) ;
#139083 = CARTESIAN_POINT('Ctrl Pts',(-27.0079273099502,12.8036245820339,
129.78818096079)) ;
#139084 = CARTESIAN_POINT('Ctrl Pts',(-26.9350149495085,12.6130123285287,
129.608417134988)) ;
#139085 = CARTESIAN_POINT('Ctrl Pts',(-26.8483991702399,12.4813447603753,
129.388452122961)) ;
#139086 = CARTESIAN_POINT('Ctrl Pts',(-26.7529748959595,12.4167223842582,
129.14284477105)) ;
#139087 = CARTESIAN_POINT('Ctrl Pts',(-26.6551280409943,12.42436559993,128.890133118099)) ;
#139088 = CARTESIAN_POINT('Ctrl Pts',(-26.5611337632536,12.5034382891946,
128.648655692995)) ;
#139089 = CARTESIAN_POINT('Ctrl Pts',(-26.4768642655678,12.6484426384731,
128.435612464504)) ;
#139090 = CARTESIAN_POINT('Ctrl Pts',(-26.4076898573312,12.8490571867036,
128.266677661264)) ;
#139091 = CARTESIAN_POINT('Ctrl Pts',(-26.3578999656574,13.0907449616811,
128.154357478156)) ;
#139092 = CARTESIAN_POINT('Ctrl Pts',(-26.3302906513053,13.3559778335449,
128.106800455251)) ;
#139093 = CARTESIAN_POINT('Ctrl Pts',(-26.3261021407339,13.626477299062,128.127720572037)) ;
#139094 = CARTESIAN_POINT('Ctrl Pts',(-26.344861958985,13.8815733654641,128.215569449386)) ;
#139095 = CARTESIAN_POINT('Ctrl Pts',(-26.3845347243026,14.1045282563564,
128.364588267836)) ;
#139096 = CARTESIAN_POINT('Ctrl Pts',(-26.4417677663433,14.2789670451528,
128.564989101919)) ;
#139097 = CARTESIAN_POINT('Ctrl Pts',(-26.5113409516761,14.3914951714323,
128.801324455963)) ;
#139098 = CARTESIAN_POINT('Ctrl Pts',(-26.5877888188324,14.434860760417,129.057773892789)) ;
#139099 = CARTESIAN_POINT('Ctrl Pts',(-26.6648607758356,14.4056890526457,
129.316047449567)) ;
#139100 = CARTESIAN_POINT('Ctrl Pts',(-26.7362631521833,14.3062653162723,
129.557733992972)) ;
#139101 = CARTESIAN_POINT('Ctrl Pts',(-26.7962306963923,14.1434405265247,
129.766045804946)) ;
#139102 = CARTESIAN_POINT('Ctrl Pts',(-26.8396812882404,13.9296996110321,
129.926022503524)) ;
#139103 = CARTESIAN_POINT('Ctrl Pts',(-26.8629433105894,13.6772902073351,
130.027334699158)) ;
#139104 = CARTESIAN_POINT('Ctrl Pts',(-26.8632838118661,13.4099497148246,
130.061254571472)) ;
#139105 = CARTESIAN_POINT('Ctrl Pts',(-26.8403078076667,13.1418739541198,
130.027275416975)) ;
#139106 = CARTESIAN_POINT('Ctrl Pts',(-26.7946473707701,12.8939990849847,
129.927034092426)) ;
#139107 = CARTESIAN_POINT('Ctrl Pts',(-26.7292679370309,12.6844791056233,
129.769080119216)) ;
#139108 = CARTESIAN_POINT('Ctrl Pts',(-26.6469601321073,12.5265062757821,
129.562016710345)) ;
#139109 = CARTESIAN_POINT('Ctrl Pts',(-26.5549146970139,12.4345049912951,
129.326048353605)) ;
#139110 = CARTESIAN_POINT('Ctrl Pts',(-26.4569589709664,12.4124896110262,
129.073148163912)) ;
#139111 = CARTESIAN_POINT('Ctrl Pts',(-26.3610245559965,12.4629154938197,
128.825883391475)) ;
#139112 = CARTESIAN_POINT('Ctrl Pts',(-26.271958028802,12.582091252431,128.598863247898)) ;
#139113 = CARTESIAN_POINT('Ctrl Pts',(-26.1958909868628,12.7624371771161,
128.409894373029)) ;
#139114 = CARTESIAN_POINT('Ctrl Pts',(-26.1381566159572,12.9881392321824,
128.27418222961)) ;
#139115 = CARTESIAN_POINT('Ctrl Pts',(-26.1011574103229,13.2462582998136,
128.199249439198)) ;
#139116 = CARTESIAN_POINT('Ctrl Pts',(-26.0874123015779,13.5176871774874,
128.192315615647)) ;
#139117 = CARTESIAN_POINT('Ctrl Pts',(-26.0969930018115,13.7805944540118,
128.253300271888)) ;
#139118 = CARTESIAN_POINT('Ctrl Pts',(-26.1286189621167,14.0195269504541,
128.378899377995)) ;
#139119 = CARTESIAN_POINT('Ctrl Pts',(-26.1792019920037,14.2150385228552,
128.559789419472)) ;
#139120 = CARTESIAN_POINT('Ctrl Pts',(-26.2444273756428,14.3538332825844,
128.783472919647)) ;
#139121 = CARTESIAN_POINT('Ctrl Pts',(-26.3186947357783,14.425964693576,129.033487360147)) ;
#139122 = CARTESIAN_POINT('Ctrl Pts',(-26.396628580836,14.4260802790596,129.294434315719)) ;
#139123 = CARTESIAN_POINT('Ctrl Pts',(-26.4706207570241,14.3549350609901,
129.543496973816)) ;
#139124 = CARTESIAN_POINT('Ctrl Pts',(-26.5361954761091,14.2162529068252,
129.768318600153)) ;
#139125 = CARTESIAN_POINT('Ctrl Pts',(-26.5867781111596,14.0213156820109,
129.949154797901)) ;
#139126 = CARTESIAN_POINT('Ctrl Pts',(-26.618586099352,13.7835942530776,130.07517850614)) ;
#139127 = CARTESIAN_POINT('Ctrl Pts',(-26.6283811897984,13.5186608640693,
130.137060334724)) ;
#139128 = CARTESIAN_POINT('Ctrl Pts',(-26.6148877785356,13.2494162372405,
130.13058771019)) ;
#139129 = CARTESIAN_POINT('Ctrl Pts',(-26.5781030924617,12.9903691341897,
130.056369042685)) ;
#139130 = CARTESIAN_POINT('Ctrl Pts',(-26.5203533297591,12.7636900645103,
129.920699862936)) ;
#139131 = CARTESIAN_POINT('Ctrl Pts',(-26.4441846986195,12.58293139644,129.731499757236)) ;
#139132 = CARTESIAN_POINT('Ctrl Pts',(-26.3560625112512,12.464078841243,129.506925147999)) ;
#139133 = CARTESIAN_POINT('Ctrl Pts',(-26.2593259056977,12.4125693581943,
129.257617605936)) ;
#139134 = CARTESIAN_POINT('Ctrl Pts',(-26.1620985485317,12.4337094194749,
129.006578106188)) ;
#139135 = CARTESIAN_POINT('Ctrl Pts',(-26.0689353443424,12.5263145270348,
128.76773619341)) ;
#139136 = CARTESIAN_POINT('Ctrl Pts',(-25.9875127410395,12.6822587422614,
128.562869973626)) ;
#139137 = CARTESIAN_POINT('Ctrl Pts',(-25.9216923690682,12.8915625531578,
128.403716354475)) ;
#139138 = CARTESIAN_POINT('Ctrl Pts',(-25.8758306390324,13.1392603074742,
128.302891273382)) ;
#139139 = CARTESIAN_POINT('Ctrl Pts',(-25.8525818054641,13.4076118636345,
128.268165012633)) ;
#139140 = CARTESIAN_POINT('Ctrl Pts',(-25.8527555620702,13.6757335658836,
128.301682288657)) ;
#139141 = CARTESIAN_POINT('Ctrl Pts',(-25.8759296819954,13.9281677247044,
128.402731498127)) ;
#139142 = CARTESIAN_POINT('Ctrl Pts',(-25.9189093686323,14.1410411495776,
128.561123729007)) ;
#139143 = CARTESIAN_POINT('Ctrl Pts',(-25.9789503429921,14.3051859901722,
128.76978572316)) ;
#139144 = CARTESIAN_POINT('Ctrl Pts',(-26.0501976675012,14.4050577733478,
129.010974927713)) ;
#139145 = CARTESIAN_POINT('Ctrl Pts',(-26.1274137398456,14.4349188598701,
129.269745582532)) ;
#139146 = CARTESIAN_POINT('Ctrl Pts',(-26.2037453942148,14.3922309368258,
129.52578709105)) ;
#139147 = CARTESIAN_POINT('Ctrl Pts',(-26.2734485850338,14.2801808251174,
129.762531073939)) ;
#139148 = CARTESIAN_POINT('Ctrl Pts',(-26.3306498021722,14.1070360117015,
129.962712893199)) ;
#139149 = CARTESIAN_POINT('Ctrl Pts',(-26.3707342932592,13.8833119581465,
130.113115180101)) ;
#139150 = CARTESIAN_POINT('Ctrl Pts',(-26.389605114305,13.6288342320535,130.20122415819)) ;
#139151 = CARTESIAN_POINT('Ctrl Pts',(-26.3856317307219,13.3582466127621,
130.222792750629)) ;
#139152 = CARTESIAN_POINT('Ctrl Pts',(-26.3582425741299,13.0930921970462,
130.175851547749)) ;
#139153 = CARTESIAN_POINT('Ctrl Pts',(-26.3086067689133,12.8509541226963,
130.064004429468)) ;
#139154 = CARTESIAN_POINT('Ctrl Pts',(-26.2396339676843,12.650062531176,129.895634211399)) ;
#139155 = CARTESIAN_POINT('Ctrl Pts',(-26.1554049626922,12.504322010349,129.682740398293)) ;
#139156 = CARTESIAN_POINT('Ctrl Pts',(-26.0612953645753,12.424693152161,129.440982032959)) ;
#139157 = CARTESIAN_POINT('Ctrl Pts',(-25.9638486832033,12.4164961973712,
129.189306529937)) ;
#139158 = CARTESIAN_POINT('Ctrl Pts',(-25.8683438504238,12.4802514111472,
128.943468158545)) ;
#139159 = CARTESIAN_POINT('Ctrl Pts',(-25.7814639524611,12.6116452910191,
128.722795866727)) ;
#139160 = CARTESIAN_POINT('Ctrl Pts',(-25.7086114716684,12.8011772311019,
128.543106694356)) ;
#139161 = CARTESIAN_POINT('Ctrl Pts',(-25.6543263351022,13.0350450036084,
128.417626071778)) ;
#139162 = CARTESIAN_POINT('Ctrl Pts',(-25.6216719385945,13.2969780565828,
128.355372970236)) ;
#139163 = CARTESIAN_POINT('Ctrl Pts',(-25.6123346990145,13.5677347022496,
128.36120696557)) ;
#139164 = CARTESIAN_POINT('Ctrl Pts',(-25.6262359141222,13.8283851985519,
128.434959187361)) ;
#139165 = CARTESIAN_POINT('Ctrl Pts',(-25.6616701800478,14.0598714357244,
128.57160098533)) ;
#139166 = CARTESIAN_POINT('Ctrl Pts',(-25.7152945842557,14.2455587727683,
128.761348553752)) ;
#139167 = CARTESIAN_POINT('Ctrl Pts',(-25.7825955492344,14.3725641558704,
128.991061393796)) ;
#139168 = CARTESIAN_POINT('Ctrl Pts',(-25.8582910585464,14.4315964719956,
129.245406755469)) ;
#139169 = CARTESIAN_POINT('Ctrl Pts',(-25.9356294866348,14.4181824180769,
129.504398426313)) ;
#139170 = CARTESIAN_POINT('Ctrl Pts',(-26.0087913243708,14.3336378097198,
129.751237877826)) ;
#139171 = CARTESIAN_POINT('Ctrl Pts',(-26.0717150052296,14.1840091136267,
129.968155126164)) ;
#139172 = CARTESIAN_POINT('Ctrl Pts',(-26.1192862891209,13.9789558298509,
130.140357900612)) ;
#139173 = CARTESIAN_POINT('Ctrl Pts',(-26.1470311145863,13.735580763414,130.254419312679)) ;
#139174 = CARTESIAN_POINT('Ctrl Pts',(-26.1525271394237,13.4678622164134,
130.303748830678)) ;
#139175 = CARTESIAN_POINT('Ctrl Pts',(-26.1345823245785,13.1991328170732,
130.284317860337)) ;
#139176 = CARTESIAN_POINT('Ctrl Pts',(-26.0937347645656,12.9452257159657,
130.198137101084)) ;
#139177 = CARTESIAN_POINT('Ctrl Pts',(-26.0322662158017,12.7259341405257,
130.051655335126)) ;
#139178 = CARTESIAN_POINT('Ctrl Pts',(-25.9535276230655,12.5559411179341,
129.854841568092)) ;
#139179 = CARTESIAN_POINT('Ctrl Pts',(-25.8627268934651,12.4485460989971,
129.622745483608)) ;
#139180 = CARTESIAN_POINT('Ctrl Pts',(-25.7658821421245,12.411159941536,129.372899865208)) ;
#139181 = CARTESIAN_POINT('Ctrl Pts',(-25.6689843987872,12.4456278245902,
129.122866641899)) ;
#139182 = CARTESIAN_POINT('Ctrl Pts',(-25.5772788439363,12.5514145649144,
128.888347222745)) ;
#139183 = CARTESIAN_POINT('Ctrl Pts',(-25.4985967290999,12.7181519501975,
128.691450514129)) ;
#139184 = CARTESIAN_POINT('Ctrl Pts',(-25.4361709012921,12.9364297118054,
128.542285418365)) ;
#139185 = CARTESIAN_POINT('Ctrl Pts',(-25.3945996241829,13.1887531889945,
128.45390307165)) ;
#139186 = CARTESIAN_POINT('Ctrl Pts',(-25.3757082658116,13.4580633394379,
128.431815240773)) ;
#139187 = CARTESIAN_POINT('Ctrl Pts',(-25.3803406060574,13.7256377913563,
128.478541525222)) ;
#139188 = CARTESIAN_POINT('Ctrl Pts',(-25.4073082148746,13.9704139495142,
128.590368684336)) ;
#139189 = CARTESIAN_POINT('Ctrl Pts',(-25.4540453085521,14.1767864400758,
128.760039568759)) ;
#139190 = CARTESIAN_POINT('Ctrl Pts',(-25.5167004953322,14.3292888579234,
128.976301083279)) ;
#139191 = CARTESIAN_POINT('Ctrl Pts',(-25.5894209897251,14.4162419047305,
129.221770975587)) ;
#139192 = CARTESIAN_POINT('Ctrl Pts',(-25.6669609282362,14.4323070590761,
129.481465117335)) ;
#139193 = CARTESIAN_POINT('Ctrl Pts',(-25.7423474735605,14.3764282439281,
129.734680874727)) ;
#139194 = CARTESIAN_POINT('Ctrl Pts',(-25.8103758869325,14.2515625460975,
129.96666241246)) ;
#139195 = CARTESIAN_POINT('Ctrl Pts',(-25.8645418505469,14.0682228318719,
130.157932110319)) ;
#139196 = CARTESIAN_POINT('Ctrl Pts',(-25.9008771851767,13.8370233843303,
130.297370202357)) ;
#139197 = CARTESIAN_POINT('Ctrl Pts',(-25.9155226415146,13.5786249866576,
130.37309985319)) ;
#139198 = CARTESIAN_POINT('Ctrl Pts',(-25.907150581353,13.3076277382397,130.381793812356)) ;
#139199 = CARTESIAN_POINT('Ctrl Pts',(-25.8754438475342,13.0452573122607,
130.322268774417)) ;
#139200 = CARTESIAN_POINT('Ctrl Pts',(-25.8218007897925,12.8091512622852,
130.198773291913)) ;
#139201 = CARTESIAN_POINT('Ctrl Pts',(-25.7494081213582,12.617551612867,130.020477149333)) ;
#139202 = CARTESIAN_POINT('Ctrl Pts',(-25.6633722315796,12.4843718023618,
129.802116135341)) ;
#139203 = CARTESIAN_POINT('Ctrl Pts',(-25.5680282554624,12.4175958724791,
129.556775885265)) ;
#139204 = CARTESIAN_POINT('Ctrl Pts',(-25.4702720597222,12.4230554954089,
129.304289864055)) ;
#139205 = CARTESIAN_POINT('Ctrl Pts',(-25.3759369019875,12.5002516562104,
129.061871713019)) ;
#139206 = CARTESIAN_POINT('Ctrl Pts',(-25.2915203838476,12.6429371553798,
128.848300314289)) ;
#139207 = CARTESIAN_POINT('Ctrl Pts',(-25.2215243889668,12.8430359620073,
128.677120783399)) ;
#139208 = CARTESIAN_POINT('Ctrl Pts',(-25.1713237180579,13.0829430987805,
128.563478292785)) ;
#139209 = CARTESIAN_POINT('Ctrl Pts',(-25.1429774609377,13.348262589156,128.513840001074)) ;
#139210 = CARTESIAN_POINT('Ctrl Pts',(-25.1380814446493,13.617980538018,128.532575804089)) ;
#139211 = CARTESIAN_POINT('Ctrl Pts',(-25.1562814256738,13.8754577927148,
128.61900340648)) ;
#139212 = CARTESIAN_POINT('Ctrl Pts',(-25.1955679750799,14.0994368224178,
128.766915779269)) ;
#139213 = CARTESIAN_POINT('Ctrl Pts',(-25.2519785797865,14.2743408293056,
128.964695140055)) ;
#139214 = CARTESIAN_POINT('Ctrl Pts',(-25.3214400334483,14.3892596729095,
129.200801570197)) ;
#139215 = CARTESIAN_POINT('Ctrl Pts',(-25.3977308716843,14.4346258040112,
129.456767831054)) ;
#139216 = CARTESIAN_POINT('Ctrl Pts',(-25.4750778381126,14.4074612330324,
129.715931930331)) ;
#139217 = CARTESIAN_POINT('Ctrl Pts',(-25.5466694832016,14.3096987835835,
129.958166513638)) ;
#139218 = CARTESIAN_POINT('Ctrl Pts',(-25.6068294845438,14.1493774031888,
130.166897650572)) ;
#139219 = CARTESIAN_POINT('Ctrl Pts',(-25.6510183732772,13.935562868649,130.329231840898)) ;
#139220 = CARTESIAN_POINT('Ctrl Pts',(-25.6747380783682,13.6861606118435,
130.431586420245)) ;
#139221 = CARTESIAN_POINT('Ctrl Pts',(-25.6758133796976,13.4167352169348,
130.467951113991)) ;
#139222 = CARTESIAN_POINT('Ctrl Pts',(-25.653459078872,13.1492793406519,130.435675091596)) ;
#139223 = CARTESIAN_POINT('Ctrl Pts',(-25.6084542619497,12.9005268787558,
130.337351258316)) ;
#139224 = CARTESIAN_POINT('Ctrl Pts',(-25.5435299244083,12.6897474261303,
130.180738845539)) ;
#139225 = CARTESIAN_POINT('Ctrl Pts',(-25.4620224695308,12.5306016297354,
129.975863624958)) ;
#139226 = CARTESIAN_POINT('Ctrl Pts',(-25.3697477074986,12.4360458848473,
129.739397853574)) ;
#139227 = CARTESIAN_POINT('Ctrl Pts',(-25.2719994495299,12.412131814889,129.48704906573)) ;
#139228 = CARTESIAN_POINT('Ctrl Pts',(-25.175740221563,12.4605358033904,129.238901405947)) ;
#139229 = CARTESIAN_POINT('Ctrl Pts',(-25.0863095489117,12.5784164440372,
129.010871104516)) ;
#139230 = CARTESIAN_POINT('Ctrl Pts',(-25.0104054959568,12.7554816677878,
128.822088090123)) ;
#139231 = CARTESIAN_POINT('Ctrl Pts',(-24.9515970266411,12.981762434369,128.683509475873)) ;
#139232 = CARTESIAN_POINT('Ctrl Pts',(-24.9141759784363,13.2381598405705,
128.607190779819)) ;
#139233 = CARTESIAN_POINT('Ctrl Pts',(-24.8996770755616,13.5101992275675,
128.598149052653)) ;
#139234 = CARTESIAN_POINT('Ctrl Pts',(-24.9086031480491,13.7733131452284,
128.657183366263)) ;
#139235 = CARTESIAN_POINT('Ctrl Pts',(-24.9398052171064,14.0140641414936,
128.781675601586)) ;
#139236 = CARTESIAN_POINT('Ctrl Pts',(-24.9896927765608,14.2098744851872,
128.960364452866)) ;
#139237 = CARTESIAN_POINT('Ctrl Pts',(-25.0544790313913,14.350580234219,129.182743841367)) ;
#139238 = CARTESIAN_POINT('Ctrl Pts',(-25.1286457194053,14.424831664933,129.432502490811)) ;
#139239 = CARTESIAN_POINT('Ctrl Pts',(-25.206490431836,14.4272048065726,129.69314833904)) ;
#139240 = CARTESIAN_POINT('Ctrl Pts',(-25.2808580019925,14.3577939538396,
129.943405474164)) ;
#139241 = CARTESIAN_POINT('Ctrl Pts',(-25.3465032391174,14.2217457510102,
130.168270717532)) ;
#139242 = CARTESIAN_POINT('Ctrl Pts',(-25.3979717151172,14.0267541205093,
130.35195733621)) ;
#139243 = CARTESIAN_POINT('Ctrl Pts',(-25.4301050307948,13.7911380012518,
130.478752074177)) ;
#139244 = CARTESIAN_POINT('Ctrl Pts',(-25.4406575499018,13.5273990690374,
130.542772384891)) ;
#139245 = CARTESIAN_POINT('Ctrl Pts',(-25.427837941042,13.2571616705375,130.538379196713)) ;
#139246 = CARTESIAN_POINT('Ctrl Pts',(-25.3916867409364,12.9974108749585,
130.466017830389)) ;
#139247 = CARTESIAN_POINT('Ctrl Pts',(-25.3344256044563,12.7695379625925,
130.331802297734)) ;
#139248 = CARTESIAN_POINT('Ctrl Pts',(-25.2591612456238,12.5879936819102,
130.145065778963)) ;
#139249 = CARTESIAN_POINT('Ctrl Pts',(-25.1708094896904,12.4663339694794,
129.920031665293)) ;
#139250 = CARTESIAN_POINT('Ctrl Pts',(-25.0742025214906,12.4130530302768,
129.671092872011)) ;
#139251 = CARTESIAN_POINT('Ctrl Pts',(-24.9771023880055,12.4321501151392,
129.420369705811)) ;
#139252 = CARTESIAN_POINT('Ctrl Pts',(-24.8838787240354,12.5224108071959,
129.181282199813)) ;
#139253 = CARTESIAN_POINT('Ctrl Pts',(-24.8016886878617,12.6773122255345,
128.974323033663)) ;
#139254 = CARTESIAN_POINT('Ctrl Pts',(-24.7354635805379,12.8853931942508,
128.813970529302)) ;
#139255 = CARTESIAN_POINT('Ctrl Pts',(-24.6891442972207,13.1311434549155,
128.711670601176)) ;
#139256 = CARTESIAN_POINT('Ctrl Pts',(-24.6650967559786,13.4000886960601,
128.674724701615)) ;
#139257 = CARTESIAN_POINT('Ctrl Pts',(-24.6646958448049,13.6679854854521,
128.706516222695)) ;
#139258 = CARTESIAN_POINT('Ctrl Pts',(-24.6869181699987,13.9198929114768,
128.804574602593)) ;
#139259 = CARTESIAN_POINT('Ctrl Pts',(-24.7299417619901,14.1367331650745,
128.963529160766)) ;
#139260 = CARTESIAN_POINT('Ctrl Pts',(-24.78899702236,14.3006761293965,129.168957484263)) ;
#139261 = CARTESIAN_POINT('Ctrl Pts',(-24.8604323902462,14.4034182515294,
129.410928254081)) ;
#139262 = CARTESIAN_POINT('Ctrl Pts',(-24.9373849419803,14.4350219442823,
129.668834674646)) ;
#139263 = CARTESIAN_POINT('Ctrl Pts',(-25.0139098900193,14.3943912084008,
129.925485785032)) ;
#139264 = CARTESIAN_POINT('Ctrl Pts',(-25.0838686001623,14.2842181176635,
130.162962649196)) ;
#139265 = CARTESIAN_POINT('Ctrl Pts',(-25.141505675191,14.1123337883522,130.364455738094)) ;
#139266 = CARTESIAN_POINT('Ctrl Pts',(-25.1819228640214,13.8914433195642,
130.515599513236)) ;
#139267 = CARTESIAN_POINT('Ctrl Pts',(-25.201613141345,13.6364805830374,130.606273016799)) ;
#139268 = CARTESIAN_POINT('Ctrl Pts',(-25.1983020491001,13.3663281514523,
130.629736093281)) ;
#139269 = CARTESIAN_POINT('Ctrl Pts',(-25.1715470228642,13.1002904677936,
130.58470870473)) ;
#139270 = CARTESIAN_POINT('Ctrl Pts',(-25.1225067421903,12.857318656671,130.474590193612)) ;
#139271 = CARTESIAN_POINT('Ctrl Pts',(-25.0540277977989,12.6550558730351,
130.307664775512)) ;
#139272 = CARTESIAN_POINT('Ctrl Pts',(-24.9702550119896,12.5076994857307,
130.096067377798)) ;
#139273 = CARTESIAN_POINT('Ctrl Pts',(-24.8763683967754,12.4260782078646,
129.854957119094)) ;
#139274 = CARTESIAN_POINT('Ctrl Pts',(-24.7789829706749,12.415541436623,129.60344254161)) ;
#139275 = CARTESIAN_POINT('Ctrl Pts',(-24.6826294458462,12.4780902877727,
129.35537895735)) ;
#139276 = CARTESIAN_POINT('Ctrl Pts',(-24.5962537093982,12.6066343882026,
129.135870949235)) ;
#139277 = CARTESIAN_POINT('Ctrl Pts',(-24.5225844167585,12.7952136199714,
128.953931288036)) ;
#139278 = CARTESIAN_POINT('Ctrl Pts',(-24.4677935144789,13.027981899229,128.826949566631)) ;
#139279 = CARTESIAN_POINT('Ctrl Pts',(-24.43445736829,13.289687480561,128.762746162363)) ;
#139280 = CARTESIAN_POINT('Ctrl Pts',(-24.4245047098199,13.5603128220289,
128.766764296195)) ;
#139281 = CARTESIAN_POINT('Ctrl Pts',(-24.4377309514563,13.8211027693198,
128.838491234365)) ;
#139282 = CARTESIAN_POINT('Ctrl Pts',(-24.4725941333539,14.0538032313773,
128.973482598895)) ;
#139283 = CARTESIAN_POINT('Ctrl Pts',(-24.5257689032639,14.241090775664,129.161927643805)) ;
#139284 = CARTESIAN_POINT('Ctrl Pts',(-24.5929703029174,14.3701941266746,
129.391446649845)) ;
#139285 = CARTESIAN_POINT('Ctrl Pts',(-24.6684647537559,14.4308809538835,
129.645172653091)) ;
#139286 = CARTESIAN_POINT('Ctrl Pts',(-24.7455934848516,14.419613884929,129.903448778638)) ;
#139287 = CARTESIAN_POINT('Ctrl Pts',(-24.8191360362311,14.336836848792,130.151480211498)) ;
#139288 = CARTESIAN_POINT('Ctrl Pts',(-24.8822457334504,14.1892311094166,
130.368855563618)) ;
#139289 = CARTESIAN_POINT('Ctrl Pts',(-24.9303421333715,13.9859053267194,
130.542561767144)) ;
#139290 = CARTESIAN_POINT('Ctrl Pts',(-24.958773115316,13.742611201067,130.658737814802)) ;
#139291 = CARTESIAN_POINT('Ctrl Pts',(-24.9649012046553,13.4761438373695,
130.709803732788)) ;
#139292 = CARTESIAN_POINT('Ctrl Pts',(-24.9476912211436,13.2070931418873,
130.692535709155)) ;
#139293 = CARTESIAN_POINT('Ctrl Pts',(-24.9074283032168,12.9521503687759,
130.608104321017)) ;
#139294 = CARTESIAN_POINT('Ctrl Pts',(-24.8465172822224,12.7315094149766,
130.463257238954)) ;
#139295 = CARTESIAN_POINT('Ctrl Pts',(-24.7678429615914,12.5595225536488,
130.266760317396)) ;
#139296 = CARTESIAN_POINT('Ctrl Pts',(-24.6780376574106,12.4509681334738,
130.037306136309)) ;
#139297 = CARTESIAN_POINT('Ctrl Pts',(-24.5805061326321,12.4111337658692,
129.785728889855)) ;
#139298 = CARTESIAN_POINT('Ctrl Pts',(-24.4839877480091,12.4436883984276,
129.536643622124)) ;
#139299 = CARTESIAN_POINT('Ctrl Pts',(-24.3919596936368,12.547486739405,129.301206635287)) ;
#139300 = CARTESIAN_POINT('Ctrl Pts',(-24.3129491036762,12.7123018084608,
129.103301088071)) ;
#139301 = CARTESIAN_POINT('Ctrl Pts',(-24.2498169239358,12.9300708055824,
128.952180938411)) ;
#139302 = CARTESIAN_POINT('Ctrl Pts',(-24.2078048366664,13.1802337524753,
128.862326668088)) ;
#139303 = CARTESIAN_POINT('Ctrl Pts',(-24.1880922707095,13.4510759220384,
128.838061182578)) ;
#139304 = CARTESIAN_POINT('Ctrl Pts',(-24.1921076852184,13.7180592996578,
128.882867446039)) ;
#139305 = CARTESIAN_POINT('Ctrl Pts',(-24.2185138890603,13.964278608138,128.993132540059)) ;
#139306 = CARTESIAN_POINT('Ctrl Pts',(-24.2646501252742,14.1712561679291,
129.160953206331)) ;
#139307 = CARTESIAN_POINT('Ctrl Pts',(-24.3266399230232,14.325372518196,129.375160905542)) ;
#139308 = CARTESIAN_POINT('Ctrl Pts',(-24.3997087634312,14.4148742609065,
129.621908054451)) ;
#139309 = CARTESIAN_POINT('Ctrl Pts',(-24.4766126097422,14.4329087895001,
129.879481483547)) ;
#139310 = CARTESIAN_POINT('Ctrl Pts',(-24.5526547839398,14.3788838445396,
130.134842622102)) ;
#139311 = CARTESIAN_POINT('Ctrl Pts',(-24.6207455540188,14.2561019956526,
130.366891479371)) ;
#139312 = CARTESIAN_POINT('Ctrl Pts',(-24.6754095977467,14.0742378272797,
130.559641849346)) ;
#139313 = CARTESIAN_POINT('Ctrl Pts',(-24.7122096656787,13.8451950259534,
130.700297086839)) ;
#139314 = CARTESIAN_POINT('Ctrl Pts',(-24.727674522459,13.5867435987056,130.778518269024)) ;
#139315 = CARTESIAN_POINT('Ctrl Pts',(-24.7198654764314,13.3144405101765,
130.789020297388)) ;
#139316 = CARTESIAN_POINT('Ctrl Pts',(-24.6889016208014,13.0528696187883,
130.731507643832)) ;
#139317 = CARTESIAN_POINT('Ctrl Pts',(-24.6360315938546,12.8160518820106,
130.610209194301)) ;
#139318 = CARTESIAN_POINT('Ctrl Pts',(-24.5640862049924,12.6226065915497,
130.433257284621)) ;
#139319 = CARTESIAN_POINT('Ctrl Pts',(-24.4782156125006,12.4871997315169,
130.215449636711)) ;
#139320 = CARTESIAN_POINT('Ctrl Pts',(-24.3826837946767,12.4184347778258,
129.969678308433)) ;
#139321 = CARTESIAN_POINT('Ctrl Pts',(-24.285484258313,12.4219001112793,129.718626572152)) ;
#139322 = CARTESIAN_POINT('Ctrl Pts',(-24.1908371872593,12.4968774308013,
129.475331098626)) ;
#139323 = CARTESIAN_POINT('Ctrl Pts',(-24.1059297242578,12.6381725760813,
129.260388880534)) ;
#139324 = CARTESIAN_POINT('Ctrl Pts',(-24.0356325005768,12.836067679816,129.088215051841)) ;
#139325 = CARTESIAN_POINT('Ctrl Pts',(-23.9845812244526,13.0762565431926,
128.9722614937)) ;
#139326 = CARTESIAN_POINT('Ctrl Pts',(-23.9557404233227,13.3398740160854,
128.921014471502)) ;
#139327 = CARTESIAN_POINT('Ctrl Pts',(-23.9500932821032,13.6103043330608,
128.937631008638)) ;
#139328 = CARTESIAN_POINT('Ctrl Pts',(-23.9676534068118,13.8681249215715,
129.02215077165)) ;
#139329 = CARTESIAN_POINT('Ctrl Pts',(-24.0062669166322,14.093287105724,129.168070149275)) ;
#139330 = CARTESIAN_POINT('Ctrl Pts',(-24.0626571938418,14.2707836403436,
129.36601232404)) ;
#139331 = CARTESIAN_POINT('Ctrl Pts',(-24.1314305220899,14.3866738384329,
129.599899487544)) ;
#139332 = CARTESIAN_POINT('Ctrl Pts',(-24.2076451382746,14.4343395639672,
129.855670337091)) ;
#139333 = CARTESIAN_POINT('Ctrl Pts',(-24.2848983556719,14.4093417175208,
130.114493222806)) ;
#139334 = CARTESIAN_POINT('Ctrl Pts',(-24.3567922015602,14.3139583331245,
130.35760755757)) ;
#139335 = CARTESIAN_POINT('Ctrl Pts',(-24.4177512909038,14.1538396141847,
130.568932173959)) ;
#139336 = CARTESIAN_POINT('Ctrl Pts',(-24.4620640818478,13.9434082127298,
130.731300630705)) ;
#139337 = CARTESIAN_POINT('Ctrl Pts',(-24.4866543542614,13.6926166165872,
130.836506821739)) ;
#139338 = CARTESIAN_POINT('Ctrl Pts',(-24.4883147442223,13.425230952717,130.874349792581)) ;
#139339 = CARTESIAN_POINT('Ctrl Pts',(-24.4666758817606,13.1569924871447,
130.844230426763)) ;
#139340 = CARTESIAN_POINT('Ctrl Pts',(-24.4223330200419,12.9074157476161,
130.747826094221)) ;
#139341 = CARTESIAN_POINT('Ctrl Pts',(-24.3576260683162,12.6946405616374,
130.591985997049)) ;
#139342 = CARTESIAN_POINT('Ctrl Pts',(-24.2771035667315,12.5348309308551,
130.389750673622)) ;
#139343 = CARTESIAN_POINT('Ctrl Pts',(-24.1844908621363,12.4376124689349,
130.152515823898)) ;
#139344 = CARTESIAN_POINT('Ctrl Pts',(-24.0873106866223,12.4118470514465,
129.90164747401)) ;
#139345 = CARTESIAN_POINT('Ctrl Pts',(-23.9907623342062,12.4580456544619,
129.652715532171)) ;
#139346 = CARTESIAN_POINT('Ctrl Pts',(-23.9012147893026,12.5736491216982,
129.424267530587)) ;
#139347 = CARTESIAN_POINT('Ctrl Pts',(-23.8245652736496,12.7495591694402,
129.23341927134)) ;
#139348 = CARTESIAN_POINT('Ctrl Pts',(-23.7650732037928,12.9753683734727,
129.092929090297)) ;
#139349 = CARTESIAN_POINT('Ctrl Pts',(-23.7271033701168,13.2312289838448,
129.015013590769)) ;
#139350 = CARTESIAN_POINT('Ctrl Pts',(-23.7119712545994,13.5022491651901,
129.004007468431)) ;
#139351 = CARTESIAN_POINT('Ctrl Pts',(-23.7203019095383,13.7663767191028,
129.061383252461)) ;
#139352 = CARTESIAN_POINT('Ctrl Pts',(-23.7506144849391,14.0063276697149,
129.183017107517)) ;
#139353 = CARTESIAN_POINT('Ctrl Pts',(-23.8001454534432,14.2048736282249,
129.360832931781)) ;
#139354 = CARTESIAN_POINT('Ctrl Pts',(-23.8648094922,14.347691195203,129.582954666991)) ;
#139355 = CARTESIAN_POINT('Ctrl Pts',(-23.9388753354998,14.4237776298714,
129.832449027665)) ;
#139356 = CARTESIAN_POINT('Ctrl Pts',(-24.0164983821894,14.4280807794616,
130.092358864372)) ;
#139357 = CARTESIAN_POINT('Ctrl Pts',(-24.0910798904586,14.3608278808949,
130.343248164158)) ;
#139358 = CARTESIAN_POINT('Ctrl Pts',(-24.1572505503088,14.2256360688744,
130.569788751767)) ;
#139359 = CARTESIAN_POINT('Ctrl Pts',(-24.2086514826109,14.0344800390557,
130.752888831951)) ;
#139360 = CARTESIAN_POINT('Ctrl Pts',(-24.2417573503002,13.7980436571723,
130.882815753271)) ;
#139361 = CARTESIAN_POINT('Ctrl Pts',(-24.2528842234986,13.5353242806262,
130.948432556299)) ;
#139362 = CARTESIAN_POINT('Ctrl Pts',(-24.2407093073429,13.2644874689488,
130.945996646237)) ;
#139363 = CARTESIAN_POINT('Ctrl Pts',(-24.2053407643436,13.0050529303368,
130.875798295924)) ;
#139364 = CARTESIAN_POINT('Ctrl Pts',(-24.1485465653022,12.7754380725172,
130.743031004446)) ;
#139365 = CARTESIAN_POINT('Ctrl Pts',(-24.0738199872738,12.5925960491714,
130.557822597348)) ;
#139366 = CARTESIAN_POINT('Ctrl Pts',(-23.9857890662773,12.4690082220502,
130.333727746733)) ;
#139367 = CARTESIAN_POINT('Ctrl Pts',(-23.8893876382777,12.4135709144517,
130.085365735719)) ;
#139368 = CARTESIAN_POINT('Ctrl Pts',(-23.7920567607928,12.4306394934732,
129.834034345841)) ;
#139369 = CARTESIAN_POINT('Ctrl Pts',(-23.6988914891641,12.518547510187,129.595010139751)) ;
#139370 = CARTESIAN_POINT('Ctrl Pts',(-23.6161714664072,12.6718440202401,
129.386557760484)) ;
#139371 = CARTESIAN_POINT('Ctrl Pts',(-23.549452793789,12.8780301734486,129.224700541014)) ;
#139372 = CARTESIAN_POINT('Ctrl Pts',(-23.5021872674409,13.1252486196316,
129.119942147481)) ;
#139373 = CARTESIAN_POINT('Ctrl Pts',(-23.4777604477291,13.3909665583226,
129.081520904008)) ;
#139374 = CARTESIAN_POINT('Ctrl Pts',(-23.4765798056597,13.6612160977101,
129.111299193796)) ;
#139375 = CARTESIAN_POINT('Ctrl Pts',(-23.4982607396798,13.9131568829426,
129.207697075482)) ;
#139376 = CARTESIAN_POINT('Ctrl Pts',(-23.5404707375718,14.1304384080909,
129.36412734294)) ;
#139377 = CARTESIAN_POINT('Ctrl Pts',(-23.5993517273674,14.2969775123332,
129.569201224497)) ;
#139378 = CARTESIAN_POINT('Ctrl Pts',(-23.6706606614751,14.4015522175217,
129.810846815782)) ;
#139379 = CARTESIAN_POINT('Ctrl Pts',(-23.7472655844458,14.4350500549688,
130.067624578881)) ;
#139380 = CARTESIAN_POINT('Ctrl Pts',(-23.8238068480449,14.3967519657553,
130.324283748109)) ;
#139381 = CARTESIAN_POINT('Ctrl Pts',(-23.8941385602596,14.288484921225,130.56289011732)) ;
#139382 = CARTESIAN_POINT('Ctrl Pts',(-23.9522769819151,14.1181740958946,
130.76587139896)) ;
#139383 = CARTESIAN_POINT('Ctrl Pts',(-23.99331192498,13.897753350153,130.918917945401)) ;
#139384 = CARTESIAN_POINT('Ctrl Pts',(-24.0135547856214,13.6446684780805,
131.01105286223)) ;
#139385 = CARTESIAN_POINT('Ctrl Pts',(-24.0109351960766,13.3734340480479,
131.036692378548)) ;
#139386 = CARTESIAN_POINT('Ctrl Pts',(-23.984750772328,13.1072276991085,130.993310697227)) ;
#139387 = CARTESIAN_POINT('Ctrl Pts',(-23.9365029867963,12.8641925809132,
130.885390202893)) ;
#139388 = CARTESIAN_POINT('Ctrl Pts',(-23.8685796909686,12.660522785721,130.720081448326)) ;
#139389 = CARTESIAN_POINT('Ctrl Pts',(-23.7853638608259,12.511411763425,130.510055511429)) ;
#139390 = CARTESIAN_POINT('Ctrl Pts',(-23.6911328337757,12.4272142219304,
130.268135624709)) ;
#139391 = CARTESIAN_POINT('Ctrl Pts',(-23.5939071495122,12.4150347964973,
130.017043202023)) ;
#139392 = CARTESIAN_POINT('Ctrl Pts',(-23.4980296480192,12.4747491007078,
129.770142716077)) ;
#139393 = CARTESIAN_POINT('Ctrl Pts',(-23.4105558276953,12.6023245536218,
129.547706835705)) ;
#139394 = CARTESIAN_POINT('Ctrl Pts',(-23.336481762881,12.7898413846695,129.364600555102)) ;
#139395 = CARTESIAN_POINT('Ctrl Pts',(-23.2813353510646,13.0206706862551,
129.23645575968)) ;
#139396 = CARTESIAN_POINT('Ctrl Pts',(-23.2473156516746,13.2818517746603,
129.170263348697)) ;
#139397 = CARTESIAN_POINT('Ctrl Pts',(-23.2366830075241,13.5521277577084,
129.172253536318)) ;
#139398 = CARTESIAN_POINT('Ctrl Pts',(-23.2492140792166,13.813956814144,129.242001480208)) ;
#139399 = CARTESIAN_POINT('Ctrl Pts',(-23.2837359052188,14.0485698568868,
129.376142320652)) ;
#139400 = CARTESIAN_POINT('Ctrl Pts',(-23.3361299078761,14.2361101273789,
129.562094932607)) ;
#139401 = CARTESIAN_POINT('Ctrl Pts',(-23.403184331613,14.3675383856298,129.791288542673)) ;
#139402 = CARTESIAN_POINT('Ctrl Pts',(-23.4783602446362,14.4300942221494,
130.044003619567)) ;
#139403 = CARTESIAN_POINT('Ctrl Pts',(-23.5556298375246,14.4208865281834,
130.302748225955)) ;
#139404 = CARTESIAN_POINT('Ctrl Pts',(-23.6291635545595,14.3405661224656,
130.550641869123)) ;
#139405 = CARTESIAN_POINT('Ctrl Pts',(-23.6931552963386,14.1934622842168,
130.770869255254)) ;
#139406 = CARTESIAN_POINT('Ctrl Pts',(-23.7415085139769,13.9917022316215,
130.945235929377)) ;
#139407 = CARTESIAN_POINT('Ctrl Pts',(-23.7704326776443,13.7502056970642,
131.06273915926)) ;
#139408 = CARTESIAN_POINT('Ctrl Pts',(-23.7772973067199,13.4844947698669,
131.115913754511)) ;
#139409 = CARTESIAN_POINT('Ctrl Pts',(-23.7606691495744,13.2141841161546,
131.100485287274)) ;
#139410 = CARTESIAN_POINT('Ctrl Pts',(-23.7211119628859,12.9589228275276,
131.018054041759)) ;
#139411 = CARTESIAN_POINT('Ctrl Pts',(-23.6603186352369,12.736270288281,130.873727443309)) ;
#139412 = CARTESIAN_POINT('Ctrl Pts',(-23.5832218993153,12.5648475025287,
130.681365345848)) ;
#139413 = CARTESIAN_POINT('Ctrl Pts',(-23.4926718163616,12.452872634964,130.450136303181)) ;
#139414 = CARTESIAN_POINT('Ctrl Pts',(-23.3961081126866,12.4112941971035,
130.201074563628)) ;
#139415 = CARTESIAN_POINT('Ctrl Pts',(-23.2986109014059,12.4419882074806,
129.949450466439)) ;
#139416 = CARTESIAN_POINT('Ctrl Pts',(-23.2072849319717,12.5427027853094,
129.715701129722)) ;
#139417 = CARTESIAN_POINT('Ctrl Pts',(-23.1272047239973,12.7067963999461,
129.514929286389)) ;
#139418 = CARTESIAN_POINT('Ctrl Pts',(-23.0638014943553,12.9221001567719,
129.362835947955)) ;
#139419 = CARTESIAN_POINT('Ctrl Pts',(-23.0207283179547,13.1741319901515,
129.270237886939)) ;
#139420 = CARTESIAN_POINT('Ctrl Pts',(-23.0005908899832,13.44270233198,129.244466406606)) ;
#139421 = CARTESIAN_POINT('Ctrl Pts',(-23.0038914292178,13.7107857110311,
129.287286348237)) ;
#139422 = CARTESIAN_POINT('Ctrl Pts',(-23.0295704967675,13.9568883161136,
129.395289261901)) ;
#139423 = CARTESIAN_POINT('Ctrl Pts',(-23.0752731994709,14.1661036759461,
129.561958208576)) ;
#139424 = CARTESIAN_POINT('Ctrl Pts',(-23.1370402944096,14.3219385035442,
129.77557262833)) ;
#139425 = CARTESIAN_POINT('Ctrl Pts',(-23.2093871602734,14.4130180760167,
130.019993869871)) ;
#139426 = CARTESIAN_POINT('Ctrl Pts',(-23.2867565065069,14.4335349357277,
130.279148804425)) ;
#139427 = CARTESIAN_POINT('Ctrl Pts',(-23.3629698219185,14.3810414404785,
130.535040474928)) ;
#139428 = CARTESIAN_POINT('Ctrl Pts',(-23.4310082584103,14.2609491196068,
130.766748403059)) ;
#139429 = CARTESIAN_POINT('Ctrl Pts',(-23.4864209908859,14.0795344573349,
130.961883840188)) ;
#139430 = CARTESIAN_POINT('Ctrl Pts',(-23.5236051645126,13.8529284696564,
131.103464693403)) ;
#139431 = CARTESIAN_POINT('Ctrl Pts',(-23.5397921027113,13.5926908131845,
131.184105008777)) ;
#139432 = CARTESIAN_POINT('Ctrl Pts',(-23.5326550813306,13.3230678960584,
131.196241501053)) ;
#139433 = CARTESIAN_POINT('Ctrl Pts',(-23.5022844153317,13.0595445585026,
131.140642603212)) ;
#139434 = CARTESIAN_POINT('Ctrl Pts',(-23.4497773248406,12.8214089952354,
131.020469155132)) ;
#139435 = CARTESIAN_POINT('Ctrl Pts',(-23.3784016727207,12.6270968112276,
130.845114797372)) ;
#139436 = CARTESIAN_POINT('Ctrl Pts',(-23.293155678087,12.4904302156697,130.629020094481)) ;
#139437 = CARTESIAN_POINT('Ctrl Pts',(-23.1981211422612,12.4195264236209,
130.384598565288)) ;
#139438 = CARTESIAN_POINT('Ctrl Pts',(-23.1004341639123,12.4206997898043,
130.132284603727)) ;
#139439 = CARTESIAN_POINT('Ctrl Pts',(-23.0054798051943,12.4940151271389,
129.888140448463)) ;
#139440 = CARTESIAN_POINT('Ctrl Pts',(-22.9204783126155,12.6331734144625,
129.672828862818)) ;
#139441 = CARTESIAN_POINT('Ctrl Pts',(-22.8497361514307,12.829325604419,129.499320879608)) ;
#139442 = CARTESIAN_POINT('Ctrl Pts',(-22.798050247268,13.0683012054675,129.381494346922)) ;
#139443 = CARTESIAN_POINT('Ctrl Pts',(-22.7684338481907,13.332296684324,129.328087201503)) ;
#139444 = CARTESIAN_POINT('Ctrl Pts',(-22.7621646024436,13.6026349235875,
129.342864411698)) ;
#139445 = CARTESIAN_POINT('Ctrl Pts',(-22.7789878211364,13.8605088298962,
129.425147516842)) ;
#139446 = CARTESIAN_POINT('Ctrl Pts',(-22.8170651937567,14.0871784145907,
129.569548535915)) ;
#139447 = CARTESIAN_POINT('Ctrl Pts',(-22.8727752484208,14.2658344085649,
129.765391197157)) ;
#139448 = CARTESIAN_POINT('Ctrl Pts',(-22.9415251904135,14.3843789538156,
129.999358621862)) ;
#139449 = CARTESIAN_POINT('Ctrl Pts',(-23.0177762015768,14.4339734253515,
130.255296131666)) ;
#139450 = CARTESIAN_POINT('Ctrl Pts',(-23.0948641012711,14.4110559285979,
130.513542055004)) ;
#139451 = CARTESIAN_POINT('Ctrl Pts',(-23.1669334987967,14.3178925023023,
130.757135194731)) ;
#139452 = CARTESIAN_POINT('Ctrl Pts',(-23.228418635195,14.159368658012,130.970043928164)) ;
#139453 = CARTESIAN_POINT('Ctrl Pts',(-23.2732913315262,13.9496805303502,
131.134118565758)) ;
#139454 = CARTESIAN_POINT('Ctrl Pts',(-23.2984065123964,13.7013469975745,
131.240648353173)) ;
#139455 = CARTESIAN_POINT('Ctrl Pts',(-23.3008248756517,13.433016471187,131.280867680268)) ;
#139456 = CARTESIAN_POINT('Ctrl Pts',(-23.2798782812281,13.1647607687427,
131.252731738856)) ;
#139457 = CARTESIAN_POINT('Ctrl Pts',(-23.2359949776677,12.9137311981176,
131.157770408831)) ;
#139458 = CARTESIAN_POINT('Ctrl Pts',(-23.1722216632218,12.7007529774686,
131.004465052763)) ;
#139459 = CARTESIAN_POINT('Ctrl Pts',(-23.0916116499635,12.5383275935417,
130.802181669735)) ;
#139460 = CARTESIAN_POINT('Ctrl Pts',(-23.0000201461418,12.4398166133593,
130.567648814099)) ;
#139461 = CARTESIAN_POINT('Ctrl Pts',(-22.9021029447549,12.4114725012227,
130.314910430739)) ;
#139462 = CARTESIAN_POINT('Ctrl Pts',(-22.8056557366078,12.4557968893907,
130.066198456197)) ;
#139463 = CARTESIAN_POINT('Ctrl Pts',(-22.7157297205741,12.5696290859636,
129.836683815397)) ;
#139464 = CARTESIAN_POINT('Ctrl Pts',(-22.638835956155,12.7436129416571,129.645045220832)) ;
#139465 = CARTESIAN_POINT('Ctrl Pts',(-22.5787413628733,12.9681022420836,
129.502789849415)) ;
#139466 = CARTESIAN_POINT('Ctrl Pts',(-22.5400609169273,13.2239471204996,
129.422880231678)) ;
#139467 = CARTESIAN_POINT('Ctrl Pts',(-22.5243053598294,13.4941632666535,
129.40996844027)) ;
#139468 = CARTESIAN_POINT('Ctrl Pts',(-22.5319445480063,13.7589186275191,
129.465347966808)) ;
#139469 = CARTESIAN_POINT('Ctrl Pts',(-22.561653260686,13.9998348960523,129.585215768084)) ;
#139470 = CARTESIAN_POINT('Ctrl Pts',(-22.6106809695864,14.1997646334102,
129.761559980421)) ;
#139471 = CARTESIAN_POINT('Ctrl Pts',(-22.6748483134623,14.3442637107108,
129.982171105828)) ;
#139472 = CARTESIAN_POINT('Ctrl Pts',(-22.7488620893119,14.4224928337565,
130.231582338807)) ;
#139473 = CARTESIAN_POINT('Ctrl Pts',(-22.826082224651,14.4291711137562,130.490143364531)) ;
#139474 = CARTESIAN_POINT('Ctrl Pts',(-22.901385737979,14.3636108814792,130.743388063258)) ;
#139475 = CARTESIAN_POINT('Ctrl Pts',(-22.9676523282968,14.2305641375214,
130.970092092409)) ;
#139476 = CARTESIAN_POINT('Ctrl Pts',(-23.0196303198745,14.0406275620916,
131.154938240201)) ;
#139477 = CARTESIAN_POINT('Ctrl Pts',(-23.0532662084991,13.8058699764793,
131.286324556169)) ;
#139478 = CARTESIAN_POINT('Ctrl Pts',(-23.0651158799014,13.5427808202944,
131.354170447612)) ;
#139479 = CARTESIAN_POINT('Ctrl Pts',(-23.0535903902688,13.2720605312769,
131.353608556185)) ;
#139480 = CARTESIAN_POINT('Ctrl Pts',(-23.0188074569815,13.0118429090763,
131.285152168977)) ;
#139481 = CARTESIAN_POINT('Ctrl Pts',(-22.9627783979762,12.7818788170933,
131.154510248436)) ;
#139482 = CARTESIAN_POINT('Ctrl Pts',(-22.8883678106929,12.5968716626886,
130.97030840387)) ;
#139483 = CARTESIAN_POINT('Ctrl Pts',(-22.8002450416258,12.4712517214802,
130.74607696204)) ;
#139484 = CARTESIAN_POINT('Ctrl Pts',(-22.7044504660725,12.4142247969978,
130.499321626759)) ;
#139485 = CARTESIAN_POINT('Ctrl Pts',(-22.6069179691138,12.4291610418386,
130.247458381608)) ;
#139486 = CARTESIAN_POINT('Ctrl Pts',(-22.513489094124,12.5152749541959,130.007682466883)) ;
#139487 = CARTESIAN_POINT('Ctrl Pts',(-22.4303075741883,12.6672522382755,
129.797931174508)) ;
#139488 = CARTESIAN_POINT('Ctrl Pts',(-22.3633981184116,12.8714563581182,
129.63539167814)) ;
#139489 = CARTESIAN_POINT('Ctrl Pts',(-22.315632303497,13.1164156516164,129.529009838952)) ;
#139490 = CARTESIAN_POINT('Ctrl Pts',(-22.2903146188003,13.3833143712004,
129.48818130268)) ;
#139491 = CARTESIAN_POINT('Ctrl Pts',(-22.2885211433467,13.6536761659143,
129.516158189572)) ;
#139492 = CARTESIAN_POINT('Ctrl Pts',(-22.309526188747,13.9063303611245,129.610570446142)) ;
#139493 = CARTESIAN_POINT('Ctrl Pts',(-22.3514235054152,14.1256565202968,
129.766227676016)) ;
#139494 = CARTESIAN_POINT('Ctrl Pts',(-22.4097256575423,14.2929703983871,
129.969486284481)) ;
#139495 = CARTESIAN_POINT('Ctrl Pts',(-22.4805872320115,14.3994043107509,
130.20975186399)) ;
#139496 = CARTESIAN_POINT('Ctrl Pts',(-22.5572422571753,14.4351253202345,
130.466735869076)) ;
#139497 = CARTESIAN_POINT('Ctrl Pts',(-22.6339302437926,14.3988243968592,
130.723845624362)) ;
#139498 = CARTESIAN_POINT('Ctrl Pts',(-22.7045413583506,14.2923293351463,
130.963281578582)) ;
#139499 = CARTESIAN_POINT('Ctrl Pts',(-22.7629217549356,14.1241731231248,
131.166869003256)) ;
#139500 = CARTESIAN_POINT('Ctrl Pts',(-22.8045864477495,13.9051614017352,
131.321752941675)) ;
#139501 = CARTESIAN_POINT('Ctrl Pts',(-22.8255003662911,13.6518311474299,
131.415971687488)) ;
#139502 = CARTESIAN_POINT('Ctrl Pts',(-22.8235852848836,13.3824708815404,
131.44346252415)) ;
#139503 = CARTESIAN_POINT('Ctrl Pts',(-22.7981865474188,13.1154253424266,
131.402424540592)) ;
#139504 = CARTESIAN_POINT('Ctrl Pts',(-22.7503632246924,12.870532663978,131.295871230707)) ;
#139505 = CARTESIAN_POINT('Ctrl Pts',(-22.6829455920271,12.6655370974074,
131.132034154533)) ;
#139506 = CARTESIAN_POINT('Ctrl Pts',(-22.5999279586424,12.5146112418993,
130.922645471943)) ;
#139507 = CARTESIAN_POINT('Ctrl Pts',(-22.5064782959341,12.4289101941166,
130.682807596149)) ;
#139508 = CARTESIAN_POINT('Ctrl Pts',(-22.4090728608906,12.414189670065,130.431264713762)) ;
#139509 = CARTESIAN_POINT('Ctrl Pts',(-22.312528515273,12.4724108557129,130.182598671296)) ;
#139510 = CARTESIAN_POINT('Ctrl Pts',(-22.225209279529,12.5978142142,129.960457180624)) ;
#139511 = CARTESIAN_POINT('Ctrl Pts',(-22.1509137345901,12.7826551877608,
129.776554350212)) ;
#139512 = CARTESIAN_POINT('Ctrl Pts',(-22.0948479657602,13.0133814811485,
129.645883919566)) ;
#139513 = CARTESIAN_POINT('Ctrl Pts',(-22.0601691205954,13.2742168699271,
129.577789609753)) ;
#139514 = CARTESIAN_POINT('Ctrl Pts',(-22.0488678992467,13.5450314863386,
129.577894446666)) ;
#139515 = CARTESIAN_POINT('Ctrl Pts',(-22.0608042409464,13.8067211996107,
129.645832849942)) ;
#139516 = CARTESIAN_POINT('Ctrl Pts',(-22.094434022848,14.041251301363,129.77717692661)) ;
#139517 = CARTESIAN_POINT('Ctrl Pts',(-22.1467135744848,14.2318697191873,
129.963049851365)) ;
#139518 = CARTESIAN_POINT('Ctrl Pts',(-22.2133209230258,14.3645253073145,
130.190851488341)) ;
#139519 = CARTESIAN_POINT('Ctrl Pts',(-22.2880127253032,14.4291513748126,
130.442024637572)) ;
#139520 = CARTESIAN_POINT('Ctrl Pts',(-22.3656045332651,14.4223448235858,
130.701832829083)) ;
#139521 = CARTESIAN_POINT('Ctrl Pts',(-22.4395795352273,14.3433928337176,
130.951141721303)) ;
#139522 = CARTESIAN_POINT('Ctrl Pts',(-22.5034115118926,14.1993297551337,
131.170623731226)) ;
#139523 = CARTESIAN_POINT('Ctrl Pts',(-22.5524972774972,13.9988090626419,
131.347214932239)) ;
#139524 = CARTESIAN_POINT('Ctrl Pts',(-22.5821223537297,13.7578101990109,
131.46682648151)) ;
#139525 = CARTESIAN_POINT('Ctrl Pts',(-22.5896179033506,13.4916491318397,
131.521951897713)) ;
#139526 = CARTESIAN_POINT('Ctrl Pts',(-22.5737359732877,13.2223243547225,
131.50855985098)) ;
#139527 = CARTESIAN_POINT('Ctrl Pts',(-22.5347221915636,12.9657468918016,
131.42780367239)) ;
#139528 = CARTESIAN_POINT('Ctrl Pts',(-22.4748529861467,12.7429296801426,
131.286000068107)) ;
#139529 = CARTESIAN_POINT('Ctrl Pts',(-22.3976682749232,12.5685157240841,
131.093622742732)) ;
#139530 = CARTESIAN_POINT('Ctrl Pts',(-22.3073711104087,12.4549912685616,
130.863119792323)) ;
#139531 = CARTESIAN_POINT('Ctrl Pts',(-22.2111174959793,12.4115665135432,
130.61489744185)) ;
#139532 = CARTESIAN_POINT('Ctrl Pts',(-22.1137558357218,12.4399153694957,
130.363592894185)) ;
#139533 = CARTESIAN_POINT('Ctrl Pts',(-22.0216969019763,12.539266271838,130.12788037676)) ;
#139534 = CARTESIAN_POINT('Ctrl Pts',(-21.9414381676257,12.7015765311082,
129.926512602715)) ;
#139535 = CARTESIAN_POINT('Ctrl Pts',(-21.8776532898284,12.9151235328842,
129.773233982734)) ;
#139536 = CARTESIAN_POINT('Ctrl Pts',(-21.8339664362384,13.1655123669942,
129.67874406302)) ;
#139537 = CARTESIAN_POINT('Ctrl Pts',(-21.8130201904645,13.4357073087156,
129.650843568944)) ;
#139538 = CARTESIAN_POINT('Ctrl Pts',(-21.8156809926834,13.7027427371582,
129.69162438137)) ;
#139539 = CARTESIAN_POINT('Ctrl Pts',(-21.8407512524161,13.9504288241065,
129.79794042058)) ;
#139540 = CARTESIAN_POINT('Ctrl Pts',(-21.8859845993865,14.1608970997243,
129.963242481406)) ;
#139541 = CARTESIAN_POINT('Ctrl Pts',(-21.9472402348266,14.3182076621176,
130.175305086424)) ;
#139542 = CARTESIAN_POINT('Ctrl Pts',(-22.0194714930934,14.4114239711584,
130.41944123239)) ;
#139543 = CARTESIAN_POINT('Ctrl Pts',(-22.0966325897837,14.4338711426872,
130.677924220104)) ;
#139544 = CARTESIAN_POINT('Ctrl Pts',(-22.1727955150631,14.3839736341,130.933575234531)) ;
#139545 = CARTESIAN_POINT('Ctrl Pts',(-22.2415712312017,14.2649033849915,
131.167660198233)) ;
#139546 = CARTESIAN_POINT('Ctrl Pts',(-22.2971026553746,14.0862373314476,
131.362925300438)) ;
#139547 = CARTESIAN_POINT('Ctrl Pts',(-22.3350972412815,13.8593709680806,
131.507089720524)) ;
#139548 = CARTESIAN_POINT('Ctrl Pts',(-22.3518156453636,13.6016402175067,
131.589035604686)) ;
#139549 = CARTESIAN_POINT('Ctrl Pts',(-22.3454434205743,13.3309241263673,
131.603556996775)) ;
#139550 = CARTESIAN_POINT('Ctrl Pts',(-22.3156922828301,13.0670233439019,
131.549755470883)) ;
#139551 = CARTESIAN_POINT('Ctrl Pts',(-22.2640083916553,12.8286261810775,
131.431877786345)) ;
#139552 = CARTESIAN_POINT('Ctrl Pts',(-22.1932065591499,12.6324569131355,
131.258208090831)) ;
#139553 = CARTESIAN_POINT('Ctrl Pts',(-22.1077589751913,12.4932133607205,
131.041732099059)) ;
#139554 = CARTESIAN_POINT('Ctrl Pts',(-22.0133476243497,12.4206918149119,
130.798970751027)) ;
#139555 = CARTESIAN_POINT('Ctrl Pts',(-21.9153477521299,12.4196226732146,
130.545851858096)) ;
#139556 = CARTESIAN_POINT('Ctrl Pts',(-21.8202845535771,12.4910154919702,
130.301366419668)) ;
#139557 = CARTESIAN_POINT('Ctrl Pts',(-21.7349087576259,12.6283739750249,
130.084970327283)) ;
#139558 = CARTESIAN_POINT('Ctrl Pts',(-21.6635187562755,12.8237069279728,
129.909657715924)) ;
#139559 = CARTESIAN_POINT('Ctrl Pts',(-21.6113756355089,13.0616748954868,
129.790472154327)) ;
#139560 = CARTESIAN_POINT('Ctrl Pts',(-21.5812201320458,13.3240382203917,
129.735346429805)) ;
#139561 = CARTESIAN_POINT('Ctrl Pts',(-21.5742019181363,13.5952493651547,
129.748031247665)) ;
#139562 = CARTESIAN_POINT('Ctrl Pts',(-21.5905171574251,13.8544594901405,
129.828928472972)) ;
#139563 = CARTESIAN_POINT('Ctrl Pts',(-21.6280422230899,14.0816539575776,
129.971653631214)) ;
#139564 = CARTESIAN_POINT('Ctrl Pts',(-21.6831210640629,14.2612879852104,
130.165544817405)) ;
#139565 = CARTESIAN_POINT('Ctrl Pts',(-21.7515285398232,14.3817634357603,
130.39850167849)) ;
#139566 = CARTESIAN_POINT('Ctrl Pts',(-21.8276692424797,14.4336477356996,
130.654125167946)) ;
#139567 = CARTESIAN_POINT('Ctrl Pts',(-21.9052481328329,14.4124733910525,
130.913995427691)) ;
#139568 = CARTESIAN_POINT('Ctrl Pts',(-21.9771206529507,14.3214777368465,
131.15683461577)) ;
#139569 = CARTESIAN_POINT('Ctrl Pts',(-22.0389770924245,14.1652192493521,
131.370776987055)) ;
#139570 = CARTESIAN_POINT('Ctrl Pts',(-22.0845865752622,13.9555650304119,
131.537191449783)) ;
#139571 = CARTESIAN_POINT('Ctrl Pts',(-22.110142037256,13.7095599623908,131.644803567879)) ;
#139572 = CARTESIAN_POINT('Ctrl Pts',(-22.1133412911239,13.4405995094296,
131.68742540987)) ;
#139573 = CARTESIAN_POINT('Ctrl Pts',(-22.0928739407392,13.1715077447804,
131.660770291061)) ;
#139574 = CARTESIAN_POINT('Ctrl Pts',(-22.0500042324198,12.9214880554527,
131.568517539565)) ;
#139575 = CARTESIAN_POINT('Ctrl Pts',(-21.986272283684,12.7055052925361,131.415601528427)) ;
#139576 = CARTESIAN_POINT('Ctrl Pts',(-21.9065002297074,12.5425196617187,
131.21556628128)) ;
#139577 = CARTESIAN_POINT('Ctrl Pts',(-21.8149731081815,12.4416160239473,
130.981304047927)) ;
#139578 = CARTESIAN_POINT('Ctrl Pts',(-21.717050858099,12.4112449647392,130.728571243266)) ;
#139579 = CARTESIAN_POINT('Ctrl Pts',(-21.6204243758217,12.4537097217899,
130.479366405329)) ;
#139580 = CARTESIAN_POINT('Ctrl Pts',(-21.5305167877764,12.5652232795711,
130.249790618881)) ;
#139581 = CARTESIAN_POINT('Ctrl Pts',(-21.4530181437376,12.7379440224027,
130.056458295685)) ;
#139582 = CARTESIAN_POINT('Ctrl Pts',(-21.3925676750595,12.960397453185,129.91304056417)) ;
#139583 = CARTESIAN_POINT('Ctrl Pts',(-21.3531347639013,13.2156634821883,
129.830962045719)) ;
#139584 = CARTESIAN_POINT('Ctrl Pts',(-21.336634573283,13.4857933764674,129.815880746042)) ;
#139585 = CARTESIAN_POINT('Ctrl Pts',(-21.343632936242,13.7522946438347,129.869550437587)) ;
#139586 = CARTESIAN_POINT('Ctrl Pts',(-21.372925446852,13.9943544460531,129.988260551423)) ;
#139587 = CARTESIAN_POINT('Ctrl Pts',(-21.4212369628702,14.1947046175958,
130.162353989947)) ;
#139588 = CARTESIAN_POINT('Ctrl Pts',(-21.4853334805668,14.3414529387325,
130.382901794377)) ;
#139589 = CARTESIAN_POINT('Ctrl Pts',(-21.5587948401416,14.4211243068953,
130.630528130011)) ;
#139590 = CARTESIAN_POINT('Ctrl Pts',(-21.6361524176439,14.4300014348132,
130.889562555299)) ;
#139591 = CARTESIAN_POINT('Ctrl Pts',(-21.7114727530929,14.3664765738552,
131.142795185518)) ;
#139592 = CARTESIAN_POINT('Ctrl Pts',(-21.778029101135,14.235605243378,131.370308686837)) ;
#139593 = CARTESIAN_POINT('Ctrl Pts',(-21.8307071352233,14.0463420855303,
131.5573397721)) ;
#139594 = CARTESIAN_POINT('Ctrl Pts',(-21.8647984605866,13.8127312117544,
131.690021475908)) ;
#139595 = CARTESIAN_POINT('Ctrl Pts',(-21.8773121091469,13.5514861581268,
131.759647215842)) ;
#139596 = CARTESIAN_POINT('Ctrl Pts',(-21.8664659862452,13.2797431877816,
131.761195196609)) ;
#139597 = CARTESIAN_POINT('Ctrl Pts',(-21.8324447030282,13.0196141695931,
131.694872542692)) ;
#139598 = CARTESIAN_POINT('Ctrl Pts',(-21.7768285980867,12.7876902143184,
131.565555325081)) ;
#139599 = CARTESIAN_POINT('Ctrl Pts',(-21.7029455016982,12.6015317639528,
131.382848114673)) ;
#139600 = CARTESIAN_POINT('Ctrl Pts',(-21.6154214666389,12.4742597537388,
131.160271970459)) ;
#139601 = CARTESIAN_POINT('Ctrl Pts',(-21.5196623512914,12.4148459760243,
130.913664546399)) ;
#139602 = CARTESIAN_POINT('Ctrl Pts',(-21.4218298173218,12.4277168050886,
130.661011819284)) ;
#139603 = CARTESIAN_POINT('Ctrl Pts',(-21.3282883705838,12.5119511552026,
130.420881834853)) ;
#139604 = CARTESIAN_POINT('Ctrl Pts',(-21.2450319287907,12.6612550924709,
130.210764914545)) ;
#139605 = CARTESIAN_POINT('Ctrl Pts',(-21.1771167844571,12.8654797795072,
130.045522770625)) ;
#139606 = CARTESIAN_POINT('Ctrl Pts',(-21.1289599445452,13.1088715817203,
129.937890486847)) ;
#139607 = CARTESIAN_POINT('Ctrl Pts',(-21.1029409415662,13.3752798847283,
129.89500636968)) ;
#139608 = CARTESIAN_POINT('Ctrl Pts',(-21.100441405058,13.6458119983222,129.920912628984)) ;
#139609 = CARTESIAN_POINT('Ctrl Pts',(-21.1208585860571,13.899465813918,130.013650363731)) ;
#139610 = CARTESIAN_POINT('Ctrl Pts',(-21.1619780714701,14.1192748992269,
130.166896304245)) ;
#139611 = CARTESIAN_POINT('Ctrl Pts',(-21.2201580360466,14.2891803091472,
130.369981381548)) ;
#139612 = CARTESIAN_POINT('Ctrl Pts',(-21.2904289832578,14.3970324953894,
130.60836272282)) ;
#139613 = CARTESIAN_POINT('Ctrl Pts',(-21.3671416455221,14.4351164741298,
130.865591429488)) ;
#139614 = CARTESIAN_POINT('Ctrl Pts',(-21.4438538638505,14.4010787684845,
131.122734088588)) ;
#139615 = CARTESIAN_POINT('Ctrl Pts',(-21.5151288839755,14.2958209248288,
131.364304880692)) ;
#139616 = CARTESIAN_POINT('Ctrl Pts',(-21.5736633584408,14.129652176779,131.568224656794)) ;
#139617 = CARTESIAN_POINT('Ctrl Pts',(-21.6158674833682,13.912176140122,131.72465380531)) ;
#139618 = CARTESIAN_POINT('Ctrl Pts',(-21.6374100082649,13.6594303550192,
131.820730010105)) ;
#139619 = CARTESIAN_POINT('Ctrl Pts',(-21.6362376323324,13.3906473187371,
131.850341742612)) ;
#139620 = CARTESIAN_POINT('Ctrl Pts',(-21.6112596121911,13.1215485791247,
131.810753715866)) ;
#139621 = CARTESIAN_POINT('Ctrl Pts',(-21.5643253393536,12.877499502744,131.706566930706)) ;
#139622 = CARTESIAN_POINT('Ctrl Pts',(-21.4971489276021,12.6702279580221,
131.543581214665)) ;
#139623 = CARTESIAN_POINT('Ctrl Pts',(-21.4148278562299,12.5183910541011,
131.336084599909)) ;
#139624 = CARTESIAN_POINT('Ctrl Pts',(-21.321592793567,12.4302683160369,131.096887067683)) ;
#139625 = CARTESIAN_POINT('Ctrl Pts',(-21.2235235030194,12.4138255854832,
130.84364383687)) ;
#139626 = CARTESIAN_POINT('Ctrl Pts',(-21.1280462202582,12.4692849661908,
130.59767471953)) ;
#139627 = CARTESIAN_POINT('Ctrl Pts',(-21.0397782209746,12.5930868189149,
130.372972296455)) ;
#139628 = CARTESIAN_POINT('Ctrl Pts',(-20.9648900702745,12.7771359268665,
130.187423563488)) ;
#139629 = CARTESIAN_POINT('Ctrl Pts',(-20.9084604382932,13.0059649491312,
130.055574675109)) ;
#139630 = CARTESIAN_POINT('Ctrl Pts',(-20.8730855953741,13.2661471501604,
129.98544681023)) ;
#139631 = CARTESIAN_POINT('Ctrl Pts',(-20.8610654562158,13.536990610461,129.983456526969)) ;
#139632 = CARTESIAN_POINT('Ctrl Pts',(-20.8723871827311,13.7997448803438,
130.049673265163)) ;
#139633 = CARTESIAN_POINT('Ctrl Pts',(-20.90538067581,14.0350783455638,130.179115882773)) ;
#139634 = CARTESIAN_POINT('Ctrl Pts',(-20.9574456253222,14.2276700912271,
130.364492989564)) ;
#139635 = CARTESIAN_POINT('Ctrl Pts',(-21.0230849241156,14.3610390987627,
130.589154695541)) ;
#139636 = CARTESIAN_POINT('Ctrl Pts',(-21.0982174668606,14.4285213562849,
130.841897239005)) ;
#139637 = CARTESIAN_POINT('Ctrl Pts',(-21.1756599652311,14.4233691506753,
131.10119816308)) ;
#139638 = CARTESIAN_POINT('Ctrl Pts',(-21.2496325844285,14.3469900608794,
131.35039585002)) ;
#139639 = CARTESIAN_POINT('Ctrl Pts',(-21.3142670386072,14.2034039826352,
131.572477885729)) ;
#139640 = CARTESIAN_POINT('Ctrl Pts',(-21.3634585175808,14.0056848042437,
131.749124315029)) ;
#139641 = CARTESIAN_POINT('Ctrl Pts',(-21.3938254756421,13.7644935379873,
131.87107326449)) ;
#139642 = CARTESIAN_POINT('Ctrl Pts',(-21.4019773023267,13.5002463759362,
131.927919962956)) ;
#139643 = CARTESIAN_POINT('Ctrl Pts',(-21.3865652696606,13.2284058241885,
131.916205863608)) ;
#139644 = CARTESIAN_POINT('Ctrl Pts',(-21.3485619428079,12.9739037522761,
131.838041629857)) ;
#139645 = CARTESIAN_POINT('Ctrl Pts',(-21.2890019447558,12.7484704180283,
131.697336737727)) ;
#139646 = CARTESIAN_POINT('Ctrl Pts',(-21.212476706466,12.5731123279677,131.506773572971)) ;
#139647 = CARTESIAN_POINT('Ctrl Pts',(-21.1224208921965,12.45735908031,131.277009163557)) ;
#139648 = CARTESIAN_POINT('Ctrl Pts',(-21.0261799251125,12.4118025440313,
131.028854605153)) ;
#139649 = CARTESIAN_POINT('Ctrl Pts',(-20.9287286020676,12.4381298273325,
130.777298657297)) ;
#139650 = CARTESIAN_POINT('Ctrl Pts',(-20.8365847097189,12.5352056627263,
130.541271205423)) ;
#139651 = CARTESIAN_POINT('Ctrl Pts',(-20.7556872818817,12.696300610242,130.338138236175)) ;
#139652 = CARTESIAN_POINT('Ctrl Pts',(-20.6914131973187,12.9082756113126,
130.183386414941)) ;
#139653 = CARTESIAN_POINT('Ctrl Pts',(-20.6469587597595,13.1596325323724,
130.086874818099)) ;
#139654 = CARTESIAN_POINT('Ctrl Pts',(-20.6256126189791,13.4259468835544,
130.057354385986)) ;
#139655 = CARTESIAN_POINT('Ctrl Pts',(-20.6274509190732,13.6953761011822,
130.095991058217)) ;
#139656 = CARTESIAN_POINT('Ctrl Pts',(-20.6519544165665,13.9437170252716,
130.20062924795)) ;
#139657 = CARTESIAN_POINT('Ctrl Pts',(-20.6967040257505,14.155711083142,130.364556823473)) ;
#139658 = CARTESIAN_POINT('Ctrl Pts',(-20.7574637860279,14.3144000216169,
130.575108733115)) ;
#139659 = CARTESIAN_POINT('Ctrl Pts',(-20.8294247939273,14.4096307873655,
130.818448393621)) ;
#139660 = CARTESIAN_POINT('Ctrl Pts',(-20.9065511570391,14.4343455413494,
131.076836805641)) ;
#139661 = CARTESIAN_POINT('Ctrl Pts',(-20.9831483409494,14.3860725328483,
131.333902273055)) ;
#139662 = CARTESIAN_POINT('Ctrl Pts',(-21.0518273806318,14.2695097224109,
131.567514159987)) ;
#139663 = CARTESIAN_POINT('Ctrl Pts',(-21.1080343518942,14.0917907818256,
131.764885399557)) ;
#139664 = CARTESIAN_POINT('Ctrl Pts',(-21.1464563378518,13.8666927390169,
131.910195855888)) ;
#139665 = CARTESIAN_POINT('Ctrl Pts',(-21.1638741215799,13.6093228948058,
131.994229909567)) ;
#139666 = CARTESIAN_POINT('Ctrl Pts',(-21.1581778671763,13.3388432041032,
132.010707129866)) ;
#139667 = CARTESIAN_POINT('Ctrl Pts',(-21.1290589624462,13.0740474373603,
131.958804416506)) ;
#139668 = CARTESIAN_POINT('Ctrl Pts',(-21.0778095064892,12.8343946472962,
131.842251800914)) ;
#139669 = CARTESIAN_POINT('Ctrl Pts',(-21.0078504214422,12.6378259475901,
131.670874797454)) ;
#139670 = CARTESIAN_POINT('Ctrl Pts',(-20.9227635942453,12.4964630119009,
131.455470160856)) ;
#139671 = CARTESIAN_POINT('Ctrl Pts',(-20.8282781982489,12.421725405798,131.212580208633)) ;
#139672 = CARTESIAN_POINT('Ctrl Pts',(-20.7303861760134,12.4187226198539,
130.959743948979)) ;
#139673 = CARTESIAN_POINT('Ctrl Pts',(-20.635461865384,12.4875916518615,130.715545608703)) ;
#139674 = CARTESIAN_POINT('Ctrl Pts',(-20.5493919591687,12.6235712310503,
130.49725175219)) ;
#139675 = CARTESIAN_POINT('Ctrl Pts',(-20.4777829693133,12.8167007524725,
130.321173584195)) ;
#139676 = CARTESIAN_POINT('Ctrl Pts',(-20.424910899171,13.053470084932,130.199863474853)) ;
#139677 = CARTESIAN_POINT('Ctrl Pts',(-20.3939411324719,13.3166529719994,
130.14252162574)) ;
#139678 = CARTESIAN_POINT('Ctrl Pts',(-20.3863238911027,13.5871781568045,
130.153366237627)) ;
#139679 = CARTESIAN_POINT('Ctrl Pts',(-20.4018167783541,13.8461110281262,
130.231734054356)) ;
#139680 = CARTESIAN_POINT('Ctrl Pts',(-20.4388065892668,14.0754123142472,
130.373009889351)) ;
#139681 = CARTESIAN_POINT('Ctrl Pts',(-20.49356997314,14.2569965366052,130.566053917608)) ;
#139682 = CARTESIAN_POINT('Ctrl Pts',(-20.5616742400838,14.3792169308405,
130.798118874428)) ;
#139683 = CARTESIAN_POINT('Ctrl Pts',(-20.6374555012612,14.4330645765252,
131.052596497103)) ;
#139684 = CARTESIAN_POINT('Ctrl Pts',(-20.7150727128244,14.4142942137405,
131.312571329954)) ;
#139685 = CARTESIAN_POINT('Ctrl Pts',(-20.7874772612268,14.3249818640555,
131.557095540597)) ;
#139686 = CARTESIAN_POINT('Ctrl Pts',(-20.8497107932074,14.1700409450456,
131.772170241937)) ;
#139687 = CARTESIAN_POINT('Ctrl Pts',(-20.8956340065545,13.9629928904563,
131.939314582627)) ;
#139688 = CARTESIAN_POINT('Ctrl Pts',(-20.9219601566609,13.716497244272,132.049365900883)) ;
#139689 = CARTESIAN_POINT('Ctrl Pts',(-20.9257864629784,13.449382384683,132.093627582631)) ;
#139690 = CARTESIAN_POINT('Ctrl Pts',(-20.9061009955916,13.179466012535,132.069323528848)) ;
#139691 = CARTESIAN_POINT('Ctrl Pts',(-20.8635521867842,12.9274139548691,
131.978183997817)) ;
#139692 = CARTESIAN_POINT('Ctrl Pts',(-20.8006998299117,12.7115777199899,
131.827639105462)) ;
#139693 = CARTESIAN_POINT('Ctrl Pts',(-20.7213500350591,12.5463884339408,
131.628868055719)) ;
#139694 = CARTESIAN_POINT('Ctrl Pts',(-20.6292985456697,12.4431786927595,
131.393338070779)) ;
#139695 = CARTESIAN_POINT('Ctrl Pts',(-20.5325248471645,12.4112124576001,
131.14359108722)) ;
#139696 = CARTESIAN_POINT('Ctrl Pts',(-20.4354101414637,12.4513454606681,
130.893090654114)) ;
#139697 = CARTESIAN_POINT('Ctrl Pts',(-20.3452469652715,12.5610016888449,
130.662758587929)) ;
#139698 = CARTESIAN_POINT('Ctrl Pts',(-20.2672178306558,12.7322315301459,
130.467913756268)) ;
#139699 = CARTESIAN_POINT('Ctrl Pts',(-20.2062037864739,12.9536821902703,
130.322869683321)) ;
#139700 = CARTESIAN_POINT('Ctrl Pts',(-20.1662123639624,13.2077095547012,
130.239091898145)) ;
#139701 = CARTESIAN_POINT('Ctrl Pts',(-20.1489841763445,13.4778389937593,
130.221903369639)) ;
#139702 = CARTESIAN_POINT('Ctrl Pts',(-20.1553409554788,13.7447250212435,
130.273702425957)) ;
#139703 = CARTESIAN_POINT('Ctrl Pts',(-20.1838475971167,13.9871379324524,
130.390012023778)) ;
#139704 = CARTESIAN_POINT('Ctrl Pts',(-20.2319890113485,14.1900736683291,
130.563825342734)) ;
#139705 = CARTESIAN_POINT('Ctrl Pts',(-20.2951088659413,14.3373317705726,
130.781206869708)) ;
#139706 = CARTESIAN_POINT('Ctrl Pts',(-20.3688107602542,14.4199335314477,
131.029762137696)) ;
#139707 = CARTESIAN_POINT('Ctrl Pts',(-20.446131773642,14.4307823932299,131.288673826951)) ;
#139708 = CARTESIAN_POINT('Ctrl Pts',(-20.5217929524515,14.3690285346023,
131.542993054621)) ;
#139709 = CARTESIAN_POINT('Ctrl Pts',(-20.5883871265995,14.2404409958973,
131.770478575448)) ;
#139710 = CARTESIAN_POINT('Ctrl Pts',(-20.6415813159015,14.0528076235366,
131.959023744489)) ;
#139711 = CARTESIAN_POINT('Ctrl Pts',(-20.6763112872876,13.8202655346865,
132.093577798832)) ;
#139712 = CARTESIAN_POINT('Ctrl Pts',(-20.6895096092303,13.5584444943241,
132.165343569218)) ;
#139713 = CARTESIAN_POINT('Ctrl Pts',(-20.6792615552115,13.2871050604655,
132.168588192677)) ;
#139714 = CARTESIAN_POINT('Ctrl Pts',(-20.6460046902205,13.0271136592546,
132.104408593774)) ;
#139715 = CARTESIAN_POINT('Ctrl Pts',(-20.590935829574,12.7938647968009,131.976722550481)) ;
#139716 = CARTESIAN_POINT('Ctrl Pts',(-20.517620628279,12.6063348260336,131.795635103324)) ;
#139717 = CARTESIAN_POINT('Ctrl Pts',(-20.4302806626542,12.4770287945195,
131.573651748548)) ;
#139718 = CARTESIAN_POINT('Ctrl Pts',(-20.3349577898321,12.4155889171301,
131.328220018841)) ;
#139719 = CARTESIAN_POINT('Ctrl Pts',(-20.2366487863863,12.4264045775595,
131.074330742108)) ;
#139720 = CARTESIAN_POINT('Ctrl Pts',(-20.1432359738446,12.5084012682064,
130.834454218698)) ;
#139721 = CARTESIAN_POINT('Ctrl Pts',(-20.0594324062122,12.6562045678091,
130.622810534766)) ;
#139722 = CARTESIAN_POINT('Ctrl Pts',(-19.9912068299662,12.8582528163381,
130.456544034109)) ;
#139723 = CARTESIAN_POINT('Ctrl Pts',(-19.9420895004565,13.1022480435351,
130.346320064404)) ;
#139724 = CARTESIAN_POINT('Ctrl Pts',(-19.9155609247342,13.3685511401161,
130.301969143821)) ;
#139725 = CARTESIAN_POINT('Ctrl Pts',(-19.9123931900497,13.6374690489365,
130.325704502981)) ;
#139726 = CARTESIAN_POINT('Ctrl Pts',(-19.9321748917974,13.8926337439443,
130.416683309371)) ;
#139727 = CARTESIAN_POINT('Ctrl Pts',(-19.9727272333172,14.1134973909665,
130.568248020198)) ;
#139728 = CARTESIAN_POINT('Ctrl Pts',(-20.030633868195,14.2854804526752,130.770621797177)) ;
#139729 = CARTESIAN_POINT('Ctrl Pts',(-20.1006583949635,14.3949169679371,
131.008278415634)) ;
#139730 = CARTESIAN_POINT('Ctrl Pts',(-20.1769463478651,14.4350950474159,
131.26412354158)) ;
#139731 = CARTESIAN_POINT('Ctrl Pts',(-20.2541792081547,14.4027523558799,
131.522987865141)) ;
#139732 = CARTESIAN_POINT('Ctrl Pts',(-20.3251151923492,14.3004224284984,
131.763273616136)) ;
#139733 = CARTESIAN_POINT('Ctrl Pts',(-20.3846198909271,14.1345848186711,
131.970325949278)) ;
#139734 = CARTESIAN_POINT('Ctrl Pts',(-20.4271315499746,13.9188292649382,
132.127540458863)) ;
#139735 = CARTESIAN_POINT('Ctrl Pts',(-20.4493383192168,13.6668968263447,
132.225559348984)) ;
#139736 = CARTESIAN_POINT('Ctrl Pts',(-20.4487750722731,13.3982258139503,
132.256962612225)) ;
#139737 = CARTESIAN_POINT('Ctrl Pts',(-20.424644928654,13.1299459979309,132.219701611108)) ;
#139738 = CARTESIAN_POINT('Ctrl Pts',(-20.3781183421514,12.8837060255956,
132.116878294644)) ;
#139739 = CARTESIAN_POINT('Ctrl Pts',(-20.3115284961441,12.6755091265604,
131.955551424455)) ;
#139740 = CARTESIAN_POINT('Ctrl Pts',(-20.2294351760645,12.5215778534682,
131.748786107997)) ;
#139741 = CARTESIAN_POINT('Ctrl Pts',(-20.1362346606042,12.4317802187368,
131.509743104052)) ;
#139742 = CARTESIAN_POINT('Ctrl Pts',(-20.0390583090231,12.4131805115513,
131.258818109629)) ;
#139743 = CARTESIAN_POINT('Ctrl Pts',(-19.9426649164388,12.4668842631246,
131.010444047681)) ;
#139744 = CARTESIAN_POINT('Ctrl Pts',(-19.8545070298818,12.5884450381112,
130.785909700319)) ;
#139745 = CARTESIAN_POINT('Ctrl Pts',(-19.7789377814184,12.7713420936062,
130.598465428946)) ;
#139746 = CARTESIAN_POINT('Ctrl Pts',(-19.7220015443685,12.9988617969997,
130.465098611114)) ;
#139747 = CARTESIAN_POINT('Ctrl Pts',(-19.6858986492706,13.2594913097142,
130.392975341362)) ;
#139748 = CARTESIAN_POINT('Ctrl Pts',(-19.6733337480537,13.5289133142041,
130.38922412671)) ;
#139749 = CARTESIAN_POINT('Ctrl Pts',(-19.6839091842483,13.7920447587741,
130.453239453652)) ;
#139750 = CARTESIAN_POINT('Ctrl Pts',(-19.7163423526536,14.028682332542,130.581083514188)) ;
#139751 = CARTESIAN_POINT('Ctrl Pts',(-19.7678307217928,14.2226477073875,
130.764735550547)) ;
#139752 = CARTESIAN_POINT('Ctrl Pts',(-19.8333291765721,14.358128004445,130.989083666605)) ;
#139753 = CARTESIAN_POINT('Ctrl Pts',(-19.9079226684156,14.427517223623,131.240089115873)) ;
#139754 = CARTESIAN_POINT('Ctrl Pts',(-19.9859801243066,14.4244373383238,
131.501449139126)) ;
#139755 = CARTESIAN_POINT('Ctrl Pts',(-20.0597164291861,14.3501368241958,
131.749777152345)) ;
#139756 = CARTESIAN_POINT('Ctrl Pts',(-20.1246192093162,14.2089998029508,
131.972568872511)) ;
#139757 = CARTESIAN_POINT('Ctrl Pts',(-20.1745043948321,14.0121251226583,
132.151352883394)) ;
#139758 = CARTESIAN_POINT('Ctrl Pts',(-20.205479708551,13.7718247542597,132.275085721787)) ;
#139759 = CARTESIAN_POINT('Ctrl Pts',(-20.2142480552375,13.5078187050463,
132.333759678721)) ;
#139760 = CARTESIAN_POINT('Ctrl Pts',(-20.1996711320823,13.2372789861246,
132.324307123579)) ;
#139761 = CARTESIAN_POINT('Ctrl Pts',(-20.1621297481922,12.9804327366812,
132.247703472472)) ;
#139762 = CARTESIAN_POINT('Ctrl Pts',(-20.103068138609,12.7540238900059,132.108444548132)) ;
#139763 = CARTESIAN_POINT('Ctrl Pts',(-20.0271058684499,12.577462748724,131.919470641086)) ;
#139764 = CARTESIAN_POINT('Ctrl Pts',(-19.9375506636755,12.4598742961996,
131.691099669398)) ;
#139765 = CARTESIAN_POINT('Ctrl Pts',(-19.8409928350901,12.4120040777539,
131.442168402122)) ;
#139766 = CARTESIAN_POINT('Ctrl Pts',(-19.7435371148839,12.4365719304023,
131.190583062223)) ;
#139767 = CARTESIAN_POINT('Ctrl Pts',(-19.6515284558936,12.5311793642618,
130.954812449025)) ;
#139768 = CARTESIAN_POINT('Ctrl Pts',(-19.5699202919936,12.6910252925006,
130.749716829182)) ;
#139769 = CARTESIAN_POINT('Ctrl Pts',(-19.5052958004438,12.901554601713,130.593894377772)) ;
#139770 = CARTESIAN_POINT('Ctrl Pts',(-19.4603082437547,13.1503193803292,
130.495615012924)) ;
#139771 = CARTESIAN_POINT('Ctrl Pts',(-19.4380452691141,13.4198238179189,
130.463850336133)) ;
#139772 = CARTESIAN_POINT('Ctrl Pts',(-19.4392649628103,13.6867201864748,
130.500325755553)) ;
#139773 = CARTESIAN_POINT('Ctrl Pts',(-19.4632228569756,13.9376559874792,
130.603602335536)) ;
#139774 = CARTESIAN_POINT('Ctrl Pts',(-19.5073954403515,14.1502428596578,
130.765749845655)) ;
#139775 = CARTESIAN_POINT('Ctrl Pts',(-19.5678164429334,14.3108380657866,
130.975357095169)) ;
#139776 = CARTESIAN_POINT('Ctrl Pts',(-19.63952920761,14.4079445311136,131.217958014036)) ;
#139777 = CARTESIAN_POINT('Ctrl Pts',(-19.7166714113582,14.4345276707165,
131.476430714807)) ;
#139778 = CARTESIAN_POINT('Ctrl Pts',(-19.7928752190649,14.3888298809399,
131.732116617467)) ;
#139779 = CARTESIAN_POINT('Ctrl Pts',(-19.862229218925,14.2738284878411,131.967870918754)) ;
#139780 = CARTESIAN_POINT('Ctrl Pts',(-19.9188081884538,14.0978368640531,
132.166288619942)) ;
#139781 = CARTESIAN_POINT('Ctrl Pts',(-19.9578752207231,13.8735407720446,
132.31354477898)) ;
#139782 = CARTESIAN_POINT('Ctrl Pts',(-19.9759059243398,13.616875079998,132.399358256203)) ;
#139783 = CARTESIAN_POINT('Ctrl Pts',(-19.9708726882155,13.3465064329097,
132.41777444154)) ;
#139784 = CARTESIAN_POINT('Ctrl Pts',(-19.9424497125854,13.0815408414728,
132.367868399297)) ;
#139785 = CARTESIAN_POINT('Ctrl Pts',(-19.8918146463953,12.8409647311381,
132.253107292745)) ;
#139786 = CARTESIAN_POINT('Ctrl Pts',(-19.8224365639408,12.642864050615,132.083409533469)) ;
#139787 = CARTESIAN_POINT('Ctrl Pts',(-19.7370034747035,12.498964683589,131.867247414225)) ;
#139788 = CARTESIAN_POINT('Ctrl Pts',(-19.6435550568839,12.4231077011215,
131.627078243334)) ;
#139789 = CARTESIAN_POINT('Ctrl Pts',(-19.5452918269363,12.4177381472718,
131.373293221748)) ;
#139790 = CARTESIAN_POINT('Ctrl Pts',(-19.4502640880226,12.4847095066073,
131.12876911611)) ;
#139791 = CARTESIAN_POINT('Ctrl Pts',(-19.3637607477036,12.6190667593984,
130.909250351995)) ;
#139792 = CARTESIAN_POINT('Ctrl Pts',(-19.2917485016945,12.8107471033722,
130.73197610566)) ;
#139793 = CARTESIAN_POINT('Ctrl Pts',(-19.2383722341429,13.0461048084143,
130.609139594497)) ;
#139794 = CARTESIAN_POINT('Ctrl Pts',(-19.2067190366217,13.3089103849839,
130.549819117407)) ;
#139795 = CARTESIAN_POINT('Ctrl Pts',(-19.1984163850956,13.5795917474079,
130.558672442477)) ;
#139796 = CARTESIAN_POINT('Ctrl Pts',(-19.2133495061686,13.839854863598,130.635502057452)) ;
#139797 = CARTESIAN_POINT('Ctrl Pts',(-19.2498210148366,14.069864909241,130.775231781513)) ;
#139798 = CARTESIAN_POINT('Ctrl Pts',(-19.303953532,14.2524396014981,130.966329916939)) ;
#139799 = CARTESIAN_POINT('Ctrl Pts',(-19.3719147269832,14.3767943035019,
131.198056739573)) ;
#139800 = CARTESIAN_POINT('Ctrl Pts',(-19.4473716314663,14.4324209572319,
131.451501532081)) ;
#139801 = CARTESIAN_POINT('Ctrl Pts',(-19.5249669302885,14.4159981206257,
131.711381779073)) ;
#139802 = CARTESIAN_POINT('Ctrl Pts',(-19.597827991755,14.3283155320889,131.957349776484)) ;
#139803 = CARTESIAN_POINT('Ctrl Pts',(-19.6602314704124,14.1755659228116,
132.172810910082)) ;
#139804 = CARTESIAN_POINT('Ctrl Pts',(-19.7067461930134,13.969906825541,132.341699515984)) ;
#139805 = CARTESIAN_POINT('Ctrl Pts',(-19.733719116319,13.7239840128541,132.45368170668)) ;
#139806 = CARTESIAN_POINT('Ctrl Pts',(-19.7382480950635,13.4571372933653,
132.500002078048)) ;
#139807 = CARTESIAN_POINT('Ctrl Pts',(-19.7190532761567,13.1860385186985,
132.477260427293)) ;
#139808 = CARTESIAN_POINT('Ctrl Pts',(-19.6774975461961,12.9351633427926,
132.388755944701)) ;
#139809 = CARTESIAN_POINT('Ctrl Pts',(-19.6146960459712,12.716280428453,132.238634235809)) ;
#139810 = CARTESIAN_POINT('Ctrl Pts',(-19.5360671274921,12.5504602967878,
132.041808804563)) ;
#139811 = CARTESIAN_POINT('Ctrl Pts',(-19.4442410734227,12.4451571780271,
131.806961913747)) ;
#139812 = CARTESIAN_POINT('Ctrl Pts',(-19.3476800781724,12.4110818136484,
131.557787015992)) ;
#139813 = CARTESIAN_POINT('Ctrl Pts',(-19.2501729684496,12.4493848627275,
131.306248653423)) ;
#139814 = CARTESIAN_POINT('Ctrl Pts',(-19.1602098012831,12.556427913144,131.076316665042)) ;
#139815 = CARTESIAN_POINT('Ctrl Pts',(-19.0812293628911,12.7270948717805,
130.878914133552)) ;
#139816 = CARTESIAN_POINT('Ctrl Pts',(-19.0199253013521,12.9467013402175,
130.732905024988)) ;
#139817 = CARTESIAN_POINT('Ctrl Pts',(-18.9791994391495,13.2005745563337,
130.647059694796)) ;
#139818 = CARTESIAN_POINT('Ctrl Pts',(-18.961416480655,13.4697556094875,130.628155579184)) ;
#139819 = CARTESIAN_POINT('Ctrl Pts',(-18.9669430878151,13.7362552359381,
130.677419445868)) ;
#139820 = CARTESIAN_POINT('Ctrl Pts',(-18.9950886554368,13.9814041933257,
130.792933897764)) ;
#139821 = CARTESIAN_POINT('Ctrl Pts',(-19.0423528665076,14.1841666830384,
130.963922155526)) ;
#139822 = CARTESIAN_POINT('Ctrl Pts',(-19.1054906760443,14.3343211929266,
131.181586250373)) ;
#139823 = CARTESIAN_POINT('Ctrl Pts',(-19.1787695169468,14.4184551111194,
131.428790827256)) ;
#139824 = CARTESIAN_POINT('Ctrl Pts',(-19.2561021849108,14.4314519975607,
131.687762211676)) ;
#139825 = CARTESIAN_POINT('Ctrl Pts',(-19.3316103231487,14.3721435273992,
131.941493904809)) ;
#139826 = CARTESIAN_POINT('Ctrl Pts',(-19.3987869878459,14.2453738509882,
132.17077888087)) ;
#139827 = CARTESIAN_POINT('Ctrl Pts',(-19.4526636136295,14.0581566958374,
132.361480983201)) ;
#139828 = CARTESIAN_POINT('Ctrl Pts',(-19.4877496207034,13.8276968106527,
132.496917353222)) ;
#139829 = CARTESIAN_POINT('Ctrl Pts',(-19.5016628587778,13.5670203755234,
132.570710388361)) ;
#139830 = CARTESIAN_POINT('Ctrl Pts',(-19.4921504180094,13.2953786744785,
132.576141543242)) ;
#139831 = CARTESIAN_POINT('Ctrl Pts',(-19.4595143011011,13.0342214950179,
132.513845802004)) ;
#139832 = CARTESIAN_POINT('Ctrl Pts',(-19.404757825179,12.7992352777049,132.3871899735)) ;
#139833 = CARTESIAN_POINT('Ctrl Pts',(-19.3323102196323,12.6113833120471,
132.208445138207)) ;
#139834 = CARTESIAN_POINT('Ctrl Pts',(-19.245255132006,12.4798503942449,131.987327845367)) ;
#139835 = CARTESIAN_POINT('Ctrl Pts',(-19.1498981315355,12.416397864002,131.741859779545)) ;
#139836 = CARTESIAN_POINT('Ctrl Pts',(-19.0518914034853,12.4249214929509,
131.48873919952)) ;
#139837 = CARTESIAN_POINT('Ctrl Pts',(-18.9577972429175,12.5053755952326,
131.247046053355)) ;
#139838 = CARTESIAN_POINT('Ctrl Pts',(-18.8740488421285,12.6507859052006,
131.03539948894)) ;
#139839 = CARTESIAN_POINT('Ctrl Pts',(-18.8051224385857,12.8517470992337,
130.867160655025)) ;
#139840 = CARTESIAN_POINT('Ctrl Pts',(-18.755477683788,13.0945614507412,130.755357286549)) ;
#139841 = CARTESIAN_POINT('Ctrl Pts',(-18.7282047545516,13.3602126376938,
130.708805044059)) ;
#139842 = CARTESIAN_POINT('Ctrl Pts',(-18.7244086987787,13.6310671963869,
130.730927107982)) ;
#139843 = CARTESIAN_POINT('Ctrl Pts',(-18.743500281934,13.8852753848623,130.819680825134)) ;
#139844 = CARTESIAN_POINT('Ctrl Pts',(-18.7834694283885,14.1076160740045,
130.969569123117)) ;
#139845 = CARTESIAN_POINT('Ctrl Pts',(-18.8408194229245,14.2808806662079,
131.17024945925)) ;
#139846 = CARTESIAN_POINT('Ctrl Pts',(-18.9105127297827,14.3926567103846,
131.406935440649)) ;
#139847 = CARTESIAN_POINT('Ctrl Pts',(-18.9872957427596,14.4348969491125,
131.664485900502)) ;
#139848 = CARTESIAN_POINT('Ctrl Pts',(-19.0638704847947,14.4049966950683,
131.921100002991)) ;
#139849 = CARTESIAN_POINT('Ctrl Pts',(-19.1357123707124,14.3037928875116,
132.164340586752)) ;
#139850 = CARTESIAN_POINT('Ctrl Pts',(-19.1951840074815,14.1405203865162,
132.371065416947)) ;
#139851 = CARTESIAN_POINT('Ctrl Pts',(-19.2383746342019,13.9258191062473,
132.530330042627)) ;
#139852 = CARTESIAN_POINT('Ctrl Pts',(-19.2612393922595,13.6747404924344,
132.630256846622)) ;
#139853 = CARTESIAN_POINT('Ctrl Pts',(-19.2612747094853,13.4052256695436,
132.663545947711)) ;
#139854 = CARTESIAN_POINT('Ctrl Pts',(-19.2380141324854,13.1384692475265,
132.628587768921)) ;
#139855 = CARTESIAN_POINT('Ctrl Pts',(-19.1918391689992,12.8897551535746,
132.527009776568)) ;
#139856 = CARTESIAN_POINT('Ctrl Pts',(-19.126091093419,12.6813707953234,132.367962858897)) ;
#139857 = CARTESIAN_POINT('Ctrl Pts',(-19.0442932969066,12.5252896402636,
132.162121171031)) ;
#139858 = CARTESIAN_POINT('Ctrl Pts',(-18.9515387706438,12.4335762079788,
131.92430473329)) ;
#139859 = CARTESIAN_POINT('Ctrl Pts',(-18.8540901109851,12.4126069664436,
131.672696703125)) ;
#139860 = CARTESIAN_POINT('Ctrl Pts',(-18.7573139352387,12.4645413764585,
131.423289841079)) ;
#139861 = CARTESIAN_POINT('Ctrl Pts',(-18.6688905994528,12.5845282668637,
131.197986389939)) ;
#139862 = CARTESIAN_POINT('Ctrl Pts',(-18.5931176264357,12.7652451064021,
131.00983237108)) ;
#139863 = CARTESIAN_POINT('Ctrl Pts',(-18.5355210589981,12.9922347341953,
130.87461739619)) ;
#139864 = CARTESIAN_POINT('Ctrl Pts',(-18.4989961498704,13.2501818574091,
130.801001377133)) ;
#139865 = CARTESIAN_POINT('Ctrl Pts',(-18.4855372905734,13.5208713010695,
130.794807344722)) ;
#139866 = CARTESIAN_POINT('Ctrl Pts',(-18.4955335672346,13.7852948748941,
130.857230166328)) ;
#139867 = CARTESIAN_POINT('Ctrl Pts',(-18.5274723089381,14.0230293879869,
130.983660181575)) ;
#139868 = CARTESIAN_POINT('Ctrl Pts',(-18.5783697625451,14.2178154382897,
131.165497530638)) ;
#139869 = CARTESIAN_POINT('Ctrl Pts',(-18.643524354548,14.3552930540828,131.388848328232)) ;
#139870 = CARTESIAN_POINT('Ctrl Pts',(-18.7182803703141,14.4265292549101,
131.640468998874)) ;
#139871 = CARTESIAN_POINT('Ctrl Pts',(-18.7954462603385,14.425752226316,131.898835298117)) ;
#139872 = CARTESIAN_POINT('Ctrl Pts',(-18.8700317215188,14.3531911968223,
132.149935023359)) ;
#139873 = CARTESIAN_POINT('Ctrl Pts',(-18.9351141529095,14.2139749127786,
132.373170205042)) ;
#139874 = CARTESIAN_POINT('Ctrl Pts',(-18.9855856813573,14.0181343155111,
132.553741039007)) ;
#139875 = CARTESIAN_POINT('Ctrl Pts',(-19.0170527791197,13.7796845152241,
132.67878717668)) ;
#139876 = CARTESIAN_POINT('Ctrl Pts',(-19.0265426890785,13.5155236059082,
132.73965320383)) ;
#139877 = CARTESIAN_POINT('Ctrl Pts',(-19.0126470434056,13.245212667821,132.732147951906)) ;
#139878 = CARTESIAN_POINT('Ctrl Pts',(-18.9757739987236,12.987705840382,132.657498715243)) ;
#139879 = CARTESIAN_POINT('Ctrl Pts',(-18.917353844323,12.7602060641004,132.520089995502)) ;
#139880 = CARTESIAN_POINT('Ctrl Pts',(-18.8416873381816,12.5817512683668,
132.332045933198)) ;
#139881 = CARTESIAN_POINT('Ctrl Pts',(-18.7527220787295,12.4625557490256,
132.105291067502)) ;
#139882 = CARTESIAN_POINT('Ctrl Pts',(-18.6561524362465,12.4124303716615,
131.85638030583)) ;
#139883 = CARTESIAN_POINT('Ctrl Pts',(-18.5587876591386,12.4345388124725,
131.604997753593)) ;
#139884 = CARTESIAN_POINT('Ctrl Pts',(-18.4657463620496,12.5283216508309,
131.366516292269)) ;
#139885 = CARTESIAN_POINT('Ctrl Pts',(-18.3846425685644,12.6848122418478,
131.162526699351)) ;
#139886 = CARTESIAN_POINT('Ctrl Pts',(-18.3189041583985,12.8954782936503,
131.003714766411)) ;
#139887 = CARTESIAN_POINT('Ctrl Pts',(-18.2735334103624,13.1430312218348,
130.904237046659)) ;
#139888 = CARTESIAN_POINT('Ctrl Pts',(-18.2506075637187,13.4109716011332,
130.870388378044)) ;
#139889 = CARTESIAN_POINT('Ctrl Pts',(-18.2510953745575,13.6794256976715,
130.904880423363)) ;
#139890 = CARTESIAN_POINT('Ctrl Pts',(-18.2745400654485,13.9314101100325,
131.006701969376)) ;
#139891 = CARTESIAN_POINT('Ctrl Pts',(-18.3180431395774,14.1445006487741,
131.166780524465)) ;
#139892 = CARTESIAN_POINT('Ctrl Pts',(-18.3779447844779,14.3067536437968,
131.374830990371)) ;
#139893 = CARTESIAN_POINT('Ctrl Pts',(-18.4494808894986,14.406048704081,131.616955707788)) ;
#139894 = CARTESIAN_POINT('Ctrl Pts',(-18.5266147943566,14.4348548847552,
131.875427792683)) ;
#139895 = CARTESIAN_POINT('Ctrl Pts',(-18.6031387758285,14.3909041630567,
132.13214715581)) ;
#139896 = CARTESIAN_POINT('Ctrl Pts',(-18.672466809759,14.2783347408893,132.367672775823)) ;
#139897 = CARTESIAN_POINT('Ctrl Pts',(-18.729768369512,14.1031935326512,132.568357731683)) ;
#139898 = CARTESIAN_POINT('Ctrl Pts',(-18.7692792357669,13.8800104531449,
132.716889273809)) ;
#139899 = CARTESIAN_POINT('Ctrl Pts',(-18.7878950784534,13.6249527431351,
132.804295026184)) ;
#139900 = CARTESIAN_POINT('Ctrl Pts',(-18.7835775171384,13.3547990106838,
132.824795353813)) ;
#139901 = CARTESIAN_POINT('Ctrl Pts',(-18.7559551907665,13.0897726871477,
132.777172665473)) ;
#139902 = CARTESIAN_POINT('Ctrl Pts',(-18.7056493126971,12.8467549358408,
132.663569693571)) ;
#139903 = CARTESIAN_POINT('Ctrl Pts',(-18.6367644882602,12.6478124194814,
132.495268377589)) ;
#139904 = CARTESIAN_POINT('Ctrl Pts',(-18.5523377209398,12.5027972017395,
132.281818498312)) ;
#139905 = CARTESIAN_POINT('Ctrl Pts',(-18.4583099874776,12.4240443631204,
132.040236913636)) ;
#139906 = CARTESIAN_POINT('Ctrl Pts',(-18.3600026659222,12.4170503620235,
131.78633891546)) ;
#139907 = CARTESIAN_POINT('Ctrl Pts',(-18.2651791024171,12.4817913910706,
131.542286722758)) ;
#139908 = CARTESIAN_POINT('Ctrl Pts',(-18.1783121098205,12.6142900720352,
131.321713466676)) ;
#139909 = CARTESIAN_POINT('Ctrl Pts',(-18.1059030417794,12.8042103797361,
131.143238469633)) ;
#139910 = CARTESIAN_POINT('Ctrl Pts',(-18.0517927161876,13.0388186679886,
131.018309361831)) ;
#139911 = CARTESIAN_POINT('Ctrl Pts',(-18.0194468757643,13.3023285356057,
130.957112158902)) ;
#139912 = CARTESIAN_POINT('Ctrl Pts',(-18.010553505915,13.5713414244093,130.964028233933)) ;
#139913 = CARTESIAN_POINT('Ctrl Pts',(-18.0248407334206,13.8329962624196,
131.039074983234)) ;
#139914 = CARTESIAN_POINT('Ctrl Pts',(-18.0606661101291,14.0635776732595,
131.176836792273)) ;
#139915 = CARTESIAN_POINT('Ctrl Pts',(-18.1144212284498,14.2479537129057,
131.366889432895)) ;
#139916 = CARTESIAN_POINT('Ctrl Pts',(-18.181823386805,14.3739504524616,131.596871180233)) ;
#139917 = CARTESIAN_POINT('Ctrl Pts',(-18.2577639652939,14.4320428202114,
131.852004261572)) ;
#139918 = CARTESIAN_POINT('Ctrl Pts',(-18.335190107087,14.4172275028747,132.111300594873)) ;
#139919 = CARTESIAN_POINT('Ctrl Pts',(-18.4079980802751,14.3318166981341,
132.356999976137)) ;
#139920 = CARTESIAN_POINT('Ctrl Pts',(-18.4707526739101,14.1811818293068,
132.573443859894)) ;
#139921 = CARTESIAN_POINT('Ctrl Pts',(-18.5179547252937,13.9759967622757,
132.744480222502)) ;
#139922 = CARTESIAN_POINT('Ctrl Pts',(-18.5455049432356,13.7313492386451,
132.858087358722)) ;
#139923 = CARTESIAN_POINT('Ctrl Pts',(-18.5505621183255,13.4634561102099,
132.90612740095)) ;
#139924 = CARTESIAN_POINT('Ctrl Pts',(-18.5323956205154,13.195884935421,132.885916030793)) ;
#139925 = CARTESIAN_POINT('Ctrl Pts',(-18.4910611657277,12.9412337002998,
132.798458784321)) ;
#139926 = CARTESIAN_POINT('Ctrl Pts',(-18.4293713026605,12.7230235152343,
132.651272706854)) ;
#139927 = CARTESIAN_POINT('Ctrl Pts',(-18.3504480692178,12.5539648154296,
132.453908084872)) ;
#139928 = CARTESIAN_POINT('Ctrl Pts',(-18.2598574156189,12.4477725877379,
132.222306799137)) ;
#139929 = CARTESIAN_POINT('Ctrl Pts',(-18.1626825266472,12.4110238126212,
131.971596895803)) ;
#139930 = CARTESIAN_POINT('Ctrl Pts',(-18.0655649689106,12.4468710250015,
131.721015136346)) ;
#139931 = CARTESIAN_POINT('Ctrl Pts',(-17.9743916784582,12.553155401547,131.487903989302)) ;
#139932 = CARTESIAN_POINT('Ctrl Pts',(-17.8956552680024,12.7211113699614,
131.29094946649)) ;
#139933 = CARTESIAN_POINT('Ctrl Pts',(-17.8335847561052,12.9400020395614,
131.142803371709)) ;
#139934 = CARTESIAN_POINT('Ctrl Pts',(-17.792384111752,13.1921120762229,131.055433053991)) ;
#139935 = CARTESIAN_POINT('Ctrl Pts',(-17.7737717164207,13.4620045651565,
131.034220681022)) ;
#139936 = CARTESIAN_POINT('Ctrl Pts',(-17.7787420438599,13.7292706567068,
131.081916802346)) ;
#139937 = CARTESIAN_POINT('Ctrl Pts',(-17.8060353128766,13.9738126182776,
131.194724636009)) ;
#139938 = CARTESIAN_POINT('Ctrl Pts',(-17.853039869841,14.1794947275424,131.365176033557)) ;
#139939 = CARTESIAN_POINT('Ctrl Pts',(-17.9159450098139,14.3311259291818,
131.582191022847)) ;
#139940 = CARTESIAN_POINT('Ctrl Pts',(-17.9885875436753,14.4169205617397,
131.827348730516)) ;
#139941 = CARTESIAN_POINT('Ctrl Pts',(-18.0663285917671,14.4320030315974,
132.087711051093)) ;
#139942 = CARTESIAN_POINT('Ctrl Pts',(-18.1415675439527,14.3751243687379,
132.340459922905)) ;
#139943 = CARTESIAN_POINT('Ctrl Pts',(-18.2096359824422,14.2488768179311,
132.572659748216)) ;
#139944 = CARTESIAN_POINT('Ctrl Pts',(-18.2634030402634,14.0648018746923,
132.762713076847)) ;
#139945 = CARTESIAN_POINT('Ctrl Pts',(-18.2993393835354,13.8343788522074,
132.900814395349)) ;
#139946 = CARTESIAN_POINT('Ctrl Pts',(-18.3138052523307,13.5736071381831,
132.976286578787)) ;
#139947 = CARTESIAN_POINT('Ctrl Pts',(-18.304900108542,13.3025525300613,132.983425008922)) ;
#139948 = CARTESIAN_POINT('Ctrl Pts',(-18.2730041011089,13.0417945957582,
132.923179652522)) ;
#139949 = CARTESIAN_POINT('Ctrl Pts',(-18.2190983791431,12.8063140685278,
132.798906207675)) ;
#139950 = CARTESIAN_POINT('Ctrl Pts',(-18.1468168584937,12.6158856975737,
132.620808271038)) ;
#139951 = CARTESIAN_POINT('Ctrl Pts',(-18.0599209734576,12.4825396970198,
132.400205037205)) ;
#139952 = CARTESIAN_POINT('Ctrl Pts',(-17.9649956111779,12.4173081237828,
132.155903217659)) ;
#139953 = CARTESIAN_POINT('Ctrl Pts',(-17.8670768307849,12.423605000428,131.903005180849)) ;
#139954 = CARTESIAN_POINT('Ctrl Pts',(-17.7728138214266,12.5018025966581,
131.660799723848)) ;
#139955 = CARTESIAN_POINT('Ctrl Pts',(-17.6884211517769,12.6458565798938,
131.44737668302)) ;
#139956 = CARTESIAN_POINT('Ctrl Pts',(-17.6190781329538,12.8453790833706,
131.27789881031)) ;
#139957 = CARTESIAN_POINT('Ctrl Pts',(-17.5689078790036,13.0865652662194,
131.164476359025)) ;
#139958 = CARTESIAN_POINT('Ctrl Pts',(-17.5409063530065,13.3521427577607,
131.11584353298)) ;
#139959 = CARTESIAN_POINT('Ctrl Pts',(-17.5363739810292,13.6222557202932,
131.135702219047)) ;
#139960 = CARTESIAN_POINT('Ctrl Pts',(-17.5548275317412,13.8783882969557,
131.2227406542)) ;
#139961 = CARTESIAN_POINT('Ctrl Pts',(-17.5943750726365,14.1022120618795,
131.37145767239)) ;
#139962 = CARTESIAN_POINT('Ctrl Pts',(-17.6511400306937,14.2765229506337,
131.570334937194)) ;
#139963 = CARTESIAN_POINT('Ctrl Pts',(-17.7204518418135,14.3902286964009,
131.805872441639)) ;
#139964 = CARTESIAN_POINT('Ctrl Pts',(-17.7972369816987,14.4347769427253,
132.063476509969)) ;
#139965 = CARTESIAN_POINT('Ctrl Pts',(-17.8740308161132,14.4066722617846,
132.320801188858)) ;
#139966 = CARTESIAN_POINT('Ctrl Pts',(-17.9456993619042,14.3082119125381,
132.563325601213)) ;
#139967 = CARTESIAN_POINT('Ctrl Pts',(-18.0059086330157,14.1460357867196,
132.772367372232)) ;
#139968 = CARTESIAN_POINT('Ctrl Pts',(-18.0495959794959,13.9328084574968,
132.933044174357)) ;
#139969 = CARTESIAN_POINT('Ctrl Pts',(-18.0731093783754,13.681774125451,133.034966341069)) ;
#139970 = CARTESIAN_POINT('Ctrl Pts',(-18.0738683957939,13.414026239165,133.070176901805)) ;
#139971 = CARTESIAN_POINT('Ctrl Pts',(-18.0511266283768,13.1453688505525,
133.036941887299)) ;
#139972 = CARTESIAN_POINT('Ctrl Pts',(-18.0059948266115,12.8977836793382,
132.938130042737)) ;
#139973 = CARTESIAN_POINT('Ctrl Pts',(-17.9402912323445,12.6861562687701,
132.779496079662)) ;
#139974 = CARTESIAN_POINT('Ctrl Pts',(-17.8590011189062,12.5289208649723,
132.575061965886)) ;
#139975 = CARTESIAN_POINT('Ctrl Pts',(-17.7663814238346,12.4351549173609,
132.337678380036)) ;
#139976 = CARTESIAN_POINT('Ctrl Pts',(-17.6692083593153,12.41223935111,132.086798615346)) ;
#139977 = CARTESIAN_POINT('Ctrl Pts',(-17.5723092010791,12.4619213802628,
131.837027428142)) ;
#139978 = CARTESIAN_POINT('Ctrl Pts',(-17.4833798800122,12.5803996576492,
131.610327628056)) ;
#139979 = CARTESIAN_POINT('Ctrl Pts',(-17.4073580775245,12.7591299029993,
131.421362280643)) ;
#139980 = CARTESIAN_POINT('Ctrl Pts',(-17.3491268284245,12.9850687098392,
131.284316932474)) ;
#139981 = CARTESIAN_POINT('Ctrl Pts',(-17.3119541347841,13.2423777054139,
131.20880655253)) ;
#139982 = CARTESIAN_POINT('Ctrl Pts',(-17.2978226688005,13.5129449016412,
131.200646200816)) ;
#139983 = CARTESIAN_POINT('Ctrl Pts',(-17.3070879903219,13.7774320597186,
131.260874076779)) ;
#139984 = CARTESIAN_POINT('Ctrl Pts',(-17.3384928099776,14.0166134042629,
131.385813340299)) ;
#139985 = CARTESIAN_POINT('Ctrl Pts',(-17.3885767506353,14.2120830530507,
131.565102403099)) ;
#139986 = CARTESIAN_POINT('Ctrl Pts',(-17.4538316971294,14.352498916215,131.788992594797)) ;
#139987 = CARTESIAN_POINT('Ctrl Pts',(-17.5281745380114,14.4253825701344,
132.039289476329)) ;
#139988 = CARTESIAN_POINT('Ctrl Pts',(-17.6054634622487,14.426768294094,132.298075516539)) ;
#139989 = CARTESIAN_POINT('Ctrl Pts',(-17.6800468801876,14.3564920185828,
132.549080337008)) ;
#139990 = CARTESIAN_POINT('Ctrl Pts',(-17.7457143234865,14.2186719371757,
132.774142097091)) ;
#139991 = CARTESIAN_POINT('Ctrl Pts',(-17.7966202311834,14.024316786925,132.955958740035)) ;
#139992 = CARTESIAN_POINT('Ctrl Pts',(-17.8286778334795,13.7866136068205,
133.082761139873)) ;
#139993 = CARTESIAN_POINT('Ctrl Pts',(-17.8387984063553,13.5238037033397,
133.145359694921)) ;
#139994 = CARTESIAN_POINT('Ctrl Pts',(-17.8256146623074,13.2527086042196,
133.140017565356)) ;
#139995 = CARTESIAN_POINT('Ctrl Pts',(-17.7891304573137,12.9936530632693,
133.066635952867)) ;
#139996 = CARTESIAN_POINT('Ctrl Pts',(-17.7315183419931,12.7662441874236,
132.93142162794)) ;
#139997 = CARTESIAN_POINT('Ctrl Pts',(-17.6561927558797,12.5858801409006,
132.744430610963)) ;
#139998 = CARTESIAN_POINT('Ctrl Pts',(-17.5674505982938,12.4648530718858,
132.518345830631)) ;
#139999 = CARTESIAN_POINT('Ctrl Pts',(-17.4708526129738,12.4128201875619,
132.269401513626)) ;
#140000 = CARTESIAN_POINT('Ctrl Pts',(-17.3738183375729,12.4330274107103,
132.018859494709)) ;
#140001 = CARTESIAN_POINT('Ctrl Pts',(-17.2809556103288,12.524012324909,131.780737711725)) ;
#140002 = CARTESIAN_POINT('Ctrl Pts',(-17.1989341049103,12.6795221282536,
131.57426239901)) ;
#140003 = CARTESIAN_POINT('Ctrl Pts',(-17.1327378420487,12.8889214141028,
131.414101802532)) ;
#140004 = CARTESIAN_POINT('Ctrl Pts',(-17.0867269430234,13.1354947089828,
131.312742856685)) ;
#140005 = CARTESIAN_POINT('Ctrl Pts',(-17.0630990286742,13.4042911436029,
131.276983650143)) ;
#140006 = CARTESIAN_POINT('Ctrl Pts',(-17.0630113893596,13.6719452313923,
131.309670318193)) ;
#140007 = CARTESIAN_POINT('Ctrl Pts',(-17.0857204958191,13.9242175336792,
131.409269871991)) ;
#140008 = CARTESIAN_POINT('Ctrl Pts',(-17.1287442358938,14.1390288741834,
131.568008046519)) ;
#140009 = CARTESIAN_POINT('Ctrl Pts',(-17.1882900238395,14.3030286144717,
131.775040930177)) ;
#140010 = CARTESIAN_POINT('Ctrl Pts',(-17.2596164114591,14.4041953326341,
132.016566385165)) ;
#140011 = CARTESIAN_POINT('Ctrl Pts',(-17.3364367314704,14.4349854779899,
132.274021676845)) ;
#140012 = CARTESIAN_POINT('Ctrl Pts',(-17.4130831782189,14.3934046886661,
132.531096520565)) ;
#140013 = CARTESIAN_POINT('Ctrl Pts',(-17.4829306248326,14.2822103121525,
132.768262973992)) ;
#140014 = CARTESIAN_POINT('Ctrl Pts',(-17.5403192864147,14.1097942363152,
132.968995643959)) ;
#140015 = CARTESIAN_POINT('Ctrl Pts',(-17.5805733706792,13.8877667094565,
133.119746822849)) ;
#140016 = CARTESIAN_POINT('Ctrl Pts',(-17.5999033803559,13.6324084420419,
133.209366061804)) ;
#140017 = CARTESIAN_POINT('Ctrl Pts',(-17.596247458933,13.3624185504467,133.231793716882)) ;
#140018 = CARTESIAN_POINT('Ctrl Pts',(-17.5691757856173,13.0965814778885,
133.185837900411)) ;
#140019 = CARTESIAN_POINT('Ctrl Pts',(-17.5197846541153,12.8540736174815,
133.074706584003)) ;
#140020 = CARTESIAN_POINT('Ctrl Pts',(-17.451348287198,12.652992435015,132.907789970015)) ;
#140021 = CARTESIAN_POINT('Ctrl Pts',(-17.3667759142286,12.5055874303856,
132.694097208918)) ;
#140022 = CARTESIAN_POINT('Ctrl Pts',(-17.2733692229142,12.4255318647486,
132.454172659202)) ;
#140023 = CARTESIAN_POINT('Ctrl Pts',(-17.1755318837841,12.4160627512278,
132.201498055215)) ;
#140024 = CARTESIAN_POINT('Ctrl Pts',(-17.0800677624105,12.4788299066414,
131.955734672931)) ;
#140025 = CARTESIAN_POINT('Ctrl Pts',(-16.9928119833877,12.6096602766835,
131.734049308796)) ;
#140026 = CARTESIAN_POINT('Ctrl Pts',(-16.9198008856656,12.7985462130252,
131.553883363849)) ;
#140027 = CARTESIAN_POINT('Ctrl Pts',(-16.8653086304422,13.031708612879,131.427766361266)) ;
#140028 = CARTESIAN_POINT('Ctrl Pts',(-16.8323684675315,13.293083578928,131.364642117709)) ;
#140029 = CARTESIAN_POINT('Ctrl Pts',(-16.8226660727472,13.5641924680593,
131.369449472426)) ;
#140030 = CARTESIAN_POINT('Ctrl Pts',(-16.8363638395971,13.8256806601297,
131.442688303253)) ;
#140031 = CARTESIAN_POINT('Ctrl Pts',(-16.8713842098541,14.0565823152587,
131.577970763861)) ;
#140032 = CARTESIAN_POINT('Ctrl Pts',(-16.9248059316069,14.2434411149003,
131.76717177554)) ;
#140033 = CARTESIAN_POINT('Ctrl Pts',(-16.9921951195004,14.3714533613372,
131.997241772447)) ;
#140034 = CARTESIAN_POINT('Ctrl Pts',(-17.0673511293183,14.4311593709141,
132.249804262029)) ;
#140035 = CARTESIAN_POINT('Ctrl Pts',(-17.1450034626173,14.4188767370812,
132.509845921802)) ;
#140036 = CARTESIAN_POINT('Ctrl Pts',(-17.2181873389402,14.3353893813971,
132.756704184413)) ;
#140037 = CARTESIAN_POINT('Ctrl Pts',(-17.2814813061672,14.1858866209329,
132.974831456389)) ;
#140038 = CARTESIAN_POINT('Ctrl Pts',(-17.3289977855556,13.9829323143578,
133.14664284081)) ;
#140039 = CARTESIAN_POINT('Ctrl Pts',(-17.3572257515771,13.7386001915966,
133.262317495533)) ;
#140040 = CARTESIAN_POINT('Ctrl Pts',(-17.3629896704757,13.472491070878,133.312245512371)) ;
#140041 = CARTESIAN_POINT('Ctrl Pts',(-17.3454245972226,13.2027754622607,
133.294032832636)) ;
#140042 = CARTESIAN_POINT('Ctrl Pts',(-17.3046250802462,12.9475729445581,
133.208125531195)) ;
#140043 = CARTESIAN_POINT('Ctrl Pts',(-17.2435833734801,12.7286906854066,
133.062766425607)) ;
#140044 = CARTESIAN_POINT('Ctrl Pts',(-17.1653001243494,12.5582194228626,
132.867194935478)) ;
#140045 = CARTESIAN_POINT('Ctrl Pts',(-17.0744878770675,12.4495814745878,
132.635124317158)) ;
#140046 = CARTESIAN_POINT('Ctrl Pts',(-16.977602091249,12.4111325030014,132.385184551978)) ;
#140047 = CARTESIAN_POINT('Ctrl Pts',(-16.8806236193526,12.4448573230465,
132.134938711957)) ;
#140048 = CARTESIAN_POINT('Ctrl Pts',(-16.7894019430177,12.5485736269638,
131.901587070824)) ;
#140049 = CARTESIAN_POINT('Ctrl Pts',(-16.7097006554741,12.7160675409956,
131.702047644044)) ;
#140050 = CARTESIAN_POINT('Ctrl Pts',(-16.6474333959251,12.9327061634172,
131.55315650852)) ;
#140051 = CARTESIAN_POINT('Ctrl Pts',(-16.6054314285535,13.1846668378338,
131.463536928802)) ;
#140052 = CARTESIAN_POINT('Ctrl Pts',(-16.5861998611225,13.4544224505961,
131.440520016968)) ;
#140053 = CARTESIAN_POINT('Ctrl Pts',(-16.5904757716003,13.7215757277082,
131.486129856679)) ;
#140054 = CARTESIAN_POINT('Ctrl Pts',(-16.6171930426673,13.9674105771419,
131.597307673441)) ;
#140055 = CARTESIAN_POINT('Ctrl Pts',(-16.6636138619868,14.173959529566,131.765990224629)) ;
#140056 = CARTESIAN_POINT('Ctrl Pts',(-16.7258970011584,14.3272528917974,
131.981094732715)) ;
#140057 = CARTESIAN_POINT('Ctrl Pts',(-16.7988063944434,14.4155297933765,
132.227255254739)) ;
#140058 = CARTESIAN_POINT('Ctrl Pts',(-16.8760210825582,14.4326688919931,
132.485862874767)) ;
#140059 = CARTESIAN_POINT('Ctrl Pts',(-16.951873050781,14.3775210851954,132.740618667098)) ;
#140060 = CARTESIAN_POINT('Ctrl Pts',(-17.0197649340033,14.2540409497735,
132.97205574517)) ;
#140061 = CARTESIAN_POINT('Ctrl Pts',(-17.0743094525665,14.0709648404294,
133.164530968928)) ;
#140062 = CARTESIAN_POINT('Ctrl Pts',(-17.1107712589207,13.8416199904244,
133.304154870266)) ;
#140063 = CARTESIAN_POINT('Ctrl Pts',(-17.1258886763416,13.582388567831,133.381421380426)) ;
#140064 = CARTESIAN_POINT('Ctrl Pts',(-17.1178138289345,13.3112804497714,
133.390993708911)) ;
#140065 = CARTESIAN_POINT('Ctrl Pts',(-17.0863471130288,13.0483997987315,
133.332210032555)) ;
#140066 = CARTESIAN_POINT('Ctrl Pts',(-17.0332668996353,12.8130298392026,
133.210187809291)) ;
#140067 = CARTESIAN_POINT('Ctrl Pts',(-16.9612682248294,12.6204060823588,
133.033025253701)) ;
#140068 = CARTESIAN_POINT('Ctrl Pts',(-16.8747379912783,12.4854479324355,
132.813466850666)) ;
#140069 = CARTESIAN_POINT('Ctrl Pts',(-16.7799596426297,12.4181326730335,
132.569603428481)) ;
#140070 = CARTESIAN_POINT('Ctrl Pts',(-16.6817627892976,12.4224942487035,
132.315980950859)) ;
#140071 = CARTESIAN_POINT('Ctrl Pts',(-16.5874095963749,12.4989653084942,
132.073488665005)) ;
#140072 = CARTESIAN_POINT('Ctrl Pts',(-16.5030227664661,12.6405919477357,
131.859938970218)) ;
#140073 = CARTESIAN_POINT('Ctrl Pts',(-16.4329418145269,12.8391593414189,
131.688400941445)) ;
#140074 = CARTESIAN_POINT('Ctrl Pts',(-16.3820975732448,13.080245962358,131.573107657497)) ;
#140075 = CARTESIAN_POINT('Ctrl Pts',(-16.3535910400909,13.3449462168028,
131.522937145774)) ;
#140076 = CARTESIAN_POINT('Ctrl Pts',(-16.3483981201149,13.6142996681917,
131.540758663562)) ;
#140077 = CARTESIAN_POINT('Ctrl Pts',(-16.3661681324322,13.8710421169928,
131.625790173589)) ;
#140078 = CARTESIAN_POINT('Ctrl Pts',(-16.4051123344729,14.0962488257935,
131.772752900092)) ;
#140079 = CARTESIAN_POINT('Ctrl Pts',(-16.4618078548578,14.2729914081674,
131.971617342725)) ;
#140080 = CARTESIAN_POINT('Ctrl Pts',(-16.5304999126162,14.38767954712,132.205165563622)) ;
#140081 = CARTESIAN_POINT('Ctrl Pts',(-16.6070330356264,14.4346057861831,
132.461982388263)) ;
#140082 = CARTESIAN_POINT('Ctrl Pts',(-16.6843229990153,14.4082599468392,
132.720943868329)) ;
#140083 = CARTESIAN_POINT('Ctrl Pts',(-16.7557875504688,14.3122705880149,
132.962668513264)) ;
#140084 = CARTESIAN_POINT('Ctrl Pts',(-16.8166821611392,14.151436185241,133.173833669416)) ;
#140085 = CARTESIAN_POINT('Ctrl Pts',(-16.8608925190079,13.9387188784377,
133.336119150085)) ;
#140086 = CARTESIAN_POINT('Ctrl Pts',(-16.8849135991378,13.6904434125759,
133.439271987478)) ;
#140087 = CARTESIAN_POINT('Ctrl Pts',(-16.8863661179106,13.4208420598601,
133.476776952907)) ;
#140088 = CARTESIAN_POINT('Ctrl Pts',(-16.8643629093214,13.1534853902676,
133.445499699409)) ;
#140089 = CARTESIAN_POINT('Ctrl Pts',(-16.8198173917774,12.9044050288982,
133.348483089943)) ;
#140090 = CARTESIAN_POINT('Ctrl Pts',(-16.7545728094688,12.6913475994885,
133.19121034881)) ;
#140091 = CARTESIAN_POINT('Ctrl Pts',(-16.6735792900983,12.5324269019675,
132.987673507823)) ;
#140092 = CARTESIAN_POINT('Ctrl Pts',(-16.5815141879572,12.4369854947191,
132.751795055161)) ;
#140093 = CARTESIAN_POINT('Ctrl Pts',(-16.484196424873,12.4119049760396,132.500565871752)) ;
#140094 = CARTESIAN_POINT('Ctrl Pts',(-16.3875232228243,12.459288588066,132.25133200756)) ;
#140095 = CARTESIAN_POINT('Ctrl Pts',(-16.2981920739487,12.5757336822765,
132.023487610852)) ;
#140096 = CARTESIAN_POINT('Ctrl Pts',(-16.221663226933,12.7527802879128,131.833046815115)) ;
#140097 = CARTESIAN_POINT('Ctrl Pts',(-16.1625644709713,12.9786618268138,
131.693629435243)) ;
#140098 = CARTESIAN_POINT('Ctrl Pts',(-16.1248303893333,13.2359088344013,
131.616537241571)) ;
#140099 = CARTESIAN_POINT('Ctrl Pts',(-16.1101106562054,13.5051026285248,
131.606499820776)) ;
#140100 = CARTESIAN_POINT('Ctrl Pts',(-16.1187976807236,13.7711208876962,
131.665181919994)) ;
#140101 = CARTESIAN_POINT('Ctrl Pts',(-16.1494970012602,14.0100003599807,
131.787889090912)) ;
#140102 = CARTESIAN_POINT('Ctrl Pts',(-16.1991678311649,14.2073724408212,
131.966043243383)) ;
#140103 = CARTESIAN_POINT('Ctrl Pts',(-16.2639738299788,14.3492226306733,
132.188560730462)) ;
#140104 = CARTESIAN_POINT('Ctrl Pts',(-16.3380263648965,14.4242519881516,
132.43797256554)) ;
#140105 = CARTESIAN_POINT('Ctrl Pts',(-16.4156431986028,14.4277364563771,
132.697856444715)) ;
#140106 = CARTESIAN_POINT('Ctrl Pts',(-16.490288927873,14.3592420110673,132.949008230295)) ;
#140107 = CARTESIAN_POINT('Ctrl Pts',(-16.5560174977799,14.2240686922171,
133.174088753831)) ;
#140108 = CARTESIAN_POINT('Ctrl Pts',(-16.6076266234123,14.0305585465179,
133.358084944611)) ;
#140109 = CARTESIAN_POINT('Ctrl Pts',(-16.6402104387998,13.7945206228156,
133.486333304394)) ;
#140110 = CARTESIAN_POINT('Ctrl Pts',(-16.651061280046,13.5313067865741,133.551183520933)) ;
#140111 = CARTESIAN_POINT('Ctrl Pts',(-16.6385182945988,13.2605192088026,
133.547666910289)) ;
#140112 = CARTESIAN_POINT('Ctrl Pts',(-16.6028442001819,13.0015411116714,
133.476558081978)) ;
#140113 = CARTESIAN_POINT('Ctrl Pts',(-16.5458000319494,12.7725523899085,
133.343047202527)) ;
#140114 = CARTESIAN_POINT('Ctrl Pts',(-16.4707277903299,12.5901314079498,
133.156883276531)) ;
#140115 = CARTESIAN_POINT('Ctrl Pts',(-16.3823389739391,12.4675131368497,
132.931805480759)) ;
#140116 = CARTESIAN_POINT('Ctrl Pts',(-16.286313729189,12.4133289133512,132.684387528141)) ;
#140117 = CARTESIAN_POINT('Ctrl Pts',(-16.1885428106146,12.4315113469885,
132.43192881401)) ;
#140118 = CARTESIAN_POINT('Ctrl Pts',(-16.0957725720943,12.5204618731953,
132.193969057206)) ;
#140119 = CARTESIAN_POINT('Ctrl Pts',(-16.0133683697875,12.6740885600686,
131.986368940502)) ;
#140120 = CARTESIAN_POINT('Ctrl Pts',(-15.9466347797837,12.8820605633652,
131.82463063258)) ;
#140121 = CARTESIAN_POINT('Ctrl Pts',(-15.8999755193379,13.1280849033747,
131.721420437203)) ;
#140122 = CARTESIAN_POINT('Ctrl Pts',(-15.8756996992524,13.3954305468035,
131.683629487919)) ;
#140123 = CARTESIAN_POINT('Ctrl Pts',(-15.8749154596136,13.6647721239679,
131.714464613994)) ;
#140124 = CARTESIAN_POINT('Ctrl Pts',(-15.8968964489419,13.9166503672092,
131.811778285468)) ;
#140125 = CARTESIAN_POINT('Ctrl Pts',(-15.9394126728008,14.1333087824096,
131.969110200075)) ;
#140126 = CARTESIAN_POINT('Ctrl Pts',(-15.9984604507846,14.2989356836214,
132.174650382244)) ;
#140127 = CARTESIAN_POINT('Ctrl Pts',(-16.069955047821,14.4025578145927,132.416862616266)) ;
#140128 = CARTESIAN_POINT('Ctrl Pts',(-16.1464394854795,14.435010397795,132.673218956648)) ;
#140129 = CARTESIAN_POINT('Ctrl Pts',(-16.2231180895877,14.3956728080676,
132.930357127469)) ;
#140130 = CARTESIAN_POINT('Ctrl Pts',(-16.2932740093016,14.2862787578303,
133.168445846428)) ;
#140131 = CARTESIAN_POINT('Ctrl Pts',(-16.3510597233741,14.1158603541274,
133.370289668947)) ;
#140132 = CARTESIAN_POINT('Ctrl Pts',(-16.392061731818,13.8934485383183,133.523446661948)) ;
#140133 = CARTESIAN_POINT('Ctrl Pts',(-16.4118475379423,13.6404741399982,
133.614166778358)) ;
#140134 = CARTESIAN_POINT('Ctrl Pts',(-16.4088703893971,13.3695007340468,
133.638723997956)) ;
#140135 = CARTESIAN_POINT('Ctrl Pts',(-16.382512592704,13.1044457267252,133.594710829848)) ;
#140136 = CARTESIAN_POINT('Ctrl Pts',(-16.3338267763214,12.860704031683,133.485653364823)) ;
#140137 = CARTESIAN_POINT('Ctrl Pts',(-16.2652943294484,12.6571154777524,
133.318695024141)) ;
#140138 = CARTESIAN_POINT('Ctrl Pts',(-16.1821466626859,12.5098080554844,
133.108743958478)) ;
#140139 = CARTESIAN_POINT('Ctrl Pts',(-16.0884174129943,12.4266891530237,
132.868087786362)) ;
#140140 = CARTESIAN_POINT('Ctrl Pts',(-15.9903350041764,12.4154229755217,
132.614782524112)) ;
#140141 = CARTESIAN_POINT('Ctrl Pts',(-15.8950587880633,12.4759770673935,
132.36945254477)) ;
#140142 = CARTESIAN_POINT('Ctrl Pts',(-15.8074607836014,12.6048252394354,
132.146767087562)) ;
#140143 = CARTESIAN_POINT('Ctrl Pts',(-15.7339345122349,12.7921645634063,
131.965101212743)) ;
#140144 = CARTESIAN_POINT('Ctrl Pts',(-15.6787573253253,13.0247862212583,
131.83705713208)) ;
#140145 = CARTESIAN_POINT('Ctrl Pts',(-15.6451872213494,13.2853105369572,
131.772049972934)) ;
#140146 = CARTESIAN_POINT('Ctrl Pts',(-15.6348692512998,13.5574331010645,
131.775190161666)) ;
#140147 = CARTESIAN_POINT('Ctrl Pts',(-15.6477474012688,13.8171021403353,
131.845722672944)) ;
#140148 = CARTESIAN_POINT('Ctrl Pts',(-15.6823995504724,14.0511738702826,
131.980211338381)) ;
#140149 = CARTESIAN_POINT('Ctrl Pts',(-15.7353430940617,14.2388281925165,
132.167944371015)) ;
#140150 = CARTESIAN_POINT('Ctrl Pts',(-15.8021504706626,14.3685839243643,
132.396210499492)) ;
#140151 = CARTESIAN_POINT('Ctrl Pts',(-15.8777413821372,14.430551147229,132.650299229092)) ;
#140152 = CARTESIAN_POINT('Ctrl Pts',(-15.9548493427787,14.4203097396042,
132.908497044861)) ;
#140153 = CARTESIAN_POINT('Ctrl Pts',(-16.0285863561776,14.3384208186475,
133.157141334588)) ;
#140154 = CARTESIAN_POINT('Ctrl Pts',(-16.0919232558738,14.191573192343,133.375198147925)) ;
#140155 = CARTESIAN_POINT('Ctrl Pts',(-16.1403208257874,13.9880715249732,
133.549888683024)) ;
#140156 = CARTESIAN_POINT('Ctrl Pts',(-16.1688197828895,13.74717256078,133.665995114336)) ;
#140157 = CARTESIAN_POINT('Ctrl Pts',(-16.1753840787558,13.4800206517718,
133.71845667894)) ;
#140158 = CARTESIAN_POINT('Ctrl Pts',(-16.1585115139942,13.2110030826081,
133.70215466538)) ;
#140159 = CARTESIAN_POINT('Ctrl Pts',(-16.1183902206883,12.9547749192264,
133.61826212713)) ;
#140160 = CARTESIAN_POINT('Ctrl Pts',(-16.0578431071565,12.7344342414435,
133.474378704329)) ;
#140161 = CARTESIAN_POINT('Ctrl Pts',(-15.9799587158776,12.56234537382,133.279982911303)) ;
#140162 = CARTESIAN_POINT('Ctrl Pts',(-15.8896136740205,12.4518692107331,
133.049210374909)) ;
#140163 = CARTESIAN_POINT('Ctrl Pts',(-15.7925458848479,12.4112334908308,
132.798839526536)) ;
#140164 = CARTESIAN_POINT('Ctrl Pts',(-15.6955857869506,12.4427491476605,
132.548603262196)) ;
#140165 = CARTESIAN_POINT('Ctrl Pts',(-15.6035799730376,12.5456206788136,
132.313181586489)) ;
#140166 = CARTESIAN_POINT('Ctrl Pts',(-15.5245257438388,12.7091960260598,
132.115080647817)) ;
#140167 = CARTESIAN_POINT('Ctrl Pts',(-15.4611054690331,12.9259029784642,
131.963079856296)) ;
#140168 = CARTESIAN_POINT('Ctrl Pts',(-15.4185548878178,13.1770736213742,
131.871835443339)) ;
#140169 = CARTESIAN_POINT('Ctrl Pts',(-15.398628373212,13.4468768316793,131.846827048019)) ;
#140170 = CARTESIAN_POINT('Ctrl Pts',(-15.4022435837397,13.7138795758086,
131.890444695793)) ;
#140171 = CARTESIAN_POINT('Ctrl Pts',(-15.4283089337862,13.9605431797111,
131.999711066717)) ;
#140172 = CARTESIAN_POINT('Ctrl Pts',(-15.4741850451082,14.1686235448508,
132.166809272783)) ;
#140173 = CARTESIAN_POINT('Ctrl Pts',(-15.536389802078,14.324111265305,132.381830675133)) ;
#140174 = CARTESIAN_POINT('Ctrl Pts',(-15.6086735020593,14.4138215777412,
132.625972723014)) ;
#140175 = CARTESIAN_POINT('Ctrl Pts',(-15.6861367295395,14.4331945078177,
132.88543907852)) ;
#140176 = CARTESIAN_POINT('Ctrl Pts',(-15.7618948329016,14.3801614828431,
133.13981815517)) ;
#140177 = CARTESIAN_POINT('Ctrl Pts',(-15.8301942788936,14.2584942969663,
133.3724909289)) ;
#140178 = CARTESIAN_POINT('Ctrl Pts',(-15.8851640878315,14.0770491987957,
133.566189678613)) ;
#140179 = CARTESIAN_POINT('Ctrl Pts',(-15.922273133789,13.848487543227,133.707756230679)) ;
#140180 = CARTESIAN_POINT('Ctrl Pts',(-15.9379802552091,13.5893550911286,
133.786801390738)) ;
#140181 = CARTESIAN_POINT('Ctrl Pts',(-15.9306077589097,13.3196922711331,
133.798256276605)) ;
#140182 = CARTESIAN_POINT('Ctrl Pts',(-15.8998800307797,13.0561134153821,
133.74164886771)) ;
#140183 = CARTESIAN_POINT('Ctrl Pts',(-15.8472473398955,12.8190741584449,
133.621021676602)) ;
#140184 = CARTESIAN_POINT('Ctrl Pts',(-15.7757708334939,12.6252976289265,
133.445352087381)) ;
#140185 = CARTESIAN_POINT('Ctrl Pts',(-15.689927661777,12.4887797079064,133.22768214269)) ;
#140186 = CARTESIAN_POINT('Ctrl Pts',(-15.594962990031,12.4190606508798,132.983404336267)) ;
#140187 = CARTESIAN_POINT('Ctrl Pts',(-15.4971275089631,12.4213023279721,
132.730711688481)) ;
#140188 = CARTESIAN_POINT('Ctrl Pts',(-15.4025332987901,12.4953372291496,
132.487520232972)) ;
#140189 = CARTESIAN_POINT('Ctrl Pts',(-15.3173685878029,12.6358732815743,
132.271860695447)) ;
#140190 = CARTESIAN_POINT('Ctrl Pts',(-15.2470295349631,12.8325869424309,
132.099478396863)) ;
#140191 = CARTESIAN_POINT('Ctrl Pts',(-15.1956790187667,13.0715962372375,
131.982579048758)) ;
#140192 = CARTESIAN_POINT('Ctrl Pts',(-15.1663012050405,13.3366928582969,
131.929977593975)) ;
#140193 = CARTESIAN_POINT('Ctrl Pts',(-15.1604318239741,13.6067853722367,
131.945897366208)) ;
#140194 = CARTESIAN_POINT('Ctrl Pts',(-15.1775882934779,13.8640946743987,
132.029130404731)) ;
#140195 = CARTESIAN_POINT('Ctrl Pts',(-15.2158372279991,14.0898397345162,
132.173966228249)) ;
#140196 = CARTESIAN_POINT('Ctrl Pts',(-15.2720097039108,14.268360163449,132.371295347158)) ;
#140197 = CARTESIAN_POINT('Ctrl Pts',(-15.3406803590063,14.3854877174078,
132.60491187324)) ;
#140198 = CARTESIAN_POINT('Ctrl Pts',(-15.4171753630051,14.4341894579408,
132.861648085869)) ;
#140199 = CARTESIAN_POINT('Ctrl Pts',(-15.4941067151991,14.4102459856392,
133.119375356917)) ;
#140200 = CARTESIAN_POINT('Ctrl Pts',(-15.5662114944303,14.3157190540823,
133.363158093056)) ;
#140201 = CARTESIAN_POINT('Ctrl Pts',(-15.6271436805455,14.1574302983803,
133.57424107157)) ;
#140202 = CARTESIAN_POINT('Ctrl Pts',(-15.6720895670541,13.9458829104796,
133.738742203992)) ;
#140203 = CARTESIAN_POINT('Ctrl Pts',(-15.6967873055417,13.6969896287775,
133.844047527021)) ;
#140204 = CARTESIAN_POINT('Ctrl Pts',(-15.698845751887,13.429280378355,133.883124165852)) ;
#140205 = CARTESIAN_POINT('Ctrl Pts',(-15.6776431235188,13.1613091049485,
133.8542162852)) ;
#140206 = CARTESIAN_POINT('Ctrl Pts',(-15.6332316360466,12.9096301880815,
133.757855277709)) ;
#140207 = CARTESIAN_POINT('Ctrl Pts',(-15.5691974920527,12.6977069165648,
133.603749145118)) ;
#140208 = CARTESIAN_POINT('Ctrl Pts',(-15.488381414163,12.5361591796786,133.400861291253)) ;
#140209 = CARTESIAN_POINT('Ctrl Pts',(-15.3965620792199,12.4388403136538,
133.165691149699)) ;
#140210 = CARTESIAN_POINT('Ctrl Pts',(-15.2992076265801,12.4115721831835,
132.914391980506)) ;
#140211 = CARTESIAN_POINT('Ctrl Pts',(-15.2023640564988,12.457029412505,132.664680437339)) ;
#140212 = CARTESIAN_POINT('Ctrl Pts',(-15.1129280472859,12.5713337507617,
132.436462007858)) ;
#140213 = CARTESIAN_POINT('Ctrl Pts',(-15.0358830275159,12.7468028515201,
132.244532777634)) ;
#140214 = CARTESIAN_POINT('Ctrl Pts',(-14.9762423377458,12.9715572990884,
132.103535866445)) ;
#140215 = CARTESIAN_POINT('Ctrl Pts',(-14.937881335131,13.2272671330663,132.024507485665)) ;
#140216 = CARTESIAN_POINT('Ctrl Pts',(-14.9224295050719,13.498061880378,132.012548209648)) ;
#140217 = CARTESIAN_POINT('Ctrl Pts',(-14.9303375882874,13.762097452862,132.068641628803)) ;
#140218 = CARTESIAN_POINT('Ctrl Pts',(-14.9605151825436,14.0037249073099,
132.190050967125)) ;
#140219 = CARTESIAN_POINT('Ctrl Pts',(-15.0097098440868,14.2024000350369,
132.366798183917)) ;
#140220 = CARTESIAN_POINT('Ctrl Pts',(-15.0743428095158,14.3463072876563,
132.588901099298)) ;
#140221 = CARTESIAN_POINT('Ctrl Pts',(-15.1479112672098,14.4229407115658,
132.836760336969)) ;
#140222 = CARTESIAN_POINT('Ctrl Pts',(-15.2255189338972,14.428708721228,133.096623695493)) ;
#140223 = CARTESIAN_POINT('Ctrl Pts',(-15.3003705645565,14.3623691718519,
133.348383670699)) ;
#140224 = CARTESIAN_POINT('Ctrl Pts',(-15.3667024411799,14.2283779712588,
133.575366531252)) ;
#140225 = CARTESIAN_POINT('Ctrl Pts',(-15.4186463452488,14.036425640657,133.760290224072)) ;
#140226 = CARTESIAN_POINT('Ctrl Pts',(-15.4517469895417,13.8020944878478,
133.889958365334)) ;
#140227 = CARTESIAN_POINT('Ctrl Pts',(-15.463285244604,13.539161382227,133.956849228233)) ;
#140228 = CARTESIAN_POINT('Ctrl Pts',(-15.4514613937325,13.2686186839106,
133.955394191152)) ;
#140229 = CARTESIAN_POINT('Ctrl Pts',(-15.4163784741773,13.008641923509,133.886067414322)) ;
#140230 = CARTESIAN_POINT('Ctrl Pts',(-15.3601157103994,12.7791080577395,
133.754740538015)) ;
#140231 = CARTESIAN_POINT('Ctrl Pts',(-15.2851636273898,12.594297732826,133.569082969986)) ;
#140232 = CARTESIAN_POINT('Ctrl Pts',(-15.1973894002634,12.4702970553751,
133.34567823782)) ;
#140233 = CARTESIAN_POINT('Ctrl Pts',(-15.1013148538407,12.4139049863059,
133.098187796925)) ;
#140234 = CARTESIAN_POINT('Ctrl Pts',(-15.0038337445877,12.4297924309748,
132.846458188587)) ;
#140235 = CARTESIAN_POINT('Ctrl Pts',(-14.9102271599336,12.5172147404821,
132.606269401608)) ;
#140236 = CARTESIAN_POINT('Ctrl Pts',(-14.8274849504,12.6696685741938,132.397703669352)) ;
#140237 = CARTESIAN_POINT('Ctrl Pts',(-14.7606686055306,12.8748935986054,
132.235504695728)) ;
#140238 = CARTESIAN_POINT('Ctrl Pts',(-14.713205274637,13.1206629289391,132.130043070784)) ;
#140239 = CARTESIAN_POINT('Ctrl Pts',(-14.6882892081952,13.3874986938653,
132.090357347663)) ;
#140240 = CARTESIAN_POINT('Ctrl Pts',(-14.6868278663472,13.6577700467963,
132.119301620178)) ;
#140241 = CARTESIAN_POINT('Ctrl Pts',(-14.7082723715754,13.9102263569756,
132.215043319294)) ;
#140242 = CARTESIAN_POINT('Ctrl Pts',(-14.7500205778049,14.1273421335156,
132.369988376134)) ;
#140243 = CARTESIAN_POINT('Ctrl Pts',(-14.8090332618092,14.2954362023137,
132.575628202352)) ;
#140244 = CARTESIAN_POINT('Ctrl Pts',(-14.8796314850833,14.4001990478318,
132.8149219263)) ;
#140245 = CARTESIAN_POINT('Ctrl Pts',(-14.9567452239667,14.4351706372086,
133.073434822023)) ;
#140246 = CARTESIAN_POINT('Ctrl Pts',(-15.0330845819348,14.3977719556556,
133.329394582239)) ;
#140247 = CARTESIAN_POINT('Ctrl Pts',(-15.1036711595281,14.2904204336126,
133.568797663084)) ;
#140248 = CARTESIAN_POINT('Ctrl Pts',(-15.1620320097608,14.1205426251184,
133.772463469909)) ;
#140249 = CARTESIAN_POINT('Ctrl Pts',(-15.2031898781849,13.9015880320261,
133.925742184152)) ;
#140250 = CARTESIAN_POINT('Ctrl Pts',(-15.2238271094252,13.6483197654843,
134.019106406211)) ;
#140251 = CARTESIAN_POINT('Ctrl Pts',(-15.2215120354708,13.3774460111694,
134.045600707171)) ;
#140252 = CARTESIAN_POINT('Ctrl Pts',(-15.1957603044427,13.1115164178379,
134.003421898838)) ;
#140253 = CARTESIAN_POINT('Ctrl Pts',(-15.1477813157542,12.8676277530858,
133.896336050308)) ;
#140254 = CARTESIAN_POINT('Ctrl Pts',(-15.0801084681596,12.6630941709717,
133.731769988801)) ;
#140255 = CARTESIAN_POINT('Ctrl Pts',(-14.9967542423809,12.5128296668561,
133.521456097352)) ;
#140256 = CARTESIAN_POINT('Ctrl Pts',(-14.9032261050874,12.4280522223888,
133.281375642958)) ;
#140257 = CARTESIAN_POINT('Ctrl Pts',(-14.8053449711548,12.4147676725694,
133.028604017027)) ;
#140258 = CARTESIAN_POINT('Ctrl Pts',(-14.7098996424149,12.4732052197203,
132.782781794289)) ;
#140259 = CARTESIAN_POINT('Ctrl Pts',(-14.6217034426985,12.6008830294735,
132.558469618926)) ;
#140260 = CARTESIAN_POINT('Ctrl Pts',(-14.5481248406048,12.7859100383565,
132.376484190379)) ;
#140261 = CARTESIAN_POINT('Ctrl Pts',(-14.4923378930718,13.0171549996097,
132.246636772306)) ;
#140262 = CARTESIAN_POINT('Ctrl Pts',(-14.4580689419293,13.277402414091,132.179626600512)) ;
#140263 = CARTESIAN_POINT('Ctrl Pts',(-14.4470325556808,13.549209197848,132.180627324106)) ;
#140264 = CARTESIAN_POINT('Ctrl Pts',(-14.4593185955846,13.8101282641669,
132.249527993347)) ;
#140265 = CARTESIAN_POINT('Ctrl Pts',(-14.4931674421932,14.0442616351561,
132.381507611934)) ;
#140266 = CARTESIAN_POINT('Ctrl Pts',(-14.54604721898,14.234899690822,132.569317012515)) ;
#140267 = CARTESIAN_POINT('Ctrl Pts',(-14.6122274527619,14.3654882849947,
132.795571754127)) ;
#140268 = CARTESIAN_POINT('Ctrl Pts',(-14.6874535549381,14.4297229165876,
133.048520613647)) ;
#140269 = CARTESIAN_POINT('Ctrl Pts',(-14.7648483414879,14.4216680213317,
133.307667405615)) ;
#140270 = CARTESIAN_POINT('Ctrl Pts',(-14.8388106024003,14.3417421219821,
133.556976424616)) ;
#140271 = CARTESIAN_POINT('Ctrl Pts',(-14.902525642574,14.1964291634702,133.776164127113)) ;
#140272 = CARTESIAN_POINT('Ctrl Pts',(-14.9512314007499,13.9955519017587,
133.951576930874)) ;
#140273 = CARTESIAN_POINT('Ctrl Pts',(-14.9805749680013,13.7541464807844,
134.070361816232)) ;
#140274 = CARTESIAN_POINT('Ctrl Pts',(-14.9877159121976,13.4873870948836,
134.124497966682)) ;
#140275 = CARTESIAN_POINT('Ctrl Pts',(-14.971521850687,13.2187119173844,134.110122717758)) ;
#140276 = CARTESIAN_POINT('Ctrl Pts',(-14.9321810397444,12.9622340564561,
134.028441205295)) ;
#140277 = CARTESIAN_POINT('Ctrl Pts',(-14.8719267297993,12.7396655137431,
133.885562044107)) ;
#140278 = CARTESIAN_POINT('Ctrl Pts',(-14.7944437126708,12.5663130240366,
133.692322304437)) ;
#140279 = CARTESIAN_POINT('Ctrl Pts',(-14.7047726635642,12.4542929808878,
133.463380163604)) ;
#140280 = CARTESIAN_POINT('Ctrl Pts',(-14.607476851049,12.4113060989113,133.212457918896)) ;
#140281 = CARTESIAN_POINT('Ctrl Pts',(-14.5106107325521,12.4409729751149,
132.962445001237)) ;
#140282 = CARTESIAN_POINT('Ctrl Pts',(-14.4188178488728,12.5408195806537,
132.727450611251)) ;
#140283 = CARTESIAN_POINT('Ctrl Pts',(-14.3384318561653,12.7045177195062,
132.525834912788)) ;
#140284 = CARTESIAN_POINT('Ctrl Pts',(-14.2748650497426,12.9194126835292,
132.373269861623)) ;
#140285 = CARTESIAN_POINT('Ctrl Pts',(-14.2317360390318,13.1689179450109,
132.280236038816)) ;
#140286 = CARTESIAN_POINT('Ctrl Pts',(-14.2110498195284,13.4397285799231,
132.253160998047)) ;
#140287 = CARTESIAN_POINT('Ctrl Pts',(-14.2140521881657,13.706427055275,132.294912707361)) ;
#140288 = CARTESIAN_POINT('Ctrl Pts',(-14.2394774806085,13.953886295735,132.4023018521)) ;
#140289 = CARTESIAN_POINT('Ctrl Pts',(-14.2847952393077,14.1631927592464,
132.567747077305)) ;
#140290 = CARTESIAN_POINT('Ctrl Pts',(-14.3466522303324,14.3205261176051,
132.78177833072)) ;
#140291 = CARTESIAN_POINT('Ctrl Pts',(-14.4186082729192,14.4121066452954,
133.024918177311)) ;
#140292 = CARTESIAN_POINT('Ctrl Pts',(-14.4960761061432,14.4337042741575,
133.284423262461)) ;
#140293 = CARTESIAN_POINT('Ctrl Pts',(-14.572045561504,14.3826278175705,133.539455649795)) ;
#140294 = CARTESIAN_POINT('Ctrl Pts',(-14.6406034509692,14.2628852550259,
133.772863254736)) ;
#140295 = CARTESIAN_POINT('Ctrl Pts',(-14.6960408758465,14.08292617671,133.967940627217)) ;
#140296 = CARTESIAN_POINT('Ctrl Pts',(-14.7336909350444,13.8556922014923,
134.111058160493)) ;
#140297 = CARTESIAN_POINT('Ctrl Pts',(-14.7500422659047,13.597259905774,134.191980102552)) ;
#140298 = CARTESIAN_POINT('Ctrl Pts',(-14.7434335291913,13.3277679144463,
134.205648606387)) ;
#140299 = CARTESIAN_POINT('Ctrl Pts',(-14.7130192503405,13.0618109735796,
134.150210773176)) ;
#140300 = CARTESIAN_POINT('Ctrl Pts',(-14.6614036916594,12.826038953014,134.032246423453)) ;
#140301 = CARTESIAN_POINT('Ctrl Pts',(-14.5901948939726,12.6298696524396,
133.857494505776)) ;
#140302 = CARTESIAN_POINT('Ctrl Pts',(-14.5047155345941,12.4917687507878,
133.640863731031)) ;
#140303 = CARTESIAN_POINT('Ctrl Pts',(-14.4098125153078,12.4199839299598,
133.39680729441)) ;
#140304 = CARTESIAN_POINT('Ctrl Pts',(-14.3120256758759,12.4203084245316,
133.144238680783)) ;
#140305 = CARTESIAN_POINT('Ctrl Pts',(-14.2174033458745,12.4922084684858,
132.900911571252)) ;
#140306 = CARTESIAN_POINT('Ctrl Pts',(-14.1318404468406,12.6309969485081,
132.684106674944)) ;
#140307 = CARTESIAN_POINT('Ctrl Pts',(-14.060980194024,12.8263311670906,132.510212790672)) ;
#140308 = CARTESIAN_POINT('Ctrl Pts',(-14.0089205509473,13.0651228622206,
132.391338918913)) ;
#140309 = CARTESIAN_POINT('Ctrl Pts',(-13.9790169020332,13.3295668395412,
132.337169347488)) ;
#140310 = CARTESIAN_POINT('Ctrl Pts',(-13.9724839583839,13.5989124476963,
132.351047713643)) ;
#140311 = CARTESIAN_POINT('Ctrl Pts',(-13.9890431321451,13.8574711293399,
132.432615710829)) ;
#140312 = CARTESIAN_POINT('Ctrl Pts',(-14.0266628835637,14.0837079504238,
132.575528226051)) ;
#140313 = CARTESIAN_POINT('Ctrl Pts',(-14.0822847624689,14.2638192247761,
132.77121833331)) ;
#140314 = CARTESIAN_POINT('Ctrl Pts',(-14.1508947644669,14.3831695883009,
133.004767867683)) ;
#140315 = CARTESIAN_POINT('Ctrl Pts',(-14.2270177030481,14.4337176696405,
133.260307152951)) ;
#140316 = CARTESIAN_POINT('Ctrl Pts',(-14.3040474224697,14.4120588650256,
133.518338090565)) ;
#140317 = CARTESIAN_POINT('Ctrl Pts',(-14.376474347551,14.3193772960994,133.763103381234)) ;
#140318 = CARTESIAN_POINT('Ctrl Pts',(-14.4378412105215,14.162817091715,133.975462148985)) ;
#140319 = CARTESIAN_POINT('Ctrl Pts',(-14.4833931112873,13.9515916217657,
134.141862753533)) ;
#140320 = CARTESIAN_POINT('Ctrl Pts',(-14.5085472628772,13.7055233203187,
134.248235176747)) ;
#140321 = CARTESIAN_POINT('Ctrl Pts',(-14.5113140037808,13.4359481909895,
134.289656318574)) ;
#140322 = CARTESIAN_POINT('Ctrl Pts',(-14.4907836142237,13.1690262543573,
134.262549097928)) ;
#140323 = CARTESIAN_POINT('Ctrl Pts',(-14.4469946766069,12.9162728223831,
134.168041991638)) ;
#140324 = CARTESIAN_POINT('Ctrl Pts',(-14.3836515410097,12.7036779666449,
134.015865151141)) ;
#140325 = CARTESIAN_POINT('Ctrl Pts',(-14.3034207076497,12.5403117621087,
133.814645347195)) ;
#140326 = CARTESIAN_POINT('Ctrl Pts',(-14.2112317925761,12.4404489575973,
133.578615475842)) ;
#140327 = CARTESIAN_POINT('Ctrl Pts',(-14.1144092292276,12.4114485633587,
133.328709169712)) ;
#140328 = CARTESIAN_POINT('Ctrl Pts',(-14.0175084056,12.4544846403687,133.078809925647)) ;
#140329 = CARTESIAN_POINT('Ctrl Pts',(-13.9274154196742,12.5672617699685,
132.84879938857)) ;
#140330 = CARTESIAN_POINT('Ctrl Pts',(-13.8498913580063,12.7417744927464,
132.655533038876)) ;
#140331 = CARTESIAN_POINT('Ctrl Pts',(-13.7901365880796,12.9633750836739,
132.513923783402)) ;
#140332 = CARTESIAN_POINT('Ctrl Pts',(-13.7507723014847,13.2203111794704,
132.432225066762)) ;
#140333 = CARTESIAN_POINT('Ctrl Pts',(-13.7347687491892,13.4905143785451,
132.418587863191)) ;
#140334 = CARTESIAN_POINT('Ctrl Pts',(-13.7420428608409,13.7550216610133,
132.472844845919)) ;
#140335 = CARTESIAN_POINT('Ctrl Pts',(-13.7714788185508,13.996749630301,132.591960053501)) ;
#140336 = CARTESIAN_POINT('Ctrl Pts',(-13.8202931282288,14.1974242710986,
132.767691700884)) ;
#140337 = CARTESIAN_POINT('Ctrl Pts',(-13.8842419043715,14.342514003419,132.987636729813)) ;
#140338 = CARTESIAN_POINT('Ctrl Pts',(-13.957804359372,14.4218015954934,133.235581296981)) ;
#140339 = CARTESIAN_POINT('Ctrl Pts',(-14.0357822793224,14.4294553492896,
133.496688274969)) ;
#140340 = CARTESIAN_POINT('Ctrl Pts',(-14.1104232002843,14.3652618267525,
133.747675313763)) ;
#140341 = CARTESIAN_POINT('Ctrl Pts',(-14.1770034660584,14.2335996642439,
133.975322494504)) ;
#140342 = CARTESIAN_POINT('Ctrl Pts',(-14.2295331975556,14.0430658671341,
134.161995180824)) ;
#140343 = CARTESIAN_POINT('Ctrl Pts',(-14.263333326228,13.8093138339715,134.293777182255)) ;
#140344 = CARTESIAN_POINT('Ctrl Pts',(-14.2754798550196,13.5459139250659,
134.362562631417)) ;
#140345 = CARTESIAN_POINT('Ctrl Pts',(-14.2643602113247,13.2769103570782,
134.362972904705)) ;
#140346 = CARTESIAN_POINT('Ctrl Pts',(-14.2299858105317,13.0160046226691,
134.295749756055)) ;
#140347 = CARTESIAN_POINT('Ctrl Pts',(-14.1741543649749,12.7850161242088,
134.165746233419)) ;
#140348 = CARTESIAN_POINT('Ctrl Pts',(-14.0999513367095,12.5991696001074,
133.982162522111)) ;
#140349 = CARTESIAN_POINT('Ctrl Pts',(-14.0120333686313,12.4727066695535,
133.758511658872)) ;
#140350 = CARTESIAN_POINT('Ctrl Pts',(-13.9165608240464,12.4146340063818,
133.512615786361)) ;
#140351 = CARTESIAN_POINT('Ctrl Pts',(-13.8188267136632,12.428272476576,133.260222062798)) ;
#140352 = CARTESIAN_POINT('Ctrl Pts',(-13.725121388422,12.5136822248399,133.019706177829)) ;
#140353 = CARTESIAN_POINT('Ctrl Pts',(-13.6420048655474,12.6640313971838,
132.810020108338)) ;
#140354 = CARTESIAN_POINT('Ctrl Pts',(-13.5742807570679,12.8694014453016,
132.645391514411)) ;
#140355 = CARTESIAN_POINT('Ctrl Pts',(-13.5265676033014,13.1128473541502,
132.538991019669)) ;
#140356 = CARTESIAN_POINT('Ctrl Pts',(-13.5008984856995,13.3794713860966,
132.497132690037)) ;
#140357 = CARTESIAN_POINT('Ctrl Pts',(-13.498756156776,13.6493875676937,132.524020269698)) ;
#140358 = CARTESIAN_POINT('Ctrl Pts',(-13.5194308106777,13.9027716863457,
132.617509983294)) ;
#140359 = CARTESIAN_POINT('Ctrl Pts',(-13.5610331702241,14.1226003969304,
132.772288082141)) ;
#140360 = CARTESIAN_POINT('Ctrl Pts',(-13.6190505001098,14.2907614924808,
132.974692661995)) ;
#140361 = CARTESIAN_POINT('Ctrl Pts',(-13.6900034594533,14.3985142703266,
133.215330636002)) ;
#140362 = CARTESIAN_POINT('Ctrl Pts',(-13.766526148139,14.4350393250072,133.471887799925)) ;
#140363 = CARTESIAN_POINT('Ctrl Pts',(-13.8431005378829,14.4000355933247,
133.728594097503)) ;
#140364 = CARTESIAN_POINT('Ctrl Pts',(-13.9141839403901,14.294019258596,133.969566022421)) ;
#140365 = CARTESIAN_POINT('Ctrl Pts',(-13.9726902525623,14.1264036808229,
134.173517618549)) ;
#140366 = CARTESIAN_POINT('Ctrl Pts',(-14.01451107899,13.9087136081249,134.328754222631)) ;
#140367 = CARTESIAN_POINT('Ctrl Pts',(-14.0358023095098,13.6545233409047,
134.42423188298)) ;
#140368 = CARTESIAN_POINT('Ctrl Pts',(-14.03411729603,13.3858501132774,134.452316017563)) ;
#140369 = CARTESIAN_POINT('Ctrl Pts',(-14.0090696513313,13.1190055325829,
134.412261309148)) ;
#140370 = CARTESIAN_POINT('Ctrl Pts',(-13.9616116706279,12.8738785417747,
134.30674275505)) ;
#140371 = CARTESIAN_POINT('Ctrl Pts',(-13.8942434743611,12.6676053740016,
134.14314714961)) ;
#140372 = CARTESIAN_POINT('Ctrl Pts',(-13.8113184980164,12.5160771056389,
133.934042303186)) ;
#140373 = CARTESIAN_POINT('Ctrl Pts',(-13.7184439168081,12.4297444721253,
133.695718949214)) ;
#140374 = CARTESIAN_POINT('Ctrl Pts',(-13.6207083074889,12.4139325819383,
133.443334307576)) ;
#140375 = CARTESIAN_POINT('Ctrl Pts',(-13.5245613685599,12.4708186398046,
133.195662451093)) ;
#140376 = CARTESIAN_POINT('Ctrl Pts',(-13.4367983720263,12.5954481483175,
132.972323924776)) ;
#140377 = CARTESIAN_POINT('Ctrl Pts',(-13.3622573334654,12.7795463119932,
132.787704186982)) ;
#140378 = CARTESIAN_POINT('Ctrl Pts',(-13.3057627898852,13.0105018776207,
132.655886775255)) ;
#140379 = CARTESIAN_POINT('Ctrl Pts',(-13.2708885411926,13.270465957133,132.587139289259)) ;
#140380 = CARTESIAN_POINT('Ctrl Pts',(-13.2592549111302,13.5415025070648,
132.586306674461)) ;
#140381 = CARTESIAN_POINT('Ctrl Pts',(-13.2708395234052,13.8030870082756,
132.653165528328)) ;
#140382 = CARTESIAN_POINT('Ctrl Pts',(-13.304367480166,14.0389747692379,132.784348177691)) ;
#140383 = CARTESIAN_POINT('Ctrl Pts',(-13.3561244599786,14.2290324339817,
132.968488370536)) ;
#140384 = CARTESIAN_POINT('Ctrl Pts',(-13.4224801597023,14.36290013857,133.195546796567)) ;
#140385 = CARTESIAN_POINT('Ctrl Pts',(-13.4974004709148,14.4288302738408,
133.447521013397)) ;
#140386 = CARTESIAN_POINT('Ctrl Pts',(-13.5749660998,14.4228365201876,133.707240841845)) ;
#140387 = CARTESIAN_POINT('Ctrl Pts',(-13.6488630271482,14.3452102352826,
133.956235673057)) ;
#140388 = CARTESIAN_POINT('Ctrl Pts',(-13.7131159667098,14.2014203196955,
134.177078915254)) ;
#140389 = CARTESIAN_POINT('Ctrl Pts',(-13.7622546708898,14.0021641937243,
134.353713580636)) ;
#140390 = CARTESIAN_POINT('Ctrl Pts',(-13.7922217713026,13.761753127779,134.474321990283)) ;
#140391 = CARTESIAN_POINT('Ctrl Pts',(-13.8000681557409,13.4956080237515,
134.530495262172)) ;
#140392 = CARTESIAN_POINT('Ctrl Pts',(-13.7845110824094,13.2262845852455,
134.518046664834)) ;
#140393 = CARTESIAN_POINT('Ctrl Pts',(-13.7459650817114,12.9698876950621,
134.438579717807)) ;
#140394 = CARTESIAN_POINT('Ctrl Pts',(-13.6862141444836,12.7457364087332,
134.297226076074)) ;
#140395 = CARTESIAN_POINT('Ctrl Pts',(-13.6093646492958,12.5708017503329,
134.105774071566)) ;
#140396 = CARTESIAN_POINT('Ctrl Pts',(-13.519124823432,12.4561497112336,133.875476397484)) ;
#140397 = CARTESIAN_POINT('Ctrl Pts',(-13.422988713799,12.4116404870858,133.62757363074)) ;
#140398 = CARTESIAN_POINT('Ctrl Pts',(-13.3252747688584,12.4391729336107,
133.375352092848)) ;
#140399 = CARTESIAN_POINT('Ctrl Pts',(-13.2335160894411,12.5371797633224,
133.140365473548)) ;
#140400 = CARTESIAN_POINT('Ctrl Pts',(-13.1529574964824,12.6985743471033,
132.938147247073)) ;
#140401 = CARTESIAN_POINT('Ctrl Pts',(-13.0887851662366,12.9117741360547,
132.783784142342)) ;
#140402 = CARTESIAN_POINT('Ctrl Pts',(-13.0447718180386,13.1624013152274,
132.688415632104)) ;
#140403 = CARTESIAN_POINT('Ctrl Pts',(-13.0236022557923,13.4305279145417,
132.659623972586)) ;
#140404 = CARTESIAN_POINT('Ctrl Pts',(-13.0258219823811,13.6988963516455,
132.699258391825)) ;
#140405 = CARTESIAN_POINT('Ctrl Pts',(-13.0506572284253,13.9472005386101,
132.804920173535)) ;
#140406 = CARTESIAN_POINT('Ctrl Pts',(-13.0955424206449,14.1580510630495,
132.969155849435)) ;
#140407 = CARTESIAN_POINT('Ctrl Pts',(-13.1567221725549,14.3165352363587,
133.181063812817)) ;
#140408 = CARTESIAN_POINT('Ctrl Pts',(-13.228807081375,14.4105996668628,133.424752925939)) ;
#140409 = CARTESIAN_POINT('Ctrl Pts',(-13.306007393883,14.4340684651961,133.683379684526)) ;
#140410 = CARTESIAN_POINT('Ctrl Pts',(-13.382228905179,14.3850543896185,133.939203970425)) ;
#140411 = CARTESIAN_POINT('Ctrl Pts',(-13.4510738585261,14.2669952300402,
134.173456810545)) ;
#140412 = CARTESIAN_POINT('Ctrl Pts',(-13.506810496423,14.0891154364107,134.369318142891)) ;
#140413 = CARTESIAN_POINT('Ctrl Pts',(-13.5451041794166,13.8629228835357,
134.5143452011)) ;
#140414 = CARTESIAN_POINT('Ctrl Pts',(-13.5621329454697,13.6044943724102,
134.597322473916)) ;
#140415 = CARTESIAN_POINT('Ctrl Pts',(-13.5560956962621,13.3352195562946,
134.612648137411)) ;
#140416 = CARTESIAN_POINT('Ctrl Pts',(-13.5266617961689,13.0705829535361,
134.559838132771)) ;
#140417 = CARTESIAN_POINT('Ctrl Pts',(-13.475276995217,12.8316692334543,134.44283011763)) ;
#140418 = CARTESIAN_POINT('Ctrl Pts',(-13.4044073000562,12.6342706260099,
134.26908401501)) ;
#140419 = CARTESIAN_POINT('Ctrl Pts',(-13.3195945751411,12.4949548036794,
134.05427628367)) ;
#140420 = CARTESIAN_POINT('Ctrl Pts',(-13.2248596249454,12.4210676160077,
133.810718608612)) ;
#140421 = CARTESIAN_POINT('Ctrl Pts',(-13.1271993154374,12.4192534817676,
133.558478104923)) ;
#140422 = CARTESIAN_POINT('Ctrl Pts',(-13.0322252201144,12.4890551014873,
133.314175173155)) ;
#140423 = CARTESIAN_POINT('Ctrl Pts',(-12.9459982367621,12.626926545497,133.095576978998)) ;
#140424 = CARTESIAN_POINT('Ctrl Pts',(-12.8751217655022,12.8196495679067,
132.921424109731)) ;
#140425 = CARTESIAN_POINT('Ctrl Pts',(-12.8222774142593,13.0580836243581,
132.800361858401)) ;
#140426 = CARTESIAN_POINT('Ctrl Pts',(-12.7917934093607,13.3214662460235,
132.744416520862)) ;
#140427 = CARTESIAN_POINT('Ctrl Pts',(-12.7845758914213,13.5912987745739,
132.756352051933)) ;
#140428 = CARTESIAN_POINT('Ctrl Pts',(-12.8003737957129,13.8497219287496,
132.835584198493)) ;
#140429 = CARTESIAN_POINT('Ctrl Pts',(-12.8377457211529,14.0789422598233,
132.978048098674)) ;
#140430 = CARTESIAN_POINT('Ctrl Pts',(-12.8928878000828,14.2597601138698,
133.172246822458)) ;
#140431 = CARTESIAN_POINT('Ctrl Pts',(-12.960949978305,14.3805241665643,133.404082488237)) ;
#140432 = CARTESIAN_POINT('Ctrl Pts',(-13.036840414061,14.4333051065353,133.658899622232)) ;
#140433 = CARTESIAN_POINT('Ctrl Pts',(-13.1142347421023,14.4135763153339,
133.91813556721)) ;
#140434 = CARTESIAN_POINT('Ctrl Pts',(-13.1867830255326,14.3230159864486,
134.163193889297)) ;
#140435 = CARTESIAN_POINT('Ctrl Pts',(-13.2487470576845,14.1669880697449,
134.377473831657)) ;
#140436 = CARTESIAN_POINT('Ctrl Pts',(-13.2942601671939,13.9601855092309,
134.543287341378)) ;
#140437 = CARTESIAN_POINT('Ctrl Pts',(-13.3203995351673,13.7121979724763,
134.652938896133)) ;
#140438 = CARTESIAN_POINT('Ctrl Pts',(-13.3238270184238,13.4453254354835,
134.695977657837)) ;
#140439 = CARTESIAN_POINT('Ctrl Pts',(-13.3037973870205,13.1756579328103,
134.670656958844)) ;
#140440 = CARTESIAN_POINT('Ctrl Pts',(-13.2611344959684,12.9248371133689,
134.579064456657)) ;
#140441 = CARTESIAN_POINT('Ctrl Pts',(-13.1978850472197,12.7087904209721,
134.427462742701)) ;
#140442 = CARTESIAN_POINT('Ctrl Pts',(-13.1180880272232,12.5441839973877,
134.227467431422)) ;
#140443 = CARTESIAN_POINT('Ctrl Pts',(-13.0261903296275,12.4422953631874,
133.992282641388)) ;
#140444 = CARTESIAN_POINT('Ctrl Pts',(-12.9292309041857,12.4112745922159,
133.742044880422)) ;
#140445 = CARTESIAN_POINT('Ctrl Pts',(-12.8324220446461,12.4523611240387,
133.492352590847)) ;
#140446 = CARTESIAN_POINT('Ctrl Pts',(-12.7422827853316,12.5627156272335,
133.262109881724)) ;
#140447 = CARTESIAN_POINT('Ctrl Pts',(-12.6640304336884,12.7362032335438,
133.066838486923)) ;
#140448 = CARTESIAN_POINT('Ctrl Pts',(-12.6038457715157,12.9562237014372,
132.923907669484)) ;
#140449 = CARTESIAN_POINT('Ctrl Pts',(-12.5638033798923,13.2127632436766,
132.840271448791)) ;
#140450 = CARTESIAN_POINT('Ctrl Pts',(-12.5471482690012,13.4814739931662,
132.824565254559)) ;
#140451 = CARTESIAN_POINT('Ctrl Pts',(-12.55368247659,13.7476020769462,132.876805340507)) ;
#140452 = CARTESIAN_POINT('Ctrl Pts',(-12.5826455210226,13.9907502707064,
132.99461409777)) ;
#140453 = CARTESIAN_POINT('Ctrl Pts',(-12.6308355205781,14.1921268766281,
133.168425407229)) ;
#140454 = CARTESIAN_POINT('Ctrl Pts',(-12.6943294952942,14.3392030436754,
133.387020626531)) ;
#140455 = CARTESIAN_POINT('Ctrl Pts',(-12.7683012220631,14.4207500230976,
133.636423571384)) ;
#140456 = CARTESIAN_POINT('Ctrl Pts',(-12.8455310116652,14.4302362583739,
133.895028948852)) ;
#140457 = CARTESIAN_POINT('Ctrl Pts',(-12.9207429495786,14.368028270843,134.147861599825)) ;
#140458 = CARTESIAN_POINT('Ctrl Pts',(-12.9877312267405,14.2375543492764,
134.376766361089)) ;
#140459 = CARTESIAN_POINT('Ctrl Pts',(-13.040561290709,14.0487159657188,134.564249356536)) ;
#140460 = CARTESIAN_POINT('Ctrl Pts',(-13.0748031716909,13.8167883871292,
134.697210227898)) ;
#140461 = CARTESIAN_POINT('Ctrl Pts',(-13.0876734641736,13.5548284865375,
134.768007071369)) ;
#140462 = CARTESIAN_POINT('Ctrl Pts',(-13.0772469786685,13.2844750332118,
134.770603967705)) ;
#140463 = CARTESIAN_POINT('Ctrl Pts',(-13.0433961018683,13.0226683900031,
134.704959155467)) ;
#140464 = CARTESIAN_POINT('Ctrl Pts',(-12.9882858427434,12.7913019843532,
134.57696772602)) ;
#140465 = CARTESIAN_POINT('Ctrl Pts',(-12.9146582473163,12.6040507467942,
134.395030630286)) ;
#140466 = CARTESIAN_POINT('Ctrl Pts',(-12.8271396558594,12.4756113935465,
134.172527392137)) ;
#140467 = CARTESIAN_POINT('Ctrl Pts',(-12.7315130264268,12.415243488117,133.92628699965)) ;
#140468 = CARTESIAN_POINT('Ctrl Pts',(-12.6338160664484,12.4269403743014,
133.673979806236)) ;
#140469 = CARTESIAN_POINT('Ctrl Pts',(-12.5401199150452,12.5099953063745,
133.433406758865)) ;
#140470 = CARTESIAN_POINT('Ctrl Pts',(-12.4565010249555,12.6587329054093,
133.222300982003)) ;
#140471 = CARTESIAN_POINT('Ctrl Pts',(-12.3884365161738,12.8618952127667,
133.056565584079)) ;
#140472 = CARTESIAN_POINT('Ctrl Pts',(-12.3398181635713,13.1054069861002,
132.94766934641)) ;
#140473 = CARTESIAN_POINT('Ctrl Pts',(-12.3135058293376,13.3721987049067,
132.903992343846)) ;
#140474 = CARTESIAN_POINT('Ctrl Pts',(-12.3107188025145,13.6415134162569,
132.928902598688)) ;
#140475 = CARTESIAN_POINT('Ctrl Pts',(-12.3306845058955,13.8954057310282,
133.020287129816)) ;
#140476 = CARTESIAN_POINT('Ctrl Pts',(-12.3717562411778,14.1169004710299,
133.173562993441)) ;
#140477 = CARTESIAN_POINT('Ctrl Pts',(-12.4295072043719,14.2868623267828,
133.375258269535)) ;
#140478 = CARTESIAN_POINT('Ctrl Pts',(-12.4997409250019,14.396013035847,133.613591802194)) ;
#140479 = CARTESIAN_POINT('Ctrl Pts',(-12.5764706947144,14.4351149224746,
133.870891973931)) ;
#140480 = CARTESIAN_POINT('Ctrl Pts',(-12.6532429349451,14.4019052027925,
134.128227117607)) ;
#140481 = CARTESIAN_POINT('Ctrl Pts',(-12.7243502344129,14.2983009187854,
134.369151253832)) ;
#140482 = CARTESIAN_POINT('Ctrl Pts',(-12.7835198481276,14.1317969224175,
134.575164716449)) ;
#140483 = CARTESIAN_POINT('Ctrl Pts',(-12.8257831979134,13.91534337541,134.731670450177)) ;
#140484 = CARTESIAN_POINT('Ctrl Pts',(-12.8476480318692,13.6633971728162,
134.828641412771)) ;
#140485 = CARTESIAN_POINT('Ctrl Pts',(-12.8467867250038,13.3943409490525,
134.859209219661)) ;
#140486 = CARTESIAN_POINT('Ctrl Pts',(-12.8222377970458,13.125759500651,134.820784175439)) ;
#140487 = CARTESIAN_POINT('Ctrl Pts',(-12.7754966528095,12.8806964753524,
134.717244165718)) ;
#140488 = CARTESIAN_POINT('Ctrl Pts',(-12.7088929602356,12.6734733763792,
134.555794010594)) ;
#140489 = CARTESIAN_POINT('Ctrl Pts',(-12.626209768345,12.5195858185458,134.347470896474)) ;
#140490 = CARTESIAN_POINT('Ctrl Pts',(-12.5330823146692,12.4310932740595,
134.108568204543)) ;
#140491 = CARTESIAN_POINT('Ctrl Pts',(-12.4359002404825,12.4134132696985,
133.857624810028)) ;
#140492 = CARTESIAN_POINT('Ctrl Pts',(-12.3394913697739,12.4681188633571,
133.609228819744)) ;
#140493 = CARTESIAN_POINT('Ctrl Pts',(-12.2514122847404,12.5909169506631,
133.384966928797)) ;
#140494 = CARTESIAN_POINT('Ctrl Pts',(-12.1764252467238,12.7734489072163,
133.199042308447)) ;
#140495 = CARTESIAN_POINT('Ctrl Pts',(-12.1194045389883,13.0028154211787,
133.0656283448)) ;
#140496 = CARTESIAN_POINT('Ctrl Pts',(-12.0838153267167,13.2626812904981,
132.994861198184)) ;
#140497 = CARTESIAN_POINT('Ctrl Pts',(-12.0714655142961,13.5323091961428,
132.991764635821)) ;
#140498 = CARTESIAN_POINT('Ctrl Pts',(-12.0824257373207,13.7963543423531,
133.057045713881)) ;
#140499 = CARTESIAN_POINT('Ctrl Pts',(-12.1152947061301,14.0324258066149,
133.186186490251)) ;
#140500 = CARTESIAN_POINT('Ctrl Pts',(-12.1666377019664,14.2243211732623,
133.369177652466)) ;
#140501 = CARTESIAN_POINT('Ctrl Pts',(-12.232476473759,14.3597396975641,133.594637060158)) ;
#140502 = CARTESIAN_POINT('Ctrl Pts',(-12.3074797976533,14.4280132150894,
133.846971383581)) ;
#140503 = CARTESIAN_POINT('Ctrl Pts',(-12.3850141728136,14.4240026931505,
134.106576784609)) ;
#140504 = CARTESIAN_POINT('Ctrl Pts',(-12.4591545841739,14.348214877112,134.356314139757)) ;
#140505 = CARTESIAN_POINT('Ctrl Pts',(-12.5235535888618,14.2066839106137,
134.577474272231)) ;
#140506 = CARTESIAN_POINT('Ctrl Pts',(-12.5733676119359,14.0084844644838,
134.756165192188)) ;
#140507 = CARTESIAN_POINT('Ctrl Pts',(-12.6039525352688,13.76791632806,134.878710146275)) ;
#140508 = CARTESIAN_POINT('Ctrl Pts',(-12.612364118678,13.5034893328133,134.936368413095)) ;
#140509 = CARTESIAN_POINT('Ctrl Pts',(-12.5974803065642,13.2335994078643,
134.925943717301)) ;
#140510 = CARTESIAN_POINT('Ctrl Pts',(-12.5595099792057,12.976407627843,134.84817680895)) ;
#140511 = CARTESIAN_POINT('Ctrl Pts',(-12.5001716230381,12.7508792337382,
134.708077669362)) ;
#140512 = CARTESIAN_POINT('Ctrl Pts',(-12.4240025586213,12.5752390532541,
134.518488422095)) ;
#140513 = CARTESIAN_POINT('Ctrl Pts',(-12.3345444898954,12.4588914929926,
134.290312537568)) ;
#140514 = CARTESIAN_POINT('Ctrl Pts',(-12.2379671531426,12.4118138328558,
134.041315824821)) ;
#140515 = CARTESIAN_POINT('Ctrl Pts',(-12.1402200536129,12.4374481799832,
133.78898690417)) ;
#140516 = CARTESIAN_POINT('Ctrl Pts',(-12.0482373710984,12.5333386552095,
133.553332360909)) ;
#140517 = CARTESIAN_POINT('Ctrl Pts',(-11.9669627091784,12.6939674039094,
133.349171653341)) ;
#140518 = CARTESIAN_POINT('Ctrl Pts',(-11.902619330109,12.9050031482846,133.194150919962)) ;
#140519 = CARTESIAN_POINT('Ctrl Pts',(-11.857873910087,13.1551455919413,133.096696395566)) ;
#140520 = CARTESIAN_POINT('Ctrl Pts',(-11.8433730930553,13.3338157805737,
133.076375626011)) ;
#140521 = CARTESIAN_POINT('Ctrl Pts',(-11.83998730453,13.4231220893089,133.077505617122)) ;
#140522 = CARTESIAN_POINT('Ctrl Pts',(-33.1829052539887,13.1734341962953,
127.851905049753)) ;
#140523 = CARTESIAN_POINT('Ctrl Pts',(-33.1822017070797,13.1676985268958,
127.850580772544)) ;
#140524 = CARTESIAN_POINT('Ctrl Pts',(-33.1707280433469,13.076204201721,127.828745770272)) ;
#140525 = CARTESIAN_POINT('Ctrl Pts',(-33.1397508853579,12.9034784200084,
127.761228635573)) ;
#140526 = CARTESIAN_POINT('Ctrl Pts',(-33.0750750970862,12.6923997924798,
127.605316905031)) ;
#140527 = CARTESIAN_POINT('Ctrl Pts',(-32.9941099257864,12.5327609197045,
127.401903291373)) ;
#140528 = CARTESIAN_POINT('Ctrl Pts',(-32.9014522171935,12.4368205686394,
127.16450033503)) ;
#140529 = CARTESIAN_POINT('Ctrl Pts',(-32.8045123363909,12.4119420237697,
126.914243813896)) ;
#140530 = CARTESIAN_POINT('Ctrl Pts',(-32.7076862120277,12.4592681498074,
126.664616426665)) ;
#140531 = CARTESIAN_POINT('Ctrl Pts',(-32.6184092522946,12.575659036236,126.436908031571)) ;
#140532 = CARTESIAN_POINT('Ctrl Pts',(-32.5418309193606,12.75283542717,126.246347133038)) ;
#140533 = CARTESIAN_POINT('Ctrl Pts',(-32.4829016852876,12.9779971811105,
126.107323458936)) ;
#140534 = CARTESIAN_POINT('Ctrl Pts',(-32.4450817095912,13.2349354675193,
126.029955963063)) ;
#140535 = CARTESIAN_POINT('Ctrl Pts',(-32.4302650083729,13.5051819451432,
126.019763187868)) ;
#140536 = CARTESIAN_POINT('Ctrl Pts',(-32.4389881142122,13.7710457079463,
126.078535238366)) ;
#140537 = CARTESIAN_POINT('Ctrl Pts',(-32.4695784674888,14.0095406593372,
126.200858990596)) ;
#140538 = CARTESIAN_POINT('Ctrl Pts',(-32.5193506356405,14.2073761046424,
126.379385142619)) ;
#140539 = CARTESIAN_POINT('Ctrl Pts',(-32.5839721986,14.3489569855306,126.601275613991)) ;
#140540 = CARTESIAN_POINT('Ctrl Pts',(-32.6582948498371,14.4243647659385,
126.851602957494)) ;
#140541 = CARTESIAN_POINT('Ctrl Pts',(-32.735855999385,14.427672591071,127.111298260045)) ;
#140542 = CARTESIAN_POINT('Ctrl Pts',(-32.8104552893985,14.3592845353793,
127.362291590965)) ;
#140543 = CARTESIAN_POINT('Ctrl Pts',(-32.8762278669798,14.2239082001409,
127.587533236593)) ;
#140544 = CARTESIAN_POINT('Ctrl Pts',(-32.927746682636,14.0309430574059,127.77118384942)) ;
#140545 = CARTESIAN_POINT('Ctrl Pts',(-32.960457263088,13.7937231411456,127.899964110698)) ;
#140546 = CARTESIAN_POINT('Ctrl Pts',(-32.9712029509523,13.5318368827659,
127.964333838362)) ;
#140547 = CARTESIAN_POINT('Ctrl Pts',(-32.9587611170759,13.260908758679,127.961130078476)) ;
#140548 = CARTESIAN_POINT('Ctrl Pts',(-32.9229367694298,13.0011530565724,
127.889686187424)) ;
#140549 = CARTESIAN_POINT('Ctrl Pts',(-32.8660948183366,12.7729626729889,
127.756647910718)) ;
#140550 = CARTESIAN_POINT('Ctrl Pts',(-32.790924635143,12.5901801237826,127.570254799383)) ;
#140551 = CARTESIAN_POINT('Ctrl Pts',(-32.7027029653519,12.4676467713314,
127.345605003568)) ;
#140552 = CARTESIAN_POINT('Ctrl Pts',(-32.6063037446173,12.413314501038,127.097226465731)) ;
#140553 = CARTESIAN_POINT('Ctrl Pts',(-32.5089710404186,12.4313809059018,
126.845895281843)) ;
#140554 = CARTESIAN_POINT('Ctrl Pts',(-32.4157240307319,12.5206603484656,
126.60670957826)) ;
#140555 = CARTESIAN_POINT('Ctrl Pts',(-32.3334682191733,12.6744196148216,
126.399508808185)) ;
#140556 = CARTESIAN_POINT('Ctrl Pts',(-32.2669019929393,12.8815893341258,
126.238150872134)) ;
#140557 = CARTESIAN_POINT('Ctrl Pts',(-32.2200131818392,13.1290193456038,
126.134455135357)) ;
#140558 = CARTESIAN_POINT('Ctrl Pts',(-32.1959308651233,13.3950772518204,
126.097064150513)) ;
#140559 = CARTESIAN_POINT('Ctrl Pts',(-32.1950470896664,13.6643422142601,
126.127596808045)) ;
#140560 = CARTESIAN_POINT('Ctrl Pts',(-32.2171232020604,13.9170737538833,
126.22530306428)) ;
#140561 = CARTESIAN_POINT('Ctrl Pts',(-32.2596149976549,14.1334228161875,
126.38252083197)) ;
#140562 = CARTESIAN_POINT('Ctrl Pts',(-32.3187058370602,14.2989215629879,
126.588198409019)) ;
#140563 = CARTESIAN_POINT('Ctrl Pts',(-32.3896496930304,14.4021434472197,
126.828560375048)) ;
#140564 = CARTESIAN_POINT('Ctrl Pts',(-32.4667661198528,14.4351203025954,
127.087043208967)) ;
#140565 = CARTESIAN_POINT('Ctrl Pts',(-32.5432148615198,14.3956460282901,
127.343411947521)) ;
#140566 = CARTESIAN_POINT('Ctrl Pts',(-32.6134644972313,14.2864256300776,
127.581799379627)) ;
#140567 = CARTESIAN_POINT('Ctrl Pts',(-32.6713951718574,14.1149875929984,
127.784205127976)) ;
#140568 = CARTESIAN_POINT('Ctrl Pts',(-32.7120127070859,13.8950778464839,
127.935876391714)) ;
#140569 = CARTESIAN_POINT('Ctrl Pts',(-32.7320620935371,13.6402948775312,
128.027626314225)) ;
#140570 = CARTESIAN_POINT('Ctrl Pts',(-32.7290666324127,13.3700134780419,
128.052035270306)) ;
#140571 = CARTESIAN_POINT('Ctrl Pts',(-32.7026474802242,13.1040820089462,
128.007955758887)) ;
#140572 = CARTESIAN_POINT('Ctrl Pts',(-32.6540267104507,12.8608603098162,
127.899019977621)) ;
#140573 = CARTESIAN_POINT('Ctrl Pts',(-32.5854756864029,12.6570994974887,
127.732029152198)) ;
#140574 = CARTESIAN_POINT('Ctrl Pts',(-32.5022717478729,12.509712563052,127.521931848437)) ;
#140575 = CARTESIAN_POINT('Ctrl Pts',(-32.4084850460521,12.4266925565407,
127.281125909087)) ;
#140576 = CARTESIAN_POINT('Ctrl Pts',(-32.310691262548,12.4153566228605,127.028564089873)) ;
#140577 = CARTESIAN_POINT('Ctrl Pts',(-32.2150851456372,12.476118398497,126.782387345234)) ;
#140578 = CARTESIAN_POINT('Ctrl Pts',(-32.127774202705,12.6046110942521,126.56043246527)) ;
#140579 = CARTESIAN_POINT('Ctrl Pts',(-32.0541365166832,12.7920330529179,
126.378478818651)) ;
#140580 = CARTESIAN_POINT('Ctrl Pts',(-31.9989567177235,13.024646117744,126.250422902348)) ;
#140581 = CARTESIAN_POINT('Ctrl Pts',(-31.9654247728656,13.2849677628749,
126.1855063369)) ;
#140582 = CARTESIAN_POINT('Ctrl Pts',(-31.9549988878817,13.5561840574451,
126.188214091077)) ;
#140583 = CARTESIAN_POINT('Ctrl Pts',(-31.9680215372011,13.8182131440166,
126.259475848264)) ;
#140584 = CARTESIAN_POINT('Ctrl Pts',(-32.0024636779742,14.0504675663447,
126.393099467081)) ;
#140585 = CARTESIAN_POINT('Ctrl Pts',(-32.0555990348147,14.2392689175362,
126.581558183895)) ;
#140586 = CARTESIAN_POINT('Ctrl Pts',(-32.1225545405442,14.3686949412613,
126.810291039521)) ;
#140587 = CARTESIAN_POINT('Ctrl Pts',(-32.1974429751412,14.4303698787607,
127.062026290213)) ;
#140588 = CARTESIAN_POINT('Ctrl Pts',(-32.2751076283904,14.4203874176643,
127.322092039128)) ;
#140589 = CARTESIAN_POINT('Ctrl Pts',(-32.3488485574625,14.3383233721809,
127.570744810303)) ;
#140590 = CARTESIAN_POINT('Ctrl Pts',(-32.4122411169408,14.1909246457993,
127.789035722479)) ;
#140591 = CARTESIAN_POINT('Ctrl Pts',(-32.4602486483851,13.9894771384923,
127.962269753473)) ;
#140592 = CARTESIAN_POINT('Ctrl Pts',(-32.4890445130519,13.7468082771736,
128.079510678355)) ;
#140593 = CARTESIAN_POINT('Ctrl Pts',(-32.4955954256572,13.4802542547444,
128.131844086168)) ;
#140594 = CARTESIAN_POINT('Ctrl Pts',(-32.478469745498,13.2092850470841,128.115057379737)) ;
#140595 = CARTESIAN_POINT('Ctrl Pts',(-32.4388473343741,12.9563426353649,
128.032190557193)) ;
#140596 = CARTESIAN_POINT('Ctrl Pts',(-32.3779866617617,12.7340442685521,
127.887643915871)) ;
#140597 = CARTESIAN_POINT('Ctrl Pts',(-32.299867961373,12.5620254310283,127.692615984056)) ;
#140598 = CARTESIAN_POINT('Ctrl Pts',(-32.2100641323022,12.4521634508898,
127.463232611462)) ;
#140599 = CARTESIAN_POINT('Ctrl Pts',(-32.1127429550496,12.4110698291516,
127.212210279697)) ;
#140600 = CARTESIAN_POINT('Ctrl Pts',(-32.0154678803892,12.4431134789288,
126.961170458623)) ;
#140601 = CARTESIAN_POINT('Ctrl Pts',(-31.9243509526054,12.544720780955,126.728008980324)) ;
#140602 = CARTESIAN_POINT('Ctrl Pts',(-31.8445157820833,12.709460812036,126.527923986169)) ;
#140603 = CARTESIAN_POINT('Ctrl Pts',(-31.7812567007112,12.9261933468861,
126.376356950201)) ;
#140604 = CARTESIAN_POINT('Ctrl Pts',(-31.7387566453158,13.1767718332297,
126.285192483539)) ;
#140605 = CARTESIAN_POINT('Ctrl Pts',(-31.7187641728704,13.4474343197197,
126.260094130827)) ;
#140606 = CARTESIAN_POINT('Ctrl Pts',(-31.722478133967,13.7143157713228,126.30399452411)) ;
#140607 = CARTESIAN_POINT('Ctrl Pts',(-31.7483943853981,13.960120914319,126.412695890686)) ;
#140608 = CARTESIAN_POINT('Ctrl Pts',(-31.7945444045731,14.1691500544874,
126.580769734858)) ;
#140609 = CARTESIAN_POINT('Ctrl Pts',(-31.8562068674074,14.3234013156229,
126.793917930162)) ;
#140610 = CARTESIAN_POINT('Ctrl Pts',(-31.9288536888432,14.4138714588237,
127.039311176437)) ;
#140611 = CARTESIAN_POINT('Ctrl Pts',(-32.0060870905907,14.4332950652812,
127.297997340453)) ;
#140612 = CARTESIAN_POINT('Ctrl Pts',(-32.0823890649229,14.37983766652,127.554210022575)) ;
#140613 = CARTESIAN_POINT('Ctrl Pts',(-32.1503082521653,14.2584887072528,
127.78560535761)) ;
#140614 = CARTESIAN_POINT('Ctrl Pts',(-32.2053364256527,14.0772214064872,
127.979479297461)) ;
#140615 = CARTESIAN_POINT('Ctrl Pts',(-32.2425093340143,13.8478579716949,
128.12133345147)) ;
#140616 = CARTESIAN_POINT('Ctrl Pts',(-32.2581355201543,13.5896598560144,
128.200019474609)) ;
#140617 = CARTESIAN_POINT('Ctrl Pts',(-32.2507950956267,13.3195388423839,
128.211625689801)) ;
#140618 = CARTESIAN_POINT('Ctrl Pts',(-32.2199693000412,13.0556169732422,
128.15477837076)) ;
#140619 = CARTESIAN_POINT('Ctrl Pts',(-32.1673744065339,12.8189342678657,
128.034219532277)) ;
#140620 = CARTESIAN_POINT('Ctrl Pts',(-32.0958634953359,12.625100278912,127.85846209906)) ;
#140621 = CARTESIAN_POINT('Ctrl Pts',(-32.0100232598123,12.4887479023081,
127.640792149346)) ;
#140622 = CARTESIAN_POINT('Ctrl Pts',(-31.9152601979825,12.4190670277806,
127.397034402997)) ;
#140623 = CARTESIAN_POINT('Ctrl Pts',(-31.8170693261966,12.4213699947317,
127.143425394833)) ;
#140624 = CARTESIAN_POINT('Ctrl Pts',(-31.7227136755124,12.4953802874648,
126.900850182708)) ;
#140625 = CARTESIAN_POINT('Ctrl Pts',(-31.6374854970419,12.6359572758876,
126.685028308691)) ;
#140626 = CARTESIAN_POINT('Ctrl Pts',(-31.5671047785113,12.8329198121217,
126.512552465339)) ;
#140627 = CARTESIAN_POINT('Ctrl Pts',(-31.5158144349701,13.0719650653609,
126.395824465428)) ;
#140628 = CARTESIAN_POINT('Ctrl Pts',(-31.4865010466435,13.3363498058402,
126.343322488749)) ;
#140629 = CARTESIAN_POINT('Ctrl Pts',(-31.4805966443912,13.6070577541681,
126.359216016363)) ;
#140630 = CARTESIAN_POINT('Ctrl Pts',(-31.4978044189705,13.8644612546569,
126.442613640301)) ;
#140631 = CARTESIAN_POINT('Ctrl Pts',(-31.5360863271803,14.0900773467752,
126.58754221147)) ;
#140632 = CARTESIAN_POINT('Ctrl Pts',(-31.5921228560885,14.2682172866369,
126.784395510653)) ;
#140633 = CARTESIAN_POINT('Ctrl Pts',(-31.6608593459301,14.38541662164,127.018239393372)) ;
#140634 = CARTESIAN_POINT('Ctrl Pts',(-31.7370055456571,14.4341663230829,
127.273806703938)) ;
#140635 = CARTESIAN_POINT('Ctrl Pts',(-31.8144395184252,14.4102121199937,
127.533219786427)) ;
#140636 = CARTESIAN_POINT('Ctrl Pts',(-31.8864208486602,14.3156228992233,
127.776589906109)) ;
#140637 = CARTESIAN_POINT('Ctrl Pts',(-31.9474114950274,14.1571117178342,
127.98788495547)) ;
#140638 = CARTESIAN_POINT('Ctrl Pts',(-31.992225383611,13.9459763961177,128.151923385783)) ;
#140639 = CARTESIAN_POINT('Ctrl Pts',(-32.016932083013,13.697562228916,128.257202644968)) ;
#140640 = CARTESIAN_POINT('Ctrl Pts',(-32.0190519674874,13.4293975021098,
128.296514762563)) ;
#140641 = CARTESIAN_POINT('Ctrl Pts',(-31.9977507903844,13.1610019423395,
128.267377292458)) ;
#140642 = CARTESIAN_POINT('Ctrl Pts',(-31.9536261139503,12.9105848484096,
128.171675551657)) ;
#140643 = CARTESIAN_POINT('Ctrl Pts',(-31.8893635388713,12.6976134704073,
128.017048897951)) ;
#140644 = CARTESIAN_POINT('Ctrl Pts',(-31.8087088478594,12.536442279252,127.814560136736)) ;
#140645 = CARTESIAN_POINT('Ctrl Pts',(-31.7167865748252,12.4387732237497,
127.579135926508)) ;
#140646 = CARTESIAN_POINT('Ctrl Pts',(-31.6191514648672,12.4116342437955,
127.327110422858)) ;
#140647 = CARTESIAN_POINT('Ctrl Pts',(-31.5227020632712,12.4569142489461,
127.078414306826)) ;
#140648 = CARTESIAN_POINT('Ctrl Pts',(-31.4329813801353,12.5714752096904,
126.849465388448)) ;
#140649 = CARTESIAN_POINT('Ctrl Pts',(-31.3560883925141,12.7468633486005,
126.657934872202)) ;
#140650 = CARTESIAN_POINT('Ctrl Pts',(-31.2965842595734,12.9706873354731,
126.517219890221)) ;
#140651 = CARTESIAN_POINT('Ctrl Pts',(-31.258075825459,13.2271705997234,126.4378699364)) ;
#140652 = CARTESIAN_POINT('Ctrl Pts',(-31.2425840183107,13.4971330615505,
126.425684440027)) ;
#140653 = CARTESIAN_POINT('Ctrl Pts',(-31.2506122404268,13.7633006467314,
126.482409435389)) ;
#140654 = CARTESIAN_POINT('Ctrl Pts',(-31.2805375313788,14.0028269061398,
126.602782532402)) ;
#140655 = CARTESIAN_POINT('Ctrl Pts',(-31.330049798945,14.2028678275338,126.780693245081)) ;
#140656 = CARTESIAN_POINT('Ctrl Pts',(-31.3940867324171,14.3455611921622,
127.000744655394)) ;
#140657 = CARTESIAN_POINT('Ctrl Pts',(-31.4682001918605,14.4231516599767,
127.250464735358)) ;
#140658 = CARTESIAN_POINT('Ctrl Pts',(-31.5457693893647,14.4286657254974,
127.510187449708)) ;
#140659 = CARTESIAN_POINT('Ctrl Pts',(-31.6206915150044,14.3621069450972,
127.762197957743)) ;
#140660 = CARTESIAN_POINT('Ctrl Pts',(-31.6867379358927,14.2287342743254,
127.988196798816)) ;
#140661 = CARTESIAN_POINT('Ctrl Pts',(-31.7388558523025,14.0363060460215,
128.1737286555)) ;
#140662 = CARTESIAN_POINT('Ctrl Pts',(-31.7718940828191,13.8023696285656,
128.303154059963)) ;
#140663 = CARTESIAN_POINT('Ctrl Pts',(-31.7834779337839,13.5388531548576,
128.370254159469)) ;
#140664 = CARTESIAN_POINT('Ctrl Pts',(-31.771593832871,13.268451758325,128.368608589023)) ;
#140665 = CARTESIAN_POINT('Ctrl Pts',(-31.7366347371057,13.0087996264663,
128.299588081835)) ;
#140666 = CARTESIAN_POINT('Ctrl Pts',(-31.6798680712665,12.7778890108915,
128.167025511007)) ;
#140667 = CARTESIAN_POINT('Ctrl Pts',(-31.6056828824239,12.5950173458057,
127.983256239013)) ;
#140668 = CARTESIAN_POINT('Ctrl Pts',(-31.5173460134283,12.4700324855763,
127.758440084226)) ;
#140669 = CARTESIAN_POINT('Ctrl Pts',(-31.4216261029277,12.4138573674352,
127.511850114614)) ;
#140670 = CARTESIAN_POINT('Ctrl Pts',(-31.32338456039,12.4301864396543,127.258169228303)) ;
#140671 = CARTESIAN_POINT('Ctrl Pts',(-31.2309191230293,12.5166844416216,
127.020906843594)) ;
#140672 = CARTESIAN_POINT('Ctrl Pts',(-31.1477558041141,12.6693065290769,
126.811250441322)) ;
#140673 = CARTESIAN_POINT('Ctrl Pts',(-31.0809176438295,12.8745471633582,
126.648985783275)) ;
#140674 = CARTESIAN_POINT('Ctrl Pts',(-31.0332964810723,13.1212024009445,
126.54318413991)) ;
#140675 = CARTESIAN_POINT('Ctrl Pts',(-31.0085143558054,13.3871939344405,
126.503779706618)) ;
#140676 = CARTESIAN_POINT('Ctrl Pts',(-31.006972425563,13.6567281897723,126.532400135199)) ;
#140677 = CARTESIAN_POINT('Ctrl Pts',(-31.0283333477867,13.90978543386,126.627950810582)) ;
#140678 = CARTESIAN_POINT('Ctrl Pts',(-31.0703972652886,14.1280196387556,
126.784017641227)) ;
#140679 = CARTESIAN_POINT('Ctrl Pts',(-31.1290079865942,14.2950455998267,
126.988254497869)) ;
#140680 = CARTESIAN_POINT('Ctrl Pts',(-31.2001423757924,14.4005267621949,
127.229371566356)) ;
#140681 = CARTESIAN_POINT('Ctrl Pts',(-31.2766579994051,14.4350836723043,
127.485868070667)) ;
#140682 = CARTESIAN_POINT('Ctrl Pts',(-31.3533027741803,14.3978038978104,
127.742855119514)) ;
#140683 = CARTESIAN_POINT('Ctrl Pts',(-31.4237378888131,14.2905756791986,
127.981744408019)) ;
#140684 = CARTESIAN_POINT('Ctrl Pts',(-31.4821047890832,14.1209511396773,
128.185413714307)) ;
#140685 = CARTESIAN_POINT('Ctrl Pts',(-31.5233617410375,13.9018371700798,
128.33901676082)) ;
#140686 = CARTESIAN_POINT('Ctrl Pts',(-31.543988548502,13.6479071174512,128.432433376555)) ;
#140687 = CARTESIAN_POINT('Ctrl Pts',(-31.5417580384384,13.3785017706424,
128.458991126292)) ;
#140688 = CARTESIAN_POINT('Ctrl Pts',(-31.5158135329586,13.1105160825095,
128.416509788881)) ;
#140689 = CARTESIAN_POINT('Ctrl Pts',(-31.467961620135,12.867723627882,128.309652962403)) ;
#140690 = CARTESIAN_POINT('Ctrl Pts',(-31.4001585537936,12.6628307247657,
128.144774957304)) ;
#140691 = CARTESIAN_POINT('Ctrl Pts',(-31.3171291891636,12.5130918366744,
127.935278432159)) ;
#140692 = CARTESIAN_POINT('Ctrl Pts',(-31.2232944076044,12.4280188888238,
127.694417876056)) ;
#140693 = CARTESIAN_POINT('Ctrl Pts',(-31.1258166367903,12.4146728717073,
127.442682245229)) ;
#140694 = CARTESIAN_POINT('Ctrl Pts',(-31.0298413739331,12.4734183176243,
127.19549995093)) ;
#140695 = CARTESIAN_POINT('Ctrl Pts',(-30.9421230224932,12.6005221105397,
126.972405284986)) ;
#140696 = CARTESIAN_POINT('Ctrl Pts',(-30.8684025674919,12.7855012395254,
126.790042156092)) ;
#140697 = CARTESIAN_POINT('Ctrl Pts',(-30.8125318740678,13.0169861501724,
126.659985042459)) ;
#140698 = CARTESIAN_POINT('Ctrl Pts',(-30.778255066982,13.2774554458054,126.592980347573)) ;
#140699 = CARTESIAN_POINT('Ctrl Pts',(-30.7672128677042,13.548371247685,126.59385523177)) ;
#140700 = CARTESIAN_POINT('Ctrl Pts',(-30.7794543750323,13.8100860909014,
126.662716445457)) ;
#140701 = CARTESIAN_POINT('Ctrl Pts',(-30.8134107463879,14.0443620867839,
126.795050916489)) ;
#140702 = CARTESIAN_POINT('Ctrl Pts',(-30.8658712807709,14.2339607222734,
126.981412466339)) ;
#140703 = CARTESIAN_POINT('Ctrl Pts',(-30.9324377678062,14.3656339915205,
127.209013801012)) ;
#140704 = CARTESIAN_POINT('Ctrl Pts',(-31.0075425407356,14.4296685525136,
127.461543585436)) ;
#140705 = CARTESIAN_POINT('Ctrl Pts',(-31.085013287722,14.4216217611559,127.720952593954)) ;
#140706 = CARTESIAN_POINT('Ctrl Pts',(-31.1587041769614,14.3422173843901,
127.969332083657)) ;
#140707 = CARTESIAN_POINT('Ctrl Pts',(-31.2227445131305,14.1963612396834,
128.189629618647)) ;
#140708 = CARTESIAN_POINT('Ctrl Pts',(-31.2713611336444,13.9958155660663,
128.364717334213)) ;
#140709 = CARTESIAN_POINT('Ctrl Pts',(-31.3007242986626,13.754087100232,128.48360934132)) ;
#140710 = CARTESIAN_POINT('Ctrl Pts',(-31.307940808174,13.4887317484018,128.537791288292)) ;
#140711 = CARTESIAN_POINT('Ctrl Pts',(-31.2915959174183,13.2176489571942,
128.523278102941)) ;
#140712 = CARTESIAN_POINT('Ctrl Pts',(-31.2524780735841,12.9629383916558,
128.442016070707)) ;
#140713 = CARTESIAN_POINT('Ctrl Pts',(-31.1920342453667,12.7394456176792,
128.298717927943)) ;
#140714 = CARTESIAN_POINT('Ctrl Pts',(-31.114816871371,12.5666312437579,128.106136236575)) ;
#140715 = CARTESIAN_POINT('Ctrl Pts',(-31.0247945803096,12.4542159326756,
127.876303092352)) ;
#140716 = CARTESIAN_POINT('Ctrl Pts',(-30.9281340923285,12.4113528378657,
127.627016638565)) ;
#140717 = CARTESIAN_POINT('Ctrl Pts',(-30.8305532126448,12.4409689783365,
127.37515875896)) ;
#140718 = CARTESIAN_POINT('Ctrl Pts',(-30.7387890398871,12.5412370853856,
127.140251323107)) ;
#140719 = CARTESIAN_POINT('Ctrl Pts',(-30.6588180682426,12.7041353032971,
126.939686811656)) ;
#140720 = CARTESIAN_POINT('Ctrl Pts',(-30.5952142862048,12.9183855317437,
126.786957456823)) ;
#140721 = CARTESIAN_POINT('Ctrl Pts',(-30.5518179667405,13.1698655551169,
126.693399866601)) ;
#140722 = CARTESIAN_POINT('Ctrl Pts',(-30.5312892737723,13.4380609721582,
126.666456787728)) ;
#140723 = CARTESIAN_POINT('Ctrl Pts',(-30.5342266781763,13.707166634389,126.708319823239)) ;
#140724 = CARTESIAN_POINT('Ctrl Pts',(-30.5596578817882,13.9538088162951,
126.815620936816)) ;
#140725 = CARTESIAN_POINT('Ctrl Pts',(-30.6050569167213,14.1634527174507,
126.981367630752)) ;
#140726 = CARTESIAN_POINT('Ctrl Pts',(-30.6666408482026,14.3201289995184,
127.194452620019)) ;
#140727 = CARTESIAN_POINT('Ctrl Pts',(-30.738741910301,14.4121341024828,127.438097163118)) ;
#140728 = CARTESIAN_POINT('Ctrl Pts',(-30.8161995675161,14.4336855920868,
127.697564927138)) ;
#140729 = CARTESIAN_POINT('Ctrl Pts',(-30.8921478214072,14.3827385765516,
127.952524857408)) ;
#140730 = CARTESIAN_POINT('Ctrl Pts',(-30.9608791025106,14.2627494122855,
128.186516125915)) ;
#140731 = CARTESIAN_POINT('Ctrl Pts',(-31.0163430481192,14.0822576460886,
128.381727901644)) ;
#140732 = CARTESIAN_POINT('Ctrl Pts',(-31.0537855670433,13.8561930768697,
128.524066496551)) ;
#140733 = CARTESIAN_POINT('Ctrl Pts',(-31.0702462538596,13.5974241277666,
128.605361301542)) ;
#140734 = CARTESIAN_POINT('Ctrl Pts',(-31.06356136907,13.3273250801774,128.618881410681)) ;
#140735 = CARTESIAN_POINT('Ctrl Pts',(-31.0332777175692,13.0622910344741,
128.563704772445)) ;
#140736 = CARTESIAN_POINT('Ctrl Pts',(-30.9814657710391,12.8256129311331,
128.445295711035)) ;
#140737 = CARTESIAN_POINT('Ctrl Pts',(-30.910480059094,12.6301797722552,128.271078496651)) ;
#140738 = CARTESIAN_POINT('Ctrl Pts',(-30.8249833770331,12.491847584192,128.054418930835)) ;
#140739 = CARTESIAN_POINT('Ctrl Pts',(-30.7299901996309,12.4199209625087,
127.810128855303)) ;
#140740 = CARTESIAN_POINT('Ctrl Pts',(-30.6319449437103,12.4204246206127,
127.55689476103)) ;
#140741 = CARTESIAN_POINT('Ctrl Pts',(-30.5376607508626,12.4921596766918,
127.314438282867)) ;
#140742 = CARTESIAN_POINT('Ctrl Pts',(-30.4519929882104,12.6310174141653,
127.097364797993)) ;
#140743 = CARTESIAN_POINT('Ctrl Pts',(-30.3811795712557,12.8262648550687,
126.923585720912)) ;
#140744 = CARTESIAN_POINT('Ctrl Pts',(-30.3292134109451,13.0646915634,126.804938556669)) ;
#140745 = CARTESIAN_POINT('Ctrl Pts',(-30.2992736928993,13.3278245942677,
126.750508221298)) ;
#140746 = CARTESIAN_POINT('Ctrl Pts',(-30.2926564922798,13.599858684379,126.764474820433)) ;
#140747 = CARTESIAN_POINT('Ctrl Pts',(-30.30917695543,13.8569828233467,126.845742313604)) ;
#140748 = CARTESIAN_POINT('Ctrl Pts',(-30.3469514300778,14.0842219920521,
126.989260072652)) ;
#140749 = CARTESIAN_POINT('Ctrl Pts',(-30.4023194112078,14.263433654148,127.184042864747)) ;
#140750 = CARTESIAN_POINT('Ctrl Pts',(-30.4711865511833,14.3833954982456,
127.418482566623)) ;
#140751 = CARTESIAN_POINT('Ctrl Pts',(-30.5472924654005,14.4336980468668,
127.67395398933)) ;
#140752 = CARTESIAN_POINT('Ctrl Pts',(-30.6242714433732,14.4120157634547,
127.931818979531)) ;
#140753 = CARTESIAN_POINT('Ctrl Pts',(-30.6967127060867,14.3192946556154,
128.176630213785)) ;
#140754 = CARTESIAN_POINT('Ctrl Pts',(-30.758053265306,14.1625582896785,128.388922784291)) ;
#140755 = CARTESIAN_POINT('Ctrl Pts',(-30.8035122758961,13.9521768642311,
128.55493374882)) ;
#140756 = CARTESIAN_POINT('Ctrl Pts',(-30.8287385977858,13.7045477344639,
128.661723129224)) ;
#140757 = CARTESIAN_POINT('Ctrl Pts',(-30.8315630481093,13.4377490318283,
128.702961656048)) ;
#140758 = CARTESIAN_POINT('Ctrl Pts',(-30.8108154625355,13.1678476288368,
128.675600753644)) ;
#140759 = CARTESIAN_POINT('Ctrl Pts',(-30.7674808535793,12.9176590168047,
128.582066704266)) ;
#140760 = CARTESIAN_POINT('Ctrl Pts',(-30.7034751148183,12.7025601714455,
128.428332483877)) ;
#140761 = CARTESIAN_POINT('Ctrl Pts',(-30.6236198842184,12.5405894740577,
128.228006763419)) ;
#140762 = CARTESIAN_POINT('Ctrl Pts',(-30.5317107486925,12.4405287581968,
127.992717121245)) ;
#140763 = CARTESIAN_POINT('Ctrl Pts',(-30.4341716126828,12.4114132280254,
127.740958058286)) ;
#140764 = CARTESIAN_POINT('Ctrl Pts',(-30.3376601408581,12.4546443860593,
127.492068415319)) ;
#140765 = CARTESIAN_POINT('Ctrl Pts',(-30.2478156786388,12.5668919860046,
127.262686548233)) ;
#140766 = CARTESIAN_POINT('Ctrl Pts',(-30.1701035113798,12.7415276460806,
127.068926106213)) ;
#140767 = CARTESIAN_POINT('Ctrl Pts',(-30.1102266276716,12.9638993361252,
126.927058750175)) ;
#140768 = CARTESIAN_POINT('Ctrl Pts',(-30.0711164557523,13.2191083147461,
126.845881048397)) ;
#140769 = CARTESIAN_POINT('Ctrl Pts',(-30.0549249492426,13.4893535433623,
126.831705526524)) ;
#140770 = CARTESIAN_POINT('Ctrl Pts',(-30.0622158105278,13.7553189464662,
126.886189778859)) ;
#140771 = CARTESIAN_POINT('Ctrl Pts',(-30.0917108612786,13.9971252301126,
127.00549241837)) ;
#140772 = CARTESIAN_POINT('Ctrl Pts',(-30.1406246191067,14.197781210739,127.181547286119)) ;
#140773 = CARTESIAN_POINT('Ctrl Pts',(-30.2043024678696,14.3424511179814,
127.400565722708)) ;
#140774 = CARTESIAN_POINT('Ctrl Pts',(-30.2785070155895,14.4220643031845,
127.650668850622)) ;
#140775 = CARTESIAN_POINT('Ctrl Pts',(-30.3556721509366,14.4294490868584,
127.909045532744)) ;
#140776 = CARTESIAN_POINT('Ctrl Pts',(-30.4307226480629,14.3652071957823,
128.161408707712)) ;
#140777 = CARTESIAN_POINT('Ctrl Pts',(-30.4971804793035,14.2335291048216,
128.388647963749)) ;
#140778 = CARTESIAN_POINT('Ctrl Pts',(-30.5497562286805,14.0429178976906,
128.575476468873)) ;
#140779 = CARTESIAN_POINT('Ctrl Pts',(-30.5834483776407,13.8093219413454,
128.706910013611)) ;
#140780 = CARTESIAN_POINT('Ctrl Pts',(-30.595700134892,13.547621689864,128.775798853004)) ;
#140781 = CARTESIAN_POINT('Ctrl Pts',(-30.5844060621216,13.275071076932,128.7761395579)) ;
#140782 = CARTESIAN_POINT('Ctrl Pts',(-30.5501753727738,13.0163163266613,
128.709067579648)) ;
#140783 = CARTESIAN_POINT('Ctrl Pts',(-30.4942243712158,12.7846450787164,
128.578813612621)) ;
#140784 = CARTESIAN_POINT('Ctrl Pts',(-30.4202779680125,12.5995255835865,
128.395852978554)) ;
#140785 = CARTESIAN_POINT('Ctrl Pts',(-30.3322269992084,12.4726551218916,
128.171878735475)) ;
#140786 = CARTESIAN_POINT('Ctrl Pts',(-30.2365765506608,12.4145513359232,
127.925517923835)) ;
#140787 = CARTESIAN_POINT('Ctrl Pts',(-30.1388101237624,12.4284690749365,
127.673046945035)) ;
#140788 = CARTESIAN_POINT('Ctrl Pts',(-30.0455202983357,12.513343198717,127.43358743129)) ;
#140789 = CARTESIAN_POINT('Ctrl Pts',(-29.9620436323982,12.6644367568353,
127.223005705298)) ;
#140790 = CARTESIAN_POINT('Ctrl Pts',(-29.8948322705706,12.8679925993142,
127.059595501891)) ;
#140791 = CARTESIAN_POINT('Ctrl Pts',(-29.8466374744008,13.1131690756933,
126.95204916951)) ;
#140792 = CARTESIAN_POINT('Ctrl Pts',(-29.8210604812711,13.380000312228,126.910471572715)) ;
#140793 = CARTESIAN_POINT('Ctrl Pts',(-29.8189544197658,13.6495651936862,
126.93742774856)) ;
#140794 = CARTESIAN_POINT('Ctrl Pts',(-29.8395558893614,13.9023389091985,
127.030620642381)) ;
#140795 = CARTESIAN_POINT('Ctrl Pts',(-29.8811896320557,14.1226577845122,
127.185548174288)) ;
#140796 = CARTESIAN_POINT('Ctrl Pts',(-29.9393151042164,14.2908247564139,
127.388306463954)) ;
#140797 = CARTESIAN_POINT('Ctrl Pts',(-30.0097936116339,14.398104059989,127.62734949335)) ;
#140798 = CARTESIAN_POINT('Ctrl Pts',(-30.0867674947376,14.4352626924574,
127.885423386131)) ;
#140799 = CARTESIAN_POINT('Ctrl Pts',(-30.1635829782001,14.3995540254238,
128.142951931714)) ;
#140800 = CARTESIAN_POINT('Ctrl Pts',(-30.2339318810488,14.2948938650605,
128.381416945128)) ;
#140801 = CARTESIAN_POINT('Ctrl Pts',(-30.2930532509891,14.1259509639325,
128.587480866756)) ;
#140802 = CARTESIAN_POINT('Ctrl Pts',(-30.3346559878636,13.9085226372069,
128.741994405636)) ;
#140803 = CARTESIAN_POINT('Ctrl Pts',(-30.3559110579538,13.6557404486892,
128.837201233893)) ;
#140804 = CARTESIAN_POINT('Ctrl Pts',(-30.3543840398925,13.3866405250996,
128.865800543519)) ;
#140805 = CARTESIAN_POINT('Ctrl Pts',(-30.3291184078958,13.1181023923962,
128.825323697214)) ;
#140806 = CARTESIAN_POINT('Ctrl Pts',(-30.2818707300597,12.8743682502049,
128.720238119545)) ;
#140807 = CARTESIAN_POINT('Ctrl Pts',(-30.2145778991752,12.6679957013257,
128.556859225096)) ;
#140808 = CARTESIAN_POINT('Ctrl Pts',(-30.1317764801247,12.5164143784842,
128.348080123108)) ;
#140809 = CARTESIAN_POINT('Ctrl Pts',(-30.0385063797381,12.4295970136061,
128.108745600341)) ;
#140810 = CARTESIAN_POINT('Ctrl Pts',(-29.9407571698938,12.4140261381013,
127.856324516585)) ;
#140811 = CARTESIAN_POINT('Ctrl Pts',(-29.8447911575134,12.4707103540387,
127.609114356662)) ;
#140812 = CARTESIAN_POINT('Ctrl Pts',(-29.7567597974375,12.595906863769,127.385107000309)) ;
#140813 = CARTESIAN_POINT('Ctrl Pts',(-29.6825520242752,12.7791143335627,
127.201300936542)) ;
#140814 = CARTESIAN_POINT('Ctrl Pts',(-29.6257812390629,13.0114294021893,
127.068868815089)) ;
#140815 = CARTESIAN_POINT('Ctrl Pts',(-29.5912358251014,13.2689900400404,
127.000770848446)) ;
#140816 = CARTESIAN_POINT('Ctrl Pts',(-29.5793857815431,13.5409258374442,
126.999421466082)) ;
#140817 = CARTESIAN_POINT('Ctrl Pts',(-29.5910200568263,13.8029841851952,
127.066485164223)) ;
#140818 = CARTESIAN_POINT('Ctrl Pts',(-29.6244387540503,14.0385609610044,
127.197290216951)) ;
#140819 = CARTESIAN_POINT('Ctrl Pts',(-29.676435866219,14.229423171085,127.382279927079)) ;
#140820 = CARTESIAN_POINT('Ctrl Pts',(-29.7425620569963,14.3627051887218,
127.608541532135)) ;
#140821 = CARTESIAN_POINT('Ctrl Pts',(-29.8175397971597,14.4288334278673,
127.860718073631)) ;
#140822 = CARTESIAN_POINT('Ctrl Pts',(-29.8950584014949,14.4228924311934,
128.120277862613)) ;
#140823 = CARTESIAN_POINT('Ctrl Pts',(-29.9691508818996,14.3451233913639,
128.369927528249)) ;
#140824 = CARTESIAN_POINT('Ctrl Pts',(-30.0334310668133,14.2008972200028,
128.590893710781)) ;
#140825 = CARTESIAN_POINT('Ctrl Pts',(-30.0824006390069,14.0023959452744,
128.766909525821)) ;
#140826 = CARTESIAN_POINT('Ctrl Pts',(-30.112430690584,13.7610317231258,128.887829500663)) ;
#140827 = CARTESIAN_POINT('Ctrl Pts',(-30.1202498275654,13.496756912036,128.943686581971)) ;
#140828 = CARTESIAN_POINT('Ctrl Pts',(-30.1046746200123,13.2257685064712,
128.931391271073)) ;
#140829 = CARTESIAN_POINT('Ctrl Pts',(-30.0660503796317,12.9695425857073,
128.85168137516)) ;
#140830 = CARTESIAN_POINT('Ctrl Pts',(-30.0063498248392,12.7456271494707,
128.710444507496)) ;
#140831 = CARTESIAN_POINT('Ctrl Pts',(-29.9295767509961,12.5709695173834,
128.519177027686)) ;
#140832 = CARTESIAN_POINT('Ctrl Pts',(-29.8397265805435,12.4565179049814,
128.289888234812)) ;
#140833 = CARTESIAN_POINT('Ctrl Pts',(-29.743150711624,12.4114773771493,128.040854735391)) ;
#140834 = CARTESIAN_POINT('Ctrl Pts',(-29.6451458107009,12.4394645505146,
127.787888159147)) ;
#140835 = CARTESIAN_POINT('Ctrl Pts',(-29.5538472801924,12.5368907047146,
127.554071664716)) ;
#140836 = CARTESIAN_POINT('Ctrl Pts',(-29.4727909904181,12.6994727146824,
127.350623684027)) ;
#140837 = CARTESIAN_POINT('Ctrl Pts',(-29.4090848375654,12.9112843843373,
127.197388701276)) ;
#140838 = CARTESIAN_POINT('Ctrl Pts',(-29.3648032660279,13.1634090082974,
127.101442481715)) ;
#140839 = CARTESIAN_POINT('Ctrl Pts',(-29.3438379371304,13.4300956045555,
127.073062362202)) ;
#140840 = CARTESIAN_POINT('Ctrl Pts',(-29.3459367193337,13.6985487061805,
127.112349022373)) ;
#140841 = CARTESIAN_POINT('Ctrl Pts',(-29.3709612229612,13.9480246768514,
127.218730380397)) ;
#140842 = CARTESIAN_POINT('Ctrl Pts',(-29.4156502273643,14.1576527966606,
127.382216588722)) ;
#140843 = CARTESIAN_POINT('Ctrl Pts',(-29.4767450790731,14.3162850326807,
127.593864273564)) ;
#140844 = CARTESIAN_POINT('Ctrl Pts',(-29.5489675079737,14.4106899990105,
127.838019760763)) ;
#140845 = CARTESIAN_POINT('Ctrl Pts',(-29.6263938236657,14.4339585104257,
128.097404223511)) ;
#140846 = CARTESIAN_POINT('Ctrl Pts',(-29.7021377868535,14.3853107488566,
128.351622410823)) ;
#140847 = CARTESIAN_POINT('Ctrl Pts',(-29.771343653763,14.2669553900087,128.587085672282)) ;
#140848 = CARTESIAN_POINT('Ctrl Pts',(-29.8271366885734,14.0883945363266,
128.78318518596)) ;
#140849 = CARTESIAN_POINT('Ctrl Pts',(-29.8651996903043,13.8631866954131,
128.927384615722)) ;
#140850 = CARTESIAN_POINT('Ctrl Pts',(-29.8822989781565,13.6057119879249,
129.01046116545)) ;
#140851 = CARTESIAN_POINT('Ctrl Pts',(-29.8762843382152,13.3350527616499,
129.026023028071)) ;
#140852 = CARTESIAN_POINT('Ctrl Pts',(-29.8468405958706,13.0707552698518,
128.973143943309)) ;
#140853 = CARTESIAN_POINT('Ctrl Pts',(-29.7955855799297,12.8321485931701,
128.856463844239)) ;
#140854 = CARTESIAN_POINT('Ctrl Pts',(-29.7246842633997,12.6344629226598,
128.682655409326)) ;
#140855 = CARTESIAN_POINT('Ctrl Pts',(-29.6399098993552,12.4951761456202,
128.467948465936)) ;
#140856 = CARTESIAN_POINT('Ctrl Pts',(-29.545305543797,12.4210995999737,128.224732967655)) ;
#140857 = CARTESIAN_POINT('Ctrl Pts',(-29.4471501611367,12.4192964340424,
127.971214797337)) ;
#140858 = CARTESIAN_POINT('Ctrl Pts',(-29.3524662110009,12.4890492714601,
127.727661006437)) ;
#140859 = CARTESIAN_POINT('Ctrl Pts',(-29.2661993967892,12.6268327661457,
127.508955192755)) ;
#140860 = CARTESIAN_POINT('Ctrl Pts',(-29.1953397269962,12.8195831784206,
127.334849135012)) ;
#140861 = CARTESIAN_POINT('Ctrl Pts',(-29.1426416993899,13.0571003299884,
127.214097852355)) ;
#140862 = CARTESIAN_POINT('Ctrl Pts',(-29.1120307486165,13.320280679744,127.15777002931)) ;
#140863 = CARTESIAN_POINT('Ctrl Pts',(-29.1047060155249,13.5914917582005,
127.169555410746)) ;
#140864 = CARTESIAN_POINT('Ctrl Pts',(-29.1206742275936,13.8505567194106,
127.249383407295)) ;
#140865 = CARTESIAN_POINT('Ctrl Pts',(-29.1577239501666,14.0777829909349,
127.390619937542)) ;
#140866 = CARTESIAN_POINT('Ctrl Pts',(-29.212717534914,14.2590886738723,127.584383986945)) ;
#140867 = CARTESIAN_POINT('Ctrl Pts',(-29.2812145769909,14.3807167115641,
127.817703884744)) ;
#140868 = CARTESIAN_POINT('Ctrl Pts',(-29.3571182980737,14.433343615208,128.072557778617)) ;
#140869 = CARTESIAN_POINT('Ctrl Pts',(-29.4346569346725,14.4133893489329,
128.332279874876)) ;
#140870 = CARTESIAN_POINT('Ctrl Pts',(-29.5068531862197,14.3229978009541,
128.576166295593)) ;
#140871 = CARTESIAN_POINT('Ctrl Pts',(-29.5686642958486,14.1680349923561,
128.789860721644)) ;
#140872 = CARTESIAN_POINT('Ctrl Pts',(-29.6145595401633,13.959434776873,128.957078689166)) ;
#140873 = CARTESIAN_POINT('Ctrl Pts',(-29.6405447655555,13.712829168107,129.066081979048)) ;
#140874 = CARTESIAN_POINT('Ctrl Pts',(-29.6439572935887,13.4442543283008,
129.109297534092)) ;
#140875 = CARTESIAN_POINT('Ctrl Pts',(-29.6241012830215,13.176694407093,129.084213601662)) ;
#140876 = CARTESIAN_POINT('Ctrl Pts',(-29.5810380555836,12.9234094710806,
128.991780301771)) ;
#140877 = CARTESIAN_POINT('Ctrl Pts',(-29.5179260136605,12.7086523175308,
128.840427686241)) ;
#140878 = CARTESIAN_POINT('Ctrl Pts',(-29.4384206751917,12.5444332801825,
128.641184040457)) ;
#140879 = CARTESIAN_POINT('Ctrl Pts',(-29.3464035868294,12.4422654275157,
128.40569652746)) ;
#140880 = CARTESIAN_POINT('Ctrl Pts',(-29.2493516171235,12.4113238215259,
128.155221462137)) ;
#140881 = CARTESIAN_POINT('Ctrl Pts',(-29.1526487800264,12.452199983914,127.905794005988)) ;
#140882 = CARTESIAN_POINT('Ctrl Pts',(-29.0620241585539,12.5635389999469,
127.674336022858)) ;
#140883 = CARTESIAN_POINT('Ctrl Pts',(-28.9845003087822,12.7354102811942,
127.480874966993)) ;
#140884 = CARTESIAN_POINT('Ctrl Pts',(-28.9238804025353,12.9568498442606,
127.336904325203)) ;
#140885 = CARTESIAN_POINT('Ctrl Pts',(-28.8840944094843,13.2117694969246,
127.253797665177)) ;
#140886 = CARTESIAN_POINT('Ctrl Pts',(-28.867247231596,13.48252854114,127.23778724413)) ;
#140887 = CARTESIAN_POINT('Ctrl Pts',(-28.8739686370942,13.748482945783,127.290563060827)) ;
#140888 = CARTESIAN_POINT('Ctrl Pts',(-28.9027248635833,13.9900671624614,
127.407555291496)) ;
#140889 = CARTESIAN_POINT('Ctrl Pts',(-28.9509775630119,14.1922209506685,
127.581640902384)) ;
#140890 = CARTESIAN_POINT('Ctrl Pts',(-29.014692765249,14.3393855753319,127.800968412475)) ;
#140891 = CARTESIAN_POINT('Ctrl Pts',(-29.0880462050529,14.4204077482377,
128.048293378874)) ;
#140892 = CARTESIAN_POINT('Ctrl Pts',(-29.1655876741887,14.4304302068623,
128.307946651833)) ;
#140893 = CARTESIAN_POINT('Ctrl Pts',(-29.2410222299655,14.3678711174913,
128.561528843684)) ;
#140894 = CARTESIAN_POINT('Ctrl Pts',(-29.3078276957715,14.2376926994235,
128.789814550899)) ;
#140895 = CARTESIAN_POINT('Ctrl Pts',(-29.3606966005294,14.0489882455827,
128.977410807902)) ;
#140896 = CARTESIAN_POINT('Ctrl Pts',(-29.3950338182995,13.8164455432918,
129.110736007563)) ;
#140897 = CARTESIAN_POINT('Ctrl Pts',(-29.4078405026359,13.5541088077793,
129.18138636938)) ;
#140898 = CARTESIAN_POINT('Ctrl Pts',(-29.3974124674152,13.2846771651641,
129.183867775352)) ;
#140899 = CARTESIAN_POINT('Ctrl Pts',(-29.3636550612449,13.0230234432121,
129.118469484008)) ;
#140900 = CARTESIAN_POINT('Ctrl Pts',(-29.3083509044896,12.7908726515439,
128.990023773957)) ;
#140901 = CARTESIAN_POINT('Ctrl Pts',(-29.2347161729155,12.6038717726337,
128.808047575783)) ;
#140902 = CARTESIAN_POINT('Ctrl Pts',(-29.1473019065763,12.4755977885113,
128.585809976829)) ;
#140903 = CARTESIAN_POINT('Ctrl Pts',(-29.051574804785,12.4151865367556,128.339309434992)) ;
#140904 = CARTESIAN_POINT('Ctrl Pts',(-28.9538949869407,12.4270410724712,
128.087048576477)) ;
#140905 = CARTESIAN_POINT('Ctrl Pts',(-28.8603899759108,12.5098502892393,
127.846962468881)) ;
#140906 = CARTESIAN_POINT('Ctrl Pts',(-28.7765666463378,12.6589866450951,
127.635344392143)) ;
#140907 = CARTESIAN_POINT('Ctrl Pts',(-28.7087215246026,12.8615687451882,
127.470148650886)) ;
#140908 = CARTESIAN_POINT('Ctrl Pts',(-28.6600385912031,13.1050266769027,
127.361069056887)) ;
#140909 = CARTESIAN_POINT('Ctrl Pts',(-28.6337144036686,13.3718444110737,
127.317363744017)) ;
#140910 = CARTESIAN_POINT('Ctrl Pts',(-28.6308308714776,13.6411904453346,
127.341985774397)) ;
#140911 = CARTESIAN_POINT('Ctrl Pts',(-28.6510730281356,13.8968635155474,
127.434435033886)) ;
#140912 = CARTESIAN_POINT('Ctrl Pts',(-28.6917302180179,14.1159779799374,
127.586141478924)) ;
#140913 = CARTESIAN_POINT('Ctrl Pts',(-28.7498275997111,14.2873257027271,
127.789085812779)) ;
#140914 = CARTESIAN_POINT('Ctrl Pts',(-28.8199093839214,14.3958947377193,
128.026877760367)) ;
#140915 = CARTESIAN_POINT('Ctrl Pts',(-28.8965301500445,14.4351265097039,
128.283821788283)) ;
#140916 = CARTESIAN_POINT('Ctrl Pts',(-28.9734020017538,14.401957868835,128.541485841149)) ;
#140917 = CARTESIAN_POINT('Ctrl Pts',(-29.04450350885,14.2982652122168,128.782398104542)) ;
#140918 = CARTESIAN_POINT('Ctrl Pts',(-29.1035127772872,14.1324802087574,
128.987829900738)) ;
#140919 = CARTESIAN_POINT('Ctrl Pts',(-29.1459631430346,13.9154628269439,
129.144988599754)) ;
#140920 = CARTESIAN_POINT('Ctrl Pts',(-29.1678311809284,13.6633712406997,
129.241982385923)) ;
#140921 = CARTESIAN_POINT('Ctrl Pts',(-29.1669352598198,13.3940849340156,
129.272479386928)) ;
#140922 = CARTESIAN_POINT('Ctrl Pts',(-29.1424881944319,13.1263052582701,
129.234248892586)) ;
#140923 = CARTESIAN_POINT('Ctrl Pts',(-29.0956268544443,12.8804158513159,
129.130464723764)) ;
#140924 = CARTESIAN_POINT('Ctrl Pts',(-29.0290020456781,12.6733662735578,
128.968940469468)) ;
#140925 = CARTESIAN_POINT('Ctrl Pts',(-28.9464646971493,12.5197379021673,
128.760988363812)) ;
#140926 = CARTESIAN_POINT('Ctrl Pts',(-28.853372820222,12.4310982059369,128.52218112472)) ;
#140927 = CARTESIAN_POINT('Ctrl Pts',(-28.7559344096338,12.4134628316865,
128.270577847274)) ;
#140928 = CARTESIAN_POINT('Ctrl Pts',(-28.6597354547319,12.4679867596538,
128.022716531487)) ;
#140929 = CARTESIAN_POINT('Ctrl Pts',(-28.5711852993659,12.5916525961337,
127.797270001978)) ;
#140930 = CARTESIAN_POINT('Ctrl Pts',(-28.496628960717,12.7734685194903,127.612433381058)) ;
#140931 = CARTESIAN_POINT('Ctrl Pts',(-28.4395894906841,13.0028689239805,
127.478980244894)) ;
#140932 = CARTESIAN_POINT('Ctrl Pts',(-28.4040144970096,13.261962548957,127.408156835628)) ;
#140933 = CARTESIAN_POINT('Ctrl Pts',(-28.3916352491005,13.5340193336117,
127.405276715523)) ;
#140934 = CARTESIAN_POINT('Ctrl Pts',(-28.4025847374665,13.7955676266414,
127.470215599722)) ;
#140935 = CARTESIAN_POINT('Ctrl Pts',(-28.4353995658411,14.0322614564451,
127.599264380229)) ;
#140936 = CARTESIAN_POINT('Ctrl Pts',(-28.4868397358784,14.2243899010379,
127.782585598631)) ;
#140937 = CARTESIAN_POINT('Ctrl Pts',(-28.5527080316366,14.3598901604785,
128.008145601297)) ;
#140938 = CARTESIAN_POINT('Ctrl Pts',(-28.6278695337408,14.4280176399282,
128.261005626896)) ;
#140939 = CARTESIAN_POINT('Ctrl Pts',(-28.7049132284027,14.4241023567618,
128.518966473141)) ;
#140940 = CARTESIAN_POINT('Ctrl Pts',(-28.7794251636048,14.3482279673457,
128.76994543598)) ;
#140941 = CARTESIAN_POINT('Ctrl Pts',(-28.8439156578016,14.2060723674291,
128.991445593633)) ;
#140942 = CARTESIAN_POINT('Ctrl Pts',(-28.8934515036008,14.0086807740354,
129.169172629331)) ;
#140943 = CARTESIAN_POINT('Ctrl Pts',(-28.9240482263405,13.7691470824975,
129.291636017452)) ;
#140944 = CARTESIAN_POINT('Ctrl Pts',(-28.9325810238934,13.5031160209837,
129.349853238854)) ;
#140945 = CARTESIAN_POINT('Ctrl Pts',(-28.9175541272843,13.2327333331826,
129.339069926924)) ;
#140946 = CARTESIAN_POINT('Ctrl Pts',(-28.8797005123668,12.976776614233,129.261497699467)) ;
#140947 = CARTESIAN_POINT('Ctrl Pts',(-28.8206976959534,12.7518156970481,
129.12225615979)) ;
#140948 = CARTESIAN_POINT('Ctrl Pts',(-28.744034594892,12.5749030333723,128.931449829078)) ;
#140949 = CARTESIAN_POINT('Ctrl Pts',(-28.6546157712723,12.4587258582811,
128.703359625527)) ;
#140950 = CARTESIAN_POINT('Ctrl Pts',(-28.5576462996642,12.4118884067616,
128.453352995457)) ;
#140951 = CARTESIAN_POINT('Ctrl Pts',(-28.4609282919855,12.4371448006442,
128.203671997539)) ;
#140952 = CARTESIAN_POINT('Ctrl Pts',(-28.3682833220301,12.5335140246063,
127.966323254618)) ;
#140953 = CARTESIAN_POINT('Ctrl Pts',(-28.2875408074332,12.6929505687292,
127.763479311416)) ;
#140954 = CARTESIAN_POINT('Ctrl Pts',(-28.2226827881692,12.9053983640665,
127.607203099237)) ;
#140955 = CARTESIAN_POINT('Ctrl Pts',(-28.1782420281259,13.1539498783259,
127.510416974053)) ;
#140956 = CARTESIAN_POINT('Ctrl Pts',(-28.1562632009264,13.422675078525,127.479377602005)) ;
#140957 = CARTESIAN_POINT('Ctrl Pts',(-28.1577935734945,13.691089143288,127.516960997828)) ;
#140958 = CARTESIAN_POINT('Ctrl Pts',(-28.1821515376259,13.9413684458137,
127.621389577109)) ;
#140959 = CARTESIAN_POINT('Ctrl Pts',(-28.226439644364,14.1526799240858,127.783773013239)) ;
#140960 = CARTESIAN_POINT('Ctrl Pts',(-28.2870558314823,14.3125333467772,
127.993960696093)) ;
#140961 = CARTESIAN_POINT('Ctrl Pts',(-28.3588077689731,14.408819463409,128.236644758816)) ;
#140962 = CARTESIAN_POINT('Ctrl Pts',(-28.4364512521204,14.4343198914763,
128.496786106316)) ;
#140963 = CARTESIAN_POINT('Ctrl Pts',(-28.5121726728494,14.3877722038871,
128.750872707546)) ;
#140964 = CARTESIAN_POINT('Ctrl Pts',(-28.5817452954328,14.2711470779282,
128.987450777919)) ;
#140965 = CARTESIAN_POINT('Ctrl Pts',(-28.6377450769826,14.0951742319451,
129.183988636599)) ;
#140966 = CARTESIAN_POINT('Ctrl Pts',(-28.6766270030896,13.870335302896,129.330724917506)) ;
#140967 = CARTESIAN_POINT('Ctrl Pts',(-28.6943466665121,13.6128358613542,
129.415688801231)) ;
#140968 = CARTESIAN_POINT('Ctrl Pts',(-28.6889851715194,13.3431052342381,
129.43306210823)) ;
#140969 = CARTESIAN_POINT('Ctrl Pts',(-28.660328849755,13.0784068980914,129.382462071094)) ;
#140970 = CARTESIAN_POINT('Ctrl Pts',(-28.6091631818449,12.8371324748468,
129.266305768313)) ;
#140971 = CARTESIAN_POINT('Ctrl Pts',(-28.5393761304624,12.639991514166,129.095436280033)) ;
#140972 = CARTESIAN_POINT('Ctrl Pts',(-28.454558582428,12.4979352238862,128.880780706304)) ;
#140973 = CARTESIAN_POINT('Ctrl Pts',(-28.3599026767257,12.4220838446985,
128.637480288422)) ;
#140974 = CARTESIAN_POINT('Ctrl Pts',(-28.2619574346768,12.4184701426874,
128.384508953084)) ;
#140975 = CARTESIAN_POINT('Ctrl Pts',(-28.1674363195264,12.4860425111682,
128.141319241242)) ;
#140976 = CARTESIAN_POINT('Ctrl Pts',(-28.0810401792008,12.62129710121,127.92213272214)) ;
#140977 = CARTESIAN_POINT('Ctrl Pts',(-28.0092963384714,12.8133840710904,
127.745605494146)) ;
#140978 = CARTESIAN_POINT('Ctrl Pts',(-27.9559959394673,13.0503650213175,
127.623143511295)) ;
#140979 = CARTESIAN_POINT('Ctrl Pts',(-27.9248374489822,13.3123038567085,
127.56512149863)) ;
#140980 = CARTESIAN_POINT('Ctrl Pts',(-27.9168020041589,13.5832779933084,
127.574796329027)) ;
#140981 = CARTESIAN_POINT('Ctrl Pts',(-27.9320454118317,13.8428844537896,
127.652487922196)) ;
#140982 = CARTESIAN_POINT('Ctrl Pts',(-27.9686240808447,14.0720013816764,
127.792453983478)) ;
#140983 = CARTESIAN_POINT('Ctrl Pts',(-28.02315885797,14.2546155978529,127.984855739173)) ;
#140984 = CARTESIAN_POINT('Ctrl Pts',(-28.0911548338665,14.3779471702252,
128.216627929247)) ;
#140985 = CARTESIAN_POINT('Ctrl Pts',(-28.1670206979292,14.4327785527786,
128.471419072253)) ;
#140986 = CARTESIAN_POINT('Ctrl Pts',(-28.2443543229282,14.4152048360803,
128.730429870402)) ;
#140987 = CARTESIAN_POINT('Ctrl Pts',(-28.3171288418279,14.3266409428597,
128.976154143631)) ;
#140988 = CARTESIAN_POINT('Ctrl Pts',(-28.3794021887183,14.1729214671605,
129.191259216607)) ;
#140989 = CARTESIAN_POINT('Ctrl Pts',(-28.4256655711301,13.9662155184911,
129.359458626253)) ;
#140990 = CARTESIAN_POINT('Ctrl Pts',(-28.4522869637337,13.7208186547473,
129.470286151888)) ;
#140991 = CARTESIAN_POINT('Ctrl Pts',(-28.4564309237617,13.4521886594885,
129.515686361507)) ;
#140992 = CARTESIAN_POINT('Ctrl Pts',(-28.4371402610968,13.1838897369756,
129.492322441034)) ;
#140993 = CARTESIAN_POINT('Ctrl Pts',(-28.395008920419,12.9313138648893,129.402409345746)) ;
#140994 = CARTESIAN_POINT('Ctrl Pts',(-28.3322804324004,12.7142071163423,
129.252310506691)) ;
#140995 = CARTESIAN_POINT('Ctrl Pts',(-28.2529695087352,12.5481822878489,
129.053703416506)) ;
#140996 = CARTESIAN_POINT('Ctrl Pts',(-28.1617320020028,12.4445945503844,
128.820309439414)) ;
#140997 = CARTESIAN_POINT('Ctrl Pts',(-28.0646800119981,12.4110615289685,
128.569866486525)) ;
#140998 = CARTESIAN_POINT('Ctrl Pts',(-27.9674199966164,12.4502003413461,
128.318970669863)) ;
#140999 = CARTESIAN_POINT('Ctrl Pts',(-27.8771422429295,12.5587981618695,
128.088294626238)) ;
#141000 = CARTESIAN_POINT('Ctrl Pts',(-27.798868329989,12.7290993092181,127.892732978884)) ;
#141001 = CARTESIAN_POINT('Ctrl Pts',(-27.737418020498,12.950564316011,127.746505773547)) ;
#141002 = CARTESIAN_POINT('Ctrl Pts',(-27.6971967474441,13.2039534170359,
127.662012965437)) ;
#141003 = CARTESIAN_POINT('Ctrl Pts',(-27.6796377184877,13.4737768777198,
127.643834921464)) ;
#141004 = CARTESIAN_POINT('Ctrl Pts',(-27.6856087062491,13.7408243981145,
127.694494054552)) ;
#141005 = CARTESIAN_POINT('Ctrl Pts',(-27.713966691118,13.9843829005592,127.81048226759)) ;
#141006 = CARTESIAN_POINT('Ctrl Pts',(-27.7614922013285,14.1867700874977,
127.982267797735)) ;
#141007 = CARTESIAN_POINT('Ctrl Pts',(-27.8248727597038,14.3360223630702,
128.200658761603)) ;
#141008 = CARTESIAN_POINT('Ctrl Pts',(-27.8980311925229,14.4190305114461,
128.447414074677)) ;
#141009 = CARTESIAN_POINT('Ctrl Pts',(-27.9755313511817,14.4311357302908,
128.706944667949)) ;
#141010 = CARTESIAN_POINT('Ctrl Pts',(-28.0510062244958,14.3708887604269,
128.960585149943)) ;
#141011 = CARTESIAN_POINT('Ctrl Pts',(-28.1182594178393,14.2422926303469,
129.190247723132)) ;
#141012 = CARTESIAN_POINT('Ctrl Pts',(-28.1714032261274,14.0562618591324,
129.378475255161)) ;
#141013 = CARTESIAN_POINT('Ctrl Pts',(-28.2066164194266,13.8231736000303,
129.51460563921)) ;
#141014 = CARTESIAN_POINT('Ctrl Pts',(-28.2199928730901,13.5622215659962,
129.586803651273)) ;
#141015 = CARTESIAN_POINT('Ctrl Pts',(-28.2102466648294,13.2923509313982,
129.591337178618)) ;
#141016 = CARTESIAN_POINT('Ctrl Pts',(-28.1772564946493,13.0307855165856,
129.528091249551)) ;
#141017 = CARTESIAN_POINT('Ctrl Pts',(-28.1223679042081,12.796715819409,129.400977122732)) ;
#141018 = CARTESIAN_POINT('Ctrl Pts',(-28.0492209458298,12.6083942037896,
129.220402711305)) ;
#141019 = CARTESIAN_POINT('Ctrl Pts',(-27.9620383490602,12.4782666718545,
128.998873123193)) ;
#141020 = CARTESIAN_POINT('Ctrl Pts',(-27.8667818789838,12.4160107552107,
128.753637616017)) ;
#141021 = CARTESIAN_POINT('Ctrl Pts',(-27.7688218289437,12.4255889321841,
128.500641595981)) ;
#141022 = CARTESIAN_POINT('Ctrl Pts',(-27.6747744769812,12.5070743683389,
128.259102889033)) ;
#141023 = CARTESIAN_POINT('Ctrl Pts',(-27.5910307718227,12.6538728233386,
128.047551316195)) ;
#141024 = CARTESIAN_POINT('Ctrl Pts',(-27.5225494662066,12.8553500132408,
127.880554242958)) ;
#141025 = CARTESIAN_POINT('Ctrl Pts',(-27.4732675164133,13.0981034422233,
127.769743109725)) ;
#141026 = CARTESIAN_POINT('Ctrl Pts',(-27.4463104814565,13.3649638787798,
127.724238327967)) ;
#141027 = CARTESIAN_POINT('Ctrl Pts',(-27.4428491935347,13.633409473525,127.747047620251)) ;
#141028 = CARTESIAN_POINT('Ctrl Pts',(-27.4622348005861,13.8886868708514,
127.836832748595)) ;
#141029 = CARTESIAN_POINT('Ctrl Pts',(-27.5025149897505,14.1104518503625,
127.987632859157)) ;
#141030 = CARTESIAN_POINT('Ctrl Pts',(-27.5602073067102,14.2832226352683,
128.189383387774)) ;
#141031 = CARTESIAN_POINT('Ctrl Pts',(-27.6299708142586,14.3937886252325,
128.426231960119)) ;
#141032 = CARTESIAN_POINT('Ctrl Pts',(-27.7068452145878,14.4350213811874,
128.684066370922)) ;
#141033 = CARTESIAN_POINT('Ctrl Pts',(-27.7834265371489,14.4038716557598,
128.940723547936)) ;
#141034 = CARTESIAN_POINT('Ctrl Pts',(-27.8549060448491,14.3020574418522,
129.182793140959)) ;
#141035 = CARTESIAN_POINT('Ctrl Pts',(-27.9143023664084,14.1377082714835,
129.389364157556)) ;
#141036 = CARTESIAN_POINT('Ctrl Pts',(-27.9571987711447,13.9225120842828,
129.547744046412)) ;
#141037 = CARTESIAN_POINT('Ctrl Pts',(-27.9797590876057,13.6705375094453,
129.646846563363)) ;
#141038 = CARTESIAN_POINT('Ctrl Pts',(-27.9794706179545,13.4018845199762,
129.679067144231)) ;
#141039 = CARTESIAN_POINT('Ctrl Pts',(-27.9558401512939,13.1344381552283,
129.643132562523)) ;
#141040 = CARTESIAN_POINT('Ctrl Pts',(-27.9093458664183,12.8864832879891,
129.540587983339)) ;
#141041 = CARTESIAN_POINT('Ctrl Pts',(-27.8435719825832,12.679196010264,129.381374767827)) ;
#141042 = CARTESIAN_POINT('Ctrl Pts',(-27.7613092533485,12.5233811225036,
129.174291094988)) ;
#141043 = CARTESIAN_POINT('Ctrl Pts',(-27.6685700885561,12.4327816487888,
128.936468632901)) ;
#141044 = CARTESIAN_POINT('Ctrl Pts',(-27.5708744742361,12.4129159597619,
128.684218615284)) ;
#141045 = CARTESIAN_POINT('Ctrl Pts',(-27.4746603999551,12.4655032985934,
128.436276111074)) ;
#141046 = CARTESIAN_POINT('Ctrl Pts',(-27.386086163872,12.5866529745153,128.21064207061)) ;
#141047 = CARTESIAN_POINT('Ctrl Pts',(-27.3107230948148,12.767439628638,128.023577427765)) ;
#141048 = CARTESIAN_POINT('Ctrl Pts',(-27.2529836630615,12.9966808158701,
127.888194922856)) ;
#141049 = CARTESIAN_POINT('Ctrl Pts',(-27.2169995959156,13.2541242728622,
127.816037280406)) ;
#141050 = CARTESIAN_POINT('Ctrl Pts',(-27.2038734867719,13.524842234863,127.810821018869)) ;
#141051 = CARTESIAN_POINT('Ctrl Pts',(-27.2141327174669,13.7882272307475,
127.873904817517)) ;
#141052 = CARTESIAN_POINT('Ctrl Pts',(-27.2464010178925,14.0260984495824,
128.001380339773)) ;
#141053 = CARTESIAN_POINT('Ctrl Pts',(-27.2974857985163,14.2200232579374,
128.183731204006)) ;
#141054 = CARTESIAN_POINT('Ctrl Pts',(-27.362908361414,14.3567722758536,128.407916901054)) ;
#141055 = CARTESIAN_POINT('Ctrl Pts',(-27.4374375225388,14.4269174595849,
128.65873883066)) ;
#141056 = CARTESIAN_POINT('Ctrl Pts',(-27.5150827034848,14.4252572802329,
128.918711429118)) ;
#141057 = CARTESIAN_POINT('Ctrl Pts',(-27.5895675801479,14.3512844314495,
129.169525398487)) ;
#141058 = CARTESIAN_POINT('Ctrl Pts',(-27.6542017158287,14.2117349601844,
129.391317457744)) ;
#141059 = CARTESIAN_POINT('Ctrl Pts',(-27.7045044465824,14.0152547415916,
129.571407076294)) ;
#141060 = CARTESIAN_POINT('Ctrl Pts',(-27.7357152512017,13.7756398670369,
129.695790498812)) ;
#141061 = CARTESIAN_POINT('Ctrl Pts',(-27.7448568548906,13.5122934272068,
129.755507542801)) ;
#141062 = CARTESIAN_POINT('Ctrl Pts',(-27.7306240640475,13.2411299536141,
129.74712858429)) ;
#141063 = CARTESIAN_POINT('Ctrl Pts',(-27.6933744004606,12.9839532693091,
129.671381426942)) ;
#141064 = CARTESIAN_POINT('Ctrl Pts',(-27.6347046882777,12.7572239501203,
129.533220708441)) ;
#141065 = CARTESIAN_POINT('Ctrl Pts',(-27.5588077749335,12.5794741125724,
129.344509108417)) ;
#141066 = CARTESIAN_POINT('Ctrl Pts',(-27.4694635855471,12.4611210628414,
129.116724569477)) ;
#141067 = CARTESIAN_POINT('Ctrl Pts',(-27.3731253977084,12.4122668253808,
128.868385474263)) ;
#141068 = CARTESIAN_POINT('Ctrl Pts',(-27.2756381680084,12.4354395157324,
128.616699151777)) ;
#141069 = CARTESIAN_POINT('Ctrl Pts',(-27.1828180490366,12.5301694906382,
128.378825987728)) ;
#141070 = CARTESIAN_POINT('Ctrl Pts',(-27.1018777065855,12.6876686677728,
128.175337732907)) ;
#141071 = CARTESIAN_POINT('Ctrl Pts',(-27.0365848293891,12.898212465334,128.017714536355)) ;
#141072 = CARTESIAN_POINT('Ctrl Pts',(-26.9912984048923,13.1472879217631,
127.918636822097)) ;
#141073 = CARTESIAN_POINT('Ctrl Pts',(-26.9687884702793,13.4151706305656,
127.885968483086)) ;
#141074 = CARTESIAN_POINT('Ctrl Pts',(-26.9696641945452,13.6833052701105,
127.921580490902)) ;
#141075 = CARTESIAN_POINT('Ctrl Pts',(-26.993178842716,13.9335262167577,128.023403835393)) ;
#141076 = CARTESIAN_POINT('Ctrl Pts',(-27.0372896845173,14.1479664881483,
128.185552207591)) ;
#141077 = CARTESIAN_POINT('Ctrl Pts',(-27.0973867629725,14.3087959188899,
128.394119491692)) ;
#141078 = CARTESIAN_POINT('Ctrl Pts',(-27.1688826353453,14.4069520257531,
128.636056957824)) ;
#141079 = CARTESIAN_POINT('Ctrl Pts',(-27.2460944940994,14.434703937208,128.894776663616)) ;
#141080 = CARTESIAN_POINT('Ctrl Pts',(-27.322455233744,14.3899170706969,129.15096525146)) ;
#141081 = CARTESIAN_POINT('Ctrl Pts',(-27.3918872573227,14.275848167113,129.386924096555)) ;
#141082 = CARTESIAN_POINT('Ctrl Pts',(-27.4485941023117,14.1010294116989,
129.585654834495)) ;
#141083 = CARTESIAN_POINT('Ctrl Pts',(-27.4880125752689,13.8772033892953,
129.733965637947)) ;
#141084 = CARTESIAN_POINT('Ctrl Pts',(-27.5063600960657,13.6206146695245,
129.820736577765)) ;
#141085 = CARTESIAN_POINT('Ctrl Pts',(-27.5017041699236,13.3509220809883,
129.840178597232)) ;
#141086 = CARTESIAN_POINT('Ctrl Pts',(-27.473598569591,13.0853828321562,129.791246985454)) ;
#141087 = CARTESIAN_POINT('Ctrl Pts',(-27.4233898154442,12.8445475509271,
129.677681035035)) ;
#141088 = CARTESIAN_POINT('Ctrl Pts',(-27.3538833905169,12.6449528168769,
129.507770820876)) ;
#141089 = CARTESIAN_POINT('Ctrl Pts',(-27.2694172510683,12.5012606134937,
129.294132382056)) ;
#141090 = CARTESIAN_POINT('Ctrl Pts',(-27.1752933143249,12.4235056415569,
129.052276160427)) ;
#141091 = CARTESIAN_POINT('Ctrl Pts',(-27.0773273129102,12.4173186288012,
128.799252781911)) ;
#141092 = CARTESIAN_POINT('Ctrl Pts',(-26.9820546641332,12.4833715210388,
128.554075191291)) ;
#141093 = CARTESIAN_POINT('Ctrl Pts',(-26.8957427187905,12.6162286422635,
128.334974337295)) ;
#141094 = CARTESIAN_POINT('Ctrl Pts',(-26.8232541348428,12.8073411346184,
128.156380628229)) ;
#141095 = CARTESIAN_POINT('Ctrl Pts',(-26.7694384260827,13.0432166498449,
128.032389957765)) ;
#141096 = CARTESIAN_POINT('Ctrl Pts',(-26.7376022204803,13.3046950611415,
127.972397092543)) ;
#141097 = CARTESIAN_POINT('Ctrl Pts',(-26.7289133019392,13.5764464662961,
127.980250837782)) ;
#141098 = CARTESIAN_POINT('Ctrl Pts',(-26.7436047960042,13.8363551234792,
128.05630676716)) ;
#141099 = CARTESIAN_POINT('Ctrl Pts',(-26.7794413994135,14.0655922643217,
128.193961346238)) ;
#141100 = CARTESIAN_POINT('Ctrl Pts',(-26.8336382377925,14.2503954850495,
128.38547143464)) ;
#141101 = CARTESIAN_POINT('Ctrl Pts',(-26.9015725255857,14.3757154300573,
128.617161479179)) ;
#141102 = CARTESIAN_POINT('Ctrl Pts',(-26.97717390156,14.4321659963664,128.871117555925)) ;
#141103 = CARTESIAN_POINT('Ctrl Pts',(-27.0542951454193,14.416734287709,129.129400399269)) ;
#141104 = CARTESIAN_POINT('Ctrl Pts',(-27.1272709315475,14.330289953115,129.375702496647)) ;
#141105 = CARTESIAN_POINT('Ctrl Pts',(-27.189990205641,14.1784243130749,129.592118462722)) ;
#141106 = CARTESIAN_POINT('Ctrl Pts',(-27.2369829461064,13.9717507261075,
129.762638532864)) ;
#141107 = CARTESIAN_POINT('Ctrl Pts',(-27.2639778254799,13.7284356402105,
129.874378327128)) ;
#141108 = CARTESIAN_POINT('Ctrl Pts',(-27.2689082133704,13.4606301532886,
129.922024727165)) ;
#141109 = CARTESIAN_POINT('Ctrl Pts',(-27.2501277788475,13.1906191848992,
129.900339303317)) ;
#141110 = CARTESIAN_POINT('Ctrl Pts',(-27.2088647894994,12.9388679746563,
129.812757148243)) ;
#141111 = CARTESIAN_POINT('Ctrl Pts',(-27.1465129550907,12.7195132138376,
129.663887017964)) ;
#141112 = CARTESIAN_POINT('Ctrl Pts',(-27.0674166967818,12.5518557372857,
129.465961436593)) ;
#141113 = CARTESIAN_POINT('Ctrl Pts',(-26.9768706070221,12.4467157582098,
129.234433433492)) ;
#141114 = CARTESIAN_POINT('Ctrl Pts',(-26.8793527844966,12.4110145773966,
128.982819997536)) ;
#141115 = CARTESIAN_POINT('Ctrl Pts',(-26.7826642470665,12.4479828338558,
128.733367252288)) ;
#141116 = CARTESIAN_POINT('Ctrl Pts',(-26.6918813929173,12.5544308131199,
128.501279219724)) ;
#141117 = CARTESIAN_POINT('Ctrl Pts',(-26.6127197999617,12.7245572228014,
128.30335122958)) ;
#141118 = CARTESIAN_POINT('Ctrl Pts',(-26.5511850159183,12.9435040036317,
128.156658473163)) ;
#141119 = CARTESIAN_POINT('Ctrl Pts',(-26.5102190611483,13.1965754591591,
128.07005407176)) ;
#141120 = CARTESIAN_POINT('Ctrl Pts',(-26.4920475738245,13.4658054703846,
128.050031979519)) ;
#141121 = CARTESIAN_POINT('Ctrl Pts',(-26.4973097875531,13.732871013944,128.098578279237)) ;
#141122 = CARTESIAN_POINT('Ctrl Pts',(-26.5249498576305,13.9772573341515,
128.212437582729)) ;
#141123 = CARTESIAN_POINT('Ctrl Pts',(-26.5722033377622,14.1820529613216,
128.383597525912)) ;
#141124 = CARTESIAN_POINT('Ctrl Pts',(-26.6352241541874,14.3328844022839,
128.60092354091)) ;
#141125 = CARTESIAN_POINT('Ctrl Pts',(-26.7084097679367,14.4178011232664,
128.847856955232)) ;
#141126 = CARTESIAN_POINT('Ctrl Pts',(-26.7854970159119,14.4318123856393,
129.106011876347)) ;
#141127 = CARTESIAN_POINT('Ctrl Pts',(-26.8614289054063,14.3732302589804,
129.36113391513)) ;
#141128 = CARTESIAN_POINT('Ctrl Pts',(-26.9286362415281,14.2469702615313,
129.590490603117)) ;
#141129 = CARTESIAN_POINT('Ctrl Pts',(-26.9823748563956,14.062146427081,129.780527825508)) ;
#141130 = CARTESIAN_POINT('Ctrl Pts',(-27.0180716868534,13.8305006230351,
129.918009774563)) ;
#141131 = CARTESIAN_POINT('Ctrl Pts',(-27.0321547042406,13.5704780261443,
129.992234873768)) ;
#141132 = CARTESIAN_POINT('Ctrl Pts',(-27.02304498105,13.2994605324582,129.99876766656)) ;
#141133 = CARTESIAN_POINT('Ctrl Pts',(-26.990642584611,13.037734227312,129.937203717605)) ;
#141134 = CARTESIAN_POINT('Ctrl Pts',(-26.9366601478888,12.803624496366,129.812576900429)) ;
#141135 = CARTESIAN_POINT('Ctrl Pts',(-26.8637477811583,12.6130122644718,
129.632813056256)) ;
#141136 = CARTESIAN_POINT('Ctrl Pts',(-26.7771319980352,12.4813447222013,
129.412848032968)) ;
#141137 = CARTESIAN_POINT('Ctrl Pts',(-26.6817077227162,12.4167223738628,
129.167240678023)) ;
#141138 = CARTESIAN_POINT('Ctrl Pts',(-26.5838608694619,12.4243656160183,
128.91452903007)) ;
#141139 = CARTESIAN_POINT('Ctrl Pts',(-26.4898665957701,12.5034383279314,
128.673051616794)) ;
#141140 = CARTESIAN_POINT('Ctrl Pts',(-26.4055971039593,12.6484426938847,
128.460008405466)) ;
#141141 = CARTESIAN_POINT('Ctrl Pts',(-26.3364227025837,12.8490572514717,
128.291073622268)) ;
#141142 = CARTESIAN_POINT('Ctrl Pts',(-26.286632817812,13.0907450284177,128.178753459324)) ;
#141143 = CARTESIAN_POINT('Ctrl Pts',(-26.2590235096436,13.3559778959346,
128.131196454483)) ;
#141144 = CARTESIAN_POINT('Ctrl Pts',(-26.2548350038944,13.6264773514175,
128.152116585356)) ;
#141145 = CARTESIAN_POINT('Ctrl Pts',(-26.2735948253303,13.8815734058857,
128.239965472009)) ;
#141146 = CARTESIAN_POINT('Ctrl Pts',(-26.3132675920051,14.1045282831523,
128.388984294423)) ;
#141147 = CARTESIAN_POINT('Ctrl Pts',(-26.3705006334924,14.2789670592856,
128.58938512689)) ;
#141148 = CARTESIAN_POINT('Ctrl Pts',(-26.4400738173777,14.391495176626,128.825720476705)) ;
#141149 = CARTESIAN_POINT('Ctrl Pts',(-26.516521682403,14.4348607601378,129.082169907306)) ;
#141150 = CARTESIAN_POINT('Ctrl Pts',(-26.5935936372758,14.4056890506022,
129.34044345786)) ;
#141151 = CARTESIAN_POINT('Ctrl Pts',(-26.6649960120157,14.3062653151645,
129.582129996569)) ;
#141152 = CARTESIAN_POINT('Ctrl Pts',(-26.7249635553657,14.143440527592,129.790441806033)) ;
#141153 = CARTESIAN_POINT('Ctrl Pts',(-26.7684141471086,13.9296996140236,
129.950418504304)) ;
#141154 = CARTESIAN_POINT('Ctrl Pts',(-26.7916761698876,13.6772902096435,
130.051730701194)) ;
#141155 = CARTESIAN_POINT('Ctrl Pts',(-26.7920166713928,13.409949714787,130.085650574175)) ;
#141156 = CARTESIAN_POINT('Ctrl Pts',(-26.7690406668665,13.1418739498075,
130.051671418724)) ;
#141157 = CARTESIAN_POINT('Ctrl Pts',(-26.723380228586,12.8939990758876,129.951430090132)) ;
#141158 = CARTESIAN_POINT('Ctrl Pts',(-26.6580007927469,12.6844790937915,
129.793476110788)) ;
#141159 = CARTESIAN_POINT('Ctrl Pts',(-26.5756929840171,12.5265062627849,
129.586412690797)) ;
#141160 = CARTESIAN_POINT('Ctrl Pts',(-26.4836475460607,12.4345049835541,
129.350444325695)) ;
#141161 = CARTESIAN_POINT('Ctrl Pts',(-26.3856918165124,12.4124896125378,
129.097544125775)) ;
#141162 = CARTESIAN_POINT('Ctrl Pts',(-26.2897573999388,12.4629155090419,
128.850279348653)) ;
#141163 = CARTESIAN_POINT('Ctrl Pts',(-26.2006908721167,12.5820912846789,
128.623259203242)) ;
#141164 = CARTESIAN_POINT('Ctrl Pts',(-26.1246238315882,12.762437228793,128.434290332495)) ;
#141165 = CARTESIAN_POINT('Ctrl Pts',(-26.0668894647953,12.9881392996051,
128.298578201089)) ;
#141166 = CARTESIAN_POINT('Ctrl Pts',(-26.0298902648549,13.2462583810271,
128.223645427311)) ;
#141167 = CARTESIAN_POINT('Ctrl Pts',(-26.0161451635682,13.5176872670076,
128.216711625548)) ;
#141168 = CARTESIAN_POINT('Ctrl Pts',(-26.0257258719504,13.7805945427873,
128.277696305593)) ;
#141169 = CARTESIAN_POINT('Ctrl Pts',(-26.0573518405434,14.0195270315699,
128.403295435911)) ;
#141170 = CARTESIAN_POINT('Ctrl Pts',(-26.1079348776956,14.215038587717,128.58418549861)) ;
#141171 = CARTESIAN_POINT('Ctrl Pts',(-26.1731602667738,14.3538333245836,
128.807869014675)) ;
#141172 = CARTESIAN_POINT('Ctrl Pts',(-26.2474276298777,14.4259647082628,
129.057883463846)) ;
#141173 = CARTESIAN_POINT('Ctrl Pts',(-26.3253614750608,14.4260802645705,
129.318830419785)) ;
#141174 = CARTESIAN_POINT('Ctrl Pts',(-26.3993536485964,14.3549350188174,
129.567893070133)) ;
#141175 = CARTESIAN_POINT('Ctrl Pts',(-26.4649283623393,14.2162528409401,
129.792714680865)) ;
#141176 = CARTESIAN_POINT('Ctrl Pts',(-26.5155109902137,14.0213155988979,
129.97355085765)) ;
#141177 = CARTESIAN_POINT('Ctrl Pts',(-26.5473189700669,13.7835941603823,
130.099574541527)) ;
#141178 = CARTESIAN_POINT('Ctrl Pts',(-26.5571140519307,13.5186607714519,
130.161456345039)) ;
#141179 = CARTESIAN_POINT('Ctrl Pts',(-26.5436206328906,13.2494161503812,
130.154983697786)) ;
#141180 = CARTESIAN_POINT('Ctrl Pts',(-26.50683594055,12.990369061565,130.080765011974)) ;
#141181 = CARTESIAN_POINT('Ctrl Pts',(-26.4490861734073,12.763690008938,129.945095819254)) ;
#141182 = CARTESIAN_POINT('Ctrl Pts',(-26.3729175406989,12.5829313612557,
129.755895708972)) ;
#141183 = CARTESIAN_POINT('Ctrl Pts',(-26.2847953527081,12.4640788232719,
129.531321097916)) ;
#141184 = CARTESIAN_POINT('Ctrl Pts',(-26.1880587495672,12.4125693563369,
129.282013562901)) ;
#141185 = CARTESIAN_POINT('Ctrl Pts',(-26.0908313951311,12.4337094288139,
129.030974071127)) ;
#141186 = CARTESIAN_POINT('Ctrl Pts',(-25.9976681952167,12.5263145417804,
128.792132170837)) ;
#141187 = CARTESIAN_POINT('Ctrl Pts',(-25.9162455950597,12.6822587586298,
128.587265960244)) ;
#141188 = CARTESIAN_POINT('Ctrl Pts',(-25.8504252260032,12.891562566965,128.428112349608)) ;
#141189 = CARTESIAN_POINT('Ctrl Pts',(-25.8045634978476,13.1392603161048,
128.327287274008)) ;
#141190 = CARTESIAN_POINT('Ctrl Pts',(-25.7813146650202,13.4076118666746,
128.292561015423)) ;
#141191 = CARTESIAN_POINT('Ctrl Pts',(-25.7814884215431,13.6757335651874,
128.326078291203)) ;
#141192 = CARTESIAN_POINT('Ctrl Pts',(-25.8046625409424,13.9281677218218,
128.427127499137)) ;
#141193 = CARTESIAN_POINT('Ctrl Pts',(-25.8476422273,14.1410411473799,128.585519729201)) ;
#141194 = CARTESIAN_POINT('Ctrl Pts',(-25.907683202068,14.3051859898324,128.794181724547)) ;
#141195 = CARTESIAN_POINT('Ctrl Pts',(-25.978930527692,14.4050577743806,129.035370932357)) ;
#141196 = CARTESIAN_POINT('Ctrl Pts',(-26.0561466019767,14.4349188602028,
129.294141592844)) ;
#141197 = CARTESIAN_POINT('Ctrl Pts',(-26.132478258172,14.3922309332557,129.550183106697)) ;
#141198 = CARTESIAN_POINT('Ctrl Pts',(-26.2021814505518,14.280180814084,129.786927094144)) ;
#141199 = CARTESIAN_POINT('Ctrl Pts',(-26.2593826682603,14.1070359905501,
129.98710891507)) ;
#141200 = CARTESIAN_POINT('Ctrl Pts',(-26.2994671587914,13.8833119230109,
130.137511200348)) ;
#141201 = CARTESIAN_POINT('Ctrl Pts',(-26.318337977065,13.6288341860585,130.225620170339)) ;
#141202 = CARTESIAN_POINT('Ctrl Pts',(-26.3143645892423,13.3582465565096,
130.247188750393)) ;
#141203 = CARTESIAN_POINT('Ctrl Pts',(-26.2869754269948,13.0930921360638,
130.200247530991)) ;
#141204 = CARTESIAN_POINT('Ctrl Pts',(-26.2373396152418,12.8509540623848,
130.088400393616)) ;
#141205 = CARTESIAN_POINT('Ctrl Pts',(-26.1683668074332,12.6500624789761,
129.920030156326)) ;
#141206 = CARTESIAN_POINT('Ctrl Pts',(-26.0841377965404,12.5043219731701,
129.707136325983)) ;
#141207 = CARTESIAN_POINT('Ctrl Pts',(-25.9900281941511,12.4246931364435,
129.465377948168)) ;
#141208 = CARTESIAN_POINT('Ctrl Pts',(-25.8925815111015,12.4164962070895,
129.213702440245)) ;
#141209 = CARTESIAN_POINT('Ctrl Pts',(-25.7970766789543,12.480251448006,128.9678640707)) ;
#141210 = CARTESIAN_POINT('Ctrl Pts',(-25.7101967844713,12.6116453538561,
128.747191789048)) ;
#141211 = CARTESIAN_POINT('Ctrl Pts',(-25.6373443096755,12.8011773158268,
128.567502634195)) ;
#141212 = CARTESIAN_POINT('Ctrl Pts',(-25.5830591810682,13.0350451037076,
128.442022034867)) ;
#141213 = CARTESIAN_POINT('Ctrl Pts',(-25.5504047936859,13.296978163916,128.379768959982)) ;
#141214 = CARTESIAN_POINT('Ctrl Pts',(-25.5410675634481,13.567734807944,128.385602982608)) ;
#141215 = CARTESIAN_POINT('Ctrl Pts',(-25.5549687871613,13.8283852939848,
128.459355229538)) ;
#141216 = CARTESIAN_POINT('Ctrl Pts',(-25.5904030600774,14.0598715137087,
128.595997047928)) ;
#141217 = CARTESIAN_POINT('Ctrl Pts',(-25.6440274690769,14.2455588284616,
128.785744630347)) ;
#141218 = CARTESIAN_POINT('Ctrl Pts',(-25.7113284363032,14.372564186769,129.015457476957)) ;
#141219 = CARTESIAN_POINT('Ctrl Pts',(-25.7870239449595,14.4315964784329,
129.269802836714)) ;
#141220 = CARTESIAN_POINT('Ctrl Pts',(-25.8643623704875,14.4181824034525,
129.528794500079)) ;
#141221 = CARTESIAN_POINT('Ctrl Pts',(-25.9375242038495,14.3336377789342,
129.775633938815)) ;
#141222 = CARTESIAN_POINT('Ctrl Pts',(-26.0004478793548,14.1840090727439,
129.992551171513)) ;
#141223 = CARTESIAN_POINT('Ctrl Pts',(-26.0480191574849,13.9789557865459,
130.164753929132)) ;
#141224 = CARTESIAN_POINT('Ctrl Pts',(-26.0757639781487,13.7355807215654,
130.278815327172)) ;
#141225 = CARTESIAN_POINT('Ctrl Pts',(-26.0812599990852,13.4678621828446,
130.328144833775)) ;
#141226 = CARTESIAN_POINT('Ctrl Pts',(-26.0633151819106,13.1991327913341,
130.308713856629)) ;
#141227 = CARTESIAN_POINT('Ctrl Pts',(-26.0224676209765,12.945225699974,130.222533094685)) ;
#141228 = CARTESIAN_POINT('Ctrl Pts',(-25.9609990724827,12.7259341324381,
130.076051329516)) ;
#141229 = CARTESIAN_POINT('Ctrl Pts',(-25.8822604809974,12.5559411157644,
129.879237566137)) ;
#141230 = CARTESIAN_POINT('Ctrl Pts',(-25.7914597527613,12.448546099201,129.647141485638)) ;
#141231 = CARTESIAN_POINT('Ctrl Pts',(-25.6946150022909,12.4111599417381,
129.39729586978)) ;
#141232 = CARTESIAN_POINT('Ctrl Pts',(-25.5977172593343,12.4456278236405,
129.147262647583)) ;
#141233 = CARTESIAN_POINT('Ctrl Pts',(-25.5060117038367,12.5514145638213,
128.91274322654)) ;
#141234 = CARTESIAN_POINT('Ctrl Pts',(-25.4273295882221,12.7181519506854,
128.715846515651)) ;
#141235 = CARTESIAN_POINT('Ctrl Pts',(-25.3649037596215,12.9364297169796,
128.566681417571)) ;
#141236 = CARTESIAN_POINT('Ctrl Pts',(-25.323332482555,13.18875320047,128.478299070981)) ;
#141237 = CARTESIAN_POINT('Ctrl Pts',(-25.3044411252258,13.4580633582235,
128.456211243148)) ;
#141238 = CARTESIAN_POINT('Ctrl Pts',(-25.3090734679159,13.7256378176803,
128.502937534738)) ;
#141239 = CARTESIAN_POINT('Ctrl Pts',(-25.3360410802481,13.9704139793173,
128.61476470412)) ;
#141240 = CARTESIAN_POINT('Ctrl Pts',(-25.3827781783647,14.1767864699774,
128.78443560151)) ;
#141241 = CARTESIAN_POINT('Ctrl Pts',(-25.4454333702109,14.3292888824905,
129.00069713083)) ;
#141242 = CARTESIAN_POINT('Ctrl Pts',(-25.5181538685983,14.4162419172546,
129.246167034807)) ;
#141243 = CARTESIAN_POINT('Ctrl Pts',(-25.5956938103097,14.4323070544899,
129.505861185904)) ;
#141244 = CARTESIAN_POINT('Ctrl Pts',(-25.6710803564494,14.3764282188079,
129.759076945677)) ;
#141245 = CARTESIAN_POINT('Ctrl Pts',(-25.7391087689832,14.2515624978579,
129.991058480962)) ;
#141246 = CARTESIAN_POINT('Ctrl Pts',(-25.7932747288291,14.0682227623741,
130.182328167812)) ;
#141247 = CARTESIAN_POINT('Ctrl Pts',(-25.8296100576166,13.8370232958438,
130.321766242783)) ;
#141248 = CARTESIAN_POINT('Ctrl Pts',(-25.8442555060527,13.5786248872284,
130.397495870533)) ;
#141249 = CARTESIAN_POINT('Ctrl Pts',(-25.8358834370233,13.3076276344917,
130.406189803794)) ;
#141250 = CARTESIAN_POINT('Ctrl Pts',(-25.8041766941054,13.0452572131087,
130.346664739274)) ;
#141251 = CARTESIAN_POINT('Ctrl Pts',(-25.7505336279653,12.8091511761324,
130.223169232237)) ;
#141252 = CARTESIAN_POINT('Ctrl Pts',(-25.6781409528713,12.6175515473568,
130.044873070202)) ;
#141253 = CARTESIAN_POINT('Ctrl Pts',(-25.592105058716,12.4843717623364,129.826512043424)) ;
#141254 = CARTESIAN_POINT('Ctrl Pts',(-25.4967610810165,12.4175958607342,
129.581171788726)) ;
#141255 = CARTESIAN_POINT('Ctrl Pts',(-25.3990048864728,12.423055511444,129.328685771011)) ;
#141256 = CARTESIAN_POINT('Ctrl Pts',(-25.304669732605,12.5002516966647,129.086267631271)) ;
#141257 = CARTESIAN_POINT('Ctrl Pts',(-25.2202532201414,12.6429372151447,
128.872696249123)) ;
#141258 = CARTESIAN_POINT('Ctrl Pts',(-25.1502572326467,12.8430360326097,
128.70151673981)) ;
#141259 = CARTESIAN_POINT('Ctrl Pts',(-25.100056569004,13.0829431740334,128.587874270422)) ;
#141260 = CARTESIAN_POINT('Ctrl Pts',(-25.0717103188712,13.3482626607442,
128.538235999123)) ;
#141261 = CARTESIAN_POINT('Ctrl Pts',(-25.0668143083415,13.6179806011048,
128.556971818961)) ;
#141262 = CARTESIAN_POINT('Ctrl Pts',(-25.0850142932641,13.875457841107,128.64339943274)) ;
#141263 = CARTESIAN_POINT('Ctrl Pts',(-25.124300844542,14.0994368558722,128.791311810996)) ;
#141264 = CARTESIAN_POINT('Ctrl Pts',(-25.1807114497818,14.2743408494019,
128.989091173341)) ;
#141265 = CARTESIAN_POINT('Ctrl Pts',(-25.2501729019598,14.3892596808428,
129.225197599148)) ;
#141266 = CARTESIAN_POINT('Ctrl Pts',(-25.3264637380068,14.4346258040279,
129.481163853611)) ;
#141267 = CARTESIAN_POINT('Ctrl Pts',(-25.4038107016267,14.4074612293383,
129.740327944683)) ;
#141268 = CARTESIAN_POINT('Ctrl Pts',(-25.4754023445781,14.309698779788,129.982562521745)) ;
#141269 = CARTESIAN_POINT('Ctrl Pts',(-25.5355623444991,14.149377401071,130.191293654527)) ;
#141270 = CARTESIAN_POINT('Ctrl Pts',(-25.579751232365,13.9355628699076,130.35362784232)) ;
#141271 = CARTESIAN_POINT('Ctrl Pts',(-25.6034709375141,13.6861606150325,
130.455982421836)) ;
#141272 = CARTESIAN_POINT('Ctrl Pts',(-25.6045462391797,13.4167352196909,
130.492347116565)) ;
#141273 = CARTESIAN_POINT('Ctrl Pts',(-25.5821919384405,13.1492793409581,
130.460071094422)) ;
#141274 = CARTESIAN_POINT('Ctrl Pts',(-25.5371871208477,12.9005268752137,
130.361747259184)) ;
#141275 = CARTESIAN_POINT('Ctrl Pts',(-25.4722627818621,12.6897474195092,
130.205134842187)) ;
#141276 = CARTESIAN_POINT('Ctrl Pts',(-25.390755324331,12.5306016213155,130.000259613854)) ;
#141277 = CARTESIAN_POINT('Ctrl Pts',(-25.2984805593987,12.4360458788129,
129.763793833998)) ;
#141278 = CARTESIAN_POINT('Ctrl Pts',(-25.2007322982766,12.412131815675,129.511445036942)) ;
#141279 = CARTESIAN_POINT('Ctrl Pts',(-25.104473068318,12.4605358152628,129.263297371341)) ;
#141280 = CARTESIAN_POINT('Ctrl Pts',(-25.015042394543,12.5784164712972,129.035267066627)) ;
#141281 = CARTESIAN_POINT('Ctrl Pts',(-24.939138342932,12.7554817105356,128.84648405616)) ;
#141282 = CARTESIAN_POINT('Ctrl Pts',(-24.8803298764375,12.9817624941524,
128.707905450152)) ;
#141283 = CARTESIAN_POINT('Ctrl Pts',(-24.8429088332853,13.238159912852,128.631586768857)) ;
#141284 = CARTESIAN_POINT('Ctrl Pts',(-24.8284099370948,13.5101993099721,
128.622545061218)) ;
#141285 = CARTESIAN_POINT('Ctrl Pts',(-24.8373360171865,13.7733132280516,
128.681579397042)) ;
#141286 = CARTESIAN_POINT('Ctrl Pts',(-24.8685380944431,14.014064219241,128.806071656317)) ;
#141287 = CARTESIAN_POINT('Ctrl Pts',(-24.9184256609091,14.209874547802,128.98476052808)) ;
#141288 = CARTESIAN_POINT('Ctrl Pts',(-24.9832119214002,14.3505802758006,
129.207139933116)) ;
#141289 = CARTESIAN_POINT('Ctrl Pts',(-25.0573786128153,14.4248316803085,
129.456898592496)) ;
#141290 = CARTESIAN_POINT('Ctrl Pts',(-25.1352233259638,14.4272047931218,
129.717544442823)) ;
#141291 = CARTESIAN_POINT('Ctrl Pts',(-25.2095908938482,14.3577939123121,
129.967801571309)) ;
#141292 = CARTESIAN_POINT('Ctrl Pts',(-25.2752361261482,14.2217456845042,
130.192666800583)) ;
#141293 = CARTESIAN_POINT('Ctrl Pts',(-25.3267045949438,14.0267540354523,
130.376353398215)) ;
#141294 = CARTESIAN_POINT('Ctrl Pts',(-25.3588379023475,13.7911379046606,
130.503148112011)) ;
#141295 = CARTESIAN_POINT('Ctrl Pts',(-25.3693904125377,13.5273989700341,
130.567168396677)) ;
#141296 = CARTESIAN_POINT('Ctrl Pts',(-25.356570795273,13.2571615768974,130.562775183947)) ;
#141297 = CARTESIAN_POINT('Ctrl Pts',(-25.3204195881661,12.9974107950377,
130.49041379717)) ;
#141298 = CARTESIAN_POINT('Ctrl Pts',(-25.2631584465656,12.7695379002692,
130.356198249557)) ;
#141299 = CARTESIAN_POINT('Ctrl Pts',(-25.1878940849675,12.5879936402029,
130.169461722707)) ;
#141300 = CARTESIAN_POINT('Ctrl Pts',(-25.0995423284155,12.4663339482719,
129.94442760723)) ;
#141301 = CARTESIAN_POINT('Ctrl Pts',(-25.0029353623396,12.4130530274037,
129.695488820152)) ;
#141302 = CARTESIAN_POINT('Ctrl Pts',(-24.9058352313859,12.4321501261291,
129.444765661347)) ;
#141303 = CARTESIAN_POINT('Ctrl Pts',(-24.8126115718343,12.5224108266138,
129.205678168256)) ;
#141304 = CARTESIAN_POINT('Ctrl Pts',(-24.7304215398182,12.677312247728,128.998719014252)) ;
#141305 = CARTESIAN_POINT('Ctrl Pts',(-24.6641964360112,12.8853932149283,
128.838366520164)) ;
#141306 = CARTESIAN_POINT('Ctrl Pts',(-24.6178771552594,13.1311434716641,
128.736066599532)) ;
#141307 = CARTESIAN_POINT('Ctrl Pts',(-24.5938296155373,13.400088705093,128.699120704413)) ;
#141308 = CARTESIAN_POINT('Ctrl Pts',(-24.5934287047137,13.6679854897532,
128.730912226515)) ;
#141309 = CARTESIAN_POINT('Ctrl Pts',(-24.6156510295128,13.9198929111463,
128.82897060526)) ;
#141310 = CARTESIAN_POINT('Ctrl Pts',(-24.6586746207821,14.1367331628791,
128.987925161323)) ;
#141311 = CARTESIAN_POINT('Ctrl Pts',(-24.7177298808385,14.300676127775,129.193353483904)) ;
#141312 = CARTESIAN_POINT('Ctrl Pts',(-24.7891652491851,14.4034182514066,
129.435324255067)) ;
#141313 = CARTESIAN_POINT('Ctrl Pts',(-24.8661178021545,14.4350219446425,
129.693230679241)) ;
#141314 = CARTESIAN_POINT('Ctrl Pts',(-24.9426427517626,14.3943912068368,
129.949881794211)) ;
#141315 = CARTESIAN_POINT('Ctrl Pts',(-25.0126014634411,14.2842181110636,
130.187358662861)) ;
#141316 = CARTESIAN_POINT('Ctrl Pts',(-25.0702385393857,14.1123337735145,
130.388851754434)) ;
#141317 = CARTESIAN_POINT('Ctrl Pts',(-25.1106557279227,13.8914432947139,
130.539995528719)) ;
#141318 = CARTESIAN_POINT('Ctrl Pts',(-25.1303460035706,13.6364805468731,
130.630669027387)) ;
#141319 = CARTESIAN_POINT('Ctrl Pts',(-25.1270349079514,13.3663281054811,
130.654132094012)) ;
#141320 = CARTESIAN_POINT('Ctrl Pts',(-25.10027987688,13.1002904156236,130.609104691335)) ;
#141321 = CARTESIAN_POINT('Ctrl Pts',(-25.0512395903328,12.8573186036191,
130.498986163059)) ;
#141322 = CARTESIAN_POINT('Ctrl Pts',(-24.9827606397883,12.655055825907,130.332060726985)) ;
#141323 = CARTESIAN_POINT('Ctrl Pts',(-24.8989878483042,12.5076994513089,
130.120463312692)) ;
#141324 = CARTESIAN_POINT('Ctrl Pts',(-24.8051012286791,12.4260781925878,
129.879353041103)) ;
#141325 = CARTESIAN_POINT('Ctrl Pts',(-24.7077158005553,12.4155414447684,
129.627838457708)) ;
#141326 = CARTESIAN_POINT('Ctrl Pts',(-24.6113622754169,12.478090322654,129.379774872544)) ;
#141327 = CARTESIAN_POINT('Ctrl Pts',(-24.5249865423267,12.6066344478164,
129.160266874238)) ;
#141328 = CARTESIAN_POINT('Ctrl Pts',(-24.4513172549699,12.7952137023379,
128.978327228472)) ;
#141329 = CARTESIAN_POINT('Ctrl Pts',(-24.3965263603158,13.0279819979312,
128.851345529342)) ;
#141330 = CARTESIAN_POINT('Ctrl Pts',(-24.3631902230821,13.2896875880003,
128.787142151235)) ;
#141331 = CARTESIAN_POINT('Ctrl Pts',(-24.353237574026,13.5603129292438,128.791160312568)) ;
#141332 = CARTESIAN_POINT('Ctrl Pts',(-24.3664638245753,13.8211028677067,
128.862887276775)) ;
#141333 = CARTESIAN_POINT('Ctrl Pts',(-24.4013270139757,14.053803313072,128.997878663223)) ;
#141334 = CARTESIAN_POINT('Ctrl Pts',(-24.4545017892813,14.2410908350298,
129.186323723895)) ;
#141335 = CARTESIAN_POINT('Ctrl Pts',(-24.5217031916119,14.3701941601828,
129.415842737755)) ;
#141336 = CARTESIAN_POINT('Ctrl Pts',(-24.597197642324,14.4308809616827,129.669568740632)) ;
#141337 = CARTESIAN_POINT('Ctrl Pts',(-24.6743263714102,14.4196138695008,
129.927844860309)) ;
#141338 = CARTESIAN_POINT('Ctrl Pts',(-24.7478689182381,14.3368368148889,
130.175876279872)) ;
#141339 = CARTESIAN_POINT('Ctrl Pts',(-24.8109786100875,14.1892310626699,
130.393251616306)) ;
#141340 = CARTESIAN_POINT('Ctrl Pts',(-24.8590750037211,13.9859052749166,
130.566957801464)) ;
#141341 = CARTESIAN_POINT('Ctrl Pts',(-24.8875059799453,13.7426111503383,
130.683133832411)) ;
#141342 = CARTESIAN_POINT('Ctrl Pts',(-24.893634064606,13.4761437933061,130.734199736731)) ;
#141343 = CARTESIAN_POINT('Ctrl Pts',(-24.876424077817,13.207093106288,130.716931703523)) ;
#141344 = CARTESIAN_POINT('Ctrl Pts',(-24.8361611582837,12.9521503447167,
130.632500310692)) ;
#141345 = CARTESIAN_POINT('Ctrl Pts',(-24.7752501370882,12.7315094010331,
130.487653228042)) ;
#141346 = CARTESIAN_POINT('Ctrl Pts',(-24.6965758178761,12.5595225483876,
130.291156310629)) ;
#141347 = CARTESIAN_POINT('Ctrl Pts',(-24.6067705147701,12.4509681320899,
130.061702132681)) ;
#141348 = CARTESIAN_POINT('Ctrl Pts',(-24.5092389918735,12.4111337662686,
129.810124891726)) ;
#141349 = CARTESIAN_POINT('Ctrl Pts',(-24.4127206080174,12.4436883981266,
129.561039626234)) ;
#141350 = CARTESIAN_POINT('Ctrl Pts',(-24.3206925540612,12.5474867377232,
129.325602640613)) ;
#141351 = CARTESIAN_POINT('Ctrl Pts',(-24.2416819636404,12.7123018064528,
129.127697092053)) ;
#141352 = CARTESIAN_POINT('Ctrl Pts',(-24.1785497831319,12.9300708063277,
128.976576940149)) ;
#141353 = CARTESIAN_POINT('Ctrl Pts',(-24.1365376956219,13.1802337565337,
128.886722669123)) ;
#141354 = CARTESIAN_POINT('Ctrl Pts',(-24.1168251300341,13.4510759335073,
128.862457184691)) ;
#141355 = CARTESIAN_POINT('Ctrl Pts',(-24.120840546179,13.7180593172982,128.907263452931)) ;
#141356 = CARTESIAN_POINT('Ctrl Pts',(-24.1472467528154,13.9642786305136,
129.017528555115)) ;
#141357 = CARTESIAN_POINT('Ctrl Pts',(-24.1933829926006,14.1712561910319,
129.18534923182)) ;
#141358 = CARTESIAN_POINT('Ctrl Pts',(-24.2553727944982,14.3253725381315,
129.399556943149)) ;
#141359 = CARTESIAN_POINT('Ctrl Pts',(-24.3284416395332,14.4148742721194,
129.646304105575)) ;
#141360 = CARTESIAN_POINT('Ctrl Pts',(-24.4053454883016,14.4329087862449,
129.90387754185)) ;
#141361 = CARTESIAN_POINT('Ctrl Pts',(-24.481387664403,14.3788838227845,130.159238685966)) ;
#141362 = CARTESIAN_POINT('Ctrl Pts',(-24.5494784339386,14.2561019527568,
130.391287541648)) ;
#141363 = CARTESIAN_POINT('Ctrl Pts',(-24.6041424746569,14.0742377640131,
130.584037902831)) ;
#141364 = CARTESIAN_POINT('Ctrl Pts',(-24.6409425374017,13.8451949445008,
130.724693125171)) ;
#141365 = CARTESIAN_POINT('Ctrl Pts',(-24.6564073870346,13.58674350493,130.802914286476)) ;
#141366 = CARTESIAN_POINT('Ctrl Pts',(-24.648598332483,13.3144404098801,130.81341628994)) ;
#141367 = CARTESIAN_POINT('Ctrl Pts',(-24.6176344680258,13.0528695222705,
130.755903610597)) ;
#141368 = CARTESIAN_POINT('Ctrl Pts',(-24.5647644326536,12.8160517966369,
130.634605136453)) ;
#141369 = CARTESIAN_POINT('Ctrl Pts',(-24.4928190367482,12.6226065253332,
130.457653206199)) ;
#141370 = CARTESIAN_POINT('Ctrl Pts',(-24.4069484394412,12.4871996902566,
130.239845544222)) ;
#141371 = CARTESIAN_POINT('Ctrl Pts',(-24.3114166195875,12.4184347650075,
129.994074210014)) ;
#141372 = CARTESIAN_POINT('Ctrl Pts',(-24.2142170838312,12.4219001268695,
129.743022475508)) ;
#141373 = CARTESIAN_POINT('Ctrl Pts',(-24.1195700162809,12.4968774725135,
129.499727012216)) ;
#141374 = CARTESIAN_POINT('Ctrl Pts',(-24.0346625589609,12.6381726387492,
129.284784810722)) ;
#141375 = CARTESIAN_POINT('Ctrl Pts',(-23.9643653426145,12.8360677562161,
129.112611003455)) ;
#141376 = CARTESIAN_POINT('Ctrl Pts',(-23.9133140744109,13.0762566249802,
128.996657468451)) ;
#141377 = CARTESIAN_POINT('Ctrl Pts',(-23.8844732807761,13.3398740968699,
128.945410468149)) ;
#141378 = CARTESIAN_POINT('Ctrl Pts',(-23.8788261461933,13.6103044053491,
128.962027024672)) ;
#141379 = CARTESIAN_POINT('Ctrl Pts',(-23.8963862756814,13.86812497933,129.046546801647)) ;
#141380 = CARTESIAN_POINT('Ctrl Pts',(-23.9349997883254,14.0932871473164,
129.19246618752)) ;
#141381 = CARTESIAN_POINT('Ctrl Pts',(-23.9913900660586,14.2707836651958,
129.390408363815)) ;
#141382 = CARTESIAN_POINT('Ctrl Pts',(-24.060163393742,14.3866738498425,129.62429552567)) ;
#141383 = CARTESIAN_POINT('Ctrl Pts',(-24.1363780076905,14.4343395644747,
129.880066368684)) ;
#141384 = CARTESIAN_POINT('Ctrl Pts',(-24.2136312221482,14.4093417118186,
130.138889245811)) ;
#141385 = CARTESIAN_POINT('Ctrl Pts',(-24.2855250652056,14.3139583253282,
130.382003572305)) ;
#141386 = CARTESIAN_POINT('Ctrl Pts',(-24.3464841520355,14.1538396084722,
130.593328181351)) ;
#141387 = CARTESIAN_POINT('Ctrl Pts',(-24.3907969417544,13.9434082094923,
130.755696634518)) ;
#141388 = CARTESIAN_POINT('Ctrl Pts',(-24.4153872134604,13.6926166180059,
130.860902823485)) ;
#141389 = CARTESIAN_POINT('Ctrl Pts',(-24.4170476036422,13.4252309557657,
130.898745794972)) ;
#141390 = CARTESIAN_POINT('Ctrl Pts',(-24.3954087414857,13.15699249017,130.868626430046)) ;
#141391 = CARTESIAN_POINT('Ctrl Pts',(-24.3510658797357,12.9074157483193,
130.772222097412)) ;
#141392 = CARTESIAN_POINT('Ctrl Pts',(-24.2863589270511,12.6946405590363,
130.61638199744)) ;
#141393 = CARTESIAN_POINT('Ctrl Pts',(-24.2058364240148,12.5348309265639,
130.414146669772)) ;
#141394 = CARTESIAN_POINT('Ctrl Pts',(-24.1132237165813,12.4376124646164,
130.176911811757)) ;
#141395 = CARTESIAN_POINT('Ctrl Pts',(-24.0160435387035,12.411847051691,129.926043454964)) ;
#141396 = CARTESIAN_POINT('Ctrl Pts',(-23.9194951840902,12.4580456629596,
129.677111506706)) ;
#141397 = CARTESIAN_POINT('Ctrl Pts',(-23.8299476378923,12.5736491425348,
129.44866350134)) ;
#141398 = CARTESIAN_POINT('Ctrl Pts',(-23.7532981226229,12.7495592043743,
129.257815243214)) ;
#141399 = CARTESIAN_POINT('Ctrl Pts',(-23.6938060546769,12.9753684252062,
129.117325067753)) ;
#141400 = CARTESIAN_POINT('Ctrl Pts',(-23.655836225325,13.2312290478431,129.039409580857)) ;
#141401 = CARTESIAN_POINT('Ctrl Pts',(-23.6407041156802,13.5022492390578,
129.028403475674)) ;
#141402 = CARTESIAN_POINT('Ctrl Pts',(-23.6490347776743,13.766376795235,129.085779280314)) ;
#141403 = CARTESIAN_POINT('Ctrl Pts',(-23.679347360503,14.0063277413084,129.20741315707)) ;
#141404 = CARTESIAN_POINT('Ctrl Pts',(-23.7288783361076,14.2048736878869,
129.385229002076)) ;
#141405 = CARTESIAN_POINT('Ctrl Pts',(-23.7935423808548,14.3476912358554,
129.607350754785)) ;
#141406 = CARTESIAN_POINT('Ctrl Pts',(-23.8676082278984,14.4237776456092,
129.856845126396)) ;
#141407 = CARTESIAN_POINT('Ctrl Pts',(-23.9452312757094,14.4280807671714,
130.116754966379)) ;
#141408 = CARTESIAN_POINT('Ctrl Pts',(-24.0198127822077,14.3608278404858,
130.367644260992)) ;
#141409 = CARTESIAN_POINT('Ctrl Pts',(-24.0859834375975,14.2256360028295,
130.59418483557)) ;
#141410 = CARTESIAN_POINT('Ctrl Pts',(-24.1373843631784,14.0344799528452,
130.77728489612)) ;
#141411 = CARTESIAN_POINT('Ctrl Pts',(-24.1704902224659,13.7980435581084,
130.907211792896)) ;
#141412 = CARTESIAN_POINT('Ctrl Pts',(-24.181617086575,13.5353241773225,130.972828569372)) ;
#141413 = CARTESIAN_POINT('Ctrl Pts',(-24.1694421615744,13.2644873700543,
130.970392633471)) ;
#141414 = CARTESIAN_POINT('Ctrl Pts',(-24.1340736108702,13.0050528435928,
130.900194260651)) ;
#141415 = CARTESIAN_POINT('Ctrl Pts',(-24.0772794060259,12.7754380039954,
130.767426952221)) ;
#141416 = CARTESIAN_POINT('Ctrl Pts',(-24.0025528244517,12.592596001974,130.582218534765)) ;
#141417 = CARTESIAN_POINT('Ctrl Pts',(-23.9145219022242,12.4690081971512,
130.358123680554)) ;
#141418 = CARTESIAN_POINT('Ctrl Pts',(-23.8181204758606,12.4135709103977,
130.109761674319)) ;
#141419 = CARTESIAN_POINT('Ctrl Pts',(-23.7207896010503,12.4306395059357,
129.858430292254)) ;
#141420 = CARTESIAN_POINT('Ctrl Pts',(-23.6276243337301,12.5185475341995,
129.619406098751)) ;
#141421 = CARTESIAN_POINT('Ctrl Pts',(-23.5449043158209,12.671844049154,129.410953733645)) ;
#141422 = CARTESIAN_POINT('Ctrl Pts',(-23.4781856474444,12.8780302029366,
129.249096526566)) ;
#141423 = CARTESIAN_POINT('Ctrl Pts',(-23.4309201247871,13.1252486430467,
129.144338143815)) ;
#141424 = CARTESIAN_POINT('Ctrl Pts',(-23.406493307167,13.3909665765868,129.105916906452)) ;
#141425 = CARTESIAN_POINT('Ctrl Pts',(-23.405312666089,13.6612161076759,129.135695199137)) ;
#141426 = CARTESIAN_POINT('Ctrl Pts',(-23.4269936000131,13.9131568870817,
129.232093080542)) ;
#141427 = CARTESIAN_POINT('Ctrl Pts',(-23.4692035971914,14.130438408173,129.388523345915)) ;
#141428 = CARTESIAN_POINT('Ctrl Pts',(-23.5280845861359,14.2969775109189,
129.593597224986)) ;
#141429 = CARTESIAN_POINT('Ctrl Pts',(-23.5993935198417,14.4015522166871,
129.835242815097)) ;
#141430 = CARTESIAN_POINT('Ctrl Pts',(-23.675998443287,14.4350500551864,130.092020579583)) ;
#141431 = CARTESIAN_POINT('Ctrl Pts',(-23.7525397078438,14.3967519658026,
130.348679751607)) ;
#141432 = CARTESIAN_POINT('Ctrl Pts',(-23.8228714214555,14.2884849185217,
130.5872861249)) ;
#141433 = CARTESIAN_POINT('Ctrl Pts',(-23.8810098442615,14.1181740873397,
130.790267409901)) ;
#141434 = CARTESIAN_POINT('Ctrl Pts',(-23.922044787637,13.8977533327247,130.943313957249)) ;
#141435 = CARTESIAN_POINT('Ctrl Pts',(-23.9422876471947,13.6446684520944,
131.035448870912)) ;
#141436 = CARTESIAN_POINT('Ctrl Pts',(-23.9396680552135,13.3734340111263,
131.061088380113)) ;
#141437 = CARTESIAN_POINT('Ctrl Pts',(-23.9134836273722,13.1072276556743,
131.017706686836)) ;
#141438 = CARTESIAN_POINT('Ctrl Pts',(-23.8652358369202,12.8641925362022,
130.909786178128)) ;
#141439 = CARTESIAN_POINT('Ctrl Pts',(-23.7973125355255,12.6605227447286,
130.744477407299)) ;
#141440 = CARTESIAN_POINT('Ctrl Pts',(-23.7140967001381,12.511411732543,130.534451455081)) ;
#141441 = CARTESIAN_POINT('Ctrl Pts',(-23.6198656680205,12.4272142071662,
130.292531553557)) ;
#141442 = CARTESIAN_POINT('Ctrl Pts',(-23.522639981657,12.415034803424,130.041439124737)) ;
#141443 = CARTESIAN_POINT('Ctrl Pts',(-23.4267624796708,12.474749132082,129.79453863735)) ;
#141444 = CARTESIAN_POINT('Ctrl Pts',(-23.3392886616417,12.6023246098268,
129.572102763682)) ;
#141445 = CARTESIAN_POINT('Ctrl Pts',(-23.26521460158,12.7898414639342,129.388996496963)) ;
#141446 = CARTESIAN_POINT('Ctrl Pts',(-23.2100681969718,13.0206707820948,
129.260851722597)) ;
#141447 = CARTESIAN_POINT('Ctrl Pts',(-23.1760485062128,13.2818518807112,
129.194659336828)) ;
#141448 = CARTESIAN_POINT('Ctrl Pts',(-23.1654158714073,13.552127865025,129.196649551748)) ;
#141449 = CARTESIAN_POINT('Ctrl Pts',(-23.1779469522343,13.8139569141608,
129.266397522322)) ;
#141450 = CARTESIAN_POINT('Ctrl Pts',(-23.2124687860924,14.0485699408796,
129.400538385715)) ;
#141451 = CARTESIAN_POINT('Ctrl Pts',(-23.2648627947572,14.2361101899088,
129.58649101522)) ;
#141452 = CARTESIAN_POINT('Ctrl Pts',(-23.3319172217269,14.3675384217247,
129.81568463473)) ;
#141453 = CARTESIAN_POINT('Ctrl Pts',(-23.4070931352948,14.4300942313948,
130.068399713215)) ;
#141454 = CARTESIAN_POINT('Ctrl Pts',(-23.4843627263749,14.420886512356,130.327144314321)) ;
#141455 = CARTESIAN_POINT('Ctrl Pts',(-23.5578964392717,14.3405660853883,
130.575037945399)) ;
#141456 = CARTESIAN_POINT('Ctrl Pts',(-23.6218881748358,14.1934622330658,
130.795265313375)) ;
#141457 = CARTESIAN_POINT('Ctrl Pts',(-23.6702413860333,13.9917021731483,
130.969631968682)) ;
#141458 = CARTESIAN_POINT('Ctrl Pts',(-23.6991655434952,13.7502056369867,
131.087135180438)) ;
#141459 = CARTESIAN_POINT('Ctrl Pts',(-23.706030166973,13.4844947151479,131.140309759337)) ;
#141460 = CARTESIAN_POINT('Ctrl Pts',(-23.6894020057051,13.2141840714607,
131.124881280057)) ;
#141461 = CARTESIAN_POINT('Ctrl Pts',(-23.6498448165609,12.958922795002,131.042450027368)) ;
#141462 = CARTESIAN_POINT('Ctrl Pts',(-23.589051488531,12.7362702687102,130.898123427805)) ;
#141463 = CARTESIAN_POINT('Ctrl Pts',(-23.5119547526697,12.5648474915298,
130.705761330521)) ;
#141464 = CARTESIAN_POINT('Ctrl Pts',(-23.4214046717168,12.452872631945,130.474532293699)) ;
#141465 = CARTESIAN_POINT('Ctrl Pts',(-23.3248409697496,12.41129419742,130.225470559134)) ;
#141466 = CARTESIAN_POINT('Ctrl Pts',(-23.2273437603083,12.4419882083232,
129.973846467319)) ;
#141467 = CARTESIAN_POINT('Ctrl Pts',(-23.1360177918426,12.5427027848013,
129.740097133431)) ;
#141468 = CARTESIAN_POINT('Ctrl Pts',(-23.0559375842205,12.7067963976432,
129.539325291128)) ;
#141469 = CARTESIAN_POINT('Ctrl Pts',(-22.9925343542045,12.9221001541686,
129.387231951601)) ;
#141470 = CARTESIAN_POINT('Ctrl Pts',(-22.9494611772759,13.1741319902504,
129.294633889042)) ;
#141471 = CARTESIAN_POINT('Ctrl Pts',(-22.9293237492918,13.4427023362762,
129.268862408672)) ;
#141472 = CARTESIAN_POINT('Ctrl Pts',(-22.9326242894509,13.7107857212086,
129.311682353004)) ;
#141473 = CARTESIAN_POINT('Ctrl Pts',(-22.9583033588113,13.956888330194,129.419685271958)) ;
#141474 = CARTESIAN_POINT('Ctrl Pts',(-23.0040060644692,14.1661036929037,
129.586354227263)) ;
#141475 = CARTESIAN_POINT('Ctrl Pts',(-23.0657731632118,14.3219385193613,
129.79996865813)) ;
#141476 = CARTESIAN_POINT('Ctrl Pts',(-23.1381200326655,14.4130180852625,
130.044389910157)) ;
#141477 = CARTESIAN_POINT('Ctrl Pts',(-23.2154893821187,14.4335349336769,
130.303544854118)) ;
#141478 = CARTESIAN_POINT('Ctrl Pts',(-23.2917026997898,14.3810414218173,
130.559436531221)) ;
#141479 = CARTESIAN_POINT('Ctrl Pts',(-23.3597411358198,14.2609490828525,
130.791144458003)) ;
#141480 = CARTESIAN_POINT('Ctrl Pts',(-23.4151538663912,14.079534400134,130.986279889569)) ;
#141481 = CARTESIAN_POINT('Ctrl Pts',(-23.4523380353655,13.8529283959852,
131.127860729194)) ;
#141482 = CARTESIAN_POINT('Ctrl Pts',(-23.468524967232,13.5926907244754,131.208501026069)) ;
#141483 = CARTESIAN_POINT('Ctrl Pts',(-23.4613879378508,13.3230678017147,
131.220637494974)) ;
#141484 = CARTESIAN_POINT('Ctrl Pts',(-23.4310172633009,13.0595444653147,
131.165038572153)) ;
#141485 = CARTESIAN_POINT('Ctrl Pts',(-23.3785101643465,12.8214089114898,
131.044865099349)) ;
#141486 = CARTESIAN_POINT('Ctrl Pts',(-23.3071345050513,12.6270967453298,
130.869510720629)) ;
#141487 = CARTESIAN_POINT('Ctrl Pts',(-23.2218885053547,12.4904301737517,
130.653416002948)) ;
#141488 = CARTESIAN_POINT('Ctrl Pts',(-23.1268539668659,12.41952640959,130.408994465976)) ;
#141489 = CARTESIAN_POINT('Ctrl Pts',(-23.0291669887329,12.4206998048116,
130.156680505045)) ;
#141490 = CARTESIAN_POINT('Ctrl Pts',(-22.9342126331685,12.4940151693159,
129.912536358994)) ;
#141491 = CARTESIAN_POINT('Ctrl Pts',(-22.8492111459651,12.6331734793058,
129.697224789051)) ;
#141492 = CARTESIAN_POINT('Ctrl Pts',(-22.7784689920698,12.8293256852298,
129.523716827136)) ;
#141493 = CARTESIAN_POINT('Ctrl Pts',(-22.7267830961436,13.0683012939604,
129.405890318511)) ;
#141494 = CARTESIAN_POINT('Ctrl Pts',(-22.6971667052242,13.3322967725392,
129.352483196923)) ;
#141495 = CARTESIAN_POINT('Ctrl Pts',(-22.6908974667905,13.6026350043085,
129.367260428482)) ;
#141496 = CARTESIAN_POINT('Ctrl Pts',(-22.7077206912287,13.8605088968992,
129.44954355041)) ;
#141497 = CARTESIAN_POINT('Ctrl Pts',(-22.7457980674478,14.0871784640944,
129.593944579997)) ;
#141498 = CARTESIAN_POINT('Ctrl Pts',(-22.8015081236511,14.265834440122,129.789787245735)) ;
#141499 = CARTESIAN_POINT('Ctrl Pts',(-22.8702580651156,14.3843789684771,
130.023754668897)) ;
#141500 = CARTESIAN_POINT('Ctrl Pts',(-22.9465090739444,14.4339734265458,
130.279692171881)) ;
#141501 = CARTESIAN_POINT('Ctrl Pts',(-23.0235969708249,14.4110559210102,
130.537938086999)) ;
#141502 = CARTESIAN_POINT('Ctrl Pts',(-23.0956663651172,14.3178924901581,
130.781531217281)) ;
#141503 = CARTESIAN_POINT('Ctrl Pts',(-23.1571514980903,14.1593686470185,
130.994439940708)) ;
#141504 = CARTESIAN_POINT('Ctrl Pts',(-23.2020241924619,13.9496805218115,
131.158514572577)) ;
#141505 = CARTESIAN_POINT('Ctrl Pts',(-23.2271393720092,13.7013469938743,
131.265044356128)) ;
#141506 = CARTESIAN_POINT('Ctrl Pts',(-23.2295577349915,13.4330164717232,
131.305263682426)) ;
#141507 = CARTESIAN_POINT('Ctrl Pts',(-23.2086111408663,13.1647607715786,
131.277127741886)) ;
#141508 = CARTESIAN_POINT('Ctrl Pts',(-23.1647278376412,12.9137312008662,
131.18216641284)) ;
#141509 = CARTESIAN_POINT('Ctrl Pts',(-23.1009545230825,12.7007529783777,
131.028861056442)) ;
#141510 = CARTESIAN_POINT('Ctrl Pts',(-23.0203445087878,12.5383275920807,
130.826577670387)) ;
#141511 = CARTESIAN_POINT('Ctrl Pts',(-22.9287530034321,12.4398166111486,
130.59204481027)) ;
#141512 = CARTESIAN_POINT('Ctrl Pts',(-22.8308357993991,12.4114725010168,
130.339306419179)) ;
#141513 = CARTESIAN_POINT('Ctrl Pts',(-22.7343885893122,12.4557968950616,
130.090594438971)) ;
#141514 = CARTESIAN_POINT('Ctrl Pts',(-22.644462571658,12.569629101587,129.861079793437)) ;
#141515 = CARTESIAN_POINT('Ctrl Pts',(-22.5675688072916,12.7436129687706,
129.669441199026)) ;
#141516 = CARTESIAN_POINT('Ctrl Pts',(-22.5074742150958,12.9681022843807,
129.527185830781)) ;
#141517 = CARTESIAN_POINT('Ctrl Pts',(-22.468793772561,13.2239471753799,129.447276223009)) ;
#141518 = CARTESIAN_POINT('Ctrl Pts',(-22.4530382205004,13.4941633310118,
129.434364446316)) ;
#141519 = CARTESIAN_POINT('Ctrl Pts',(-22.4606774149823,13.7589186956337,
129.489743991273)) ;
#141520 = CARTESIAN_POINT('Ctrl Pts',(-22.4903861345707,13.9998349614895,
129.609611812731)) ;
#141521 = CARTESIAN_POINT('Ctrl Pts',(-22.5394138503083,14.1997646891006,
129.785956045042)) ;
#141522 = CARTESIAN_POINT('Ctrl Pts',(-22.6035812001282,14.344263749604,130.006567187812)) ;
#141523 = CARTESIAN_POINT('Ctrl Pts',(-22.6775949801385,14.4224928496146,
130.255978432946)) ;
#141524 = CARTESIAN_POINT('Ctrl Pts',(-22.7548151168621,14.4291711030004,
130.514539462714)) ;
#141525 = CARTESIAN_POINT('Ctrl Pts',(-22.8301186292218,14.3636108427049,
130.767784158612)) ;
#141526 = CARTESIAN_POINT('Ctrl Pts',(-22.8963852155264,14.2305640728087,
130.994488176039)) ;
#141527 = CARTESIAN_POINT('Ctrl Pts',(-22.9483632007256,14.0406274763076,
131.179334305198)) ;
#141528 = CARTESIAN_POINT('Ctrl Pts',(-22.9819990811783,13.8058698761943,
131.310720597295)) ;
#141529 = CARTESIAN_POINT('Ctrl Pts',(-22.9938487433692,13.5427807142404,
131.378566461829)) ;
#141530 = CARTESIAN_POINT('Ctrl Pts',(-22.9823232445732,13.2720604281958,
131.378004543633)) ;
#141531 = CARTESIAN_POINT('Ctrl Pts',(-22.9475403030834,13.0118428173477,
131.309548132463)) ;
#141532 = CARTESIAN_POINT('Ctrl Pts',(-22.8915112375159,12.7818787427455,
131.178906192752)) ;
#141533 = CARTESIAN_POINT('Ctrl Pts',(-22.8171006460482,12.5968716108038,
130.994704335963)) ;
#141534 = CARTESIAN_POINT('Ctrl Pts',(-22.7289778755317,12.4712516936664,
130.770472889898)) ;
#141535 = CARTESIAN_POINT('Ctrl Pts',(-22.6331833007374,12.4142247915804,
130.523717556835)) ;
#141536 = CARTESIAN_POINT('Ctrl Pts',(-22.5356508064631,12.4291610555867,
130.271854319525)) ;
#141537 = CARTESIAN_POINT('Ctrl Pts',(-22.4422219359673,12.5152749819563,
130.032078417929)) ;
#141538 = CARTESIAN_POINT('Ctrl Pts',(-22.3590404214073,12.6672522728085,
129.822327141258)) ;
#141539 = CARTESIAN_POINT('Ctrl Pts',(-22.2921309701618,12.8714563958125,
129.659787658127)) ;
#141540 = CARTESIAN_POINT('Ctrl Pts',(-22.2443651596895,13.1164156857726,
129.553405831915)) ;
#141541 = CARTESIAN_POINT('Ctrl Pts',(-22.2190474781447,13.3833143982509,
129.512577304851)) ;
#141542 = CARTESIAN_POINT('Ctrl Pts',(-22.2172540043482,13.6536761836367,
129.540554196584)) ;
#141543 = CARTESIAN_POINT('Ctrl Pts',(-22.2382590501835,13.9063303712051,
129.634966454425)) ;
#141544 = CARTESIAN_POINT('Ctrl Pts',(-22.2801563660598,14.1256565234766,
129.790623681986)) ;
#141545 = CARTESIAN_POINT('Ctrl Pts',(-22.3384585173566,14.2929703987116,
129.993882288025)) ;
#141546 = CARTESIAN_POINT('Ctrl Pts',(-22.4093200906847,14.3994043098715,
130.2341478642)) ;
#141547 = CARTESIAN_POINT('Ctrl Pts',(-22.4859751155258,14.4351253202518,
130.491131868344)) ;
#141548 = CARTESIAN_POINT('Ctrl Pts',(-22.5626631024897,14.3988243976867,
130.748241624642)) ;
#141549 = CARTESIAN_POINT('Ctrl Pts',(-22.6332742180642,14.2923293350233,
130.987677581832)) ;
#141550 = CARTESIAN_POINT('Ctrl Pts',(-22.6916546156017,14.1241731198379,
131.191265009288)) ;
#141551 = CARTESIAN_POINT('Ctrl Pts',(-22.7333193090981,13.9051613921294,
131.346148949701)) ;
#141552 = CARTESIAN_POINT('Ctrl Pts',(-22.754233227271,13.6518311296983,131.440367694437)) ;
#141553 = CARTESIAN_POINT('Ctrl Pts',(-22.7523181442158,13.382470855745,131.467858526285)) ;
#141554 = CARTESIAN_POINT('Ctrl Pts',(-22.7269194037075,13.1154253093326,
131.426820533837)) ;
#141555 = CARTESIAN_POINT('Ctrl Pts',(-22.6790960766581,12.870532627165,131.320267211323)) ;
#141556 = CARTESIAN_POINT('Ctrl Pts',(-22.6116784390235,12.6655370623813,
131.156430120632)) ;
#141557 = CARTESIAN_POINT('Ctrl Pts',(-22.52866080056,12.5146112144562,130.947041423206)) ;
#141558 = CARTESIAN_POINT('Ctrl Pts',(-22.4352111334049,12.4289101805898,
130.707203534422)) ;
#141559 = CARTESIAN_POINT('Ctrl Pts',(-22.337805695785,12.414189675376,130.455660644508)) ;
#141560 = CARTESIAN_POINT('Ctrl Pts',(-22.2412613487243,12.4724108843215,
130.206994597826)) ;
#141561 = CARTESIAN_POINT('Ctrl Pts',(-22.1539421150866,12.5978142660017,
129.984853113308)) ;
#141562 = CARTESIAN_POINT('Ctrl Pts',(-22.0796465742663,12.7826552616513,
129.800950294926)) ;
#141563 = CARTESIAN_POINT('Ctrl Pts',(-22.023580811912,13.0133815728599,129.670279883198)) ;
#141564 = CARTESIAN_POINT('Ctrl Pts',(-21.9889019749618,13.2742169731993,
129.602185597382)) ;
#141565 = CARTESIAN_POINT('Ctrl Pts',(-21.9776007628016,13.5450315924184,
129.602290461137)) ;
#141566 = CARTESIAN_POINT('Ctrl Pts',(-21.9895371136341,13.8067212996898,
129.670228891093)) ;
#141567 = CARTESIAN_POINT('Ctrl Pts',(-22.0231669037331,14.041251387199,129.801572991707)) ;
#141568 = CARTESIAN_POINT('Ctrl Pts',(-22.0754464617893,14.2318697837458,
129.987445935215)) ;
#141569 = CARTESIAN_POINT('Ctrl Pts',(-22.1420538141681,14.3645253457052,
130.215247583402)) ;
#141570 = CARTESIAN_POINT('Ctrl Pts',(-22.2167456177527,14.4291513856489,
130.466420736451)) ;
#141571 = CARTESIAN_POINT('Ctrl Pts',(-22.2943374241322,14.4223448074479,
130.72622892334)) ;
#141572 = CARTESIAN_POINT('Ctrl Pts',(-22.3683124218705,14.3433927947591,
130.975537803221)) ;
#141573 = CARTESIAN_POINT('Ctrl Pts',(-22.4321443929052,14.1993296986607,
131.195019796695)) ;
#141574 = CARTESIAN_POINT('Ctrl Pts',(-22.4812301514825,13.9988089965648,
131.37161097718)) ;
#141575 = CARTESIAN_POINT('Ctrl Pts',(-22.5108552207397,13.7578101300497,
131.491222506074)) ;
#141576 = CARTESIAN_POINT('Ctrl Pts',(-22.5183507639506,13.4916490682303,
131.546347903552)) ;
#141577 = CARTESIAN_POINT('Ctrl Pts',(-22.5024688288655,13.2223242995655,
131.532955842147)) ;
#141578 = CARTESIAN_POINT('Ctrl Pts',(-22.4634550439045,12.9657468504133,
131.452199654102)) ;
#141579 = CARTESIAN_POINT('Ctrl Pts',(-22.4035858370445,12.7429296521264,
131.310396045604)) ;
#141580 = CARTESIAN_POINT('Ctrl Pts',(-22.3264011259672,12.5685157086448,
131.118018720655)) ;
#141581 = CARTESIAN_POINT('Ctrl Pts',(-22.2361039633969,12.4549912632195,
130.887515775926)) ;
#141582 = CARTESIAN_POINT('Ctrl Pts',(-22.1398503506461,12.4115665136302,
130.639293430357)) ;
#141583 = CARTESIAN_POINT('Ctrl Pts',(-22.0424886926386,12.4399153720153,
130.387988889265)) ;
#141584 = CARTESIAN_POINT('Ctrl Pts',(-21.9504297608399,12.5392662733084,
130.152276377526)) ;
#141585 = CARTESIAN_POINT('Ctrl Pts',(-21.8701710273988,12.7015765304021,
129.950908606138)) ;
#141586 = CARTESIAN_POINT('Ctrl Pts',(-21.8063861498009,12.9151235302472,
129.79762998674)) ;
#141587 = CARTESIAN_POINT('Ctrl Pts',(-21.7626992958939,13.1655123638567,
129.7031400661)) ;
#141588 = CARTESIAN_POINT('Ctrl Pts',(-21.7417530497949,13.4357073085102,
129.675239571074)) ;
#141589 = CARTESIAN_POINT('Ctrl Pts',(-21.7444138523188,13.7027427406616,
129.716020384392)) ;
#141590 = CARTESIAN_POINT('Ctrl Pts',(-21.7694841131605,13.9504288317899,
129.822336426841)) ;
#141591 = CARTESIAN_POINT('Ctrl Pts',(-21.8147174623756,14.1608971109305,
129.987638494224)) ;
#141592 = CARTESIAN_POINT('Ctrl Pts',(-21.8759731008052,14.3182076735822,
130.199701107976)) ;
#141593 = CARTESIAN_POINT('Ctrl Pts',(-21.94820436243,14.4114239786406,130.443837263751)) ;
#141594 = CARTESIAN_POINT('Ctrl Pts',(-22.0253654620152,14.4338711414245,
130.702320259921)) ;
#141595 = CARTESIAN_POINT('Ctrl Pts',(-22.101528389536,14.3839736196214,130.957971280896)) ;
#141596 = CARTESIAN_POINT('Ctrl Pts',(-22.1703041063366,14.2649033535115,
131.192056246532)) ;
#141597 = CARTESIAN_POINT('Ctrl Pts',(-22.2258355288632,14.0862372824977,
131.387321343928)) ;
#141598 = CARTESIAN_POINT('Ctrl Pts',(-22.2638301112426,13.8593709017047,
131.531485753709)) ;
#141599 = CARTESIAN_POINT('Ctrl Pts',(-22.2805485096342,13.6016401376878,
131.613431621248)) ;
#141600 = CARTESIAN_POINT('Ctrl Pts',(-22.2741762775947,13.3309240386314,
131.627952992157)) ;
#141601 = CARTESIAN_POINT('Ctrl Pts',(-22.2444251317103,13.0670232558749,
131.574151442485)) ;
#141602 = CARTESIAN_POINT('Ctrl Pts',(-22.1927412324025,12.828626100883,131.456273734189)) ;
#141603 = CARTESIAN_POINT('Ctrl Pts',(-22.1219393925841,12.6324568485675,
131.282604017312)) ;
#141604 = CARTESIAN_POINT('Ctrl Pts',(-22.0364918031217,12.4932133187338,
131.066128009462)) ;
#141605 = CARTESIAN_POINT('Ctrl Pts',(-21.9420804492648,12.4206918000049,
130.823366652621)) ;
#141606 = CARTESIAN_POINT('Ctrl Pts',(-21.8440805767233,12.4196226873693,
130.57024775875)) ;
#141607 = CARTESIAN_POINT('Ctrl Pts',(-21.7490173808445,12.491015534073,130.325762328134)) ;
#141608 = CARTESIAN_POINT('Ctrl Pts',(-21.6636415900144,12.6283740411058,
130.109366250709)) ;
#141609 = CARTESIAN_POINT('Ctrl Pts',(-21.5922515959559,12.8237070115403,
129.934053660651)) ;
#141610 = CARTESIAN_POINT('Ctrl Pts',(-21.5401084835492,13.061674988434,129.814868123476)) ;
#141611 = CARTESIAN_POINT('Ctrl Pts',(-21.509952988586,13.32403831549,129.759742423784)) ;
#141612 = CARTESIAN_POINT('Ctrl Pts',(-21.5029347827011,13.5952494532198,
129.772427265086)) ;
#141613 = CARTESIAN_POINT('Ctrl Pts',(-21.5192500283624,13.8544595639362,
129.853324509009)) ;
#141614 = CARTESIAN_POINT('Ctrl Pts',(-21.5567750983994,14.0816540138682,
129.996049680023)) ;
#141615 = CARTESIAN_POINT('Ctrl Pts',(-21.6118539418553,14.2612880227879,
130.189940873468)) ;
#141616 = CARTESIAN_POINT('Ctrl Pts',(-21.6802614176699,14.3817634541805,
130.422897734711)) ;
#141617 = CARTESIAN_POINT('Ctrl Pts',(-21.7564021182027,14.4336477376616,
130.678521217963)) ;
#141618 = CARTESIAN_POINT('Ctrl Pts',(-21.8339810050049,14.4124733819028,
130.938391467335)) ;
#141619 = CARTESIAN_POINT('Ctrl Pts',(-21.9058535221447,14.3214777204803,
131.181230646715)) ;
#141620 = CARTESIAN_POINT('Ctrl Pts',(-21.9677099575383,14.1652192318908,
131.39517300608)) ;
#141621 = CARTESIAN_POINT('Ctrl Pts',(-22.0133194373746,13.955565015999,131.56158746004)) ;
#141622 = CARTESIAN_POINT('Ctrl Pts',(-22.0388748975272,13.709559951643,131.669199572757)) ;
#141623 = CARTESIAN_POINT('Ctrl Pts',(-22.0420741504065,13.4405995053874,
131.711821411861)) ;
#141624 = CARTESIAN_POINT('Ctrl Pts',(-22.0216068001038,13.1715077449996,
131.685166293291)) ;
#141625 = CARTESIAN_POINT('Ctrl Pts',(-21.9787370922207,12.9214880577471,
131.592913543069)) ;
#141626 = CARTESIAN_POINT('Ctrl Pts',(-21.9150051439039,12.7055052948916,
131.439997533155)) ;
#141627 = CARTESIAN_POINT('Ctrl Pts',(-21.8352330897024,12.5425196624815,
131.239962285351)) ;
#141628 = CARTESIAN_POINT('Ctrl Pts',(-21.7437059672795,12.4416160232308,
131.005700049378)) ;
#141629 = CARTESIAN_POINT('Ctrl Pts',(-21.6457837150915,12.4112449643292,
130.752967238567)) ;
#141630 = CARTESIAN_POINT('Ctrl Pts',(-21.5491572309789,12.4537097251659,
130.503762395268)) ;
#141631 = CARTESIAN_POINT('Ctrl Pts',(-21.4592496415054,12.5652232898652,
130.274186604649)) ;
#141632 = CARTESIAN_POINT('Ctrl Pts',(-21.3817509969093,12.7379440423451,
130.080854279824)) ;
#141633 = CARTESIAN_POINT('Ctrl Pts',(-21.3213005288273,12.9603974854775,
129.93743655005)) ;
#141634 = CARTESIAN_POINT('Ctrl Pts',(-21.2818676200916,13.2156635264027,
129.855358038676)) ;
#141635 = CARTESIAN_POINT('Ctrl Pts',(-21.2653674335359,13.4857934304202,
129.840276750867)) ;
#141636 = CARTESIAN_POINT('Ctrl Pts',(-21.2723658021236,13.7522947042676,
129.893946458855)) ;
#141637 = CARTESIAN_POINT('Ctrl Pts',(-21.3016583192635,13.9943545056691,
130.012656591767)) ;
#141638 = CARTESIAN_POINT('Ctrl Pts',(-21.3499698414391,14.1947046686213,
130.186750048278)) ;
#141639 = CARTESIAN_POINT('Ctrl Pts',(-21.4140663653601,14.341452975733,130.407297870891)) ;
#141640 = CARTESIAN_POINT('Ctrl Pts',(-21.4875277289265,14.4211243225131,
130.654924218185)) ;
#141641 = CARTESIAN_POINT('Ctrl Pts',(-21.5648853083263,14.4300014254347,
130.913958649016)) ;
#141642 = CARTESIAN_POINT('Ctrl Pts',(-21.6402056432869,14.3664765373256,
131.167191277808)) ;
#141643 = CARTESIAN_POINT('Ctrl Pts',(-21.7067619878926,14.2356051810154,
131.394704769089)) ;
#141644 = CARTESIAN_POINT('Ctrl Pts',(-21.7594400160825,14.0463420011333,
131.581735837121)) ;
#141645 = CARTESIAN_POINT('Ctrl Pts',(-21.7935313335368,13.8127311118514,
131.714417517825)) ;
#141646 = CARTESIAN_POINT('Ctrl Pts',(-21.8060449730169,13.5514860506215,
131.784043231233)) ;
#141647 = CARTESIAN_POINT('Ctrl Pts',(-21.7951988407191,13.2797430818136,
131.785591184551)) ;
#141648 = CARTESIAN_POINT('Ctrl Pts',(-21.7611775488476,13.0196140734991,
131.719268505353)) ;
#141649 = CARTESIAN_POINT('Ctrl Pts',(-21.7055614368075,12.7876901355889,
131.589951267005)) ;
#141650 = CARTESIAN_POINT('Ctrl Pts',(-21.6316783355603,12.6015317076786,
131.407244042403)) ;
#141651 = CARTESIAN_POINT('Ctrl Pts',(-21.5441542981735,12.474259722316,131.18466789139)) ;
#141652 = CARTESIAN_POINT('Ctrl Pts',(-21.4483951831579,12.41484596922,130.9380604683)) ;
#141653 = CARTESIAN_POINT('Ctrl Pts',(-21.3505626518937,12.4277168198839,
130.685407749088)) ;
#141654 = CARTESIAN_POINT('Ctrl Pts',(-21.257021209583,12.511951186466,130.44527777759)) ;
#141655 = CARTESIAN_POINT('Ctrl Pts',(-21.1737647731563,12.6612551341691,
130.235160872959)) ;
#141656 = CARTESIAN_POINT('Ctrl Pts',(-21.1058496345299,12.8654798246469,
130.069918745711)) ;
#141657 = CARTESIAN_POINT('Ctrl Pts',(-21.0576927996032,13.1088716253824,
129.962286476496)) ;
#141658 = CARTESIAN_POINT('Ctrl Pts',(-21.0316738007053,13.3752799217244,
129.919402371251)) ;
#141659 = CARTESIAN_POINT('Ctrl Pts',(-21.0291742667073,13.6458120251598,
129.945308637888)) ;
#141660 = CARTESIAN_POINT('Ctrl Pts',(-21.0495914487314,13.8994658312756,
130.03804637563)) ;
#141661 = CARTESIAN_POINT('Ctrl Pts',(-21.0907109338922,14.1192749080617,
130.191292315407)) ;
#141662 = CARTESIAN_POINT('Ctrl Pts',(-21.1488908973672,14.2891803120814,
130.394377389492)) ;
#141663 = CARTESIAN_POINT('Ctrl Pts',(-21.2191618432277,14.3970324954729,
130.632758726818)) ;
#141664 = CARTESIAN_POINT('Ctrl Pts',(-21.2958745043866,14.4351164738745,
130.889987430257)) ;
#141665 = CARTESIAN_POINT('Ctrl Pts',(-21.3725867221997,14.4010787693592,
131.147130087852)) ;
#141666 = CARTESIAN_POINT('Ctrl Pts',(-21.4438617427851,14.2958209261601,
131.388700881301)) ;
#141667 = CARTESIAN_POINT('Ctrl Pts',(-21.5023962179495,14.1296521769512,
131.592620659444)) ;
#141668 = CARTESIAN_POINT('Ctrl Pts',(-21.5446003436252,13.9121761365587,
131.749049810147)) ;
#141669 = CARTESIAN_POINT('Ctrl Pts',(-21.5661428686401,13.6594303450515,
131.845126015287)) ;
#141670 = CARTESIAN_POINT('Ctrl Pts',(-21.56497049185,13.3906473022496,131.874737745289)) ;
#141671 = CARTESIAN_POINT('Ctrl Pts',(-21.5399924692855,13.1215485534994,
131.835149711464)) ;
#141672 = CARTESIAN_POINT('Ctrl Pts',(-21.4930581932203,12.8774994745799,
131.730962916876)) ;
#141673 = CARTESIAN_POINT('Ctrl Pts',(-21.4258817768746,12.6702279287505,
131.567977187413)) ;
#141674 = CARTESIAN_POINT('Ctrl Pts',(-21.3435607012276,12.5183910310168,
131.360480560169)) ;
#141675 = CARTESIAN_POINT('Ctrl Pts',(-21.2503256342203,12.4302683036152,
131.121283015252)) ;
#141676 = CARTESIAN_POINT('Ctrl Pts',(-21.1522563402183,12.4138255898749,
130.868039774348)) ;
#141677 = CARTESIAN_POINT('Ctrl Pts',(-21.0567790567561,12.4692849906945,
130.622070654961)) ;
#141678 = CARTESIAN_POINT('Ctrl Pts',(-20.9685110583371,12.593086865603,130.397368234412)) ;
#141679 = CARTESIAN_POINT('Ctrl Pts',(-20.8936229110052,12.7771359957172,
130.211819511284)) ;
#141680 = CARTESIAN_POINT('Ctrl Pts',(-20.8371932849537,13.0059650352549,
130.079970640227)) ;
#141681 = CARTESIAN_POINT('Ctrl Pts',(-20.8018184496472,13.2661472489738,
130.009842797586)) ;
#141682 = CARTESIAN_POINT('Ctrl Pts',(-20.7897983193479,13.5369907136561,
130.007852540205)) ;
#141683 = CARTESIAN_POINT('Ctrl Pts',(-20.8011200549456,13.7997449792612,
130.074069304931)) ;
#141684 = CARTESIAN_POINT('Ctrl Pts',(-20.8341135563802,14.0350784316614,
130.20351194695)) ;
#141685 = CARTESIAN_POINT('Ctrl Pts',(-20.8861785126658,14.2276701569779,
130.388889073528)) ;
#141686 = CARTESIAN_POINT('Ctrl Pts',(-20.9518178159271,14.3610391391533,
130.613550792557)) ;
#141687 = CARTESIAN_POINT('Ctrl Pts',(-21.0269503603294,14.4285213682471,
130.866293340862)) ;
#141688 = CARTESIAN_POINT('Ctrl Pts',(-21.1043928575752,14.4233691347863,
131.125594261652)) ;
#141689 = CARTESIAN_POINT('Ctrl Pts',(-21.1783654730741,14.3469900200021,
131.374791937787)) ;
#141690 = CARTESIAN_POINT('Ctrl Pts',(-21.2429999211689,14.2034039230656,
131.596873955724)) ;
#141691 = CARTESIAN_POINT('Ctrl Pts',(-21.2921913933265,14.0056847317555,
131.773520365113)) ;
#141692 = CARTESIAN_POINT('Ctrl Pts',(-21.3225583436973,13.7644934618712,
131.895469292107)) ;
#141693 = CARTESIAN_POINT('Ctrl Pts',(-21.3307101633366,13.5002463021735,
131.952315969993)) ;
#141694 = CARTESIAN_POINT('Ctrl Pts',(-21.3152981248906,13.2284057614088,
131.940601853759)) ;
#141695 = CARTESIAN_POINT('Ctrl Pts',(-21.2772947936541,12.9739037003026,
131.862437607203)) ;
#141696 = CARTESIAN_POINT('Ctrl Pts',(-21.2177347936152,12.7484703827135,
131.721732709268)) ;
#141697 = CARTESIAN_POINT('Ctrl Pts',(-21.1412095546896,12.5731123065293,
131.531169542656)) ;
#141698 = CARTESIAN_POINT('Ctrl Pts',(-21.0511537422027,12.4573590720307,
131.301405138449)) ;
#141699 = CARTESIAN_POINT('Ctrl Pts',(-20.9549127769704,12.4118025437708,
131.053250585454)) ;
#141700 = CARTESIAN_POINT('Ctrl Pts',(-20.8574614565724,12.4381298316287,
130.80169464533)) ;
#141701 = CARTESIAN_POINT('Ctrl Pts',(-20.7653175667387,12.5352056674708,
130.565667200803)) ;
#141702 = CARTESIAN_POINT('Ctrl Pts',(-20.6844201407059,12.6963006126537,
130.362534236826)) ;
#141703 = CARTESIAN_POINT('Ctrl Pts',(-20.6201460569402,12.9082756109017,
130.207782417921)) ;
#141704 = CARTESIAN_POINT('Ctrl Pts',(-20.5756916195102,13.1596325292673,
130.111270821457)) ;
#141705 = CARTESIAN_POINT('Ctrl Pts',(-20.5543454783755,13.4259468803236,
130.08175038831)) ;
#141706 = CARTESIAN_POINT('Ctrl Pts',(-20.5561837783325,13.6953761001562,
130.120387060139)) ;
#141707 = CARTESIAN_POINT('Ctrl Pts',(-20.5806872762992,13.943717027651,130.225025251255)) ;
#141708 = CARTESIAN_POINT('Ctrl Pts',(-20.625436887015,14.1557110892649,130.388952831254)) ;
#141709 = CARTESIAN_POINT('Ctrl Pts',(-20.6861966494772,14.3144000289701,
130.599504747278)) ;
#141710 = CARTESIAN_POINT('Ctrl Pts',(-20.7581576601897,14.4096307928531,
130.842844416002)) ;
#141711 = CARTESIAN_POINT('Ctrl Pts',(-20.8352840260227,14.4343455409311,
131.10123283597)) ;
#141712 = CARTESIAN_POINT('Ctrl Pts',(-20.9118812127441,14.3860725213322,
131.358298311597)) ;
#141713 = CARTESIAN_POINT('Ctrl Pts',(-20.9805602529552,14.269509697164,131.591910200073)) ;
#141714 = CARTESIAN_POINT('Ctrl Pts',(-21.0367672235713,14.0917907400684,
131.789281437755)) ;
#141715 = CARTESIAN_POINT('Ctrl Pts',(-21.0751892066154,13.8666926815631,
131.934591885575)) ;
#141716 = CARTESIAN_POINT('Ctrl Pts',(-21.0926069855701,13.6093228235484,
132.01862592531)) ;
#141717 = CARTESIAN_POINT('Ctrl Pts',(-21.0869107246577,13.3388431242067,
132.035103126594)) ;
#141718 = CARTESIAN_POINT('Ctrl Pts',(-21.0577918123157,13.0740473551912,
131.983200390998)) ;
#141719 = CARTESIAN_POINT('Ctrl Pts',(-21.0065423484218,12.834394570963,131.86664775222)) ;
#141720 = CARTESIAN_POINT('Ctrl Pts',(-20.9365832563614,12.6378258855697,
131.695270728272)) ;
#141721 = CARTESIAN_POINT('Ctrl Pts',(-20.851496423393,12.4964629704439,131.479866074815)) ;
#141722 = CARTESIAN_POINT('Ctrl Pts',(-20.7570110239039,12.4217253903026,
131.236976112388)) ;
#141723 = CARTESIAN_POINT('Ctrl Pts',(-20.6591190008919,12.4187226329277,
130.984139850466)) ;
#141724 = CARTESIAN_POINT('Ctrl Pts',(-20.5641946923653,12.4875916931866,
130.739941516333)) ;
#141725 = CARTESIAN_POINT('Ctrl Pts',(-20.4781247909421,12.6235712974209,
130.521647673819)) ;
#141726 = CARTESIAN_POINT('Ctrl Pts',(-20.4065158080652,12.8167008380917,
130.34556952621)) ;
#141727 = CARTESIAN_POINT('Ctrl Pts',(-20.353643746356,13.053470182096,130.224259441503)) ;
#141728 = CARTESIAN_POINT('Ctrl Pts',(-20.3226739885955,13.3166530721009,
130.166917618502)) ;
#141729 = CARTESIAN_POINT('Ctrl Pts',(-20.31505675572,13.5871782516177,130.177762255202)) ;
#141730 = CARTESIAN_POINT('Ctrl Pts',(-20.3305496502409,13.8461111103248,
130.256130093167)) ;
#141731 = CARTESIAN_POINT('Ctrl Pts',(-20.3675394662945,14.0754123777246,
130.39740594318)) ;
#141732 = CARTESIAN_POINT('Ctrl Pts',(-20.4223028531838,14.2569965796042,
130.590449980248)) ;
#141733 = CARTESIAN_POINT('Ctrl Pts',(-20.4904071207389,14.3792169528627,
130.822514938853)) ;
#141734 = CARTESIAN_POINT('Ctrl Pts',(-20.566188380446,14.4330645797171,131.076992557233)) ;
#141735 = CARTESIAN_POINT('Ctrl Pts',(-20.6438055884923,14.4142942026361,
131.33696737981)) ;
#141736 = CARTESIAN_POINT('Ctrl Pts',(-20.7162101331673,14.3249818434921,
131.581491579565)) ;
#141737 = CARTESIAN_POINT('Ctrl Pts',(-20.7784436604938,14.1700409218133,
131.796566267309)) ;
#141738 = CARTESIAN_POINT('Ctrl Pts',(-20.8243668704006,13.9629928676694,
131.963710597949)) ;
#141739 = CARTESIAN_POINT('Ctrl Pts',(-20.8506930176227,13.7164972263621,
132.073761907779)) ;
#141740 = CARTESIAN_POINT('Ctrl Pts',(-20.8545193223202,13.4493823729498,
132.118023584794)) ;
#141741 = CARTESIAN_POINT('Ctrl Pts',(-20.8348338544616,13.1794660077169,
132.093719529633)) ;
#141742 = CARTESIAN_POINT('Ctrl Pts',(-20.7922850460746,12.9274139547086,
132.002579999831)) ;
#141743 = CARTESIAN_POINT('Ctrl Pts',(-20.7294326898175,12.7115777217288,
131.852035109273)) ;
#141744 = CARTESIAN_POINT('Ctrl Pts',(-20.6500828954979,12.5463884356972,
131.653264061087)) ;
#141745 = CARTESIAN_POINT('Ctrl Pts',(-20.5580314056843,12.443178693002,131.417734074908)) ;
#141746 = CARTESIAN_POINT('Ctrl Pts',(-20.4612577062668,12.4112124572602,
131.167987088684)) ;
#141747 = CARTESIAN_POINT('Ctrl Pts',(-20.3641429989321,12.4513454619086,
130.917486650805)) ;
#141748 = CARTESIAN_POINT('Ctrl Pts',(-20.2739798213262,12.5610016946322,
130.68715458049)) ;
#141749 = CARTESIAN_POINT('Ctrl Pts',(-20.1959506857722,12.732231543376,130.492309746088)) ;
#141750 = CARTESIAN_POINT('Ctrl Pts',(-20.1349366415907,12.9536822141676,
130.347265673142)) ;
#141751 = CARTESIAN_POINT('Ctrl Pts',(-20.0949452207664,13.2077095887355,
130.263487892895)) ;
#141752 = CARTESIAN_POINT('Ctrl Pts',(-20.0777170362633,13.4778390375596,
130.246299373488)) ;
#141753 = CARTESIAN_POINT('Ctrl Pts',(-20.0840738202005,13.7447250723396,
130.298098443837)) ;
#141754 = CARTESIAN_POINT('Ctrl Pts',(-20.1125804674209,13.9871379837623,
130.414408057966)) ;
#141755 = CARTESIAN_POINT('Ctrl Pts',(-20.1607218878349,14.1900737145365,
130.588221394981)) ;
#141756 = CARTESIAN_POINT('Ctrl Pts',(-20.2238417477086,14.3373318040479,
130.805602937382)) ;
#141757 = CARTESIAN_POINT('Ctrl Pts',(-20.2975436467262,14.419933546752,131.054158219114)) ;
#141758 = CARTESIAN_POINT('Ctrl Pts',(-20.3748646623211,14.4307823852778,
131.313069914816)) ;
#141759 = CARTESIAN_POINT('Ctrl Pts',(-20.4505258413519,14.3690285004678,
131.567389143133)) ;
#141760 = CARTESIAN_POINT('Ctrl Pts',(-20.5171200124224,14.2404409367686,
131.794874654969)) ;
#141761 = CARTESIAN_POINT('Ctrl Pts',(-20.5703141964463,14.0528075419849,
131.983419808591)) ;
#141762 = CARTESIAN_POINT('Ctrl Pts',(-20.6050441603483,13.8202654365076,
132.117973841072)) ;
#141763 = CARTESIAN_POINT('Ctrl Pts',(-20.618242473377,13.5584443869878,132.189739585417)) ;
#141764 = CARTESIAN_POINT('Ctrl Pts',(-20.6079944099217,13.2871049531719,
132.19298418131)) ;
#141765 = CARTESIAN_POINT('Ctrl Pts',(-20.5747375359983,13.0271135604128,
132.128804556313)) ;
#141766 = CARTESIAN_POINT('Ctrl Pts',(-20.519668667754,12.7938647144907,132.001118490825)) ;
#141767 = CARTESIAN_POINT('Ctrl Pts',(-20.4463534609398,12.6063347659711,
131.820031027545)) ;
#141768 = CARTESIAN_POINT('Ctrl Pts',(-20.3590134924532,12.4770287601625,
131.598047664409)) ;
#141769 = CARTESIAN_POINT('Ctrl Pts',(-20.2636906192186,12.4155889088205,
131.352615933497)) ;
#141770 = CARTESIAN_POINT('Ctrl Pts',(-20.16538161851,12.4264045930434,131.098726664761)) ;
#141771 = CARTESIAN_POINT('Ctrl Pts',(-20.0719688100384,12.5084013028489,
130.85885015324)) ;
#141772 = CARTESIAN_POINT('Ctrl Pts',(-19.9881652481842,12.6562046151244,
130.647206486187)) ;
#141773 = CARTESIAN_POINT('Ctrl Pts',(-19.9199396779561,12.8582528702238,
130.48094000311)) ;
#141774 = CARTESIAN_POINT('Ctrl Pts',(-19.8708223545684,13.10224809555,130.370716051289)) ;
#141775 = CARTESIAN_POINT('Ctrl Pts',(-19.8442937835913,13.3685511856617,
130.326365144569)) ;
#141776 = CARTESIAN_POINT('Ctrl Pts',(-19.8411260523443,13.6374690862059,
130.350100513771)) ;
#141777 = CARTESIAN_POINT('Ctrl Pts',(-19.86090775583,13.8926337693761,130.441079325237)) ;
#141778 = CARTESIAN_POINT('Ctrl Pts',(-19.9014600976165,14.1134974060216,
130.592644036844)) ;
#141779 = CARTESIAN_POINT('Ctrl Pts',(-19.9593667313595,14.2854804589728,
130.795017810507)) ;
#141780 = CARTESIAN_POINT('Ctrl Pts',(-20.0293912566406,14.394916969494,131.03267442462)) ;
#141781 = CARTESIAN_POINT('Ctrl Pts',(-20.1056792081533,14.435095047054,131.288519546508)) ;
#141782 = CARTESIAN_POINT('Ctrl Pts',(-20.1829120670562,14.4027523560096,
131.547383866018)) ;
#141783 = CARTESIAN_POINT('Ctrl Pts',(-20.2538480508494,14.3004224301193,
131.787669615841)) ;
#141784 = CARTESIAN_POINT('Ctrl Pts',(-20.3133527497641,14.1345848207203,
131.994721949967)) ;
#141785 = CARTESIAN_POINT('Ctrl Pts',(-20.355864409434,13.9188292654447,132.15193646137)) ;
#141786 = CARTESIAN_POINT('Ctrl Pts',(-20.378071179084,13.6668968226668,132.249955352682)) ;
#141787 = CARTESIAN_POINT('Ctrl Pts',(-20.3775079318251,13.3982258049414,
132.281358615002)) ;
#141788 = CARTESIAN_POINT('Ctrl Pts',(-20.3533777867425,13.1299459818543,
132.24409760961)) ;
#141789 = CARTESIAN_POINT('Ctrl Pts',(-20.3068511976437,12.8837060048702,
132.141274285562)) ;
#141790 = CARTESIAN_POINT('Ctrl Pts',(-20.240261347845,12.6755091037675,131.979947404298)) ;
#141791 = CARTESIAN_POINT('Ctrl Pts',(-20.1581680238177,12.5215778341602,
131.773182076307)) ;
#141792 = CARTESIAN_POINT('Ctrl Pts',(-20.0649675040375,12.4317802078497,
131.534139059742)) ;
#141793 = CARTESIAN_POINT('Ctrl Pts',(-19.9677911498579,12.4131805145463,
131.283214057728)) ;
#141794 = CARTESIAN_POINT('Ctrl Pts',(-19.8713977553643,12.4668842843224,
131.034839990203)) ;
#141795 = CARTESIAN_POINT('Ctrl Pts',(-19.7832398695149,12.5884450791791,
130.810305644908)) ;
#141796 = CARTESIAN_POINT('Ctrl Pts',(-19.7076706234563,12.7713421564293,
130.62286138056)) ;
#141797 = CARTESIAN_POINT('Ctrl Pts',(-19.650734391685,12.9988618767288,130.489494578148)) ;
#141798 = CARTESIAN_POINT('Ctrl Pts',(-19.6146315035451,13.259491403766,130.417371328723)) ;
#141799 = CARTESIAN_POINT('Ctrl Pts',(-19.602066610751,13.5289134128762,130.413620138675)) ;
#141800 = CARTESIAN_POINT('Ctrl Pts',(-19.6126420557654,13.792044854945,130.477635491383)) ;
#141801 = CARTESIAN_POINT('Ctrl Pts',(-19.6450752325787,14.0286824176204,
130.605479576481)) ;
#141802 = CARTESIAN_POINT('Ctrl Pts',(-19.6965636088298,14.2226477736602,
130.789131633615)) ;
#141803 = CARTESIAN_POINT('Ctrl Pts',(-19.7620620684361,14.3581280459106,
131.013479763775)) ;
#141804 = CARTESIAN_POINT('Ctrl Pts',(-19.8366555625925,14.4275172368953,
131.264485219799)) ;
#141805 = CARTESIAN_POINT('Ctrl Pts',(-19.914713017642,14.4244373227483,131.525845240593)) ;
#141806 = CARTESIAN_POINT('Ctrl Pts',(-19.9884493193164,14.3501367823951,
131.77417324445)) ;
#141807 = CARTESIAN_POINT('Ctrl Pts',(-20.0533520936969,14.2089997399679,
131.99696494782)) ;
#141808 = CARTESIAN_POINT('Ctrl Pts',(-20.1032372720437,14.0121250451069,
132.17574893776)) ;
#141809 = CARTESIAN_POINT('Ctrl Pts',(-20.1342125776709,13.7718246711113,
132.299481752515)) ;
#141810 = CARTESIAN_POINT('Ctrl Pts',(-20.1429809167067,13.5078186231509,
132.358155687099)) ;
#141811 = CARTESIAN_POINT('Ctrl Pts',(-20.1284039868733,13.2372789127591,
132.348703112449)) ;
#141812 = CARTESIAN_POINT('Ctrl Pts',(-20.0908625978491,12.980432676453,132.272099446344)) ;
#141813 = CARTESIAN_POINT('Ctrl Pts',(-20.0318009855664,12.7540238473754,
132.132840514117)) ;
#141814 = CARTESIAN_POINT('Ctrl Pts',(-19.9558387140201,12.5774627214212,
131.943866603019)) ;
#141815 = CARTESIAN_POINT('Ctrl Pts',(-19.8662835104376,12.4598742845048,
131.715495634813)) ;
#141816 = CARTESIAN_POINT('Ctrl Pts',(-19.7697256841548,12.4120040771025,
131.466564374263)) ;
#141817 = CARTESIAN_POINT('Ctrl Pts',(-19.6722699667815,12.4365719363613,
131.21497904264)) ;
#141818 = CARTESIAN_POINT('Ctrl Pts',(-19.5802613105046,12.5311793730478,
130.979208437368)) ;
#141819 = CARTESIAN_POINT('Ctrl Pts',(-19.4986531494467,12.6910252991536,
130.774112825828)) ;
#141820 = CARTESIAN_POINT('Ctrl Pts',(-19.4340286592284,12.9015546057863,
130.618290378308)) ;
#141821 = CARTESIAN_POINT('Ctrl Pts',(-19.3890411033215,13.1503193802668,
130.520011015745)) ;
#141822 = CARTESIAN_POINT('Ctrl Pts',(-19.3667781285979,13.4198238149612,
130.488246338711)) ;
#141823 = CARTESIAN_POINT('Ctrl Pts',(-19.3679978219409,13.6867201832379,
130.524721757099)) ;
#141824 = CARTESIAN_POINT('Ctrl Pts',(-19.3919557160883,13.9376559863072,
130.62799833703)) ;
#141825 = CARTESIAN_POINT('Ctrl Pts',(-19.4361283002266,14.1502428615257,
130.790145849377)) ;
#141826 = CARTESIAN_POINT('Ctrl Pts',(-19.4965493043583,14.3108380697217,
130.999753103418)) ;
#141827 = CARTESIAN_POINT('Ctrl Pts',(-19.568262071274,14.4079445348436,131.242354028825)) ;
#141828 = CARTESIAN_POINT('Ctrl Pts',(-19.6454042775569,14.4345276706247,
131.500826737002)) ;
#141829 = CARTESIAN_POINT('Ctrl Pts',(-19.7216080873504,14.3888298731307,
131.756512645757)) ;
#141830 = CARTESIAN_POINT('Ctrl Pts',(-19.7909620886184,14.273828468375,131.992266951157)) ;
#141831 = CARTESIAN_POINT('Ctrl Pts',(-19.8475410580093,14.0978368302853,
132.190684651942)) ;
#141832 = CARTESIAN_POINT('Ctrl Pts',(-19.8866080882812,13.8735407233332,
132.337940805145)) ;
#141833 = CARTESIAN_POINT('Ctrl Pts',(-19.9046387879488,13.6168750178338,
132.423754270832)) ;
#141834 = CARTESIAN_POINT('Ctrl Pts',(-19.8996055461185,13.346506361492,132.4421704395)) ;
#141835 = CARTESIAN_POINT('Ctrl Pts',(-19.8711825635662,13.0815407666398,
132.392264377035)) ;
#141836 = CARTESIAN_POINT('Ctrl Pts',(-19.8205474898722,12.8409646602013,
132.277503248563)) ;
#141837 = CARTESIAN_POINT('Ctrl Pts',(-19.7511694006213,12.6428639918128,
132.107805469433)) ;
#141838 = CARTESIAN_POINT('Ctrl Pts',(-19.6657363050394,12.4989646430065,
131.891643331655)) ;
#141839 = CARTESIAN_POINT('Ctrl Pts',(-19.5722878839265,12.4231076853541,
131.651474151143)) ;
#141840 = CARTESIAN_POINT('Ctrl Pts',(-19.4740246524998,12.4177381591252,
131.397689125236)) ;
#141841 = CARTESIAN_POINT('Ctrl Pts',(-19.3789969152326,12.4847095466627,
131.153165024408)) ;
#141842 = CARTESIAN_POINT('Ctrl Pts',(-19.2924935792413,12.6190668251906,
130.933646272935)) ;
#141843 = CARTESIAN_POINT('Ctrl Pts',(-19.2204813399372,12.8107471895688,
130.756372046187)) ;
#141844 = CARTESIAN_POINT('Ctrl Pts',(-19.1671050807076,13.0461049078406,
130.633535559335)) ;
#141845 = CARTESIAN_POINT('Ctrl Pts',(-19.1354518923136,13.3089104890012,
130.574215108908)) ;
#141846 = CARTESIAN_POINT('Ctrl Pts',(-19.1271492497169,13.5795918474296,
130.583068460063)) ;
#141847 = CARTESIAN_POINT('Ctrl Pts',(-19.1420823786064,13.8398549511919,
130.659898097872)) ;
#141848 = CARTESIAN_POINT('Ctrl Pts',(-19.1785538930754,14.0698649783882,
130.79962783888)) ;
#141849 = CARTESIAN_POINT('Ctrl Pts',(-19.2326864141405,14.2524396498396,
130.990725985703)) ;
#141850 = CARTESIAN_POINT('Ctrl Pts',(-19.3006476101395,14.3767943288433,
131.222452811304)) ;
#141851 = CARTESIAN_POINT('Ctrl Pts',(-19.37610451377,14.4324209617662,131.475897601322)) ;
#141852 = CARTESIAN_POINT('Ctrl Pts',(-19.4536998093068,14.4159981078524,
131.735777838716)) ;
#141853 = CARTESIAN_POINT('Ctrl Pts',(-19.5265608664841,14.3283155075796,
131.981745823597)) ;
#141854 = CARTESIAN_POINT('Ctrl Pts',(-19.5889643403077,14.1755658927935,
132.197206943075)) ;
#141855 = CARTESIAN_POINT('Ctrl Pts',(-19.6354790586532,13.9699067943466,
132.366095536546)) ;
#141856 = CARTESIAN_POINT('Ctrl Pts',(-19.6624519781793,13.7239839863066,
132.478077716201)) ;
#141857 = CARTESIAN_POINT('Ctrl Pts',(-19.666980954464,13.4571372735282,132.524398080383)) ;
#141858 = CARTESIAN_POINT('Ctrl Pts',(-19.6477861345708,13.1860385080971,
132.501656426746)) ;
#141859 = CARTESIAN_POINT('Ctrl Pts',(-19.6062304044814,12.9351633372793,
132.413151943778)) ;
#141860 = CARTESIAN_POINT('Ctrl Pts',(-19.5434289051781,12.7162804283108,
132.263030237578)) ;
#141861 = CARTESIAN_POINT('Ctrl Pts',(-19.4647999874014,12.5504602978257,
132.066204808384)) ;
#141862 = CARTESIAN_POINT('Ctrl Pts',(-19.3729739339425,12.4451571789981,
131.831357919352)) ;
#141863 = CARTESIAN_POINT('Ctrl Pts',(-19.2764129384417,12.4110818133835,
131.582183020865)) ;
#141864 = CARTESIAN_POINT('Ctrl Pts',(-19.1789058275452,12.4493848627309,
131.330644654867)) ;
#141865 = CARTESIAN_POINT('Ctrl Pts',(-19.0889426594496,12.5564279149636,
131.100712663772)) ;
#141866 = CARTESIAN_POINT('Ctrl Pts',(-19.0099622196206,12.7270948796437,
130.903310128084)) ;
#141867 = CARTESIAN_POINT('Ctrl Pts',(-18.9486581578239,12.9467013560163,
130.757301018768)) ;
#141868 = CARTESIAN_POINT('Ctrl Pts',(-18.9079322965114,13.2005745815833,
130.671455691176)) ;
#141869 = CARTESIAN_POINT('Ctrl Pts',(-18.8901493403744,13.4697556430519,
130.652551582451)) ;
#141870 = CARTESIAN_POINT('Ctrl Pts',(-18.8956759511923,13.736255276326,130.70181545982)) ;
#141871 = CARTESIAN_POINT('Ctrl Pts',(-18.9238215240828,13.9814042376555,
130.817329927107)) ;
#141872 = CARTESIAN_POINT('Ctrl Pts',(-18.9710857402053,14.1841667225104,
130.988318199626)) ;
#141873 = CARTESIAN_POINT('Ctrl Pts',(-19.0342235553262,14.3343212234818,
131.205982310787)) ;
#141874 = CARTESIAN_POINT('Ctrl Pts',(-19.1075024006883,14.4184551255459,
131.453186900697)) ;
#141875 = CARTESIAN_POINT('Ctrl Pts',(-19.1848350711925,14.4314519910157,
131.712158292538)) ;
#141876 = CARTESIAN_POINT('Ctrl Pts',(-19.260343209931,14.3721434966701,131.965889987133)) ;
#141877 = CARTESIAN_POINT('Ctrl Pts',(-19.3275198723999,14.245373795937,132.195174956684)) ;
#141878 = CARTESIAN_POINT('Ctrl Pts',(-19.381396493653,14.0581566175582,132.38587704578)) ;
#141879 = CARTESIAN_POINT('Ctrl Pts',(-19.4164824936223,13.8276967157625,
132.521313395047)) ;
#141880 = CARTESIAN_POINT('Ctrl Pts',(-19.4303957231885,13.5670202701056,
132.595106405332)) ;
#141881 = CARTESIAN_POINT('Ctrl Pts',(-19.4208832730529,13.2953785672156,
132.600537532849)) ;
#141882 = CARTESIAN_POINT('Ctrl Pts',(-19.3882471470235,13.0342213948757,
132.538241764966)) ;
#141883 = CARTESIAN_POINT('Ctrl Pts',(-19.3334906631503,12.799235193231,132.411585913234)) ;
#141884 = CARTESIAN_POINT('Ctrl Pts',(-19.261043051524,12.6113832489784,132.232841060181)) ;
#141885 = CARTESIAN_POINT('Ctrl Pts',(-19.1739879603888,12.4798503572911,
132.011723757091)) ;
#141886 = CARTESIAN_POINT('Ctrl Pts',(-19.0786309591327,12.4163978542697,
131.766255688974)) ;
#141887 = CARTESIAN_POINT('Ctrl Pts',(-18.98062423312,12.4249215089451,131.513135114901)) ;
#141888 = CARTESIAN_POINT('Ctrl Pts',(-18.8865300769159,12.505375632336,131.271441981484)) ;
#141889 = CARTESIAN_POINT('Ctrl Pts',(-18.8027816816541,12.6507859579669,
131.059795433215)) ;
#141890 = CARTESIAN_POINT('Ctrl Pts',(-18.7338552847486,12.8517471604921,
130.891556618689)) ;
#141891 = CARTESIAN_POINT('Ctrl Pts',(-18.6842105366579,13.0945615121704,
130.779753269807)) ;
#141892 = CARTESIAN_POINT('Ctrl Pts',(-18.6569376131211,13.3602126938648,
130.733201043966)) ;
#141893 = CARTESIAN_POINT('Ctrl Pts',(-18.6531415615538,13.6310672418703,
130.755323120175)) ;
#141894 = CARTESIAN_POINT('Ctrl Pts',(-18.6722331473898,13.8852754196112,
130.844076845159)) ;
#141895 = CARTESIAN_POINT('Ctrl Pts',(-18.7122022947617,14.1076160961634,
130.993965145821)) ;
#141896 = CARTESIAN_POINT('Ctrl Pts',(-18.7695522886427,14.2808806775566,
131.194645480041)) ;
#141897 = CARTESIAN_POINT('Ctrl Pts',(-18.83924559398,14.3926567140697,131.431331456996)) ;
#141898 = CARTESIAN_POINT('Ctrl Pts',(-18.9160286047029,14.4348969487797,
131.688881910265)) ;
#141899 = CARTESIAN_POINT('Ctrl Pts',(-18.9926033453051,14.4049966938089,
131.945496008568)) ;
#141900 = CARTESIAN_POINT('Ctrl Pts',(-19.0644452296558,14.3037928879971,
132.188736587752)) ;
#141901 = CARTESIAN_POINT('Ctrl Pts',(-19.1239168662076,14.1405203886364,
132.395461417312)) ;
#141902 = CARTESIAN_POINT('Ctrl Pts',(-19.167107493149,13.9258191090176,132.554726043637)) ;
#141903 = CARTESIAN_POINT('Ctrl Pts',(-19.1899722517165,13.6747404934951,
132.654652849122)) ;
#141904 = CARTESIAN_POINT('Ctrl Pts',(-19.1900075690217,13.4052256661744,
132.687941950443)) ;
#141905 = CARTESIAN_POINT('Ctrl Pts',(-19.166746991383,13.138469239792,132.652983769787)) ;
#141906 = CARTESIAN_POINT('Ctrl Pts',(-19.1205720258971,12.8897551396211,
132.551405771592)) ;
#141907 = CARTESIAN_POINT('Ctrl Pts',(-19.0548239476007,12.6813707794316,
132.392358845986)) ;
#141908 = CARTESIAN_POINT('Ctrl Pts',(-18.9730261476444,12.5252896254052,
132.18651714806)) ;
#141909 = CARTESIAN_POINT('Ctrl Pts',(-18.8802716176398,12.4335761990142,
131.948700699389)) ;
#141910 = CARTESIAN_POINT('Ctrl Pts',(-18.7828229550223,12.4126069682806,
131.697092660579)) ;
#141911 = CARTESIAN_POINT('Ctrl Pts',(-18.6860467767773,12.4645413943428,
131.447685791234)) ;
#141912 = CARTESIAN_POINT('Ctrl Pts',(-18.5976234412375,12.5845283028617,
131.222382340814)) ;
#141913 = CARTESIAN_POINT('Ctrl Pts',(-18.5218504701098,12.7652451622035,
131.034228327474)) ;
#141914 = CARTESIAN_POINT('Ctrl Pts',(-18.4642539071398,12.9922348070079,
130.899013365635)) ;
#141915 = CARTESIAN_POINT('Ctrl Pts',(-18.4277290043019,13.2501819432392,
130.825397364952)) ;
#141916 = CARTESIAN_POINT('Ctrl Pts',(-18.414270152757,13.5208713939763,130.819203355187)) ;
#141917 = CARTESIAN_POINT('Ctrl Pts',(-18.4242664380075,13.7852949674506,
130.881626201884)) ;
#141918 = CARTESIAN_POINT('Ctrl Pts',(-18.4562051880654,14.0230294711121,
131.008056241537)) ;
#141919 = CARTESIAN_POINT('Ctrl Pts',(-18.5071026488867,14.217815504055,131.189893611675)) ;
#141920 = CARTESIAN_POINT('Ctrl Pts',(-18.5722572460804,14.355293096106,131.413244424432)) ;
#141921 = CARTESIAN_POINT('Ctrl Pts',(-18.6470132645676,14.4265292690715,
131.664865103024)) ;
#141922 = CARTESIAN_POINT('Ctrl Pts',(-18.7241791544619,14.4257522115435,
131.923231401887)) ;
#141923 = CARTESIAN_POINT('Ctrl Pts',(-18.798764612649,14.353191154613,132.174331118384)) ;
#141924 = CARTESIAN_POINT('Ctrl Pts',(-18.863847038587,14.2139748477186,132.397566284138)) ;
#141925 = CARTESIAN_POINT('Ctrl Pts',(-18.9143185597732,14.0181342342469,
132.57813709689)) ;
#141926 = CARTESIAN_POINT('Ctrl Pts',(-18.945785649306,13.7796844257176,132.703183210523)) ;
#141927 = CARTESIAN_POINT('Ctrl Pts',(-18.9552755509885,13.515523516605,132.764049213495)) ;
#141928 = CARTESIAN_POINT('Ctrl Pts',(-18.9413798979237,13.2452125858444,
132.756543939979)) ;
#141929 = CARTESIAN_POINT('Ctrl Pts',(-18.9045068472628,12.9877057714763,
132.681894685849)) ;
#141930 = CARTESIAN_POINT('Ctrl Pts',(-18.8460866892425,12.760206013501,132.544485955534)) ;
#141931 = CARTESIAN_POINT('Ctrl Pts',(-18.7704201812073,12.5817512352831,
132.356441887698)) ;
#141932 = CARTESIAN_POINT('Ctrl Pts',(-18.6814549221541,12.4625557335165,
132.129687023167)) ;
#141933 = CARTESIAN_POINT('Ctrl Pts',(-18.5848852819742,12.4124303702056,
131.880776268223)) ;
#141934 = CARTESIAN_POINT('Ctrl Pts',(-18.4875205077328,12.4345388206878,
131.62939372436)) ;
#141935 = CARTESIAN_POINT('Ctrl Pts',(-18.3944792146438,12.5283216628162,
131.390912274721)) ;
#141936 = CARTESIAN_POINT('Ctrl Pts',(-18.313375423817,12.6848122547612,131.186922689569)) ;
#141937 = CARTESIAN_POINT('Ctrl Pts',(-18.2476370162531,12.8954783028643,
131.02811076423)) ;
#141938 = CARTESIAN_POINT('Ctrl Pts',(-18.2022662694842,13.143031226721,130.92863304818)) ;
#141939 = CARTESIAN_POINT('Ctrl Pts',(-18.1793404232656,13.4109716015929,
130.894784380807)) ;
#141940 = CARTESIAN_POINT('Ctrl Pts',(-18.1798282338456,13.6794256952143,
130.929276425369)) ;
#141941 = CARTESIAN_POINT('Ctrl Pts',(-18.2032729243198,13.9314101071075,
131.031097970165)) ;
#141942 = CARTESIAN_POINT('Ctrl Pts',(-18.2467759985431,14.1445006476294,
131.19117652553)) ;
#141943 = CARTESIAN_POINT('Ctrl Pts',(-18.3066776441594,14.3067536446236,
131.399226993527)) ;
#141944 = CARTESIAN_POINT('Ctrl Pts',(-18.3782137507977,14.4060487060152,
131.641351715669)) ;
#141945 = CARTESIAN_POINT('Ctrl Pts',(-18.4553476578096,14.4348548850669,
131.899823806856)) ;
#141946 = CARTESIAN_POINT('Ctrl Pts',(-18.5318716415341,14.3909041577753,
132.156543176564)) ;
#141947 = CARTESIAN_POINT('Ctrl Pts',(-18.6011996766594,14.2783347271922,
132.392068800067)) ;
#141948 = CARTESIAN_POINT('Ctrl Pts',(-18.6585012371958,14.1031935059032,
132.592753758215)) ;
#141949 = CARTESIAN_POINT('Ctrl Pts',(-18.6980121020502,13.880010412854,132.741285296251)) ;
#141950 = CARTESIAN_POINT('Ctrl Pts',(-18.7166279415518,13.6249526911944,
132.828691039322)) ;
#141951 = CARTESIAN_POINT('Ctrl Pts',(-18.7123103754502,13.354798949211,132.849191352967)) ;
#141952 = CARTESIAN_POINT('Ctrl Pts',(-18.6846880430549,13.0897726213642,
132.801568647031)) ;
#141953 = CARTESIAN_POINT('Ctrl Pts',(-18.6343821577113,12.8467548703801,
132.687965653879)) ;
#141954 = CARTESIAN_POINT('Ctrl Pts',(-18.5654973268203,12.6478123647641,
132.519664319044)) ;
#141955 = CARTESIAN_POINT('Ctrl Pts',(-18.48107055355,12.5027971632239,132.306214422385)) ;
#141956 = CARTESIAN_POINT('Ctrl Pts',(-18.3870428160206,12.4240443471672,
132.064632825828)) ;
#141957 = CARTESIAN_POINT('Ctrl Pts',(-18.2887354925409,12.4170503727496,
131.81073482203)) ;
#141958 = CARTESIAN_POINT('Ctrl Pts',(-18.1939119303328,12.4817914292567,
131.566682633117)) ;
#141959 = CARTESIAN_POINT('Ctrl Pts',(-18.1070449414969,12.6142901362916,
131.346109388021)) ;
#141960 = CARTESIAN_POINT('Ctrl Pts',(-18.0346358797705,12.8042104652996,
131.167634409426)) ;
#141961 = CARTESIAN_POINT('Ctrl Pts',(-17.9805255623072,13.0388187683455,
131.042705325369)) ;
#141962 = CARTESIAN_POINT('Ctrl Pts',(-17.9481797311077,13.3023286417973,
130.981508149385)) ;
#141963 = CARTESIAN_POINT('Ctrl Pts',(-17.9392863704219,13.571341528554,130.988424251185)) ;
#141964 = CARTESIAN_POINT('Ctrl Pts',(-17.953573606269,13.8329963549421,131.063471024854)) ;
#141965 = CARTESIAN_POINT('Ctrl Pts',(-17.9893989895141,14.0635777479953,
131.201232852988)) ;
#141966 = CARTESIAN_POINT('Ctrl Pts',(-18.0431541123013,14.2479537659708,
131.391285506657)) ;
#141967 = CARTESIAN_POINT('Ctrl Pts',(-18.1105562726005,14.3739504814687,
131.621267259674)) ;
#141968 = CARTESIAN_POINT('Ctrl Pts',(-18.1864968499214,14.4320428256961,
131.876400337601)) ;
#141969 = CARTESIAN_POINT('Ctrl Pts',(-18.2639229888398,14.417227489115,132.135696662505)) ;
#141970 = CARTESIAN_POINT('Ctrl Pts',(-18.3367309580096,14.3318166696858,
132.38139603203)) ;
#141971 = CARTESIAN_POINT('Ctrl Pts',(-18.3994855464605,14.1811817924182,
132.597839900643)) ;
#141972 = CARTESIAN_POINT('Ctrl Pts',(-18.4466875926336,13.9759967234678,
132.76887624803)) ;
#141973 = CARTESIAN_POINT('Ctrl Pts',(-18.4742378060519,13.7313492030733,
132.882483371035)) ;
#141974 = CARTESIAN_POINT('Ctrl Pts',(-18.4792949779045,13.4634560829624,
132.930523403806)) ;
#141975 = CARTESIAN_POINT('Ctrl Pts',(-18.461128478173,13.1958849143636,132.910312028036)) ;
#141976 = CARTESIAN_POINT('Ctrl Pts',(-18.4197940229711,12.9412336892527,
132.822854780355)) ;
#141977 = CARTESIAN_POINT('Ctrl Pts',(-18.3581041603467,12.7230235102752,
132.675668704181)) ;
#141978 = CARTESIAN_POINT('Ctrl Pts',(-18.2791809280835,12.5539648148601,
132.478304085645)) ;
#141979 = CARTESIAN_POINT('Ctrl Pts',(-18.1885902754786,12.4477725883293,
132.246702802813)) ;
#141980 = CARTESIAN_POINT('Ctrl Pts',(-18.0914153871671,12.4110238127138,
131.995992901408)) ;
#141981 = CARTESIAN_POINT('Ctrl Pts',(-17.994297829235,12.4468710240649,131.74541114138)) ;
#141982 = CARTESIAN_POINT('Ctrl Pts',(-17.9031245377903,12.5531554013667,
131.512299991437)) ;
#141983 = CARTESIAN_POINT('Ctrl Pts',(-17.8243881263639,12.7211113727201,
131.31534546579)) ;
#141984 = CARTESIAN_POINT('Ctrl Pts',(-17.7623176137726,12.9400020484962,
131.167199368981)) ;
#141985 = CARTESIAN_POINT('Ctrl Pts',(-17.721116969805,13.1921120918715,131.07982905239)) ;
#141986 = CARTESIAN_POINT('Ctrl Pts',(-17.7025045759027,13.4620045892925,
131.058616683595)) ;
#141987 = CARTESIAN_POINT('Ctrl Pts',(-17.7074749062916,13.7292706883455,
131.106312813536)) ;
#141988 = CARTESIAN_POINT('Ctrl Pts',(-17.7347681793512,13.9738126531135,
131.219120659009)) ;
#141989 = CARTESIAN_POINT('Ctrl Pts',(-17.7817727411794,14.179494761427,131.389572070766)) ;
#141990 = CARTESIAN_POINT('Ctrl Pts',(-17.844677886555,14.3311259562621,131.606587075838)) ;
#141991 = CARTESIAN_POINT('Ctrl Pts',(-17.9173204242354,14.4169205750236,
131.851744794664)) ;
#141992 = CARTESIAN_POINT('Ctrl Pts',(-17.995061475666,14.4320030262707,132.112107124994)) ;
#141993 = CARTESIAN_POINT('Ctrl Pts',(-18.0703004283371,14.3751243416082,
132.364855998224)) ;
#141994 = CARTESIAN_POINT('Ctrl Pts',(-18.1383688657966,14.2488767663409,
132.597055820527)) ;
#141995 = CARTESIAN_POINT('Ctrl Pts',(-18.1921359192542,14.0648018016439,
132.78710913641)) ;
#141996 = CARTESIAN_POINT('Ctrl Pts',(-18.2280722562178,13.8343787612975,
132.925210436483)) ;
#141997 = CARTESIAN_POINT('Ctrl Pts',(-18.242538116868,13.57360703546,133.000682596127)) ;
#141998 = CARTESIAN_POINT('Ctrl Pts',(-18.2336329639187,13.3025524242793,
133.007820999502)) ;
#141999 = CARTESIAN_POINT('Ctrl Pts',(-18.2017369474132,13.0417944958654,
132.947575616599)) ;
#142000 = CARTESIAN_POINT('Ctrl Pts',(-18.1478312171758,12.8063139825281,
132.823302147589)) ;
#142001 = CARTESIAN_POINT('Ctrl Pts',(-18.0755496900259,12.6158856325691,
132.645204191962)) ;
#142002 = CARTESIAN_POINT('Ctrl Pts',(-17.9886538009937,12.4825396581066,
132.424600946456)) ;
#142003 = CARTESIAN_POINT('Ctrl Pts',(-17.8937284373199,12.4173081126312,
132.180299122837)) ;
#142004 = CARTESIAN_POINT('Ctrl Pts',(-17.7958096584206,12.4236050164849,
131.92740109039)) ;
#142005 = CARTESIAN_POINT('Ctrl Pts',(-17.7015466531236,12.5018026361359,
131.685195645254)) ;
#142006 = CARTESIAN_POINT('Ctrl Pts',(-17.6171539893032,12.6458566369947,
131.471772621455)) ;
#142007 = CARTESIAN_POINT('Ctrl Pts',(-17.5478109773661,12.8453791511498,
131.302294768861)) ;
#142008 = CARTESIAN_POINT('Ctrl Pts',(-17.4976407306197,13.0865653368531,
131.18887233862)) ;
#142009 = CARTESIAN_POINT('Ctrl Pts',(-17.4696392111755,13.3521428238873,
131.140239531717)) ;
#142010 = CARTESIAN_POINT('Ctrl Pts',(-17.4651068443978,13.6222557770976,
131.160098232974)) ;
#142011 = CARTESIAN_POINT('Ctrl Pts',(-17.4835603986076,13.878388340665,131.247136678345)) ;
#142012 = CARTESIAN_POINT('Ctrl Pts',(-17.5231079409385,14.1022120909712,
131.395853700729)) ;
#142013 = CARTESIAN_POINT('Ctrl Pts',(-17.5798728990191,14.2765229673721,
131.594730965601)) ;
#142014 = CARTESIAN_POINT('Ctrl Pts',(-17.6491847088976,14.3902287028563,
131.830268466419)) ;
#142015 = CARTESIAN_POINT('Ctrl Pts',(-17.7259698460983,14.4347769425123,
132.087872526908)) ;
#142016 = CARTESIAN_POINT('Ctrl Pts',(-17.8027636785654,14.406672259026,132.345197200108)) ;
#142017 = CARTESIAN_POINT('Ctrl Pts',(-17.8744322223128,14.3082119103095,
132.587721606493)) ;
#142018 = CARTESIAN_POINT('Ctrl Pts',(-17.9346414922608,14.146035786889,132.796763374113)) ;
#142019 = CARTESIAN_POINT('Ctrl Pts',(-17.978328838425,13.9328084599434,132.957440175315)) ;
#142020 = CARTESIAN_POINT('Ctrl Pts',(-18.0018422375615,13.6817741285683,
133.059362342777)) ;
#142021 = CARTESIAN_POINT('Ctrl Pts',(-18.0026012553216,13.4140262407359,
133.094572904511)) ;
#142022 = CARTESIAN_POINT('Ctrl Pts',(-17.9798594877152,13.1453688481844,
133.061337889453)) ;
#142023 = CARTESIAN_POINT('Ctrl Pts',(-17.9347276850374,12.8977836730895,
132.962526042225)) ;
#142024 = CARTESIAN_POINT('Ctrl Pts',(-17.8690240884409,12.6861562581584,
132.803892072345)) ;
#142025 = CARTESIAN_POINT('Ctrl Pts',(-17.7877339722851,12.5289208542769,
132.599457950631)) ;
#142026 = CARTESIAN_POINT('Ctrl Pts',(-17.6951142737879,12.43515491016,132.362074354773)) ;
#142027 = CARTESIAN_POINT('Ctrl Pts',(-17.5979412066733,12.4122393521451,
132.111194582501)) ;
#142028 = CARTESIAN_POINT('Ctrl Pts',(-17.5010420457257,12.461921394401,131.861423387377)) ;
#142029 = CARTESIAN_POINT('Ctrl Pts',(-17.4121127241867,12.5803996881322,
131.634723585912)) ;
#142030 = CARTESIAN_POINT('Ctrl Pts',(-17.3360909230878,12.7591299511845,
131.445758242556)) ;
#142031 = CARTESIAN_POINT('Ctrl Pts',(-17.2778596775834,12.9850687744513,
131.30871290489)) ;
#142032 = CARTESIAN_POINT('Ctrl Pts',(-17.2406869894393,13.2423777832249,
131.233202541002)) ;
#142033 = CARTESIAN_POINT('Ctrl Pts',(-17.2265555305213,13.5129449874981,
131.225042209929)) ;
#142034 = CARTESIAN_POINT('Ctrl Pts',(-17.2358208600922,13.7774321466873,
131.285270109407)) ;
#142035 = CARTESIAN_POINT('Ctrl Pts',(-17.2672256879663,14.0166134840393,
131.410209396935)) ;
#142036 = CARTESIAN_POINT('Ctrl Pts',(-17.3173096357002,14.2120831170415,
131.589498480406)) ;
#142037 = CARTESIAN_POINT('Ctrl Pts',(-17.3825645879294,14.3524989582878,
131.813388688858)) ;
#142038 = CARTESIAN_POINT('Ctrl Pts',(-17.4569074319178,14.4253825851082,
132.063685579465)) ;
#142039 = CARTESIAN_POINT('Ctrl Pts',(-17.5341963564748,14.4267682802424,
132.322471620608)) ;
#142040 = CARTESIAN_POINT('Ctrl Pts',(-17.6087797719604,14.3564919766321,
132.573476433911)) ;
#142041 = CARTESIAN_POINT('Ctrl Pts',(-17.6744472100706,14.2186718710266,
132.798538178836)) ;
#142042 = CARTESIAN_POINT('Ctrl Pts',(-17.72535311061,14.024316702861,132.980354800871)) ;
#142043 = CARTESIAN_POINT('Ctrl Pts',(-17.7574107045078,13.7866135128635,
133.107157176176)) ;
#142044 = CARTESIAN_POINT('Ctrl Pts',(-17.7675312687633,13.5238036073327,
133.169755706042)) ;
#142045 = CARTESIAN_POINT('Ctrl Pts',(-17.7543475166113,13.2527085149488,
133.164413552802)) ;
#142046 = CARTESIAN_POINT('Ctrl Pts',(-17.7178633050782,12.9936529878453,
133.09103192121)) ;
#142047 = CARTESIAN_POINT('Ctrl Pts',(-17.6602511851627,12.7662441294868,
132.95581758286)) ;
#142048 = CARTESIAN_POINT('Ctrl Pts',(-17.5849255965554,12.5858801023732,
132.768826558598)) ;
#142049 = CARTESIAN_POINT('Ctrl Pts',(-17.4961834389353,12.4648530530782,
132.542741778166)) ;
#142050 = CARTESIAN_POINT('Ctrl Pts',(-17.3995854558629,12.4128201852834,
132.293797467727)) ;
#142051 = CARTESIAN_POINT('Ctrl Pts',(-17.3025511829403,12.4330274205639,
132.04325545605)) ;
#142052 = CARTESIAN_POINT('Ctrl Pts',(-17.2096884596466,12.5240123419654,
131.805133684606)) ;
#142053 = CARTESIAN_POINT('Ctrl Pts',(-17.1276669580838,12.6795221471728,
131.598658383154)) ;
#142054 = CARTESIAN_POINT('Ctrl Pts',(-17.0614706985305,12.8889214300487,
131.438497796341)) ;
#142055 = CARTESIAN_POINT('Ctrl Pts',(-17.0154598015636,13.1354947204779,
131.337138856507)) ;
#142056 = CARTESIAN_POINT('Ctrl Pts',(-16.9918318882357,13.4042911484909,
131.301379652949)) ;
#142057 = CARTESIAN_POINT('Ctrl Pts',(-16.9917442489886,13.6719452324486,
131.334066321195)) ;
#142058 = CARTESIAN_POINT('Ctrl Pts',(-17.0144533549174,13.9242175313922,
131.433665873443)) ;
#142059 = CARTESIAN_POINT('Ctrl Pts',(-17.0574770945585,14.1390288718251,
131.592404046704)) ;
#142060 = CARTESIAN_POINT('Ctrl Pts',(-17.1170228825635,14.3030286134432,
131.799436930536)) ;
#142061 = CARTESIAN_POINT('Ctrl Pts',(-17.1883492711194,14.404195333154,132.040962388259)) ;
#142062 = CARTESIAN_POINT('Ctrl Pts',(-17.2651695925288,14.4349854783543,
132.298417684023)) ;
#142063 = CARTESIAN_POINT('Ctrl Pts',(-17.3418160412074,14.3934046860553,
132.555492533382)) ;
#142064 = CARTESIAN_POINT('Ctrl Pts',(-17.4116634894223,14.2822103029933,
132.792658991486)) ;
#142065 = CARTESIAN_POINT('Ctrl Pts',(-17.4690521516874,14.1097942178576,
132.993391663448)) ;
#142066 = CARTESIAN_POINT('Ctrl Pts',(-17.5093062354731,13.8877666791924,
133.144142840939)) ;
#142067 = CARTESIAN_POINT('Ctrl Pts',(-17.5286362429465,13.6324083997063,
133.233762073457)) ;
#142068 = CARTESIAN_POINT('Ctrl Pts',(-17.5249803176019,13.3624184985193,
133.25618971708)) ;
#142069 = CARTESIAN_POINT('Ctrl Pts',(-17.4979086389593,13.0965814202268,
133.210233885048)) ;
#142070 = CARTESIAN_POINT('Ctrl Pts',(-17.448517501126,12.8540735599423,133.099102550144)) ;
#142071 = CARTESIAN_POINT('Ctrl Pts',(-17.3800811280718,12.6529923851621,
132.932185918228)) ;
#142072 = CARTESIAN_POINT('Ctrl Pts',(-17.2955087487444,12.5055873938463,
132.718493138558)) ;
#142073 = CARTESIAN_POINT('Ctrl Pts',(-17.2021020536049,12.4255318492028,
132.478568577667)) ;
#142074 = CARTESIAN_POINT('Ctrl Pts',(-17.1042647123247,12.41606276029,132.2258939674)) ;
#142075 = CARTESIAN_POINT('Ctrl Pts',(-17.0088005914449,12.478829942444,131.980130586559)) ;
#142076 = CARTESIAN_POINT('Ctrl Pts',(-16.9215448155793,12.6096603386007,
131.758445231646)) ;
#142077 = CARTESIAN_POINT('Ctrl Pts',(-16.848533723708,12.7985462969973,131.578279303791)) ;
#142078 = CARTESIAN_POINT('Ctrl Pts',(-16.7940414763144,13.0317087125592,
131.452162324081)) ;
#142079 = CARTESIAN_POINT('Ctrl Pts',(-16.7611013224607,13.2930836864475,
131.389038106982)) ;
#142080 = CARTESIAN_POINT('Ctrl Pts',(-16.7513989370885,13.5641925745626,
131.393845489194)) ;
#142081 = CARTESIAN_POINT('Ctrl Pts',(-16.7650967126463,13.8256807565213,
131.46708434546)) ;
#142082 = CARTESIAN_POINT('Ctrl Pts',(-16.8001170901404,14.0565823950309,
131.602366827208)) ;
#142083 = CARTESIAN_POINT('Ctrl Pts',(-16.853538816955,14.2434411721512,131.791567853675)) ;
#142084 = CARTESIAN_POINT('Ctrl Pts',(-16.9209280070917,14.3714533932326,
132.021637857135)) ;
#142085 = CARTESIAN_POINT('Ctrl Pts',(-16.9960840169429,14.4311593781317,
132.274200346814)) ;
#142086 = CARTESIAN_POINT('Ctrl Pts',(-17.0737363474756,14.4188767221607,
132.534241998506)) ;
#142087 = CARTESIAN_POINT('Ctrl Pts',(-17.1469202195293,14.3353893492018,
132.781100248646)) ;
#142088 = CARTESIAN_POINT('Ctrl Pts',(-17.2102141809998,14.1858865785186,
132.999227503805)) ;
#142089 = CARTESIAN_POINT('Ctrl Pts',(-17.257730654902,13.982932266947,133.171038872199)) ;
#142090 = CARTESIAN_POINT('Ctrl Pts',(-17.2859586154811,13.7386001468469,
133.286713511024)) ;
#142091 = CARTESIAN_POINT('Ctrl Pts',(-17.291722530296,13.472491032427,133.336641515932)) ;
#142092 = CARTESIAN_POINT('Ctrl Pts',(-17.2741574542646,13.2027754330182,
133.318428828081)) ;
#142093 = CARTESIAN_POINT('Ctrl Pts',(-17.233357936349,12.947572926699,133.232521523896)) ;
#142094 = CARTESIAN_POINT('Ctrl Pts',(-17.1723162295254,12.7286906750514,
133.08716241814)) ;
#142095 = CARTESIAN_POINT('Ctrl Pts',(-17.0940329814276,12.5582194191414,
132.891590931029)) ;
#142096 = CARTESIAN_POINT('Ctrl Pts',(-17.003220735762,12.4495814743775,132.65952031743)) ;
#142097 = CARTESIAN_POINT('Ctrl Pts',(-16.9063349510849,12.4111325032394,
132.409580555585)) ;
#142098 = CARTESIAN_POINT('Ctrl Pts',(-16.8093564797719,12.4448573223553,
132.159334717268)) ;
#142099 = CARTESIAN_POINT('Ctrl Pts',(-16.7181348033276,12.5485736252265,
131.925983075815)) ;
#142100 = CARTESIAN_POINT('Ctrl Pts',(-16.6384335148824,12.7160675406203,
131.726443646401)) ;
#142101 = CARTESIAN_POINT('Ctrl Pts',(-16.5761662546992,12.9327061663297,
131.577552509025)) ;
#142102 = CARTESIAN_POINT('Ctrl Pts',(-16.5341642871538,13.1846668461228,
131.4879329288)) ;
#142103 = CARTESIAN_POINT('Ctrl Pts',(-16.5149327205021,13.4544224662781,
131.464916019242)) ;
#142104 = CARTESIAN_POINT('Ctrl Pts',(-16.5192086330336,13.7215757501031,
131.510525864953)) ;
#142105 = CARTESIAN_POINT('Ctrl Pts',(-16.5459259073865,13.9674106040572,
131.621703691313)) ;
#142106 = CARTESIAN_POINT('Ctrl Pts',(-16.5923467307556,14.1739595566239,
131.790386254332)) ;
#142107 = CARTESIAN_POINT('Ctrl Pts',(-16.6546298745393,14.3272529144105,
132.00549077589)) ;
#142108 = CARTESIAN_POINT('Ctrl Pts',(-16.7275392721876,14.4155298054197,
132.25165131066)) ;
#142109 = CARTESIAN_POINT('Ctrl Pts',(-16.8047539631414,14.4326688880929,
132.510258938982)) ;
#142110 = CARTESIAN_POINT('Ctrl Pts',(-16.8806059328636,14.3775210612736,
132.765014735693)) ;
#142111 = CARTESIAN_POINT('Ctrl Pts',(-16.948497815144,14.2540409039206,132.996451811014)) ;
#142112 = CARTESIAN_POINT('Ctrl Pts',(-17.0030423303969,14.0709647731437,
133.188927025101)) ;
#142113 = CARTESIAN_POINT('Ctrl Pts',(-17.0395041310645,13.8416199051522,
133.328550909828)) ;
#142114 = CARTESIAN_POINT('Ctrl Pts',(-17.0546215409426,13.5823884703292,
133.405817397953)) ;
#142115 = CARTESIAN_POINT('Ctrl Pts',(-17.0465466847866,13.3112803473401,
133.41538970088)) ;
#142116 = CARTESIAN_POINT('Ctrl Pts',(-17.0150799598172,13.0483997002377,
133.356605998046)) ;
#142117 = CARTESIAN_POINT('Ctrl Pts',(-16.9619997380882,12.8130297532618,
133.234583750432)) ;
#142118 = CARTESIAN_POINT('Ctrl Pts',(-16.8900010563963,12.6204060162552,
133.057421174726)) ;
#142119 = CARTESIAN_POINT('Ctrl Pts',(-16.8034708183318,12.4854478919258,
132.837862758507)) ;
#142120 = CARTESIAN_POINT('Ctrl Pts',(-16.7086924678089,12.4181326606572,
132.593999330846)) ;
#142121 = CARTESIAN_POINT('Ctrl Pts',(-16.6104956156241,12.4224942646145,
132.340376856576)) ;
#142122 = CARTESIAN_POINT('Ctrl Pts',(-16.5161424264609,12.4989653492952,
132.097884581704)) ;
#142123 = CARTESIAN_POINT('Ctrl Pts',(-16.4317556020667,12.6405920086238,
131.884334903027)) ;
#142124 = CARTESIAN_POINT('Ctrl Pts',(-16.3616746574105,12.8391594148647,
131.71279689553)) ;
#142125 = CARTESIAN_POINT('Ctrl Pts',(-16.3108304239017,13.0802460396382,
131.59750363429)) ;
#142126 = CARTESIAN_POINT('Ctrl Pts',(-16.2823238978487,13.3449462912613,
131.54733314331)) ;
#142127 = CARTESIAN_POINT('Ctrl Pts',(-16.2771309839151,13.614299734848,131.565154678749)) ;
#142128 = CARTESIAN_POINT('Ctrl Pts',(-16.2949010006599,13.8710421702277,
131.65018620171)) ;
#142129 = CARTESIAN_POINT('Ctrl Pts',(-16.3338452049706,14.0962488627573,
131.797148934845)) ;
#142130 = CARTESIAN_POINT('Ctrl Pts',(-16.3905407253916,14.272991429521,131.996013377583)) ;
#142131 = CARTESIAN_POINT('Ctrl Pts',(-16.4592327826985,14.3876795568682,
132.229561597162)) ;
#142132 = CARTESIAN_POINT('Ctrl Pts',(-16.5357659030759,14.4346057862448,
132.486378414112)) ;
#142133 = CARTESIAN_POINT('Ctrl Pts',(-16.613055863645,14.4082599424993,132.74533988594)) ;
#142134 = CARTESIAN_POINT('Ctrl Pts',(-16.6845204129575,14.3122705822436,
132.98706452462)) ;
#142135 = CARTESIAN_POINT('Ctrl Pts',(-16.7454150213927,14.1514361820495,
133.198229674243)) ;
#142136 = CARTESIAN_POINT('Ctrl Pts',(-16.7896253783432,13.9387188784373,
133.36051515223)) ;
#142137 = CARTESIAN_POINT('Ctrl Pts',(-16.8136464583059,13.6904434149952,
133.463667989134)) ;
#142138 = CARTESIAN_POINT('Ctrl Pts',(-16.8150989773608,13.4208420632377,
133.501172955387)) ;
#142139 = CARTESIAN_POINT('Ctrl Pts',(-16.7930957689776,13.1534853920285,
133.469895702491)) ;
#142140 = CARTESIAN_POINT('Ctrl Pts',(-16.7485502511386,12.9044050276542,
133.372879092163)) ;
#142141 = CARTESIAN_POINT('Ctrl Pts',(-16.6833056672716,12.691347593862,133.215606346478)) ;
#142142 = CARTESIAN_POINT('Ctrl Pts',(-16.6023121457365,12.5324268950077,
133.012069499167)) ;
#142143 = CARTESIAN_POINT('Ctrl Pts',(-16.510247041001,12.4369854895294,132.776191038926)) ;
#142144 = CARTESIAN_POINT('Ctrl Pts',(-16.4129292753124,12.4119049764517,
132.52496184791)) ;
#142145 = CARTESIAN_POINT('Ctrl Pts',(-16.3162560708554,12.4592885985088,
132.275727976682)) ;
#142146 = CARTESIAN_POINT('Ctrl Pts',(-16.2269249209603,12.575733706437,132.047883576996)) ;
#142147 = CARTESIAN_POINT('Ctrl Pts',(-16.1503960745848,12.7527803278304,
131.857442783129)) ;
#142148 = CARTESIAN_POINT('Ctrl Pts',(-16.0912973211166,12.9786618836061,
131.718025410541)) ;
#142149 = CARTESIAN_POINT('Ctrl Pts',(-16.053563244281,13.2359089048801,131.640933230899)) ;
#142150 = CARTESIAN_POINT('Ctrl Pts',(-16.0388435174732,13.5051027063819,
131.630895828566)) ;
#142151 = CARTESIAN_POINT('Ctrl Pts',(-16.047530549604,13.771120969237,131.689577950022)) ;
#142152 = CARTESIAN_POINT('Ctrl Pts',(-16.078229877861,14.0100004351276,131.812285143493)) ;
#142153 = CARTESIAN_POINT('Ctrl Pts',(-16.1279007148338,14.2073725024461,
131.990439316612)) ;
#142154 = CARTESIAN_POINT('Ctrl Pts',(-16.1927067195232,14.3492226720416,
132.212956820855)) ;
#142155 = CARTESIAN_POINT('Ctrl Pts',(-16.2667592579309,14.4242520037555,
132.462368666128)) ;
#142156 = CARTESIAN_POINT('Ctrl Pts',(-16.3443760925168,14.4277364435235,
132.722252547872)) ;
#142157 = CARTESIAN_POINT('Ctrl Pts',(-16.4190218197498,14.3592419699784,
132.973404327502)) ;
#142158 = CARTESIAN_POINT('Ctrl Pts',(-16.4847503849809,14.2240686259208,
133.198484837379)) ;
#142159 = CARTESIAN_POINT('Ctrl Pts',(-16.5363595036201,14.0305584607837,
133.38248100773)) ;
#142160 = CARTESIAN_POINT('Ctrl Pts',(-16.5689433106285,13.7945205251559,
133.510729343035)) ;
#142161 = CARTESIAN_POINT('Ctrl Pts',(-16.5797941428791,13.5313066856814,
133.575579533295)) ;
#142162 = CARTESIAN_POINT('Ctrl Pts',(-16.567251148853,13.2605191131678,133.57206289759)) ;
#142163 = CARTESIAN_POINT('Ctrl Pts',(-16.5315770470974,13.0015410285169,
133.50095404784)) ;
#142164 = CARTESIAN_POINT('Ctrl Pts',(-16.4745328734589,12.7725523248786,
133.367443152597)) ;
#142165 = CARTESIAN_POINT('Ctrl Pts',(-16.3994606288027,12.5901313640957,
133.181279217731)) ;
#142166 = CARTESIAN_POINT('Ctrl Pts',(-16.3110718117679,12.4675131143056,
132.956201420078)) ;
#142167 = CARTESIAN_POINT('Ctrl Pts',(-16.2150465684198,12.4133289099041,
132.708783471555)) ;
#142168 = CARTESIAN_POINT('Ctrl Pts',(-16.1172756530906,12.4315113584402,
132.456324766904)) ;
#142169 = CARTESIAN_POINT('Ctrl Pts',(-16.0245054184323,12.5204618944922,
132.218365021381)) ;
#142170 = CARTESIAN_POINT('Ctrl Pts',(-15.9421012205372,12.6740885855686,
132.010764917566)) ;
#142171 = CARTESIAN_POINT('Ctrl Pts',(-15.875367634635,12.8820605871686,131.849026621626)) ;
#142172 = CARTESIAN_POINT('Ctrl Pts',(-15.8287083770857,13.1280849227168,
131.74581643471)) ;
#142173 = CARTESIAN_POINT('Ctrl Pts',(-15.8044325587747,13.3954305595711,
131.70802549061)) ;
#142174 = CARTESIAN_POINT('Ctrl Pts',(-15.8036483197092,13.664772130159,131.738860618359)) ;
#142175 = CARTESIAN_POINT('Ctrl Pts',(-15.825629308736,13.916650368435,131.836174288953)) ;
#142176 = CARTESIAN_POINT('Ctrl Pts',(-15.8681455318913,14.1333087809813,
131.993506201505)) ;
#142177 = CARTESIAN_POINT('Ctrl Pts',(-15.927193309252,14.2989356818664,132.199046381853)) ;
#142178 = CARTESIAN_POINT('Ctrl Pts',(-15.9986879065092,14.4025578141661,
132.44125861652)) ;
#142179 = CARTESIAN_POINT('Ctrl Pts',(-16.0751723449273,14.4350103980761,
132.697614959121)) ;
#142180 = CARTESIAN_POINT('Ctrl Pts',(-16.1518509504202,14.3956728073431,
132.954753133988)) ;
#142181 = CARTESIAN_POINT('Ctrl Pts',(-16.2220068716851,14.2862787528374,
133.192841857477)) ;
#142182 = CARTESIAN_POINT('Ctrl Pts',(-16.2797925866452,14.1158603426533,
133.394685682589)) ;
#142183 = CARTESIAN_POINT('Ctrl Pts',(-16.3207945954701,13.8934485150928,
133.547842676703)) ;
#142184 = CARTESIAN_POINT('Ctrl Pts',(-16.3405803998949,13.6404741079279,
133.638562788148)) ;
#142185 = CARTESIAN_POINT('Ctrl Pts',(-16.3376032483563,13.3695006911583,
133.663119999001)) ;
#142186 = CARTESIAN_POINT('Ctrl Pts',(-16.3112454472243,13.1044456788723,
133.619106817927)) ;
#142187 = CARTESIAN_POINT('Ctrl Pts',(-16.2625596253282,12.8607039818763,
133.510049336795)) ;
#142188 = CARTESIAN_POINT('Ctrl Pts',(-16.1940271721615,12.6571154322834,
133.343090977728)) ;
#142189 = CARTESIAN_POINT('Ctrl Pts',(-16.1108795002955,12.509808022699,133.133139897156)) ;
#142190 = CARTESIAN_POINT('Ctrl Pts',(-16.0171502461323,12.4266891378063,
132.892483711977)) ;
#142191 = CARTESIAN_POINT('Ctrl Pts',(-15.919067834617,12.4154229833254,132.639178441848)) ;
#142192 = CARTESIAN_POINT('Ctrl Pts',(-15.8237916187375,12.4759771003581,
132.393848463188)) ;
#142193 = CARTESIAN_POINT('Ctrl Pts',(-15.7361936167486,12.6048252979973,
132.171163013204)) ;
#142194 = CARTESIAN_POINT('Ctrl Pts',(-15.6626673506394,12.792164644416,131.989497153743)) ;
#142195 = CARTESIAN_POINT('Ctrl Pts',(-15.6074901711292,13.0247863190839,
131.861453094695)) ;
#142196 = CARTESIAN_POINT('Ctrl Pts',(-15.5739200759961,13.2853106439738,
131.796445961381)) ;
#142197 = CARTESIAN_POINT('Ctrl Pts',(-15.5636021153955,13.5574332084958,
131.799586177716)) ;
#142198 = CARTESIAN_POINT('Ctrl Pts',(-15.5764802743328,13.8171022396022,
131.870118715194)) ;
#142199 = CARTESIAN_POINT('Ctrl Pts',(-15.611132431221,14.051173953077,132.004607403079)) ;
#142200 = CARTESIAN_POINT('Ctrl Pts',(-15.6640759803966,14.2388282531697,
132.192340452033)) ;
#142201 = CARTESIAN_POINT('Ctrl Pts',(-15.7308833601088,14.3685839592775,
132.420606589598)) ;
#142202 = CARTESIAN_POINT('Ctrl Pts',(-15.8064742715662,14.4305511556418,
132.674695319148)) ;
#142203 = CARTESIAN_POINT('Ctrl Pts',(-15.8835822303502,14.4203097239978,
132.93289312949)) ;
#142204 = CARTESIAN_POINT('Ctrl Pts',(-15.9573192391447,14.3384207836783,
133.181537405768)) ;
#142205 = CARTESIAN_POINT('Ctrl Pts',(-16.0206561333224,14.1915731436481,
133.399594202983)) ;
#142206 = CARTESIAN_POINT('Ctrl Pts',(-16.0690536966344,13.9880714714153,
133.574284718797)) ;
#142207 = CARTESIAN_POINT('Ctrl Pts',(-16.0975526481624,13.7471725052838,
133.690391133825)) ;
#142208 = CARTESIAN_POINT('Ctrl Pts',(-16.1041169388077,13.4800206037099,
133.742852683177)) ;
#142209 = CARTESIAN_POINT('Ctrl Pts',(-16.0872443704174,13.2110030429649,
133.726550659017)) ;
#142210 = CARTESIAN_POINT('Ctrl Pts',(-16.0471230753564,12.9547748927777,
133.64265811564)) ;
#142211 = CARTESIAN_POINT('Ctrl Pts',(-15.9865759612961,12.7344342247069,
133.498774691296)) ;
#142212 = CARTESIAN_POINT('Ctrl Pts',(-15.9086915708439,12.5623453660856,
133.304378900685)) ;
#142213 = CARTESIAN_POINT('Ctrl Pts',(-15.8183465306617,12.4518692088092,
133.073606369183)) ;
#142214 = CARTESIAN_POINT('Ctrl Pts',(-15.7212787432989,12.4112334911996,
132.823235526097)) ;
#142215 = CARTESIAN_POINT('Ctrl Pts',(-15.6243186466118,12.442749147776,132.572999265293)) ;
#142216 = CARTESIAN_POINT('Ctrl Pts',(-15.5323128334074,12.5456206773071,
132.337577591656)) ;
#142217 = CARTESIAN_POINT('Ctrl Pts',(-15.453258603987,12.7091960236905,132.139476652336)) ;
#142218 = CARTESIAN_POINT('Ctrl Pts',(-15.3898383285792,12.9259029773537,
131.987475859056)) ;
#142219 = CARTESIAN_POINT('Ctrl Pts',(-15.3472877469184,13.1770736237047,
131.896231444798)) ;
#142220 = CARTESIAN_POINT('Ctrl Pts',(-15.3273612325374,13.4468768400015,
131.871223050135)) ;
#142221 = CARTESIAN_POINT('Ctrl Pts',(-15.3309764443274,13.7138795897728,
131.914840701596)) ;
#142222 = CARTESIAN_POINT('Ctrl Pts',(-15.3570417967896,13.9605431985016,
132.024107079577)) ;
#142223 = CARTESIAN_POINT('Ctrl Pts',(-15.4029179113879,14.1686235654109,
132.191205295214)) ;
#142224 = CARTESIAN_POINT('Ctrl Pts',(-15.4651226728873,14.324111284162,132.406226710796)) ;
#142225 = CARTESIAN_POINT('Ctrl Pts',(-15.5374063763882,14.4138215880485,
132.650368768959)) ;
#142226 = CARTESIAN_POINT('Ctrl Pts',(-15.6148696071944,14.4331945050443,
132.909835134181)) ;
#142227 = CARTESIAN_POINT('Ctrl Pts',(-15.6906277120936,14.3801614626116,
133.164214215321)) ;
#142228 = CARTESIAN_POINT('Ctrl Pts',(-15.7589271578745,14.2584942565519,
133.396886988434)) ;
#142229 = CARTESIAN_POINT('Ctrl Pts',(-15.8138969641916,14.0770491380578,
133.590585730492)) ;
#142230 = CARTESIAN_POINT('Ctrl Pts',(-15.8510060052898,13.8484874642558,
133.732152268361)) ;
#142231 = CARTESIAN_POINT('Ctrl Pts',(-15.8667131197633,13.5893549989453,
133.811197408128)) ;
#142232 = CARTESIAN_POINT('Ctrl Pts',(-15.8593406152276,13.319692173746,133.822652269934)) ;
#142233 = CARTESIAN_POINT('Ctrl Pts',(-15.8286128783071,13.0561133199218,
133.76604483536)) ;
#142234 = CARTESIAN_POINT('Ctrl Pts',(-15.7759801790062,12.8190740737043,
133.645417619665)) ;
#142235 = CARTESIAN_POINT('Ctrl Pts',(-15.7045036655101,12.6252975626819,
133.469748009719)) ;
#142236 = CARTESIAN_POINT('Ctrl Pts',(-15.6186604888065,12.4887796662223,
133.252078050461)) ;
#142237 = CARTESIAN_POINT('Ctrl Pts',(-15.5236958147091,12.4190606373648,
133.007800237169)) ;
#142238 = CARTESIAN_POINT('Ctrl Pts',(-15.4258603341632,12.4213023433048,
132.755107590907)) ;
#142239 = CARTESIAN_POINT('Ctrl Pts',(-15.3312661273055,12.4953372710628,
132.511916145083)) ;
#142240 = CARTESIAN_POINT('Ctrl Pts',(-15.2461014219628,12.6358733450884,
132.296256624047)) ;
#142241 = CARTESIAN_POINT('Ctrl Pts',(-15.1757623763379,12.8325870207608,
132.12387434654)) ;
#142242 = CARTESIAN_POINT('Ctrl Pts',(-15.1244118681695,13.0715963225307,
132.006975021887)) ;
#142243 = CARTESIAN_POINT('Ctrl Pts',(-15.0950340623661,13.336692941588,131.954373590249)) ;
#142244 = CARTESIAN_POINT('Ctrl Pts',(-15.0891646881233,13.6067854476423,
131.970293382415)) ;
#142245 = CARTESIAN_POINT('Ctrl Pts',(-15.1063211628653,13.8640947363139,
132.05352643624)) ;
#142246 = CARTESIAN_POINT('Ctrl Pts',(-15.1445701006616,14.089839779911,132.198362269326)) ;
#142247 = CARTESIAN_POINT('Ctrl Pts',(-15.2007425773632,14.2683601910573,
132.395691390543)) ;
#142248 = CARTESIAN_POINT('Ctrl Pts',(-15.2694132319916,14.385487730189,132.629307915259)) ;
#142249 = CARTESIAN_POINT('Ctrl Pts',(-15.3459082333124,14.4341894586694,
132.886044120066)) ;
#142250 = CARTESIAN_POINT('Ctrl Pts',(-15.4228395829729,14.4102459791679,
133.143771383713)) ;
#142251 = CARTESIAN_POINT('Ctrl Pts',(-15.494944359048,14.3157190447574,133.387554110632)) ;
#142252 = CARTESIAN_POINT('Ctrl Pts',(-15.5558765426031,14.1574302898824,
133.598637081667)) ;
#142253 = CARTESIAN_POINT('Ctrl Pts',(-15.6008224271939,13.9458829058386,
133.763138208487)) ;
#142254 = CARTESIAN_POINT('Ctrl Pts',(-15.6255201649115,13.6969896283466,
133.868443529266)) ;
#142255 = CARTESIAN_POINT('Ctrl Pts',(-15.6275786112566,13.4292803806108,
133.907520168097)) ;
#142256 = CARTESIAN_POINT('Ctrl Pts',(-15.6063759832611,13.1613091083809,
133.878612288534)) ;
#142257 = CARTESIAN_POINT('Ctrl Pts',(-15.5619644958359,12.9096301895175,
133.78225128118)) ;
#142258 = CARTESIAN_POINT('Ctrl Pts',(-15.4979303513307,12.6977069155964,
133.628145147095)) ;
#142259 = CARTESIAN_POINT('Ctrl Pts',(-15.417114271924,12.536159176258,133.425257288799)) ;
#142260 = CARTESIAN_POINT('Ctrl Pts',(-15.3252949349401,12.4388403103588,
133.190087141283)) ;
#142261 = CARTESIAN_POINT('Ctrl Pts',(-15.2279404799318,12.4115721830993,
132.93878796517)) ;
#142262 = CARTESIAN_POINT('Ctrl Pts',(-15.1310969074068,12.457029419961,132.689076414865)) ;
#142263 = CARTESIAN_POINT('Ctrl Pts',(-15.0416608970638,12.5713337690677,
132.460857982082)) ;
#142264 = CARTESIAN_POINT('Ctrl Pts',(-14.9646158772577,12.7468028835324,
132.268928751753)) ;
#142265 = CARTESIAN_POINT('Ctrl Pts',(-14.9049751892106,12.9715573467482,
132.127931845598)) ;
#142266 = CARTESIAN_POINT('Ctrl Pts',(-14.8666141904923,13.2272671930713,
132.0489034762)) ;
#142267 = CARTESIAN_POINT('Ctrl Pts',(-14.8511623659717,13.4980619502807,
132.036944216363)) ;
#142268 = CARTESIAN_POINT('Ctrl Pts',(-14.8590704558367,13.7620975253013,
132.093037654942)) ;
#142269 = CARTESIAN_POINT('Ctrl Pts',(-14.8892480575814,14.0037249771829,
132.21444701514)) ;
#142270 = CARTESIAN_POINT('Ctrl Pts',(-14.9384427260129,14.202400093294,132.391194252055)) ;
#142271 = CARTESIAN_POINT('Ctrl Pts',(-15.0030756975973,14.3463073278919,
132.613297185418)) ;
#142272 = CARTESIAN_POINT('Ctrl Pts',(-15.0766441588427,14.4229407274136,
132.861156433463)) ;
#142273 = CARTESIAN_POINT('Ctrl Pts',(-15.1542518269372,14.4287087096985,
133.121019796098)) ;
#142274 = CARTESIAN_POINT('Ctrl Pts',(-15.2291034561164,14.3623691322231,
133.37277976698)) ;
#142275 = CARTESIAN_POINT('Ctrl Pts',(-15.2954353285377,14.2283779056864,
133.599762615258)) ;
#142276 = CARTESIAN_POINT('Ctrl Pts',(-15.3473792259273,14.0364255545022,
133.784686288565)) ;
#142277 = CARTESIAN_POINT('Ctrl Pts',(-15.3804798619707,13.8020943881553,
133.914354405728)) ;
#142278 = CARTESIAN_POINT('Ctrl Pts',(-15.3920181078753,13.5391612776222,
133.981245241876)) ;
#142279 = CARTESIAN_POINT('Ctrl Pts',(-15.3801942480057,13.268618582974,133.979790178508)) ;
#142280 = CARTESIAN_POINT('Ctrl Pts',(-15.3451113205383,13.0086418344895,
133.910463378564)) ;
#142281 = CARTESIAN_POINT('Ctrl Pts',(-15.2888485505009,12.7791079862287,
133.779136483972)) ;
#142282 = CARTESIAN_POINT('Ctrl Pts',(-15.2138964639745,12.5942976841109,
133.59347890567)) ;
#142283 = CARTESIAN_POINT('Ctrl Pts',(-15.1261222353351,12.4702970290912,
133.370074169085)) ;
#142284 = CARTESIAN_POINT('Ctrl Pts',(-15.0300476900928,12.4139049816003,
133.122583731637)) ;
#142285 = CARTESIAN_POINT('Ctrl Pts',(-14.9325665835877,12.4297924440583,
132.870854131327)) ;
#142286 = CARTESIAN_POINT('Ctrl Pts',(-14.838960003689,12.5172147656158,132.63066535824)) ;
#142287 = CARTESIAN_POINT('Ctrl Pts',(-14.7562177989916,12.6696686051205,
132.422099640111)) ;
#142288 = CARTESIAN_POINT('Ctrl Pts',(-14.6894014584479,12.8748936311913,
132.259900679124)) ;
#142289 = CARTESIAN_POINT('Ctrl Pts',(-14.6419381314949,13.1206629569548,
132.154439065691)) ;
#142290 = CARTESIAN_POINT('Ctrl Pts',(-14.617022067619,13.3874987151297,132.114753350066)) ;
#142291 = CARTESIAN_POINT('Ctrl Pts',(-14.6155607269755,13.6577700593923,
132.143697626099)) ;
#142292 = CARTESIAN_POINT('Ctrl Pts',(-14.6370052322387,13.9102263629719,
132.239439325318)) ;
#142293 = CARTESIAN_POINT('Ctrl Pts',(-14.6787534379256,14.127342135122,132.394384380573)) ;
#142294 = CARTESIAN_POINT('Ctrl Pts',(-14.737766120839,14.2954362012379,132.600024203604)) ;
#142295 = CARTESIAN_POINT('Ctrl Pts',(-14.8083643434813,14.400199046936,132.839317925707)) ;
#142296 = CARTESIAN_POINT('Ctrl Pts',(-14.8854780825288,14.4351706373417,
133.097830821909)) ;
#142297 = CARTESIAN_POINT('Ctrl Pts',(-14.9618174412002,14.3977719560938,
133.35379058418)) ;
#142298 = CARTESIAN_POINT('Ctrl Pts',(-15.0324040200964,14.2904204320916,
133.59319366883)) ;
#142299 = CARTESIAN_POINT('Ctrl Pts',(-15.090764871553,14.1205426182846,133.796859479231)) ;
#142300 = CARTESIAN_POINT('Ctrl Pts',(-15.1319227402497,13.9015880180689,
133.95013819427)) ;
#142301 = CARTESIAN_POINT('Ctrl Pts',(-15.1525599707839,13.6483197429669,
134.043502414266)) ;
#142302 = CARTESIAN_POINT('Ctrl Pts',(-15.1502448946848,13.3774459783215,
134.069996708961)) ;
#142303 = CARTESIAN_POINT('Ctrl Pts',(-15.1244931600293,13.1115163789139,
134.027817890031)) ;
#142304 = CARTESIAN_POINT('Ctrl Pts',(-15.0765141667085,12.867627711837,133.920732027969)) ;
#142305 = CARTESIAN_POINT('Ctrl Pts',(-15.0088413137702,12.6630941323673,
133.756165950852)) ;
#142306 = CARTESIAN_POINT('Ctrl Pts',(-14.9254870825308,12.5128296370691,
133.545852043451)) ;
#142307 = CARTESIAN_POINT('Ctrl Pts',(-14.8319589407702,12.4280522080275,
133.305771576008)) ;
#142308 = CARTESIAN_POINT('Ctrl Pts',(-14.7340778039936,12.4147676790035,
133.052999941768)) ;
#142309 = CARTESIAN_POINT('Ctrl Pts',(-14.6386324749928,12.4732052495888,
132.807177718268)) ;
#142310 = CARTESIAN_POINT('Ctrl Pts',(-14.5504362769443,12.6008830846757,
132.582865547777)) ;
#142311 = CARTESIAN_POINT('Ctrl Pts',(-14.4768576797366,12.7859101152191,
132.400880133504)) ;
#142312 = CARTESIAN_POINT('Ctrl Pts',(-14.4210707390125,13.0171550939707,
132.271032735321)) ;
#142313 = CARTESIAN_POINT('Ctrl Pts',(-14.3868017963535,13.2774025189781,
132.204022588309)) ;
#142314 = CARTESIAN_POINT('Ctrl Pts',(-14.3757654194404,13.5492093049786,
132.205023339175)) ;
#142315 = CARTESIAN_POINT('Ctrl Pts',(-14.3880514684394,13.8101283643081,
132.273924034985)) ;
#142316 = CARTESIAN_POINT('Ctrl Pts',(-14.4219003231422,14.0442617204232,
132.405903677218)) ;
#142317 = CARTESIAN_POINT('Ctrl Pts',(-14.4747801059438,14.2348997538622,
132.593713095369)) ;
#142318 = CARTESIAN_POINT('Ctrl Pts',(-14.5409603434691,14.3654883224984,
132.819967847917)) ;
#142319 = CARTESIAN_POINT('Ctrl Pts',(-14.6161864464348,14.4297229265612,
133.072916709743)) ;
#142320 = CARTESIAN_POINT('Ctrl Pts',(-14.6935812312555,14.421668005349,133.33206349666)) ;
#142321 = CARTESIAN_POINT('Ctrl Pts',(-14.7675434877312,14.3417420843685,
133.5813725027)) ;
#142322 = CARTESIAN_POINT('Ctrl Pts',(-14.8312585222105,14.1964291100303,
133.800560188562)) ;
#142323 = CARTESIAN_POINT('Ctrl Pts',(-14.8799642737121,13.9955518397601,
133.975972972826)) ;
#142324 = CARTESIAN_POINT('Ctrl Pts',(-14.9093078343249,13.7541464168563,
134.094757838791)) ;
#142325 = CARTESIAN_POINT('Ctrl Pts',(-14.9164487725813,13.4873870374965,
134.148893971889)) ;
#142326 = CARTESIAN_POINT('Ctrl Pts',(-14.9002547065785,13.2187118678006,
134.134518709842)) ;
#142327 = CARTESIAN_POINT('Ctrl Pts',(-14.8609138929022,12.9622340205071,
134.052837189393)) ;
#142328 = CARTESIAN_POINT('Ctrl Pts',(-14.8006595820543,12.7396654906289,
133.909958025568)) ;
#142329 = CARTESIAN_POINT('Ctrl Pts',(-14.7231765654135,12.5663130117826,
133.716718287322)) ;
#142330 = CARTESIAN_POINT('Ctrl Pts',(-14.6335055175769,12.4542929765583,
133.487776150199)) ;
#142331 = CARTESIAN_POINT('Ctrl Pts',(-14.536209707559,12.4113060992836,133.236853912787)) ;
#142332 = CARTESIAN_POINT('Ctrl Pts',(-14.4393435905948,12.4409729765678,
132.986840999606)) ;
#142333 = CARTESIAN_POINT('Ctrl Pts',(-14.3475507084136,12.5408195809103,
132.751846613996)) ;
#142334 = CARTESIAN_POINT('Ctrl Pts',(-14.2671647163194,12.7045177174677,
132.550230917324)) ;
#142335 = CARTESIAN_POINT('Ctrl Pts',(-14.2035979096792,12.919412680773,132.397665865524)) ;
#142336 = CARTESIAN_POINT('Ctrl Pts',(-14.1604688985404,13.1689179430447,
132.304632041467)) ;
#142337 = CARTESIAN_POINT('Ctrl Pts',(-14.139782678841,13.4397285825566,132.277557000125)) ;
#142338 = CARTESIAN_POINT('Ctrl Pts',(-14.142785048101,13.7064270622518,132.319308711258)) ;
#142339 = CARTESIAN_POINT('Ctrl Pts',(-14.1682103421544,13.9538863073551,
132.426697860702)) ;
#142340 = CARTESIAN_POINT('Ctrl Pts',(-14.2135281033141,14.163192773507,132.592143093095)) ;
#142341 = CARTESIAN_POINT('Ctrl Pts',(-14.2753850982946,14.3205261321744,
132.806174358066)) ;
#142342 = CARTESIAN_POINT('Ctrl Pts',(-14.3473411439298,14.4121066537417,
133.049314213563)) ;
#142343 = CARTESIAN_POINT('Ctrl Pts',(-14.4248089805252,14.433704272446,133.308819308561)) ;
#142344 = CARTESIAN_POINT('Ctrl Pts',(-14.5007784378179,14.3826278008681,
133.563851701539)) ;
#142345 = CARTESIAN_POINT('Ctrl Pts',(-14.5693363275554,14.2628852203127,
133.797259307275)) ;
#142346 = CARTESIAN_POINT('Ctrl Pts',(-14.6247737505551,14.0829261229302,
133.992336674271)) ;
#142347 = CARTESIAN_POINT('Ctrl Pts',(-14.6624238056517,13.8556921301219,
134.135454195566)) ;
#142348 = CARTESIAN_POINT('Ctrl Pts',(-14.6787751303134,13.5972598207812,
134.216376119518)) ;
#142349 = CARTESIAN_POINT('Ctrl Pts',(-14.6721663860168,13.3277678231801,
134.230044601199)) ;
#142350 = CARTESIAN_POINT('Ctrl Pts',(-14.6417520985073,13.061810881333,134.174606742694)) ;
#142351 = CARTESIAN_POINT('Ctrl Pts',(-14.5901365318131,12.8260388711121,
134.056642369562)) ;
#142352 = CARTESIAN_POINT('Ctrl Pts',(-14.5189277267524,12.6298695868286,
133.881890430345)) ;
#142353 = CARTESIAN_POINT('Ctrl Pts',(-14.4334483620761,12.491768708706,133.665259640123)) ;
#142354 = CARTESIAN_POINT('Ctrl Pts',(-14.3385453399518,12.4199839155212,
133.421203195212)) ;
#142355 = CARTESIAN_POINT('Ctrl Pts',(-14.2407585005838,12.4203084391601,
133.168634581772)) ;
#142356 = CARTESIAN_POINT('Ctrl Pts',(-14.1461361734331,12.492208510643,132.925307480569)) ;
#142357 = CARTESIAN_POINT('Ctrl Pts',(-14.0605732797982,12.630997013847,132.708502600032)) ;
#142358 = CARTESIAN_POINT('Ctrl Pts',(-13.9897130342082,12.8263312491105,
132.53460873687)) ;
#142359 = CARTESIAN_POINT('Ctrl Pts',(-13.9376533995034,13.0651229525308,
132.415734889569)) ;
#142360 = CARTESIAN_POINT('Ctrl Pts',(-13.9077497589157,13.3295669294852,
132.361565342467)) ;
#142361 = CARTESIAN_POINT('Ctrl Pts',(-13.901216822791,13.5989125314577,132.375443730603)) ;
#142362 = CARTESIAN_POINT('Ctrl Pts',(-13.9177760025398,13.8574711990645,
132.457011745281)) ;
#142363 = CARTESIAN_POINT('Ctrl Pts',(-13.9553957581231,14.08370800358,132.599924272669)) ;
#142364 = CARTESIAN_POINT('Ctrl Pts',(-14.0110176386716,14.2638192585231,
132.795614384729)) ;
#142365 = CARTESIAN_POINT('Ctrl Pts',(-14.0796276403271,14.3831696043844,
133.029163918101)) ;
#142366 = CARTESIAN_POINT('Ctrl Pts',(-14.1557505767541,14.4337176712718,
133.284703197076)) ;
#142367 = CARTESIAN_POINT('Ctrl Pts',(-14.2327802934375,14.4120588565301,
133.542734126691)) ;
#142368 = CARTESIAN_POINT('Ctrl Pts',(-14.3052072147828,14.3193772826324,
133.787499406446)) ;
#142369 = CARTESIAN_POINT('Ctrl Pts',(-14.3665740744773,14.1628170776178,
133.999858164627)) ;
#142370 = CARTESIAN_POINT('Ctrl Pts',(-14.4121259724299,13.9515916120412,
134.166258760957)) ;
#142371 = CARTESIAN_POINT('Ctrl Pts',(-14.4372801227629,13.7055233139094,
134.272631180499)) ;
#142372 = CARTESIAN_POINT('Ctrl Pts',(-14.440046863088,13.4359481903885,134.314052320636)) ;
#142373 = CARTESIAN_POINT('Ctrl Pts',(-14.4195164737538,13.1690262561277,
134.286945100641)) ;
#142374 = CARTESIAN_POINT('Ctrl Pts',(-14.375727536596,12.9162728254293,134.192437995692)) ;
#142375 = CARTESIAN_POINT('Ctrl Pts',(-14.3123844010594,12.7036779683092,
134.040261155373)) ;
#142376 = CARTESIAN_POINT('Ctrl Pts',(-14.2321535671344,12.5403117617381,
133.839041349776)) ;
#142377 = CARTESIAN_POINT('Ctrl Pts',(-14.1399646502613,12.4404489557871,
133.603011473166)) ;
#142378 = CARTESIAN_POINT('Ctrl Pts',(-14.0431420853103,12.4114485631191,
133.353105162355)) ;
#142379 = CARTESIAN_POINT('Ctrl Pts',(-13.9462412595183,12.4544846447878,
133.103205911968)) ;
#142380 = CARTESIAN_POINT('Ctrl Pts',(-13.8561482718694,12.5672617831098,
132.873195369857)) ;
#142381 = CARTESIAN_POINT('Ctrl Pts',(-13.7786242096377,12.741774518216,132.679929018516)) ;
#142382 = CARTESIAN_POINT('Ctrl Pts',(-13.7188694411303,12.9633751206612,
132.538319767188)) ;
#142383 = CARTESIAN_POINT('Ctrl Pts',(-13.6795051572281,13.2203112306522,
132.456621058414)) ;
#142384 = CARTESIAN_POINT('Ctrl Pts',(-13.6635016097314,13.4905144393576,
132.442983868862)) ;
#142385 = CARTESIAN_POINT('Ctrl Pts',(-13.6707757272997,13.7550217254887,
132.497240868873)) ;
#142386 = CARTESIAN_POINT('Ctrl Pts',(-13.7002116917388,13.9967496932403,
132.616356096113)) ;
#142387 = CARTESIAN_POINT('Ctrl Pts',(-13.7490260081706,14.1974243252069,
132.792087763225)) ;
#142388 = CARTESIAN_POINT('Ctrl Pts',(-13.8129747901669,14.3425140414095,
133.012032809254)) ;
#142389 = CARTESIAN_POINT('Ctrl Pts',(-13.8865372491761,14.4218016114581,
133.259977388133)) ;
#142390 = CARTESIAN_POINT('Ctrl Pts',(-13.9645151712435,14.4294553389326,
133.521084372305)) ;
#142391 = CARTESIAN_POINT('Ctrl Pts',(-14.0391560909907,14.3652617891387,
133.772071407551)) ;
#142392 = CARTESIAN_POINT('Ctrl Pts',(-14.1057363531632,14.2335996006041,
133.999718577771)) ;
#142393 = CARTESIAN_POINT('Ctrl Pts',(-14.1582660784627,14.0430657817291,
134.186391245985)) ;
#142394 = CARTESIAN_POINT('Ctrl Pts',(-14.1920661990571,13.8093137336756,
134.318173223818)) ;
#142395 = CARTESIAN_POINT('Ctrl Pts',(-14.2042127186391,13.5459138184761,
134.386958646077)) ;
#142396 = CARTESIAN_POINT('Ctrl Pts',(-14.1930930657431,13.2769102523372,
134.387368892485)) ;
#142397 = CARTESIAN_POINT('Ctrl Pts',(-14.1587186564867,13.0160045287208,
134.320145719112)) ;
#142398 = CARTESIAN_POINT('Ctrl Pts',(-14.1028872041378,12.7850160477838,
134.190142176635)) ;
#142399 = CARTESIAN_POINT('Ctrl Pts',(-14.028684171418,12.5991695463159,134.006558452314)) ;
#142400 = CARTESIAN_POINT('Ctrl Pts',(-13.9407662015876,12.4727066402134,
133.782907583956)) ;
#142401 = CARTESIAN_POINT('Ctrl Pts',(-13.8452936573205,12.414634000185,133.537011712374)) ;
#142402 = CARTESIAN_POINT('Ctrl Pts',(-13.7475595496828,12.4282724908794,
133.28461799683)) ;
#142403 = CARTESIAN_POINT('Ctrl Pts',(-13.6538542291428,12.5136822539145,
133.044102125595)) ;
#142404 = CARTESIAN_POINT('Ctrl Pts',(-13.5707377115012,12.6640314349918,
132.834416071391)) ;
#142405 = CARTESIAN_POINT('Ctrl Pts',(-13.5030136084428,12.8694014847424,
132.669787493301)) ;
#142406 = CARTESIAN_POINT('Ctrl Pts',(-13.4553004590304,13.11284739186,132.563387011279)) ;
#142407 = CARTESIAN_POINT('Ctrl Pts',(-13.4296313449615,13.3794714169119,
132.521528691967)) ;
#142408 = CARTESIAN_POINT('Ctrl Pts',(-13.4274890180519,13.649387589438,132.548416277511)) ;
#142409 = CARTESIAN_POINT('Ctrl Pts',(-13.4481636726345,13.9027716993511,
132.641905993097)) ;
#142410 = CARTESIAN_POINT('Ctrl Pts',(-13.489766031508,14.1226004021729,132.796684089978)) ;
#142411 = CARTESIAN_POINT('Ctrl Pts',(-13.5477833605945,14.2907614939367,
132.999088667497)) ;
#142412 = CARTESIAN_POINT('Ctrl Pts',(-13.6187363184265,14.3985142695992,
133.239726637088)) ;
#142413 = CARTESIAN_POINT('Ctrl Pts',(-13.6952590065994,14.4350393249369,
133.496283799514)) ;
#142414 = CARTESIAN_POINT('Ctrl Pts',(-13.7718333962932,14.4000355942845,
133.752990096946)) ;
#142415 = CARTESIAN_POINT('Ctrl Pts',(-13.8429167997199,14.294019259171,133.99396202455)) ;
#142416 = CARTESIAN_POINT('Ctrl Pts',(-13.9014231128193,14.1264036787102,
134.197913623386)) ;
#142417 = CARTESIAN_POINT('Ctrl Pts',(-13.9432439398755,13.908713601209,134.353150229304)) ;
#142418 = CARTESIAN_POINT('Ctrl Pts',(-13.9645351703535,13.6545233253026,
134.448627889531)) ;
#142419 = CARTESIAN_POINT('Ctrl Pts',(-13.9628501553954,13.385850090519,134.476712019796)) ;
#142420 = CARTESIAN_POINT('Ctrl Pts',(-13.9378025080024,13.1190055030057,
134.43665730351)) ;
#142421 = CARTESIAN_POINT('Ctrl Pts',(-13.8903445233776,12.8738785083339,
134.331138737956)) ;
#142422 = CARTESIAN_POINT('Ctrl Pts',(-13.822976322165,12.6676053408392,134.167543118068)) ;
#142423 = CARTESIAN_POINT('Ctrl Pts',(-13.7400513407993,12.5160770794409,
133.958438256977)) ;
#142424 = CARTESIAN_POINT('Ctrl Pts',(-13.6471767557041,12.429744459131,133.72011489165)) ;
#142425 = CARTESIAN_POINT('Ctrl Pts',(-13.5494411433701,12.4139325867349,
133.467730241205)) ;
#142426 = CARTESIAN_POINT('Ctrl Pts',(-13.4532942032315,12.470818666654,133.220058381188)) ;
#142427 = CARTESIAN_POINT('Ctrl Pts',(-13.3655312082867,12.5954481980338,
132.996719859513)) ;
#142428 = CARTESIAN_POINT('Ctrl Pts',(-13.2909901735497,12.7795463836638,
132.812100132889)) ;
#142429 = CARTESIAN_POINT('Ctrl Pts',(-13.2344956361294,13.0105019678005,
132.680282739157)) ;
#142430 = CARTESIAN_POINT('Ctrl Pts',(-13.1996213955,13.2704660588973,132.611535276715)) ;
#142431 = CARTESIAN_POINT('Ctrl Pts',(-13.1879877745145,13.5415026123175,
132.610702688434)) ;
#142432 = CARTESIAN_POINT('Ctrl Pts',(-13.1995723958978,13.8030871080867,
132.677561568908)) ;
#142433 = CARTESIAN_POINT('Ctrl Pts',(-13.2331003609654,14.0389748553007,
132.808744242538)) ;
#142434 = CARTESIAN_POINT('Ctrl Pts',(-13.2848573473153,14.2290324993106,
132.992884454479)) ;
#142435 = CARTESIAN_POINT('Ctrl Pts',(-13.3512130512097,14.3629001779689,
133.219942892695)) ;
#142436 = CARTESIAN_POINT('Ctrl Pts',(-13.4261333638039,14.428830285179,133.471917113561)) ;
#142437 = CARTESIAN_POINT('Ctrl Pts',(-13.5036989912694,14.4228365042112,
133.731636937861)) ;
#142438 = CARTESIAN_POINT('Ctrl Pts',(-13.5775959146896,14.3452101955046,
133.980631757599)) ;
#142439 = CARTESIAN_POINT('Ctrl Pts',(-13.641848848355,14.2014202619827,134.201474982571)) ;
#142440 = CARTESIAN_POINT('Ctrl Pts',(-13.6909875456321,14.0021641250436,
134.378109627788)) ;
#142441 = CARTESIAN_POINT('Ctrl Pts',(-13.7209546388244,13.7617530552763,
134.498718016342)) ;
#142442 = CARTESIAN_POINT('Ctrl Pts',(-13.7288010165101,13.4956079562807,
134.554891268505)) ;
#142443 = CARTESIAN_POINT('Ctrl Pts',(-13.7132439378269,13.2262845260177,
134.542442655534)) ;
#142444 = CARTESIAN_POINT('Ctrl Pts',(-13.6746979333842,12.9698876491267,
134.462975697567)) ;
#142445 = CARTESIAN_POINT('Ctrl Pts',(-13.6149469945644,12.7457363777613,
134.321622051184)) ;
#142446 = CARTESIAN_POINT('Ctrl Pts',(-13.5380974991867,12.5708017324576,
134.130170046121)) ;
#142447 = CARTESIAN_POINT('Ctrl Pts',(-13.4478576752863,12.4561497047602,
133.899872377774)) ;
#142448 = CARTESIAN_POINT('Ctrl Pts',(-13.3517215673195,12.4116404870753,
133.651969615898)) ;
#142449 = CARTESIAN_POINT('Ctrl Pts',(-13.2540076250656,12.4391729366694,
133.399748085855)) ;
#142450 = CARTESIAN_POINT('Ctrl Pts',(-13.1622489475353,12.53717976609,133.164761472067)) ;
#142451 = CARTESIAN_POINT('Ctrl Pts',(-13.0816903558919,12.6985743476714,
132.962543249434)) ;
#142452 = CARTESIAN_POINT('Ctrl Pts',(-13.0175180261292,12.9117741339943,
132.808180146115)) ;
#142453 = CARTESIAN_POINT('Ctrl Pts',(-12.9735046777524,13.1624013119324,
132.712811635355)) ;
#142454 = CARTESIAN_POINT('Ctrl Pts',(-12.9523351151535,13.4305279124855,
132.684019974806)) ;
#142455 = CARTESIAN_POINT('Ctrl Pts',(-12.9545548418119,13.6988963529668,
132.723654394249)) ;
#142456 = CARTESIAN_POINT('Ctrl Pts',(-12.9793900887543,13.9472005440968,
132.829316178582)) ;
#142457 = CARTESIAN_POINT('Ctrl Pts',(-13.0242752828077,14.1580510718868,
132.993551859839)) ;
#142458 = CARTESIAN_POINT('Ctrl Pts',(-13.0854550375843,14.3165352463583,
133.205459831595)) ;
#142459 = CARTESIAN_POINT('Ctrl Pts',(-13.157539949544,14.4105996736352,133.449148953889)) ;
#142460 = CARTESIAN_POINT('Ctrl Pts',(-13.2347402649807,14.4340684642594,
133.707775721031)) ;
#142461 = CARTESIAN_POINT('Ctrl Pts',(-13.3109617785798,14.3850543763753,
133.963600013658)) ;
#142462 = CARTESIAN_POINT('Ctrl Pts',(-13.3798067326629,14.2669952008499,
134.197852855929)) ;
#142463 = CARTESIAN_POINT('Ctrl Pts',(-13.4355433691654,14.0891153904615,
134.393714184201)) ;
#142464 = CARTESIAN_POINT('Ctrl Pts',(-13.4738370489843,13.862922820575,134.538741233136)) ;
#142465 = CARTESIAN_POINT('Ctrl Pts',(-13.4908658096809,13.6044942948714,
134.621718490304)) ;
#142466 = CARTESIAN_POINT('Ctrl Pts',(-13.4848285534881,13.3352194719608,
134.637044133393)) ;
#142467 = CARTESIAN_POINT('Ctrl Pts',(-13.4553946454675,13.0705828677346,
134.584234105595)) ;
#142468 = CARTESIAN_POINT('Ctrl Pts',(-13.4040098364742,12.8316691546943,
134.467226066963)) ;
#142469 = CARTESIAN_POINT('Ctrl Pts',(-13.33314013384,12.6342705619082,134.293479942512)) ;
#142470 = CARTESIAN_POINT('Ctrl Pts',(-13.2483274035502,12.4949547618174,
134.078672195471)) ;
#142471 = CARTESIAN_POINT('Ctrl Pts',(-13.1535924500394,12.4210676007864,
133.835114510728)) ;
#142472 = CARTESIAN_POINT('Ctrl Pts',(-13.0559321401126,12.4192534953992,
133.582874005816)) ;
#142473 = CARTESIAN_POINT('Ctrl Pts',(-12.9609580471452,12.4890551433301,
133.338571080929)) ;
#142474 = CARTESIAN_POINT('Ctrl Pts',(-12.8747310689753,12.6269266116115,
133.119972901911)) ;
#142475 = CARTESIAN_POINT('Ctrl Pts',(-12.8038546046608,12.8196496525906,
132.945820052933)) ;
#142476 = CARTESIAN_POINT('Ctrl Pts',(-12.7510102619763,13.0580837190484,
132.824757826606)) ;
#142477 = CARTESIAN_POINT('Ctrl Pts',(-12.7205262657728,13.3214663424209,
132.768812514467)) ;
#142478 = CARTESIAN_POINT('Ctrl Pts',(-12.7133087559554,13.5912988654113,
132.780748069265)) ;
#142479 = CARTESIAN_POINT('Ctrl Pts',(-12.729106667133,13.8497220068298,132.85998023594)) ;
#142480 = CARTESIAN_POINT('Ctrl Pts',(-12.7664785971369,14.0789423187272,
133.002444149453)) ;
#142481 = CARTESIAN_POINT('Ctrl Pts',(-12.8216206784442,14.259760152893,133.196642880183)) ;
#142482 = CARTESIAN_POINT('Ctrl Pts',(-12.8896828571919,14.3805241864287,
133.428478547497)) ;
#142483 = CARTESIAN_POINT('Ctrl Pts',(-12.9655732912177,14.4333051091104,
133.683295676437)) ;
#142484 = CARTESIAN_POINT('Ctrl Pts',(-13.042967616016,14.4135763051709,133.942531611941)) ;
#142485 = CARTESIAN_POINT('Ctrl Pts',(-13.1155158955077,14.3230159686918,
134.187589922523)) ;
#142486 = CARTESIAN_POINT('Ctrl Pts',(-13.1774799234643,14.1669880508,134.401869852628)) ;
#142487 = CARTESIAN_POINT('Ctrl Pts',(-13.2229930301975,13.960185490464,134.567683354239)) ;
#142488 = CARTESIAN_POINT('Ctrl Pts',(-13.2491323955846,13.7121979598798,
134.677334901438)) ;
#142489 = CARTESIAN_POINT('Ctrl Pts',(-13.2525598777593,13.445325428157,134.720373659982)) ;
#142490 = CARTESIAN_POINT('Ctrl Pts',(-13.2325302461836,13.1756579311624,
134.695052960486)) ;
#142491 = CARTESIAN_POINT('Ctrl Pts',(-13.1898673555691,12.9248371147139,
134.603460459577)) ;
#142492 = CARTESIAN_POINT('Ctrl Pts',(-13.1266179073973,12.7087904234027,
134.451858747306)) ;
#142493 = CARTESIAN_POINT('Ctrl Pts',(-13.0468208875135,12.5441839986788,
134.251863436356)) ;
#142494 = CARTESIAN_POINT('Ctrl Pts',(-12.9549231889871,12.4422953627895,
134.016678643604)) ;
#142495 = CARTESIAN_POINT('Ctrl Pts',(-12.8579637622449,12.4112745918663,
133.766440878839)) ;
#142496 = CARTESIAN_POINT('Ctrl Pts',(-12.7611549009883,12.4523611263307,
133.516748584247)) ;
#142497 = CARTESIAN_POINT('Ctrl Pts',(-12.6710156401631,12.5627156351226,
133.286505870711)) ;
#142498 = CARTESIAN_POINT('Ctrl Pts',(-12.5927632872927,12.7362032520556,
133.091234472325)) ;
#142499 = CARTESIAN_POINT('Ctrl Pts',(-12.5325786259911,12.9562237292826,
132.948303657431)) ;
#142500 = CARTESIAN_POINT('Ctrl Pts',(-12.4925362362005,13.2127632851082,
132.864667442093)) ;
#142501 = CARTESIAN_POINT('Ctrl Pts',(-12.4758811291573,13.4814740425718,
132.848961259101)) ;
#142502 = CARTESIAN_POINT('Ctrl Pts',(-12.482415341822,13.7476021325284,132.901201359878)) ;
#142503 = CARTESIAN_POINT('Ctrl Pts',(-12.5113783925367,13.9907503270219,
133.019010135492)) ;
#142504 = CARTESIAN_POINT('Ctrl Pts',(-12.5595683982425,14.1921269255571,
133.192821462917)) ;
#142505 = CARTESIAN_POINT('Ctrl Pts',(-12.6230623786545,14.3392030791961,
133.411416698859)) ;
#142506 = CARTESIAN_POINT('Ctrl Pts',(-12.6970341102038,14.4207500388282,
133.660819657676)) ;
#142507 = CARTESIAN_POINT('Ctrl Pts',(-12.774263901664,14.4302362494743,133.919425040572)) ;
#142508 = CARTESIAN_POINT('Ctrl Pts',(-12.8494758392042,14.3680282355215,
134.172257690455)) ;
#142509 = CARTESIAN_POINT('Ctrl Pts',(-12.9164641133178,14.2375542878188,
134.401162442814)) ;
#142510 = CARTESIAN_POINT('Ctrl Pts',(-12.9692941715123,14.0487158820881,
134.588645421394)) ;
#142511 = CARTESIAN_POINT('Ctrl Pts',(-13.0035360447327,13.8167882878437,
134.721606270082)) ;
#142512 = CARTESIAN_POINT('Ctrl Pts',(-13.0164063281861,13.5548283790035,
134.792403087177)) ;
#142513 = CARTESIAN_POINT('Ctrl Pts',(-13.0059798332764,13.2844749263172,
134.794999956039)) ;
#142514 = CARTESIAN_POINT('Ctrl Pts',(-12.9721289476738,13.0226682928204,
134.729355118088)) ;
#142515 = CARTESIAN_POINT('Ctrl Pts',(-12.917018681203,12.7913019037466,134.601363667181)) ;
#142516 = CARTESIAN_POINT('Ctrl Pts',(-12.8433910805977,12.6040506886806,
134.41942655632)) ;
#142517 = CARTESIAN_POINT('Ctrl Pts',(-12.7558724866451,12.4756113608574,
134.19692331088)) ;
#142518 = CARTESIAN_POINT('Ctrl Pts',(-12.6602458572947,12.4152434806169,
133.950682918633)) ;
#142519 = CARTESIAN_POINT('Ctrl Pts',(-12.5625488997366,12.4269403893897,
133.69837573229)) ;
#142520 = CARTESIAN_POINT('Ctrl Pts',(-12.4688527527708,12.5099953392157,
133.457802697882)) ;
#142521 = CARTESIAN_POINT('Ctrl Pts',(-12.3852338683453,12.6587329493789,
133.246696937566)) ;
#142522 = CARTESIAN_POINT('Ctrl Pts',(-12.3171693653744,12.8618952615055,
133.080961556617)) ;
#142523 = CARTESIAN_POINT('Ctrl Pts',(-12.2685510182443,13.105407033224,132.972065334935)) ;
#142524 = CARTESIAN_POINT('Ctrl Pts',(-12.2422386883744,13.372198744835,132.928388345119)) ;
#142525 = CARTESIAN_POINT('Ctrl Pts',(-12.2394516643981,13.6415134475053,
132.953298608277)) ;
#142526 = CARTESIAN_POINT('Ctrl Pts',(-12.2594173692579,13.8954057522976,
133.044683143725)) ;
#142527 = CARTESIAN_POINT('Ctrl Pts',(-12.3004891041707,14.1169004817223,
133.19795900627)) ;
#142528 = CARTESIAN_POINT('Ctrl Pts',(-12.3582400665715,14.2868623314226,
133.399654280047)) ;
#142529 = CARTESIAN_POINT('Ctrl Pts',(-12.4284737856363,14.3960130363954,
133.637987808134)) ;
#142530 = CARTESIAN_POINT('Ctrl Pts',(-12.5052035539747,14.4351149221843,
133.895287975856)) ;
#142531 = CARTESIAN_POINT('Ctrl Pts',(-12.581975793469,14.4019052033915,134.152623117381)) ;
#142532 = CARTESIAN_POINT('Ctrl Pts',(-12.6530830929324,14.2983009205314,
134.393547253594)) ;
#142533 = CARTESIAN_POINT('Ctrl Pts',(-12.7122527073782,14.1317969233753,
134.599560718346)) ;
#142534 = CARTESIAN_POINT('Ctrl Pts',(-12.7545160578287,13.9153433735369,
134.756066454016)) ;
#142535 = CARTESIAN_POINT('Ctrl Pts',(-12.7763808920198,13.6633971657659,
134.853037417297)) ;
#142536 = CARTESIAN_POINT('Ctrl Pts',(-12.7755195845432,13.3943409356125,
134.883605222402)) ;
#142537 = CARTESIAN_POINT('Ctrl Pts',(-12.7509706545826,13.125759479102,134.84518017233)) ;
#142538 = CARTESIAN_POINT('Ctrl Pts',(-12.7042295073339,12.8806964502858,
134.741640153808)) ;
#142539 = CARTESIAN_POINT('Ctrl Pts',(-12.6376258108186,12.6734733504626,
134.580189987171)) ;
#142540 = CARTESIAN_POINT('Ctrl Pts',(-12.5549426142071,12.5195857964099,
134.371866859259)) ;
#142541 = CARTESIAN_POINT('Ctrl Pts',(-12.46181515628,12.431093262312,134.13296415491)) ;
#142542 = CARTESIAN_POINT('Ctrl Pts',(-12.3646330795371,12.4134132732782,
133.882020752927)) ;
#142543 = CARTESIAN_POINT('Ctrl Pts',(-12.2682242070371,12.4681188865971,
133.63362475741)) ;
#142544 = CARTESIAN_POINT('Ctrl Pts',(-12.1801451229978,12.5909169952097,
133.409362869367)) ;
#142545 = CARTESIAN_POINT('Ctrl Pts',(-12.1051580880957,12.7734489728906,
133.223438258115)) ;
#142546 = CARTESIAN_POINT('Ctrl Pts',(-12.0481373858043,13.0028155052197,
133.090024310372)) ;
#142547 = CARTESIAN_POINT('Ctrl Pts',(-12.0125481809866,13.2626813874081,
133.01925718553)) ;
#142548 = CARTESIAN_POINT('Ctrl Pts',(-12.0001983771847,13.5323092973528,
133.016160648346)) ;
#142549 = CARTESIAN_POINT('Ctrl Pts',(-12.0111586092843,13.7963544405994,
133.081441752916)) ;
#142550 = CARTESIAN_POINT('Ctrl Pts',(-12.0440275864981,14.0324258924939,
133.210582553837)) ;
#142551 = CARTESIAN_POINT('Ctrl Pts',(-12.0953705891647,14.2243212394665,
133.393573736006)) ;
#142552 = CARTESIAN_POINT('Ctrl Pts',(-12.1612093656614,14.3597397385498,
133.61903315744)) ;
#142553 = CARTESIAN_POINT('Ctrl Pts',(-12.2362126914327,14.4280132276383,
133.871367486346)) ;
#142554 = CARTESIAN_POINT('Ctrl Pts',(-12.3137470656388,14.4240026774031,
134.130972884586)) ;
#142555 = CARTESIAN_POINT('Ctrl Pts',(-12.38788747333,14.3482148360276,134.380710229016)) ;
#142556 = CARTESIAN_POINT('Ctrl Pts',(-12.452286472395,14.2066838492508,134.601870345064)) ;
#142557 = CARTESIAN_POINT('Ctrl Pts',(-12.502100488198,14.0084843901798,134.78056124378)) ;
#142558 = CARTESIAN_POINT('Ctrl Pts',(-12.5326854037367,13.7679162492584,
134.903106175098)) ;
#142559 = CARTESIAN_POINT('Ctrl Pts',(-12.5410969798908,13.5034892563332,
134.960764420724)) ;
#142560 = CARTESIAN_POINT('Ctrl Pts',(-12.5262131615707,13.2335993396584,
134.9503397068)) ;
#142561 = CARTESIAN_POINT('Ctrl Pts',(-12.4882428296575,12.9764075734903,
134.872572785143)) ;
#142562 = CARTESIAN_POINT('Ctrl Pts',(-12.4289044713352,12.7508791959946,
134.732473639261)) ;
#142563 = CARTESIAN_POINT('Ctrl Pts',(-12.3527354057446,12.5752390295055,
134.542884388565)) ;
#142564 = CARTESIAN_POINT('Ctrl Pts',(-12.2632773386131,12.4588914827239,
134.314708508696)) ;
#142565 = CARTESIAN_POINT('Ctrl Pts',(-12.166700002866,12.4118138337187,134.065711798887)) ;
#142566 = CARTESIAN_POINT('Ctrl Pts',(-12.0689529096772,12.4374481802068,
133.813382896759)) ;
#142567 = CARTESIAN_POINT('Ctrl Pts',(-11.9769702221726,12.5333386761198,
133.577728338921)) ;
#142568 = CARTESIAN_POINT('Ctrl Pts',(-11.8956955766465,12.6939673682458,
133.373567679243)) ;
#142569 = CARTESIAN_POINT('Ctrl Pts',(-11.8313521769806,12.905003236762,133.218546885697)) ;
#142570 = CARTESIAN_POINT('Ctrl Pts',(-11.7866067831211,13.1551454221065,
133.121092437729)) ;
#142571 = CARTESIAN_POINT('Ctrl Pts',(-11.7721059446934,13.3338159430811,
133.100771605669)) ;
#142572 = CARTESIAN_POINT('Ctrl Pts',(-11.7687201639657,13.423122164697,133.10190161956)) ;
#142573 = CARTESIAN_POINT('Ctrl Pts',(-33.2064616283861,13.1551399285885,
127.920719415945)) ;
#142574 = CARTESIAN_POINT('Ctrl Pts',(-33.2057227295762,13.1489709760559,
127.919291866388)) ;
#142575 = CARTESIAN_POINT('Ctrl Pts',(-33.1936688649743,13.0505875198745,
127.895761948055)) ;
#142576 = CARTESIAN_POINT('Ctrl Pts',(-33.160921840628,12.8648901900081,127.82307456361)) ;
#142577 = CARTESIAN_POINT('Ctrl Pts',(-33.0921833510773,12.637899642759,127.655294615791)) ;
#142578 = CARTESIAN_POINT('Ctrl Pts',(-33.0059288840404,12.4661938429578,
127.436429577543)) ;
#142579 = CARTESIAN_POINT('Ctrl Pts',(-32.9070996303315,12.3629468652583,
127.180997914754)) ;
#142580 = CARTESIAN_POINT('Ctrl Pts',(-32.8036494006583,12.3360866593215,
126.911722952076)) ;
#142581 = CARTESIAN_POINT('Ctrl Pts',(-32.7003181752768,12.3868468010151,
126.643092453762)) ;
#142582 = CARTESIAN_POINT('Ctrl Pts',(-32.6050897103573,12.5118616654237,
126.397998146605)) ;
#142583 = CARTESIAN_POINT('Ctrl Pts',(-32.5235050196537,12.7022377085439,
126.192812360252)) ;
#142584 = CARTESIAN_POINT('Ctrl Pts',(-32.4608859591013,12.9442212424904,
126.043009732538)) ;
#142585 = CARTESIAN_POINT('Ctrl Pts',(-32.4209546422374,13.2203923683254,
125.959474453867)) ;
#142586 = CARTESIAN_POINT('Ctrl Pts',(-32.405749339523,13.5109002567873,125.948146471616)) ;
#142587 = CARTESIAN_POINT('Ctrl Pts',(-32.4158543282408,13.7967279051741,
126.010955365665)) ;
#142588 = CARTESIAN_POINT('Ctrl Pts',(-32.44946277106,14.053163616969,126.142095751459)) ;
#142589 = CARTESIAN_POINT('Ctrl Pts',(-32.5037010294867,14.2659162320927,
126.333668528097)) ;
#142590 = CARTESIAN_POINT('Ctrl Pts',(-32.5739098208083,14.4182156131257,
126.571880763336)) ;
#142591 = CARTESIAN_POINT('Ctrl Pts',(-32.6545587102474,14.4993926376335,
126.840688712835)) ;
#142592 = CARTESIAN_POINT('Ctrl Pts',(-32.7386970776525,14.5030673759949,
127.119597798947)) ;
#142593 = CARTESIAN_POINT('Ctrl Pts',(-32.8196605589341,14.4296657361334,
127.389182606704)) ;
#142594 = CARTESIAN_POINT('Ctrl Pts',(-32.891145728035,14.2842404294125,127.631112234882)) ;
#142595 = CARTESIAN_POINT('Ctrl Pts',(-32.9473175863939,14.0768884033213,
127.828355609425)) ;
#142596 = CARTESIAN_POINT('Ctrl Pts',(-32.9832788532576,13.8219373708246,
127.966631980771)) ;
#142597 = CARTESIAN_POINT('Ctrl Pts',(-32.9956260618082,13.5404395793698,
128.035680171597)) ;
#142598 = CARTESIAN_POINT('Ctrl Pts',(-32.9830519454183,13.2491901831122,
128.032089979617)) ;
#142599 = CARTESIAN_POINT('Ctrl Pts',(-32.9453417855078,12.969918720115,127.955137134767)) ;
#142600 = CARTESIAN_POINT('Ctrl Pts',(-32.8850287367867,12.7245501655325,
127.811958868713)) ;
#142601 = CARTESIAN_POINT('Ctrl Pts',(-32.8050106729142,12.5279693790049,
127.61140382253)) ;
#142602 = CARTESIAN_POINT('Ctrl Pts',(-32.7109505070757,12.3961376577074,
127.369698243799)) ;
#142603 = CARTESIAN_POINT('Ctrl Pts',(-32.608093202144,12.3376103607184,127.102453943038)) ;
#142604 = CARTESIAN_POINT('Ctrl Pts',(-32.5042165214054,12.3569098768634,
126.832006082133)) ;
#142605 = CARTESIAN_POINT('Ctrl Pts',(-32.4047263008834,12.4527690637887,
126.574582317231)) ;
#142606 = CARTESIAN_POINT('Ctrl Pts',(-32.317039240674,12.6179594101214,126.35151544099)) ;
#142607 = CARTESIAN_POINT('Ctrl Pts',(-32.2462108306946,12.8405880896203,
126.177706544888)) ;
#142608 = CARTESIAN_POINT('Ctrl Pts',(-32.1965338574651,13.1065246819692,
126.065865852924)) ;
#142609 = CARTESIAN_POINT('Ctrl Pts',(-32.1713639236927,13.3925179969382,
126.02529765245)) ;
#142610 = CARTESIAN_POINT('Ctrl Pts',(-32.1711356447092,13.6819916806813,
126.057745187493)) ;
#142611 = CARTESIAN_POINT('Ctrl Pts',(-32.1955942855959,13.953724245336,126.16241143608)) ;
#142612 = CARTESIAN_POINT('Ctrl Pts',(-32.2420024149265,14.1863734270825,
126.331069844754)) ;
#142613 = CARTESIAN_POINT('Ctrl Pts',(-32.3062614393706,14.3643807952629,
126.551845049774)) ;
#142614 = CARTESIAN_POINT('Ctrl Pts',(-32.3832731449588,14.4754559836596,
126.809932800703)) ;
#142615 = CARTESIAN_POINT('Ctrl Pts',(-32.46693246729,14.5110246745496,127.087529153579)) ;
#142616 = CARTESIAN_POINT('Ctrl Pts',(-32.5498802722831,14.468706357864,127.362883365774)) ;
#142617 = CARTESIAN_POINT('Ctrl Pts',(-32.6261767345985,14.3514018733064,
127.618935169129)) ;
#142618 = CARTESIAN_POINT('Ctrl Pts',(-32.6892389357437,14.1671964526519,
127.836331456435)) ;
#142619 = CARTESIAN_POINT('Ctrl Pts',(-32.7336924477987,13.9308607646815,
127.999208617667)) ;
#142620 = CARTESIAN_POINT('Ctrl Pts',(-32.7560437331624,13.6570089391064,
128.09768299258)) ;
#142621 = CARTESIAN_POINT('Ctrl Pts',(-32.7536233967398,13.3664658768335,
128.123772039366)) ;
#142622 = CARTESIAN_POINT('Ctrl Pts',(-32.726020561585,13.0805680543038,128.076234678783)) ;
#142623 = CARTESIAN_POINT('Ctrl Pts',(-32.6745478724091,12.8190538509803,
127.958967690888)) ;
#142624 = CARTESIAN_POINT('Ctrl Pts',(-32.6016486027217,12.599933753752,127.77927449631)) ;
#142625 = CARTESIAN_POINT('Ctrl Pts',(-32.5129827012049,12.4413956885076,
127.553221361994)) ;
#142626 = CARTESIAN_POINT('Ctrl Pts',(-32.4129362071219,12.3520377966892,
127.294128922931)) ;
#142627 = CARTESIAN_POINT('Ctrl Pts',(-32.3085709639735,12.3397344016033,
127.022370141575)) ;
#142628 = CARTESIAN_POINT('Ctrl Pts',(-32.2065472158637,12.4049383820741,
126.757445808132)) ;
#142629 = CARTESIAN_POINT('Ctrl Pts',(-32.1134309497632,12.5429636135127,
126.518532052174)) ;
#142630 = CARTESIAN_POINT('Ctrl Pts',(-32.0350063547161,12.744355559365,126.322594585157)) ;
#142631 = CARTESIAN_POINT('Ctrl Pts',(-31.9764168702957,12.99435234836,126.184578080748)) ;
#142632 = CARTESIAN_POINT('Ctrl Pts',(-31.9410923640507,13.2741649900779,
126.114424971979)) ;
#142633 = CARTESIAN_POINT('Ctrl Pts',(-31.9306079711779,13.5657204845938,
126.116961809238)) ;
#142634 = CARTESIAN_POINT('Ctrl Pts',(-31.945333022402,13.8474317542271,126.1931967302)) ;
#142635 = CARTESIAN_POINT('Ctrl Pts',(-31.9830832898237,14.0971651338937,
126.336484257145)) ;
#142636 = CARTESIAN_POINT('Ctrl Pts',(-32.0409399787663,14.300212406185,126.538735226936)) ;
#142637 = CARTESIAN_POINT('Ctrl Pts',(-32.1136595413229,14.439451037695,126.784306408733)) ;
#142638 = CARTESIAN_POINT('Ctrl Pts',(-32.1949128964174,14.5058688377535,
127.05463526644)) ;
#142639 = CARTESIAN_POINT('Ctrl Pts',(-32.2791660586006,14.4952594512815,
127.333947782969)) ;
#142640 = CARTESIAN_POINT('Ctrl Pts',(-32.3592129092692,14.4071576201155,
127.601021809783)) ;
#142641 = CARTESIAN_POINT('Ctrl Pts',(-32.4281419451805,14.2488069359853,
127.835486225876)) ;
#142642 = CARTESIAN_POINT('Ctrl Pts',(-32.4805375156639,14.0323324822322,
128.021538873071)) ;
#142643 = CARTESIAN_POINT('Ctrl Pts',(-32.512289642295,13.7715184536488,128.147415816655)) ;
#142644 = CARTESIAN_POINT('Ctrl Pts',(-32.5201337915764,13.4849967549257,
128.20352710882)) ;
#142645 = CARTESIAN_POINT('Ctrl Pts',(-32.5025273372398,13.1936953531143,
128.185335934368)) ;
#142646 = CARTESIAN_POINT('Ctrl Pts',(-32.4607259546474,12.9217410379526,
128.096103762869)) ;
#142647 = CARTESIAN_POINT('Ctrl Pts',(-32.3960971896468,12.6826992816898,
127.940549532299)) ;
#142648 = CARTESIAN_POINT('Ctrl Pts',(-32.3129069984928,12.4976839055064,
127.730706441742)) ;
#142649 = CARTESIAN_POINT('Ctrl Pts',(-32.2171411071609,12.37947113767,127.483906316843)) ;
#142650 = CARTESIAN_POINT('Ctrl Pts',(-32.1132911001469,12.3351744205894,
127.21381155579)) ;
#142651 = CARTESIAN_POINT('Ctrl Pts',(-32.0094764720966,12.3695012767601,
126.943667978939)) ;
#142652 = CARTESIAN_POINT('Ctrl Pts',(-31.9122693293976,12.4786183713965,
126.69271538078)) ;
#142653 = CARTESIAN_POINT('Ctrl Pts',(-31.827183667738,12.6556201650726,126.477292320838)) ;
#142654 = CARTESIAN_POINT('Ctrl Pts',(-31.7599124151507,12.8885376927875,
126.314004677371)) ;
#142655 = CARTESIAN_POINT('Ctrl Pts',(-31.714947288412,13.1578672301346,126.215639088923)) ;
#142656 = CARTESIAN_POINT('Ctrl Pts',(-31.6941824964107,13.4488181207259,
126.188284587737)) ;
#142657 = CARTESIAN_POINT('Ctrl Pts',(-31.698897103108,13.7357351510131,126.235108130151)) ;
#142658 = CARTESIAN_POINT('Ctrl Pts',(-31.7274809073415,14.0000244491373,
126.351602120279)) ;
#142659 = CARTESIAN_POINT('Ctrl Pts',(-31.7778273453152,14.2248064092014,
126.531934807809)) ;
#142660 = CARTESIAN_POINT('Ctrl Pts',(-31.844851717,14.3907221874245,126.760746549466)) ;
#142661 = CARTESIAN_POINT('Ctrl Pts',(-31.9236967438235,14.4880878252355,
127.0242463843)) ;
#142662 = CARTESIAN_POINT('Ctrl Pts',(-32.0074797583405,14.5090844466389,
127.302065690259)) ;
#142663 = CARTESIAN_POINT('Ctrl Pts',(-32.0902772487515,14.4517330875411,
127.577253483703)) ;
#142664 = CARTESIAN_POINT('Ctrl Pts',(-32.1640651859993,14.3213872706393,
127.825792981418)) ;
#142665 = CARTESIAN_POINT('Ctrl Pts',(-32.2240068107159,14.1266125068475,
128.034020404948)) ;
#142666 = CARTESIAN_POINT('Ctrl Pts',(-32.2647640498464,13.8801112237431,
128.186345332148)) ;
#142667 = CARTESIAN_POINT('Ctrl Pts',(-32.2823576448507,13.6025838419119,
128.270778674212)) ;
#142668 = CARTESIAN_POINT('Ctrl Pts',(-32.2752642468574,13.3122087049322,
128.283106518981)) ;
#142669 = CARTESIAN_POINT('Ctrl Pts',(-32.2429269674404,13.0284663697123,
128.221843758155)) ;
#142670 = CARTESIAN_POINT('Ctrl Pts',(-32.1871815503845,12.7739763347418,
128.092081411688)) ;
#142671 = CARTESIAN_POINT('Ctrl Pts',(-32.111096935218,12.5655227594086,127.902962986094)) ;
#142672 = CARTESIAN_POINT('Ctrl Pts',(-32.0195990424995,12.4188417655465,
127.668765531469)) ;
#142673 = CARTESIAN_POINT('Ctrl Pts',(-31.9184991684207,12.343819791052,127.406496289624)) ;
#142674 = CARTESIAN_POINT('Ctrl Pts',(-31.8137079351686,12.3461750188478,
127.133605889349)) ;
#142675 = CARTESIAN_POINT('Ctrl Pts',(-31.7130252080803,12.4256200301873,
126.872547622651)) ;
#142676 = CARTESIAN_POINT('Ctrl Pts',(-31.6221469061099,12.5766361181176,
126.640220251546)) ;
#142677 = CARTESIAN_POINT('Ctrl Pts',(-31.547220653387,12.7882866055861,126.454465707021)) ;
#142678 = CARTESIAN_POINT('Ctrl Pts',(-31.492809784499,13.0452021106171,126.328621831613)) ;
#142679 = CARTESIAN_POINT('Ctrl Pts',(-31.4620208452283,13.3293878961544,
126.271809382364)) ;
#142680 = CARTESIAN_POINT('Ctrl Pts',(-31.4563957226866,13.6204037391964,
126.288518759348)) ;
#142681 = CARTESIAN_POINT('Ctrl Pts',(-31.4756176952845,13.8971497414612,
126.3778003854)) ;
#142682 = CARTESIAN_POINT('Ctrl Pts',(-31.5174981860061,14.1397539982186,
126.53324136256)) ;
#142683 = CARTESIAN_POINT('Ctrl Pts',(-31.5784731662082,14.3313465280224,
126.744521176888)) ;
#142684 = CARTESIAN_POINT('Ctrl Pts',(-31.6531070542541,14.4574458886048,
126.995592910948)) ;
#142685 = CARTESIAN_POINT('Ctrl Pts',(-31.7357182581869,14.509972396165,127.27004619928)) ;
#142686 = CARTESIAN_POINT('Ctrl Pts',(-31.8197265109475,14.4843439557881,
127.548664482844)) ;
#142687 = CARTESIAN_POINT('Ctrl Pts',(-31.8978809400863,14.3827749210334,
127.810067848139)) ;
#142688 = CARTESIAN_POINT('Ctrl Pts',(-31.9642304853554,14.2124739765949,
128.037017650735)) ;
#142689 = CARTESIAN_POINT('Ctrl Pts',(-32.0131976388995,13.9855789270548,
128.213188860414)) ;
#142690 = CARTESIAN_POINT('Ctrl Pts',(-32.0405543494933,13.7185805831256,
128.326209499296)) ;
#142691 = CARTESIAN_POINT('Ctrl Pts',(-32.0436331723574,13.4303185672317,
128.368322928117)) ;
#142692 = CARTESIAN_POINT('Ctrl Pts',(-32.0215333257744,13.1417758390937,
128.33685233434)) ;
#142693 = CARTESIAN_POINT('Ctrl Pts',(-31.9748976328392,12.8725286087569,
128.233815253822)) ;
#142694 = CARTESIAN_POINT('Ctrl Pts',(-31.9066058992129,12.6435096250976,
128.067418368168)) ;
#142695 = CARTESIAN_POINT('Ctrl Pts',(-31.8206856918917,12.470154617103,127.849547648784)) ;
#142696 = CARTESIAN_POINT('Ctrl Pts',(-31.7226433988074,12.3650501816311,
127.596245250201)) ;
#142697 = CARTESIAN_POINT('Ctrl Pts',(-31.6184519258737,12.3357586673989,
127.325066885764)) ;
#142698 = CARTESIAN_POINT('Ctrl Pts',(-31.5155220134888,12.3843195645159,
127.057439493129)) ;
#142699 = CARTESIAN_POINT('Ctrl Pts',(-31.4198179572413,12.5073667033233,
126.811011568101)) ;
#142700 = CARTESIAN_POINT('Ctrl Pts',(-31.3378940321144,12.695820098274,126.604784360148)) ;
#142701 = CARTESIAN_POINT('Ctrl Pts',(-31.2746568300074,12.9363650189031,
126.453164101291)) ;
#142702 = CARTESIAN_POINT('Ctrl Pts',(-31.2339861564669,13.2120463476192,
126.367497677483)) ;
#142703 = CARTESIAN_POINT('Ctrl Pts',(-31.218054736522,13.5022482408363,126.354027956631)) ;
#142704 = CARTESIAN_POINT('Ctrl Pts',(-31.2274123863003,13.788401757224,126.414636560072)) ;
#142705 = CARTESIAN_POINT('Ctrl Pts',(-31.2603056788409,14.0459452112238,
126.543679970572)) ;
#142706 = CARTESIAN_POINT('Ctrl Pts',(-31.3142676028335,14.261068186074,126.734589300308)) ;
#142707 = CARTESIAN_POINT('Ctrl Pts',(-31.3838448851807,14.4145624952327,
126.970825527176)) ;
#142708 = CARTESIAN_POINT('Ctrl Pts',(-31.464268747959,14.4980852442795,127.238979955351)) ;
#142709 = CARTESIAN_POINT('Ctrl Pts',(-31.5484155641688,14.5041312509629,
127.517917624269)) ;
#142710 = CARTESIAN_POINT('Ctrl Pts',(-31.6297274762448,14.4326961548768,
127.788594379386)) ;
#142711 = CARTESIAN_POINT('Ctrl Pts',(-31.7015057073872,14.2894246996344,
128.031337346009)) ;
#142712 = CARTESIAN_POINT('Ctrl Pts',(-31.7583243957012,14.0826506129639,
128.230601393984)) ;
#142713 = CARTESIAN_POINT('Ctrl Pts',(-31.7946301927493,13.8312289814619,
128.369572219819)) ;
#142714 = CARTESIAN_POINT('Ctrl Pts',(-31.8078849388079,13.5479803719868,
128.441553443391)) ;
#142715 = CARTESIAN_POINT('Ctrl Pts',(-31.7959085692955,13.257297898438,128.439638332041)) ;
#142716 = CARTESIAN_POINT('Ctrl Pts',(-31.7591260014045,12.9781390141801,
128.365290983036)) ;
#142717 = CARTESIAN_POINT('Ctrl Pts',(-31.6989001455544,12.7298469956755,
128.222623208126)) ;
#142718 = CARTESIAN_POINT('Ctrl Pts',(-31.619935033866,12.5331717504731,128.024890524041)) ;
#142719 = CARTESIAN_POINT('Ctrl Pts',(-31.5257553511796,12.3987049958051,
127.783005973355)) ;
#142720 = CARTESIAN_POINT('Ctrl Pts',(-31.4236240780026,12.3381977038027,
127.517686726716)) ;
#142721 = CARTESIAN_POINT('Ctrl Pts',(-31.3187777933959,12.3556286047268,
127.244711651246)) ;
#142722 = CARTESIAN_POINT('Ctrl Pts',(-31.2201199323636,12.4484986932729,
126.989359567954)) ;
#142723 = CARTESIAN_POINT('Ctrl Pts',(-31.1314620599124,12.6124652381156,
126.763652129256)) ;
#142724 = CARTESIAN_POINT('Ctrl Pts',(-31.0603390629678,12.833019455732,126.588870336055)) ;
#142725 = CARTESIAN_POINT('Ctrl Pts',(-31.0098757034308,13.0981217097557,
126.474765888058)) ;
#142726 = CARTESIAN_POINT('Ctrl Pts',(-30.9839541223414,13.3840424084956,
126.432032804447)) ;
#142727 = CARTESIAN_POINT('Ctrl Pts',(-30.9830184122512,13.673804350161,126.462424161424)) ;
#142728 = CARTESIAN_POINT('Ctrl Pts',(-31.0067064338544,13.9458856599705,
126.564772906119)) ;
#142729 = CARTESIAN_POINT('Ctrl Pts',(-31.0526563993131,14.1805609779054,
126.732191904978)) ;
#142730 = CARTESIAN_POINT('Ctrl Pts',(-31.1163979299656,14.3602096691543,
126.951417205331)) ;
#142731 = CARTESIAN_POINT('Ctrl Pts',(-31.1936186238981,14.47371465445,127.210313970921)) ;
#142732 = CARTESIAN_POINT('Ctrl Pts',(-31.276626453563,14.5109817362897,127.485775916908)) ;
#142733 = CARTESIAN_POINT('Ctrl Pts',(-31.3597859403266,14.4710234549687,
127.761794153221)) ;
#142734 = CARTESIAN_POINT('Ctrl Pts',(-31.4362807735142,14.3558611737084,
128.018385473721)) ;
#142735 = CARTESIAN_POINT('Ctrl Pts',(-31.4998116237642,14.173605953239,128.237140036393)) ;
#142736 = CARTESIAN_POINT('Ctrl Pts',(-31.5449540416273,13.9381264570577,
128.402093551021)) ;
#142737 = CARTESIAN_POINT('Ctrl Pts',(-31.5679255836761,13.6651920565378,
128.502359753407)) ;
#142738 = CARTESIAN_POINT('Ctrl Pts',(-31.5663255356321,13.3755914390975,
128.530759248685)) ;
#142739 = CARTESIAN_POINT('Ctrl Pts',(-31.5392380980967,13.0874856739398,
128.484939106277)) ;
#142740 = CARTESIAN_POINT('Ctrl Pts',(-31.4885879922083,12.8264336867777,
128.369908021904)) ;
#142741 = CARTESIAN_POINT('Ctrl Pts',(-31.4164911780433,12.6060973636301,
128.192486850099)) ;
#142742 = CARTESIAN_POINT('Ctrl Pts',(-31.3280152859864,12.4450312815742,
127.967079585755)) ;
#142743 = CARTESIAN_POINT('Ctrl Pts',(-31.2279193062099,12.3534665915943,
127.7079284228)) ;
#142744 = CARTESIAN_POINT('Ctrl Pts',(-31.1238917413468,12.3390030026154,
127.437059120732)) ;
#142745 = CARTESIAN_POINT('Ctrl Pts',(-31.0214731199007,12.4020393022516,
127.171054081183)) ;
#142746 = CARTESIAN_POINT('Ctrl Pts',(-30.9279202793389,12.5385712255671,
126.930915337845)) ;
#142747 = CARTESIAN_POINT('Ctrl Pts',(-30.8494032021172,12.7373374755761,
126.734540013757)) ;
#142748 = CARTESIAN_POINT('Ctrl Pts',(-30.7900716797921,12.9861208763485,
126.594372908603)) ;
#142749 = CARTESIAN_POINT('Ctrl Pts',(-30.7539485891286,13.2660912868939,
126.521974733773)) ;
#142750 = CARTESIAN_POINT('Ctrl Pts',(-30.7428010893841,13.5573229974737,
126.522542007644)) ;
#142751 = CARTESIAN_POINT('Ctrl Pts',(-30.7566839096316,13.8386954173301,
126.596197928137)) ;
#142752 = CARTESIAN_POINT('Ctrl Pts',(-30.7939147647464,14.0906009261112,
126.738098027588)) ;
#142753 = CARTESIAN_POINT('Ctrl Pts',(-30.8510431537068,14.2945041038628,
126.938095608529)) ;
#142754 = CARTESIAN_POINT('Ctrl Pts',(-30.9233443651782,14.4361574942565,
127.18244958177)) ;
#142755 = CARTESIAN_POINT('Ctrl Pts',(-31.0048336013044,14.5051117773277,
127.453630062579)) ;
#142756 = CARTESIAN_POINT('Ctrl Pts',(-31.0888759648342,14.4965825882903,
127.732236491623)) ;
#142757 = CARTESIAN_POINT('Ctrl Pts',(-31.168865676846,14.4113394048867,127.999016499472)) ;
#142758 = CARTESIAN_POINT('Ctrl Pts',(-31.2384933243905,14.2546478359796,
128.235636040619)) ;
#142759 = CARTESIAN_POINT('Ctrl Pts',(-31.2915451356608,14.0391437504434,
128.423680114953)) ;
#142760 = CARTESIAN_POINT('Ctrl Pts',(-31.3239067519199,13.7793415261531,
128.551331386748)) ;
#142761 = CARTESIAN_POINT('Ctrl Pts',(-31.3324639869936,13.4941094654563,
128.609429945624)) ;
#142762 = CARTESIAN_POINT('Ctrl Pts',(-31.3156967226184,13.2026873964626,
128.593682895648)) ;
#142763 = CARTESIAN_POINT('Ctrl Pts',(-31.274441049515,12.9288332689777,128.506175701619)) ;
#142764 = CARTESIAN_POINT('Ctrl Pts',(-31.2102613525706,12.6885083227908,
128.351964103388)) ;
#142765 = CARTESIAN_POINT('Ctrl Pts',(-31.1280360942476,12.5026390523848,
128.144753064434)) ;
#142766 = CARTESIAN_POINT('Ctrl Pts',(-31.0320401303252,12.3816810142256,
127.897469250246)) ;
#142767 = CARTESIAN_POINT('Ctrl Pts',(-30.9288964149733,12.3354826601101,
127.629243583753)) ;
#142768 = CARTESIAN_POINT('Ctrl Pts',(-30.8247552318205,12.3671988695935,
127.358221331888)) ;
#142769 = CARTESIAN_POINT('Ctrl Pts',(-30.7268557425413,12.4748749590594,
127.105391022476)) ;
#142770 = CARTESIAN_POINT('Ctrl Pts',(-30.6416225436775,12.6498955161038,
126.889454161025)) ;
#142771 = CARTESIAN_POINT('Ctrl Pts',(-30.5739773175829,12.8801431271714,
126.724918684966)) ;
#142772 = CARTESIAN_POINT('Ctrl Pts',(-30.5280533743189,13.1504415256103,
126.623977240751)) ;
#142773 = CARTESIAN_POINT('Ctrl Pts',(-30.5067059098186,13.4387392039499,
126.594642314902)) ;
#142774 = CARTESIAN_POINT('Ctrl Pts',(-30.5105905683589,13.7280473627643,
126.639272529026)) ;
#142775 = CARTESIAN_POINT('Ctrl Pts',(-30.5386531607722,13.9932362270437,
126.754260621585)) ;
#142776 = CARTESIAN_POINT('Ctrl Pts',(-30.5881891176015,14.2186784013421,
126.932092352736)) ;
#142777 = CARTESIAN_POINT('Ctrl Pts',(-30.6551326283065,14.3872014595801,
127.160834082923)) ;
#142778 = CARTESIAN_POINT('Ctrl Pts',(-30.7333872632998,14.4862165376707,
127.422454831296)) ;
#142779 = CARTESIAN_POINT('Ctrl Pts',(-30.8174140558742,14.5095010534955,
127.701112767902)) ;
#142780 = CARTESIAN_POINT('Ctrl Pts',(-30.8998260095477,14.4548476370639,
127.974954865684)) ;
#142781 = CARTESIAN_POINT('Ctrl Pts',(-30.9744919161141,14.3259645840264,
128.226282736462)) ;
#142782 = CARTESIAN_POINT('Ctrl Pts',(-31.0349033731148,14.132023950122,128.435947494583)) ;
#142783 = CARTESIAN_POINT('Ctrl Pts',(-31.0759430220492,13.8890686102105,
128.588794252599)) ;
#142784 = CARTESIAN_POINT('Ctrl Pts',(-31.0944376075796,13.6109286818878,
128.676030610899)) ;
#142785 = CARTESIAN_POINT('Ctrl Pts',(-31.0880487774346,13.3205779167508,
128.690415573638)) ;
#142786 = CARTESIAN_POINT('Ctrl Pts',(-31.0562963474654,13.0356408417454,
128.630948247247)) ;
#142787 = CARTESIAN_POINT('Ctrl Pts',(-31.0013892817443,12.7811566928917,
128.503497528563)) ;
#142788 = CARTESIAN_POINT('Ctrl Pts',(-30.9258694959649,12.5709849974497,
128.316035091874)) ;
#142789 = CARTESIAN_POINT('Ctrl Pts',(-30.8347412757522,12.4221765780121,
128.082924321767)) ;
#142790 = CARTESIAN_POINT('Ctrl Pts',(-30.7333975989525,12.3447406523641,
127.820082767003)) ;
#142791 = CARTESIAN_POINT('Ctrl Pts',(-30.6287619755561,12.3451621896592,
127.547596475717)) ;
#142792 = CARTESIAN_POINT('Ctrl Pts',(-30.5281543228765,12.4221618578868,
127.286667507964)) ;
#142793 = CARTESIAN_POINT('Ctrl Pts',(-30.4368045692654,12.5713294888185,
127.052995432794)) ;
#142794 = CARTESIAN_POINT('Ctrl Pts',(-30.361412617843,12.781135912573,126.86584125208)) ;
#142795 = CARTESIAN_POINT('Ctrl Pts',(-30.3062767402564,13.0373855963871,
126.73793450979)) ;
#142796 = CARTESIAN_POINT('Ctrl Pts',(-30.2748125276942,13.3202249658799,
126.679050724831)) ;
#142797 = CARTESIAN_POINT('Ctrl Pts',(-30.2684246244409,13.6126651184226,
126.693687161756)) ;
#142798 = CARTESIAN_POINT('Ctrl Pts',(-30.2869050355454,13.8891096825995,
126.780680178363)) ;
#142799 = CARTESIAN_POINT('Ctrl Pts',(-30.328241457162,14.1334577296797,126.934603321344)) ;
#142800 = CARTESIAN_POINT('Ctrl Pts',(-30.3884948782566,14.3262011562841,
127.143657768574)) ;
#142801 = CARTESIAN_POINT('Ctrl Pts',(-30.4632736474801,14.4552702569289,
127.395366894377)) ;
#142802 = CARTESIAN_POINT('Ctrl Pts',(-30.5458417500547,14.5094659908496,
127.669716069013)) ;
#142803 = CARTESIAN_POINT('Ctrl Pts',(-30.6293554000449,14.4862792648155,
127.946670555011)) ;
#142804 = CARTESIAN_POINT('Ctrl Pts',(-30.7080061524191,14.3867194046613,
128.209621341823)) ;
#142805 = CARTESIAN_POINT('Ctrl Pts',(-30.7747309805075,14.2183273088974,
128.437642777903)) ;
#142806 = CARTESIAN_POINT('Ctrl Pts',(-30.8243935899846,13.992244078071,128.615933560403)) ;
#142807 = CARTESIAN_POINT('Ctrl Pts',(-30.8523086752982,13.7260908725509,
128.730577525946)) ;
#142808 = CARTESIAN_POINT('Ctrl Pts',(-30.8561418503764,13.4392990631296,
128.774762803047)) ;
#142809 = CARTESIAN_POINT('Ctrl Pts',(-30.8346412184545,13.1491383959326,
128.745202054093)) ;
#142810 = CARTESIAN_POINT('Ctrl Pts',(-30.7888519514244,12.8801381500525,
128.644497302745)) ;
#142811 = CARTESIAN_POINT('Ctrl Pts',(-30.7208398901881,12.64883120769,128.479059560541)) ;
#142812 = CARTESIAN_POINT('Ctrl Pts',(-30.6357753911745,12.4746173054018,
128.26351619677)) ;
#142813 = CARTESIAN_POINT('Ctrl Pts',(-30.5377496366726,12.3669410554066,
128.010358301652)) ;
#142814 = CARTESIAN_POINT('Ctrl Pts',(-30.4336611805425,12.3355244461353,
127.739466951913)) ;
#142815 = CARTESIAN_POINT('Ctrl Pts',(-30.3306644329952,12.3818824720289,
127.4716321127)) ;
#142816 = CARTESIAN_POINT('Ctrl Pts',(-30.234825873423,12.5024424639559,127.224739910609)) ;
#142817 = CARTESIAN_POINT('Ctrl Pts',(-30.1520250480759,12.6900860834509,
127.0161141599)) ;
#142818 = CARTESIAN_POINT('Ctrl Pts',(-30.0883858330113,12.9290694340201,
126.863256044418)) ;
#142819 = CARTESIAN_POINT('Ctrl Pts',(-30.0470668431947,13.2033803581446,
126.775625804674)) ;
#142820 = CARTESIAN_POINT('Ctrl Pts',(-30.0303844725595,13.4938855393019,
126.760016339724)) ;
#142821 = CARTESIAN_POINT('Ctrl Pts',(-30.0389475792244,13.7798209622441,
126.818217155643)) ;
#142822 = CARTESIAN_POINT('Ctrl Pts',(-30.071382390156,14.0398148496058,126.946107608102)) ;
#142823 = CARTESIAN_POINT('Ctrl Pts',(-30.1246984855742,14.2555982023478,
127.135022862139)) ;
#142824 = CARTESIAN_POINT('Ctrl Pts',(-30.1938899332028,14.4112165805385,
127.370147971488)) ;
#142825 = CARTESIAN_POINT('Ctrl Pts',(-30.2744141343331,14.4969136071728,
127.638712469549)) ;
#142826 = CARTESIAN_POINT('Ctrl Pts',(-30.3581226245091,14.5049696606859,
127.916204012444)) ;
#142827 = CARTESIAN_POINT('Ctrl Pts',(-30.439571695334,14.4360248987559,128.187259104422)) ;
#142828 = CARTESIAN_POINT('Ctrl Pts',(-30.5117927626852,14.2945753095186,
128.431334289227)) ;
#142829 = CARTESIAN_POINT('Ctrl Pts',(-30.5691023350333,14.0897547152948,
128.631991536531)) ;
#142830 = CARTESIAN_POINT('Ctrl Pts',(-30.6061131460944,13.8386999371902,
128.773119766257)) ;
#142831 = CARTESIAN_POINT('Ctrl Pts',(-30.6200817649539,13.557404245294,128.847024010029)) ;
#142832 = CARTESIAN_POINT('Ctrl Pts',(-30.6087458782112,13.2644127915957,
128.847242565271)) ;
#142833 = CARTESIAN_POINT('Ctrl Pts',(-30.5727419671278,12.9862193835362,
128.774990539839)) ;
#142834 = CARTESIAN_POINT('Ctrl Pts',(-30.5133912275406,12.7371110279746,
128.634805043641)) ;
#142835 = CARTESIAN_POINT('Ctrl Pts',(-30.4346856662007,12.5380202146654,
128.437941656666)) ;
#142836 = CARTESIAN_POINT('Ctrl Pts',(-30.3408137582206,12.4015272035531,
128.196962918917)) ;
#142837 = CARTESIAN_POINT('Ctrl Pts',(-30.2387580740374,12.3389469979449,
127.931890728957)) ;
#142838 = CARTESIAN_POINT('Ctrl Pts',(-30.1344188320465,12.3537865285607,
127.66021882814)) ;
#142839 = CARTESIAN_POINT('Ctrl Pts',(-30.0348799647077,12.4449099781865,
127.402504219006)) ;
#142840 = CARTESIAN_POINT('Ctrl Pts',(-29.9458853225937,12.6072328334928,
127.175803032903)) ;
#142841 = CARTESIAN_POINT('Ctrl Pts',(-29.8743601595728,12.8259752277409,
126.999791081331)) ;
#142842 = CARTESIAN_POINT('Ctrl Pts',(-29.8232788134169,13.0894865992637,
126.883812376946)) ;
#142843 = CARTESIAN_POINT('Ctrl Pts',(-29.7965060135308,13.3763086885043,
126.838741513895)) ;
#142844 = CARTESIAN_POINT('Ctrl Pts',(-29.7949634120603,13.6661024734113,
126.867343704578)) ;
#142845 = CARTESIAN_POINT('Ctrl Pts',(-29.8178316934814,13.9378774690874,
126.967158551912)) ;
#142846 = CARTESIAN_POINT('Ctrl Pts',(-29.8633214379128,14.1747933111433,
127.133350479076)) ;
#142847 = CARTESIAN_POINT('Ctrl Pts',(-29.9265395417689,14.3556679919274,
127.350985685476)) ;
#142848 = CARTESIAN_POINT('Ctrl Pts',(-30.0030508632442,14.4711053285872,
127.6076521516)) ;
#142849 = CARTESIAN_POINT('Ctrl Pts',(-30.0865564445511,14.5111709794694,
127.884806852964)) ;
#142850 = CARTESIAN_POINT('Ctrl Pts',(-30.1699004127553,14.4729025358904,
128.161406819813)) ;
#142851 = CARTESIAN_POINT('Ctrl Pts',(-30.2462983206917,14.3605014207988,
128.417542568319)) ;
#142852 = CARTESIAN_POINT('Ctrl Pts',(-30.3106448741099,14.1789799465746,
128.63887062547)) ;
#142853 = CARTESIAN_POINT('Ctrl Pts',(-30.3561566067274,13.9453130634453,
128.804803369269)) ;
#142854 = CARTESIAN_POINT('Ctrl Pts',(-30.3798024914641,13.6736132719233,
128.906994396133)) ;
#142855 = CARTESIAN_POINT('Ctrl Pts',(-30.3789584446791,13.3843416076431,
128.937588844635)) ;
#142856 = CARTESIAN_POINT('Ctrl Pts',(-30.3526013931557,13.0956424209517,
128.893923674973)) ;
#142857 = CARTESIAN_POINT('Ctrl Pts',(-30.3026011006858,12.8335786861196,
128.780796985994)) ;
#142858 = CARTESIAN_POINT('Ctrl Pts',(-30.231053128041,12.611652190356,128.604987703306)) ;
#142859 = CARTESIAN_POINT('Ctrl Pts',(-30.1428236509105,12.4486057551385,
128.380351815953)) ;
#142860 = CARTESIAN_POINT('Ctrl Pts',(-30.0433319916567,12.3551665725231,
128.12284248329)) ;
#142861 = CARTESIAN_POINT('Ctrl Pts',(-29.939015371523,12.338311146402,127.851236266649)) ;
#142862 = CARTESIAN_POINT('Ctrl Pts',(-29.8366056665798,12.39913191908,127.585202385857)) ;
#142863 = CARTESIAN_POINT('Ctrl Pts',(-29.7427166487443,12.5336134533254,
127.344083270442)) ;
#142864 = CARTESIAN_POINT('Ctrl Pts',(-29.663675565517,12.7304748931974,127.146157836652)) ;
#142865 = CARTESIAN_POINT('Ctrl Pts',(-29.6033823042093,12.9801495362985,
127.003435636053)) ;
#142866 = CARTESIAN_POINT('Ctrl Pts',(-29.5669638511879,13.2569932871313,
126.929866029654)) ;
#142867 = CARTESIAN_POINT('Ctrl Pts',(-29.554951047838,13.5493203158773,126.928041183197)) ;
#142868 = CARTESIAN_POINT('Ctrl Pts',(-29.5681806364269,13.8310611217576,
126.999765211193)) ;
#142869 = CARTESIAN_POINT('Ctrl Pts',(-29.6048343695299,14.0843639820839,
127.14002065473)) ;
#142870 = CARTESIAN_POINT('Ctrl Pts',(-29.6614640820528,14.2896245798539,
127.338543409109)) ;
#142871 = CARTESIAN_POINT('Ctrl Pts',(-29.7332906010218,14.433006390985,127.581457172281)) ;
#142872 = CARTESIAN_POINT('Ctrl Pts',(-29.8146433905983,14.5042107644556,
127.852256910045)) ;
#142873 = CARTESIAN_POINT('Ctrl Pts',(-29.8987371113395,14.4979449677576,
128.131024343594)) ;
#142874 = CARTESIAN_POINT('Ctrl Pts',(-29.9791604149128,14.4144600975177,
128.399168008958)) ;
#142875 = CARTESIAN_POINT('Ctrl Pts',(-30.0490448554192,14.259520873967,128.636505696184)) ;
#142876 = CARTESIAN_POINT('Ctrl Pts',(-30.1024733512287,14.0462147796788,
128.825547199947)) ;
#142877 = CARTESIAN_POINT('Ctrl Pts',(-30.1355535398746,13.7868051984224,
128.955377427376)) ;
#142878 = CARTESIAN_POINT('Ctrl Pts',(-30.1447564168258,13.5027355977882,
129.015276777012)) ;
#142879 = CARTESIAN_POINT('Ctrl Pts',(-30.1288158056883,13.2114163358095,
129.001914025961)) ;
#142880 = CARTESIAN_POINT('Ctrl Pts',(-30.0880935176902,12.9359342039492,
128.916075180905)) ;
#142881 = CARTESIAN_POINT('Ctrl Pts',(-30.0247104416128,12.6951561372944,
128.764080699704)) ;
#142882 = CARTESIAN_POINT('Ctrl Pts',(-29.942963545196,12.5073060889563,128.558283375642)) ;
#142883 = CARTESIAN_POINT('Ctrl Pts',(-29.8471539839523,12.3841592537523,
128.311585634468)) ;
#142884 = CARTESIAN_POINT('Ctrl Pts',(-29.744101814774,12.3356200242118,128.043633158241)) ;
#142885 = CARTESIAN_POINT('Ctrl Pts',(-29.6395080858797,12.3655842342963,
127.771418882123)) ;
#142886 = CARTESIAN_POINT('Ctrl Pts',(-29.5421036027909,12.4702048662911,
127.519765293934)) ;
#142887 = CARTESIAN_POINT('Ctrl Pts',(-29.4557101506611,12.6448837990351,
127.300726057939)) ;
#142888 = CARTESIAN_POINT('Ctrl Pts',(-29.3879505080204,12.8725084203653,
127.135649765193)) ;
#142889 = CARTESIAN_POINT('Ctrl Pts',(-29.3410790256385,13.1434988264021,
127.03213773474)) ;
#142890 = CARTESIAN_POINT('Ctrl Pts',(-29.3192584705184,13.4301737730148,
127.001259274478)) ;
#142891 = CARTESIAN_POINT('Ctrl Pts',(-29.3222385561352,13.718779591721,127.043120453796)) ;
#142892 = CARTESIAN_POINT('Ctrl Pts',(-29.3498696871251,13.9870154535706,
127.157116456129)) ;
#142893 = CARTESIAN_POINT('Ctrl Pts',(-29.3986379964539,14.2124398495338,
127.3325193873)) ;
#142894 = CARTESIAN_POINT('Ctrl Pts',(-29.4650553209786,14.3830654639858,
127.559715415461)) ;
#142895 = CARTESIAN_POINT('Ctrl Pts',(-29.5434438005476,14.4846609671348,
127.821883558811)) ;
#142896 = CARTESIAN_POINT('Ctrl Pts',(-29.6274369403362,14.5097913596576,
128.100451442334)) ;
#142897 = CARTESIAN_POINT('Ctrl Pts',(-29.7096257062941,14.4576092834796,
128.373496593985)) ;
#142898 = CARTESIAN_POINT('Ctrl Pts',(-29.7848036126788,14.3304830753539,
128.626405753905)) ;
#142899 = CARTESIAN_POINT('Ctrl Pts',(-29.845566912938,14.1386182913456,128.837024720556)) ;
#142900 = CARTESIAN_POINT('Ctrl Pts',(-29.8872745466126,13.8965845637284,
128.991871079085)) ;
#142901 = CARTESIAN_POINT('Ctrl Pts',(-29.9064534682672,13.6198364139058,
129.081022786347)) ;
#142902 = CARTESIAN_POINT('Ctrl Pts',(-29.900787063049,13.3288843077371,129.097601934331)) ;
#142903 = CARTESIAN_POINT('Ctrl Pts',(-29.8699337024441,13.0447398144614,
129.040604983945)) ;
#142904 = CARTESIAN_POINT('Ctrl Pts',(-29.8156278311616,12.7881834818384,
128.91501253398)) ;
#142905 = CARTESIAN_POINT('Ctrl Pts',(-29.7402027720901,12.5755908845443,
128.727989057223)) ;
#142906 = CARTESIAN_POINT('Ctrl Pts',(-29.6498474075775,12.4257573634701,
128.496978543416)) ;
#142907 = CARTESIAN_POINT('Ctrl Pts',(-29.5489205160236,12.3460112100503,
128.235293254381)) ;
#142908 = CARTESIAN_POINT('Ctrl Pts',(-29.4441677154177,12.3439532777376,
127.962502290802)) ;
#142909 = CARTESIAN_POINT('Ctrl Pts',(-29.3431323111502,12.4188219737117,
127.700394231621)) ;
#142910 = CARTESIAN_POINT('Ctrl Pts',(-29.2511415646043,12.5668342389243,
127.464967305872)) ;
#142911 = CARTESIAN_POINT('Ctrl Pts',(-29.1756958712415,12.7739567012615,
127.277464266888)) ;
#142912 = CARTESIAN_POINT('Ctrl Pts',(-29.1197743038431,13.0292277214245,
127.147296176479)) ;
#142913 = CARTESIAN_POINT('Ctrl Pts',(-29.0875900956306,13.3121169680532,
127.086372454532)) ;
#142914 = CARTESIAN_POINT('Ctrl Pts',(-29.080439208884,13.603671342882,127.098665686775)) ;
#142915 = CARTESIAN_POINT('Ctrl Pts',(-29.0983297264476,13.8822011658837,
127.184109243225)) ;
#142916 = CARTESIAN_POINT('Ctrl Pts',(-29.1388833388726,14.1265341471654,
127.335581557334)) ;
#142917 = CARTESIAN_POINT('Ctrl Pts',(-29.1987356919885,14.3215277974717,
127.543539347123)) ;
#142918 = CARTESIAN_POINT('Ctrl Pts',(-29.273115428844,14.4523872873454,127.794044143669)) ;
#142919 = CARTESIAN_POINT('Ctrl Pts',(-29.3554651301705,14.509081275177,128.067728441316)) ;
#142920 = CARTESIAN_POINT('Ctrl Pts',(-29.4395851874039,14.4877530377578,
128.346676598338)) ;
#142921 = CARTESIAN_POINT('Ctrl Pts',(-29.5179673179766,14.3906972119634,
128.608633598773)) ;
#142922 = CARTESIAN_POINT('Ctrl Pts',(-29.5851982952717,14.2242126836462,
128.838160883835)) ;
#142923 = CARTESIAN_POINT('Ctrl Pts',(-29.635328017071,14.0000453573048,129.01774887383)) ;
#142924 = CARTESIAN_POINT('Ctrl Pts',(-29.6640587815373,13.7349940893193,
129.134772605438)) ;
#142925 = CARTESIAN_POINT('Ctrl Pts',(-29.66853047681,13.4462937932098,129.181082266472)) ;
#142926 = CARTESIAN_POINT('Ctrl Pts',(-29.6479806661709,13.1586523998495,
129.15397156145)) ;
#142927 = CARTESIAN_POINT('Ctrl Pts',(-29.6024908386361,12.8863235955885,
129.05444952426)) ;
#142928 = CARTESIAN_POINT('Ctrl Pts',(-29.5354346072489,12.6553854618845,
128.891574893748)) ;
#142929 = CARTESIAN_POINT('Ctrl Pts',(-29.450747956121,12.4787538622729,128.677195270721)) ;
#142930 = CARTESIAN_POINT('Ctrl Pts',(-29.3526089804549,12.3688114819393,
128.423824114578)) ;
#142931 = CARTESIAN_POINT('Ctrl Pts',(-29.2490412806159,12.3354319131045,
128.154314887623)) ;
#142932 = CARTESIAN_POINT('Ctrl Pts',(-29.1458394576041,12.3792576345139,
127.885902184127)) ;
#142933 = CARTESIAN_POINT('Ctrl Pts',(-29.04916679697,12.4988399158766,127.636776287795)) ;
#142934 = CARTESIAN_POINT('Ctrl Pts',(-28.9665629773405,12.6835118837374,
127.428475303792)) ;
#142935 = CARTESIAN_POINT('Ctrl Pts',(-28.9021265706556,12.9214924452222,
127.273355660426)) ;
#142936 = CARTESIAN_POINT('Ctrl Pts',(-28.8600821072398,13.1954917190088,
127.18365141452)) ;
#142937 = CARTESIAN_POINT('Ctrl Pts',(-28.842696665374,13.4865486647074,127.166068582976)) ;
#142938 = CARTESIAN_POINT('Ctrl Pts',(-28.850646619642,13.7724716992733,127.222433313962)) ;
#142939 = CARTESIAN_POINT('Ctrl Pts',(-28.8822838217838,14.0322260172615,
127.34784163249)) ;
#142940 = CARTESIAN_POINT('Ctrl Pts',(-28.9348883192046,14.249618629869,127.534639990214)) ;
#142941 = CARTESIAN_POINT('Ctrl Pts',(-29.0041241934943,14.4079187286369,
127.770094835747)) ;
#142942 = CARTESIAN_POINT('Ctrl Pts',(-29.0837267477703,14.4951289707047,
128.035675109478)) ;
#142943 = CARTESIAN_POINT('Ctrl Pts',(-29.1678434679254,14.5060206612055,
128.314536420415)) ;
#142944 = CARTESIAN_POINT('Ctrl Pts',(-29.2497073469964,14.4388851270518,
128.586900356964)) ;
#142945 = CARTESIAN_POINT('Ctrl Pts',(-29.3223025667751,14.2990478381217,
128.832099458619)) ;
#142946 = CARTESIAN_POINT('Ctrl Pts',(-29.3799249295879,14.0962769263581,
129.033581817066)) ;
#142947 = CARTESIAN_POINT('Ctrl Pts',(-29.4176290706378,13.8463550292072,
129.176742685336)) ;
#142948 = CARTESIAN_POINT('Ctrl Pts',(-29.4321974247897,13.5643760642883,
129.252539348112)) ;
#142949 = CARTESIAN_POINT('Ctrl Pts',(-29.4217829780266,13.2747378724678,
129.255060449538)) ;
#142950 = CARTESIAN_POINT('Ctrl Pts',(-29.3862948352972,12.9934295019574,
129.1846062214)) ;
#142951 = CARTESIAN_POINT('Ctrl Pts',(-29.3276375405367,12.7438066422354,
129.046365113135)) ;
#142952 = CARTESIAN_POINT('Ctrl Pts',(-29.2492689518633,12.542694227186,128.850560073051)) ;
#142953 = CARTESIAN_POINT('Ctrl Pts',(-29.156078800014,12.4046935574579,128.611449593072)) ;
#142954 = CARTESIAN_POINT('Ctrl Pts',(-29.0539430372178,12.3396331607935,
128.346227666517)) ;
#142955 = CARTESIAN_POINT('Ctrl Pts',(-28.9496962563366,12.3522551180279,
128.074782981399)) ;
#142956 = CARTESIAN_POINT('Ctrl Pts',(-28.849926492838,12.4411586824075,127.816395883758)) ;
#142957 = CARTESIAN_POINT('Ctrl Pts',(-28.7605590312039,12.6013770610415,
127.588581938705)) ;
#142958 = CARTESIAN_POINT('Ctrl Pts',(-28.6883543070743,12.819071741669,127.410650651919)) ;
#142959 = CARTESIAN_POINT('Ctrl Pts',(-28.6367460501826,13.0807347129293,
127.293025418326)) ;
#142960 = CARTESIAN_POINT('Ctrl Pts',(-28.6091712936872,13.3675409458687,
127.245666864385)) ;
#142961 = CARTESIAN_POINT('Ctrl Pts',(-28.6067914289987,13.6570979950049,
127.271760239889)) ;
#142962 = CARTESIAN_POINT('Ctrl Pts',(-28.6292800088116,13.9319894333905,
127.370771892158)) ;
#142963 = CARTESIAN_POINT('Ctrl Pts',(-28.6737114216624,14.1676085516927,
127.5335038352)) ;
#142964 = CARTESIAN_POINT('Ctrl Pts',(-28.7369049369059,14.3519029701599,
127.751335315566)) ;
#142965 = CARTESIAN_POINT('Ctrl Pts',(-28.8129872581851,14.4687263887883,
128.006656410294)) ;
#142966 = CARTESIAN_POINT('Ctrl Pts',(-28.8961104028969,14.5110206737837,
128.282595596457)) ;
#142967 = CARTESIAN_POINT('Ctrl Pts',(-28.9795137356919,14.475483911121,128.559339823648)) ;
#142968 = CARTESIAN_POINT('Ctrl Pts',(-29.0567266802165,14.3641243915887,
128.818105203385)) ;
#142969 = CARTESIAN_POINT('Ctrl Pts',(-29.120945343812,14.185998118253,129.038755013211)) ;
#142970 = CARTESIAN_POINT('Ctrl Pts',(-29.1673724631696,13.9527739610766,
129.207530855678)) ;
#142971 = CARTESIAN_POINT('Ctrl Pts',(-29.1916772905069,13.6818171752754,
129.311643144904)) ;
#142972 = CARTESIAN_POINT('Ctrl Pts',(-29.191513082233,13.392345635537,129.344277671689)) ;
#142973 = CARTESIAN_POINT('Ctrl Pts',(-29.1660326258556,13.1044624962765,
129.303028370569)) ;
#142974 = CARTESIAN_POINT('Ctrl Pts',(-29.1164519209928,12.8400819723837,
129.191300221752)) ;
#142975 = CARTESIAN_POINT('Ctrl Pts',(-29.0456199048285,12.6174282729713,
129.017485608075)) ;
#142976 = CARTESIAN_POINT('Ctrl Pts',(-28.9576757901538,12.452181454216,128.793738916405)) ;
#142977 = CARTESIAN_POINT('Ctrl Pts',(-28.8583760496555,12.3567834927398,
128.536796874985)) ;
#142978 = CARTESIAN_POINT('Ctrl Pts',(-28.7543916660935,12.3377092342152,
128.266071088682)) ;
#142979 = CARTESIAN_POINT('Ctrl Pts',(-28.6517324722958,12.396207648245,127.999337715851)) ;
#142980 = CARTESIAN_POINT('Ctrl Pts',(-28.5572877270569,12.5290433262916,
127.756671538889)) ;
#142981 = CARTESIAN_POINT('Ctrl Pts',(-28.4778718732435,12.7244086521529,
127.557638995965)) ;
#142982 = CARTESIAN_POINT('Ctrl Pts',(-28.4172847882494,12.970950220754,127.41382234341)) ;
#142983 = CARTESIAN_POINT('Ctrl Pts',(-28.3797659678261,13.24944047257,127.337320504979)) ;
#142984 = CARTESIAN_POINT('Ctrl Pts',(-28.3671847047696,13.5418969111079,
127.333850245581)) ;
#142985 = CARTESIAN_POINT('Ctrl Pts',(-28.3796755155786,13.8230885860474,
127.403291738133)) ;
#142986 = CARTESIAN_POINT('Ctrl Pts',(-28.4156802442814,14.0775912623992,
127.541659056659)) ;
#142987 = CARTESIAN_POINT('Ctrl Pts',(-28.4717102355528,14.2842120208938,
127.738388350272)) ;
#142988 = CARTESIAN_POINT('Ctrl Pts',(-28.5432604389653,14.4299776255762,
127.980546699844)) ;
#142989 = CARTESIAN_POINT('Ctrl Pts',(-28.6248137961591,14.5033310573158,
128.252079015529)) ;
#142990 = CARTESIAN_POINT('Ctrl Pts',(-28.7083919312205,14.4992417521952,
128.529128681056)) ;
#142991 = CARTESIAN_POINT('Ctrl Pts',(-28.7892681436748,14.4177938992537,
128.79869937182)) ;
#142992 = CARTESIAN_POINT('Ctrl Pts',(-28.8593764558841,14.2650804914184,
129.036610653591)) ;
#142993 = CARTESIAN_POINT('Ctrl Pts',(-28.9134147220646,14.0529680000281,
129.227490443514)) ;
#142994 = CARTESIAN_POINT('Ctrl Pts',(-28.9471011414545,13.7955268691578,
129.3589796482)) ;
#142995 = CARTESIAN_POINT('Ctrl Pts',(-28.9570776705698,13.5095707979293,
129.421414389121)) ;
#142996 = CARTESIAN_POINT('Ctrl Pts',(-28.9417243006281,13.2189035142274,
129.409677362568)) ;
#142997 = CARTESIAN_POINT('Ctrl Pts',(-28.9018277588826,12.9437119836813,
129.326137208322)) ;
#142998 = CARTESIAN_POINT('Ctrl Pts',(-28.8391939509021,12.7018112503585,
129.17628858698)) ;
#142999 = CARTESIAN_POINT('Ctrl Pts',(-28.7575688794774,12.5115374305282,
128.970987035415)) ;
#143000 = CARTESIAN_POINT('Ctrl Pts',(-28.6622219712875,12.3865362301687,
128.725579337275)) ;
#143001 = CARTESIAN_POINT('Ctrl Pts',(-28.5587510574966,12.3360647675439,
128.456580284187)) ;
#143002 = CARTESIAN_POINT('Ctrl Pts',(-28.4555305358195,12.3630945112241,
128.187903732276)) ;
#143003 = CARTESIAN_POINT('Ctrl Pts',(-28.3566879058951,12.466576968382,127.932449994111)) ;
#143004 = CARTESIAN_POINT('Ctrl Pts',(-28.2706251997226,12.6378737412179,
127.714064371724)) ;
#143005 = CARTESIAN_POINT('Ctrl Pts',(-28.2016344309745,12.8661806777279,
127.545715311069)) ;
#143006 = CARTESIAN_POINT('Ctrl Pts',(-28.1545836946371,13.133327748888,127.441304758509)) ;
#143007 = CARTESIAN_POINT('Ctrl Pts',(-28.1316798850368,13.4221934769942,
127.407563269515)) ;
#143008 = CARTESIAN_POINT('Ctrl Pts',(-28.1340477421079,13.7107571262916,
127.447593177881)) ;
#143009 = CARTESIAN_POINT('Ctrl Pts',(-28.1609619636342,13.9798563789946,
127.559489257503)) ;
#143010 = CARTESIAN_POINT('Ctrl Pts',(-28.2093006124176,14.2070905645433,
127.733705392524)) ;
#143011 = CARTESIAN_POINT('Ctrl Pts',(-28.2752017753927,14.3790287585347,
127.959331880187)) ;
#143012 = CARTESIAN_POINT('Ctrl Pts',(-28.3530820320636,14.4826462603949,
128.219918375423)) ;
#143013 = CARTESIAN_POINT('Ctrl Pts',(-28.4373112880813,14.5101765741511,
128.49929849806)) ;
#143014 = CARTESIAN_POINT('Ctrl Pts',(-28.519474085672,14.4602520915312,128.772202055633)) ;
#143015 = CARTESIAN_POINT('Ctrl Pts',(-28.5950471255898,14.3349862853441,
129.026308923663)) ;
#143016 = CARTESIAN_POINT('Ctrl Pts',(-28.6560285639578,14.1459035788167,
129.237399512473)) ;
#143017 = CARTESIAN_POINT('Ctrl Pts',(-28.698619817941,13.9042673527481,129.394971716019)) ;
#143018 = CARTESIAN_POINT('Ctrl Pts',(-28.7184673372425,13.6274932797063,
129.486151626671)) ;
#143019 = CARTESIAN_POINT('Ctrl Pts',(-28.7135006465235,13.3375399739688,
129.504678260935)) ;
#143020 = CARTESIAN_POINT('Ctrl Pts',(-28.6834932097191,13.0529654851711,
129.450131261485)) ;
#143021 = CARTESIAN_POINT('Ctrl Pts',(-28.6292897606013,12.7935418575334,
129.325100800843)) ;
#143022 = CARTESIAN_POINT('Ctrl Pts',(-28.5550549856277,12.5815360245405,
129.141238342052)) ;
#143023 = CARTESIAN_POINT('Ctrl Pts',(-28.4646576427796,12.4287257654979,
128.910282719979)) ;
#143024 = CARTESIAN_POINT('Ctrl Pts',(-28.363677082995,12.3470719681604,128.64850632388)) ;
#143025 = CARTESIAN_POINT('Ctrl Pts',(-28.2591488468396,12.3430683476044,
128.376304331127)) ;
#143026 = CARTESIAN_POINT('Ctrl Pts',(-28.1582862016969,12.4155936903918,
128.114589342041)) ;
#143027 = CARTESIAN_POINT('Ctrl Pts',(-28.0661544614373,12.5608877107137,
127.878647626776)) ;
#143028 = CARTESIAN_POINT('Ctrl Pts',(-27.9897622819606,12.76729595803,127.688541378532)) ;
#143029 = CARTESIAN_POINT('Ctrl Pts',(-27.9331944991847,13.021989825902,127.556534508152)) ;
#143030 = CARTESIAN_POINT('Ctrl Pts',(-27.9004198086109,13.303543839919,127.493791149837)) ;
#143031 = CARTESIAN_POINT('Ctrl Pts',(-27.8925042874101,13.5948424473805,
127.503816308611)) ;
#143032 = CARTESIAN_POINT('Ctrl Pts',(-27.9096152355407,13.8739531403396,
127.586963478625)) ;
#143033 = CARTESIAN_POINT('Ctrl Pts',(-27.9496646620447,14.1203175585331,
127.737068535428)) ;
#143034 = CARTESIAN_POINT('Ctrl Pts',(-28.0090231272187,14.3167169570115,
127.943561552684)) ;
#143035 = CARTESIAN_POINT('Ctrl Pts',(-28.0828620310095,14.4494067343281,
128.192402472001)) ;
#143036 = CARTESIAN_POINT('Ctrl Pts',(-28.1651717407411,14.5084702765568,
128.466017783128)) ;
#143037 = CARTESIAN_POINT('Ctrl Pts',(-28.2490683969256,14.4897007225782,
128.744200921648)) ;
#143038 = CARTESIAN_POINT('Ctrl Pts',(-28.3280752188241,14.3946105615284,
129.008131391206)) ;
#143039 = CARTESIAN_POINT('Ctrl Pts',(-28.3958042440866,14.2294634797175,
129.23917393567)) ;
#143040 = CARTESIAN_POINT('Ctrl Pts',(-28.4463272391741,14.0073333338193,
129.419816794305)) ;
#143041 = CARTESIAN_POINT('Ctrl Pts',(-28.4757409397969,13.743582797636,129.538801386051)) ;
#143042 = CARTESIAN_POINT('Ctrl Pts',(-28.4810001371008,13.4548247152231,
129.587459496954)) ;
#143043 = CARTESIAN_POINT('Ctrl Pts',(-28.461059887965,13.1663898310179,129.562197963423)) ;
#143044 = CARTESIAN_POINT('Ctrl Pts',(-28.41656739466,12.8948251828515,129.465387320094)) ;
#143045 = CARTESIAN_POINT('Ctrl Pts',(-28.3499271169494,12.661361440579,129.303861114263)) ;
#143046 = CARTESIAN_POINT('Ctrl Pts',(-28.2654515362701,12.4827884895572,
129.090166702319)) ;
#143047 = CARTESIAN_POINT('Ctrl Pts',(-28.1681467304688,12.3713199015498,
128.839048548618)) ;
#143048 = CARTESIAN_POINT('Ctrl Pts',(-28.0645799433211,12.3351536533699,
128.569574159567)) ;
#143049 = CARTESIAN_POINT('Ctrl Pts',(-27.9607827823663,12.3771106009455,
128.299581621144)) ;
#143050 = CARTESIAN_POINT('Ctrl Pts',(-27.8644780082732,12.4937460494275,
128.051299065574)) ;
#143051 = CARTESIAN_POINT('Ctrl Pts',(-27.7810699349148,12.6767291591256,
127.840739185193)) ;
#143052 = CARTESIAN_POINT('Ctrl Pts',(-27.7157445671607,12.9147363341255,
127.683191915483)) ;
#143053 = CARTESIAN_POINT('Ctrl Pts',(-27.6732296957668,13.1870897744472,
127.59199890341)) ;
#143054 = CARTESIAN_POINT('Ctrl Pts',(-27.6550770827887,13.4771403047647,
127.572086844516)) ;
#143055 = CARTESIAN_POINT('Ctrl Pts',(-27.6622219471036,13.7642377896945,
127.626175179984)) ;
#143056 = CARTESIAN_POINT('Ctrl Pts',(-27.6934344667264,14.0261140993903,
127.750502240094)) ;
#143057 = CARTESIAN_POINT('Ctrl Pts',(-27.7452532633533,14.2437566933168,
127.934829589344)) ;
#143058 = CARTESIAN_POINT('Ctrl Pts',(-27.814130143941,14.4043005148666,128.169276756387)) ;
#143059 = CARTESIAN_POINT('Ctrl Pts',(-27.8935228607594,14.4936452056158,
128.434244053094)) ;
#143060 = CARTESIAN_POINT('Ctrl Pts',(-27.9775948902962,14.5067755080675,
128.712972810078)) ;
#143061 = CARTESIAN_POINT('Ctrl Pts',(-28.0595004608224,14.4421250993153,
128.98539905036)) ;
#143062 = CARTESIAN_POINT('Ctrl Pts',(-28.1325782921938,14.3039890578845,
129.232076923519)) ;
#143063 = CARTESIAN_POINT('Ctrl Pts',(-28.1904918232912,14.1040920585568,
129.434238070627)) ;
#143064 = CARTESIAN_POINT('Ctrl Pts',(-28.2291431873281,13.8535850410252,
129.580412255891)) ;
#143065 = CARTESIAN_POINT('Ctrl Pts',(-28.2443210492215,13.573095030684,129.657872655295)) ;
#143066 = CARTESIAN_POINT('Ctrl Pts',(-28.2346408638536,13.2829859633842,
129.662599052892)) ;
#143067 = CARTESIAN_POINT('Ctrl Pts',(-28.1999752849308,13.0017735288795,
129.594458814166)) ;
#143068 = CARTESIAN_POINT('Ctrl Pts',(-28.1417676131385,12.7500889121872,
129.457648777599)) ;
#143069 = CARTESIAN_POINT('Ctrl Pts',(-28.0639229564631,12.5475576765503,
129.263351153657)) ;
#143070 = CARTESIAN_POINT('Ctrl Pts',(-27.9709828123923,12.4075651763914,
129.02500225527)) ;
#143071 = CARTESIAN_POINT('Ctrl Pts',(-27.8693506787333,12.3405227195362,
128.761141757557)) ;
#143072 = CARTESIAN_POINT('Ctrl Pts',(-27.7648049873815,12.3506976033877,
128.488907346772)) ;
#143073 = CARTESIAN_POINT('Ctrl Pts',(-27.6644555408828,12.4381775614935,
128.228958563771)) ;
#143074 = CARTESIAN_POINT('Ctrl Pts',(-27.5751702428162,12.5958828969702,
128.001218540191)) ;
#143075 = CARTESIAN_POINT('Ctrl Pts',(-27.502283193488,12.8123888981795,127.821351130497)) ;
#143076 = CARTESIAN_POINT('Ctrl Pts',(-27.450031586974,13.0732935402693,127.701864848652)) ;
#143077 = CARTESIAN_POINT('Ctrl Pts',(-27.4217776748689,13.3601445566741,
127.652571547418)) ;
#143078 = CARTESIAN_POINT('Ctrl Pts',(-27.418773970736,13.6487325565986,127.676717562199)) ;
#143079 = CARTESIAN_POINT('Ctrl Pts',(-27.4403379990912,13.9231969676619,
127.772866432049)) ;
#143080 = CARTESIAN_POINT('Ctrl Pts',(-27.4843681376287,14.161664923211,127.934621131012)) ;
#143081 = CARTESIAN_POINT('Ctrl Pts',(-27.5471256039461,14.3474885312589,
128.151168293149)) ;
#143082 = CARTESIAN_POINT('Ctrl Pts',(-27.6228649944064,14.4664584642889,
128.405473991337)) ;
#143083 = CARTESIAN_POINT('Ctrl Pts',(-27.7062638841247,14.5109046596075,
128.682368151807)) ;
#143084 = CARTESIAN_POINT('Ctrl Pts',(-27.7893507587579,14.4775384051983,
128.958029757662)) ;
#143085 = CARTESIAN_POINT('Ctrl Pts',(-27.8669709430451,14.3681997153804,
129.218037882252)) ;
#143086 = CARTESIAN_POINT('Ctrl Pts',(-27.9316058833016,14.1916180826176,
129.439912282084)) ;
#143087 = CARTESIAN_POINT('Ctrl Pts',(-27.9785106186434,13.9603525000671,
129.610001559058)) ;
#143088 = CARTESIAN_POINT('Ctrl Pts',(-28.0035618824634,13.6895220896488,
129.716380788557)) ;
#143089 = CARTESIAN_POINT('Ctrl Pts',(-28.0040495835783,13.4007319535163,
129.750868768487)) ;
#143090 = CARTESIAN_POINT('Ctrl Pts',(-27.9794449922936,13.1132078069033,
129.712088512607)) ;
#143091 = CARTESIAN_POINT('Ctrl Pts',(-27.9302630163752,12.846606824237,129.601692481036)) ;
#143092 = CARTESIAN_POINT('Ctrl Pts',(-27.8603417733815,12.623698437481,129.430363738554)) ;
#143093 = CARTESIAN_POINT('Ctrl Pts',(-27.772694620763,12.4561011636242,129.207550748791)) ;
#143094 = CARTESIAN_POINT('Ctrl Pts',(-27.6737731829943,12.3585967931485,
128.951668241225)) ;
#143095 = CARTESIAN_POINT('Ctrl Pts',(-27.5695149442883,12.3371246783343,
128.680247071619)) ;
#143096 = CARTESIAN_POINT('Ctrl Pts',(-27.466838847916,12.3935413864574,128.413427301181)) ;
#143097 = CARTESIAN_POINT('Ctrl Pts',(-27.3723658112914,12.5236724613545,
128.170561312785)) ;
#143098 = CARTESIAN_POINT('Ctrl Pts',(-27.2920858688792,12.7179305396398,
127.969133189608)) ;
#143099 = CARTESIAN_POINT('Ctrl Pts',(-27.2307490661673,12.9643002141067,
127.823241817984)) ;
#143100 = CARTESIAN_POINT('Ctrl Pts',(-27.1927875893493,13.2410163015689,
127.74530764181)) ;
#143101 = CARTESIAN_POINT('Ctrl Pts',(-27.1794002354583,13.5320328266363,
127.739328215748)) ;
#143102 = CARTESIAN_POINT('Ctrl Pts',(-27.1911525976807,13.8151978209727,
127.806773844443)) ;
#143103 = CARTESIAN_POINT('Ctrl Pts',(-27.226570298699,14.0709652782984,127.943449594362)) ;
#143104 = CARTESIAN_POINT('Ctrl Pts',(-27.2822196281639,14.2795163173677,
128.139134706522)) ;
#143105 = CARTESIAN_POINT('Ctrl Pts',(-27.3532889376274,14.4266234403896,
128.379816035706)) ;
#143106 = CARTESIAN_POINT('Ctrl Pts',(-27.4341580000532,14.5021445242865,
128.649158484748)) ;
#143107 = CARTESIAN_POINT('Ctrl Pts',(-27.5183881057503,14.5004798974739,
128.928367380574)) ;
#143108 = CARTESIAN_POINT('Ctrl Pts',(-27.5992329747341,14.4210757518903,
129.197760560483)) ;
#143109 = CARTESIAN_POINT('Ctrl Pts',(-27.6694923473982,14.2711636067417,
129.435985416657)) ;
#143110 = CARTESIAN_POINT('Ctrl Pts',(-27.7243575187803,14.0600318658462,
129.629403124372)) ;
#143111 = CARTESIAN_POINT('Ctrl Pts',(-27.7587068568811,13.8025044724255,
129.762955028685)) ;
#143112 = CARTESIAN_POINT('Ctrl Pts',(-27.7693309736884,13.5194348559979,
129.827002883379)) ;
#143113 = CARTESIAN_POINT('Ctrl Pts',(-27.7548332219261,13.2279296915562,
129.817849904189)) ;
#143114 = CARTESIAN_POINT('Ctrl Pts',(-27.7155874618165,12.9514278673655,
129.736271623692)) ;
#143115 = CARTESIAN_POINT('Ctrl Pts',(-27.653314484704,12.7076269304905,129.587584820316)) ;
#143116 = CARTESIAN_POINT('Ctrl Pts',(-27.572509924976,12.5164543303433,129.384536694103)) ;
#143117 = CARTESIAN_POINT('Ctrl Pts',(-27.4772456621855,12.3891143614251,
129.139458063282)) ;
#143118 = CARTESIAN_POINT('Ctrl Pts',(-27.3744497556545,12.3364756135891,
128.872254272894)) ;
#143119 = CARTESIAN_POINT('Ctrl Pts',(-27.2704082203507,12.3612642379946,
128.601421099459)) ;
#143120 = CARTESIAN_POINT('Ctrl Pts',(-27.1713773382745,12.4629839046161,
128.345404662449)) ;
#143121 = CARTESIAN_POINT('Ctrl Pts',(-27.0851007677242,12.6321971909499,
128.126327881533)) ;
#143122 = CARTESIAN_POINT('Ctrl Pts',(-27.015641032897,12.8584558944589,127.956532197619)) ;
#143123 = CARTESIAN_POINT('Ctrl Pts',(-26.9676850720169,13.126164869302,127.84965606525)) ;
#143124 = CARTESIAN_POINT('Ctrl Pts',(-26.9442084970736,13.4141234527586,
127.814163915492)) ;
#143125 = CARTESIAN_POINT('Ctrl Pts',(-26.9458709815039,13.7023852281616,
127.852074256674)) ;
#143126 = CARTESIAN_POINT('Ctrl Pts',(-26.9718751244399,13.9714211958417,
127.961170070242)) ;
#143127 = CARTESIAN_POINT('Ctrl Pts',(-27.0200293376702,14.2020200814189,
128.135130194059)) ;
#143128 = CARTESIAN_POINT('Ctrl Pts',(-27.0853698779214,14.3750071777218,
128.359015009443)) ;
#143129 = CARTESIAN_POINT('Ctrl Pts',(-27.1629746883779,14.4806351397631,
128.618798290785)) ;
#143130 = CARTESIAN_POINT('Ctrl Pts',(-27.2467360159308,14.5105855300703,
128.896650717923)) ;
#143131 = CARTESIAN_POINT('Ctrl Pts',(-27.3295913980905,14.4625550533332,
129.171811865125)) ;
#143132 = CARTESIAN_POINT('Ctrl Pts',(-27.4050082321251,14.3400369090667,
129.425253916033)) ;
#143133 = CARTESIAN_POINT('Ctrl Pts',(-27.4667526234034,14.1521956958397,
129.638700651972)) ;
#143134 = CARTESIAN_POINT('Ctrl Pts',(-27.509920728559,13.9116488292757,129.797965117592)) ;
#143135 = CARTESIAN_POINT('Ctrl Pts',(-27.5304424424998,13.6358543135724,
129.891087447677)) ;
#143136 = CARTESIAN_POINT('Ctrl Pts',(-27.5262343520398,13.3459426369887,
129.911837713114)) ;
#143137 = CARTESIAN_POINT('Ctrl Pts',(-27.4968203591533,13.0604648346963,
129.859083942663)) ;
#143138 = CARTESIAN_POINT('Ctrl Pts',(-27.4436406639866,12.8015142493302,
129.736839092141)) ;
#143139 = CARTESIAN_POINT('Ctrl Pts',(-27.3697110305104,12.5868713096869,
129.554007522395)) ;
#143140 = CARTESIAN_POINT('Ctrl Pts',(-27.2796913738203,12.432303139715,129.324145798948)) ;
#143141 = CARTESIAN_POINT('Ctrl Pts',(-27.1792802958715,12.3486039806668,
129.063923184096)) ;
#143142 = CARTESIAN_POINT('Ctrl Pts',(-27.0747302802551,12.3418345477554,
128.791666168228)) ;
#143143 = CARTESIAN_POINT('Ctrl Pts',(-26.9730648540773,12.4127258480294,
128.527813593233)) ;
#143144 = CARTESIAN_POINT('Ctrl Pts',(-26.8810202662406,12.5554431662894,
128.291966182553)) ;
#143145 = CARTESIAN_POINT('Ctrl Pts',(-26.8038302880742,12.7608030962308,
128.099638464274)) ;
#143146 = CARTESIAN_POINT('Ctrl Pts',(-26.7467082859449,13.0143081230203,
127.965989241137)) ;
#143147 = CARTESIAN_POINT('Ctrl Pts',(-26.713205468323,13.29536631424,127.901127763773)) ;
#143148 = CARTESIAN_POINT('Ctrl Pts',(-26.7045894976719,13.5874993963847,
127.909194608933)) ;
#143149 = CARTESIAN_POINT('Ctrl Pts',(-26.7211066559591,13.8669340437894,
127.990583783677)) ;
#143150 = CARTESIAN_POINT('Ctrl Pts',(-26.7603551603999,14.1134264974216,
128.13820542311)) ;
#143151 = CARTESIAN_POINT('Ctrl Pts',(-26.8193522325074,14.312178191849,128.34373825684)) ;
#143152 = CARTESIAN_POINT('Ctrl Pts',(-26.8931267445792,14.447005080599,128.592489132649)) ;
#143153 = CARTESIAN_POINT('Ctrl Pts',(-26.9751504369521,14.50780864275,128.865206484874)) ;
#143154 = CARTESIAN_POINT('Ctrl Pts',(-27.0588159564451,14.4913412466958,
129.142606878717)) ;
#143155 = CARTESIAN_POINT('Ctrl Pts',(-27.1380385087885,14.3985298499944,
129.40715742329)) ;
#143156 = CARTESIAN_POINT('Ctrl Pts',(-27.2062467307682,14.23537642446,129.639608049856)) ;
#143157 = CARTESIAN_POINT('Ctrl Pts',(-27.2575581083356,14.0132823702427,
129.822743994824)) ;
#143158 = CARTESIAN_POINT('Ctrl Pts',(-27.2873688840562,13.7517705184138,
129.942709762938)) ;
#143159 = CARTESIAN_POINT('Ctrl Pts',(-27.293472251736,13.4639004109061,129.993782745323)) ;
#143160 = CARTESIAN_POINT('Ctrl Pts',(-27.2740851665503,13.1736259239267,
129.970325135161)) ;
#143161 = CARTESIAN_POINT('Ctrl Pts',(-27.2305215118996,12.9029494163379,
129.876022131441)) ;
#143162 = CARTESIAN_POINT('Ctrl Pts',(-27.1642896249734,12.6670694779248,
129.715817346972)) ;
#143163 = CARTESIAN_POINT('Ctrl Pts',(-27.0800464564361,12.4867414541686,
129.502856286838)) ;
#143164 = CARTESIAN_POINT('Ctrl Pts',(-26.9834820409465,12.3736046966953,
129.253747171097)) ;
#143165 = CARTESIAN_POINT('Ctrl Pts',(-26.879418915152,12.3351061358333,128.983013182515)) ;
#143166 = CARTESIAN_POINT('Ctrl Pts',(-26.7762312191263,12.3747297398712,
128.714574685413)) ;
#143167 = CARTESIAN_POINT('Ctrl Pts',(-26.6793849366064,12.4890530278271,
128.46477378363)) ;
#143168 = CARTESIAN_POINT('Ctrl Pts',(-26.5950275521023,12.671847392328,128.251667519718)) ;
#143169 = CARTESIAN_POINT('Ctrl Pts',(-26.5296066139418,12.9071471276995,
128.093622284971)) ;
#143170 = CARTESIAN_POINT('Ctrl Pts',(-26.4862925849143,13.1791584028572,
128.000158541116)) ;
#143171 = CARTESIAN_POINT('Ctrl Pts',(-26.4674803411247,13.4685703859445,
127.978264630818)) ;
#143172 = CARTESIAN_POINT('Ctrl Pts',(-26.4738622862666,13.7556866314948,
128.030081960704)) ;
#143173 = CARTESIAN_POINT('Ctrl Pts',(-26.5043022522006,14.0184521546514,
128.152120496671)) ;
#143174 = CARTESIAN_POINT('Ctrl Pts',(-26.5558322179965,14.2386836272176,
128.335773179578)) ;
#143175 = CARTESIAN_POINT('Ctrl Pts',(-26.6243219235215,14.4009245820624,
128.569075258418)) ;
#143176 = CARTESIAN_POINT('Ctrl Pts',(-26.7037459041493,14.4923209355322,
128.834232583563)) ;
#143177 = CARTESIAN_POINT('Ctrl Pts',(-26.7873700011777,14.5074993707076,
129.111483360412)) ;
#143178 = CARTESIAN_POINT('Ctrl Pts',(-26.869769976205,14.4446390736038,129.38550037864)) ;
#143179 = CARTESIAN_POINT('Ctrl Pts',(-26.942794278446,14.3090137807522,129.63184995493)) ;
#143180 = CARTESIAN_POINT('Ctrl Pts',(-27.001348624657,14.1104147854154,129.835955195458)) ;
#143181 = CARTESIAN_POINT('Ctrl Pts',(-27.0405182096425,13.8614586698981,
129.983581974093)) ;
#143182 = CARTESIAN_POINT('Ctrl Pts',(-27.0564545067552,13.5819684927305,
130.063220990945)) ;
#143183 = CARTESIAN_POINT('Ctrl Pts',(-27.0474617770525,13.2906276884224,
130.070095552532)) ;
#143184 = CARTESIAN_POINT('Ctrl Pts',(-27.0134271462375,13.0092431055299,
130.003763417619)) ;
#143185 = CARTESIAN_POINT('Ctrl Pts',(-26.9561897398293,12.7575166399562,
129.869627977763)) ;
#143186 = CARTESIAN_POINT('Ctrl Pts',(-26.878600427533,12.5525238857448,129.676201545283)) ;
#143187 = CARTESIAN_POINT('Ctrl Pts',(-26.786267640891,12.4108769573351,129.439535650803)) ;
#143188 = CARTESIAN_POINT('Ctrl Pts',(-26.6844582304523,12.3412908932615,
129.175275636481)) ;
#143189 = CARTESIAN_POINT('Ctrl Pts',(-26.5800334572457,12.3493862056845,
128.903348153925)) ;
#143190 = CARTESIAN_POINT('Ctrl Pts',(-26.4797393076399,12.434272868394,128.643467145807)) ;
#143191 = CARTESIAN_POINT('Ctrl Pts',(-26.3898901908696,12.5900490117304,
128.414124382121)) ;
#143192 = CARTESIAN_POINT('Ctrl Pts',(-26.3162603078544,12.8056267290578,
128.232173964895)) ;
#143193 = CARTESIAN_POINT('Ctrl Pts',(-26.2634623259816,13.065385008078,128.111066358889)) ;
#143194 = CARTESIAN_POINT('Ctrl Pts',(-26.2345041414233,13.3504852311182,
128.059568931144)) ;
#143195 = CARTESIAN_POINT('Ctrl Pts',(-26.2307238031498,13.6412799194347,
128.081681426423)) ;
#143196 = CARTESIAN_POINT('Ctrl Pts',(-26.2516126185945,13.9155482376954,
128.175749664471)) ;
#143197 = CARTESIAN_POINT('Ctrl Pts',(-26.2949893624843,14.1552942576475,
128.335588778516)) ;
#143198 = CARTESIAN_POINT('Ctrl Pts',(-26.3572525364643,14.3429102218091,
128.550683951018)) ;
#143199 = CARTESIAN_POINT('Ctrl Pts',(-26.4327879058784,14.4639893151741,
128.804436412996)) ;
#143200 = CARTESIAN_POINT('Ctrl Pts',(-26.5157245235423,14.5107279947802,
129.079841196809)) ;
#143201 = CARTESIAN_POINT('Ctrl Pts',(-26.599342755531,14.4794893711203,129.357238144724)) ;
#143202 = CARTESIAN_POINT('Ctrl Pts',(-26.6768758741317,14.3727211556821,
129.616834198873)) ;
#143203 = CARTESIAN_POINT('Ctrl Pts',(-26.742126370631,14.1977799605459,129.840578904122)) ;
#143204 = CARTESIAN_POINT('Ctrl Pts',(-26.7896263521605,13.9680803092071,
130.012384935134)) ;
#143205 = CARTESIAN_POINT('Ctrl Pts',(-26.8154360590847,13.6967826979273,
130.121139587608)) ;
#143206 = CARTESIAN_POINT('Ctrl Pts',(-26.8165967221177,13.4094043760134,
130.157455368201)) ;
#143207 = CARTESIAN_POINT('Ctrl Pts',(-26.7926969292554,13.1212039235338,
130.120777584093)) ;
#143208 = CARTESIAN_POINT('Ctrl Pts',(-26.7444083705524,12.8546896055266,
130.012858824521)) ;
#143209 = CARTESIAN_POINT('Ctrl Pts',(-26.6749139207326,12.6293810119528,
129.842883806981)) ;
#143210 = CARTESIAN_POINT('Ctrl Pts',(-26.5872220070184,12.4594635136683,
129.62009200021)) ;
#143211 = CARTESIAN_POINT('Ctrl Pts',(-26.4890425150724,12.3604529147884,
129.366204449936)) ;
#143212 = CARTESIAN_POINT('Ctrl Pts',(-26.3845073686079,12.3366695110087,
129.094084042648)) ;
#143213 = CARTESIAN_POINT('Ctrl Pts',(-26.2821289297751,12.3907630911244,
128.827994581518)) ;
#143214 = CARTESIAN_POINT('Ctrl Pts',(-26.187128095685,12.5187718172597,128.583638766626)) ;
#143215 = CARTESIAN_POINT('Ctrl Pts',(-26.1060949547663,12.7125554078675,
128.380162610462)) ;
#143216 = CARTESIAN_POINT('Ctrl Pts',(-26.0447561615951,12.9551209833767,
128.233921001561)) ;
#143217 = CARTESIAN_POINT('Ctrl Pts',(-26.0057078064282,13.2325621685243,
128.153002106468)) ;
#143218 = CARTESIAN_POINT('Ctrl Pts',(-25.9916571139282,13.5243421587289,
128.145175592515)) ;
#143219 = CARTESIAN_POINT('Ctrl Pts',(-26.0026775791259,13.8069928303566,
128.210366181038)) ;
#143220 = CARTESIAN_POINT('Ctrl Pts',(-26.0374047644475,14.0639001821586,
128.345024781301)) ;
#143221 = CARTESIAN_POINT('Ctrl Pts',(-26.0925147260829,14.274156022816,128.539139181305)) ;
#143222 = CARTESIAN_POINT('Ctrl Pts',(-26.1633735273204,14.4234616465823,
128.779279376222)) ;
#143223 = CARTESIAN_POINT('Ctrl Pts',(-26.2439599577869,14.5011170980349,
129.047753483437)) ;
#143224 = CARTESIAN_POINT('Ctrl Pts',(-26.3285030639104,14.501361448933,129.328007829175)) ;
#143225 = CARTESIAN_POINT('Ctrl Pts',(-26.4088108195145,14.4249955787507,
129.595519956069)) ;
#143226 = CARTESIAN_POINT('Ctrl Pts',(-26.4800874345285,14.2760170248169,
129.836998320279)) ;
#143227 = CARTESIAN_POINT('Ctrl Pts',(-26.5352515744716,14.0665440737742,
130.031218298945)) ;
#143228 = CARTESIAN_POINT('Ctrl Pts',(-26.5702400842864,13.8110526556412,
130.166533147419)) ;
#143229 = CARTESIAN_POINT('Ctrl Pts',(-26.5815726590234,13.5262784611541,
130.232906371947)) ;
#143230 = CARTESIAN_POINT('Ctrl Pts',(-26.5678635340945,13.2368368163846,
130.225803590966)) ;
#143231 = CARTESIAN_POINT('Ctrl Pts',(-26.5291217423332,12.9583254451164,
130.145867702787)) ;
#143232 = CARTESIAN_POINT('Ctrl Pts',(-26.4678331545185,12.7145798984787,
129.999860683866)) ;
#143233 = CARTESIAN_POINT('Ctrl Pts',(-26.3867440068472,12.5201729680917,
129.796286454842)) ;
#143234 = CARTESIAN_POINT('Ctrl Pts',(-26.2927852183014,12.3922976801848,
129.554661598127)) ;
#143235 = CARTESIAN_POINT('Ctrl Pts',(-26.1895660009278,12.3368042006491,
129.28641664148)) ;
#143236 = CARTESIAN_POINT('Ctrl Pts',(-26.0858016380748,12.3594079761625,
129.016280828409)) ;
#143237 = CARTESIAN_POINT('Ctrl Pts',(-25.9864031337543,12.458842653819,128.759223963542)) ;
#143238 = CARTESIAN_POINT('Ctrl Pts',(-25.8996090906676,12.6263833262832,
128.538666355053)) ;
#143239 = CARTESIAN_POINT('Ctrl Pts',(-25.8295827174989,12.8513078347283,
128.367225899866)) ;
#143240 = CARTESIAN_POINT('Ctrl Pts',(-25.781006901016,13.1175342113745,128.258472258186)) ;
#143241 = CARTESIAN_POINT('Ctrl Pts',(-25.7567380807917,13.4059955031651,
128.220766348)) ;
#143242 = CARTESIAN_POINT('Ctrl Pts',(-25.7576446857111,13.6942419631863,
128.256424466659)) ;
#143243 = CARTESIAN_POINT('Ctrl Pts',(-25.7832873182616,13.9656571301542,
128.36468485081)) ;
#143244 = CARTESIAN_POINT('Ctrl Pts',(-25.8302149885515,14.1945698171883,
128.53461018047)) ;
#143245 = CARTESIAN_POINT('Ctrl Pts',(-25.895500840112,14.3711224521538,128.758593840646)) ;
#143246 = CARTESIAN_POINT('Ctrl Pts',(-25.9728377548636,14.4785950112144,
129.017572340248)) ;
#143247 = CARTESIAN_POINT('Ctrl Pts',(-26.056604347087,14.5108133119048,129.295478786872)) ;
#143248 = CARTESIAN_POINT('Ctrl Pts',(-26.1394268468674,14.465039412922,129.570481762383)) ;
#143249 = CARTESIAN_POINT('Ctrl Pts',(-26.2151348850256,14.3446919180205,
129.824767484077)) ;
#143250 = CARTESIAN_POINT('Ctrl Pts',(-26.2774107699029,14.1586507475217,
130.039773742848)) ;
#143251 = CARTESIAN_POINT('Ctrl Pts',(-26.3212982659288,13.9182141888542,
130.201285607756)) ;
#143252 = CARTESIAN_POINT('Ctrl Pts',(-26.3423778627286,13.6446893381856,
130.295847000978)) ;
#143253 = CARTESIAN_POINT('Ctrl Pts',(-26.3389066565706,13.3538162430507,
130.318882585942)) ;
#143254 = CARTESIAN_POINT('Ctrl Pts',(-26.3102603550136,13.0687528103835,
130.268268932066)) ;
#143255 = CARTESIAN_POINT('Ctrl Pts',(-26.2576977023151,12.808402450481,130.147871722525)) ;
#143256 = CARTESIAN_POINT('Ctrl Pts',(-26.1843413480049,12.5923661463697,
129.966695992935)) ;
#143257 = CARTESIAN_POINT('Ctrl Pts',(-26.0945780045174,12.4355966192842,
129.737634921388)) ;
#143258 = CARTESIAN_POINT('Ctrl Pts',(-25.9941838470144,12.3498833858894,
129.477517705028)) ;
#143259 = CARTESIAN_POINT('Ctrl Pts',(-25.8901883755494,12.3409543002999,
129.206711463543)) ;
#143260 = CARTESIAN_POINT('Ctrl Pts',(-25.7882740958192,12.4093757985287,
128.942149411662)) ;
#143261 = CARTESIAN_POINT('Ctrl Pts',(-25.6956212849253,12.5505197572112,
128.704612922647)) ;
#143262 = CARTESIAN_POINT('Ctrl Pts',(-25.6180396767608,12.7541804700571,
128.511108725249)) ;
#143263 = CARTESIAN_POINT('Ctrl Pts',(-25.5604107173287,13.0055269427028,
128.375859916493)) ;
#143264 = CARTESIAN_POINT('Ctrl Pts',(-25.526031444965,13.2870727031463,128.308567998837)) ;
#143265 = CARTESIAN_POINT('Ctrl Pts',(-25.5167159350328,13.5781356431356,
128.314465472164)) ;
#143266 = CARTESIAN_POINT('Ctrl Pts',(-25.532383711498,13.8583664416102,128.393378284334)) ;
#143267 = CARTESIAN_POINT('Ctrl Pts',(-25.5712031763481,14.1072756620479,
128.539909138783)) ;
#143268 = CARTESIAN_POINT('Ctrl Pts',(-25.6295827662988,14.3069767003197,
128.743547855544)) ;
#143269 = CARTESIAN_POINT('Ctrl Pts',(-25.7026733511847,14.4436141295833,
128.990173698217)) ;
#143270 = CARTESIAN_POINT('Ctrl Pts',(-25.7848004053856,14.5071928211091,
129.263307294218)) ;
#143271 = CARTESIAN_POINT('Ctrl Pts',(-25.8687007298245,14.4928944928021,
129.541467990308)) ;
#143272 = CARTESIAN_POINT('Ctrl Pts',(-25.9481227868581,14.4021254320443,
129.80659518902)) ;
#143273 = CARTESIAN_POINT('Ctrl Pts',(-26.0165481319324,14.2413769659717,
130.039584245616)) ;
#143274 = CARTESIAN_POINT('Ctrl Pts',(-26.0684809468175,14.0210257728375,
130.224528199235)) ;
#143275 = CARTESIAN_POINT('Ctrl Pts',(-26.0991009049518,13.7594507578406,
130.346988630004)) ;
#143276 = CARTESIAN_POINT('Ctrl Pts',(-26.1058130306325,13.4716752359127,
130.399870698281)) ;
#143277 = CARTESIAN_POINT('Ctrl Pts',(-26.0873198572873,13.1827800209618,
130.378837828388)) ;
#143278 = CARTESIAN_POINT('Ctrl Pts',(-26.0442075196764,12.9097866027274,
130.286041057869)) ;
#143279 = CARTESIAN_POINT('Ctrl Pts',(-25.9789209888468,12.6739760958484,
130.128405961843)) ;
#143280 = CARTESIAN_POINT('Ctrl Pts',(-25.8950644284899,12.4911376309814,
129.916641264972)) ;
#143281 = CARTESIAN_POINT('Ctrl Pts',(-25.7982306766349,12.375575879239,129.666921135392)) ;
#143282 = CARTESIAN_POINT('Ctrl Pts',(-25.6948872153544,12.3352662333604,
129.398091075705)) ;
#143283 = CARTESIAN_POINT('Ctrl Pts',(-25.591475557297,12.3722006124299,129.129028993969)) ;
#143284 = CARTESIAN_POINT('Ctrl Pts',(-25.4936430630205,12.4858118700224,
128.876611173075)) ;
#143285 = CARTESIAN_POINT('Ctrl Pts',(-25.4097931267157,12.6649628036957,
128.664617898589)) ;
#143286 = CARTESIAN_POINT('Ctrl Pts',(-25.3434171037584,12.8995424395387,
128.503913243776)) ;
#143287 = CARTESIAN_POINT('Ctrl Pts',(-25.2994520917775,13.1707490219764,
128.408538167925)) ;
#143288 = CARTESIAN_POINT('Ctrl Pts',(-25.2798667180845,13.4602465795,128.384422935853)) ;
#143289 = CARTESIAN_POINT('Ctrl Pts',(-25.2855719032732,13.7479094630808,
128.434283282751)) ;
#143290 = CARTESIAN_POINT('Ctrl Pts',(-25.3152873758232,14.0110934234083,
128.554137674801)) ;
#143291 = CARTESIAN_POINT('Ctrl Pts',(-25.3662625164448,14.233019589697,128.736189009337)) ;
#143292 = CARTESIAN_POINT('Ctrl Pts',(-25.4343591120224,14.3970564643661,
128.968346310512)) ;
#143293 = CARTESIAN_POINT('Ctrl Pts',(-25.5132805122452,14.4906411189315,
129.231930680055)) ;
#143294 = CARTESIAN_POINT('Ctrl Pts',(-25.5973959591667,14.5080280038905,
129.510833611735)) ;
#143295 = CARTESIAN_POINT('Ctrl Pts',(-25.6792022536452,14.4480724922228,
129.782803145259)) ;
#143296 = CARTESIAN_POINT('Ctrl Pts',(-25.7531141454623,14.3139469642534,
130.031971871347)) ;
#143297 = CARTESIAN_POINT('Ctrl Pts',(-25.8121272678128,14.1169436134283,
130.237401395038)) ;
#143298 = CARTESIAN_POINT('Ctrl Pts',(-25.8519851660838,13.8684680278967,
130.387129822211)) ;
#143299 = CARTESIAN_POINT('Ctrl Pts',(-25.8685225668081,13.5907241662415,
130.468386340342)) ;
#143300 = CARTESIAN_POINT('Ctrl Pts',(-25.8603228056423,13.2994060447749,
130.477583630266)) ;
#143301 = CARTESIAN_POINT('Ctrl Pts',(-25.827036095678,13.0173300828137,130.413443066431)) ;
#143302 = CARTESIAN_POINT('Ctrl Pts',(-25.7701669280763,12.7634585275692,
130.280523268416)) ;
#143303 = CARTESIAN_POINT('Ctrl Pts',(-25.6931351589582,12.5574052301983,
130.088675092408)) ;
#143304 = CARTESIAN_POINT('Ctrl Pts',(-25.6014237918118,12.4141337315889,
129.853734516058)) ;
#143305 = CARTESIAN_POINT('Ctrl Pts',(-25.4997017590006,12.3422331852162,
129.589762284572)) ;
#143306 = CARTESIAN_POINT('Ctrl Pts',(-25.3953738695026,12.3479816705834,
129.318078617136)) ;
#143307 = CARTESIAN_POINT('Ctrl Pts',(-25.2947149038502,12.4308509408022,
129.057186959594)) ;
#143308 = CARTESIAN_POINT('Ctrl Pts',(-25.2047058731085,12.5841343909331,
128.827278360344)) ;
#143309 = CARTESIAN_POINT('Ctrl Pts',(-25.1301965858679,12.7991565720161,
128.642914315101)) ;
#143310 = CARTESIAN_POINT('Ctrl Pts',(-25.0769545406197,13.0570001115815,
128.520387169891)) ;
#143311 = CARTESIAN_POINT('Ctrl Pts',(-25.0472058635231,13.3421922466227,
128.466652040374)) ;
#143312 = CARTESIAN_POINT('Ctrl Pts',(-25.0426624131729,13.6321455836602,
128.486417781107)) ;
#143313 = CARTESIAN_POINT('Ctrl Pts',(-25.0629539703241,13.9089726379876,
128.57895542738)) ;
#143314 = CARTESIAN_POINT('Ctrl Pts',(-25.1059158440566,14.1498189010042,
128.73760438917)) ;
#143315 = CARTESIAN_POINT('Ctrl Pts',(-25.1672896859518,14.3379335627546,
128.949882671248)) ;
#143316 = CARTESIAN_POINT('Ctrl Pts',(-25.2427067211349,14.4615825928275,
129.203386921482)) ;
#143317 = CARTESIAN_POINT('Ctrl Pts',(-25.3254735430017,14.5104718340286,
129.478271233911)) ;
#143318 = CARTESIAN_POINT('Ctrl Pts',(-25.4093890445753,14.4813917007992,
129.756623752072)) ;
#143319 = CARTESIAN_POINT('Ctrl Pts',(-25.487125210729,14.376410140061,130.016808097636)) ;
#143320 = CARTESIAN_POINT('Ctrl Pts',(-25.5525788833299,14.2041612959408,
130.241003440752)) ;
#143321 = CARTESIAN_POINT('Ctrl Pts',(-25.6008773224437,13.974383981629,130.415342708694)) ;
#143322 = CARTESIAN_POINT('Ctrl Pts',(-25.6271719709242,13.7063210465707,
130.525219374997)) ;
#143323 = CARTESIAN_POINT('Ctrl Pts',(-25.6291300522666,13.4167011729611,
130.56416290139)) ;
#143324 = CARTESIAN_POINT('Ctrl Pts',(-25.6058960644918,13.1291677764475,
130.529317082054)) ;
#143325 = CARTESIAN_POINT('Ctrl Pts',(-25.5583125907459,12.8617102719658,
130.423460313947)) ;
#143326 = CARTESIAN_POINT('Ctrl Pts',(-25.4893078563168,12.6350478347594,
130.254927988591)) ;
#143327 = CARTESIAN_POINT('Ctrl Pts',(-25.4024730274085,12.4638699496821,
130.034490107221)) ;
#143328 = CARTESIAN_POINT('Ctrl Pts',(-25.3040512171019,12.3621126749229,
129.780067190961)) ;
#143329 = CARTESIAN_POINT('Ctrl Pts',(-25.1997380119896,12.336288295009,129.508540465744)) ;
#143330 = CARTESIAN_POINT('Ctrl Pts',(-25.0970121081987,12.3882079371413,
129.241501944942)) ;
#143331 = CARTESIAN_POINT('Ctrl Pts',(-25.0016211651868,12.5148240574062,
128.996060126096)) ;
#143332 = CARTESIAN_POINT('Ctrl Pts',(-24.920756965554,12.7050813508199,128.792787218599)) ;
#143333 = CARTESIAN_POINT('Ctrl Pts',(-24.8582697031265,12.9482678416441,
128.64346188212)) ;
#143334 = CARTESIAN_POINT('Ctrl Pts',(-24.8187646180453,13.2238579668187,
128.56105516626)) ;
#143335 = CARTESIAN_POINT('Ctrl Pts',(-24.803905764497,13.5162934097049,128.550961928654)) ;
#143336 = CARTESIAN_POINT('Ctrl Pts',(-24.8142217184009,13.7991654054394,
128.614056451591)) ;
#143337 = CARTESIAN_POINT('Ctrl Pts',(-24.848496068521,14.0580269319691,128.747523628204)) ;
#143338 = CARTESIAN_POINT('Ctrl Pts',(-24.9028546228909,14.2686029381806,
128.939273431809)) ;
#143339 = CARTESIAN_POINT('Ctrl Pts',(-24.9732407127939,14.419961933364,129.178011411683)) ;
#143340 = CARTESIAN_POINT('Ctrl Pts',(-25.0537195338019,14.49989585267,129.446209462079)) ;
#143341 = CARTESIAN_POINT('Ctrl Pts',(-25.1381655958701,14.5025664525356,
129.726139589141)) ;
#143342 = CARTESIAN_POINT('Ctrl Pts',(-25.2188788130462,14.4280651994865,
129.994934028458)) ;
#143343 = CARTESIAN_POINT('Ctrl Pts',(-25.2902271151953,14.2819176182956,
130.236459424966)) ;
#143344 = CARTESIAN_POINT('Ctrl Pts',(-25.346349360693,14.0723875526179,130.433740928495)) ;
#143345 = CARTESIAN_POINT('Ctrl Pts',(-25.3816831121814,13.8191593341655,
130.569884981309)) ;
#143346 = CARTESIAN_POINT('Ctrl Pts',(-25.3938278972864,13.5356700868247,
130.638556719779)) ;
#143347 = CARTESIAN_POINT('Ctrl Pts',(-25.3808456816373,13.2451624741664,
130.633688514316)) ;
#143348 = CARTESIAN_POINT('Ctrl Pts',(-25.3427850618204,12.9658957798679,
130.555749230615)) ;
#143349 = CARTESIAN_POINT('Ctrl Pts',(-25.2820224790504,12.7208678253265,
130.41130505217)) ;
#143350 = CARTESIAN_POINT('Ctrl Pts',(-25.2019014171005,12.5256177762791,
130.210380825888)) ;
#143351 = CARTESIAN_POINT('Ctrl Pts',(-25.1077011701678,12.3947248965929,
129.968261731413)) ;
#143352 = CARTESIAN_POINT('Ctrl Pts',(-25.0046214201826,12.3373274071284,
129.700414239671)) ;
#143353 = CARTESIAN_POINT('Ctrl Pts',(-24.9009929151909,12.3577351595859,
129.430619982872)) ;
#143354 = CARTESIAN_POINT('Ctrl Pts',(-24.8015282893426,12.4546492902735,
129.173300985343)) ;
#143355 = CARTESIAN_POINT('Ctrl Pts',(-24.7139128643915,12.6210677035252,
128.950492831251)) ;
#143356 = CARTESIAN_POINT('Ctrl Pts',(-24.6434512146242,12.8446767267699,
128.777764271832)) ;
#143357 = CARTESIAN_POINT('Ctrl Pts',(-24.5943806100842,13.1088081967542,
128.667427010549)) ;
#143358 = CARTESIAN_POINT('Ctrl Pts',(-24.5692555646321,13.3979062800969,
128.627333437601)) ;
#143359 = CARTESIAN_POINT('Ctrl Pts',(-24.5695431905959,13.6859097693729,
128.6611363567)) ;
#143360 = CARTESIAN_POINT('Ctrl Pts',(-24.594157481065,13.9567565274245,128.766182296297)) ;
#143361 = CARTESIAN_POINT('Ctrl Pts',(-24.6411416936085,14.1899349081331,
128.936706868906)) ;
#143362 = CARTESIAN_POINT('Ctrl Pts',(-24.7053594546824,14.3662692594446,
129.157216214963)) ;
#143363 = CARTESIAN_POINT('Ctrl Pts',(-24.782903699173,14.4768289977238,129.417032620335)) ;
#143364 = CARTESIAN_POINT('Ctrl Pts',(-24.866384635766,14.5109207097569,129.694010170453)) ;
#143365 = CARTESIAN_POINT('Ctrl Pts',(-24.9494158435752,14.4673589922836,
129.96966777721)) ;
#143366 = CARTESIAN_POINT('Ctrl Pts',(-25.0253981397071,14.3490297985362,
130.224741120684)) ;
#143367 = CARTESIAN_POINT('Ctrl Pts',(-25.0881434075069,14.1643442277036,
130.441156584524)) ;
#143368 = CARTESIAN_POINT('Ctrl Pts',(-25.1323829486443,13.9269540267458,
130.603466456372)) ;
#143369 = CARTESIAN_POINT('Ctrl Pts',(-25.1543475264281,13.6529086343547,
130.700783789999)) ;
#143370 = CARTESIAN_POINT('Ctrl Pts',(-25.1515873002568,13.3625039506586,
130.725856091348)) ;
#143371 = CARTESIAN_POINT('Ctrl Pts',(-25.123624185757,13.0764916582392,130.677299559346)) ;
#143372 = CARTESIAN_POINT('Ctrl Pts',(-25.0717015091459,12.8152456791565,
130.558760811629)) ;
#143373 = CARTESIAN_POINT('Ctrl Pts',(-24.9988762003653,12.5977359905825,
130.37913851997)) ;
#143374 = CARTESIAN_POINT('Ctrl Pts',(-24.9096025778513,12.439230107941,130.151471731367)) ;
#143375 = CARTESIAN_POINT('Ctrl Pts',(-24.8094482485441,12.3513755687183,
129.892051831185)) ;
#143376 = CARTESIAN_POINT('Ctrl Pts',(-24.7055184930905,12.339931649505,129.621419546249)) ;
#143377 = CARTESIAN_POINT('Ctrl Pts',(-24.6026979852918,12.4070555048895,
129.3544642037)) ;
#143378 = CARTESIAN_POINT('Ctrl Pts',(-24.510580365153,12.5451371061637,129.118182642952)) ;
#143379 = CARTESIAN_POINT('Ctrl Pts',(-24.432124078182,12.7477728516222,128.922258912151)) ;
#143380 = CARTESIAN_POINT('Ctrl Pts',(-24.3739511399616,12.9979369346779,
128.785397374143)) ;
#143381 = CARTESIAN_POINT('Ctrl Pts',(-24.3388401109884,13.2792373127526,
128.716009070394)) ;
#143382 = CARTESIAN_POINT('Ctrl Pts',(-24.3288627638645,13.570158269964,128.719955082171)) ;
#143383 = CARTESIAN_POINT('Ctrl Pts',(-24.3438038378766,13.850537969179,128.796691496782)) ;
#143384 = CARTESIAN_POINT('Ctrl Pts',(-24.382009729182,14.1007514006134,128.941447794759)) ;
#143385 = CARTESIAN_POINT('Ctrl Pts',(-24.4399060508627,14.302171677131,129.143685734349)) ;
#143386 = CARTESIAN_POINT('Ctrl Pts',(-24.5128915120813,14.4410638896651,
129.390101505646)) ;
#143387 = CARTESIAN_POINT('Ctrl Pts',(-24.5948014466677,14.5064205925433,
129.662568824423)) ;
#143388 = CARTESIAN_POINT('Ctrl Pts',(-24.6784736579456,14.4944296430568,
129.939960176772)) ;
#143389 = CARTESIAN_POINT('Ctrl Pts',(-24.7583064519586,14.405561123776,130.206367062894)) ;
#143390 = CARTESIAN_POINT('Ctrl Pts',(-24.8269294458247,14.2469874685197,
130.439848204688)) ;
#143391 = CARTESIAN_POINT('Ctrl Pts',(-24.879425711808,14.0284941679127,130.626407574217)) ;
#143392 = CARTESIAN_POINT('Ctrl Pts',(-24.9107857517225,13.7670073728255,
130.751140170549)) ;
#143393 = CARTESIAN_POINT('Ctrl Pts',(-24.9181746250829,13.480578033378,130.805889170149)) ;
#143394 = CARTESIAN_POINT('Ctrl Pts',(-24.9004718610314,13.1913387346796,
130.787181604797)) ;
#143395 = CARTESIAN_POINT('Ctrl Pts',(-24.8579892099205,12.9172330452571,
130.696265791956)) ;
#143396 = CARTESIAN_POINT('Ctrl Pts',(-24.7933025062214,12.6799728424888,
130.54038894737)) ;
#143397 = CARTESIAN_POINT('Ctrl Pts',(-24.7095184083986,12.4949910313751,
130.328965022333)) ;
#143398 = CARTESIAN_POINT('Ctrl Pts',(-24.6137491483049,12.3781840419528,
130.082088557106)) ;
#143399 = CARTESIAN_POINT('Ctrl Pts',(-24.5096740314932,12.3352411031327,
129.811395756904)) ;
#143400 = CARTESIAN_POINT('Ctrl Pts',(-24.4066670559684,12.3701183951614,
129.543355608262)) ;
#143401 = CARTESIAN_POINT('Ctrl Pts',(-24.3084885990164,12.4815908336551,
129.289951677576)) ;
#143402 = CARTESIAN_POINT('Ctrl Pts',(-24.2242844198451,12.6586744423265,
129.076874290103)) ;
#143403 = CARTESIAN_POINT('Ctrl Pts',(-24.1571513402064,12.8927064520039,
128.914066459456)) ;
#143404 = CARTESIAN_POINT('Ctrl Pts',(-24.1127083684764,13.161589606751,128.817110936231)) ;
#143405 = CARTESIAN_POINT('Ctrl Pts',(-24.0922448928208,13.452733819126,128.790651846091)) ;
#143406 = CARTESIAN_POINT('Ctrl Pts',(-24.0972841912124,13.7397606616034,
128.838449143832)) ;
#143407 = CARTESIAN_POINT('Ctrl Pts',(-24.1263977298111,14.0044957325971,
128.95662307499)) ;
#143408 = CARTESIAN_POINT('Ctrl Pts',(-24.17672470396,14.2270717509881,129.136685989293)) ;
#143409 = CARTESIAN_POINT('Ctrl Pts',(-24.2441033416361,14.3928428929851,
129.366635907636)) ;
#143410 = CARTESIAN_POINT('Ctrl Pts',(-24.3234048929595,14.4891680120794,
129.631590444853)) ;
#143411 = CARTESIAN_POINT('Ctrl Pts',(-24.4068303427356,14.5086708871169,
129.908215193314)) ;
#143412 = CARTESIAN_POINT('Ctrl Pts',(-24.4893464782002,14.4507090768999,
130.182488475895)) ;
#143413 = CARTESIAN_POINT('Ctrl Pts',(-24.5633225195788,14.3188233795464,
130.431729758912)) ;
#143414 = CARTESIAN_POINT('Ctrl Pts',(-24.6228714288218,14.1234066158898,
130.638750106157)) ;
#143415 = CARTESIAN_POINT('Ctrl Pts',(-24.6632253427087,13.8772494948289,
130.789787062655)) ;
#143416 = CARTESIAN_POINT('Ctrl Pts',(-24.6806457149312,13.5994496671663,
130.873720819945)) ;
#143417 = CARTESIAN_POINT('Ctrl Pts',(-24.6730550166184,13.306728753329,130.884860699526)) ;
#143418 = CARTESIAN_POINT('Ctrl Pts',(-24.6405630151421,13.0255130150403,
130.822883930019)) ;
#143419 = CARTESIAN_POINT('Ctrl Pts',(-24.5845233822454,12.7708775179562,
130.692326227787)) ;
#143420 = CARTESIAN_POINT('Ctrl Pts',(-24.5079734619455,12.5628411654916,
130.50192327057)) ;
#143421 = CARTESIAN_POINT('Ctrl Pts',(-24.4164416886935,12.4171763297159,
130.267577824475)) ;
#143422 = CARTESIAN_POINT('Ctrl Pts',(-24.3145207569583,12.3431378103405,
130.003142213765)) ;
#143423 = CARTESIAN_POINT('Ctrl Pts',(-24.2107870625428,12.346743528454,129.733002482958)) ;
#143424 = CARTESIAN_POINT('Ctrl Pts',(-24.1097939762825,12.4272275492429,
129.471168629618)) ;
#143425 = CARTESIAN_POINT('Ctrl Pts',(-24.0192589501256,12.5790159402385,
129.23978681913)) ;
#143426 = CARTESIAN_POINT('Ctrl Pts',(-23.9444236233476,12.7916689357573,
129.054355997432)) ;
#143427 = CARTESIAN_POINT('Ctrl Pts',(-23.8902712760071,13.0498140627792,
128.929343394403)) ;
#143428 = CARTESIAN_POINT('Ctrl Pts',(-23.8599875189387,13.3331758335929,
128.873881118229)) ;
#143429 = CARTESIAN_POINT('Ctrl Pts',(-23.8546383050908,13.6238936791233,
128.891367979456)) ;
#143430 = CARTESIAN_POINT('Ctrl Pts',(-23.8742411013974,13.9010886430072,
128.981854923374)) ;
#143431 = CARTESIAN_POINT('Ctrl Pts',(-23.9164786379271,14.1432055625841,
129.138361036176)) ;
#143432 = CARTESIAN_POINT('Ctrl Pts',(-23.9778352999634,14.334107077719,129.350811327269)) ;
#143433 = CARTESIAN_POINT('Ctrl Pts',(-24.0525075482063,14.4587992015315,
129.601930787677)) ;
#143434 = CARTESIAN_POINT('Ctrl Pts',(-24.1351926047194,14.5101605092006,
129.876603495337)) ;
#143435 = CARTESIAN_POINT('Ctrl Pts',(-24.2190053195467,14.4834097462587,
130.154588398391)) ;
#143436 = CARTESIAN_POINT('Ctrl Pts',(-24.2970658510404,14.3809866888584,
130.415717243842)) ;
#143437 = CARTESIAN_POINT('Ctrl Pts',(-24.3633845701292,14.2089571493578,
130.642698748449)) ;
#143438 = CARTESIAN_POINT('Ctrl Pts',(-24.4118081071485,13.9828180389134,
130.81707577575)) ;
#143439 = CARTESIAN_POINT('Ctrl Pts',(-24.43904614768,13.7132629238328,130.930016793868)) ;
#143440 = CARTESIAN_POINT('Ctrl Pts',(-24.4416278169151,13.4258376467274,
130.970551063788)) ;
#143441 = CARTESIAN_POINT('Ctrl Pts',(-24.4191648497253,13.1374631126408,
130.938024271275)) ;
#143442 = CARTESIAN_POINT('Ctrl Pts',(-24.3722929118948,12.8691197020598,
130.834231842167)) ;
#143443 = CARTESIAN_POINT('Ctrl Pts',(-24.3035253027477,12.6403113391648,
130.666529496578)) ;
#143444 = CARTESIAN_POINT('Ctrl Pts',(-24.2177440216527,12.4684206936737,
130.448931894944)) ;
#143445 = CARTESIAN_POINT('Ctrl Pts',(-24.1189641371196,12.3638000131135,
130.193681090473)) ;
#143446 = CARTESIAN_POINT('Ctrl Pts',(-24.0152577190491,12.3359859149595,
129.923747869451)) ;
#143447 = CARTESIAN_POINT('Ctrl Pts',(-23.9122225721519,12.3855342860159,
129.655866294705)) ;
#143448 = CARTESIAN_POINT('Ctrl Pts',(-23.8167044562249,12.5097023553619,
129.409976684742)) ;
#143449 = CARTESIAN_POINT('Ctrl Pts',(-23.7350415696029,12.6987170593864,
129.204483050259)) ;
#143450 = CARTESIAN_POINT('Ctrl Pts',(-23.6718214474125,12.9413959891016,
129.053102247864)) ;
#143451 = CARTESIAN_POINT('Ctrl Pts',(-23.6317266635016,13.2164085190981,
128.968979209855)) ;
#143452 = CARTESIAN_POINT('Ctrl Pts',(-23.6161846853452,13.5077477594262,
128.956775771091)) ;
#143453 = CARTESIAN_POINT('Ctrl Pts',(-23.6258623623192,13.7917086517815,
129.018086560944)) ;
#143454 = CARTESIAN_POINT('Ctrl Pts',(-23.6591748256657,14.0497091065288,
129.148483877937)) ;
#143455 = CARTESIAN_POINT('Ctrl Pts',(-23.7131536163967,14.2632251224131,
129.339292961049)) ;
#143456 = CARTESIAN_POINT('Ctrl Pts',(-23.7834103537624,14.4168538521645,
129.577752440174)) ;
#143457 = CARTESIAN_POINT('Ctrl Pts',(-23.8637812419505,14.498759930122,129.845665495601)) ;
#143458 = CARTESIAN_POINT('Ctrl Pts',(-23.9479867757916,14.5035045472666,
130.124804508874)) ;
#143459 = CARTESIAN_POINT('Ctrl Pts',(-24.0289297957099,14.4313229189066,
130.394277457633)) ;
#143460 = CARTESIAN_POINT('Ctrl Pts',(-24.1008459108954,14.2860965422893,
130.63760203165)) ;
#143461 = CARTESIAN_POINT('Ctrl Pts',(-24.1568860900922,14.0806886832094,
130.834254572376)) ;
#143462 = CARTESIAN_POINT('Ctrl Pts',(-24.1932719079745,13.8265803466444,
130.973763090983)) ;
#143463 = CARTESIAN_POINT('Ctrl Pts',(-24.2060319927351,13.5441877343299,
131.044150934557)) ;
#143464 = CARTESIAN_POINT('Ctrl Pts',(-24.1937444777174,13.2530368711715,
131.041386093533)) ;
#143465 = CARTESIAN_POINT('Ctrl Pts',(-24.1565222164124,12.9741112441056,
130.965772544337)) ;
#143466 = CARTESIAN_POINT('Ctrl Pts',(-24.0962637236049,12.727211784615,130.82288513937)) ;
#143467 = CARTESIAN_POINT('Ctrl Pts',(-24.0167199464712,12.5305676715835,
130.623604426394)) ;
#143468 = CARTESIAN_POINT('Ctrl Pts',(-23.9228649380525,12.3976028269524,
130.382495884254)) ;
#143469 = CARTESIAN_POINT('Ctrl Pts',(-23.8200059844747,12.3378877483635,
130.115269742189)) ;
#143470 = CARTESIAN_POINT('Ctrl Pts',(-23.7161313122626,12.3561146706411,
129.844822206421)) ;
#143471 = CARTESIAN_POINT('Ctrl Pts',(-23.6167274273655,12.4504996571453,
129.58757336973)) ;
#143472 = CARTESIAN_POINT('Ctrl Pts',(-23.5285438481367,12.6151918757671,
129.363160504632)) ;
#143473 = CARTESIAN_POINT('Ctrl Pts',(-23.4575504842079,12.8367628546182,
129.188815787231)) ;
#143474 = CARTESIAN_POINT('Ctrl Pts',(-23.4074694454012,13.1024713310692,
129.075832540994)) ;
#143475 = CARTESIAN_POINT('Ctrl Pts',(-23.3819286365241,13.3880985112024,
129.034157042022)) ;
#143476 = CARTESIAN_POINT('Ctrl Pts',(-23.3813836420094,13.6786302833929,
129.065792225384)) ;
#143477 = CARTESIAN_POINT('Ctrl Pts',(-23.4054139281742,13.9495118102634,
129.169053182591)) ;
#143478 = CARTESIAN_POINT('Ctrl Pts',(-23.4515197088819,14.1831630718956,
129.33686405637)) ;
#143479 = CARTESIAN_POINT('Ctrl Pts',(-23.5155530868319,14.3622887223182,
129.556989419024)) ;
#143480 = CARTESIAN_POINT('Ctrl Pts',(-23.5929622025893,14.4748192512671,
129.816455245563)) ;
#143481 = CARTESIAN_POINT('Ctrl Pts',(-23.6760665889331,14.5109473635331,
130.092219650908)) ;
#143482 = CARTESIAN_POINT('Ctrl Pts',(-23.7591142385176,14.4698938664046,
130.367885685175)) ;
#143483 = CARTESIAN_POINT('Ctrl Pts',(-23.8354983853783,14.3536144682459,
130.62417280819)) ;
#143484 = CARTESIAN_POINT('Ctrl Pts',(-23.8987831172299,14.1706211200802,
130.84218781578)) ;
#143485 = CARTESIAN_POINT('Ctrl Pts',(-23.9436890861957,13.9337365390504,
131.0065426473)) ;
#143486 = CARTESIAN_POINT('Ctrl Pts',(-23.9662439925048,13.6617103922721,
131.105431657837)) ;
#143487 = CARTESIAN_POINT('Ctrl Pts',(-23.9642309252639,13.3701431433412,
131.132842985535)) ;
#143488 = CARTESIAN_POINT('Ctrl Pts',(-23.936880730123,13.0839500606497,131.086055779472)) ;
#143489 = CARTESIAN_POINT('Ctrl Pts',(-23.8858072445162,12.8226368169183,
130.969880672048)) ;
#143490 = CARTESIAN_POINT('Ctrl Pts',(-23.8135792178995,12.603615233857,130.791996666625)) ;
#143491 = CARTESIAN_POINT('Ctrl Pts',(-23.7249031771877,12.443223881209,130.566020018471)) ;
#143492 = CARTESIAN_POINT('Ctrl Pts',(-23.6243834508961,12.3525997217998,
130.305729187183)) ;
#143493 = CARTESIAN_POINT('Ctrl Pts',(-23.5206245740586,12.339390379435,130.035551590509)) ;
#143494 = CARTESIAN_POINT('Ctrl Pts',(-23.4183108359919,12.4034681613504,
129.769849164582)) ;
#143495 = CARTESIAN_POINT('Ctrl Pts',(-23.3250195012801,12.5405073209883,
129.530418794464)) ;
#143496 = CARTESIAN_POINT('Ctrl Pts',(-23.246128657495,12.742000710491,129.333241435513)) ;
#143497 = CARTESIAN_POINT('Ctrl Pts',(-23.1875710322953,12.9900803066021,
129.195131588516)) ;
#143498 = CARTESIAN_POINT('Ctrl Pts',(-23.1517255791024,13.2708160842573,
129.123605670452)) ;
#143499 = CARTESIAN_POINT('Ctrl Pts',(-23.1410164930884,13.5613606280666,
129.125372551299)) ;
#143500 = CARTESIAN_POINT('Ctrl Pts',(-23.1552114470279,13.8428562082264,
129.199981132927)) ;
#143501 = CARTESIAN_POINT('Ctrl Pts',(-23.1930535350395,14.0951248182504,
129.343821332079)) ;
#143502 = CARTESIAN_POINT('Ctrl Pts',(-23.2501057955293,14.2968155376203,
129.543381940502)) ;
#143503 = CARTESIAN_POINT('Ctrl Pts',(-23.3229353073403,14.4382063534547,
129.789446101916)) ;
#143504 = CARTESIAN_POINT('Ctrl Pts',(-23.404500721367,14.5055714123115,130.060826591937)) ;
#143505 = CARTESIAN_POINT('Ctrl Pts',(-23.4883253092773,14.4957941615493,
130.338720063012)) ;
#143506 = CARTESIAN_POINT('Ctrl Pts',(-23.5681456294195,14.4095661599452,
130.604978527462)) ;
#143507 = CARTESIAN_POINT('Ctrl Pts',(-23.6377229031392,14.2515334104405,
130.841522721531)) ;
#143508 = CARTESIAN_POINT('Ctrl Pts',(-23.6904929025794,14.0347235705321,
131.028791977006)) ;
#143509 = CARTESIAN_POINT('Ctrl Pts',(-23.722380178782,13.7751698912538,131.154951237933)) ;
#143510 = CARTESIAN_POINT('Ctrl Pts',(-23.7305596953239,13.489554992756,131.211966965207)) ;
#143511 = CARTESIAN_POINT('Ctrl Pts',(-23.7134857949628,13.1989623651925,
131.195236364621)) ;
#143512 = CARTESIAN_POINT('Ctrl Pts',(-23.6717605104891,12.9245155111551,
131.106471534992)) ;
#143513 = CARTESIAN_POINT('Ctrl Pts',(-23.607204735429,12.6850931696754,130.951153837753)) ;
#143514 = CARTESIAN_POINT('Ctrl Pts',(-23.5251058801955,12.5007200280461,
130.744179233861)) ;
#143515 = CARTESIAN_POINT('Ctrl Pts',(-23.4285456899501,12.3802347954754,
130.495393086658)) ;
#143516 = CARTESIAN_POINT('Ctrl Pts',(-23.3255044334404,12.3354177836866,
130.227408711233)) ;
#143517 = CARTESIAN_POINT('Ctrl Pts',(-23.2214527235259,12.3682931667049,
129.956637199255)) ;
#143518 = CARTESIAN_POINT('Ctrl Pts',(-23.1240214979293,12.4764500212594,
129.705052803222)) ;
#143519 = CARTESIAN_POINT('Ctrl Pts',(-23.0386731819847,12.6527561710341,
129.488891430682)) ;
#143520 = CARTESIAN_POINT('Ctrl Pts',(-22.9712446345339,12.8841372623909,
129.325039080064)) ;
#143521 = CARTESIAN_POINT('Ctrl Pts',(-22.9256685603981,13.1550291138396,
129.225129396424)) ;
#143522 = CARTESIAN_POINT('Ctrl Pts',(-22.9047424564583,13.4437302446049,
129.197053986198)) ;
#143523 = CARTESIAN_POINT('Ctrl Pts',(-22.9090153289593,13.7319393210826,
129.242714369187)) ;
#143524 = CARTESIAN_POINT('Ctrl Pts',(-22.9373439751867,13.996548190544,129.358457399253)) ;
#143525 = CARTESIAN_POINT('Ctrl Pts',(-22.9872072567607,14.2215298509627,
129.537280491404)) ;
#143526 = CARTESIAN_POINT('Ctrl Pts',(-23.0543476264601,14.38914835891,129.76659166035)) ;
#143527 = CARTESIAN_POINT('Ctrl Pts',(-23.132867941208,14.4871687209254,130.029047170173)) ;
#143528 = CARTESIAN_POINT('Ctrl Pts',(-23.2167986272204,14.5093408038881,
130.307369504363)) ;
#143529 = CARTESIAN_POINT('Ctrl Pts',(-23.2994992889762,14.4530254210031,
130.582212420233)) ;
#143530 = CARTESIAN_POINT('Ctrl Pts',(-23.3734144406411,14.3240304850431,
130.831087779391)) ;
#143531 = CARTESIAN_POINT('Ctrl Pts',(-23.4337726380514,14.1290978573837,
131.040670220681)) ;
#143532 = CARTESIAN_POINT('Ctrl Pts',(-23.4745345852949,13.8855602682148,
131.192702691882)) ;
#143533 = CARTESIAN_POINT('Ctrl Pts',(-23.4927384577347,13.605841493294,131.279235002887)) ;
#143534 = CARTESIAN_POINT('Ctrl Pts',(-23.4858621472011,13.3160019490386,
131.292133100213)) ;
#143535 = CARTESIAN_POINT('Ctrl Pts',(-23.4540121299607,13.0326884812318,
131.232212628337)) ;
#143536 = CARTESIAN_POINT('Ctrl Pts',(-23.3983642412574,12.7766370515925,
131.102864082558)) ;
#143537 = CARTESIAN_POINT('Ctrl Pts',(-23.3224252508295,12.5676696843858,
130.914179013247)) ;
#143538 = CARTESIAN_POINT('Ctrl Pts',(-23.2315623998387,12.4206516952527,
130.681675995429)) ;
#143539 = CARTESIAN_POINT('Ctrl Pts',(-23.1301738864212,12.34431502245,130.418692826269)) ;
#143540 = CARTESIAN_POINT('Ctrl Pts',(-23.0259203389995,12.345456773331,130.147196189081)) ;
#143541 = CARTESIAN_POINT('Ctrl Pts',(-22.9245983595864,12.4241540990105,
129.884450538708)) ;
#143542 = CARTESIAN_POINT('Ctrl Pts',(-22.8339604250744,12.5736455946733,
129.652673423447)) ;
#143543 = CARTESIAN_POINT('Ctrl Pts',(-22.7586463627445,12.7844245874558,
129.465809714269)) ;
#143544 = CARTESIAN_POINT('Ctrl Pts',(-22.7038116606386,13.0412646550238,
129.338784714396)) ;
#143545 = CARTESIAN_POINT('Ctrl Pts',(-22.672696634036,13.3250315602578,129.280999683653)) ;
#143546 = CARTESIAN_POINT('Ctrl Pts',(-22.6666782489099,13.615649410723,129.296509723596)) ;
#143547 = CARTESIAN_POINT('Ctrl Pts',(-22.6854869927878,13.8929004143671,
129.384593069969)) ;
#143548 = CARTESIAN_POINT('Ctrl Pts',(-22.7271490627597,14.1366367418866,
129.53946593282)) ;
#143549 = CARTESIAN_POINT('Ctrl Pts',(-22.7877716926247,14.3287834464846,
129.749659518345)) ;
#143550 = CARTESIAN_POINT('Ctrl Pts',(-22.8624217458546,14.4563288635319,
130.000862719859)) ;
#143551 = CARTESIAN_POINT('Ctrl Pts',(-22.9451469435644,14.5097636487804,
130.275713031449)) ;
#143552 = CARTESIAN_POINT('Ctrl Pts',(-23.0287793650505,14.4852491667338,
130.553077224357)) ;
#143553 = CARTESIAN_POINT('Ctrl Pts',(-23.1070274154926,14.3852131560936,
130.814719834429)) ;
#143554 = CARTESIAN_POINT('Ctrl Pts',(-23.1739124562573,14.2148994142931,
131.043403108811)) ;
#143555 = CARTESIAN_POINT('Ctrl Pts',(-23.2229394678138,13.9895604970269,
131.219613593883)) ;
#143556 = CARTESIAN_POINT('Ctrl Pts',(-23.2507366610269,13.722649621575,131.333978244755)) ;
#143557 = CARTESIAN_POINT('Ctrl Pts',(-23.2541372508295,13.4342098870415,
131.377066913897)) ;
#143558 = CARTESIAN_POINT('Ctrl Pts',(-23.2324178885211,13.145818281647,131.346673514171)) ;
#143559 = CARTESIAN_POINT('Ctrl Pts',(-23.1860426545478,12.8759127187507,
131.244432599894)) ;
#143560 = CARTESIAN_POINT('Ctrl Pts',(-23.1182744949016,12.646886857505,131.079457250169)) ;
#143561 = CARTESIAN_POINT('Ctrl Pts',(-23.0324041722189,12.4721832267463,
130.861807119644)) ;
#143562 = CARTESIAN_POINT('Ctrl Pts',(-22.9347158667363,12.3661739230268,
130.609463902656)) ;
#143563 = CARTESIAN_POINT('Ctrl Pts',(-22.8302237560895,12.3355863381279,
130.337518479939)) ;
#143564 = CARTESIAN_POINT('Ctrl Pts',(-22.7272957874238,12.383119877217,130.06987449926)) ;
#143565 = CARTESIAN_POINT('Ctrl Pts',(-22.6313718290583,12.5053833335783,
129.822838291288)) ;
#143566 = CARTESIAN_POINT('Ctrl Pts',(-22.549444806847,12.6923271245218,129.616496226826)) ;
#143567 = CARTESIAN_POINT('Ctrl Pts',(-22.4855769767943,12.933586655108,129.46321823843)) ;
#143568 = CARTESIAN_POINT('Ctrl Pts',(-22.4447201723286,13.2085815637178,
129.376950905108)) ;
#143569 = CARTESIAN_POINT('Ctrl Pts',(-22.428506211567,13.499055887524,129.362699996165)) ;
#143570 = CARTESIAN_POINT('Ctrl Pts',(-22.4374411004653,13.7836908824952,
129.421864605484)) ;
#143571 = CARTESIAN_POINT('Ctrl Pts',(-22.4701043315475,14.0427282723312,
129.550363332339)) ;
#143572 = CARTESIAN_POINT('Ctrl Pts',(-22.5235419982417,14.2577310864089,
129.73959019157)) ;
#143573 = CARTESIAN_POINT('Ctrl Pts',(-22.5932633108271,14.4131665395365,
129.976425920683)) ;
#143574 = CARTESIAN_POINT('Ctrl Pts',(-22.6735795483315,14.4973756020118,
130.244248302139)) ;
#143575 = CARTESIAN_POINT('Ctrl Pts',(-22.7573477862148,14.5046723914937,
130.521938057957)) ;
#143576 = CARTESIAN_POINT('Ctrl Pts',(-22.8390722337888,14.4343110972272,
130.793939994731)) ;
#143577 = CARTESIAN_POINT('Ctrl Pts',(-22.9110884796083,14.2913902739099,
131.037440280102)) ;
#143578 = CARTESIAN_POINT('Ctrl Pts',(-22.9677500828963,14.0872938687907,
131.235968489753)) ;
#143579 = CARTESIAN_POINT('Ctrl Pts',(-23.0047032783507,13.8349905737135,
131.377045531599)) ;
#143580 = CARTESIAN_POINT('Ctrl Pts',(-23.0182429611947,13.5522016078203,
131.449828390998)) ;
#143581 = CARTESIAN_POINT('Ctrl Pts',(-23.0066529011385,13.261176925901,131.449077872334)) ;
#143582 = CARTESIAN_POINT('Ctrl Pts',(-22.9700608928401,12.9814105366867,
131.375336701068)) ;
#143583 = CARTESIAN_POINT('Ctrl Pts',(-22.9106223405697,12.7341368123324,
131.234734753748)) ;
#143584 = CARTESIAN_POINT('Ctrl Pts',(-22.831420465707,12.5351661127334,131.036536297695)) ;
#143585 = CARTESIAN_POINT('Ctrl Pts',(-22.7374700882341,12.4000170335594,
130.795280878613)) ;
#143586 = CARTESIAN_POINT('Ctrl Pts',(-22.6352599088003,12.3385940998212,
130.529783876629)) ;
#143587 = CARTESIAN_POINT('Ctrl Pts',(-22.5311701984334,12.3545286959988,
130.258765286088)) ;
#143588 = CARTESIAN_POINT('Ctrl Pts',(-22.4314837094175,12.4469846985816,
130.000709234555)) ;
#143589 = CARTESIAN_POINT('Ctrl Pts',(-22.3428054266133,12.6102580102747,
129.774900451722)) ;
#143590 = CARTESIAN_POINT('Ctrl Pts',(-22.2716044309603,12.8296978065605,
129.599824238354)) ;
#143591 = CARTESIAN_POINT('Ctrl Pts',(-22.220982217263,13.0929764235486,129.485098106775)) ;
#143592 = CARTESIAN_POINT('Ctrl Pts',(-22.1944879827316,13.3798715648176,
129.440832558787)) ;
#143593 = CARTESIAN_POINT('Ctrl Pts',(-22.1932838176779,13.6705227890218,
129.47053097622)) ;
#143594 = CARTESIAN_POINT('Ctrl Pts',(-22.216586984954,13.9421700624616,129.571656651199)) ;
#143595 = CARTESIAN_POINT('Ctrl Pts',(-22.2623594128797,14.1780191075409,
129.738634100291)) ;
#143596 = CARTESIAN_POINT('Ctrl Pts',(-22.3257673108184,14.3579768131381,
129.956807935287)) ;
#143597 = CARTESIAN_POINT('Ctrl Pts',(-22.402693163682,14.4725057536027,130.214788867147)) ;
#143598 = CARTESIAN_POINT('Ctrl Pts',(-22.4858525447118,14.5110248787741,
130.490773806693)) ;
#143599 = CARTESIAN_POINT('Ctrl Pts',(-22.5690583642843,14.4721191985818,
130.766923866594)) ;
#143600 = CARTESIAN_POINT('Ctrl Pts',(-22.6457431338845,14.3577454334386,
131.024102564944)) ;
#143601 = CARTESIAN_POINT('Ctrl Pts',(-22.709285526216,14.1770688600788,131.242769537148)) ;
#143602 = CARTESIAN_POINT('Ctrl Pts',(-22.7548684342017,13.9416997135302,
131.409099612895)) ;
#143603 = CARTESIAN_POINT('Ctrl Pts',(-22.7781477410586,13.6694103999149,
131.510228280328)) ;
#143604 = CARTESIAN_POINT('Ctrl Pts',(-22.7768870761297,13.3798585419127,
131.539630839804)) ;
#143605 = CARTESIAN_POINT('Ctrl Pts',(-22.750382745593,13.0927639720694,131.495363128211)) ;
#143606 = CARTESIAN_POINT('Ctrl Pts',(-22.6997687083182,12.8294541996799,
131.380657407185)) ;
#143607 = CARTESIAN_POINT('Ctrl Pts',(-22.6280842619235,12.6090079342562,
131.204355845863)) ;
#143608 = CARTESIAN_POINT('Ctrl Pts',(-22.5396228094031,12.4466659033485,
130.979064335721)) ;
#143609 = CARTESIAN_POINT('Ctrl Pts',(-22.4399385081326,12.3544265083851,
130.7210134408)) ;
#143610 = CARTESIAN_POINT('Ctrl Pts',(-22.3359884293059,12.338485561048,130.450351932456)) ;
#143611 = CARTESIAN_POINT('Ctrl Pts',(-22.2329622684113,12.4009576642386,
130.182750802671)) ;
#143612 = CARTESIAN_POINT('Ctrl Pts',(-22.1398337600932,12.5356623711056,
129.943638898752)) ;
#143613 = CARTESIAN_POINT('Ctrl Pts',(-22.0607017790479,12.7342794409358,
129.745607566337)) ;
#143614 = CARTESIAN_POINT('Ctrl Pts',(-22.0011596910477,12.9822472239535,
129.604781893021)) ;
#143615 = CARTESIAN_POINT('Ctrl Pts',(-21.9646063758927,13.2626106306711,
129.531211763355)) ;
#143616 = CARTESIAN_POINT('Ctrl Pts',(-21.9531801864884,13.5537332478673,
129.530951535747)) ;
#143617 = CARTESIAN_POINT('Ctrl Pts',(-21.9667343017209,13.835078244523,129.603615881096)) ;
#143618 = CARTESIAN_POINT('Ctrl Pts',(-22.0036132721382,14.0872564093589,
129.744451692133)) ;
#143619 = CARTESIAN_POINT('Ctrl Pts',(-22.0605479104735,14.2922554026262,
129.943923349653)) ;
#143620 = CARTESIAN_POINT('Ctrl Pts',(-22.1328947465888,14.4349646687422,
130.18849153958)) ;
#143621 = CARTESIAN_POINT('Ctrl Pts',(-22.213936585761,14.50455407939,130.458214816929)) ;
#143622 = CARTESIAN_POINT('Ctrl Pts',(-22.2981099146983,14.4973581073499,
130.737249362425)) ;
#143623 = CARTESIAN_POINT('Ctrl Pts',(-22.3784072001466,14.4126016063702,
131.0050273077)) ;
#143624 = CARTESIAN_POINT('Ctrl Pts',(-22.447805875919,14.2578369760295,131.240771109956)) ;
#143625 = CARTESIAN_POINT('Ctrl Pts',(-22.5013649795716,14.0423605049128,
131.430430107999)) ;
#143626 = CARTESIAN_POINT('Ctrl Pts',(-22.534006961752,13.7833429469769,131.558854833022)) ;
#143627 = CARTESIAN_POINT('Ctrl Pts',(-22.5428671924125,13.4972453189194,
131.617966841361)) ;
#143628 = CARTESIAN_POINT('Ctrl Pts',(-22.5265920281103,13.2077136867894,
131.603426053842)) ;
#143629 = CARTESIAN_POINT('Ctrl Pts',(-22.4854531315834,12.9318530296234,
131.516461855721)) ;
#143630 = CARTESIAN_POINT('Ctrl Pts',(-22.4218868621433,12.6922551548189,
131.363858154752)) ;
#143631 = CARTESIAN_POINT('Ctrl Pts',(-22.339699493421,12.5046664561304,131.156866750708)) ;
#143632 = CARTESIAN_POINT('Ctrl Pts',(-22.2434112650807,12.3825157092279,
130.908862326724)) ;
#143633 = CARTESIAN_POINT('Ctrl Pts',(-22.1407022451927,12.3357140446238,
130.641782038687)) ;
#143634 = CARTESIAN_POINT('Ctrl Pts',(-22.0367950143925,12.36606795923,130.371356157515)) ;
#143635 = CARTESIAN_POINT('Ctrl Pts',(-21.9385800776849,12.4727573842292,
130.117660335976)) ;
#143636 = CARTESIAN_POINT('Ctrl Pts',(-21.8530384367553,12.6471452972706,
129.900859802065)) ;
#143637 = CARTESIAN_POINT('Ctrl Pts',(-21.7851981669221,12.8766362128536,
129.735734315131)) ;
#143638 = CARTESIAN_POINT('Ctrl Pts',(-21.738959998301,13.1457609498557,129.633791333078)) ;
#143639 = CARTESIAN_POINT('Ctrl Pts',(-21.7171693051141,13.4362085163513,
129.603423986028)) ;
#143640 = CARTESIAN_POINT('Ctrl Pts',(-21.7207505372234,13.7232902090159,
129.646893616354)) ;
#143641 = CARTESIAN_POINT('Ctrl Pts',(-21.7484265203704,13.9896012437994,
129.760821659193)) ;
#143642 = CARTESIAN_POINT('Ctrl Pts',(-21.7977851645391,14.215929645434,129.938174798434)) ;
#143643 = CARTESIAN_POINT('Ctrl Pts',(-21.8643742193588,14.3851342373848,
130.165817724569)) ;
#143644 = CARTESIAN_POINT('Ctrl Pts',(-21.9427712554755,14.4854517125692,
130.42796572971)) ;
#143645 = CARTESIAN_POINT('Ctrl Pts',(-22.0264764252796,14.5096986582257,
130.705565676572)) ;
#143646 = CARTESIAN_POINT('Ctrl Pts',(-22.1091205178272,14.4561737442075,
130.980149885645)) ;
#143647 = CARTESIAN_POINT('Ctrl Pts',(-22.1838332613068,14.3282784828902,
131.231578468129)) ;
#143648 = CARTESIAN_POINT('Ctrl Pts',(-22.2443137255644,14.1363002885468,
131.441301018419)) ;
#143649 = CARTESIAN_POINT('Ctrl Pts',(-22.2859518160171,13.8924838529507,
131.596109073872)) ;
#143650 = CARTESIAN_POINT('Ctrl Pts',(-22.3047209382812,13.6154600840217,
131.684045645423)) ;
#143651 = CARTESIAN_POINT('Ctrl Pts',(-22.2986702811419,13.3244464776438,
131.699506421331)) ;
#143652 = CARTESIAN_POINT('Ctrl Pts',(-22.2674859080266,13.0407280398606,
131.641518038007)) ;
#143653 = CARTESIAN_POINT('Ctrl Pts',(-22.2127203231953,12.7843964023836,
131.514637915739)) ;
#143654 = CARTESIAN_POINT('Ctrl Pts',(-22.137398507186,12.5734337589229,131.327764159491)) ;
#143655 = CARTESIAN_POINT('Ctrl Pts',(-22.0463241028875,12.4236458719393,
131.094850745407)) ;
#143656 = CARTESIAN_POINT('Ctrl Pts',(-21.9456019274968,12.3455712337427,
130.833653818815)) ;
#143657 = CARTESIAN_POINT('Ctrl Pts',(-21.8410149058486,12.3443023954149,
130.561292129649)) ;
#143658 = CARTESIAN_POINT('Ctrl Pts',(-21.7395756953206,12.4209332624995,
130.298180683002)) ;
#143659 = CARTESIAN_POINT('Ctrl Pts',(-21.6485359377366,12.5684898191716,
130.065238668739)) ;
#143660 = CARTESIAN_POINT('Ctrl Pts',(-21.5725277270908,12.7783873972307,
129.876435053139)) ;
#143661 = CARTESIAN_POINT('Ctrl Pts',(-21.5172012263658,13.0341437387016,
129.747950001213)) ;
#143662 = CARTESIAN_POINT('Ctrl Pts',(-21.4855037051697,13.3161554584295,
129.68831963719)) ;
#143663 = CARTESIAN_POINT('Ctrl Pts',(-21.4786823629391,13.6077103928711,
129.701579568902)) ;
#143664 = CARTESIAN_POINT('Ctrl Pts',(-21.4969471387102,13.8863968339185,
129.78817190297)) ;
#143665 = CARTESIAN_POINT('Ctrl Pts',(-21.5380140006036,14.1306964208414,
129.941243579544)) ;
#143666 = CARTESIAN_POINT('Ctrl Pts',(-21.597955468829,14.3238933798465,130.14933977895)) ;
#143667 = CARTESIAN_POINT('Ctrl Pts',(-21.6722368019592,14.4535138148578,
130.399455722399)) ;
#143668 = CARTESIAN_POINT('Ctrl Pts',(-21.7548431705078,14.5094099207336,
130.673967122569)) ;
#143669 = CARTESIAN_POINT('Ctrl Pts',(-21.8390074433957,14.4867701490887,
130.953075016823)) ;
#143670 = CARTESIAN_POINT('Ctrl Pts',(-21.9170393419491,14.3890643501402,
131.213907369447)) ;
#143671 = CARTESIAN_POINT('Ctrl Pts',(-21.9843219419799,14.2211868758739,
131.443700982914)) ;
#143672 = CARTESIAN_POINT('Ctrl Pts',(-22.034145358508,13.9958857732727,131.622425454293)) ;
#143673 = CARTESIAN_POINT('Ctrl Pts',(-22.0624108594708,13.731479333369,131.737954309001)) ;
#143674 = CARTESIAN_POINT('Ctrl Pts',(-22.0666539748557,13.44236393195,131.783625544948)) ;
#143675 = CARTESIAN_POINT('Ctrl Pts',(-22.0454519447672,13.1530743208287,
131.754824233389)) ;
#143676 = CARTESIAN_POINT('Ctrl Pts',(-22.0001608256054,12.884256615766,131.655497903819)) ;
#143677 = CARTESIAN_POINT('Ctrl Pts',(-21.9324437444424,12.6519995409111,
131.490940272545)) ;
#143678 = CARTESIAN_POINT('Ctrl Pts',(-21.8474698625417,12.4766942451725,
131.275709117702)) ;
#143679 = CARTESIAN_POINT('Ctrl Pts',(-21.7498528975863,12.3681120664589,
131.023656849795)) ;
#143680 = CARTESIAN_POINT('Ctrl Pts',(-21.6453559537401,12.3353450088633,
130.751717635271)) ;
#143681 = CARTESIAN_POINT('Ctrl Pts',(-21.542236103773,12.380878936013,130.483543962322)) ;
#143682 = CARTESIAN_POINT('Ctrl Pts',(-21.4463295322367,12.5006496945069,
130.236443567169)) ;
#143683 = CARTESIAN_POINT('Ctrl Pts',(-21.3637539981775,12.6862349323656,
130.028280312864)) ;
#143684 = CARTESIAN_POINT('Ctrl Pts',(-21.2995009859174,12.9253055935091,
129.873754351436)) ;
#143685 = CARTESIAN_POINT('Ctrl Pts',(-21.2578359992807,13.1996775352275,
129.785155353514)) ;
#143686 = CARTESIAN_POINT('Ctrl Pts',(-21.2408217231033,13.4900584277301,
129.768572274844)) ;
#143687 = CARTESIAN_POINT('Ctrl Pts',(-21.2490712614427,13.7765695978382,
129.825896978974)) ;
#143688 = CARTESIAN_POINT('Ctrl Pts',(-21.2812883123373,14.036835781509,129.953150444439)) ;
#143689 = CARTESIAN_POINT('Ctrl Pts',(-21.3339524991672,14.2522895995138,
130.139959179499)) ;
#143690 = CARTESIAN_POINT('Ctrl Pts',(-21.4036007042656,14.410142724822,130.376724923373)) ;
#143691 = CARTESIAN_POINT('Ctrl Pts',(-21.4833190971745,14.4959011671627,
130.642629699404)) ;
#143692 = CARTESIAN_POINT('Ctrl Pts',(-21.5672364300302,14.5055615409164,
130.920826895733)) ;
#143693 = CARTESIAN_POINT('Ctrl Pts',(-21.6489772963134,14.4373878436055,
131.192815585546)) ;
#143694 = CARTESIAN_POINT('Ctrl Pts',(-21.721303833013,14.2968054840673,131.437185325856)) ;
#143695 = CARTESIAN_POINT('Ctrl Pts',(-21.7787209509657,14.0934338457394,
131.63806052176)) ;
#143696 = CARTESIAN_POINT('Ctrl Pts',(-21.8161626773945,13.8423636115969,
131.780529628432)) ;
#143697 = CARTESIAN_POINT('Ctrl Pts',(-21.8304120659341,13.5615575056706,
131.855225921439)) ;
#143698 = CARTESIAN_POINT('Ctrl Pts',(-21.8195551963924,13.2694346825445,
131.85674250842)) ;
#143699 = CARTESIAN_POINT('Ctrl Pts',(-21.7837797080597,12.9897645897098,
131.785295359872)) ;
#143700 = CARTESIAN_POINT('Ctrl Pts',(-21.7247880088678,12.7403850896867,
131.646117143433)) ;
#143701 = CARTESIAN_POINT('Ctrl Pts',(-21.6461522200936,12.5401777346667,
131.449526068275)) ;
#143702 = CARTESIAN_POINT('Ctrl Pts',(-21.552843515609,12.403253810304,131.2100513829)) ;
#143703 = CARTESIAN_POINT('Ctrl Pts',(-21.4506728701617,12.3392654629647,
130.944714192732)) ;
#143704 = CARTESIAN_POINT('Ctrl Pts',(-21.3462630111135,12.3529796001613,
130.672847368747)) ;
#143705 = CARTESIAN_POINT('Ctrl Pts',(-21.2464552737874,12.4434150313968,
130.414411901)) ;
#143706 = CARTESIAN_POINT('Ctrl Pts',(-21.1576935500326,12.6038143238447,
130.188212603758)) ;
#143707 = CARTESIAN_POINT('Ctrl Pts',(-21.0854169254923,12.8232747601352,
130.010229428693)) ;
#143708 = CARTESIAN_POINT('Ctrl Pts',(-21.0343721327219,13.0848674968843,
129.894160674788)) ;
#143709 = CARTESIAN_POINT('Ctrl Pts',(-21.0071238887452,13.3712341167296,
129.847685621154)) ;
#143710 = CARTESIAN_POINT('Ctrl Pts',(-21.0051604192748,13.662067069188,129.875157873121)) ;
#143711 = CARTESIAN_POINT('Ctrl Pts',(-21.0278323583826,13.9347879566426,
129.974482349287)) ;
#143712 = CARTESIAN_POINT('Ctrl Pts',(-21.0727651018897,14.1711547211457,
130.138867819652)) ;
#143713 = CARTESIAN_POINT('Ctrl Pts',(-21.1360453755805,14.3538986016763,
130.356852241416)) ;
#143714 = CARTESIAN_POINT('Ctrl Pts',(-21.2123321193934,14.4699515412555,
130.612807306947)) ;
#143715 = CARTESIAN_POINT('Ctrl Pts',(-21.2955547074011,14.5110117292323,
130.889053219107)) ;
#143716 = CARTESIAN_POINT('Ctrl Pts',(-21.3787853405023,14.4745400439387,
131.165237882417)) ;
#143717 = CARTESIAN_POINT('Ctrl Pts',(-21.4561885971438,14.3614975022745,
131.424710865457)) ;
#143718 = CARTESIAN_POINT('Ctrl Pts',(-21.519893734885,14.1829580281289,131.64373550919)) ;
#143719 = CARTESIAN_POINT('Ctrl Pts',(-21.5660558437163,13.94924048582,131.811726969927)) ;
#143720 = CARTESIAN_POINT('Ctrl Pts',(-21.5900114787157,13.6775800783231,
131.914852504217)) ;
#143721 = CARTESIAN_POINT('Ctrl Pts',(-21.5895481401675,13.3886494305686,
131.946535521547)) ;
#143722 = CARTESIAN_POINT('Ctrl Pts',(-21.5635014834957,13.0993477502972,
131.903825726572)) ;
#143723 = CARTESIAN_POINT('Ctrl Pts',(-21.513837759379,12.8369457747394,131.791665496349)) ;
#143724 = CARTESIAN_POINT('Ctrl Pts',(-21.4424162592507,12.6140529182667,
131.616278760656)) ;
#143725 = CARTESIAN_POINT('Ctrl Pts',(-21.3547003822089,12.4507322880218,
131.393022499549)) ;
#143726 = CARTESIAN_POINT('Ctrl Pts',(-21.2552473216185,12.3558899058093,
131.135660559877)) ;
#143727 = CARTESIAN_POINT('Ctrl Pts',(-21.1505893270676,12.3380969168945,
130.863169991664)) ;
#143728 = CARTESIAN_POINT('Ctrl Pts',(-21.0487008205765,12.3976017184894,
130.598472003428)) ;
#143729 = CARTESIAN_POINT('Ctrl Pts',(-20.9545575211431,12.5305839180843,
130.356606283238)) ;
#143730 = CARTESIAN_POINT('Ctrl Pts',(-20.8747906198652,12.7283491883042,
130.156805436594)) ;
#143731 = CARTESIAN_POINT('Ctrl Pts',(-20.814855044514,12.97427729496,130.014714765469)) ;
#143732 = CARTESIAN_POINT('Ctrl Pts',(-20.7775537383068,13.2539378203869,
129.938959194661)) ;
#143733 = CARTESIAN_POINT('Ctrl Pts',(-20.7653549702161,13.5450905398915,
129.936447089367)) ;
#143734 = CARTESIAN_POINT('Ctrl Pts',(-20.778250046486,13.8275789493197,130.007259996117)) ;
#143735 = CARTESIAN_POINT('Ctrl Pts',(-20.8144440542377,14.0806196920483,
130.146052159019)) ;
#143736 = CARTESIAN_POINT('Ctrl Pts',(-20.8711507634857,14.2877393448121,
130.344989067034)) ;
#143737 = CARTESIAN_POINT('Ctrl Pts',(-20.9424498938353,14.4312139219373,
130.586184629812)) ;
#143738 = CARTESIAN_POINT('Ctrl Pts',(-21.0239714683594,14.5038738405656,
130.85759121572)) ;
#143739 = CARTESIAN_POINT('Ctrl Pts',(-21.1079824326602,14.4984557258389,
131.13608035658)) ;
#143740 = CARTESIAN_POINT('Ctrl Pts',(-21.1882743598749,14.4164646007505,
131.403738404483)) ;
#143741 = CARTESIAN_POINT('Ctrl Pts',(-21.2585413217483,14.262213927018,131.642274476708)) ;
#143742 = CARTESIAN_POINT('Ctrl Pts',(-21.3122078056105,14.0497488038025,
131.831993572367)) ;
#143743 = CARTESIAN_POINT('Ctrl Pts',(-21.3456511109205,13.7905256830516,
131.962929341245)) ;
#143744 = CARTESIAN_POINT('Ctrl Pts',(-21.3552119916928,13.5064863468517,
132.023892257237)) ;
#143745 = CARTESIAN_POINT('Ctrl Pts',(-21.3394492991724,13.2142514411646,
132.011153788034)) ;
#143746 = CARTESIAN_POINT('Ctrl Pts',(-21.2993880623109,12.9406231812218,
131.926977857705)) ;
#143747 = CARTESIAN_POINT('Ctrl Pts',(-21.236159113355,12.6982138034392,131.775554994669)) ;
#143748 = CARTESIAN_POINT('Ctrl Pts',(-21.1546783206131,12.5096111619529,
131.570515351654)) ;
#143749 = CARTESIAN_POINT('Ctrl Pts',(-21.0586507848846,12.3850648455084,
131.323305972789)) ;
#143750 = CARTESIAN_POINT('Ctrl Pts',(-20.9559564799004,12.3359713262841,
131.056299516685)) ;
#143751 = CARTESIAN_POINT('Ctrl Pts',(-20.8519535030408,12.3641515786215,
130.785604464466)) ;
#143752 = CARTESIAN_POINT('Ctrl Pts',(-20.7536461523058,12.4683944870956,
130.531571929203)) ;
#143753 = CARTESIAN_POINT('Ctrl Pts',(-20.667420355021,12.6414744959111,130.312873391049)) ;
#143754 = CARTESIAN_POINT('Ctrl Pts',(-20.5990533195231,12.8692739699043,
130.146164983405)) ;
#143755 = CARTESIAN_POINT('Ctrl Pts',(-20.5519947072442,13.1394382776975,
130.042045907124)) ;
#143756 = CARTESIAN_POINT('Ctrl Pts',(-20.5297640471579,13.4257125359272,
130.009941561444)) ;
#143757 = CARTESIAN_POINT('Ctrl Pts',(-20.5324664686264,13.7153678906251,
130.051102559557)) ;
#143758 = CARTESIAN_POINT('Ctrl Pts',(-20.5595324760176,13.9823826139753,
130.163226514843)) ;
#143759 = CARTESIAN_POINT('Ctrl Pts',(-20.608371754187,14.2103512804348,130.339101089377)) ;
#143760 = CARTESIAN_POINT('Ctrl Pts',(-20.6744261305736,14.3810373660196,
130.565119965549)) ;
#143761 = CARTESIAN_POINT('Ctrl Pts',(-20.7525322815134,14.4835203984391,
130.826411205508)) ;
#143762 = CARTESIAN_POINT('Ctrl Pts',(-20.8362000596334,14.5102051461734,
131.103908811644)) ;
#143763 = CARTESIAN_POINT('Ctrl Pts',(-20.9193142204875,14.4584272237243,
131.380012083211)) ;
#143764 = CARTESIAN_POINT('Ctrl Pts',(-20.9939183747902,14.3332271033523,
131.630932788698)) ;
#143765 = CARTESIAN_POINT('Ctrl Pts',(-21.0551280057048,14.1422678192608,
131.842918113244)) ;
#143766 = CARTESIAN_POINT('Ctrl Pts',(-21.0972229529673,13.9003525396715,
131.998958255873)) ;
#143767 = CARTESIAN_POINT('Ctrl Pts',(-21.1167448448093,13.6237174619485,
132.089138962996)) ;
#143768 = CARTESIAN_POINT('Ctrl Pts',(-21.1114203041332,13.3329586763548,
132.106702057009)) ;
#143769 = CARTESIAN_POINT('Ctrl Pts',(-21.080916791115,13.0482789829305,132.050754538744)) ;
#143770 = CARTESIAN_POINT('Ctrl Pts',(-21.0266195937754,12.7905982685052,
131.925298668968)) ;
#143771 = CARTESIAN_POINT('Ctrl Pts',(-20.9521997292132,12.5792073074467,
131.7408905552)) ;
#143772 = CARTESIAN_POINT('Ctrl Pts',(-20.8615137418709,12.4271419499118,
131.509129299022)) ;
#143773 = CARTESIAN_POINT('Ctrl Pts',(-20.7607142920707,12.3466854310429,
131.247794334763)) ;
#143774 = CARTESIAN_POINT('Ctrl Pts',(-20.6562427076659,12.3433384713207,
130.975737443275)) ;
#143775 = CARTESIAN_POINT('Ctrl Pts',(-20.5549504108213,12.4172569566232,
130.712936540163)) ;
#143776 = CARTESIAN_POINT('Ctrl Pts',(-20.4631678141765,12.5633305895845,
130.47795441216)) ;
#143777 = CARTESIAN_POINT('Ctrl Pts',(-20.386921679344,12.7708595617965,130.288329923847)) ;
#143778 = CARTESIAN_POINT('Ctrl Pts',(-20.3308120046874,13.025326544213,130.157561920011)) ;
#143779 = CARTESIAN_POINT('Ctrl Pts',(-20.2982429233288,13.3082180027096,
130.095548052008)) ;
#143780 = CARTESIAN_POINT('Ctrl Pts',(-20.2907757621212,13.5990346851552,
130.106831087445)) ;
#143781 = CARTESIAN_POINT('Ctrl Pts',(-20.3081537505599,13.8774217687766,
130.190705780526)) ;
#143782 = CARTESIAN_POINT('Ctrl Pts',(-20.3486475693887,14.1239850259666,
130.342217744254)) ;
#143783 = CARTESIAN_POINT('Ctrl Pts',(-20.40825134073,14.3192777030772,130.549401817463)) ;
#143784 = CARTESIAN_POINT('Ctrl Pts',(-20.482206299086,14.450773280104,130.798558182801)) ;
#143785 = CARTESIAN_POINT('Ctrl Pts',(-20.5644237207708,14.5087792742394,
131.071837523224)) ;
#143786 = CARTESIAN_POINT('Ctrl Pts',(-20.6486285547493,14.4887238114624,
131.351056533869)) ;
#143787 = CARTESIAN_POINT('Ctrl Pts',(-20.7272350805244,14.3928284673273,
131.613698351731)) ;
#143788 = CARTESIAN_POINT('Ctrl Pts',(-20.794923502291,14.2263681576049,131.844708220877)) ;
#143789 = CARTESIAN_POINT('Ctrl Pts',(-20.84507946644,14.0038696004935,132.024217539971)) ;
#143790 = CARTESIAN_POINT('Ctrl Pts',(-20.8741779141571,13.7389371650263,
132.142367468664)) ;
#143791 = CARTESIAN_POINT('Ctrl Pts',(-20.8790905217415,13.4518073481161,
132.189802522045)) ;
#143792 = CARTESIAN_POINT('Ctrl Pts',(-20.858730901802,13.1616327343089,132.163529091199)) ;
#143793 = CARTESIAN_POINT('Ctrl Pts',(-20.8137892339047,12.8906304369754,
132.065399389232)) ;
#143794 = CARTESIAN_POINT('Ctrl Pts',(-20.7470135686821,12.6585325356575,
131.903393481101)) ;
#143795 = CARTESIAN_POINT('Ctrl Pts',(-20.6624947858425,12.4808578781887,
131.689522457705)) ;
#143796 = CARTESIAN_POINT('Ctrl Pts',(-20.5643202030253,12.3697949694261,
131.436105306196)) ;
#143797 = CARTESIAN_POINT('Ctrl Pts',(-20.4610498700862,12.3353140236409,
131.167379944547)) ;
#143798 = CARTESIAN_POINT('Ctrl Pts',(-20.3574082392478,12.3783402030792,
130.89781264628)) ;
#143799 = CARTESIAN_POINT('Ctrl Pts',(-20.2612268033925,12.4961138022352,
130.649899660601)) ;
#143800 = CARTESIAN_POINT('Ctrl Pts',(-20.1780818919777,12.680095634731,130.440110299312)) ;
#143801 = CARTESIAN_POINT('Ctrl Pts',(-20.1132235209398,12.9180877630852,
130.283835936512)) ;
#143802 = CARTESIAN_POINT('Ctrl Pts',(-20.0709566929653,13.1911275854678,
130.193411093563)) ;
#143803 = CARTESIAN_POINT('Ctrl Pts',(-20.0531602513411,13.4815073291889,
130.174562545783)) ;
#143804 = CARTESIAN_POINT('Ctrl Pts',(-20.0607201513665,13.7684315330807,
130.229876234887)) ;
#143805 = CARTESIAN_POINT('Ctrl Pts',(-20.0920900302076,14.0290764110969,
130.354550101899)) ;
#143806 = CARTESIAN_POINT('Ctrl Pts',(-20.1445760208522,14.247309485019,130.54105507157)) ;
#143807 = CARTESIAN_POINT('Ctrl Pts',(-20.2131672327109,14.4057092189414,
130.774419872493)) ;
#143808 = CARTESIAN_POINT('Ctrl Pts',(-20.2931490018152,14.4946179014392,
131.041320306837)) ;
#143809 = CARTESIAN_POINT('Ctrl Pts',(-20.3770264287286,14.5063975048984,
131.319385004787)) ;
#143810 = CARTESIAN_POINT('Ctrl Pts',(-20.4591355130039,14.4401277902918,
131.592540260583)) ;
#143811 = CARTESIAN_POINT('Ctrl Pts',(-20.5314992276366,14.3020000140496,
131.836880126924)) ;
#143812 = CARTESIAN_POINT('Ctrl Pts',(-20.5894710367744,14.1003807123236,
132.03938198034)) ;
#143813 = CARTESIAN_POINT('Ctrl Pts',(-20.6275991795873,13.8504600276244,
132.183862987364)) ;
#143814 = CARTESIAN_POINT('Ctrl Pts',(-20.6425877337758,13.5690358349625,
132.260858497093)) ;
#143815 = CARTESIAN_POINT('Ctrl Pts',(-20.632372444611,13.2773475296497,132.264198835309)) ;
#143816 = CARTESIAN_POINT('Ctrl Pts',(-20.5974164630217,12.9978263790817,
132.19505566985)) ;
#143817 = CARTESIAN_POINT('Ctrl Pts',(-20.5390138830624,12.7470236955785,
132.05763095546)) ;
#143818 = CARTESIAN_POINT('Ctrl Pts',(-20.4609877883318,12.545343046617,131.862781749307)) ;
#143819 = CARTESIAN_POINT('Ctrl Pts',(-20.3678785101158,12.4062332571894,
131.623944714736)) ;
#143820 = CARTESIAN_POINT('Ctrl Pts',(-20.2661748246587,12.3400677783264,
131.359872952747)) ;
#143821 = CARTESIAN_POINT('Ctrl Pts',(-20.1612567497015,12.3515723275397,
131.086676839459)) ;
#143822 = CARTESIAN_POINT('Ctrl Pts',(-20.0615848469451,12.4396026158797,
130.82851586695)) ;
#143823 = CARTESIAN_POINT('Ctrl Pts',(-19.9722369368756,12.5983880408564,
130.600675700158)) ;
#143824 = CARTESIAN_POINT('Ctrl Pts',(-19.8996242883099,12.8155082856179,
130.421593407092)) ;
#143825 = CARTESIAN_POINT('Ctrl Pts',(-19.8475518785741,13.0777481932152,
130.302736870524)) ;
#143826 = CARTESIAN_POINT('Ctrl Pts',(-19.8197563730186,13.364000804506,130.254684914467)) ;
#143827 = CARTESIAN_POINT('Ctrl Pts',(-19.8170697551175,13.6530970935561,
130.27982574218)) ;
#143828 = CARTESIAN_POINT('Ctrl Pts',(-19.839060486369,13.9274411059631,130.377257704675)) ;
#143829 = CARTESIAN_POINT('Ctrl Pts',(-19.8833826907644,14.1649405749744,
130.539835176495)) ;
#143830 = CARTESIAN_POINT('Ctrl Pts',(-19.946370690104,14.3499177041157,130.757052955588)) ;
#143831 = CARTESIAN_POINT('Ctrl Pts',(-20.0223920281984,14.4676736772021,
131.012227837299)) ;
#143832 = CARTESIAN_POINT('Ctrl Pts',(-20.1051541931323,14.5109849191037,
131.286985839572)) ;
#143833 = CARTESIAN_POINT('Ctrl Pts',(-20.18894891482,14.4763368013962,131.565019086318)) ;
#143834 = CARTESIAN_POINT('Ctrl Pts',(-20.2659802707125,14.3664425306899,
131.823111021419)) ;
#143835 = CARTESIAN_POINT('Ctrl Pts',(-20.3307357805088,14.188260258707,132.045502355382)) ;
#143836 = CARTESIAN_POINT('Ctrl Pts',(-20.3772257856926,13.9563928722856,
132.214338660589)) ;
#143837 = CARTESIAN_POINT('Ctrl Pts',(-20.4018956542535,13.6856074997971,
132.319552911824)) ;
#143838 = CARTESIAN_POINT('Ctrl Pts',(-20.402087534473,13.3967977975017,132.353162100239)) ;
#143839 = CARTESIAN_POINT('Ctrl Pts',(-20.3769488824518,13.1083771825577,
132.312954980926)) ;
#143840 = CARTESIAN_POINT('Ctrl Pts',(-20.3277277023517,12.8436200801875,
132.202260047876)) ;
#143841 = CARTESIAN_POINT('Ctrl Pts',(-20.2569355974636,12.6197329194616,
132.028657274242)) ;
#143842 = CARTESIAN_POINT('Ctrl Pts',(-20.1694662975559,12.4541609796659,
131.80618730668)) ;
#143843 = CARTESIAN_POINT('Ctrl Pts',(-20.0700517699011,12.357518085621,131.548991538675)) ;
#143844 = CARTESIAN_POINT('Ctrl Pts',(-19.966347191366,12.3374075405641,131.278995876173)) ;
#143845 = CARTESIAN_POINT('Ctrl Pts',(-19.8634803419964,12.3950240901617,
131.011711144262)) ;
#143846 = CARTESIAN_POINT('Ctrl Pts',(-19.7694521450956,12.5255975503683,
130.770028076305)) ;
#143847 = CARTESIAN_POINT('Ctrl Pts',(-19.6889554236045,12.7221237769604,
130.568189360195)) ;
#143848 = CARTESIAN_POINT('Ctrl Pts',(-19.6284746226204,12.9666439794892,
130.424467938799)) ;
#143849 = CARTESIAN_POINT('Ctrl Pts',(-19.59039372203,13.2467844847395,130.346566394817)) ;
#143850 = CARTESIAN_POINT('Ctrl Pts',(-19.5776057553389,13.5364086840901,
130.342163547303)) ;
#143851 = CARTESIAN_POINT('Ctrl Pts',(-19.5896981839258,13.8193015445878,
130.410610408146)) ;
#143852 = CARTESIAN_POINT('Ctrl Pts',(-19.6252906608147,14.0737432295645,
130.547683639879)) ;
#143853 = CARTESIAN_POINT('Ctrl Pts',(-19.6813765478133,14.28233845815,130.744766235332)) ;
#143854 = CARTESIAN_POINT('Ctrl Pts',(-19.7525262423754,14.428082061538,130.985623109379)) ;
#143855 = CARTESIAN_POINT('Ctrl Pts',(-19.8334644514673,14.5027907453993,
131.255163146721)) ;
#143856 = CARTESIAN_POINT('Ctrl Pts',(-19.9181420687845,14.4996008871204,
131.535862402913)) ;
#143857 = CARTESIAN_POINT('Ctrl Pts',(-19.9981755813607,14.419843429899,131.802586216274)) ;
#143858 = CARTESIAN_POINT('Ctrl Pts',(-20.0687288547216,14.2682254316152,
132.041884513473)) ;
#143859 = CARTESIAN_POINT('Ctrl Pts',(-20.1231433501969,14.0566690769085,
132.233899830116)) ;
#143860 = CARTESIAN_POINT('Ctrl Pts',(-20.1572405438189,13.7984045254372,
132.366752500805)) ;
#143861 = CARTESIAN_POINT('Ctrl Pts',(-20.1674646547526,13.5146253545805,
132.429679127936)) ;
#143862 = CARTESIAN_POINT('Ctrl Pts',(-20.1525953490523,13.223790028339,132.419372446335)) ;
#143863 = CARTESIAN_POINT('Ctrl Pts',(-20.1130358657083,12.9476428894619,
132.336873395723)) ;
#143864 = CARTESIAN_POINT('Ctrl Pts',(-20.0503426230759,12.7041857857084,
132.187005515754)) ;
#143865 = CARTESIAN_POINT('Ctrl Pts',(-19.9694659663671,12.5142907834555,
131.983675392732)) ;
#143866 = CARTESIAN_POINT('Ctrl Pts',(-19.8739753931397,12.3877724095918,
131.737965648296)) ;
#143867 = CARTESIAN_POINT('Ctrl Pts',(-19.7709443029584,12.336191203021,131.470124280929)) ;
#143868 = CARTESIAN_POINT('Ctrl Pts',(-19.6669365691679,12.3624798343251,
131.199398785677)) ;
#143869 = CARTESIAN_POINT('Ctrl Pts',(-19.5687719098967,12.4640688198504,
130.945644876183)) ;
#143870 = CARTESIAN_POINT('Ctrl Pts',(-19.4817848481537,12.6358046378966,
130.724836080655)) ;
#143871 = CARTESIAN_POINT('Ctrl Pts',(-19.4130402249853,12.8620488663086,
130.556977640894)) ;
#143872 = CARTESIAN_POINT('Ctrl Pts',(-19.3654039404876,13.1294243702491,
130.450960645276)) ;
#143873 = CARTESIAN_POINT('Ctrl Pts',(-19.3421969031624,13.4191275485285,
130.416438112994)) ;
#143874 = CARTESIAN_POINT('Ctrl Pts',(-19.3442262557683,13.7060585191979,
130.455278759065)) ;
#143875 = CARTESIAN_POINT('Ctrl Pts',(-19.3707106093196,13.9758635048128,
130.565935791541)) ;
#143876 = CARTESIAN_POINT('Ctrl Pts',(-19.4189272476174,14.2044690848735,
130.739897049957)) ;
#143877 = CARTESIAN_POINT('Ctrl Pts',(-19.4846182490666,14.3772046545246,
130.964899352542)) ;
#143878 = CARTESIAN_POINT('Ctrl Pts',(-19.5624570312064,14.4817041714967,
131.225395979999)) ;
#143879 = CARTESIAN_POINT('Ctrl Pts',(-19.6461425521004,14.5103977603672,
131.502983431525)) ;
#143880 = CARTESIAN_POINT('Ctrl Pts',(-19.7288282612474,14.4613877005576,
131.777604673512)) ;
#143881 = CARTESIAN_POINT('Ctrl Pts',(-19.8041618277618,14.3378670133984,
132.030826862098)) ;
#143882 = CARTESIAN_POINT('Ctrl Pts',(-19.8657702567754,14.1487648805611,
132.243936937615)) ;
#143883 = CARTESIAN_POINT('Ctrl Pts',(-19.9085599505618,13.9077123498208,
132.402067970361)) ;
#143884 = CARTESIAN_POINT('Ctrl Pts',(-19.9287403578106,13.6318347847728,
132.494161297536)) ;
#143885 = CARTESIAN_POINT('Ctrl Pts',(-19.9241285333911,13.3411960486728,
132.513808537463)) ;
#143886 = CARTESIAN_POINT('Ctrl Pts',(-19.8943722337192,13.0563345512955,
132.460007505097)) ;
#143887 = CARTESIAN_POINT('Ctrl Pts',(-19.8407354442242,12.7976620834808,
132.336477575288)) ;
#143888 = CARTESIAN_POINT('Ctrl Pts',(-19.7669398342799,12.5846251876044,
132.153875056264)) ;
#143889 = CARTESIAN_POINT('Ctrl Pts',(-19.6758878336454,12.429833205716,131.921298618884)) ;
#143890 = CARTESIAN_POINT('Ctrl Pts',(-19.5761959977977,12.3481748441672,
131.662890781629)) ;
#143891 = CARTESIAN_POINT('Ctrl Pts',(-19.4713288624757,12.3422836443017,
131.389814015339)) ;
#143892 = CARTESIAN_POINT('Ctrl Pts',(-19.3699251221927,12.4141623973689,
131.126663932511)) ;
#143893 = CARTESIAN_POINT('Ctrl Pts',(-19.2776778514234,12.5584918127645,
130.890365636612)) ;
#143894 = CARTESIAN_POINT('Ctrl Pts',(-19.2009980997659,12.7644626666543,
130.699456378474)) ;
#143895 = CARTESIAN_POINT('Ctrl Pts',(-19.1443455018427,13.0174117066364,
130.567048844427)) ;
#143896 = CARTESIAN_POINT('Ctrl Pts',(-19.1110423418376,13.2998966428893,
130.502908392849)) ;
#143897 = CARTESIAN_POINT('Ctrl Pts',(-19.1028387268705,13.5908801629709,
130.512051029699)) ;
#143898 = CARTESIAN_POINT('Ctrl Pts',(-19.1196170916764,13.8706961833489,
130.594271086926)) ;
#143899 = CARTESIAN_POINT('Ctrl Pts',(-19.159552960718,14.1180204039502,130.74412111884)) ;
#143900 = CARTESIAN_POINT('Ctrl Pts',(-19.2184761004089,14.3143766861394,
130.949213922764)) ;
#143901 = CARTESIAN_POINT('Ctrl Pts',(-19.2922787411306,14.4481661316014,
131.198005144871)) ;
#143902 = CARTESIAN_POINT('Ctrl Pts',(-19.3741452353846,14.508083869743,131.470174035041)) ;
#143903 = CARTESIAN_POINT('Ctrl Pts',(-19.4583253760916,14.490551827571,131.749290337179)) ;
#143904 = CARTESIAN_POINT('Ctrl Pts',(-19.5374248602333,14.3964091806781,
132.013482408106)) ;
#143905 = CARTESIAN_POINT('Ctrl Pts',(-19.6052930437783,14.2323049271919,
132.244907382024)) ;
#143906 = CARTESIAN_POINT('Ctrl Pts',(-19.6560850193192,14.0113006230555,
132.426290968773)) ;
#143907 = CARTESIAN_POINT('Ctrl Pts',(-19.6858796266344,13.7469852751569,
132.546516040551)) ;
#143908 = CARTESIAN_POINT('Ctrl Pts',(-19.6915477871688,13.4601450927403,
132.596164261453)) ;
#143909 = CARTESIAN_POINT('Ctrl Pts',(-19.6717188591123,13.1687002988962,
132.571570210908)) ;
#143910 = CARTESIAN_POINT('Ctrl Pts',(-19.6278387509683,12.8989650808956,
132.476275608127)) ;
#143911 = CARTESIAN_POINT('Ctrl Pts',(-19.5611246263324,12.6635916502146,
132.314724093995)) ;
#143912 = CARTESIAN_POINT('Ctrl Pts',(-19.4773775734119,12.4852398029377,
132.102947245662)) ;
#143913 = CARTESIAN_POINT('Ctrl Pts',(-19.3794463063608,12.371925952002,131.850265421701)) ;
#143914 = CARTESIAN_POINT('Ctrl Pts',(-19.2764036885513,12.3351771027553,
131.582155999456)) ;
#143915 = CARTESIAN_POINT('Ctrl Pts',(-19.1723427206771,12.3762351051066,
131.311472093278)) ;
#143916 = CARTESIAN_POINT('Ctrl Pts',(-19.0763723598902,12.4911992471527,
131.06399151218)) ;
#143917 = CARTESIAN_POINT('Ctrl Pts',(-18.9922096682478,12.6745749417996,
130.851450255868)) ;
#143918 = CARTESIAN_POINT('Ctrl Pts',(-18.9270369780191,12.9105841492293,
130.694139865369)) ;
#143919 = CARTESIAN_POINT('Ctrl Pts',(-18.8839823300028,13.1834575977754,
130.601491539362)) ;
#143920 = CARTESIAN_POINT('Ctrl Pts',(-18.8655874201825,13.472817267858,130.580799753087)) ;
#143921 = CARTESIAN_POINT('Ctrl Pts',(-18.8722524231717,13.7593252919433,
130.633389173602)) ;
#143922 = CARTESIAN_POINT('Ctrl Pts',(-18.9032397697211,14.0229112267302,
130.757205209474)) ;
#143923 = CARTESIAN_POINT('Ctrl Pts',(-18.9547768664526,14.2409569319606,
130.940675690362)) ;
#143924 = CARTESIAN_POINT('Ctrl Pts',(-19.0233923114078,14.4024703207306,
131.174341399345)) ;
#143925 = CARTESIAN_POINT('Ctrl Pts',(-19.1029165563042,14.4930253207348,
131.43979044431)) ;
#143926 = CARTESIAN_POINT('Ctrl Pts',(-19.1868068466344,14.5071137946879,
131.717918368786)) ;
#143927 = CARTESIAN_POINT('Ctrl Pts',(-19.2687479247028,14.4434721690138,
131.99044237149)) ;
#143928 = CARTESIAN_POINT('Ctrl Pts',(-19.3417397331137,14.3072990407348,
132.236714912124)) ;
#143929 = CARTESIAN_POINT('Ctrl Pts',(-19.4004487381664,14.1061280190249,
132.441533665576)) ;
#143930 = CARTESIAN_POINT('Ctrl Pts',(-19.4389556441804,13.8584456467317,
132.586963381329)) ;
#143931 = CARTESIAN_POINT('Ctrl Pts',(-19.4547110225428,13.5782525507237,
132.666137792883)) ;
#143932 = CARTESIAN_POINT('Ctrl Pts',(-19.445287263111,13.2862403685174,132.671828009305)) ;
#143933 = CARTESIAN_POINT('Ctrl Pts',(-19.4110002332987,13.0054671404376,
132.604709517203)) ;
#143934 = CARTESIAN_POINT('Ctrl Pts',(-19.3529363497825,12.7527976757228,
132.468391881073)) ;
#143935 = CARTESIAN_POINT('Ctrl Pts',(-19.2758383987832,12.5507720823643,
132.276062163398)) ;
#143936 = CARTESIAN_POINT('Ctrl Pts',(-19.183036429821,12.4092692851511,132.038156718385)) ;
#143937 = CARTESIAN_POINT('Ctrl Pts',(-19.0812978335299,12.3409405879061,
131.774046332401)) ;
#143938 = CARTESIAN_POINT('Ctrl Pts',(-18.9767024131274,12.3499819514293,
131.501678448741)) ;
#143939 = CARTESIAN_POINT('Ctrl Pts',(-18.8763024196267,12.4363532900494,
131.241564305693)) ;
#143940 = CARTESIAN_POINT('Ctrl Pts',(-18.7870104329141,12.592566468637,131.013723468433)) ;
#143941 = CARTESIAN_POINT('Ctrl Pts',(-18.7136463936558,12.808517161013,130.832521133127)) ;
#143942 = CARTESIAN_POINT('Ctrl Pts',(-18.6610063634179,13.0694867381501,
130.711967777011)) ;
#143943 = CARTESIAN_POINT('Ctrl Pts',(-18.632410200303,13.3550372325075,130.661550020128)) ;
#143944 = CARTESIAN_POINT('Ctrl Pts',(-18.629052962816,13.6462143914832,130.684953987523)) ;
#143945 = CARTESIAN_POINT('Ctrl Pts',(-18.6502970918763,13.9195288326514,
130.779995857368)) ;
#143946 = CARTESIAN_POINT('Ctrl Pts',(-18.6939926671848,14.1586151342569,
130.940770034127)) ;
#143947 = CARTESIAN_POINT('Ctrl Pts',(-18.7563803737566,14.3449690064031,
131.156166852151)) ;
#143948 = CARTESIAN_POINT('Ctrl Pts',(-18.8320450450556,14.4652397459023,
131.410296759735)) ;
#143949 = CARTESIAN_POINT('Ctrl Pts',(-18.9153450746737,14.5107689860091,
131.686885139385)) ;
#143950 = CARTESIAN_POINT('Ctrl Pts',(-18.9984240823211,14.4787461953136,
131.962499912619)) ;
#143951 = CARTESIAN_POINT('Ctrl Pts',(-19.0764363731335,14.3700644333909,
132.223765872129)) ;
#143952 = CARTESIAN_POINT('Ctrl Pts',(-19.1411505492463,14.1946408209154,
132.445805538787)) ;
#143953 = CARTESIAN_POINT('Ctrl Pts',(-19.1883722206098,13.9639077381356,
132.616845906245)) ;
#143954 = CARTESIAN_POINT('Ctrl Pts',(-19.2137492404945,13.6940409342519,
132.724111687935)) ;
#143955 = CARTESIAN_POINT('Ctrl Pts',(-19.2145880477621,13.4043243870117,
132.759747994875)) ;
#143956 = CARTESIAN_POINT('Ctrl Pts',(-19.1903786530231,13.1175424203496,
132.722018069961)) ;
#143957 = CARTESIAN_POINT('Ctrl Pts',(-19.1415408484447,12.8501253800453,
132.612661218455)) ;
#143958 = CARTESIAN_POINT('Ctrl Pts',(-19.0716495724154,12.6260375072132,
132.441510922512)) ;
#143959 = CARTESIAN_POINT('Ctrl Pts',(-18.9844995837982,12.4581544955602,
132.220034073742)) ;
#143960 = CARTESIAN_POINT('Ctrl Pts',(-18.8855629159112,12.3594525317711,
131.964157974244)) ;
#143961 = CARTESIAN_POINT('Ctrl Pts',(-18.781568439516,12.3367944106136,131.69342789164)) ;
#143962 = CARTESIAN_POINT('Ctrl Pts',(-18.6782922396415,12.3925085766977,
131.425032749455)) ;
#143963 = CARTESIAN_POINT('Ctrl Pts',(-18.5839790247587,12.5213899475148,
131.182523412252)) ;
#143964 = CARTESIAN_POINT('Ctrl Pts',(-18.5032609434197,12.715572513745,130.979923431317)) ;
#143965 = CARTESIAN_POINT('Ctrl Pts',(-18.4420722767198,12.9595222132268,
130.834214989689)) ;
#143966 = CARTESIAN_POINT('Ctrl Pts',(-18.40353217852,13.2367790657483,130.754712073368)) ;
#143967 = CARTESIAN_POINT('Ctrl Pts',(-18.3897870456702,13.5277645483974,
130.747681760714)) ;
#143968 = CARTESIAN_POINT('Ctrl Pts',(-18.4012590895738,13.8120455612361,
130.814415686742)) ;
#143969 = CARTESIAN_POINT('Ctrl Pts',(-18.4363207056852,14.0676656402339,
130.949968439689)) ;
#143970 = CARTESIAN_POINT('Ctrl Pts',(-18.4917693507281,14.2771421243593,
131.145101016195)) ;
#143971 = CARTESIAN_POINT('Ctrl Pts',(-18.5625493538873,14.4250319650245,
131.384885119588)) ;
#143972 = CARTESIAN_POINT('Ctrl Pts',(-18.643665197432,14.5017260343279,131.655084520159)) ;
#143973 = CARTESIAN_POINT('Ctrl Pts',(-18.7273753185774,14.5010098763796,
131.93256823998)) ;
#143974 = CARTESIAN_POINT('Ctrl Pts',(-18.8083279001163,14.4231232861786,
132.202267998652)) ;
#143975 = CARTESIAN_POINT('Ctrl Pts',(-18.8790721039087,14.2735699420865,
132.442042706819)) ;
#143976 = CARTESIAN_POINT('Ctrl Pts',(-18.934118330524,14.0631259217895,132.635977437453)) ;
#143977 = CARTESIAN_POINT('Ctrl Pts',(-18.9687409921237,13.8068511447586,
132.77024180709)) ;
#143978 = CARTESIAN_POINT('Ctrl Pts',(-18.9797426090043,13.5229066982492,
132.835523927713)) ;
#143979 = CARTESIAN_POINT('Ctrl Pts',(-18.9656045700259,13.2323183656793,
132.827310581068)) ;
#143980 = CARTESIAN_POINT('Ctrl Pts',(-18.9267636321704,12.9554622848227,
132.746912610664)) ;
#143981 = CARTESIAN_POINT('Ctrl Pts',(-18.8647595657246,12.7108336294588,
132.599034340916)) ;
#143982 = CARTESIAN_POINT('Ctrl Pts',(-18.7842026722726,12.5189036240624,
132.396704170719)) ;
#143983 = CARTESIAN_POINT('Ctrl Pts',(-18.6893441361919,12.390658589764,132.152733493589)) ;
#143984 = CARTESIAN_POINT('Ctrl Pts',(-18.5863020448112,12.3366531307129,
131.884915005918)) ;
#143985 = CARTESIAN_POINT('Ctrl Pts',(-18.4823911075163,12.3602977893096,
131.614409397646)) ;
#143986 = CARTESIAN_POINT('Ctrl Pts',(-18.3831235087243,12.4609988755096,
131.357739271015)) ;
#143987 = CARTESIAN_POINT('Ctrl Pts',(-18.2966708436327,12.6291274896935,
131.13812421699)) ;
#143988 = CARTESIAN_POINT('Ctrl Pts',(-18.2267347033546,12.8555169939373,
130.967049610023)) ;
#143989 = CARTESIAN_POINT('Ctrl Pts',(-18.178684786641,13.1215885619852,130.859745333703)) ;
#143990 = CARTESIAN_POINT('Ctrl Pts',(-18.1547618093871,13.4096083947618,
130.822983784196)) ;
#143991 = CARTESIAN_POINT('Ctrl Pts',(-18.1560074176891,13.6982129377788,
130.859689555193)) ;
#143992 = CARTESIAN_POINT('Ctrl Pts',(-18.1819407569754,13.969145223664,130.968781097798)) ;
#143993 = CARTESIAN_POINT('Ctrl Pts',(-18.2294348519779,14.1982918384811,
131.140518474738)) ;
#143994 = CARTESIAN_POINT('Ctrl Pts',(-18.2945663581642,14.3728095638234,
131.363846741243)) ;
#143995 = CARTESIAN_POINT('Ctrl Pts',(-18.3722159348404,14.4796622896265,
131.623830517624)) ;
#143996 = CARTESIAN_POINT('Ctrl Pts',(-18.4558928969119,14.5107460885462,
131.901416593924)) ;
#143997 = CARTESIAN_POINT('Ctrl Pts',(-18.5389249565536,14.4636147877097,
132.177147765495)) ;
#143998 = CARTESIAN_POINT('Ctrl Pts',(-18.6142268417918,14.3427084446703,
132.430124576738)) ;
#143999 = CARTESIAN_POINT('Ctrl Pts',(-18.6766156566363,14.1545213571348,
132.645670743121)) ;
#144000 = CARTESIAN_POINT('Ctrl Pts',(-18.7198818709583,13.9146657038493,
132.805172644963)) ;
#144001 = CARTESIAN_POINT('Ctrl Pts',(-18.7406883952545,13.6405171669677,
132.898977954723)) ;
#144002 = CARTESIAN_POINT('Ctrl Pts',(-18.7368457016297,13.3501101589506,
132.920865495942)) ;
#144003 = CARTESIAN_POINT('Ctrl Pts',(-18.7079487411962,13.0651841999784,
132.869519266352)) ;
#144004 = CARTESIAN_POINT('Ctrl Pts',(-18.6546706091732,12.8038875928186,
132.747233558968)) ;
#144005 = CARTESIAN_POINT('Ctrl Pts',(-18.5814042568152,12.5899464176031,
132.566132647451)) ;
#144006 = CARTESIAN_POINT('Ctrl Pts',(-18.4914287730643,12.4339562439877,
132.336473507997)) ;
#144007 = CARTESIAN_POINT('Ctrl Pts',(-18.3911210751021,12.3491846670138,
132.076546495149)) ;
#144008 = CARTESIAN_POINT('Ctrl Pts',(-18.2862071161722,12.3415474496416,
131.803348771399)) ;
#144009 = CARTESIAN_POINT('Ctrl Pts',(-18.185020267949,12.4110292965116,131.540707750202)) ;
#144010 = CARTESIAN_POINT('Ctrl Pts',(-18.0923825798042,12.5533606733183,
131.303276774471)) ;
#144011 = CARTESIAN_POINT('Ctrl Pts',(-18.0152756269635,12.7574393223527,
131.111078020155)) ;
#144012 = CARTESIAN_POINT('Ctrl Pts',(-17.9578353710385,13.009581913367,130.976421309906)) ;
#144013 = CARTESIAN_POINT('Ctrl Pts',(-17.9237910313609,13.2928228925075,
130.910262343832)) ;
#144014 = CARTESIAN_POINT('Ctrl Pts',(-17.9149479043077,13.582012204951,130.917325191259)) ;
#144015 = CARTESIAN_POINT('Ctrl Pts',(-17.9310342367056,13.8633231100431,
130.997627599138)) ;
#144016 = CARTESIAN_POINT('Ctrl Pts',(-17.9702736832324,14.1112604273849,
131.145362804117)) ;
#144017 = CARTESIAN_POINT('Ctrl Pts',(-18.0287922044005,14.3095522815314,
131.349330597399)) ;
#144018 = CARTESIAN_POINT('Ctrl Pts',(-18.1019911045966,14.44510578155,131.596246152401)) ;
#144019 = CARTESIAN_POINT('Ctrl Pts',(-18.1843833903802,14.5076745879146,
131.870226367737)) ;
#144020 = CARTESIAN_POINT('Ctrl Pts',(-18.2683793556834,14.4918702238892,
132.148714883584)) ;
#144021 = CARTESIAN_POINT('Ctrl Pts',(-18.3474187695467,14.4001695332023,
132.412617942134)) ;
#144022 = CARTESIAN_POINT('Ctrl Pts',(-18.4156630172785,14.2383391968108,
132.645098549425)) ;
#144023 = CARTESIAN_POINT('Ctrl Pts',(-18.467196959154,14.0178456765348,132.828789503516)) ;
#144024 = CARTESIAN_POINT('Ctrl Pts',(-18.4976105450035,13.7549023993413,
132.950761290453)) ;
#144025 = CARTESIAN_POINT('Ctrl Pts',(-18.5038507504708,13.4669383110673,
133.002257275435)) ;
#144026 = CARTESIAN_POINT('Ctrl Pts',(-18.4851160162367,13.179287796842,132.980385937109)) ;
#144027 = CARTESIAN_POINT('Ctrl Pts',(-18.4414836298312,12.9054935054356,
132.886215827744)) ;
#144028 = CARTESIAN_POINT('Ctrl Pts',(-18.3759576029619,12.6708451736549,
132.727823306595)) ;
#144029 = CARTESIAN_POINT('Ctrl Pts',(-18.2919020242458,12.489010935019,132.515465753891)) ;
#144030 = CARTESIAN_POINT('Ctrl Pts',(-18.195291179958,12.3747427452421,132.266277907465)) ;
#144031 = CARTESIAN_POINT('Ctrl Pts',(-18.091594831957,12.3351181280502,131.996517106783)) ;
#144032 = CARTESIAN_POINT('Ctrl Pts',(-17.9879486999613,12.3735357239234,
131.726863664562)) ;
#144033 = CARTESIAN_POINT('Ctrl Pts',(-17.8906852858916,12.4876827047378,
131.475961664461)) ;
#144034 = CARTESIAN_POINT('Ctrl Pts',(-17.8067791669803,12.6681438766094,
131.263905063417)) ;
#144035 = CARTESIAN_POINT('Ctrl Pts',(-17.7407847508741,12.9033828008646,
131.104296212358)) ;
#144036 = CARTESIAN_POINT('Ctrl Pts',(-17.6972166763221,13.1743601977476,
131.010010008373)) ;
#144037 = CARTESIAN_POINT('Ctrl Pts',(-17.6779325586506,13.4644840524054,
130.986835357892)) ;
#144038 = CARTESIAN_POINT('Ctrl Pts',(-17.6840007503613,13.7518156372007,
131.037738629709)) ;
#144039 = CARTESIAN_POINT('Ctrl Pts',(-17.7140670121059,14.0147481121993,
131.158647104721)) ;
#144040 = CARTESIAN_POINT('Ctrl Pts',(-17.7653297228469,14.2359323146828,
131.341537689732)) ;
#144041 = CARTESIAN_POINT('Ctrl Pts',(-17.8336956152316,14.3990328961567,
131.574504973464)) ;
#144042 = CARTESIAN_POINT('Ctrl Pts',(-17.9125313999844,14.4913721477539,
131.83775479626)) ;
#144043 = CARTESIAN_POINT('Ctrl Pts',(-17.9968649663334,14.5077030506771,
132.117375597015)) ;
#144044 = CARTESIAN_POINT('Ctrl Pts',(-18.0785119061021,14.4466726392651,
132.388843886304)) ;
#144045 = CARTESIAN_POINT('Ctrl Pts',(-18.1524693054502,14.3110619945875,
132.638246915545)) ;
#144046 = CARTESIAN_POINT('Ctrl Pts',(-18.2110525859729,14.1132679223134,
132.842369697694)) ;
#144047 = CARTESIAN_POINT('Ctrl Pts',(-18.2504776017827,13.8656263142686,
132.990662346473)) ;
#144048 = CARTESIAN_POINT('Ctrl Pts',(-18.2668284491577,13.5853315264496,
133.071641048268)) ;
#144049 = CARTESIAN_POINT('Ctrl Pts',(-18.2580557921982,13.2939510978671,
133.07916650733)) ;
#144050 = CARTESIAN_POINT('Ctrl Pts',(-18.2245616027976,13.0136079092844,
133.014252441019)) ;
#144051 = CARTESIAN_POINT('Ctrl Pts',(-18.1674098083939,12.7604082845335,
132.880496364703)) ;
#144052 = CARTESIAN_POINT('Ctrl Pts',(-18.090494442978,12.5556139237626,132.688861748547)) ;
#144053 = CARTESIAN_POINT('Ctrl Pts',(-17.997864980143,12.4121627059908,132.451509225692)) ;
#144054 = CARTESIAN_POINT('Ctrl Pts',(-17.8965884139111,12.3419224610127,
132.188653868652)) ;
#144055 = CARTESIAN_POINT('Ctrl Pts',(-17.792087088157,12.3485705952627,131.916526485213)) ;
#144056 = CARTESIAN_POINT('Ctrl Pts',(-17.6915055460129,12.4325162963297,
131.655862931741)) ;
#144057 = CARTESIAN_POINT('Ctrl Pts',(-17.6015237275694,12.5872707160174,
131.42611251694)) ;
#144058 = CARTESIAN_POINT('Ctrl Pts',(-17.5277116214108,12.8016743120911,
131.2435792644)) ;
#144059 = CARTESIAN_POINT('Ctrl Pts',(-17.474505078703,13.0608928169866,131.121287014814)) ;
#144060 = CARTESIAN_POINT('Ctrl Pts',(-17.4451268590908,13.3463628711479,
131.068632504424)) ;
#144061 = CARTESIAN_POINT('Ctrl Pts',(-17.4409756319216,13.6367414871714,
131.089604614589)) ;
#144062 = CARTESIAN_POINT('Ctrl Pts',(-17.4615369886941,13.9121235287477,
131.182800505553)) ;
#144063 = CARTESIAN_POINT('Ctrl Pts',(-17.5047804458157,14.1528033818472,
131.342314267092)) ;
#144064 = CARTESIAN_POINT('Ctrl Pts',(-17.5665368051181,14.3402810469184,
131.555772727796)) ;
#144065 = CARTESIAN_POINT('Ctrl Pts',(-17.6417901561433,14.4626257228514,
131.808667033106)) ;
#144066 = CARTESIAN_POINT('Ctrl Pts',(-17.7250930723354,14.5106364095724,
132.085311240385)) ;
#144067 = CARTESIAN_POINT('Ctrl Pts',(-17.8084089248018,14.4805445911802,
132.361688449539)) ;
#144068 = CARTESIAN_POINT('Ctrl Pts',(-17.8862294224432,14.3748126734896,
132.62218433143)) ;
#144069 = CARTESIAN_POINT('Ctrl Pts',(-17.9517402542539,14.2005693780012,
132.846713355767)) ;
#144070 = CARTESIAN_POINT('Ctrl Pts',(-17.9994948910566,13.9714225005758,
133.019271782795)) ;
#144071 = CARTESIAN_POINT('Ctrl Pts',(-18.0255718526998,13.7016038518799,
133.128682790687)) ;
#144072 = CARTESIAN_POINT('Ctrl Pts',(-18.0271841884768,13.4137877751622,
133.166386118846)) ;
#144073 = CARTESIAN_POINT('Ctrl Pts',(-18.0035377111098,13.1249621012608,
133.130508208661)) ;
#144074 = CARTESIAN_POINT('Ctrl Pts',(-17.9558148290788,12.8587597894488,
133.024127137134)) ;
#144075 = CARTESIAN_POINT('Ctrl Pts',(-17.8859782679843,12.6311848852698,
132.853419690908)) ;
#144076 = CARTESIAN_POINT('Ctrl Pts',(-17.7993724447725,12.462061420416,132.633456990691)) ;
#144077 = CARTESIAN_POINT('Ctrl Pts',(-17.7005818136129,12.3611529098997,
132.378046477399)) ;
#144078 = CARTESIAN_POINT('Ctrl Pts',(-17.5968820347917,12.3364027391132,
132.10810046349)) ;
#144079 = CARTESIAN_POINT('Ctrl Pts',(-17.4934737132323,12.3896955050154,
131.839314298154)) ;
#144080 = CARTESIAN_POINT('Ctrl Pts',(-17.3986186118639,12.5169546340526,
131.595303735162)) ;
#144081 = CARTESIAN_POINT('Ctrl Pts',(-17.3176313423662,12.709001546384,131.391832952582)) ;
#144082 = CARTESIAN_POINT('Ctrl Pts',(-17.2557611142785,12.9518210421532,
131.244157189681)) ;
#144083 = CARTESIAN_POINT('Ctrl Pts',(-17.2165247568354,13.2283912816006,
131.162618305046)) ;
#144084 = CARTESIAN_POINT('Ctrl Pts',(-17.2020566522433,13.5192446194064,
131.153474543528)) ;
#144085 = CARTESIAN_POINT('Ctrl Pts',(-17.2127416793211,13.8035931145738,
131.217849752997)) ;
#144086 = CARTESIAN_POINT('Ctrl Pts',(-17.2472308211586,14.0607676757129,
131.351799133051)) ;
#144087 = CARTESIAN_POINT('Ctrl Pts',(-17.3018010878718,14.2709777793726,
131.544193934465)) ;
#144088 = CARTESIAN_POINT('Ctrl Pts',(-17.3726941931638,14.4220258992613,
131.784554671216)) ;
#144089 = CARTESIAN_POINT('Ctrl Pts',(-17.4533630606129,14.5004900232679,
132.053331540465)) ;
#144090 = CARTESIAN_POINT('Ctrl Pts',(-17.5372064933208,14.5020985489184,
132.331265024116)) ;
#144091 = CARTESIAN_POINT('Ctrl Pts',(-17.6181545095247,14.4266675394507,
132.600862510344)) ;
#144092 = CARTESIAN_POINT('Ctrl Pts',(-17.6895299584939,14.2786156866751,
132.842598856471)) ;
#144093 = CARTESIAN_POINT('Ctrl Pts',(-17.7450422967288,14.0697688504795,
133.037872094707)) ;
#144094 = CARTESIAN_POINT('Ctrl Pts',(-17.7803002307335,13.8142974441725,
133.174023505257)) ;
#144095 = CARTESIAN_POINT('Ctrl Pts',(-17.7919769771061,13.5318060155786,
133.241168052371)) ;
#144096 = CARTESIAN_POINT('Ctrl Pts',(-17.7786061454648,13.2403760089107,
133.235279390626)) ;
#144097 = CARTESIAN_POINT('Ctrl Pts',(-17.7401864120296,12.9618560085294,
133.156243590285)) ;
#144098 = CARTESIAN_POINT('Ctrl Pts',(-17.6790471041912,12.7173262571543,
133.010725408051)) ;
#144099 = CARTESIAN_POINT('Ctrl Pts',(-17.598858303532,12.5233446116289,132.809527661974)) ;
#144100 = CARTESIAN_POINT('Ctrl Pts',(-17.5042403431588,12.3931311939353,
132.566278115897)) ;
#144101 = CARTESIAN_POINT('Ctrl Pts',(-17.4011692780146,12.3370752417009,
132.298424229784)) ;
#144102 = CARTESIAN_POINT('Ctrl Pts',(-17.297611106788,12.35867646463,132.028824194911)) ;
#144103 = CARTESIAN_POINT('Ctrl Pts',(-17.1985322921028,12.4563696655718,
131.772543585188)) ;
#144104 = CARTESIAN_POINT('Ctrl Pts',(-17.1110977243364,12.6234424548744,
131.550255293278)) ;
#144105 = CARTESIAN_POINT('Ctrl Pts',(-17.0406693325323,12.8484690633149,
131.377731534728)) ;
#144106 = CARTESIAN_POINT('Ctrl Pts',(-16.9919310653804,13.1134860837276,
131.268405229023)) ;
#144107 = CARTESIAN_POINT('Ctrl Pts',(-16.9672563212509,13.4024250602232,
131.229587957196)) ;
#144108 = CARTESIAN_POINT('Ctrl Pts',(-16.967880389663,13.6901681965896,131.264353710665)) ;
#144109 = CARTESIAN_POINT('Ctrl Pts',(-16.9930208750078,13.9614083334907,
131.371055961702)) ;
#144110 = CARTESIAN_POINT('Ctrl Pts',(-17.0400006387744,14.1924050626967,
131.541350722063)) ;
#144111 = CARTESIAN_POINT('Ctrl Pts',(-17.1047498618222,14.3688010138631,
131.763584208451)) ;
#144112 = CARTESIAN_POINT('Ctrl Pts',(-17.1821740977121,14.4776662108143,
132.022923082352)) ;
#144113 = CARTESIAN_POINT('Ctrl Pts',(-17.2655114072571,14.5108828487548,
132.29941621485)) ;
#144114 = CARTESIAN_POINT('Ctrl Pts',(-17.3486749040906,14.4662997659133,
132.575529076312)) ;
#144115 = CARTESIAN_POINT('Ctrl Pts',(-17.424537978016,14.3468724175,132.830268759673)) ;
#144116 = CARTESIAN_POINT('Ctrl Pts',(-17.487015387752,14.1616148952727,133.045867001742)) ;
#144117 = CARTESIAN_POINT('Ctrl Pts',(-17.5310816258823,13.9230022148217,
133.20775448503)) ;
#144118 = CARTESIAN_POINT('Ctrl Pts',(-17.5526588839964,13.6485313215457,
133.303938527978)) ;
#144119 = CARTESIAN_POINT('Ctrl Pts',(-17.5495272912202,13.3583010704495,
133.327897885114)) ;
#144120 = CARTESIAN_POINT('Ctrl Pts',(-17.5212236932149,13.0725041550786,
133.278343292719)) ;
#144121 = CARTESIAN_POINT('Ctrl Pts',(-17.4689241155059,12.8117565584391,
133.158715640019)) ;
#144122 = CARTESIAN_POINT('Ctrl Pts',(-17.3961417753446,12.5955170585835,
132.979103295085)) ;
#144123 = CARTESIAN_POINT('Ctrl Pts',(-17.3060142614099,12.4369579838143,
132.749182506099)) ;
#144124 = CARTESIAN_POINT('Ctrl Pts',(-17.2063706296485,12.3507869319176,
132.491038212779)) ;
#144125 = CARTESIAN_POINT('Ctrl Pts',(-17.1019586891201,12.3404899824772,
132.219157468743)) ;
#144126 = CARTESIAN_POINT('Ctrl Pts',(-17.0000872852129,12.4078495192289,
131.954676728806)) ;
#144127 = CARTESIAN_POINT('Ctrl Pts',(-16.9070324900772,12.548387321603,131.716050913228)) ;
#144128 = CARTESIAN_POINT('Ctrl Pts',(-16.8292801740909,12.7513534766359,
131.522034622583)) ;
#144129 = CARTESIAN_POINT('Ctrl Pts',(-16.7714279753808,13.0019415175825,
131.386102341255)) ;
#144130 = CARTESIAN_POINT('Ctrl Pts',(-16.7367407995622,13.2828870424453,
131.317874613442)) ;
#144131 = CARTESIAN_POINT('Ctrl Pts',(-16.7270336805474,13.5743280761341,
131.322668167423)) ;
#144132 = CARTESIAN_POINT('Ctrl Pts',(-16.7424845135658,13.8554589732171,
131.401028165635)) ;
#144133 = CARTESIAN_POINT('Ctrl Pts',(-16.7808557497941,14.1037392604584,
131.546099387152)) ;
#144134 = CARTESIAN_POINT('Ctrl Pts',(-16.8390183501908,14.3046991320609,
131.749149752379)) ;
#144135 = CARTESIAN_POINT('Ctrl Pts',(-16.9122058795314,14.4424189349425,
131.99615822982)) ;
#144136 = CARTESIAN_POINT('Ctrl Pts',(-16.993748194292,14.5067209378496,132.267376795982)) ;
#144137 = CARTESIAN_POINT('Ctrl Pts',(-17.0779887847319,14.4936392386325,
132.54666448779)) ;
#144138 = CARTESIAN_POINT('Ctrl Pts',(-17.1574333119646,14.4040066761143,
132.811811758465)) ;
#144139 = CARTESIAN_POINT('Ctrl Pts',(-17.2262595929588,14.2433941808528,
133.046100374082)) ;
#144140 = CARTESIAN_POINT('Ctrl Pts',(-17.2781278639299,14.0252992108477,
133.230624486337)) ;
#144141 = CARTESIAN_POINT('Ctrl Pts',(-17.3092719455246,13.7626962224851,
133.354817881569)) ;
#144142 = CARTESIAN_POINT('Ctrl Pts',(-17.316267594569,13.4766512855246,133.408344106023)) ;
#144143 = CARTESIAN_POINT('Ctrl Pts',(-17.2981853151813,13.186696570853,133.388620530966)) ;
#144144 = CARTESIAN_POINT('Ctrl Pts',(-17.2551278866597,12.9123106604455,
133.296117275778)) ;
#144145 = CARTESIAN_POINT('Ctrl Pts',(-17.1902973642623,12.676940859845,133.139690042966)) ;
#144146 = CARTESIAN_POINT('Ctrl Pts',(-17.1069284764214,12.4935889461196,
132.929262064253)) ;
#144147 = CARTESIAN_POINT('Ctrl Pts',(-17.010083943622,12.3766908564608,132.679569553018)) ;
#144148 = CARTESIAN_POINT('Ctrl Pts',(-16.9066971430059,12.3352383867213,
132.41063861344)) ;
#144149 = CARTESIAN_POINT('Ctrl Pts',(-16.8031994099977,12.3713735993149,
132.141348296765)) ;
#144150 = CARTESIAN_POINT('Ctrl Pts',(-16.705881826715,12.482759025907,131.890188907889)) ;
#144151 = CARTESIAN_POINT('Ctrl Pts',(-16.6209434982664,12.6627224299211,
131.67535070706)) ;
#144152 = CARTESIAN_POINT('Ctrl Pts',(-16.5547338499338,12.8955397907263,
131.514942816909)) ;
#144153 = CARTESIAN_POINT('Ctrl Pts',(-16.5103062642366,13.1663559129077,
131.418237368089)) ;
#144154 = CARTESIAN_POINT('Ctrl Pts',(-16.4903565413196,13.4563321375684,
131.393122535293)) ;
#144155 = CARTESIAN_POINT('Ctrl Pts',(-16.4956768644731,13.7435418421396,
131.441783379302)) ;
#144156 = CARTESIAN_POINT('Ctrl Pts',(-16.5251249616778,14.0078637990346,
131.560938657713)) ;
#144157 = CARTESIAN_POINT('Ctrl Pts',(-16.5757586121628,14.2299792933114,
131.74192799708)) ;
#144158 = CARTESIAN_POINT('Ctrl Pts',(-16.6434535774873,14.3948659933446,
131.97284187312)) ;
#144159 = CARTESIAN_POINT('Ctrl Pts',(-16.7225810687213,14.489874104301,132.237167095108)) ;
#144160 = CARTESIAN_POINT('Ctrl Pts',(-16.806343644156,14.5084149170405,132.514902816577)) ;
#144161 = CARTESIAN_POINT('Ctrl Pts',(-16.8886542888971,14.4492458860129,
132.788526102146)) ;
#144162 = CARTESIAN_POINT('Ctrl Pts',(-16.9624159138355,14.3166093969371,
133.037110239956)) ;
#144163 = CARTESIAN_POINT('Ctrl Pts',(-17.0218381999614,14.1198899210566,
133.243834706)) ;
#144164 = CARTESIAN_POINT('Ctrl Pts',(-17.0618275788481,13.8734077643859,
133.393763574749)) ;
#144165 = CARTESIAN_POINT('Ctrl Pts',(-17.0788760119436,13.5947692208086,
133.476671089743)) ;
#144166 = CARTESIAN_POINT('Ctrl Pts',(-17.0709959555774,13.3033323132003,
133.486812454175)) ;
#144167 = CARTESIAN_POINT('Ctrl Pts',(-17.0379682213309,13.0207082772212,
133.423468632668)) ;
#144168 = CARTESIAN_POINT('Ctrl Pts',(-16.9816999774438,12.7676285186634,
133.292133333742)) ;
#144169 = CARTESIAN_POINT('Ctrl Pts',(-16.9050914223552,12.5604750217273,
133.101504105218)) ;
#144170 = CARTESIAN_POINT('Ctrl Pts',(-16.8128546592574,12.4152915919243,
132.865275428246)) ;
#144171 = CARTESIAN_POINT('Ctrl Pts',(-16.7117366179799,12.3428120384338,
132.602892096191)) ;
#144172 = CARTESIAN_POINT('Ctrl Pts',(-16.6069387357596,12.3473797731266,
132.329986276711)) ;
#144173 = CARTESIAN_POINT('Ctrl Pts',(-16.5062600023837,12.4294696184163,
132.069015423166)) ;
#144174 = CARTESIAN_POINT('Ctrl Pts',(-16.4162815450884,12.5816149593444,
131.839131113819)) ;
#144175 = CARTESIAN_POINT('Ctrl Pts',(-16.3416786434313,12.7949908749712,
131.654383280298)) ;
#144176 = CARTESIAN_POINT('Ctrl Pts',(-16.2877499448409,13.0541013315914,
131.530079485041)) ;
#144177 = CARTESIAN_POINT('Ctrl Pts',(-16.2578276039007,13.3386275615382,
131.47577302621)) ;
#144178 = CARTESIAN_POINT('Ctrl Pts',(-16.2529639798073,13.6281886067776,
131.494556503773)) ;
#144179 = CARTESIAN_POINT('Ctrl Pts',(-16.2727902240412,13.9042250282851,
131.585594807978)) ;
#144180 = CARTESIAN_POINT('Ctrl Pts',(-16.3153850284575,14.1463904196779,
131.743221904152)) ;
#144181 = CARTESIAN_POINT('Ctrl Pts',(-16.3770706873026,14.3364820143999,
131.956663853719)) ;
#144182 = CARTESIAN_POINT('Ctrl Pts',(-16.451653444678,14.4598817897301,132.207420357655)) ;
#144183 = CARTESIAN_POINT('Ctrl Pts',(-16.5346837427855,14.5104486172097,
132.483217139684)) ;
#144184 = CARTESIAN_POINT('Ctrl Pts',(-16.6185369661693,14.4822486282368,
132.761351628534)) ;
#144185 = CARTESIAN_POINT('Ctrl Pts',(-16.6961329602209,14.3791732925603,
133.020987830093)) ;
#144186 = CARTESIAN_POINT('Ctrl Pts',(-16.7623831735156,14.2063740239316,
133.247798110192)) ;
#144187 = CARTESIAN_POINT('Ctrl Pts',(-16.8107019337629,13.977776586442,133.422085314861)) ;
#144188 = CARTESIAN_POINT('Ctrl Pts',(-16.8373185524501,13.7109259547803,
133.5328204031)) ;
#144189 = CARTESIAN_POINT('Ctrl Pts',(-16.8396831884313,13.4211174219504,
133.572989902815)) ;
#144190 = CARTESIAN_POINT('Ctrl Pts',(-16.8168260927309,13.1336909374666,
133.539218220475)) ;
#144191 = CARTESIAN_POINT('Ctrl Pts',(-16.7697357035739,12.8658812614538,
133.434767371646)) ;
#144192 = CARTESIAN_POINT('Ctrl Pts',(-16.7003932528539,12.6367690077997,
133.265523679042)) ;
#144193 = CARTESIAN_POINT('Ctrl Pts',(-16.6141071851622,12.4658337758404,
133.046525912297)) ;
#144194 = CARTESIAN_POINT('Ctrl Pts',(-16.5159102908414,12.363124510772,132.792734881814)) ;
#144195 = CARTESIAN_POINT('Ctrl Pts',(-16.4120568421875,12.3360466249849,
132.522413241757)) ;
#144196 = CARTESIAN_POINT('Ctrl Pts',(-16.3088888182374,12.3868688211213,
132.254206294469)) ;
#144197 = CARTESIAN_POINT('Ctrl Pts',(-16.2136026177267,12.5119418808478,
132.008965625596)) ;
#144198 = CARTESIAN_POINT('Ctrl Pts',(-16.1320705940404,12.7021784508198,
131.80390923486)) ;
#144199 = CARTESIAN_POINT('Ctrl Pts',(-16.0692715430123,12.9449354906641,
131.653682319898)) ;
#144200 = CARTESIAN_POINT('Ctrl Pts',(-16.0294330752892,13.2214385193801,
131.570442661055)) ;
#144201 = CARTESIAN_POINT('Ctrl Pts',(-16.0143292105081,13.5108149265418,
131.559283090765)) ;
#144202 = CARTESIAN_POINT('Ctrl Pts',(-16.024395738529,13.7968085806489,131.621995082752)) ;
#144203 = CARTESIAN_POINT('Ctrl Pts',(-16.0581227273194,14.0536577586376,
131.753546869173)) ;
#144204 = CARTESIAN_POINT('Ctrl Pts',(-16.1122503754108,14.2659121796834,
131.944720560037)) ;
#144205 = CARTESIAN_POINT('Ctrl Pts',(-16.1826593705253,14.4185013343906,
132.183605873283)) ;
#144206 = CARTESIAN_POINT('Ctrl Pts',(-16.2630150868534,14.4992712533562,
132.451430959388)) ;
#144207 = CARTESIAN_POINT('Ctrl Pts',(-16.3472138704315,14.5031359858994,
132.730542445583)) ;
#144208 = CARTESIAN_POINT('Ctrl Pts',(-16.4282278041652,14.42962012524,133.000297431596)) ;
#144209 = CARTESIAN_POINT('Ctrl Pts',(-16.4996649079536,14.2844129921914,
133.242054084249)) ;
#144210 = CARTESIAN_POINT('Ctrl Pts',(-16.555935794527,14.07647539704,133.439668505005)) ;
#144211 = CARTESIAN_POINT('Ctrl Pts',(-16.5917569598566,13.8227945386488,
133.577374015525)) ;
#144212 = CARTESIAN_POINT('Ctrl Pts',(-16.6042213644859,13.5398700971536,
133.646937875095)) ;
#144213 = CARTESIAN_POINT('Ctrl Pts',(-16.5915381268133,13.2487715870731,
133.643011550727)) ;
#144214 = CARTESIAN_POINT('Ctrl Pts',(-16.5539869821841,12.9703360488667,
133.566419364886)) ;
#144215 = CARTESIAN_POINT('Ctrl Pts',(-16.4934594117706,12.724109148074,133.422732551231)) ;
#144216 = CARTESIAN_POINT('Ctrl Pts',(-16.4135452640998,12.5279170556122,
133.222424143852)) ;
#144217 = CARTESIAN_POINT('Ctrl Pts',(-16.3193068200252,12.3959938215062,
132.980258046712)) ;
#144218 = CARTESIAN_POINT('Ctrl Pts',(-16.2168484516887,12.3376260911869,
132.714047247702)) ;
#144219 = CARTESIAN_POINT('Ctrl Pts',(-16.1125041885171,12.3570498023057,
132.442386064704)) ;
#144220 = CARTESIAN_POINT('Ctrl Pts',(-16.0135226857535,12.4525560159372,
132.18628157101)) ;
#144221 = CARTESIAN_POINT('Ctrl Pts',(-15.925676910732,12.6176036615847,131.962785188827)) ;
#144222 = CARTESIAN_POINT('Ctrl Pts',(-15.8546709466239,12.841094749517,131.788566152118)) ;
#144223 = CARTESIAN_POINT('Ctrl Pts',(-15.8052367164706,13.1055203905307,
131.677249540122)) ;
#144224 = CARTESIAN_POINT('Ctrl Pts',(-15.7798623786128,13.3928980582864,
131.636249531326)) ;
#144225 = CARTESIAN_POINT('Ctrl Pts',(-15.7797414082747,13.682454377304,131.66902224139)) ;
#144226 = CARTESIAN_POINT('Ctrl Pts',(-15.8040952873856,13.953269278216,131.773267748027)) ;
#144227 = CARTESIAN_POINT('Ctrl Pts',(-15.8505306674575,14.1862511207232,
131.942048548818)) ;
#144228 = CARTESIAN_POINT('Ctrl Pts',(-15.9147431639295,14.3643962047435,
132.162676232254)) ;
#144229 = CARTESIAN_POINT('Ctrl Pts',(-15.9923526478993,14.4759024798905,
132.42275165957)) ;
#144230 = CARTESIAN_POINT('Ctrl Pts',(-16.0753259172169,14.5109062470025,
132.698063584178)) ;
#144231 = CARTESIAN_POINT('Ctrl Pts',(-16.1585231199198,14.4687351613561,
132.974244296309)) ;
#144232 = CARTESIAN_POINT('Ctrl Pts',(-16.2347182143026,14.3512437869113,
133.229975033208)) ;
#144233 = CARTESIAN_POINT('Ctrl Pts',(-16.2976212045528,14.1681343320696,
133.446767765667)) ;
#144234 = CARTESIAN_POINT('Ctrl Pts',(-16.342496750101,13.9291093087556,133.611240379679)) ;
#144235 = CARTESIAN_POINT('Ctrl Pts',(-16.3645583959615,13.6572014758575,
133.708608822739)) ;
#144236 = CARTESIAN_POINT('Ctrl Pts',(-16.3621600211972,13.3659145810937,
133.734856792979)) ;
#144237 = CARTESIAN_POINT('Ctrl Pts',(-16.3346204183379,13.0809590498869,
133.687391258314)) ;
#144238 = CARTESIAN_POINT('Ctrl Pts',(-16.2830794550255,12.8188858312814,
133.569993158216)) ;
#144239 = CARTESIAN_POINT('Ctrl Pts',(-16.2101996415637,12.5999509531083,
133.390335016311)) ;
#144240 = CARTESIAN_POINT('Ctrl Pts',(-16.1215938088304,12.441498416931,133.164439212171)) ;
#144241 = CARTESIAN_POINT('Ctrl Pts',(-16.0216086754502,12.3520342804443,
132.90550795831)) ;
#144242 = CARTESIAN_POINT('Ctrl Pts',(-15.9169354902678,12.339805477818,132.632949304706)) ;
#144243 = CARTESIAN_POINT('Ctrl Pts',(-15.8152636813313,12.404786593097,132.368936116434)) ;
#144244 = CARTESIAN_POINT('Ctrl Pts',(-15.7218412987795,12.543193504082,132.129236118801)) ;
#144245 = CARTESIAN_POINT('Ctrl Pts',(-15.6435355946438,12.7444967223723,
131.933608263687)) ;
#144246 = CARTESIAN_POINT('Ctrl Pts',(-15.5849489993876,12.9945027181083,
131.795604404436)) ;
#144247 = CARTESIAN_POINT('Ctrl Pts',(-15.5495839140457,13.2745331235142,
131.725353632572)) ;
#144248 = CARTESIAN_POINT('Ctrl Pts',(-15.5392180445128,13.5670628518901,
131.72835389432)) ;
#144249 = CARTESIAN_POINT('Ctrl Pts',(-15.5537810725356,13.8462372757585,
131.803808377595)) ;
#144250 = CARTESIAN_POINT('Ctrl Pts',(-15.5917625445911,14.0979242906841,
131.948022870834)) ;
#144251 = CARTESIAN_POINT('Ctrl Pts',(-15.6494094412975,14.299738463193,132.149495635102)) ;
#144252 = CARTESIAN_POINT('Ctrl Pts',(-15.7219689570077,14.4393312892027,
132.394565274966)) ;
#144253 = CARTESIAN_POINT('Ctrl Pts',(-15.8039842180224,14.5060643737482,
132.667421219409)) ;
#144254 = CARTESIAN_POINT('Ctrl Pts',(-15.8876335375387,14.4951758470579,
132.94472806509)) ;
#144255 = CARTESIAN_POINT('Ctrl Pts',(-15.9676762287012,14.4072622582047,
133.211792898155)) ;
#144256 = CARTESIAN_POINT('Ctrl Pts',(-16.036543722577,14.2495038720977,133.44600603181)) ;
#144257 = CARTESIAN_POINT('Ctrl Pts',(-16.089366133658,14.0308220187667,133.633622691749)) ;
#144258 = CARTESIAN_POINT('Ctrl Pts',(-16.120792732328,13.7719099555025,133.758281534103)) ;
#144259 = CARTESIAN_POINT('Ctrl Pts',(-16.1286533928309,13.4847455489294,
133.814530120636)) ;
#144260 = CARTESIAN_POINT('Ctrl Pts',(-16.1113129075323,13.1955424238471,
133.796861187968)) ;
#144261 = CARTESIAN_POINT('Ctrl Pts',(-16.0689855848103,12.9200552439899,
133.706524257301)) ;
#144262 = CARTESIAN_POINT('Ctrl Pts',(-16.0046877923632,12.6831184051196,
133.551684114638)) ;
#144263 = CARTESIAN_POINT('Ctrl Pts',(-15.9217483090797,12.4980281051702,
133.342521067972)) ;
#144264 = CARTESIAN_POINT('Ctrl Pts',(-15.8254049942899,12.3791543391629,
133.094225998351)) ;
#144265 = CARTESIAN_POINT('Ctrl Pts',(-15.7218252727384,12.3353503724763,
132.824832082411)) ;
#144266 = CARTESIAN_POINT('Ctrl Pts',(-15.6183467338859,12.3691099624238,
132.555553737279)) ;
#144267 = CARTESIAN_POINT('Ctrl Pts',(-15.5201912749977,12.4795856754925,
132.302167330869)) ;
#144268 = CARTESIAN_POINT('Ctrl Pts',(-15.4359387494791,12.655336096254,132.088880801219)) ;
#144269 = CARTESIAN_POINT('Ctrl Pts',(-15.3684950766273,12.8882259195335,
131.925126605676)) ;
#144270 = CARTESIAN_POINT('Ctrl Pts',(-15.3234771421884,13.1581921439883,
131.826674404974)) ;
#144271 = CARTESIAN_POINT('Ctrl Pts',(-15.3027810611371,13.4482190553547,
131.799417903735)) ;
#144272 = CARTESIAN_POINT('Ctrl Pts',(-15.3073896332409,13.7352663481711,
131.845937422089)) ;
#144273 = CARTESIAN_POINT('Ctrl Pts',(-15.3361366056611,14.0004787801146,
131.963037517509)) ;
#144274 = CARTESIAN_POINT('Ctrl Pts',(-15.3861846693765,14.224240187898,132.1423230941)) ;
#144275 = CARTESIAN_POINT('Ctrl Pts',(-15.4537984970937,14.391486040761,132.373145815163)) ;
#144276 = CARTESIAN_POINT('Ctrl Pts',(-15.5322488697613,14.4880342043903,
132.635302336254)) ;
#144277 = CARTESIAN_POINT('Ctrl Pts',(-15.6162814316108,14.508976716731,132.913959445703)) ;
#144278 = CARTESIAN_POINT('Ctrl Pts',(-15.6984885960337,14.4520806960152,
133.187177926299)) ;
#144279 = CARTESIAN_POINT('Ctrl Pts',(-15.7726891524608,14.3213934161067,
133.437089396067)) ;
#144280 = CARTESIAN_POINT('Ctrl Pts',(-15.832567950564,14.1264275067293,133.645128594592)) ;
#144281 = CARTESIAN_POINT('Ctrl Pts',(-15.8732541213187,13.8807879238241,
133.797144869293)) ;
#144282 = CARTESIAN_POINT('Ctrl Pts',(-15.8909376658887,13.6022564662603,
133.88196368139)) ;
#144283 = CARTESIAN_POINT('Ctrl Pts',(-15.8838084227577,13.3123737627951,
133.894129173828)) ;
#144284 = CARTESIAN_POINT('Ctrl Pts',(-15.8515754461964,13.0290002093282,
133.833124538385)) ;
#144285 = CARTESIAN_POINT('Ctrl Pts',(-15.7957904346099,12.7741269018416,
133.703288589335)) ;
#144286 = CARTESIAN_POINT('Ctrl Pts',(-15.7197425124795,12.5657350925596,
133.514264692283)) ;
#144287 = CARTESIAN_POINT('Ctrl Pts',(-15.6282416938175,12.4188761283997,
133.28006727262)) ;
#144288 = CARTESIAN_POINT('Ctrl Pts',(-15.5269267217761,12.3438128182006,
133.017238568564)) ;
#144289 = CARTESIAN_POINT('Ctrl Pts',(-15.4225146726752,12.346102551177,132.745334035542)) ;
#144290 = CARTESIAN_POINT('Ctrl Pts',(-15.3215773838207,12.4255736713201,
132.483612778592)) ;
#144291 = CARTESIAN_POINT('Ctrl Pts',(-15.2307667619573,12.5765458005785,
132.251460050158)) ;
#144292 = CARTESIAN_POINT('Ctrl Pts',(-15.1558846692699,12.7879288159169,
132.065806337038)) ;
#144293 = CARTESIAN_POINT('Ctrl Pts',(-15.1014092188235,13.0448055751977,
131.939778233867)) ;
#144294 = CARTESIAN_POINT('Ctrl Pts',(-15.0705529522139,13.3297564879043,
131.882857829171)) ;
#144295 = CARTESIAN_POINT('Ctrl Pts',(-15.0649638067235,13.6201108686768,
131.899596243117)) ;
#144296 = CARTESIAN_POINT('Ctrl Pts',(-15.0841303044588,13.8967555620889,
131.988701102709)) ;
#144297 = CARTESIAN_POINT('Ctrl Pts',(-15.1259754124002,14.1394984275279,
132.144042294626)) ;
#144298 = CARTESIAN_POINT('Ctrl Pts',(-15.1870982940081,14.3315002121409,
132.355832850618)) ;
#144299 = CARTESIAN_POINT('Ctrl Pts',(-15.2616606243926,14.4575223198637,
132.606660509906)) ;
#144300 = CARTESIAN_POINT('Ctrl Pts',(-15.3446502895168,14.5099977953481,
132.882369335938)) ;
#144301 = CARTESIAN_POINT('Ctrl Pts',(-15.4281132070526,14.4843800737971,
133.159177027372)) ;
#144302 = CARTESIAN_POINT('Ctrl Pts',(-15.5064015464553,14.3828781274989,
133.421023569231)) ;
#144303 = CARTESIAN_POINT('Ctrl Pts',(-15.5726872563074,14.2128161512202,
133.647745598719)) ;
#144304 = CARTESIAN_POINT('Ctrl Pts',(-15.6217981618111,13.9854781588929,
133.824413847127)) ;
#144305 = CARTESIAN_POINT('Ctrl Pts',(-15.6491464955149,13.7179644901035,
133.937462255945)) ;
#144306 = CARTESIAN_POINT('Ctrl Pts',(-15.6521578575077,13.4301920421151,
133.979322612002)) ;
#144307 = CARTESIAN_POINT('Ctrl Pts',(-15.6301625185461,13.1421055702502,
133.948099015158)) ;
#144308 = CARTESIAN_POINT('Ctrl Pts',(-15.5832226689965,12.871501287512,133.844351996978)) ;
#144309 = CARTESIAN_POINT('Ctrl Pts',(-15.5151730259063,12.6436097972574,
133.678515535288)) ;
#144310 = CARTESIAN_POINT('Ctrl Pts',(-15.4290810051553,12.469849836909,133.460215264565)) ;
#144311 = CARTESIAN_POINT('Ctrl Pts',(-15.3311482913841,12.3651221790713,
133.207186335415)) ;
#144312 = CARTESIAN_POINT('Ctrl Pts',(-15.2272564454248,12.3356922244687,
132.936789720777)) ;
#144313 = CARTESIAN_POINT('Ctrl Pts',(-15.1239058803988,12.3844432220599,
132.668069533847)) ;
#144314 = CARTESIAN_POINT('Ctrl Pts',(-15.0285056070021,12.5072148267233,
132.422427919904)) ;
#144315 = CARTESIAN_POINT('Ctrl Pts',(-14.9464192845507,12.695755079112,132.215771718577)) ;
#144316 = CARTESIAN_POINT('Ctrl Pts',(-14.8830378580334,12.9373000432248,
132.063847131515)) ;
#144317 = CARTESIAN_POINT('Ctrl Pts',(-14.8425232798133,13.2121500744088,
131.978527590025)) ;
#144318 = CARTESIAN_POINT('Ctrl Pts',(-14.8266372192779,13.503246650252,131.96529981272)) ;
#144319 = CARTESIAN_POINT('Ctrl Pts',(-14.8358595928672,13.7871081777778,
132.025232619903)) ;
#144320 = CARTESIAN_POINT('Ctrl Pts',(-14.8690306285163,14.04691061429,132.155386588116)) ;
#144321 = CARTESIAN_POINT('Ctrl Pts',(-14.922645952623,14.260565028937,132.345047723229)) ;
#144322 = CARTESIAN_POINT('Ctrl Pts',(-14.9928707940905,14.4153650292754,
132.583485979597)) ;
#144323 = CARTESIAN_POINT('Ctrl Pts',(-15.0727028439604,14.4978583100618,
132.849642817734)) ;
#144324 = CARTESIAN_POINT('Ctrl Pts',(-15.1568916183296,14.5041773759635,
133.128731323045)) ;
#144325 = CARTESIAN_POINT('Ctrl Pts',(-15.2381267118911,14.4329778405108,
133.399139072621)) ;
#144326 = CARTESIAN_POINT('Ctrl Pts',(-15.310215281974,14.2890421003468,133.642938749112)) ;
#144327 = CARTESIAN_POINT('Ctrl Pts',(-15.3668446015009,14.0827792612075,
133.841549772997)) ;
#144328 = CARTESIAN_POINT('Ctrl Pts',(-15.403218936125,13.830933510425,133.980781224856)) ;
#144329 = CARTESIAN_POINT('Ctrl Pts',(-15.416422867439,13.5483118095736,134.052537966208)) ;
#144330 = CARTESIAN_POINT('Ctrl Pts',(-15.4045116247788,13.2574775512287,
134.050827634668)) ;
#144331 = CARTESIAN_POINT('Ctrl Pts',(-15.3675972987209,12.9779695749568,
133.976150837606)) ;
#144332 = CARTESIAN_POINT('Ctrl Pts',(-15.3079074469604,12.7311578821155,
133.834812535713)) ;
#144333 = CARTESIAN_POINT('Ctrl Pts',(-15.2281264002969,12.5323979618,133.635048294444)) ;
#144334 = CARTESIAN_POINT('Ctrl Pts',(-15.1345460077119,12.3989896763175,
133.394682225535)) ;
#144335 = CARTESIAN_POINT('Ctrl Pts',(-15.0320366735209,12.3382487508946,
133.128394076734)) ;
#144336 = CARTESIAN_POINT('Ctrl Pts',(-14.9280016502807,12.3552058345121,
132.85751876148)) ;
#144337 = CARTESIAN_POINT('Ctrl Pts',(-14.828126334543,12.449068120654,132.599017361818)) ;
#144338 = CARTESIAN_POINT('Ctrl Pts',(-14.7399179314426,12.6128543666523,
132.374483440093)) ;
#144339 = CARTESIAN_POINT('Ctrl Pts',(-14.6688184323609,12.8333918946772,
132.199772246187)) ;
#144340 = CARTESIAN_POINT('Ctrl Pts',(-14.6185220942431,13.0975419716129,
132.086034661743)) ;
#144341 = CARTESIAN_POINT('Ctrl Pts',(-14.5924589370379,13.38437019925,132.042997984616)) ;
#144342 = CARTESIAN_POINT('Ctrl Pts',(-14.5916118196615,13.6749248877936,
132.073736568238)) ;
#144343 = CARTESIAN_POINT('Ctrl Pts',(-14.615388619572,13.9463602698171,132.17629151353)) ;
#144344 = CARTESIAN_POINT('Ctrl Pts',(-14.6609947039576,14.179832441143,132.34250644721)) ;
#144345 = CARTESIAN_POINT('Ctrl Pts',(-14.7251736432412,14.3606302747574,
132.563238264022)) ;
#144346 = CARTESIAN_POINT('Ctrl Pts',(-14.8018119805842,14.4733618846649,
132.820176750005)) ;
#144347 = CARTESIAN_POINT('Ctrl Pts',(-14.8854691744736,14.5110756603655,
133.097804799088)) ;
#144348 = CARTESIAN_POINT('Ctrl Pts',(-14.9682970766034,14.4709889018576,
133.372719303669)) ;
#144349 = CARTESIAN_POINT('Ctrl Pts',(-15.0449564076789,14.3556941953622,
133.629862494971)) ;
#144350 = CARTESIAN_POINT('Ctrl Pts',(-15.108481062133,14.1731666349653,133.848613132394)) ;
#144351 = CARTESIAN_POINT('Ctrl Pts',(-15.1535160847987,13.9378583888153,
134.013218034185)) ;
#144352 = CARTESIAN_POINT('Ctrl Pts',(-15.1764968053545,13.665635486159,134.113428205125)) ;
#144353 = CARTESIAN_POINT('Ctrl Pts',(-15.1748102635303,13.3744562424158,
134.141758613948)) ;
#144354 = CARTESIAN_POINT('Ctrl Pts',(-15.1479237720966,13.0885611024712,
134.096264872109)) ;
#144355 = CARTESIAN_POINT('Ctrl Pts',(-15.097140483322,12.8263305673749,133.980986925495)) ;
#144356 = CARTESIAN_POINT('Ctrl Pts',(-15.0251820302,12.6063806997543,133.803901483058)) ;
#144357 = CARTESIAN_POINT('Ctrl Pts',(-14.9363600437793,12.4447492337382,
133.577614824626)) ;
#144358 = CARTESIAN_POINT('Ctrl Pts',(-14.8365909935855,12.353502559508,133.319303022106)) ;
#144359 = CARTESIAN_POINT('Ctrl Pts',(-14.7321331307677,12.3391045182876,
133.04731904121)) ;
#144360 = CARTESIAN_POINT('Ctrl Pts',(-14.6302798500926,12.4018104838522,
132.782777505341)) ;
#144361 = CARTESIAN_POINT('Ctrl Pts',(-14.5362174086835,12.5389587593729,
132.541328494992)) ;
#144362 = CARTESIAN_POINT('Ctrl Pts',(-14.4578519480753,12.7377765995817,
132.345359393595)) ;
#144363 = CARTESIAN_POINT('Ctrl Pts',(-14.3986096579226,12.9863021610025,
132.205418010863)) ;
#144364 = CARTESIAN_POINT('Ctrl Pts',(-14.3624943762826,13.26603407284,132.133014222054)) ;
#144365 = CARTESIAN_POINT('Ctrl Pts',(-14.3513554744166,13.5582234410802,
132.133715470598)) ;
#144366 = CARTESIAN_POINT('Ctrl Pts',(-14.3652841770306,13.8387406073518,
132.20741478973)) ;
#144367 = CARTESIAN_POINT('Ctrl Pts',(-14.402398537324,14.0904926888755,132.348933832789)) ;
#144368 = CARTESIAN_POINT('Ctrl Pts',(-14.4599824766091,14.2955137272415,
132.550485329431)) ;
#144369 = CARTESIAN_POINT('Ctrl Pts',(-14.5318636954427,14.4360007562524,
132.793394148)) ;
#144370 = CARTESIAN_POINT('Ctrl Pts',(-14.6134847888935,14.5051703131075,
133.065024459182)) ;
#144371 = CARTESIAN_POINT('Ctrl Pts',(-14.6974445904021,14.4966323444729,
133.34334938671)) ;
#144372 = CARTESIAN_POINT('Ctrl Pts',(-14.7777292058018,14.4108290646986,
133.611127666164)) ;
#144373 = CARTESIAN_POINT('Ctrl Pts',(-14.8470034884994,14.2547208432748,
133.846555378337)) ;
#144374 = CARTESIAN_POINT('Ctrl Pts',(-14.9001526523347,14.0388604849956,
134.034948538747)) ;
#144375 = CARTESIAN_POINT('Ctrl Pts',(-14.9324920252192,13.7794054501878,
134.162484960282)) ;
#144376 = CARTESIAN_POINT('Ctrl Pts',(-14.9409722546491,13.4926640432345,
134.220533515023)) ;
#144377 = CARTESIAN_POINT('Ctrl Pts',(-14.9243598314647,13.2038301120676,
134.204936121479)) ;
#144378 = CARTESIAN_POINT('Ctrl Pts',(-14.8828700391429,12.9280759212708,
134.116976868931)) ;
#144379 = CARTESIAN_POINT('Ctrl Pts',(-14.8188908380602,12.6887447030163,
133.963216320727)) ;
#144380 = CARTESIAN_POINT('Ctrl Pts',(-14.7363827544312,12.5022966098147,
133.755297039805)) ;
#144381 = CARTESIAN_POINT('Ctrl Pts',(-14.6407612364118,12.3817639702232,
133.508972013868)) ;
#144382 = CARTESIAN_POINT('Ctrl Pts',(-14.5369394844871,12.3354318122153,
133.238985783327)) ;
#144383 = CARTESIAN_POINT('Ctrl Pts',(-14.4335611887344,12.3672035542546,
132.969949082775)) ;
#144384 = CARTESIAN_POINT('Ctrl Pts',(-14.3356308343994,12.4744264817991,
132.717025526438)) ;
#144385 = CARTESIAN_POINT('Ctrl Pts',(-14.2499549471161,12.6503068789,132.499956654344)) ;
#144386 = CARTESIAN_POINT('Ctrl Pts',(-14.1823507038926,12.88124813694,132.335597188222)) ;
#144387 = CARTESIAN_POINT('Ctrl Pts',(-14.1367086423717,13.1494231043328,
132.235222082954)) ;
#144388 = CARTESIAN_POINT('Ctrl Pts',(-14.1151990196335,13.4405328336443,
132.205741664821)) ;
#144389 = CARTESIAN_POINT('Ctrl Pts',(-14.1191469684865,13.7272524235385,
132.250255662763)) ;
#144390 = CARTESIAN_POINT('Ctrl Pts',(-14.1472055291928,13.9933198018618,
132.365337276901)) ;
#144391 = CARTESIAN_POINT('Ctrl Pts',(-14.1966526863445,14.2183989347204,
132.542845561358)) ;
#144392 = CARTESIAN_POINT('Ctrl Pts',(-14.263893080412,14.3876287809154,132.772603151364)) ;
#144393 = CARTESIAN_POINT('Ctrl Pts',(-14.3419899874594,14.4861871139801,
133.033682078537)) ;
#144394 = CARTESIAN_POINT('Ctrl Pts',(-14.4260278724583,14.5095212263095,
133.312380013365)) ;
#144395 = CARTESIAN_POINT('Ctrl Pts',(-14.5084628588285,14.4547286941079,
133.586299917709)) ;
#144396 = CARTESIAN_POINT('Ctrl Pts',(-14.5829405589946,14.3261104850367,
133.837000847086)) ;
#144397 = CARTESIAN_POINT('Ctrl Pts',(-14.6433221281086,14.1327423956962,
134.046521365604)) ;
#144398 = CARTESIAN_POINT('Ctrl Pts',(-14.6845889897072,13.8885304573601,
134.200204530242)) ;
#144399 = CARTESIAN_POINT('Ctrl Pts',(-14.7029647633418,13.6107522710193,
134.28704040231)) ;
#144400 = CARTESIAN_POINT('Ctrl Pts',(-14.6966560072645,13.3210540758006,
134.301585228587)) ;
#144401 = CARTESIAN_POINT('Ctrl Pts',(-14.6647660833951,13.0351249391052,
134.241836648231)) ;
#144402 = CARTESIAN_POINT('Ctrl Pts',(-14.6100670255446,12.7816148571452,
134.114864586357)) ;
#144403 = CARTESIAN_POINT('Ctrl Pts',(-14.534310267785,12.5706516748794,133.926826881026)) ;
#144404 = CARTESIAN_POINT('Ctrl Pts',(-14.4432001449626,12.4220918167394,
133.693747165107)) ;
#144405 = CARTESIAN_POINT('Ctrl Pts',(-14.3419526728907,12.3448083545055,
133.431156912992)) ;
#144406 = CARTESIAN_POINT('Ctrl Pts',(-14.2375927674014,12.3450375900235,
133.159386644344)) ;
#144407 = CARTESIAN_POINT('Ctrl Pts',(-14.1366243467377,12.4222141215766,
132.897520934609)) ;
#144408 = CARTESIAN_POINT('Ctrl Pts',(-14.0453864330863,12.5713074000372,
132.664137827729)) ;
#144409 = CARTESIAN_POINT('Ctrl Pts',(-13.9699446216825,12.7812070105723,
132.47686000557)) ;
#144410 = CARTESIAN_POINT('Ctrl Pts',(-13.9147092621739,13.0378488607775,
132.348709030643)) ;
#144411 = CARTESIAN_POINT('Ctrl Pts',(-13.8832871777118,13.3220974223082,
132.290103709443)) ;
#144412 = CARTESIAN_POINT('Ctrl Pts',(-13.8769825405473,13.611647883706,132.304649018805)) ;
#144413 = CARTESIAN_POINT('Ctrl Pts',(-13.8955086499777,13.8896345343945,
132.39196295235)) ;
#144414 = CARTESIAN_POINT('Ctrl Pts',(-13.9366753833046,14.1329049356831,
132.54523713465)) ;
#144415 = CARTESIAN_POINT('Ctrl Pts',(-13.9972054024135,14.3266158098986,
132.755265210383)) ;
#144416 = CARTESIAN_POINT('Ctrl Pts',(-14.0717046716822,14.4550272244897,
133.006018843489)) ;
#144417 = CARTESIAN_POINT('Ctrl Pts',(-14.1542914623274,14.5094869188899,
133.280440740806)) ;
#144418 = CARTESIAN_POINT('Ctrl Pts',(-14.23786007523,14.4863254941317,133.55757350622)) ;
#144419 = CARTESIAN_POINT('Ctrl Pts',(-14.3164953259384,14.3868080621077,
133.820474949002)) ;
#144420 = CARTESIAN_POINT('Ctrl Pts',(-14.3832481636959,14.2186053489218,
134.048567565763)) ;
#144421 = CARTESIAN_POINT('Ctrl Pts',(-14.433013492223,13.9916146636668,134.227276700998)) ;
#144422 = CARTESIAN_POINT('Ctrl Pts',(-14.4608459895121,13.7271394613145,
134.341473276466)) ;
#144423 = CARTESIAN_POINT('Ctrl Pts',(-14.4646255722011,13.4373621630931,
134.385853195471)) ;
#144424 = CARTESIAN_POINT('Ctrl Pts',(-14.443349249692,13.1504054567353,134.35656690841)) ;
#144425 = CARTESIAN_POINT('Ctrl Pts',(-14.3970798767142,12.8786465082132,
134.254813797913)) ;
#144426 = CARTESIAN_POINT('Ctrl Pts',(-14.3297712578551,12.6500332847712,
134.091052737694)) ;
#144427 = CARTESIAN_POINT('Ctrl Pts',(-14.2443077145905,12.4743183889617,
133.874546811681)) ;
#144428 = CARTESIAN_POINT('Ctrl Pts',(-14.1459829063076,12.3668547885935,
133.620592382301)) ;
#144429 = CARTESIAN_POINT('Ctrl Pts',(-14.0426593854965,12.3355629410877,
133.35169506941)) ;
#144430 = CARTESIAN_POINT('Ctrl Pts',(-13.9392469880479,12.3817108160481,
133.082773805456)) ;
#144431 = CARTESIAN_POINT('Ctrl Pts',(-13.843143436717,12.5028398511796,132.835204825882)) ;
#144432 = CARTESIAN_POINT('Ctrl Pts',(-13.7605436154981,12.6903514923922,
132.627110847511)) ;
#144433 = CARTESIAN_POINT('Ctrl Pts',(-13.6970335294607,12.9285060131068,
132.474531325953)) ;
#144434 = CARTESIAN_POINT('Ctrl Pts',(-13.6554462176405,13.2046732930674,
132.386338568047)) ;
#144435 = CARTESIAN_POINT('Ctrl Pts',(-13.6389656541903,13.4951334329262,
132.371307889567)) ;
#144436 = CARTESIAN_POINT('Ctrl Pts',(-13.6475068620829,13.7795013395347,
132.429266393857)) ;
#144437 = CARTESIAN_POINT('Ctrl Pts',(-13.679877816188,14.0394109591315,132.556955498111)) ;
#144438 = CARTESIAN_POINT('Ctrl Pts',(-13.7330862586516,14.2552142278511,
132.745523563383)) ;
#144439 = CARTESIAN_POINT('Ctrl Pts',(-13.8025719368285,14.4112842986504,
132.981643339771)) ;
#144440 = CARTESIAN_POINT('Ctrl Pts',(-13.8823995551984,14.4966304081093,
133.247890097308)) ;
#144441 = CARTESIAN_POINT('Ctrl Pts',(-13.9669897571776,14.5049768575903,
133.528313290587)) ;
#144442 = CARTESIAN_POINT('Ctrl Pts',(-14.0479944860348,14.4360834976797,
133.797890686312)) ;
#144443 = CARTESIAN_POINT('Ctrl Pts',(-14.1203483029127,14.2946512650185,
134.04240392863)) ;
#144444 = CARTESIAN_POINT('Ctrl Pts',(-14.1776079248902,14.0899138392311,
134.242893869283)) ;
#144445 = CARTESIAN_POINT('Ctrl Pts',(-14.2147355846971,13.8386915040984,
134.384396464482)) ;
#144446 = CARTESIAN_POINT('Ctrl Pts',(-14.2285960401478,13.5555689993548,
134.45818874425)) ;
#144447 = CARTESIAN_POINT('Ctrl Pts',(-14.2174370565147,13.2663899085958,
134.458484095202)) ;
#144448 = CARTESIAN_POINT('Ctrl Pts',(-14.1812851642328,12.9858845454111,
134.386068426283)) ;
#144449 = CARTESIAN_POINT('Ctrl Pts',(-14.1220605741677,12.737510093137,134.246152635889)) ;
#144450 = CARTESIAN_POINT('Ctrl Pts',(-14.0430821999498,12.5376375211986,
134.048618882787)) ;
#144451 = CARTESIAN_POINT('Ctrl Pts',(-13.9493516901009,12.4015826391132,
133.807988055911)) ;
#144452 = CARTESIAN_POINT('Ctrl Pts',(-13.847485963073,12.3390360778661,133.543416015632)) ;
#144453 = CARTESIAN_POINT('Ctrl Pts',(-13.7431811033581,12.3535754317009,
133.271827404683)) ;
#144454 = CARTESIAN_POINT('Ctrl Pts',(-13.6431991335962,12.4452741320202,
133.012975789816)) ;
#144455 = CARTESIAN_POINT('Ctrl Pts',(-13.5545881261613,12.6067972439988,
132.78723888543)) ;
#144456 = CARTESIAN_POINT('Ctrl Pts',(-13.4825179247784,12.8274893323333,
132.609914210707)) ;
#144457 = CARTESIAN_POINT('Ctrl Pts',(-13.4319485828918,13.0891409681253,
132.495170039007)) ;
#144458 = CARTESIAN_POINT('Ctrl Pts',(-13.405076521648,13.3757401842095,132.449797594403)) ;
#144459 = CARTESIAN_POINT('Ctrl Pts',(-13.403495750014,13.6659116467556,132.478325630475)) ;
#144460 = CARTESIAN_POINT('Ctrl Pts',(-13.4264445635729,13.9383430933064,
132.578458762523)) ;
#144461 = CARTESIAN_POINT('Ctrl Pts',(-13.4718993493954,14.1747318891546,
132.74449081178)) ;
#144462 = CARTESIAN_POINT('Ctrl Pts',(-13.5350003238588,14.3556000253484,
132.961746054639)) ;
#144463 = CARTESIAN_POINT('Ctrl Pts',(-13.6120266374697,14.4715471838241,
133.220125893983)) ;
#144464 = CARTESIAN_POINT('Ctrl Pts',(-13.6950425828247,14.5109306883494,
133.495651568683)) ;
#144465 = CARTESIAN_POINT('Ctrl Pts',(-13.7781244502882,14.4734197529204,
133.771367920486)) ;
#144466 = CARTESIAN_POINT('Ctrl Pts',(-13.8553206961182,14.3595613324345,
134.030197068802)) ;
#144467 = CARTESIAN_POINT('Ctrl Pts',(-13.9189983306387,14.1794661673076,
134.249255457911)) ;
#144468 = CARTESIAN_POINT('Ctrl Pts',(-13.9647465680392,13.945518104717,134.415965062651)) ;
#144469 = CARTESIAN_POINT('Ctrl Pts',(-13.9884352930972,13.6723045433651,
134.518446435358)) ;
#144470 = CARTESIAN_POINT('Ctrl Pts',(-13.9874200608317,13.3834915419228,
134.548487177175)) ;
#144471 = CARTESIAN_POINT('Ctrl Pts',(-13.961292173295,13.096613347718,134.505276795414)) ;
#144472 = CARTESIAN_POINT('Ctrl Pts',(-13.9110701574395,12.8330520382444,
134.391683767702)) ;
#144473 = CARTESIAN_POINT('Ctrl Pts',(-13.8394412414765,12.611232367513,134.215641479407)) ;
#144474 = CARTESIAN_POINT('Ctrl Pts',(-13.7510797643784,12.4482428501487,
133.990655184354)) ;
#144475 = CARTESIAN_POINT('Ctrl Pts',(-13.6520098987817,12.3553252132509,
133.734233775121)) ;
#144476 = CARTESIAN_POINT('Ctrl Pts',(-13.5477078598646,12.3382107203878,
133.462666865456)) ;
#144477 = CARTESIAN_POINT('Ctrl Pts',(-13.4451051943709,12.3992481995866,
133.196136133625)) ;
#144478 = CARTESIAN_POINT('Ctrl Pts',(-13.3515020692413,12.533120575299,132.955737055526)) ;
#144479 = CARTESIAN_POINT('Ctrl Pts',(-13.2721063140921,12.7309389352082,
132.75693541364)) ;
#144480 = CARTESIAN_POINT('Ctrl Pts',(-13.2121057414651,12.9791526214122,
132.614875968898)) ;
#144481 = CARTESIAN_POINT('Ctrl Pts',(-13.1753406281424,13.2585792633392,
132.540604769992)) ;
#144482 = CARTESIAN_POINT('Ctrl Pts',(-13.1635578925844,13.5499400001449,
132.539336578873)) ;
#144483 = CARTESIAN_POINT('Ctrl Pts',(-13.1767327841943,13.831171440361,132.610841057035)) ;
#144484 = CARTESIAN_POINT('Ctrl Pts',(-13.2135052261466,14.0848087373092,
132.751501701129)) ;
#144485 = CARTESIAN_POINT('Ctrl Pts',(-13.2698735591139,14.2892042753313,
132.949112869563)) ;
#144486 = CARTESIAN_POINT('Ctrl Pts',(-13.3419495547469,14.4332159857665,
133.192881784659)) ;
#144487 = CARTESIAN_POINT('Ctrl Pts',(-13.4232398552977,14.5042074008981,
133.463464415944)) ;
#144488 = CARTESIAN_POINT('Ctrl Pts',(-13.507384649746,14.4978850234615,133.742403717604)) ;
#144489 = CARTESIAN_POINT('Ctrl Pts',(-13.5875958441071,14.4145533230364,
134.009844183663)) ;
#144490 = CARTESIAN_POINT('Ctrl Pts',(-13.6574499514611,14.2600829811303,
134.24704991028)) ;
#144491 = CARTESIAN_POINT('Ctrl Pts',(-13.711063219599,14.0459658246631,134.436755953918)) ;
#144492 = CARTESIAN_POINT('Ctrl Pts',(-13.7440726911672,13.7875806302573,
134.566251929894)) ;
#144493 = CARTESIAN_POINT('Ctrl Pts',(-13.7533105607091,13.5015007624486,
134.626490095641)) ;
#144494 = CARTESIAN_POINT('Ctrl Pts',(-13.7373844729382,13.2119710918027,
134.612963509928)) ;
#144495 = CARTESIAN_POINT('Ctrl Pts',(-13.6967466416228,12.9363052863804,
134.527385775247)) ;
#144496 = CARTESIAN_POINT('Ctrl Pts',(-13.6333101280341,12.6952735982691,
134.375265595291)) ;
#144497 = CARTESIAN_POINT('Ctrl Pts',(-13.5514819956674,12.5071256429724,
134.169269681796)) ;
#144498 = CARTESIAN_POINT('Ctrl Pts',(-13.4552564937098,12.383762838378,133.921486273109)) ;
#144499 = CARTESIAN_POINT('Ctrl Pts',(-13.3526734621167,12.3357954087545,
133.654750351329)) ;
#144500 = CARTESIAN_POINT('Ctrl Pts',(-13.248390208345,12.3652711313032,133.383338134123)) ;
#144501 = CARTESIAN_POINT('Ctrl Pts',(-13.1504948799325,12.4705156862028,
133.130424748745)) ;
#144502 = CARTESIAN_POINT('Ctrl Pts',(-13.064631594807,12.6439184984734,132.912710120954)) ;
#144503 = CARTESIAN_POINT('Ctrl Pts',(-12.9963758778862,12.8730354014428,
132.746418369545)) ;
#144504 = CARTESIAN_POINT('Ctrl Pts',(-12.9497883269641,13.1424159380097,
132.643529935982)) ;
#144505 = CARTESIAN_POINT('Ctrl Pts',(-12.9277522729892,13.4306391713404,
132.612207026215)) ;
#144506 = CARTESIAN_POINT('Ctrl Pts',(-12.9308623319706,13.7191539467883,
132.654442340638)) ;
#144507 = CARTESIAN_POINT('Ctrl Pts',(-12.9582863068314,13.9861294006722,
132.767666480281)) ;
#144508 = CARTESIAN_POINT('Ctrl Pts',(-13.007269468484,14.2128684177951,132.943873402988)) ;
#144509 = CARTESIAN_POINT('Ctrl Pts',(-13.0737783621588,14.3833348165239,
133.171349191452)) ;
#144510 = CARTESIAN_POINT('Ctrl Pts',(-13.1520175298029,14.4845639234701,
133.433016513638)) ;
#144511 = CARTESIAN_POINT('Ctrl Pts',(-13.2357654256101,14.5099092452808,
133.710770485551)) ;
#144512 = CARTESIAN_POINT('Ctrl Pts',(-13.3184724571213,14.4573340950599,
133.985540682199)) ;
#144513 = CARTESIAN_POINT('Ctrl Pts',(-13.3932587277117,14.3305257687139,
134.237149673029)) ;
#144514 = CARTESIAN_POINT('Ctrl Pts',(-13.453959624611,14.1393929887669,134.447512911923)) ;
#144515 = CARTESIAN_POINT('Ctrl Pts',(-13.4959188907949,13.8963011605845,
134.60324810303)) ;
#144516 = CARTESIAN_POINT('Ctrl Pts',(-13.5150245929042,13.6185277978384,
134.692292652566)) ;
#144517 = CARTESIAN_POINT('Ctrl Pts',(-13.5093297939817,13.3290636880528,
134.708618703529)) ;
#144518 = CARTESIAN_POINT('Ctrl Pts',(-13.478487997988,13.0445547365035,134.651695864734)) ;
#144519 = CARTESIAN_POINT('Ctrl Pts',(-13.4240438635045,12.7876682378207,
134.525750731676)) ;
#144520 = CARTESIAN_POINT('Ctrl Pts',(-13.3486520787745,12.5753841966509,
134.33879441597)) ;
#144521 = CARTESIAN_POINT('Ctrl Pts',(-13.2582557575008,12.4255193729721,
134.107675530931)) ;
#144522 = CARTESIAN_POINT('Ctrl Pts',(-13.1571893879613,12.3459765323798,
133.845622114518)) ;
#144523 = CARTESIAN_POINT('Ctrl Pts',(-13.052964824145,12.3439073605975,133.574205697266)) ;
#144524 = CARTESIAN_POINT('Ctrl Pts',(-12.9516198217642,12.4188280799993,
133.3112916701)) ;
#144525 = CARTESIAN_POINT('Ctrl Pts',(-12.8596716620883,12.5669348779127,
133.075980414901)) ;
#144526 = CARTESIAN_POINT('Ctrl Pts',(-12.7842079537086,12.7740278443755,
132.888427019291)) ;
#144527 = CARTESIAN_POINT('Ctrl Pts',(-12.7281316399476,13.0302841857639,
132.757923355197)) ;
#144528 = CARTESIAN_POINT('Ctrl Pts',(-12.6960840940017,13.313391034623,132.697410502884)) ;
#144529 = CARTESIAN_POINT('Ctrl Pts',(-12.6890448913152,13.603463825877,132.70986693963)) ;
#144530 = CARTESIAN_POINT('Ctrl Pts',(-12.7067501795814,13.881303539034,132.794671056419)) ;
#144531 = CARTESIAN_POINT('Ctrl Pts',(-12.7476563868859,14.1277804532013,
132.947459523477)) ;
#144532 = CARTESIAN_POINT('Ctrl Pts',(-12.807668461047,14.3222500271651,133.155884784261)) ;
#144533 = CARTESIAN_POINT('Ctrl Pts',(-12.8815759825536,14.4521801534422,
133.404796235282)) ;
#144534 = CARTESIAN_POINT('Ctrl Pts',(-12.9639114339177,14.5090397064551,
133.678440955096)) ;
#144535 = CARTESIAN_POINT('Ctrl Pts',(-13.0478748509612,14.4879536180509,
133.956866936907)) ;
#144536 = CARTESIAN_POINT('Ctrl Pts',(-13.12663874727,14.3907168838663,134.220082699091)) ;
#144537 = CARTESIAN_POINT('Ctrl Pts',(-13.1940374997755,14.2230874548014,
134.450238889046)) ;
#144538 = CARTESIAN_POINT('Ctrl Pts',(-13.2437494985685,14.0008520915057,
134.628318458797)) ;
#144539 = CARTESIAN_POINT('Ctrl Pts',(-13.2726507285596,13.7343152411408,
134.746038138861)) ;
#144540 = CARTESIAN_POINT('Ctrl Pts',(-13.2771331648552,13.4474451384185,
134.7921586958)) ;
#144541 = CARTESIAN_POINT('Ctrl Pts',(-13.2564031610437,13.1575373566889,
134.764792024668)) ;
#144542 = CARTESIAN_POINT('Ctrl Pts',(-13.2113358398759,12.8878586213282,
134.666175549562)) ;
#144543 = CARTESIAN_POINT('Ctrl Pts',(-13.1441355018156,12.6555337208909,
134.503032248599)) ;
#144544 = CARTESIAN_POINT('Ctrl Pts',(-13.059137517177,12.4784852889698,134.287843551478)) ;
#144545 = CARTESIAN_POINT('Ctrl Pts',(-12.9611258595703,12.3688435118071,
134.034798276015)) ;
#144546 = CARTESIAN_POINT('Ctrl Pts',(-12.8576569308719,12.3353790498827,
133.765544543762)) ;
#144547 = CARTESIAN_POINT('Ctrl Pts',(-12.7543421492588,12.3794309096132,
133.496846744508)) ;
#144548 = CARTESIAN_POINT('Ctrl Pts',(-12.6581868323014,12.4979553163596,
133.249029548583)) ;
#144549 = CARTESIAN_POINT('Ctrl Pts',(-12.5748068823933,12.6843641883006,
133.038779090593)) ;
#144550 = CARTESIAN_POINT('Ctrl Pts',(-12.5108333068289,12.9208195747622,
132.884779860558)) ;
#144551 = CARTESIAN_POINT('Ctrl Pts',(-12.4685180268136,13.1965599985602,
132.794503935178)) ;
#144552 = CARTESIAN_POINT('Ctrl Pts',(-12.4513334564237,13.4854151022566,
132.777251050598)) ;
#144553 = CARTESIAN_POINT('Ctrl Pts',(-12.4590824100926,13.7715246215189,
132.833039729551)) ;
#144554 = CARTESIAN_POINT('Ctrl Pts',(-12.4909465763308,14.0329604460064,
132.959323426921)) ;
#144555 = CARTESIAN_POINT('Ctrl Pts',(-12.543481678053,14.2495175049027,133.145827922929)) ;
#144556 = CARTESIAN_POINT('Ctrl Pts',(-12.6124777949629,14.4077222066367,
133.380496347068)) ;
#144557 = CARTESIAN_POINT('Ctrl Pts',(-12.6927510621182,14.4954975109272,
133.648307749174)) ;
#144558 = CARTESIAN_POINT('Ctrl Pts',(-12.7765296871443,14.5058124049383,
133.926043997693)) ;
#144559 = CARTESIAN_POINT('Ctrl Pts',(-12.8581519695846,14.4390539454557,
134.197602951378)) ;
#144560 = CARTESIAN_POINT('Ctrl Pts',(-12.930945670173,14.2988993787837,134.443466881682)) ;
#144561 = CARTESIAN_POINT('Ctrl Pts',(-12.9885263190073,14.0959845150152,
134.644827585225)) ;
#144562 = CARTESIAN_POINT('Ctrl Pts',(-13.0261259536014,13.8467236092075,
134.787597338179)) ;
#144563 = CARTESIAN_POINT('Ctrl Pts',(-13.0407617343322,13.5651497445093,
134.863551637252)) ;
#144564 = CARTESIAN_POINT('Ctrl Pts',(-13.0303516451087,13.2745208567972,
134.866196431429)) ;
#144565 = CARTESIAN_POINT('Ctrl Pts',(-12.9947636873513,12.9930479903862,
134.795477148735)) ;
#144566 = CARTESIAN_POINT('Ctrl Pts',(-12.9363121229771,12.744268366307,134.657724887669)) ;
#144567 = CARTESIAN_POINT('Ctrl Pts',(-12.8579516687104,12.5428868462353,
134.461961866201)) ;
#144568 = CARTESIAN_POINT('Ctrl Pts',(-12.764650310326,12.4047082626809,134.222565644588)) ;
#144569 = CARTESIAN_POINT('Ctrl Pts',(-12.6626217646199,12.3396945376806,
133.957623570518)) ;
#144570 = CARTESIAN_POINT('Ctrl Pts',(-12.5583566636078,12.3521469878651,
133.68612910926)) ;
#144571 = CARTESIAN_POINT('Ctrl Pts',(-12.4583830396902,12.4413144196275,
133.42721791323)) ;
#144572 = CARTESIAN_POINT('Ctrl Pts',(-12.369233426393,12.6011044167591,133.199955438854)) ;
#144573 = CARTESIAN_POINT('Ctrl Pts',(-12.296795109846,12.8194225372239,133.021442997756)) ;
#144574 = CARTESIAN_POINT('Ctrl Pts',(-12.245256136277,13.0811435285209,132.904014857809)) ;
#144575 = CARTESIAN_POINT('Ctrl Pts',(-12.2176939794846,13.3679218651448,
132.856686794612)) ;
#144576 = CARTESIAN_POINT('Ctrl Pts',(-12.2154180287801,13.6574454628282,
132.883090037096)) ;
#144577 = CARTESIAN_POINT('Ctrl Pts',(-12.2376037442581,13.9304219315962,
132.980959807401)) ;
#144578 = CARTESIAN_POINT('Ctrl Pts',(-12.2824887862547,14.1686008809453,
133.145375342875)) ;
#144579 = CARTESIAN_POINT('Ctrl Pts',(-12.3453046157036,14.3514046906987,
133.361866425527)) ;
#144580 = CARTESIAN_POINT('Ctrl Pts',(-12.4215524934275,14.4688537021457,
133.617768892991)) ;
#144581 = CARTESIAN_POINT('Ctrl Pts',(-12.5047937799249,14.5110084059665,
133.894090918055)) ;
#144582 = CARTESIAN_POINT('Ctrl Pts',(-12.5880891539146,14.4754271671864,
134.170481851329)) ;
#144583 = CARTESIAN_POINT('Ctrl Pts',(-12.6653082061899,14.3641624837098,
134.429260025213)) ;
#144584 = CARTESIAN_POINT('Ctrl Pts',(-12.7297019423071,14.1852632714168,
134.650534523629)) ;
#144585 = CARTESIAN_POINT('Ctrl Pts',(-12.7759253627988,13.9526451363771,
134.818608665659)) ;
#144586 = CARTESIAN_POINT('Ctrl Pts',(-12.8002263769998,13.6818446977071,
134.922696351685)) ;
#144587 = CARTESIAN_POINT('Ctrl Pts',(-12.8000986222463,13.3926206183681,
134.955407057366)) ;
#144588 = CARTESIAN_POINT('Ctrl Pts',(-12.7745111191584,13.1038754492096,
134.91394806215)) ;
#144589 = CARTESIAN_POINT('Ctrl Pts',(-12.7250570523891,12.840383579606,134.802482892193)) ;
#144590 = CARTESIAN_POINT('Ctrl Pts',(-12.6542480453106,12.6175434058043,
134.628747907332)) ;
#144591 = CARTESIAN_POINT('Ctrl Pts',(-12.5661484572041,12.452017834643,134.40460207524)) ;
#144592 = CARTESIAN_POINT('Ctrl Pts',(-12.466810665612,12.3567780373273,134.147557352768)) ;
#144593 = CARTESIAN_POINT('Ctrl Pts',(-12.3630998015103,12.3376561181457,
133.877541645615)) ;
#144594 = CARTESIAN_POINT('Ctrl Pts',(-12.2602167543945,12.3963495269004,
133.610232883161)) ;
#144595 = CARTESIAN_POINT('Ctrl Pts',(-12.1662740877371,12.5282530119487,
133.36884192798)) ;
#144596 = CARTESIAN_POINT('Ctrl Pts',(-12.0863990846921,12.7243874356401,
133.168638276115)) ;
#144597 = CARTESIAN_POINT('Ctrl Pts',(-12.0258318101677,12.9708925599776,
133.024863858059)) ;
#144598 = CARTESIAN_POINT('Ctrl Pts',(-11.9882998267701,13.2502128136118,
132.948421366033)) ;
#144599 = CARTESIAN_POINT('Ctrl Pts',(-11.9757436014194,13.5400585853171,
132.944721817268)) ;
#144600 = CARTESIAN_POINT('Ctrl Pts',(-11.9882527010253,13.8239340251458,
133.014527571327)) ;
#144601 = CARTESIAN_POINT('Ctrl Pts',(-12.024314175027,14.0777678447128,133.152994495197)) ;
#144602 = CARTESIAN_POINT('Ctrl Pts',(-12.0802386867807,14.2841379825029,
133.349369470604)) ;
#144603 = CARTESIAN_POINT('Ctrl Pts',(-12.1517568327263,14.4298157397374,
133.591419824173)) ;
#144604 = CARTESIAN_POINT('Ctrl Pts',(-12.2331386991357,14.5033259419055,
133.862387548151)) ;
#144605 = CARTESIAN_POINT('Ctrl Pts',(-12.3172490667229,14.499135083616,134.141203152847)) ;
#144606 = CARTESIAN_POINT('Ctrl Pts',(-12.3977223834432,14.4177797503692,
134.409440590375)) ;
#144607 = CARTESIAN_POINT('Ctrl Pts',(-12.4677306111638,14.2657375874764,
134.646986738776)) ;
#144608 = CARTESIAN_POINT('Ctrl Pts',(-12.5220714640845,14.0527572687347,
134.838901719408)) ;
#144609 = CARTESIAN_POINT('Ctrl Pts',(-12.5557480287328,13.7942042748117,
134.970478170915)) ;
#144610 = CARTESIAN_POINT('Ctrl Pts',(-12.5655893514791,13.5099720674089,
135.032313082312)) ;
#144611 = CARTESIAN_POINT('Ctrl Pts',(-12.5503883535898,13.2198346279653,
135.020961803302)) ;
#144612 = CARTESIAN_POINT('Ctrl Pts',(-12.5103698968678,12.943315390008,134.937211770159)) ;
#144613 = CARTESIAN_POINT('Ctrl Pts',(-12.4473782776272,12.7008041601945,
134.786440487952)) ;
#144614 = CARTESIAN_POINT('Ctrl Pts',(-12.3662789009973,12.5118987867612,
134.582448501668)) ;
#144615 = CARTESIAN_POINT('Ctrl Pts',(-12.2708904646129,12.3867144274878,
134.336948453018)) ;
#144616 = CARTESIAN_POINT('Ctrl Pts',(-12.1678380844892,12.3359851179155,
134.069036435236)) ;
#144617 = CARTESIAN_POINT('Ctrl Pts',(-12.0635192151034,12.3634203975105,
133.797509645721)) ;
#144618 = CARTESIAN_POINT('Ctrl Pts',(-11.9653834956935,12.4663876776292,
133.543880463579)) ;
#144619 = CARTESIAN_POINT('Ctrl Pts',(-11.8787531345459,12.638970046877,133.32407434828)) ;
#144620 = CARTESIAN_POINT('Ctrl Pts',(-11.8103116788291,12.8657476347374,
133.157082057629)) ;
#144621 = CARTESIAN_POINT('Ctrl Pts',(-11.7629363114797,13.1346340040003,
133.051944760251)) ;
#144622 = CARTESIAN_POINT('Ctrl Pts',(-11.74782998282,13.3266515427633,133.029855138178)) ;
#144623 = CARTESIAN_POINT('Ctrl Pts',(-11.7444305159761,13.4226803244344,
133.030945169693)) ;
#144624 = CARTESIAN_POINT('Ctrl Pts',(-33.2300180027834,13.1368456608817,
127.989533782136)) ;
#144625 = CARTESIAN_POINT('Ctrl Pts',(-33.2292437520727,13.130243425216,127.988002960232)) ;
#144626 = CARTESIAN_POINT('Ctrl Pts',(-33.2166096866017,13.0249708380281,
127.962778125839)) ;
#144627 = CARTESIAN_POINT('Ctrl Pts',(-33.182092795898,12.8263019600079,127.884920491647)) ;
#144628 = CARTESIAN_POINT('Ctrl Pts',(-33.1092916050684,12.5833994930382,
127.705272326551)) ;
#144629 = CARTESIAN_POINT('Ctrl Pts',(-33.0177478422943,12.399626766211,127.470955863714)) ;
#144630 = CARTESIAN_POINT('Ctrl Pts',(-32.9127470434696,12.2890731618772,
127.197495494478)) ;
#144631 = CARTESIAN_POINT('Ctrl Pts',(-32.8027864649256,12.2602312948732,
126.909202090255)) ;
#144632 = CARTESIAN_POINT('Ctrl Pts',(-32.6929501385259,12.3144254522227,
126.621568480859)) ;
#144633 = CARTESIAN_POINT('Ctrl Pts',(-32.59177016842,12.4480642946114,126.359088261639)) ;
#144634 = CARTESIAN_POINT('Ctrl Pts',(-32.5051791199469,12.6516399899179,
126.139277587465)) ;
#144635 = CARTESIAN_POINT('Ctrl Pts',(-32.4388702329151,12.9104453038702,
125.97869600614)) ;
#144636 = CARTESIAN_POINT('Ctrl Pts',(-32.3968275748835,13.2058492691314,
125.888992944671)) ;
#144637 = CARTESIAN_POINT('Ctrl Pts',(-32.3812336706731,13.5166185684314,
125.876529755364)) ;
#144638 = CARTESIAN_POINT('Ctrl Pts',(-32.3927205422695,13.8224101024019,
125.943375492965)) ;
#144639 = CARTESIAN_POINT('Ctrl Pts',(-32.4293470746311,14.0967865746008,
126.083332512321)) ;
#144640 = CARTESIAN_POINT('Ctrl Pts',(-32.4880514233328,14.3244563595429,
126.287951913574)) ;
#144641 = CARTESIAN_POINT('Ctrl Pts',(-32.5638474430166,14.4874742407207,
126.54248591268)) ;
#144642 = CARTESIAN_POINT('Ctrl Pts',(-32.6508225706577,14.5744205093284,
126.829774468175)) ;
#144643 = CARTESIAN_POINT('Ctrl Pts',(-32.7415381559199,14.5784621609188,
127.127897337849)) ;
#144644 = CARTESIAN_POINT('Ctrl Pts',(-32.8288658284697,14.5000469368875,
127.416073622444)) ;
#144645 = CARTESIAN_POINT('Ctrl Pts',(-32.9060635890902,14.344572658684,127.67469123317)) ;
#144646 = CARTESIAN_POINT('Ctrl Pts',(-32.9668884901517,14.1228337492368,
127.88552736943)) ;
#144647 = CARTESIAN_POINT('Ctrl Pts',(-33.0061004434272,13.8501516005036,
128.033299850844)) ;
#144648 = CARTESIAN_POINT('Ctrl Pts',(-33.0200491726642,13.5490422759736,
128.107026504832)) ;
#144649 = CARTESIAN_POINT('Ctrl Pts',(-33.0073427737607,13.2374716075454,
128.103049880758)) ;
#144650 = CARTESIAN_POINT('Ctrl Pts',(-32.9677468015857,12.9386843836575,
128.020588082111)) ;
#144651 = CARTESIAN_POINT('Ctrl Pts',(-32.9039626552368,12.6761376580761,
127.867269826708)) ;
#144652 = CARTESIAN_POINT('Ctrl Pts',(-32.8190967106854,12.4657586342273,
127.652552845677)) ;
#144653 = CARTESIAN_POINT('Ctrl Pts',(-32.7191980487996,12.3246285440834,
127.39379148403)) ;
#144654 = CARTESIAN_POINT('Ctrl Pts',(-32.6098826596707,12.2619062203987,
127.107681420346)) ;
#144655 = CARTESIAN_POINT('Ctrl Pts',(-32.4994620023921,12.282438847825,126.818116882423)) ;
#144656 = CARTESIAN_POINT('Ctrl Pts',(-32.3937285710348,12.3848777791117,
126.542455056202)) ;
#144657 = CARTESIAN_POINT('Ctrl Pts',(-32.3006102621747,12.5614992054213,
126.303522073794)) ;
#144658 = CARTESIAN_POINT('Ctrl Pts',(-32.2255196684499,12.7995868451149,
126.117262217641)) ;
#144659 = CARTESIAN_POINT('Ctrl Pts',(-32.1730545330911,13.0840300183346,
125.99727657049)) ;
#144660 = CARTESIAN_POINT('Ctrl Pts',(-32.1467969822621,13.3899587420559,
125.953531154388)) ;
#144661 = CARTESIAN_POINT('Ctrl Pts',(-32.147224199752,13.6996411471026,125.987893566941)) ;
#144662 = CARTESIAN_POINT('Ctrl Pts',(-32.1740653691313,13.9903747367888,
126.099519807881)) ;
#144663 = CARTESIAN_POINT('Ctrl Pts',(-32.2243898321981,14.2393240379775,
126.279618857538)) ;
#144664 = CARTESIAN_POINT('Ctrl Pts',(-32.2938170416811,14.4298400275378,
126.51549169053)) ;
#144665 = CARTESIAN_POINT('Ctrl Pts',(-32.3768965968871,14.5487685200995,
126.791305226358)) ;
#144666 = CARTESIAN_POINT('Ctrl Pts',(-32.4670988147272,14.5869290465038,
127.088015098191)) ;
#144667 = CARTESIAN_POINT('Ctrl Pts',(-32.5565456830465,14.5417666874379,
127.382354784027)) ;
#144668 = CARTESIAN_POINT('Ctrl Pts',(-32.6388889719656,14.4163781165351,
127.656070958631)) ;
#144669 = CARTESIAN_POINT('Ctrl Pts',(-32.70708269963,14.2194053123055,127.888457784894)) ;
#144670 = CARTESIAN_POINT('Ctrl Pts',(-32.7553721885115,13.966643682879,128.06254084362)) ;
#144671 = CARTESIAN_POINT('Ctrl Pts',(-32.7800253727878,13.6737230006816,
128.167739670936)) ;
#144672 = CARTESIAN_POINT('Ctrl Pts',(-32.7781801610669,13.3629182756251,
128.195508808425)) ;
#144673 = CARTESIAN_POINT('Ctrl Pts',(-32.7493936429457,13.0570540996615,
128.144513598679)) ;
#144674 = CARTESIAN_POINT('Ctrl Pts',(-32.6950690343676,12.7772473921445,
128.018915404156)) ;
#144675 = CARTESIAN_POINT('Ctrl Pts',(-32.6178215190404,12.5427680100154,
127.826519840422)) ;
#144676 = CARTESIAN_POINT('Ctrl Pts',(-32.5236936545369,12.3730788139632,
127.584510875552)) ;
#144677 = CARTESIAN_POINT('Ctrl Pts',(-32.4173873681917,12.2773830368376,
127.307131936776)) ;
#144678 = CARTESIAN_POINT('Ctrl Pts',(-32.306450665399,12.2641121803462,127.016176193277)) ;
#144679 = CARTESIAN_POINT('Ctrl Pts',(-32.1980092860901,12.3337583656513,
126.732504271029)) ;
#144680 = CARTESIAN_POINT('Ctrl Pts',(-32.0990876968215,12.4813161327732,
126.476631639078)) ;
#144681 = CARTESIAN_POINT('Ctrl Pts',(-32.0158761927489,12.6966780658121,
126.266710351662)) ;
#144682 = CARTESIAN_POINT('Ctrl Pts',(-31.9538770228678,12.9640585789761,
126.118733259147)) ;
#144683 = CARTESIAN_POINT('Ctrl Pts',(-31.9167599552358,13.263362217281,126.043343607058)) ;
#144684 = CARTESIAN_POINT('Ctrl Pts',(-31.9062170544741,13.5752569117425,
126.045709527399)) ;
#144685 = CARTESIAN_POINT('Ctrl Pts',(-31.9226445076029,13.8766503644376,
126.126917612135)) ;
#144686 = CARTESIAN_POINT('Ctrl Pts',(-31.9637029016732,14.1438627014427,
126.279869047209)) ;
#144687 = CARTESIAN_POINT('Ctrl Pts',(-32.0262809227179,14.3611558948339,
126.495912269976)) ;
#144688 = CARTESIAN_POINT('Ctrl Pts',(-32.1047645421015,14.5102071341288,
126.758321777945)) ;
#144689 = CARTESIAN_POINT('Ctrl Pts',(-32.1923828176935,14.5813677967462,
127.047244242667)) ;
#144690 = CARTESIAN_POINT('Ctrl Pts',(-32.2832244888106,14.5701314848988,
127.34580352681)) ;
#144691 = CARTESIAN_POINT('Ctrl Pts',(-32.3695772610759,14.4759918680502,
127.631298809263)) ;
#144692 = CARTESIAN_POINT('Ctrl Pts',(-32.4440427734201,14.3066892261713,
127.881936729274)) ;
#144693 = CARTESIAN_POINT('Ctrl Pts',(-32.5008263829426,14.0751878259722,
128.080807992668)) ;
#144694 = CARTESIAN_POINT('Ctrl Pts',(-32.5355347715382,13.7962286301239,
128.215320954955)) ;
#144695 = CARTESIAN_POINT('Ctrl Pts',(-32.5446721574957,13.489739255107,128.275210131471)) ;
#144696 = CARTESIAN_POINT('Ctrl Pts',(-32.5265849289817,13.1781056591445,
128.255614488998)) ;
#144697 = CARTESIAN_POINT('Ctrl Pts',(-32.4826045749206,12.8871394405402,
128.160016968544)) ;
#144698 = CARTESIAN_POINT('Ctrl Pts',(-32.4142077175318,12.6313542948275,
127.993455148727)) ;
#144699 = CARTESIAN_POINT('Ctrl Pts',(-32.3259460356126,12.4333423799844,
127.768796899427)) ;
#144700 = CARTESIAN_POINT('Ctrl Pts',(-32.2242180820195,12.3067788244502,
127.504580022225)) ;
#144701 = CARTESIAN_POINT('Ctrl Pts',(-32.1138392452441,12.2592790120272,
127.215412831883)) ;
#144702 = CARTESIAN_POINT('Ctrl Pts',(-32.003485063804,12.2958890745914,126.926165499256)) ;
#144703 = CARTESIAN_POINT('Ctrl Pts',(-31.9001877061898,12.412515961838,126.657421781237)) ;
#144704 = CARTESIAN_POINT('Ctrl Pts',(-31.8098515533927,12.6017795181092,
126.426660655506)) ;
#144705 = CARTESIAN_POINT('Ctrl Pts',(-31.7385681295902,12.8508820386888,
126.251652404541)) ;
#144706 = CARTESIAN_POINT('Ctrl Pts',(-31.6911379315082,13.1389626270395,
126.146085694306)) ;
#144707 = CARTESIAN_POINT('Ctrl Pts',(-31.6696008199509,13.4502019217322,
126.116475044646)) ;
#144708 = CARTESIAN_POINT('Ctrl Pts',(-31.675316072249,13.7571545307035,126.166221736191)) ;
#144709 = CARTESIAN_POINT('Ctrl Pts',(-31.706567429285,14.0399279839555,126.290508349871)) ;
#144710 = CARTESIAN_POINT('Ctrl Pts',(-31.7611102860572,14.2804627639154,
126.483099880761)) ;
#144711 = CARTESIAN_POINT('Ctrl Pts',(-31.8334965665926,14.4580430592262,
126.727575168769)) ;
#144712 = CARTESIAN_POINT('Ctrl Pts',(-31.9185397988038,14.5623041916472,
127.009181592164)) ;
#144713 = CARTESIAN_POINT('Ctrl Pts',(-32.0088724260903,14.5848738279965,
127.306134040065)) ;
#144714 = CARTESIAN_POINT('Ctrl Pts',(-32.0981654325802,14.5236285085623,
127.60029694483)) ;
#144715 = CARTESIAN_POINT('Ctrl Pts',(-32.1778221198332,14.3842858340258,
127.865980605226)) ;
#144716 = CARTESIAN_POINT('Ctrl Pts',(-32.2426771957791,14.1760036072079,
128.088561512435)) ;
#144717 = CARTESIAN_POINT('Ctrl Pts',(-32.2870187656786,13.9123644757914,
128.251357212827)) ;
#144718 = CARTESIAN_POINT('Ctrl Pts',(-32.3065797695472,13.6155078278093,
128.341537873815)) ;
#144719 = CARTESIAN_POINT('Ctrl Pts',(-32.299733398088,13.3048785674805,128.354587348161)) ;
#144720 = CARTESIAN_POINT('Ctrl Pts',(-32.2658846348396,13.0013157661824,
128.288909145549)) ;
#144721 = CARTESIAN_POINT('Ctrl Pts',(-32.2069886942351,12.7290184016179,
128.1499432911)) ;
#144722 = CARTESIAN_POINT('Ctrl Pts',(-32.1263303751001,12.5059452399051,
127.947463873129)) ;
#144723 = CARTESIAN_POINT('Ctrl Pts',(-32.0291748251866,12.3489356287849,
127.696738913591)) ;
#144724 = CARTESIAN_POINT('Ctrl Pts',(-31.9217381388589,12.2685725543234,
127.415958176252)) ;
#144725 = CARTESIAN_POINT('Ctrl Pts',(-31.8103465441405,12.2709800429639,
127.123786383864)) ;
#144726 = CARTESIAN_POINT('Ctrl Pts',(-31.7033367406482,12.3558597729099,
126.844245062595)) ;
#144727 = CARTESIAN_POINT('Ctrl Pts',(-31.6068083151779,12.5173149603475,
126.595412194401)) ;
#144728 = CARTESIAN_POINT('Ctrl Pts',(-31.5273365282627,12.7436533990505,
126.396378948702)) ;
#144729 = CARTESIAN_POINT('Ctrl Pts',(-31.4698051340278,13.0184391558732,
126.261419197798)) ;
#144730 = CARTESIAN_POINT('Ctrl Pts',(-31.4375406438131,13.3224259864685,
126.200296275979)) ;
#144731 = CARTESIAN_POINT('Ctrl Pts',(-31.4321948009819,13.6337497242247,
126.217821502333)) ;
#144732 = CARTESIAN_POINT('Ctrl Pts',(-31.4534309715984,13.9298382282655,
126.312987130498)) ;
#144733 = CARTESIAN_POINT('Ctrl Pts',(-31.4989100448319,14.189430649662,126.47894051365)) ;
#144734 = CARTESIAN_POINT('Ctrl Pts',(-31.564823476328,14.394475769408,126.704646843122)) ;
#144735 = CARTESIAN_POINT('Ctrl Pts',(-31.6453547625781,14.5294751555696,
126.972946428523)) ;
#144736 = CARTESIAN_POINT('Ctrl Pts',(-31.7344309707167,14.5857784692471,
127.266285694623)) ;
#144737 = CARTESIAN_POINT('Ctrl Pts',(-31.8250135034699,14.5584757915825,
127.564109179261)) ;
#144738 = CARTESIAN_POINT('Ctrl Pts',(-31.9093410315124,14.4499269428434,
127.843545790168)) ;
#144739 = CARTESIAN_POINT('Ctrl Pts',(-31.9810494756834,14.2678362353556,
128.086150346001)) ;
#144740 = CARTESIAN_POINT('Ctrl Pts',(-32.034169894188,14.025181457992,128.274454335045)) ;
#144741 = CARTESIAN_POINT('Ctrl Pts',(-32.0641766159735,13.7395989373351,
128.395216353623)) ;
#144742 = CARTESIAN_POINT('Ctrl Pts',(-32.0682143772273,13.4312396323536,
128.440131093672)) ;
#144743 = CARTESIAN_POINT('Ctrl Pts',(-32.0453158611644,13.1225497358479,
128.406327376222)) ;
#144744 = CARTESIAN_POINT('Ctrl Pts',(-31.996169151728,12.8344723691042,128.295954955988)) ;
#144745 = CARTESIAN_POINT('Ctrl Pts',(-31.9238482595544,12.5894057797878,
128.117787838384)) ;
#144746 = CARTESIAN_POINT('Ctrl Pts',(-31.832662535924,12.403866954954,127.884535160831)) ;
#144747 = CARTESIAN_POINT('Ctrl Pts',(-31.7285002227895,12.2913271395126,
127.613354573894)) ;
#144748 = CARTESIAN_POINT('Ctrl Pts',(-31.6177523868802,12.2598830910024,
127.32302334867)) ;
#144749 = CARTESIAN_POINT('Ctrl Pts',(-31.5083419637065,12.3117248800856,
127.036464679432)) ;
#144750 = CARTESIAN_POINT('Ctrl Pts',(-31.4066545343474,12.4432581969561,
126.772557747754)) ;
#144751 = CARTESIAN_POINT('Ctrl Pts',(-31.3196996717147,12.6447768479475,
126.551633848093)) ;
#144752 = CARTESIAN_POINT('Ctrl Pts',(-31.2527294004413,12.9020427023331,
126.389108312362)) ;
#144753 = CARTESIAN_POINT('Ctrl Pts',(-31.2098964874748,13.1969220955149,
126.297125418566)) ;
#144754 = CARTESIAN_POINT('Ctrl Pts',(-31.1935254547332,13.5073634201221,
126.282371473235)) ;
#144755 = CARTESIAN_POINT('Ctrl Pts',(-31.2042125321738,13.8135028677167,
126.346863684754)) ;
#144756 = CARTESIAN_POINT('Ctrl Pts',(-31.2400738263031,14.0890635163078,
126.484577408742)) ;
#144757 = CARTESIAN_POINT('Ctrl Pts',(-31.2984854067219,14.3192685446141,
126.688485355535)) ;
#144758 = CARTESIAN_POINT('Ctrl Pts',(-31.3736030379443,14.4835637983032,
126.940906398959)) ;
#144759 = CARTESIAN_POINT('Ctrl Pts',(-31.4603373040575,14.5730188285823,
127.227495175343)) ;
#144760 = CARTESIAN_POINT('Ctrl Pts',(-31.5510617389729,14.5795967764284,
127.52564779883)) ;
#144761 = CARTESIAN_POINT('Ctrl Pts',(-31.6387634374852,14.5032853646564,
127.814990801029)) ;
#144762 = CARTESIAN_POINT('Ctrl Pts',(-31.7162734788817,14.3501151249434,
128.074477893202)) ;
#144763 = CARTESIAN_POINT('Ctrl Pts',(-31.7777929390999,14.1289951799062,
128.287474132469)) ;
#144764 = CARTESIAN_POINT('Ctrl Pts',(-31.8173663026795,13.8600883343583,
128.435990379675)) ;
#144765 = CARTESIAN_POINT('Ctrl Pts',(-31.8322919438319,13.5571075891159,
128.512852727312)) ;
#144766 = CARTESIAN_POINT('Ctrl Pts',(-31.82022330572,13.246144038551,128.51066807506)) ;
#144767 = CARTESIAN_POINT('Ctrl Pts',(-31.7816172657033,12.9474784018938,
128.430993884236)) ;
#144768 = CARTESIAN_POINT('Ctrl Pts',(-31.7179322198423,12.6818049804595,
128.278220905245)) ;
#144769 = CARTESIAN_POINT('Ctrl Pts',(-31.6341871853082,12.4713261551404,
128.06652480907)) ;
#144770 = CARTESIAN_POINT('Ctrl Pts',(-31.5341646889309,12.3273775060339,
127.807571862483)) ;
#144771 = CARTESIAN_POINT('Ctrl Pts',(-31.4256220530774,12.2625380401702,
127.523523338818)) ;
#144772 = CARTESIAN_POINT('Ctrl Pts',(-31.3141710264018,12.2810707697993,
127.231254074188)) ;
#144773 = CARTESIAN_POINT('Ctrl Pts',(-31.2093207416978,12.3803129449242,
126.957812292313)) ;
#144774 = CARTESIAN_POINT('Ctrl Pts',(-31.1151683157107,12.5556239471542,
126.716053817191)) ;
#144775 = CARTESIAN_POINT('Ctrl Pts',(-31.0397604821061,12.7914917481058,
126.528754888834)) ;
#144776 = CARTESIAN_POINT('Ctrl Pts',(-30.9864549257893,13.0750410185669,
126.406347636205)) ;
#144777 = CARTESIAN_POINT('Ctrl Pts',(-30.9593938888774,13.3808908825506,
126.360285902276)) ;
#144778 = CARTESIAN_POINT('Ctrl Pts',(-30.9590643989393,13.6908805105498,
126.392448187648)) ;
#144779 = CARTESIAN_POINT('Ctrl Pts',(-30.985079519922,13.9819858860809,126.501595001656)) ;
#144780 = CARTESIAN_POINT('Ctrl Pts',(-31.0349155333376,14.2331023170552,
126.680366168729)) ;
#144781 = CARTESIAN_POINT('Ctrl Pts',(-31.103787873337,14.425373738482,126.914579912793)) ;
#144782 = CARTESIAN_POINT('Ctrl Pts',(-31.1870948720038,14.5469025467051,
127.191256375485)) ;
#144783 = CARTESIAN_POINT('Ctrl Pts',(-31.2765949077209,14.5868798002751,
127.48568376315)) ;
#144784 = CARTESIAN_POINT('Ctrl Pts',(-31.3662691064729,14.544243012127,127.780733186927)) ;
#144785 = CARTESIAN_POINT('Ctrl Pts',(-31.4488236582154,14.4211466682183,
128.055026539422)) ;
#144786 = CARTESIAN_POINT('Ctrl Pts',(-31.5175184584452,14.2262607668007,
128.28886635848)) ;
#144787 = CARTESIAN_POINT('Ctrl Pts',(-31.566546342217,13.9744157440355,128.465170341222)) ;
#144788 = CARTESIAN_POINT('Ctrl Pts',(-31.5918626188502,13.6824769956245,
128.572286130259)) ;
#144789 = CARTESIAN_POINT('Ctrl Pts',(-31.5908930328258,13.3726811075526,
128.602527371079)) ;
#144790 = CARTESIAN_POINT('Ctrl Pts',(-31.5626626632348,13.0644552653701,
128.553368423674)) ;
#144791 = CARTESIAN_POINT('Ctrl Pts',(-31.5092143642815,12.7851437456734,
128.430163081405)) ;
#144792 = CARTESIAN_POINT('Ctrl Pts',(-31.4328238022929,12.5493640024945,
128.240198742894)) ;
#144793 = CARTESIAN_POINT('Ctrl Pts',(-31.3389013828092,12.376970726474,127.998880739351)) ;
#144794 = CARTESIAN_POINT('Ctrl Pts',(-31.2325442048154,12.2789142943649,
127.721438969545)) ;
#144795 = CARTESIAN_POINT('Ctrl Pts',(-31.1219668459032,12.2633331335236,
127.431435996235)) ;
#144796 = CARTESIAN_POINT('Ctrl Pts',(-31.0131048658682,12.3306602868788,
127.146608211436)) ;
#144797 = CARTESIAN_POINT('Ctrl Pts',(-30.9137175361845,12.4766203405944,
126.889425390704)) ;
#144798 = CARTESIAN_POINT('Ctrl Pts',(-30.8304038367424,12.6891737116268,
126.679037871423)) ;
#144799 = CARTESIAN_POINT('Ctrl Pts',(-30.7676114855164,12.9552556025245,
126.528760774747)) ;
#144800 = CARTESIAN_POINT('Ctrl Pts',(-30.7296421112751,13.2547271279824,
126.450969119973)) ;
#144801 = CARTESIAN_POINT('Ctrl Pts',(-30.7183893110639,13.5662747472623,
126.451228783518)) ;
#144802 = CARTESIAN_POINT('Ctrl Pts',(-30.733913444231,13.8673047437589,126.529679410817)) ;
#144803 = CARTESIAN_POINT('Ctrl Pts',(-30.7744187831049,14.1368397654386,
126.681145138688)) ;
#144804 = CARTESIAN_POINT('Ctrl Pts',(-30.8362150266428,14.3550474854522,
126.894778750719)) ;
#144805 = CARTESIAN_POINT('Ctrl Pts',(-30.9142509625502,14.5066809969925,
127.155885362528)) ;
#144806 = CARTESIAN_POINT('Ctrl Pts',(-31.0021246618732,14.5805550021418,
127.445716539722)) ;
#144807 = CARTESIAN_POINT('Ctrl Pts',(-31.0927386419464,14.5715434154247,
127.743520389293)) ;
#144808 = CARTESIAN_POINT('Ctrl Pts',(-31.1790271767305,14.4804614253832,
128.028700915286)) ;
#144809 = CARTESIAN_POINT('Ctrl Pts',(-31.2542421356505,14.3129344322758,
128.281642462591)) ;
#144810 = CARTESIAN_POINT('Ctrl Pts',(-31.3117291376772,14.0824719348205,
128.482642895694)) ;
#144811 = CARTESIAN_POINT('Ctrl Pts',(-31.3470892051773,13.8045959520742,
128.619053432175)) ;
#144812 = CARTESIAN_POINT('Ctrl Pts',(-31.3569871658133,13.4994871825109,
128.681068602957)) ;
#144813 = CARTESIAN_POINT('Ctrl Pts',(-31.3397975278184,13.1877258357311,
128.664087688354)) ;
#144814 = CARTESIAN_POINT('Ctrl Pts',(-31.2964040254458,12.8947281462995,
128.570335332532)) ;
#144815 = CARTESIAN_POINT('Ctrl Pts',(-31.2284884597744,12.6375710279023,
128.405210278833)) ;
#144816 = CARTESIAN_POINT('Ctrl Pts',(-31.1412553171242,12.4386468610117,
128.183369892293)) ;
#144817 = CARTESIAN_POINT('Ctrl Pts',(-31.0392856803408,12.3091460957756,
127.918635408139)) ;
#144818 = CARTESIAN_POINT('Ctrl Pts',(-30.9296587376181,12.2596124823544,
127.631470528942)) ;
#144819 = CARTESIAN_POINT('Ctrl Pts',(-30.8189572509962,12.2934287608505,
127.341283904815)) ;
#144820 = CARTESIAN_POINT('Ctrl Pts',(-30.7149224451956,12.4085128327331,
127.070530721846)) ;
#144821 = CARTESIAN_POINT('Ctrl Pts',(-30.6244270191123,12.5956557289105,
126.839221510393)) ;
#144822 = CARTESIAN_POINT('Ctrl Pts',(-30.552740348961,12.8419007225992,126.662879913109)) ;
#144823 = CARTESIAN_POINT('Ctrl Pts',(-30.5042887818973,13.1310174961036,
126.554554614901)) ;
#144824 = CARTESIAN_POINT('Ctrl Pts',(-30.4821225458649,13.4394174357417,
126.522827842075)) ;
#144825 = CARTESIAN_POINT('Ctrl Pts',(-30.4869544585416,13.7489280911395,
126.570225234814)) ;
#144826 = CARTESIAN_POINT('Ctrl Pts',(-30.5176484397562,14.0326636377924,
126.692900306353)) ;
#144827 = CARTESIAN_POINT('Ctrl Pts',(-30.5713213184817,14.2739040852335,
126.882817074721)) ;
#144828 = CARTESIAN_POINT('Ctrl Pts',(-30.6436244084103,14.4542739196418,
127.127215545827)) ;
#144829 = CARTESIAN_POINT('Ctrl Pts',(-30.7280326162985,14.5602989728585,
127.406812499474)) ;
#144830 = CARTESIAN_POINT('Ctrl Pts',(-30.8186285442324,14.5853165149043,
127.704660608665)) ;
#144831 = CARTESIAN_POINT('Ctrl Pts',(-30.9075041976881,14.5269566975762,
127.997384873959)) ;
#144832 = CARTESIAN_POINT('Ctrl Pts',(-30.9881047297177,14.3891797557674,
128.266049347008)) ;
#144833 = CARTESIAN_POINT('Ctrl Pts',(-31.0534636981104,14.1817902541555,
128.490167087522)) ;
#144834 = CARTESIAN_POINT('Ctrl Pts',(-31.0981004770551,13.9219441435514,
128.653522008646)) ;
#144835 = CARTESIAN_POINT('Ctrl Pts',(-31.1186289612997,13.6244332360091,
128.746699920256)) ;
#144836 = CARTESIAN_POINT('Ctrl Pts',(-31.1125361857991,13.3138307533241,
128.761949736596)) ;
#144837 = CARTESIAN_POINT('Ctrl Pts',(-31.0793149773615,13.0089906490168,
128.698191722049)) ;
#144838 = CARTESIAN_POINT('Ctrl Pts',(-31.0213127924495,12.7367004546504,
128.56169934609)) ;
#144839 = CARTESIAN_POINT('Ctrl Pts',(-30.9412589328357,12.5117902226442,
128.360991687097)) ;
#144840 = CARTESIAN_POINT('Ctrl Pts',(-30.8444991744712,12.3525055718321,
128.111429712698)) ;
#144841 = CARTESIAN_POINT('Ctrl Pts',(-30.736804998274,12.2695603422194,127.830036678703)) ;
#144842 = CARTESIAN_POINT('Ctrl Pts',(-30.6255790074019,12.2698997587057,
127.538298190404)) ;
#144843 = CARTESIAN_POINT('Ctrl Pts',(-30.5186478948904,12.3521640390818,
127.258896733062)) ;
#144844 = CARTESIAN_POINT('Ctrl Pts',(-30.4216161503203,12.5116415634716,
127.008626067595)) ;
#144845 = CARTESIAN_POINT('Ctrl Pts',(-30.3416456644303,12.7360069700772,
126.808096783249)) ;
#144846 = CARTESIAN_POINT('Ctrl Pts',(-30.2833400695677,13.0100796293743,
126.670930462911)) ;
#144847 = CARTESIAN_POINT('Ctrl Pts',(-30.250351362489,13.3126253374921,126.607593228363)) ;
#144848 = CARTESIAN_POINT('Ctrl Pts',(-30.2441927566021,13.6254715524663,
126.622899503079)) ;
#144849 = CARTESIAN_POINT('Ctrl Pts',(-30.2646331156608,13.9212365418522,
126.715618043122)) ;
#144850 = CARTESIAN_POINT('Ctrl Pts',(-30.3095314842463,14.1826934673073,
126.879946570036)) ;
#144851 = CARTESIAN_POINT('Ctrl Pts',(-30.3746703453055,14.3889686584202,
127.103272672401)) ;
#144852 = CARTESIAN_POINT('Ctrl Pts',(-30.4553607437768,14.5271450156122,
127.372251222131)) ;
#144853 = CARTESIAN_POINT('Ctrl Pts',(-30.5443910347089,14.5852339348323,
127.665478148695)) ;
#144854 = CARTESIAN_POINT('Ctrl Pts',(-30.6344393567166,14.5605427661762,
127.96152213049)) ;
#144855 = CARTESIAN_POINT('Ctrl Pts',(-30.7192995987514,14.4541441537073,
128.242612469861)) ;
#144856 = CARTESIAN_POINT('Ctrl Pts',(-30.791408695709,14.2740963281162,128.486362771515)) ;
#144857 = CARTESIAN_POINT('Ctrl Pts',(-30.8452749040731,14.0323112919108,
128.676933371986)) ;
#144858 = CARTESIAN_POINT('Ctrl Pts',(-30.8758787528105,13.747634010638,128.799431922669)) ;
#144859 = CARTESIAN_POINT('Ctrl Pts',(-30.8807206526435,13.4408490944308,
128.846563950046)) ;
#144860 = CARTESIAN_POINT('Ctrl Pts',(-30.8584669743735,13.1304291630284,
128.814803354541)) ;
#144861 = CARTESIAN_POINT('Ctrl Pts',(-30.8102230492694,12.8426172833002,
128.706927901223)) ;
#144862 = CARTESIAN_POINT('Ctrl Pts',(-30.738204665558,12.5951022439345,128.529786637205)) ;
#144863 = CARTESIAN_POINT('Ctrl Pts',(-30.6479308981306,12.4086451367459,
128.299025630122)) ;
#144864 = CARTESIAN_POINT('Ctrl Pts',(-30.5437885246526,12.2933533526165,
128.027999482058)) ;
#144865 = CARTESIAN_POINT('Ctrl Pts',(-30.4331507484022,12.2596356642452,
127.737975845541)) ;
#144866 = CARTESIAN_POINT('Ctrl Pts',(-30.3236687251324,12.3091205579985,
127.451195810082)) ;
#144867 = CARTESIAN_POINT('Ctrl Pts',(-30.2218360682073,12.4379929419073,
127.186793272986)) ;
#144868 = CARTESIAN_POINT('Ctrl Pts',(-30.133946584772,12.6386445208212,126.963302213587)) ;
#144869 = CARTESIAN_POINT('Ctrl Pts',(-30.0665450383509,12.8942395319149,
126.799453338661)) ;
#144870 = CARTESIAN_POINT('Ctrl Pts',(-30.0230172306372,13.1876524015431,
126.705370560951)) ;
#144871 = CARTESIAN_POINT('Ctrl Pts',(-30.0058439958763,13.4984175352415,
126.688327152923)) ;
#144872 = CARTESIAN_POINT('Ctrl Pts',(-30.0156793479209,13.804322978022,126.750244532428)) ;
#144873 = CARTESIAN_POINT('Ctrl Pts',(-30.0510539190333,14.0825044690989,
126.886722797835)) ;
#144874 = CARTESIAN_POINT('Ctrl Pts',(-30.1087723520417,14.3134151939565,
127.08849843816)) ;
#144875 = CARTESIAN_POINT('Ctrl Pts',(-30.1834773985359,14.4799820430956,
127.339730220267)) ;
#144876 = CARTESIAN_POINT('Ctrl Pts',(-30.2703212530767,14.5717629111611,
127.626756088476)) ;
#144877 = CARTESIAN_POINT('Ctrl Pts',(-30.3605730980817,14.5804902345133,
127.923362492144)) ;
#144878 = CARTESIAN_POINT('Ctrl Pts',(-30.4484207426051,14.5068426017295,
128.213109501132)) ;
#144879 = CARTESIAN_POINT('Ctrl Pts',(-30.5264050460669,14.3556215142155,
128.474020614704)) ;
#144880 = CARTESIAN_POINT('Ctrl Pts',(-30.5884484413862,14.1365915328991,
128.68850660419)) ;
#144881 = CARTESIAN_POINT('Ctrl Pts',(-30.6287779145481,13.8680779330351,
128.839329518904)) ;
#144882 = CARTESIAN_POINT('Ctrl Pts',(-30.6444633950159,13.567186800724,128.918249167054)) ;
#144883 = CARTESIAN_POINT('Ctrl Pts',(-30.6330856943008,13.2537545062593,
128.918345572643)) ;
#144884 = CARTESIAN_POINT('Ctrl Pts',(-30.5953085614819,12.9561224404112,
128.840913500029)) ;
#144885 = CARTESIAN_POINT('Ctrl Pts',(-30.5325580838653,12.6895769772328,
128.690796474662)) ;
#144886 = CARTESIAN_POINT('Ctrl Pts',(-30.4490933643888,12.4765148457442,
128.480030334778)) ;
#144887 = CARTESIAN_POINT('Ctrl Pts',(-30.3494005172327,12.3303992852147,
128.22204710236)) ;
#144888 = CARTESIAN_POINT('Ctrl Pts',(-30.2409395974139,12.2633426599666,
127.938263534079)) ;
#144889 = CARTESIAN_POINT('Ctrl Pts',(-30.1300275403306,12.279103982185,127.647390711244)) ;
#144890 = CARTESIAN_POINT('Ctrl Pts',(-30.0242396310796,12.3764767576561,
127.371421006722)) ;
#144891 = CARTESIAN_POINT('Ctrl Pts',(-29.9297270127892,12.5500289101503,
127.128600360507)) ;
#144892 = CARTESIAN_POINT('Ctrl Pts',(-29.8538880485749,12.7839578561676,
126.939986660771)) ;
#144893 = CARTESIAN_POINT('Ctrl Pts',(-29.799920152433,13.0658041228342,126.815575584381)) ;
#144894 = CARTESIAN_POINT('Ctrl Pts',(-29.7719515457904,13.3726170647806,
126.767011455076)) ;
#144895 = CARTESIAN_POINT('Ctrl Pts',(-29.7709724043549,13.6826397531364,
126.797259660595)) ;
#144896 = CARTESIAN_POINT('Ctrl Pts',(-29.7961074976013,13.9734160289762,
126.903696461442)) ;
#144897 = CARTESIAN_POINT('Ctrl Pts',(-29.8454532437699,14.2269288377743,
127.081152783863)) ;
#144898 = CARTESIAN_POINT('Ctrl Pts',(-29.9137639793214,14.4205112274409,
127.313664906998)) ;
#144899 = CARTESIAN_POINT('Ctrl Pts',(-29.9963081148544,14.5441065971854,
127.58795480985)) ;
#144900 = CARTESIAN_POINT('Ctrl Pts',(-30.0863453943646,14.5870792664814,
127.884190319798)) ;
#144901 = CARTESIAN_POINT('Ctrl Pts',(-30.1762178473104,14.5462510463569,
128.179861707913)) ;
#144902 = CARTESIAN_POINT('Ctrl Pts',(-30.2586647603345,14.426108976537,128.453668191511)) ;
#144903 = CARTESIAN_POINT('Ctrl Pts',(-30.3282364972307,14.2320089292168,
128.690260384184)) ;
#144904 = CARTESIAN_POINT('Ctrl Pts',(-30.3776572255911,13.9821034896837,
128.867612332903)) ;
#144905 = CARTESIAN_POINT('Ctrl Pts',(-30.4036939249744,13.6914860951574,
128.976787558372)) ;
#144906 = CARTESIAN_POINT('Ctrl Pts',(-30.4035328494657,13.3820426901867,
129.00937714575)) ;
#144907 = CARTESIAN_POINT('Ctrl Pts',(-30.3760843784156,13.0731824495073,
128.962523652732)) ;
#144908 = CARTESIAN_POINT('Ctrl Pts',(-30.3233314713119,12.7927891220342,
128.841355852443)) ;
#144909 = CARTESIAN_POINT('Ctrl Pts',(-30.2475283569067,12.5553086793863,
128.653116181517)) ;
#144910 = CARTESIAN_POINT('Ctrl Pts',(-30.1538708216962,12.3807971317929,
128.412623508798)) ;
#144911 = CARTESIAN_POINT('Ctrl Pts',(-30.0481576035752,12.2807361314401,
128.136939366239)) ;
#144912 = CARTESIAN_POINT('Ctrl Pts',(-29.9372735731522,12.2625961547027,
127.846148016714)) ;
#144913 = CARTESIAN_POINT('Ctrl Pts',(-29.8284201756463,12.3275534841213,
127.561290415052)) ;
#144914 = CARTESIAN_POINT('Ctrl Pts',(-29.7286735000512,12.4713200428819,
127.303059540576)) ;
#144915 = CARTESIAN_POINT('Ctrl Pts',(-29.6447991067587,12.6818354528321,
127.091014736761)) ;
#144916 = CARTESIAN_POINT('Ctrl Pts',(-29.5809833693557,12.9488696704077,
126.938002457017)) ;
#144917 = CARTESIAN_POINT('Ctrl Pts',(-29.5426918772744,13.2449965342222,
126.858961210863)) ;
#144918 = CARTESIAN_POINT('Ctrl Pts',(-29.5305163141329,13.5577147943103,
126.856660900313)) ;
#144919 = CARTESIAN_POINT('Ctrl Pts',(-29.5453412160275,13.85913805832,126.933045258162)) ;
#144920 = CARTESIAN_POINT('Ctrl Pts',(-29.5852299850096,14.1301670031634,
127.082751092509)) ;
#144921 = CARTESIAN_POINT('Ctrl Pts',(-29.6464922978866,14.3498259886228,
127.294806891139)) ;
#144922 = CARTESIAN_POINT('Ctrl Pts',(-29.7240191450472,14.5033075932482,
127.554372812427)) ;
#144923 = CARTESIAN_POINT('Ctrl Pts',(-29.811746984037,14.5795881010438,127.84379574646)) ;
#144924 = CARTESIAN_POINT('Ctrl Pts',(-29.902415821184,14.5729975043218,128.141770824574)) ;
#144925 = CARTESIAN_POINT('Ctrl Pts',(-29.989169947926,14.4837968036715,128.428408489667)) ;
#144926 = CARTESIAN_POINT('Ctrl Pts',(-30.0646586440251,14.3181445279312,
128.682117681586)) ;
#144927 = CARTESIAN_POINT('Ctrl Pts',(-30.1225460634505,14.0900336140832,
128.884184874073)) ;
#144928 = CARTESIAN_POINT('Ctrl Pts',(-30.1586763891653,13.812578673719,129.02292535409)) ;
#144929 = CARTESIAN_POINT('Ctrl Pts',(-30.1692630060862,13.5087142835403,
129.086866972052)) ;
#144930 = CARTESIAN_POINT('Ctrl Pts',(-30.1529569913643,13.1970641651478,
129.072436780848)) ;
#144931 = CARTESIAN_POINT('Ctrl Pts',(-30.1101366557487,12.9023258221912,
128.98046898665)) ;
#144932 = CARTESIAN_POINT('Ctrl Pts',(-30.0430710583863,12.644685125118,128.817716891912)) ;
#144933 = CARTESIAN_POINT('Ctrl Pts',(-29.9563503393959,12.4436426605292,
128.597389723599)) ;
#144934 = CARTESIAN_POINT('Ctrl Pts',(-29.8545813873611,12.3118006025232,
128.333283034123)) ;
#144935 = CARTESIAN_POINT('Ctrl Pts',(-29.745052917924,12.2597626712743,128.046411581091)) ;
#144936 = CARTESIAN_POINT('Ctrl Pts',(-29.6338703610585,12.291703918078,127.754949605098)) ;
#144937 = CARTESIAN_POINT('Ctrl Pts',(-29.5303599253894,12.4035190278675,
127.485458923152)) ;
#144938 = CARTESIAN_POINT('Ctrl Pts',(-29.4386293109041,12.5902948833878,
127.250828431852)) ;
#144939 = CARTESIAN_POINT('Ctrl Pts',(-29.3668161784755,12.8337324563932,
127.07391082911)) ;
#144940 = CARTESIAN_POINT('Ctrl Pts',(-29.317354785249,13.1235886445067,126.962832987765)) ;
#144941 = CARTESIAN_POINT('Ctrl Pts',(-29.2946790039063,13.4302519414742,
126.929456186755)) ;
#144942 = CARTESIAN_POINT('Ctrl Pts',(-29.2985403929367,13.7390104772614,
126.97389188522)) ;
#144943 = CARTESIAN_POINT('Ctrl Pts',(-29.328778151289,14.0260062302898,127.095502531862)) ;
#144944 = CARTESIAN_POINT('Ctrl Pts',(-29.3816257655434,14.267226902407,127.282822185877)) ;
#144945 = CARTESIAN_POINT('Ctrl Pts',(-29.453365562884,14.4498458952908,127.525566557357)) ;
#144946 = CARTESIAN_POINT('Ctrl Pts',(-29.5379200931215,14.5586319352592,
127.805747356859)) ;
#144947 = CARTESIAN_POINT('Ctrl Pts',(-29.6284800570067,14.5856242088894,
128.103498661156)) ;
#144948 = CARTESIAN_POINT('Ctrl Pts',(-29.7171136257346,14.5299078181027,
128.395370777147)) ;
#144949 = CARTESIAN_POINT('Ctrl Pts',(-29.7982635715947,14.3940107606991,
128.665725835528)) ;
#144950 = CARTESIAN_POINT('Ctrl Pts',(-29.8639971373026,14.1888420463645,
128.890864255151)) ;
#144951 = CARTESIAN_POINT('Ctrl Pts',(-29.9093494029208,13.9299824320437,
129.056357542449)) ;
#144952 = CARTESIAN_POINT('Ctrl Pts',(-29.9306079583778,13.6339608398866,
129.151584407244)) ;
#144953 = CARTESIAN_POINT('Ctrl Pts',(-29.9252897878826,13.3227158538243,
129.16918084059)) ;
#144954 = CARTESIAN_POINT('Ctrl Pts',(-29.8930268090175,13.018724359071,129.10806602458)) ;
#144955 = CARTESIAN_POINT('Ctrl Pts',(-29.8356700823935,12.7442183705068,
128.973561223721)) ;
#144956 = CARTESIAN_POINT('Ctrl Pts',(-29.7557212807804,12.5167188464288,
128.773322705119)) ;
#144957 = CARTESIAN_POINT('Ctrl Pts',(-29.6597849157997,12.3563385813199,
128.526008620895)) ;
#144958 = CARTESIAN_POINT('Ctrl Pts',(-29.5525354882502,12.2709228201269,
128.245853541108)) ;
#144959 = CARTESIAN_POINT('Ctrl Pts',(-29.4411852696987,12.2686101214329,
127.953789784267)) ;
#144960 = CARTESIAN_POINT('Ctrl Pts',(-29.3337984112996,12.3485946759632,
127.673127456804)) ;
#144961 = CARTESIAN_POINT('Ctrl Pts',(-29.2360837324195,12.5068357117029,
127.420979418989)) ;
#144962 = CARTESIAN_POINT('Ctrl Pts',(-29.1560520154867,12.7283302241023,
127.220079398763)) ;
#144963 = CARTESIAN_POINT('Ctrl Pts',(-29.0969069082964,13.0013551128606,
127.080494500603)) ;
#144964 = CARTESIAN_POINT('Ctrl Pts',(-29.0631494426447,13.3039532563625,
127.014974879755)) ;
#144965 = CARTESIAN_POINT('Ctrl Pts',(-29.056172402243,13.6158509275634,127.027775962805)) ;
#144966 = CARTESIAN_POINT('Ctrl Pts',(-29.0759852253016,13.9138456123568,
127.118835079156)) ;
#144967 = CARTESIAN_POINT('Ctrl Pts',(-29.1200427275785,14.1752853033959,
127.280543177125)) ;
#144968 = CARTESIAN_POINT('Ctrl Pts',(-29.184753849063,14.3839669210711,127.502694707301)) ;
#144969 = CARTESIAN_POINT('Ctrl Pts',(-29.2650162806971,14.5240578631267,
127.770384402593)) ;
#144970 = CARTESIAN_POINT('Ctrl Pts',(-29.3538119622672,14.584818935146,128.062899104014)) ;
#144971 = CARTESIAN_POINT('Ctrl Pts',(-29.4445134401354,14.5621167265827,
128.3610733218)) ;
#144972 = CARTESIAN_POINT('Ctrl Pts',(-29.5290814497335,14.4583966229727,
128.641100901953)) ;
#144973 = CARTESIAN_POINT('Ctrl Pts',(-29.6017322946948,14.2803903749363,
128.886461046025)) ;
#144974 = CARTESIAN_POINT('Ctrl Pts',(-29.6560964939787,14.0406559377366,
129.078419058495)) ;
#144975 = CARTESIAN_POINT('Ctrl Pts',(-29.687572797519,13.7571590105316,129.203463231829)) ;
#144976 = CARTESIAN_POINT('Ctrl Pts',(-29.6931036600313,13.4483332581187,
129.252866998852)) ;
#144977 = CARTESIAN_POINT('Ctrl Pts',(-29.6718600493204,13.140610392606,129.223729521239)) ;
#144978 = CARTESIAN_POINT('Ctrl Pts',(-29.6239436216886,12.8492377200964,
129.117118746748)) ;
#144979 = CARTESIAN_POINT('Ctrl Pts',(-29.5529432008373,12.6021186062381,
128.942722101255)) ;
#144980 = CARTESIAN_POINT('Ctrl Pts',(-29.4630752370502,12.4130744443633,
128.713206500985)) ;
#144981 = CARTESIAN_POINT('Ctrl Pts',(-29.3588143740803,12.2953575363629,
128.441951701695)) ;
#144982 = CARTESIAN_POINT('Ctrl Pts',(-29.2487309441084,12.259540004683,128.153408313109)) ;
#144983 = CARTESIAN_POINT('Ctrl Pts',(-29.1390301351818,12.3063152851138,
127.866010362267)) ;
#144984 = CARTESIAN_POINT('Ctrl Pts',(-29.0363094353862,12.4341408318063,
127.599216552733)) ;
#144985 = CARTESIAN_POINT('Ctrl Pts',(-28.9486256458988,12.6316134862806,
127.376075640592)) ;
#144986 = CARTESIAN_POINT('Ctrl Pts',(-28.8803727387758,12.8861350461837,
127.209806995649)) ;
#144987 = CARTESIAN_POINT('Ctrl Pts',(-28.8360698049953,13.179213941093,127.113505163863)) ;
#144988 = CARTESIAN_POINT('Ctrl Pts',(-28.818146099152,13.4905687882747,127.094349921822)) ;
#144989 = CARTESIAN_POINT('Ctrl Pts',(-28.8273246021898,13.7964604527636,
127.154303567097)) ;
#144990 = CARTESIAN_POINT('Ctrl Pts',(-28.8618427799844,14.0743848720617,
127.288127973483)) ;
#144991 = CARTESIAN_POINT('Ctrl Pts',(-28.9187990753972,14.3070163090694,
127.487639078043)) ;
#144992 = CARTESIAN_POINT('Ctrl Pts',(-28.9935556217395,14.4764518819419,
127.739221259018)) ;
#144993 = CARTESIAN_POINT('Ctrl Pts',(-29.0794072904876,14.5698501931718,
128.023056840081)) ;
#144994 = CARTESIAN_POINT('Ctrl Pts',(-29.1700992616621,14.5816111155488,
128.321126188998)) ;
#144995 = CARTESIAN_POINT('Ctrl Pts',(-29.2583924640271,14.5098991366122,
128.612271870243)) ;
#144996 = CARTESIAN_POINT('Ctrl Pts',(-29.3367774377786,14.3604029768198,
128.874384366338)) ;
#144997 = CARTESIAN_POINT('Ctrl Pts',(-29.3991532586463,14.1435656071336,
129.089752826229)) ;
#144998 = CARTESIAN_POINT('Ctrl Pts',(-29.4402243229761,13.8762645151226,
129.24274936311)) ;
#144999 = CARTESIAN_POINT('Ctrl Pts',(-29.4565543469436,13.5746433207973,
129.323692326844)) ;
#145000 = CARTESIAN_POINT('Ctrl Pts',(-29.446153488638,13.2647985797715,129.326253123723)) ;
#145001 = CARTESIAN_POINT('Ctrl Pts',(-29.4089346093494,12.9638355607027,
129.250742958793)) ;
#145002 = CARTESIAN_POINT('Ctrl Pts',(-29.3469241765837,12.6967406329269,
129.102706452313)) ;
#145003 = CARTESIAN_POINT('Ctrl Pts',(-29.2638217308112,12.4815166817384,
128.89307257032)) ;
#145004 = CARTESIAN_POINT('Ctrl Pts',(-29.1648556934516,12.3337893264045,
128.637089209316)) ;
#145005 = CARTESIAN_POINT('Ctrl Pts',(-29.0563112696507,12.2640797848313,
128.353145898042)) ;
#145006 = CARTESIAN_POINT('Ctrl Pts',(-28.9454975257324,12.2774691635847,
128.06251738632)) ;
#145007 = CARTESIAN_POINT('Ctrl Pts',(-28.8394630097651,12.3724670755757,
127.785829298635)) ;
#145008 = CARTESIAN_POINT('Ctrl Pts',(-28.74455141607,12.5437674769879,127.541819485266)) ;
#145009 = CARTESIAN_POINT('Ctrl Pts',(-28.667987089546,12.7765747381498,127.351152652953)) ;
#145010 = CARTESIAN_POINT('Ctrl Pts',(-28.6134535091621,13.056442748956,127.224981779766)) ;
#145011 = CARTESIAN_POINT('Ctrl Pts',(-28.5846281837057,13.3632374806636,
127.173969984753)) ;
#145012 = CARTESIAN_POINT('Ctrl Pts',(-28.5827519865197,13.6730055446753,
127.201534705381)) ;
#145013 = CARTESIAN_POINT('Ctrl Pts',(-28.6074869894877,13.9671153512335,
127.30710875043)) ;
#145014 = CARTESIAN_POINT('Ctrl Pts',(-28.6556926253068,14.2192391234479,
127.480866191476)) ;
#145015 = CARTESIAN_POINT('Ctrl Pts',(-28.7239822741008,14.4164802375927,
127.713584818354)) ;
#145016 = CARTESIAN_POINT('Ctrl Pts',(-28.8060651324488,14.5415580398573,
127.986435060222)) ;
#145017 = CARTESIAN_POINT('Ctrl Pts',(-28.8956906557492,14.5869148378636,
128.281369404631)) ;
#145018 = CARTESIAN_POINT('Ctrl Pts',(-28.98562546963,14.549009953407,128.577193806147)) ;
#145019 = CARTESIAN_POINT('Ctrl Pts',(-29.0689498515829,14.4299835709606,
128.853812302228)) ;
#145020 = CARTESIAN_POINT('Ctrl Pts',(-29.1383779103369,14.2395160277486,
129.089680125683)) ;
#145021 = CARTESIAN_POINT('Ctrl Pts',(-29.1887817833045,13.9900850952094,
129.270073111603)) ;
#145022 = CARTESIAN_POINT('Ctrl Pts',(-29.2155234000854,13.7002631098511,
129.381303903886)) ;
#145023 = CARTESIAN_POINT('Ctrl Pts',(-29.2160909046462,13.3906063370585,
129.41607595645)) ;
#145024 = CARTESIAN_POINT('Ctrl Pts',(-29.1895770572792,13.0826197342829,
129.371807848553)) ;
#145025 = CARTESIAN_POINT('Ctrl Pts',(-29.1372769875413,12.7997480934514,
129.252135719739)) ;
#145026 = CARTESIAN_POINT('Ctrl Pts',(-29.0622377639789,12.5614902723847,
129.066030746683)) ;
#145027 = CARTESIAN_POINT('Ctrl Pts',(-28.9688868831584,12.3846250062646,
128.826489468998)) ;
#145028 = CARTESIAN_POINT('Ctrl Pts',(-28.863379279089,12.2824687795427,128.551412625249)) ;
#145029 = CARTESIAN_POINT('Ctrl Pts',(-28.7528489225533,12.2619556367439,
128.26156433009)) ;
#145030 = CARTESIAN_POINT('Ctrl Pts',(-28.6437294898597,12.3244285368361,
127.975958900215)) ;
#145031 = CARTESIAN_POINT('Ctrl Pts',(-28.543390154748,12.4664340564494,127.7160730758)) ;
#145032 = CARTESIAN_POINT('Ctrl Pts',(-28.45911478577,12.6753487848156,127.502844610872)) ;
#145033 = CARTESIAN_POINT('Ctrl Pts',(-28.3949800858147,12.9390315175275,
127.348664441927)) ;
#145034 = CARTESIAN_POINT('Ctrl Pts',(-28.3555174386426,13.2369183961831,
127.266484174329)) ;
#145035 = CARTESIAN_POINT('Ctrl Pts',(-28.3427341604387,13.5497744886041,
127.262423775639)) ;
#145036 = CARTESIAN_POINT('Ctrl Pts',(-28.3567662936906,13.8506095454533,
127.336367876544)) ;
#145037 = CARTESIAN_POINT('Ctrl Pts',(-28.3959609227216,14.1229210683533,
127.484053733088)) ;
#145038 = CARTESIAN_POINT('Ctrl Pts',(-28.4565807352272,14.3440341407498,
127.694191101912)) ;
#145039 = CARTESIAN_POINT('Ctrl Pts',(-28.533812846294,14.5000650906738,127.95294779839)) ;
#145040 = CARTESIAN_POINT('Ctrl Pts',(-28.6217580585773,14.5786444747034,
128.243152404162)) ;
#145041 = CARTESIAN_POINT('Ctrl Pts',(-28.7118706340383,14.5743811476286,
128.539290888972)) ;
#145042 = CARTESIAN_POINT('Ctrl Pts',(-28.7991111237447,14.4873598311618,
128.82745330766)) ;
#145043 = CARTESIAN_POINT('Ctrl Pts',(-28.8748372539666,14.3240886154077,
129.081775713549)) ;
#145044 = CARTESIAN_POINT('Ctrl Pts',(-28.9333779405285,14.0972552260208,
129.285808257697)) ;
#145045 = CARTESIAN_POINT('Ctrl Pts',(-28.9701540565685,13.8219066558181,
129.426323278948)) ;
#145046 = CARTESIAN_POINT('Ctrl Pts',(-28.9815743172463,13.516025574875,129.492975539389)) ;
#145047 = CARTESIAN_POINT('Ctrl Pts',(-28.9658944739719,13.2050736952722,
129.480284798213)) ;
#145048 = CARTESIAN_POINT('Ctrl Pts',(-28.9239550053985,12.9106473531297,
129.390776717177)) ;
#145049 = CARTESIAN_POINT('Ctrl Pts',(-28.8576902058508,12.6518068036689,
129.230321014171)) ;
#145050 = CARTESIAN_POINT('Ctrl Pts',(-28.7711031640628,12.4481718276841,
129.010524241751)) ;
#145051 = CARTESIAN_POINT('Ctrl Pts',(-28.6698281713027,12.3143466020562,
128.747799049023)) ;
#145052 = CARTESIAN_POINT('Ctrl Pts',(-28.5598558153291,12.2602411283263,
128.459807572917)) ;
#145053 = CARTESIAN_POINT('Ctrl Pts',(-28.4501327796536,12.289044221804,128.172135467012)) ;
#145054 = CARTESIAN_POINT('Ctrl Pts',(-28.3450924897601,12.3996399121577,
127.898576733604)) ;
#145055 = CARTESIAN_POINT('Ctrl Pts',(-28.2537095920121,12.5827969137066,
127.664649432031)) ;
#145056 = CARTESIAN_POINT('Ctrl Pts',(-28.1805860737797,12.8269629913892,
127.4842275229)) ;
#145057 = CARTESIAN_POINT('Ctrl Pts',(-28.1309253611483,13.1127056194501,
127.372192542966)) ;
#145058 = CARTESIAN_POINT('Ctrl Pts',(-28.1070965691472,13.4217118754633,
127.335748937024)) ;
#145059 = CARTESIAN_POINT('Ctrl Pts',(-28.1103019107213,13.7304251092952,
127.378225357934)) ;
#145060 = CARTESIAN_POINT('Ctrl Pts',(-28.1397723896426,14.0183443121755,
127.497588937897)) ;
#145061 = CARTESIAN_POINT('Ctrl Pts',(-28.1921615804711,14.2615012050008,
127.68363777181)) ;
#145062 = CARTESIAN_POINT('Ctrl Pts',(-28.2633477193032,14.4455241702922,
127.924703064281)) ;
#145063 = CARTESIAN_POINT('Ctrl Pts',(-28.3473562951541,14.5564730573808,
128.20319199203)) ;
#145064 = CARTESIAN_POINT('Ctrl Pts',(-28.4381713240423,14.5860332568258,
128.501810889804)) ;
#145065 = CARTESIAN_POINT('Ctrl Pts',(-28.5267754984946,14.5327319791753,
128.79353140372)) ;
#145066 = CARTESIAN_POINT('Ctrl Pts',(-28.6083489557468,14.3988254927601,
129.065167069407)) ;
#145067 = CARTESIAN_POINT('Ctrl Pts',(-28.674312050933,14.1966329256883,129.290810388347)) ;
#145068 = CARTESIAN_POINT('Ctrl Pts',(-28.7206126327925,13.9381994026002,
129.459218514531)) ;
#145069 = CARTESIAN_POINT('Ctrl Pts',(-28.7425880079729,13.6421506980583,
129.55661445211)) ;
#145070 = CARTESIAN_POINT('Ctrl Pts',(-28.7380161215275,13.3319747136995,
129.576294413639)) ;
#145071 = CARTESIAN_POINT('Ctrl Pts',(-28.7066575696832,13.0275240722509,
129.517800451875)) ;
#145072 = CARTESIAN_POINT('Ctrl Pts',(-28.6494163393576,12.7499512402199,
129.383895833374)) ;
#145073 = CARTESIAN_POINT('Ctrl Pts',(-28.570733840793,12.5230805349149,129.187040404072)) ;
#145074 = CARTESIAN_POINT('Ctrl Pts',(-28.4747567031311,12.3595163071095,
128.939784733654)) ;
#145075 = CARTESIAN_POINT('Ctrl Pts',(-28.3674514892643,12.2720600916224,
128.659532359337)) ;
#145076 = CARTESIAN_POINT('Ctrl Pts',(-28.2563402590024,12.2676665525214,
128.36809970917)) ;
#145077 = CARTESIAN_POINT('Ctrl Pts',(-28.1491360838674,12.3451448696153,
128.08785944284)) ;
#145078 = CARTESIAN_POINT('Ctrl Pts',(-28.0512687436739,12.5004783202174,
127.835162531413)) ;
#145079 = CARTESIAN_POINT('Ctrl Pts',(-27.9702282254497,12.7212078449696,
127.631477262919)) ;
#145080 = CARTESIAN_POINT('Ctrl Pts',(-27.9103930589021,12.9936146304865,
127.489925505009)) ;
#145081 = CARTESIAN_POINT('Ctrl Pts',(-27.8760021682395,13.2947838231295,
127.422460801043)) ;
#145082 = CARTESIAN_POINT('Ctrl Pts',(-27.8682065706614,13.6064069014527,
127.432836288194)) ;
#145083 = CARTESIAN_POINT('Ctrl Pts',(-27.8871850592498,13.9050218268895,
127.521439035055)) ;
#145084 = CARTESIAN_POINT('Ctrl Pts',(-27.9307052432448,14.1686337353897,
127.681683087378)) ;
#145085 = CARTESIAN_POINT('Ctrl Pts',(-27.9948873964674,14.3788183161701,
127.902267366194)) ;
#145086 = CARTESIAN_POINT('Ctrl Pts',(-28.0745692281525,14.520866298431,128.168177014756)) ;
#145087 = CARTESIAN_POINT('Ctrl Pts',(-28.1633227835529,14.5841620003351,
128.460616494003)) ;
#145088 = CARTESIAN_POINT('Ctrl Pts',(-28.2537824709229,14.5641966090762,
128.757971972895)) ;
#145089 = CARTESIAN_POINT('Ctrl Pts',(-28.3390215958204,14.4625801801971,
129.040108638781)) ;
#145090 = CARTESIAN_POINT('Ctrl Pts',(-28.4122062994549,14.2860054922745,
129.287088654733)) ;
#145091 = CARTESIAN_POINT('Ctrl Pts',(-28.466988907218,14.0484511491475,129.480174962356)) ;
#145092 = CARTESIAN_POINT('Ctrl Pts',(-28.4991949158601,13.7663469405247,
129.607316620214)) ;
#145093 = CARTESIAN_POINT('Ctrl Pts',(-28.5055693504399,13.4574607709576,
129.659232632401)) ;
#145094 = CARTESIAN_POINT('Ctrl Pts',(-28.4849795148332,13.1488899250601,
129.632073485812)) ;
#145095 = CARTESIAN_POINT('Ctrl Pts',(-28.438125868901,12.8583365008137,129.528365294442)) ;
#145096 = CARTESIAN_POINT('Ctrl Pts',(-28.3675738014983,12.6085157648157,
129.355411721836)) ;
#145097 = CARTESIAN_POINT('Ctrl Pts',(-28.2779335638049,12.4173946912655,
129.126629988132)) ;
#145098 = CARTESIAN_POINT('Ctrl Pts',(-28.1745614589347,12.2980452527152,
128.857787657823)) ;
#145099 = CARTESIAN_POINT('Ctrl Pts',(-28.0644798746441,12.2592457777712,
128.569281832608)) ;
#145100 = CARTESIAN_POINT('Ctrl Pts',(-27.9541455681162,12.3040208605449,
128.280192572425)) ;
#145101 = CARTESIAN_POINT('Ctrl Pts',(-27.8518137736169,12.4286939369855,
128.01430350491)) ;
#145102 = CARTESIAN_POINT('Ctrl Pts',(-27.7632715398407,12.6243590090332,
127.788745391501)) ;
#145103 = CARTESIAN_POINT('Ctrl Pts',(-27.6940711138233,12.8789083522399,
127.619878057419)) ;
#145104 = CARTESIAN_POINT('Ctrl Pts',(-27.6492626440896,13.1702261318585,
127.521984841382)) ;
#145105 = CARTESIAN_POINT('Ctrl Pts',(-27.6305164470897,13.4805037318096,
127.500338767568)) ;
#145106 = CARTESIAN_POINT('Ctrl Pts',(-27.638835187958,13.7876511812746,127.557856305416)) ;
#145107 = CARTESIAN_POINT('Ctrl Pts',(-27.6729022423348,14.0678452982214,
127.690522212597)) ;
#145108 = CARTESIAN_POINT('Ctrl Pts',(-27.7290143253781,14.3007432991358,
127.887391380954)) ;
#145109 = CARTESIAN_POINT('Ctrl Pts',(-27.8033875281781,14.472578666663,128.137894751171)) ;
#145110 = CARTESIAN_POINT('Ctrl Pts',(-27.8890145289959,14.5682598997855,
128.42107403151)) ;
#145111 = CARTESIAN_POINT('Ctrl Pts',(-27.9796584294107,14.5824152858443,
128.719000952207)) ;
#145112 = CARTESIAN_POINT('Ctrl Pts',(-28.0679946971491,14.5133614382036,
129.010212950777)) ;
#145113 = CARTESIAN_POINT('Ctrl Pts',(-28.1468971665483,14.3656854854221,
129.273906123905)) ;
#145114 = CARTESIAN_POINT('Ctrl Pts',(-28.209580420455,14.1519222579812,129.490000886093)) ;
#145115 = CARTESIAN_POINT('Ctrl Pts',(-28.2516699552296,13.8839964820202,
129.646218872573)) ;
#145116 = CARTESIAN_POINT('Ctrl Pts',(-28.268649225353,13.5839684953717,129.728941659316)) ;
#145117 = CARTESIAN_POINT('Ctrl Pts',(-28.2590350628778,13.2736209953703,
129.733860927166)) ;
#145118 = CARTESIAN_POINT('Ctrl Pts',(-28.2226940752123,12.9727615411734,
129.66082637878)) ;
#145119 = CARTESIAN_POINT('Ctrl Pts',(-28.1611673220689,12.7034620049653,
129.514320432465)) ;
#145120 = CARTESIAN_POINT('Ctrl Pts',(-28.0786249670964,12.4867211493109,
129.306299596008)) ;
#145121 = CARTESIAN_POINT('Ctrl Pts',(-27.9799272757244,12.3368636809282,
129.051131387346)) ;
#145122 = CARTESIAN_POINT('Ctrl Pts',(-27.8719194784827,12.2650346838616,
128.768645899096)) ;
#145123 = CARTESIAN_POINT('Ctrl Pts',(-27.7607881458193,12.2758062745913,
128.477173097563)) ;
#145124 = CARTESIAN_POINT('Ctrl Pts',(-27.6541366047843,12.3692807546481,
128.198814238508)) ;
#145125 = CARTESIAN_POINT('Ctrl Pts',(-27.5593097138098,12.5378929706017,
127.954885764186)) ;
#145126 = CARTESIAN_POINT('Ctrl Pts',(-27.4820169207693,12.7694277831183,
127.762148018036)) ;
#145127 = CARTESIAN_POINT('Ctrl Pts',(-27.4267956575346,13.0484836383152,
127.633986587578)) ;
#145128 = CARTESIAN_POINT('Ctrl Pts',(-27.3972448682813,13.3553252345684,
127.580904766868)) ;
#145129 = CARTESIAN_POINT('Ctrl Pts',(-27.3946987479372,13.6640556396721,
127.606387504147)) ;
#145130 = CARTESIAN_POINT('Ctrl Pts',(-27.4184411975963,13.9577070644724,
127.708900115504)) ;
#145131 = CARTESIAN_POINT('Ctrl Pts',(-27.4662212855069,14.2128779960594,
127.881609402868)) ;
#145132 = CARTESIAN_POINT('Ctrl Pts',(-27.5340439011821,14.4117544272494,
128.112953198524)) ;
#145133 = CARTESIAN_POINT('Ctrl Pts',(-27.6157591745542,14.5391283033453,
128.384716022554)) ;
#145134 = CARTESIAN_POINT('Ctrl Pts',(-27.7056825536617,14.5867879380275,
128.680669932691)) ;
#145135 = CARTESIAN_POINT('Ctrl Pts',(-27.7952749803668,14.5512051546367,
128.975335967388)) ;
#145136 = CARTESIAN_POINT('Ctrl Pts',(-27.879035841241,14.4343419889086,129.253282623546)) ;
#145137 = CARTESIAN_POINT('Ctrl Pts',(-27.9489094001948,14.2455278937518,
129.490460406613)) ;
#145138 = CARTESIAN_POINT('Ctrl Pts',(-27.999822466142,13.9981929158514,129.672259071705)) ;
#145139 = CARTESIAN_POINT('Ctrl Pts',(-28.027364677321,13.7085066698523,129.785915013751)) ;
#145140 = CARTESIAN_POINT('Ctrl Pts',(-28.0286285492022,13.3995793870564,
129.822670392743)) ;
#145141 = CARTESIAN_POINT('Ctrl Pts',(-28.0030498332934,13.0919774585784,
129.781044462692)) ;
#145142 = CARTESIAN_POINT('Ctrl Pts',(-27.9511801663322,12.8067303604848,
129.662796978732)) ;
#145143 = CARTESIAN_POINT('Ctrl Pts',(-27.8771115641797,12.5682008646981,
129.479352709281)) ;
#145144 = CARTESIAN_POINT('Ctrl Pts',(-27.7840799881775,12.3888212047449,
129.240810402594)) ;
#145145 = CARTESIAN_POINT('Ctrl Pts',(-27.6789762774325,12.2844119375082,
128.966867849549)) ;
#145146 = CARTESIAN_POINT('Ctrl Pts',(-27.5681554143404,12.2613333969067,
128.676275527954)) ;
#145147 = CARTESIAN_POINT('Ctrl Pts',(-27.4590172958769,12.3215794743214,
128.390578491288)) ;
#145148 = CARTESIAN_POINT('Ctrl Pts',(-27.3586454587107,12.4606919481936,
128.13048055496)) ;
#145149 = CARTESIAN_POINT('Ctrl Pts',(-27.2734486429436,12.6684214506416,
127.914688951451)) ;
#145150 = CARTESIAN_POINT('Ctrl Pts',(-27.2085144692729,12.9319196123432,
127.758288713112)) ;
#145151 = CARTESIAN_POINT('Ctrl Pts',(-27.1685755827829,13.2279083302756,
127.674578003213)) ;
#145152 = CARTESIAN_POINT('Ctrl Pts',(-27.1549269841447,13.5392234184095,
127.667835412627)) ;
#145153 = CARTESIAN_POINT('Ctrl Pts',(-27.1681724778946,13.8421684111979,
127.73964287137)) ;
#145154 = CARTESIAN_POINT('Ctrl Pts',(-27.2067395795055,14.1158321070144,
127.885518848952)) ;
#145155 = CARTESIAN_POINT('Ctrl Pts',(-27.2669534578115,14.339009376798,128.094538209038)) ;
#145156 = CARTESIAN_POINT('Ctrl Pts',(-27.3436695138408,14.4964746049257,
128.351715170359)) ;
#145157 = CARTESIAN_POINT('Ctrl Pts',(-27.4308784775676,14.5773715889881,
128.639578138836)) ;
#145158 = CARTESIAN_POINT('Ctrl Pts',(-27.5216935080159,14.5757025147149,
128.93802333203)) ;
#145159 = CARTESIAN_POINT('Ctrl Pts',(-27.6088983693204,14.490867072331,129.225995722479)) ;
#145160 = CARTESIAN_POINT('Ctrl Pts',(-27.6847829789678,14.330592253299,129.48065337557)) ;
#145161 = CARTESIAN_POINT('Ctrl Pts',(-27.7442105909782,14.1048089901007,
129.687399172449)) ;
#145162 = CARTESIAN_POINT('Ctrl Pts',(-27.7816984625605,13.8293690778141,
129.830119558559)) ;
#145163 = CARTESIAN_POINT('Ctrl Pts',(-27.7938050924863,13.526576284789,129.898498223956)) ;
#145164 = CARTESIAN_POINT('Ctrl Pts',(-27.7790423798048,13.2147294294983,
129.888571224088)) ;
#145165 = CARTESIAN_POINT('Ctrl Pts',(-27.7378005231724,12.9189024654219,
129.801161820441)) ;
#145166 = CARTESIAN_POINT('Ctrl Pts',(-27.6719242811303,12.6580299108607,
129.641948932191)) ;
#145167 = CARTESIAN_POINT('Ctrl Pts',(-27.5862120750185,12.4534345481142,
129.424564279788)) ;
#145168 = CARTESIAN_POINT('Ctrl Pts',(-27.4850277388239,12.3171076600088,
129.162191557086)) ;
#145169 = CARTESIAN_POINT('Ctrl Pts',(-27.3757741136007,12.2606844017973,
128.876123071525)) ;
#145170 = CARTESIAN_POINT('Ctrl Pts',(-27.2651782726929,12.2870889602567,
128.586143047142)) ;
#145171 = CARTESIAN_POINT('Ctrl Pts',(-27.1599366275124,12.3957983185939,
128.311983337171)) ;
#145172 = CARTESIAN_POINT('Ctrl Pts',(-27.068323828863,12.576725714127,128.07731803016)) ;
#145173 = CARTESIAN_POINT('Ctrl Pts',(-26.9946972364049,12.8186993235838,
127.895349858883)) ;
#145174 = CARTESIAN_POINT('Ctrl Pts',(-26.9440717391415,13.1050418168408,
127.780675308402)) ;
#145175 = CARTESIAN_POINT('Ctrl Pts',(-26.9196285238679,13.4130762749516,
127.742359347898)) ;
#145176 = CARTESIAN_POINT('Ctrl Pts',(-26.9220777684625,13.7214651862128,
127.782568022446)) ;
#145177 = CARTESIAN_POINT('Ctrl Pts',(-26.9505714061639,14.0093161749257,
127.898936305092)) ;
#145178 = CARTESIAN_POINT('Ctrl Pts',(-27.0027689908232,14.2560736746896,
128.084708180528)) ;
#145179 = CARTESIAN_POINT('Ctrl Pts',(-27.0733529928704,14.4412184365536,
128.323910527195)) ;
#145180 = CARTESIAN_POINT('Ctrl Pts',(-27.1570667414105,14.5543182537731,
128.601539623747)) ;
#145181 = CARTESIAN_POINT('Ctrl Pts',(-27.2473775377621,14.5864671229327,
128.89852477223)) ;
#145182 = CARTESIAN_POINT('Ctrl Pts',(-27.3367275624371,14.5351930359694,
129.19265847879)) ;
#145183 = CARTESIAN_POINT('Ctrl Pts',(-27.4181292069275,14.4042256510203,
129.463583735512)) ;
#145184 = CARTESIAN_POINT('Ctrl Pts',(-27.4849111444952,14.2033619799806,
129.691746469449)) ;
#145185 = CARTESIAN_POINT('Ctrl Pts',(-27.5318288818491,13.9460942692561,
129.861964597238)) ;
#145186 = CARTESIAN_POINT('Ctrl Pts',(-27.5545247889339,13.6510939576202,
129.96143831759)) ;
#145187 = CARTESIAN_POINT('Ctrl Pts',(-27.550764534156,13.3409631929891,129.983496828996)) ;
#145188 = CARTESIAN_POINT('Ctrl Pts',(-27.5200421487155,13.0355468372364,
129.926920899871)) ;
#145189 = CARTESIAN_POINT('Ctrl Pts',(-27.463891512529,12.7584809477333,129.795997149247)) ;
#145190 = CARTESIAN_POINT('Ctrl Pts',(-27.3855386705038,12.5287898024968,
129.600244223915)) ;
#145191 = CARTESIAN_POINT('Ctrl Pts',(-27.2899654965722,12.3633456659364,
129.35415921584)) ;
#145192 = CARTESIAN_POINT('Ctrl Pts',(-27.1832672774182,12.2737023197767,
129.075570207765)) ;
#145193 = CARTESIAN_POINT('Ctrl Pts',(-27.0721332475999,12.2663504667095,
128.784079554544)) ;
#145194 = CARTESIAN_POINT('Ctrl Pts',(-26.9640750440213,12.34208017502,128.501551995175)) ;
#145195 = CARTESIAN_POINT('Ctrl Pts',(-26.8662978136907,12.4946576903152,
128.248958027811)) ;
#145196 = CARTESIAN_POINT('Ctrl Pts',(-26.7844064413056,12.7142650578431,
128.042896300319)) ;
#145197 = CARTESIAN_POINT('Ctrl Pts',(-26.7239781458071,12.9853995961956,
127.899588524508)) ;
#145198 = CARTESIAN_POINT('Ctrl Pts',(-26.6888087161657,13.2860375673385,
127.829858435003)) ;
#145199 = CARTESIAN_POINT('Ctrl Pts',(-26.6802656934047,13.5985523264733,
127.838138380085)) ;
#145200 = CARTESIAN_POINT('Ctrl Pts',(-26.6986085159139,13.8975129640997,
127.924860800194)) ;
#145201 = CARTESIAN_POINT('Ctrl Pts',(-26.7412689213863,14.1612607305214,
128.082449499982)) ;
#145202 = CARTESIAN_POINT('Ctrl Pts',(-26.8050662272223,14.3739608986485,
128.302005079039)) ;
#145203 = CARTESIAN_POINT('Ctrl Pts',(-26.8846809635726,14.5182947311408,
128.567816786118)) ;
#145204 = CARTESIAN_POINT('Ctrl Pts',(-26.9731269723443,14.5834512891337,
128.859295413823)) ;
#145205 = CARTESIAN_POINT('Ctrl Pts',(-27.063336767471,14.5659482056826,129.155813358164)) ;
#145206 = CARTESIAN_POINT('Ctrl Pts',(-27.1488060860294,14.4667697468738,
129.438612349934)) ;
#145207 = CARTESIAN_POINT('Ctrl Pts',(-27.2225032558955,14.2923285358451,
129.68709763699)) ;
#145208 = CARTESIAN_POINT('Ctrl Pts',(-27.2781332705648,14.0548140143778,
129.882849456784)) ;
#145209 = CARTESIAN_POINT('Ctrl Pts',(-27.3107599426325,13.7751053966171,
130.011041198749)) ;
#145210 = CARTESIAN_POINT('Ctrl Pts',(-27.3180362901016,13.4671706685235,
130.065540763481)) ;
#145211 = CARTESIAN_POINT('Ctrl Pts',(-27.298042554253,13.1566326629542,130.040310967005)) ;
#145212 = CARTESIAN_POINT('Ctrl Pts',(-27.2521782342998,12.8670308580196,
129.939287114639)) ;
#145213 = CARTESIAN_POINT('Ctrl Pts',(-27.1820662948561,12.614625742012,129.767747675979)) ;
#145214 = CARTESIAN_POINT('Ctrl Pts',(-27.0926762160904,12.4216271710516,
129.539751137083)) ;
#145215 = CARTESIAN_POINT('Ctrl Pts',(-26.9900934748709,12.3004936351809,
129.273060908702)) ;
#145216 = CARTESIAN_POINT('Ctrl Pts',(-26.8794850458073,12.2591976942699,
128.983206367494)) ;
#145217 = CARTESIAN_POINT('Ctrl Pts',(-26.769798191186,12.3014766458867,128.695782118538)) ;
#145218 = CARTESIAN_POINT('Ctrl Pts',(-26.6668884802955,12.4236752425343,
128.428268347536)) ;
#145219 = CARTESIAN_POINT('Ctrl Pts',(-26.5773353042428,12.6191375618547,
128.199983809857)) ;
#145220 = CARTESIAN_POINT('Ctrl Pts',(-26.5080282119653,12.8707902517674,
128.030586096778)) ;
#145221 = CARTESIAN_POINT('Ctrl Pts',(-26.4623661086803,13.1617413465553,
127.930263010471)) ;
#145222 = CARTESIAN_POINT('Ctrl Pts',(-26.4429131084249,13.4713353015044,
127.906497282117)) ;
#145223 = CARTESIAN_POINT('Ctrl Pts',(-26.4504147849802,13.7785022490456,
127.961585642172)) ;
#145224 = CARTESIAN_POINT('Ctrl Pts',(-26.4836546467707,14.0596469751513,
128.091803410612)) ;
#145225 = CARTESIAN_POINT('Ctrl Pts',(-26.5394610982308,14.2953142931135,
128.287948833244)) ;
#145226 = CARTESIAN_POINT('Ctrl Pts',(-26.6134196928557,14.468964761841,128.537226975926)) ;
#145227 = CARTESIAN_POINT('Ctrl Pts',(-26.6990820403619,14.566840747798,128.820608211893)) ;
#145228 = CARTESIAN_POINT('Ctrl Pts',(-26.7892429864435,14.5831863557758,
129.116954844477)) ;
#145229 = CARTESIAN_POINT('Ctrl Pts',(-26.8781110470037,14.5160478882273,
129.409866842151)) ;
#145230 = CARTESIAN_POINT('Ctrl Pts',(-26.956952315364,14.3710572999732,129.673209306742)) ;
#145231 = CARTESIAN_POINT('Ctrl Pts',(-27.0203223929184,14.1586831437498,
129.891382565407)) ;
#145232 = CARTESIAN_POINT('Ctrl Pts',(-27.0629647324315,13.8924167167611,
130.049154173624)) ;
#145233 = CARTESIAN_POINT('Ctrl Pts',(-27.0807543092698,13.5934589593166,
130.134207108121)) ;
#145234 = CARTESIAN_POINT('Ctrl Pts',(-27.0718785730549,13.2817948443867,
130.141423438504)) ;
#145235 = CARTESIAN_POINT('Ctrl Pts',(-27.036211707864,12.9807519837477,130.070323117634)) ;
#145236 = CARTESIAN_POINT('Ctrl Pts',(-26.9757193317698,12.7114087835464,
129.926679055096)) ;
#145237 = CARTESIAN_POINT('Ctrl Pts',(-26.8934530739077,12.4920355070178,
129.71959003431)) ;
#145238 = CARTESIAN_POINT('Ctrl Pts',(-26.7954032837469,12.340409192469,129.466223268637)) ;
#145239 = CARTESIAN_POINT('Ctrl Pts',(-26.6872087381884,12.2658594126602,
129.183310594939)) ;
#145240 = CARTESIAN_POINT('Ctrl Pts',(-26.5762060450296,12.2744067953506,
128.892167277779)) ;
#145241 = CARTESIAN_POINT('Ctrl Pts',(-26.4696120195096,12.3651074088565,
128.61388267482)) ;
#145242 = CARTESIAN_POINT('Ctrl Pts',(-26.3741832777799,12.5316553295761,
128.368240358776)) ;
#145243 = CARTESIAN_POINT('Ctrl Pts',(-26.2960979131251,12.7621962066438,
128.173274307522)) ;
#145244 = CARTESIAN_POINT('Ctrl Pts',(-26.2402918341511,13.0400249877383,
128.043379258454)) ;
#145245 = CARTESIAN_POINT('Ctrl Pts',(-26.209984773203,13.3449925663018,127.987941407805)) ;
#145246 = CARTESIAN_POINT('Ctrl Pts',(-26.2066126024052,13.6560824874518,
128.01124626749)) ;
#145247 = CARTESIAN_POINT('Ctrl Pts',(-26.2296304118587,13.949523069505,128.111533856934)) ;
#145248 = CARTESIAN_POINT('Ctrl Pts',(-26.2767111329634,14.2060602321428,
128.282193262609)) ;
#145249 = CARTESIAN_POINT('Ctrl Pts',(-26.3440044394362,14.4068533843326,
128.511982775146)) ;
#145250 = CARTESIAN_POINT('Ctrl Pts',(-26.4255019943792,14.5364834537221,
128.783152349287)) ;
#145251 = CARTESIAN_POINT('Ctrl Pts',(-26.5149273646816,14.5865952294226,
129.077512486312)) ;
#145252 = CARTESIAN_POINT('Ctrl Pts',(-26.6050918737861,14.5532896916384,
129.374032831588)) ;
#145253 = CARTESIAN_POINT('Ctrl Pts',(-26.6887557362477,14.4391769961996,
129.651538401177)) ;
#145254 = CARTESIAN_POINT('Ctrl Pts',(-26.7592891858962,14.2521193934998,
129.890716002212)) ;
#145255 = CARTESIAN_POINT('Ctrl Pts',(-26.8108385572124,14.0064610043906,
130.074351365964)) ;
#145256 = CARTESIAN_POINT('Ctrl Pts',(-26.8391959482818,13.7162751862111,
130.190548474023)) ;
#145257 = CARTESIAN_POINT('Ctrl Pts',(-26.8411767728426,13.4088590372399,
130.229260162228)) ;
#145258 = CARTESIAN_POINT('Ctrl Pts',(-26.8163531916444,13.10053389726,130.189883749462)) ;
#145259 = CARTESIAN_POINT('Ctrl Pts',(-26.7654365125188,12.8153801351655,
130.07428755891)) ;
#145260 = CARTESIAN_POINT('Ctrl Pts',(-26.6918270487183,12.5742829301141,
129.892291503174)) ;
#145261 = CARTESIAN_POINT('Ctrl Pts',(-26.5987510300196,12.3924207645517,
129.653771309622)) ;
#145262 = CARTESIAN_POINT('Ctrl Pts',(-26.494437484084,12.2864008460228,129.381964574177)) ;
#145263 = CARTESIAN_POINT('Ctrl Pts',(-26.3833229207034,12.2608494094795,
129.090623959521)) ;
#145264 = CARTESIAN_POINT('Ctrl Pts',(-26.2745004596113,12.318610673207,128.805709814383)) ;
#145265 = CARTESIAN_POINT('Ctrl Pts',(-26.1735653192533,12.4554523498405,
128.544018330009)) ;
#145266 = CARTESIAN_POINT('Ctrl Pts',(-26.0875660779443,12.6626735869421,
128.326034888429)) ;
#145267 = CARTESIAN_POINT('Ctrl Pts',(-26.0226228583949,12.9221026671482,
128.169263802032)) ;
#145268 = CARTESIAN_POINT('Ctrl Pts',(-25.9815253480016,13.2188659560216,
128.082358785624)) ;
#145269 = CARTESIAN_POINT('Ctrl Pts',(-25.9671690642881,13.5309970504502,
128.073639559481)) ;
#145270 = CARTESIAN_POINT('Ctrl Pts',(-25.9796292863015,13.833391117926,128.143036056483)) ;
#145271 = CARTESIAN_POINT('Ctrl Pts',(-26.0174576883516,14.1082733327472,
128.286754126692)) ;
#145272 = CARTESIAN_POINT('Ctrl Pts',(-26.0770945744703,14.333273457915,128.494092864001)) ;
#145273 = CARTESIAN_POINT('Ctrl Pts',(-26.1535867878669,14.493089968581,128.750689737769)) ;
#145274 = CARTESIAN_POINT('Ctrl Pts',(-26.240492285696,14.5762694878071,129.037623503028)) ;
#145275 = CARTESIAN_POINT('Ctrl Pts',(-26.3316446527599,14.5766426332955,
129.337185238566)) ;
#145276 = CARTESIAN_POINT('Ctrl Pts',(-26.4182679904325,14.4950561386841,
129.623146842004)) ;
#145277 = CARTESIAN_POINT('Ctrl Pts',(-26.4952465067177,14.3357812086937,
129.881281959693)) ;
#145278 = CARTESIAN_POINT('Ctrl Pts',(-26.5549921587296,14.1117725486506,
130.08888574024)) ;
#145279 = CARTESIAN_POINT('Ctrl Pts',(-26.5931611985058,13.8385111509001,
130.233491753311)) ;
#145280 = CARTESIAN_POINT('Ctrl Pts',(-26.6060312661162,13.5338961508562,
130.304356398855)) ;
#145281 = CARTESIAN_POINT('Ctrl Pts',(-26.5921064352985,13.224257482388,130.296623484146)) ;
#145282 = CARTESIAN_POINT('Ctrl Pts',(-26.5514075441165,12.9262818286679,
130.210970393599)) ;
#145283 = CARTESIAN_POINT('Ctrl Pts',(-26.4865801356298,12.6654697880194,
130.054625548478)) ;
#145284 = CARTESIAN_POINT('Ctrl Pts',(-26.4005704729957,12.4574145749278,
129.836677200713)) ;
#145285 = CARTESIAN_POINT('Ctrl Pts',(-26.3007750838948,12.3205165370977,
129.578002098338)) ;
#145286 = CARTESIAN_POINT('Ctrl Pts',(-26.1910732522884,12.2610390449612,
129.290819720059)) ;
#145287 = CARTESIAN_POINT('Ctrl Pts',(-26.0807718810186,12.2851065235111,
129.00158758569)) ;
#145288 = CARTESIAN_POINT('Ctrl Pts',(-25.9751380722918,12.3913707658575,
128.726315756247)) ;
#145289 = CARTESIAN_POINT('Ctrl Pts',(-25.8829725862754,12.5705078939367,
128.490066749863)) ;
#145290 = CARTESIAN_POINT('Ctrl Pts',(-25.8087402089946,12.8110531024917,
128.306339450124)) ;
#145291 = CARTESIAN_POINT('Ctrl Pts',(-25.7574503041843,13.0958081066442,
128.189657242365)) ;
#145292 = CARTESIAN_POINT('Ctrl Pts',(-25.7321614965632,13.4043791396556,
128.148971680577)) ;
#145293 = CARTESIAN_POINT('Ctrl Pts',(-25.7338009498791,13.7127503611852,
128.186770642114)) ;
#145294 = CARTESIAN_POINT('Ctrl Pts',(-25.7619120955808,14.0031465384866,
128.302242202483)) ;
#145295 = CARTESIAN_POINT('Ctrl Pts',(-25.8127877498031,14.2480984869967,
128.483700631739)) ;
#145296 = CARTESIAN_POINT('Ctrl Pts',(-25.883318478156,14.4370589144751,128.723005956744)) ;
#145297 = CARTESIAN_POINT('Ctrl Pts',(-25.9667449820352,14.5521322480481,
128.999773748139)) ;
#145298 = CARTESIAN_POINT('Ctrl Pts',(-26.0570620921973,14.5867077636068,
129.296815980901)) ;
#145299 = CARTESIAN_POINT('Ctrl Pts',(-26.1463754355628,14.5378478925882,
129.59078041807)) ;
#145300 = CARTESIAN_POINT('Ctrl Pts',(-26.2280883194995,14.409203021957,129.862607874009)) ;
#145301 = CARTESIAN_POINT('Ctrl Pts',(-26.2954388715456,14.2102655044933,
130.092438570625)) ;
#145302 = CARTESIAN_POINT('Ctrl Pts',(-26.3431293730661,13.9531164546974,
130.265060015164)) ;
#145303 = CARTESIAN_POINT('Ctrl Pts',(-26.3664177483922,13.6605444903127,
130.366073831618)) ;
#145304 = CARTESIAN_POINT('Ctrl Pts',(-26.3634487238989,13.3493859295917,
130.390576421491)) ;
#145305 = CARTESIAN_POINT('Ctrl Pts',(-26.3335452830324,13.0444134847032,
130.336290333141)) ;
#145306 = CARTESIAN_POINT('Ctrl Pts',(-26.2780557893883,12.7658508385772,
130.207343051435)) ;
#145307 = CARTESIAN_POINT('Ctrl Pts',(-26.2003158885766,12.5346698137633,
130.013361829543)) ;
#145308 = CARTESIAN_POINT('Ctrl Pts',(-26.1050182124943,12.3668712653983,
129.768133516794)) ;
#145309 = CARTESIAN_POINT('Ctrl Pts',(-25.9983394998777,12.2750736353354,
129.489657461887)) ;
#145310 = CARTESIAN_POINT('Ctrl Pts',(-25.8877952399973,12.2654123935104,
129.19972048684)) ;
#145311 = CARTESIAN_POINT('Ctrl Pts',(-25.7794715126841,12.3385001490515,
128.916434752625)) ;
#145312 = CARTESIAN_POINT('Ctrl Pts',(-25.6810457853793,12.4893941605664,
128.662034056247)) ;
#145313 = CARTESIAN_POINT('Ctrl Pts',(-25.5987350438462,12.7071836242874,
128.454714816302)) ;
#145314 = CARTESIAN_POINT('Ctrl Pts',(-25.5377622535892,12.976008781698,128.309697798118)) ;
#145315 = CARTESIAN_POINT('Ctrl Pts',(-25.5016580962441,13.2771672423765,
128.237367037692)) ;
#145316 = CARTESIAN_POINT('Ctrl Pts',(-25.4923643066174,13.5885364783272,
128.24332796172)) ;
#145317 = CARTESIAN_POINT('Ctrl Pts',(-25.5097986358348,13.8883475892356,
128.32740133913)) ;
#145318 = CARTESIAN_POINT('Ctrl Pts',(-25.5520032926188,14.1546798103871,
128.483821229637)) ;
#145319 = CARTESIAN_POINT('Ctrl Pts',(-25.6151380635207,14.3683945721778,
128.701351080741)) ;
#145320 = CARTESIAN_POINT('Ctrl Pts',(-25.6940182660661,14.5146640723976,
128.964889919477)) ;
#145321 = CARTESIAN_POINT('Ctrl Pts',(-25.7825768658118,14.5827891637854,
129.256811751722)) ;
#145322 = CARTESIAN_POINT('Ctrl Pts',(-25.8730390891615,14.5676065821518,
129.554141480536)) ;
#145323 = CARTESIAN_POINT('Ctrl Pts',(-25.9587213698666,14.4706130851543,
129.837556439225)) ;
#145324 = CARTESIAN_POINT('Ctrl Pts',(-26.03264838451,14.2987448591994,130.086617319719)) ;
#145325 = CARTESIAN_POINT('Ctrl Pts',(-26.0889427361501,14.063095759129,130.284302469339)) ;
#145326 = CARTESIAN_POINT('Ctrl Pts',(-26.1224378317549,13.7833207941159,
130.415161932836)) ;
#145327 = CARTESIAN_POINT('Ctrl Pts',(-26.1303660621799,13.4754882889809,
130.471596562787)) ;
#145328 = CARTESIAN_POINT('Ctrl Pts',(-26.111324532664,13.1664272505894,130.448961800146)) ;
#145329 = CARTESIAN_POINT('Ctrl Pts',(-26.0659474183763,12.8743475054809,
130.349549021052)) ;
#145330 = CARTESIAN_POINT('Ctrl Pts',(-25.9968429052108,12.6220180592587,
130.180760594169)) ;
#145331 = CARTESIAN_POINT('Ctrl Pts',(-25.9078683759823,12.4263341461984,
129.954044963807)) ;
#145332 = CARTESIAN_POINT('Ctrl Pts',(-25.8050016005084,12.3026056592769,
129.686700785145)) ;
#145333 = CARTESIAN_POINT('Ctrl Pts',(-25.6951594284179,12.2593725249827,
129.398886281629)) ;
#145334 = CARTESIAN_POINT('Ctrl Pts',(-25.5852338552597,12.2987734012192,
129.110795340355)) ;
#145335 = CARTESIAN_POINT('Ctrl Pts',(-25.4812744222043,12.4202091762236,
128.84047911961)) ;
#145336 = CARTESIAN_POINT('Ctrl Pts',(-25.3922566652092,12.611773656706,128.613389281527)) ;
#145337 = CARTESIAN_POINT('Ctrl Pts',(-25.3219304478952,12.8626551620978,
128.44114506998)) ;
#145338 = CARTESIAN_POINT('Ctrl Pts',(-25.2755717009999,13.1527448434828,
128.338777264869)) ;
#145339 = CARTESIAN_POINT('Ctrl Pts',(-25.2552923109432,13.4624298007765,
128.312634628559)) ;
#145340 = CARTESIAN_POINT('Ctrl Pts',(-25.2620703386305,13.7701811084813,
128.365629030765)) ;
#145341 = CARTESIAN_POINT('Ctrl Pts',(-25.2945336713983,14.0517728674994,
128.493510645481)) ;
#145342 = CARTESIAN_POINT('Ctrl Pts',(-25.3497468545249,14.2892527094167,
128.687942417164)) ;
#145343 = CARTESIAN_POINT('Ctrl Pts',(-25.423284853834,14.4648240462418,128.935995490194)) ;
#145344 = CARTESIAN_POINT('Ctrl Pts',(-25.5084071558922,14.5650403206084,
129.217694325303)) ;
#145345 = CARTESIAN_POINT('Ctrl Pts',(-25.5990981080236,14.583748953291,129.515806037567)) ;
#145346 = CARTESIAN_POINT('Ctrl Pts',(-25.6873241508409,14.5197167656378,
129.806529344841)) ;
#145347 = CARTESIAN_POINT('Ctrl Pts',(-25.7671195219414,14.3763314306489,
130.072885261732)) ;
#145348 = CARTESIAN_POINT('Ctrl Pts',(-25.8309798067965,14.1656644644825,
130.292474622263)) ;
#145349 = CARTESIAN_POINT('Ctrl Pts',(-25.874360274551,13.8999127599495,130.452493401639)) ;
#145350 = CARTESIAN_POINT('Ctrl Pts',(-25.8927896275635,13.6028234452547,
130.53927681015)) ;
#145351 = CARTESIAN_POINT('Ctrl Pts',(-25.8847621742614,13.291184455058,130.548977456738)) ;
#145352 = CARTESIAN_POINT('Ctrl Pts',(-25.8498954972506,12.9894029525186,
130.480221393588)) ;
#145353 = CARTESIAN_POINT('Ctrl Pts',(-25.7898002281872,12.717765879006,130.337877304595)) ;
#145354 = CARTESIAN_POINT('Ctrl Pts',(-25.708129365045,12.4972589130398,130.132477114614)) ;
#145355 = CARTESIAN_POINT('Ctrl Pts',(-25.6107425249076,12.3438957008414,
129.880956988692)) ;
#145356 = CARTESIAN_POINT('Ctrl Pts',(-25.5026424369846,12.2668705096983,
129.598352780418)) ;
#145357 = CARTESIAN_POINT('Ctrl Pts',(-25.3917428525325,12.2729078297229,
129.30747146326)) ;
#145358 = CARTESIAN_POINT('Ctrl Pts',(-25.2847600750955,12.3614501849398,
129.028106287917)) ;
#145359 = CARTESIAN_POINT('Ctrl Pts',(-25.1891585260755,12.5253315667214,
128.781860471565)) ;
#145360 = CARTESIAN_POINT('Ctrl Pts',(-25.110135939089,12.7552771114224,128.584311890392)) ;
#145361 = CARTESIAN_POINT('Ctrl Pts',(-25.0538525122355,13.0310570491295,
128.45290006936)) ;
#145362 = CARTESIAN_POINT('Ctrl Pts',(-25.0227014081751,13.3361218325012,
128.395068081625)) ;
#145363 = CARTESIAN_POINT('Ctrl Pts',(-25.0185105180042,13.6463105662156,
128.415863743252)) ;
#145364 = CARTESIAN_POINT('Ctrl Pts',(-25.040893647384,13.9424874348681,128.514511422021)) ;
#145365 = CARTESIAN_POINT('Ctrl Pts',(-25.0875308435713,14.2002009461362,
128.683896967344)) ;
#145366 = CARTESIAN_POINT('Ctrl Pts',(-25.1538679221218,14.4015262761072,
128.910674169156)) ;
#145367 = CARTESIAN_POINT('Ctrl Pts',(-25.23524054031,14.5339055048123,129.181576243816)) ;
#145368 = CARTESIAN_POINT('Ctrl Pts',(-25.3244833479966,14.5863178640293,
129.475378614211)) ;
#145369 = CARTESIAN_POINT('Ctrl Pts',(-25.4149673875239,14.55532217226,129.772919559462)) ;
#145370 = CARTESIAN_POINT('Ctrl Pts',(-25.4988480768799,14.4431215003341,
130.051053673527)) ;
#145371 = CARTESIAN_POINT('Ctrl Pts',(-25.5695954221607,14.2589451908106,
130.290713226978)) ;
#145372 = CARTESIAN_POINT('Ctrl Pts',(-25.6220034125225,14.0132050933504,
130.477057575067)) ;
#145373 = CARTESIAN_POINT('Ctrl Pts',(-25.6508730043343,13.7264814781089,
130.594456328158)) ;
#145374 = CARTESIAN_POINT('Ctrl Pts',(-25.6537138653535,13.4166671262314,
130.635978686215)) ;
#145375 = CARTESIAN_POINT('Ctrl Pts',(-25.6296001905431,13.1090562119369,
130.598563069686)) ;
#145376 = CARTESIAN_POINT('Ctrl Pts',(-25.5794380606441,12.8228936687179,
130.485173368709)) ;
#145377 = CARTESIAN_POINT('Ctrl Pts',(-25.5063529307715,12.5803482500096,
130.304721134994)) ;
#145378 = CARTESIAN_POINT('Ctrl Pts',(-25.414190730486,12.3971382780487,130.068720600588)) ;
#145379 = CARTESIAN_POINT('Ctrl Pts',(-25.3096218748052,12.2881794710329,
129.796340547925)) ;
#145380 = CARTESIAN_POINT('Ctrl Pts',(-25.1987437257025,12.260444774343,129.505635894546)) ;
#145381 = CARTESIAN_POINT('Ctrl Pts',(-25.0895511480794,12.3158800590199,
129.219706518543)) ;
#145382 = CARTESIAN_POINT('Ctrl Pts',(-24.9881999358306,12.4512316435153,
128.956853185564)) ;
#145383 = CARTESIAN_POINT('Ctrl Pts',(-24.9023755881761,12.6546809911043,
128.739090381038)) ;
#145384 = CARTESIAN_POINT('Ctrl Pts',(-24.8362095298155,12.9147731891358,
128.579018314088)) ;
#145385 = CARTESIAN_POINT('Ctrl Pts',(-24.7946204028052,13.2095560207855,
128.490523563663)) ;
#145386 = CARTESIAN_POINT('Ctrl Pts',(-24.7794015918992,13.5223875094378,
128.479378796091)) ;
#145387 = CARTESIAN_POINT('Ctrl Pts',(-24.7911074196154,13.8250175828272,
128.54653350614)) ;
#145388 = CARTESIAN_POINT('Ctrl Pts',(-24.8284540425988,14.1019896446971,
128.688975600091)) ;
#145389 = CARTESIAN_POINT('Ctrl Pts',(-24.8872835848728,14.3273313285593,
128.893786335539)) ;
#145390 = CARTESIAN_POINT('Ctrl Pts',(-24.9632695041877,14.4893435909273,
129.148882890249)) ;
#145391 = CARTESIAN_POINT('Ctrl Pts',(-25.0500604547885,14.5749600250314,
129.435520331663)) ;
#145392 = CARTESIAN_POINT('Ctrl Pts',(-25.1411078657764,14.5779281119493,
129.734734735459)) ;
#145393 = CARTESIAN_POINT('Ctrl Pts',(-25.2281667322443,14.4983364866609,
130.022066485608)) ;
#145394 = CARTESIAN_POINT('Ctrl Pts',(-25.3052181042423,14.3420895520869,
130.280252049349)) ;
#145395 = CARTESIAN_POINT('Ctrl Pts',(-25.3659941264421,14.1180210697834,
130.491128458774)) ;
#145396 = CARTESIAN_POINT('Ctrl Pts',(-25.4045283220153,13.8471807636704,
130.636621850606)) ;
#145397 = CARTESIAN_POINT('Ctrl Pts',(-25.4182653820351,13.5439412036153,
130.709945042882)) ;
#145398 = CARTESIAN_POINT('Ctrl Pts',(-25.4051205680015,13.2331633714353,
130.704601844684)) ;
#145399 = CARTESIAN_POINT('Ctrl Pts',(-25.3651505354746,12.9343807646982,
130.621084664061)) ;
#145400 = CARTESIAN_POINT('Ctrl Pts',(-25.3008865115351,12.6721977503837,
130.466411854782)) ;
#145401 = CARTESIAN_POINT('Ctrl Pts',(-25.2159087492335,12.4632419123552,
130.25129992907)) ;
#145402 = CARTESIAN_POINT('Ctrl Pts',(-25.1158600119201,12.3231158449139,
129.992095855596)) ;
#145403 = CARTESIAN_POINT('Ctrl Pts',(-25.0063074780256,12.2616017868531,
129.70533965919)) ;
#145404 = CARTESIAN_POINT('Ctrl Pts',(-24.8961505989959,12.2833201930426,
129.416474304397)) ;
#145405 = CARTESIAN_POINT('Ctrl Pts',(-24.7904450068508,12.3868877539332,
129.14092380243)) ;
#145406 = CARTESIAN_POINT('Ctrl Pts',(-24.6974041889648,12.5648231593225,
128.90226664825)) ;
#145407 = CARTESIAN_POINT('Ctrl Pts',(-24.6227059932372,12.8039602386114,
128.7171620235)) ;
#145408 = CARTESIAN_POINT('Ctrl Pts',(-24.5708840649089,13.0864729218444,
128.598787421566)) ;
#145409 = CARTESIAN_POINT('Ctrl Pts',(-24.5446815137269,13.3957238551008,
128.55554617079)) ;
#145410 = CARTESIAN_POINT('Ctrl Pts',(-24.545657676478,13.7038340489926,128.591360486886)) ;
#145411 = CARTESIAN_POINT('Ctrl Pts',(-24.5726639326172,13.9936201437027,
128.703393987333)) ;
#145412 = CARTESIAN_POINT('Ctrl Pts',(-24.623608766435,14.2431366533872,128.885488576488)) ;
#145413 = CARTESIAN_POINT('Ctrl Pts',(-24.6929890285264,14.4318623911142,
129.121078946022)) ;
#145414 = CARTESIAN_POINT('Ctrl Pts',(-24.7766421491609,14.5502397440411,
129.398740985602)) ;
#145415 = CARTESIAN_POINT('Ctrl Pts',(-24.8666514693775,14.5868194748713,
129.694789661665)) ;
#145416 = CARTESIAN_POINT('Ctrl Pts',(-24.9561889353879,14.5403267777303,
129.989453760209)) ;
#145417 = CARTESIAN_POINT('Ctrl Pts',(-25.0381948159731,14.4138414860088,
130.262123578507)) ;
#145418 = CARTESIAN_POINT('Ctrl Pts',(-25.1060482756281,14.2163546818928,
130.493461414613)) ;
#145419 = CARTESIAN_POINT('Ctrl Pts',(-25.1541101693659,13.9624647587777,
130.666937384025)) ;
#145420 = CARTESIAN_POINT('Ctrl Pts',(-25.1783490492856,13.6693367218364,
130.770898552611)) ;
#145421 = CARTESIAN_POINT('Ctrl Pts',(-25.1761396925621,13.3586797958361,
130.797580088685)) ;
#145422 = CARTESIAN_POINT('Ctrl Pts',(-25.146968494634,13.0526929008547,130.745494427357)) ;
#145423 = CARTESIAN_POINT('Ctrl Pts',(-25.0921634279591,12.7731727546938,
130.618535460199)) ;
#145424 = CARTESIAN_POINT('Ctrl Pts',(-25.0149917609423,12.5404161552581,
130.426216312955)) ;
#145425 = CARTESIAN_POINT('Ctrl Pts',(-24.9202173073984,12.370760764573,130.182480150042)) ;
#145426 = CARTESIAN_POINT('Ctrl Pts',(-24.813795268409,12.2766729448487,129.904750621267)) ;
#145427 = CARTESIAN_POINT('Ctrl Pts',(-24.7033211856258,12.2643218542415,
129.615000634789)) ;
#145428 = CARTESIAN_POINT('Ctrl Pts',(-24.5940336951667,12.336020687125,129.329153534857)) ;
#145429 = CARTESIAN_POINT('Ctrl Pts',(-24.4961741879793,12.4836397645111,
129.076098411666)) ;
#145430 = CARTESIAN_POINT('Ctrl Pts',(-24.4129309013941,12.7003320009064,
128.866190595829)) ;
#145431 = CARTESIAN_POINT('Ctrl Pts',(-24.3513759196075,12.9678918714247,
128.719449218943)) ;
#145432 = CARTESIAN_POINT('Ctrl Pts',(-24.3144899988947,13.2687870375049,
128.644875989553)) ;
#145433 = CARTESIAN_POINT('Ctrl Pts',(-24.3044879537029,13.5800036106842,
128.648749851774)) ;
#145434 = CARTESIAN_POINT('Ctrl Pts',(-24.3211438511778,13.8799730706512,
128.730495716788)) ;
#145435 = CARTESIAN_POINT('Ctrl Pts',(-24.3626924443883,14.1476994881547,
128.885016926294)) ;
#145436 = CARTESIAN_POINT('Ctrl Pts',(-24.4253103124442,14.3632525192321,
129.101047744803)) ;
#145437 = CARTESIAN_POINT('Ctrl Pts',(-24.5040798325508,14.5119336191473,
129.364360273537)) ;
#145438 = CARTESIAN_POINT('Ctrl Pts',(-24.5924052510114,14.5819602234039,
129.655568908214)) ;
#145439 = CARTESIAN_POINT('Ctrl Pts',(-24.682620944481,14.5692454166129,129.952075493236)) ;
#145440 = CARTESIAN_POINT('Ctrl Pts',(-24.7687439856791,14.4742854326631,
130.236857845916)) ;
#145441 = CARTESIAN_POINT('Ctrl Pts',(-24.8428802815619,14.3047438743695,
130.48644479307)) ;
#145442 = CARTESIAN_POINT('Ctrl Pts',(-24.8997764198948,14.0710830609088,
130.68585734697)) ;
#145443 = CARTESIAN_POINT('Ctrl Pts',(-24.9340655234998,13.7914035953126,
130.819146508686)) ;
#145444 = CARTESIAN_POINT('Ctrl Pts',(-24.9427151855598,13.48501227345,130.877578603568)) ;
#145445 = CARTESIAN_POINT('Ctrl Pts',(-24.9245196442458,13.1755843630713,
130.85743150607)) ;
#145446 = CARTESIAN_POINT('Ctrl Pts',(-24.8798172615573,12.8823157457974,
130.760031273221)) ;
#145447 = CARTESIAN_POINT('Ctrl Pts',(-24.8113548753546,12.6284362839445,
130.593124666697)) ;
#145448 = CARTESIAN_POINT('Ctrl Pts',(-24.7224609989211,12.4304595143626,
130.366773734036)) ;
#145449 = CARTESIAN_POINT('Ctrl Pts',(-24.6207277818397,12.3053999518157,
130.102474981531)) ;
#145450 = CARTESIAN_POINT('Ctrl Pts',(-24.510109071113,12.2593484399968,129.812666622082)) ;
#145451 = CARTESIAN_POINT('Ctrl Pts',(-24.4006135039195,12.2965483921961,
129.52567159029)) ;
#145452 = CARTESIAN_POINT('Ctrl Pts',(-24.2962846439716,12.4156949295869,
129.25430071454)) ;
#145453 = CARTESIAN_POINT('Ctrl Pts',(-24.2068868760499,12.6050470782002,
129.026051488153)) ;
#145454 = CARTESIAN_POINT('Ctrl Pts',(-24.1357528972809,12.85534209768,128.851555978763)) ;
#145455 = CARTESIAN_POINT('Ctrl Pts',(-24.0888790413308,13.1429454569684,
128.747499203338)) ;
#145456 = CARTESIAN_POINT('Ctrl Pts',(-24.0676646556075,13.4543917047447,
128.718846507491)) ;
#145457 = CARTESIAN_POINT('Ctrl Pts',(-24.0737278362457,13.7614620059086,
128.769634834732)) ;
#145458 = CARTESIAN_POINT('Ctrl Pts',(-24.1055487068068,14.0447128346805,
128.895717594865)) ;
#145459 = CARTESIAN_POINT('Ctrl Pts',(-24.1600664153194,14.2828873109444,
129.088022746766)) ;
#145460 = CARTESIAN_POINT('Ctrl Pts',(-24.2328338887739,14.4603132478387,
129.333714872122)) ;
#145461 = CARTESIAN_POINT('Ctrl Pts',(-24.3183681463858,14.5634617520393,
129.61687678413)) ;
#145462 = CARTESIAN_POINT('Ctrl Pts',(-24.4083151971696,14.5844329879889,
129.912552844779)) ;
#145463 = CARTESIAN_POINT('Ctrl Pts',(-24.4973052919974,14.5225343310152,
130.205738265823)) ;
#145464 = CARTESIAN_POINT('Ctrl Pts',(-24.5771666052191,14.381544806336,130.472171976175)) ;
#145465 = CARTESIAN_POINT('Ctrl Pts',(-24.6416003829867,14.1725754677665,
130.693462309482)) ;
#145466 = CARTESIAN_POINT('Ctrl Pts',(-24.6855081480157,13.9093040451571,
130.854881000139)) ;
#145467 = CARTESIAN_POINT('Ctrl Pts',(-24.7048840428278,13.6121558294026,
130.944527353415)) ;
#145468 = CARTESIAN_POINT('Ctrl Pts',(-24.6975117007538,13.2990170967779,
130.956305109112)) ;
#145469 = CARTESIAN_POINT('Ctrl Pts',(-24.6634915622585,12.9981565078101,
130.889864249442)) ;
#145470 = CARTESIAN_POINT('Ctrl Pts',(-24.6042823318373,12.7257032392755,
130.75004731912)) ;
#145471 = CARTESIAN_POINT('Ctrl Pts',(-24.5231278871429,12.50307580565,130.546193334941)) ;
#145472 = CARTESIAN_POINT('Ctrl Pts',(-24.4259349379458,12.3471529691752,
130.295310104727)) ;
#145473 = CARTESIAN_POINT('Ctrl Pts',(-24.317624894329,12.2678408556735,130.012210217516)) ;
#145474 = CARTESIAN_POINT('Ctrl Pts',(-24.2073570412543,12.2715869300384,
129.722982490408)) ;
#145475 = CARTESIAN_POINT('Ctrl Pts',(-24.1000179362842,12.3575776259723,
129.442610247021)) ;
#145476 = CARTESIAN_POINT('Ctrl Pts',(-24.0038553412902,12.5198592417277,
129.194788827538)) ;
#145477 = CARTESIAN_POINT('Ctrl Pts',(-23.9244819040808,12.7472701152985,
128.996100991408)) ;
#145478 = CARTESIAN_POINT('Ctrl Pts',(-23.8672284776034,13.0233715005783,
128.862029320355)) ;
#145479 = CARTESIAN_POINT('Ctrl Pts',(-23.8355017571013,13.3264775703159,
128.80235176831)) ;
#145480 = CARTESIAN_POINT('Ctrl Pts',(-23.8304504639882,13.6374829528976,
128.82070893424)) ;
#145481 = CARTESIAN_POINT('Ctrl Pts',(-23.8520959271135,13.9340523066843,
128.917163045102)) ;
#145482 = CARTESIAN_POINT('Ctrl Pts',(-23.8979574875289,14.1931239778517,
129.084255884832)) ;
#145483 = CARTESIAN_POINT('Ctrl Pts',(-23.9642805338681,14.3974304902421,
129.311214290723)) ;
#145484 = CARTESIAN_POINT('Ctrl Pts',(-24.0448517026705,14.5309245532204,
129.579566049685)) ;
#145485 = CARTESIAN_POINT('Ctrl Pts',(-24.1340072017482,14.5859814539265,
129.873140621991)) ;
#145486 = CARTESIAN_POINT('Ctrl Pts',(-24.2243794169451,14.5574777806989,
130.17028755097)) ;
#145487 = CARTESIAN_POINT('Ctrl Pts',(-24.3086066368753,14.4480150523887,
130.449430915378)) ;
#145488 = CARTESIAN_POINT('Ctrl Pts',(-24.3802849882229,14.2640746902433,
130.692069315547)) ;
#145489 = CARTESIAN_POINT('Ctrl Pts',(-24.4328192725426,14.0222278683344,
130.878454916982)) ;
#145490 = CARTESIAN_POINT('Ctrl Pts',(-24.4627050818997,13.7339092296597,
130.99913076425)) ;
#145491 = CARTESIAN_POINT('Ctrl Pts',(-24.4662080301879,13.4264443376891,
131.042356332604)) ;
#145492 = CARTESIAN_POINT('Ctrl Pts',(-24.4429209579648,13.1179337351116,
131.007422112503)) ;
#145493 = CARTESIAN_POINT('Ctrl Pts',(-24.3935199440539,12.8308236558004,
130.896241586922)) ;
#145494 = CARTESIAN_POINT('Ctrl Pts',(-24.3206916784442,12.5859821192932,
130.716676995717)) ;
#145495 = CARTESIAN_POINT('Ctrl Pts',(-24.2296516192907,12.4020104607834,
130.483717120117)) ;
#145496 = CARTESIAN_POINT('Ctrl Pts',(-24.1247045576579,12.2899875616105,
130.21045036919)) ;
#145497 = CARTESIAN_POINT('Ctrl Pts',(-24.0144718993948,12.260124778228,129.921452283938)) ;
#145498 = CARTESIAN_POINT('Ctrl Pts',(-23.9049499602136,12.3130229090721,
129.634621082704)) ;
#145499 = CARTESIAN_POINT('Ctrl Pts',(-23.8034612745574,12.445755568189,129.371289868144)) ;
#145500 = CARTESIAN_POINT('Ctrl Pts',(-23.716785016583,12.6478749143986,129.151150857304)) ;
#145501 = CARTESIAN_POINT('Ctrl Pts',(-23.6498368401481,12.9074235529971,
128.988879427975)) ;
#145502 = CARTESIAN_POINT('Ctrl Pts',(-23.6076171016782,13.201587990353,128.898548838853)) ;
#145503 = CARTESIAN_POINT('Ctrl Pts',(-23.5916652550101,13.5132462797945,
128.885148066507)) ;
#145504 = CARTESIAN_POINT('Ctrl Pts',(-23.6026899469641,13.8170405083281,
128.950393841574)) ;
#145505 = CARTESIAN_POINT('Ctrl Pts',(-23.6390022908284,14.0930904717493,
129.089554598804)) ;
#145506 = CARTESIAN_POINT('Ctrl Pts',(-23.6974288966858,14.3215765569393,
129.293356920021)) ;
#145507 = CARTESIAN_POINT('Ctrl Pts',(-23.7732783266701,14.4860164684736,
129.548154125562)) ;
#145508 = CARTESIAN_POINT('Ctrl Pts',(-23.8599542560027,14.5737422146348,
129.834485864806)) ;
#145509 = CARTESIAN_POINT('Ctrl Pts',(-23.9507422758738,14.5789283273619,
130.13285405137)) ;
#145510 = CARTESIAN_POINT('Ctrl Pts',(-24.0380468092121,14.5018179973275,
130.420910654275)) ;
#145511 = CARTESIAN_POINT('Ctrl Pts',(-24.1157083841933,14.3465570817491,
130.68101922773)) ;
#145512 = CARTESIAN_POINT('Ctrl Pts',(-24.176387817006,14.1268974135735,130.891224248633)) ;
#145513 = CARTESIAN_POINT('Ctrl Pts',(-24.2160535934832,13.8551171351805,
131.04031438907)) ;
#145514 = CARTESIAN_POINT('Ctrl Pts',(-24.2304468988952,13.5530512913373,
131.115473299743)) ;
#145515 = CARTESIAN_POINT('Ctrl Pts',(-24.2180467938604,13.2415863722887,
131.112379553594)) ;
#145516 = CARTESIAN_POINT('Ctrl Pts',(-24.1789708219546,12.9431696446184,
131.031350828024)) ;
#145517 = CARTESIAN_POINT('Ctrl Pts',(-24.1152480411839,12.6789855652346,
130.878343326519)) ;
#145518 = CARTESIAN_POINT('Ctrl Pts',(-24.0308870684906,12.4685393411929,
130.664990318022)) ;
#145519 = CARTESIAN_POINT('Ctrl Pts',(-23.9312079738808,12.3261974567536,
130.406868087954)) ;
#145520 = CARTESIAN_POINT('Ctrl Pts',(-23.8218914930888,12.2622045863294,
130.12077781006)) ;
#145521 = CARTESIAN_POINT('Ctrl Pts',(-23.711473023475,12.2815898353466,129.831214120587)) ;
#145522 = CARTESIAN_POINT('Ctrl Pts',(-23.605830521001,12.3824517800912,129.55574064071)) ;
#145523 = CARTESIAN_POINT('Ctrl Pts',(-23.5121833804525,12.5585397023802,
129.31536727562)) ;
#145524 = CARTESIAN_POINT('Ctrl Pts',(-23.4369153209714,12.7954955062998,
129.128535047897)) ;
#145525 = CARTESIAN_POINT('Ctrl Pts',(-23.3840187660153,13.0796940190917,
129.007326938172)) ;
#145526 = CARTESIAN_POINT('Ctrl Pts',(-23.3573639658812,13.3852304458179,
128.962397177592)) ;
#145527 = CARTESIAN_POINT('Ctrl Pts',(-23.3574546179297,13.69604445911,128.995889251632)) ;
#145528 = CARTESIAN_POINT('Ctrl Pts',(-23.3838342563352,13.985866733445,129.106013284641)) ;
#145529 = CARTESIAN_POINT('Ctrl Pts',(-23.4338358205724,14.2358877356182,
129.285204766825)) ;
#145530 = CARTESIAN_POINT('Ctrl Pts',(-23.5030215875279,14.4275999337175,
129.520381613063)) ;
#145531 = CARTESIAN_POINT('Ctrl Pts',(-23.586530885337,14.5480862858471,129.79766767603)) ;
#145532 = CARTESIAN_POINT('Ctrl Pts',(-23.6761347345792,14.5868446718797,
130.092418722233)) ;
#145533 = CARTESIAN_POINT('Ctrl Pts',(-23.7656887691914,14.5430357670067,
130.387091618743)) ;
#145534 = CARTESIAN_POINT('Ctrl Pts',(-23.8481253493012,14.41874401797,130.66105949148)) ;
#145535 = CARTESIAN_POINT('Ctrl Pts',(-23.9165563901983,14.2230681528207,
130.894108221658)) ;
#145536 = CARTESIAN_POINT('Ctrl Pts',(-23.9653333847544,13.9697197453762,
131.069771337352)) ;
#145537 = CARTESIAN_POINT('Ctrl Pts',(-23.990200337815,13.6787523324498,131.175414444762)) ;
#145538 = CARTESIAN_POINT('Ctrl Pts',(-23.9887937953144,13.3668522755562,
131.204597590958)) ;
#145539 = CARTESIAN_POINT('Ctrl Pts',(-23.9602778328738,13.060672465625,131.154404872108)) ;
#145540 = CARTESIAN_POINT('Ctrl Pts',(-23.9063786521122,12.7810810976344,
131.029975165967)) ;
#145541 = CARTESIAN_POINT('Ctrl Pts',(-23.8298459002734,12.5467077229853,
130.839515925952)) ;
#145542 = CARTESIAN_POINT('Ctrl Pts',(-23.7357096542374,12.375036029875,130.597588581862)) ;
#145543 = CARTESIAN_POINT('Ctrl Pts',(-23.6289012337717,12.2779852364334,
130.318926820808)) ;
#145544 = CARTESIAN_POINT('Ctrl Pts',(-23.5186091664602,12.263745955446,130.029664056281)) ;
#145545 = CARTESIAN_POINT('Ctrl Pts',(-23.409859192313,12.3321871906188,129.745159691814)) ;
#145546 = CARTESIAN_POINT('Ctrl Pts',(-23.3107503409185,12.4786900321498,
129.488734825247)) ;
#145547 = CARTESIAN_POINT('Ctrl Pts',(-23.2270427134099,12.6941599570478,
129.277486374064)) ;
#145548 = CARTESIAN_POINT('Ctrl Pts',(-23.1650738676188,12.9594898311094,
129.129411454435)) ;
#145549 = CARTESIAN_POINT('Ctrl Pts',(-23.127402651992,13.2597802878034,129.052552004075)) ;
#145550 = CARTESIAN_POINT('Ctrl Pts',(-23.1166171147694,13.5705933911082,
129.054095550851)) ;
#145551 = CARTESIAN_POINT('Ctrl Pts',(-23.1324759418215,13.8717555022921,
129.133564743532)) ;
#145552 = CARTESIAN_POINT('Ctrl Pts',(-23.1736382839865,14.1416796956212,
129.287104278442)) ;
#145553 = CARTESIAN_POINT('Ctrl Pts',(-23.2353487963013,14.3575208853318,
129.500272865785)) ;
#145554 = CARTESIAN_POINT('Ctrl Pts',(-23.3139533929537,14.5088742851846,
129.763207569102)) ;
#145555 = CARTESIAN_POINT('Ctrl Pts',(-23.4019083074391,14.5810485932283,
130.05325347066)) ;
#145556 = CARTESIAN_POINT('Ctrl Pts',(-23.4922878921798,14.5707018107426,
130.350295811704)) ;
#145557 = CARTESIAN_POINT('Ctrl Pts',(-23.5783948195674,14.4785662345022,
130.634919109524)) ;
#145558 = CARTESIAN_POINT('Ctrl Pts',(-23.6535576314426,14.3096045878152,
130.887780129686)) ;
#145559 = CARTESIAN_POINT('Ctrl Pts',(-23.7107444191254,14.0777449679159,
131.087951985329)) ;
#145560 = CARTESIAN_POINT('Ctrl Pts',(-23.7455948140687,13.8001341455209,
131.222767295429)) ;
#145561 = CARTESIAN_POINT('Ctrl Pts',(-23.7550892236747,13.4946152703642,
131.283624171076)) ;
#145562 = CARTESIAN_POINT('Ctrl Pts',(-23.7375695842205,13.1837406589244,
131.265591449185)) ;
#145563 = CARTESIAN_POINT('Ctrl Pts',(-23.6936762044173,12.8901082273082,
131.170493042617)) ;
#145564 = CARTESIAN_POINT('Ctrl Pts',(-23.625357982327,12.6339160706406,131.004184247701)) ;
#145565 = CARTESIAN_POINT('Ctrl Pts',(-23.5382570077213,12.4365925645623,
130.782597137202)) ;
#145566 = CARTESIAN_POINT('Ctrl Pts',(-23.4356867081835,12.3075969590058,
130.516253879618)) ;
#145567 = CARTESIAN_POINT('Ctrl Pts',(-23.3261678971312,12.2595413699531,
130.229346863333)) ;
#145568 = CARTESIAN_POINT('Ctrl Pts',(-23.2155616867436,12.2945981250866,
129.939427931191)) ;
#145569 = CARTESIAN_POINT('Ctrl Pts',(-23.112025204016,12.4101972577176,129.670008473014)) ;
#145570 = CARTESIAN_POINT('Ctrl Pts',(-23.0214087797488,12.598715944425,129.438457570237)) ;
#145571 = CARTESIAN_POINT('Ctrl Pts',(-22.9499549148632,12.8461743706132,
129.262846208528)) ;
#145572 = CARTESIAN_POINT('Ctrl Pts',(-22.9018759435203,13.1359262374288,
129.155624903807)) ;
#145573 = CARTESIAN_POINT('Ctrl Pts',(-22.8801611636247,13.4447581529336,
129.125245563724)) ;
#145574 = CARTESIAN_POINT('Ctrl Pts',(-22.8854063684676,13.7530929209566,
129.17374638537)) ;
#145575 = CARTESIAN_POINT('Ctrl Pts',(-22.916384591562,14.0362080508941,129.297229526547)) ;
#145576 = CARTESIAN_POINT('Ctrl Pts',(-22.9704084490522,14.2769560090218,
129.488206755545)) ;
#145577 = CARTESIAN_POINT('Ctrl Pts',(-23.0429220897085,14.4563581984587,
129.733214662571)) ;
#145578 = CARTESIAN_POINT('Ctrl Pts',(-23.1276158497506,14.5613193565883,
130.013704430188)) ;
#145579 = CARTESIAN_POINT('Ctrl Pts',(-23.2181078723221,14.5851466740993,
130.311194154607)) ;
#145580 = CARTESIAN_POINT('Ctrl Pts',(-23.3072958781627,14.5250094201889,
130.604988309245)) ;
#145581 = CARTESIAN_POINT('Ctrl Pts',(-23.3870877454623,14.3871118872338,
130.87103110078)) ;
#145582 = CARTESIAN_POINT('Ctrl Pts',(-23.4523914097116,14.1786613146333,
131.095060551793)) ;
#145583 = CARTESIAN_POINT('Ctrl Pts',(-23.4967311352243,13.9181921404444,
131.25754465457)) ;
#145584 = CARTESIAN_POINT('Ctrl Pts',(-23.5169519482374,13.6189922621126,
131.349968979705)) ;
#145585 = CARTESIAN_POINT('Ctrl Pts',(-23.5103363565515,13.3089360963624,
131.363628705452)) ;
#145586 = CARTESIAN_POINT('Ctrl Pts',(-23.4770069966206,13.0058324971489,
131.29938668452)) ;
#145587 = CARTESIAN_POINT('Ctrl Pts',(-23.4182183181683,12.7318651916952,
131.160863065766)) ;
#145588 = CARTESIAN_POINT('Ctrl Pts',(-23.3377159966076,12.5082426234418,
130.958847305866)) ;
#145589 = CARTESIAN_POINT('Ctrl Pts',(-23.2412362943228,12.3508732167538,
130.709935987911)) ;
#145590 = CARTESIAN_POINT('Ctrl Pts',(-23.1334938059766,12.2691036353101,
130.428391186563)) ;
#145591 = CARTESIAN_POINT('Ctrl Pts',(-23.0226736892661,12.2702137418504,
130.137711873116)) ;
#145592 = CARTESIAN_POINT('Ctrl Pts',(-22.9149840860042,12.3542930287051,
129.856364718422)) ;
#145593 = CARTESIAN_POINT('Ctrl Pts',(-22.8187097041837,12.5141177100409,
129.608122057843)) ;
#145594 = CARTESIAN_POINT('Ctrl Pts',(-22.7388237334191,12.7395234896818,
129.407902601402)) ;
#145595 = CARTESIAN_POINT('Ctrl Pts',(-22.6808402251335,13.0142280160873,
129.271679110281)) ;
#145596 = CARTESIAN_POINT('Ctrl Pts',(-22.6482265628477,13.3177663479764,
129.209516170382)) ;
#145597 = CARTESIAN_POINT('Ctrl Pts',(-22.6424590310294,13.6286638171374,
129.22575901871)) ;
#145598 = CARTESIAN_POINT('Ctrl Pts',(-22.6632532943469,13.925291931835,129.319642589528)) ;
#145599 = CARTESIAN_POINT('Ctrl Pts',(-22.7085000580716,14.1860950196788,
129.484987285644)) ;
#145600 = CARTESIAN_POINT('Ctrl Pts',(-22.7740352615984,14.3917324528471,
129.709531790955)) ;
#145601 = CARTESIAN_POINT('Ctrl Pts',(-22.8545854265937,14.5282787585867,
129.977970770821)) ;
#145602 = CARTESIAN_POINT('Ctrl Pts',(-22.9437848131845,14.585553871015,130.271733891018)) ;
#145603 = CARTESIAN_POINT('Ctrl Pts',(-23.0339617592761,14.5594424124574,
130.568216361715)) ;
#145604 = CARTESIAN_POINT('Ctrl Pts',(-23.1183884658679,14.452533822029,130.847908451577)) ;
#145605 = CARTESIAN_POINT('Ctrl Pts',(-23.1906734144242,14.2704301815678,
131.092366276915)) ;
#145606 = CARTESIAN_POINT('Ctrl Pts',(-23.2438547431658,14.0294404722423,
131.280712615189)) ;
#145607 = CARTESIAN_POINT('Ctrl Pts',(-23.2743339500446,13.7439522492757,
131.402912133382)) ;
#145608 = CARTESIAN_POINT('Ctrl Pts',(-23.2787167666675,13.4354033023599,
131.448870145367)) ;
#145609 = CARTESIAN_POINT('Ctrl Pts',(-23.2562246361759,13.1268757917154,
131.416219286457)) ;
#145610 = CARTESIAN_POINT('Ctrl Pts',(-23.2073574714543,12.8380942366352,
131.306698786949)) ;
#145611 = CARTESIAN_POINT('Ctrl Pts',(-23.1355944667206,12.5930207366324,
131.130053443896)) ;
#145612 = CARTESIAN_POINT('Ctrl Pts',(-23.0444638356501,12.406038861412,130.897036568901)) ;
#145613 = CARTESIAN_POINT('Ctrl Pts',(-22.9406787300405,12.292531234905,130.626882995043)) ;
#145614 = CARTESIAN_POINT('Ctrl Pts',(-22.8296117127798,12.259700175239,130.335730540699)) ;
#145615 = CARTESIAN_POINT('Ctrl Pts',(-22.7202029855353,12.3104428593725,
130.049154559549)) ;
#145616 = CARTESIAN_POINT('Ctrl Pts',(-22.6182810864586,12.4411375655696,
129.784596789139)) ;
#145617 = CARTESIAN_POINT('Ctrl Pts',(-22.5313208064023,12.6410412802729,
129.563551254626)) ;
#145618 = CARTESIAN_POINT('Ctrl Pts',(-22.4636797384928,12.8990710258353,
129.399250646078)) ;
#145619 = CARTESIAN_POINT('Ctrl Pts',(-22.4206465720963,13.1932159520557,
129.306625587208)) ;
#145620 = CARTESIAN_POINT('Ctrl Pts',(-22.4039742026336,13.5039484440362,
129.291035546014)) ;
#145621 = CARTESIAN_POINT('Ctrl Pts',(-22.4142047859484,13.8084630693567,
129.353985219695)) ;
#145622 = CARTESIAN_POINT('Ctrl Pts',(-22.4498225285243,14.0856215831729,
129.491114851947)) ;
#145623 = CARTESIAN_POINT('Ctrl Pts',(-22.507670146175,14.3156974837171,129.693224338099)) ;
#145624 = CARTESIAN_POINT('Ctrl Pts',(-22.5829454215261,14.482069329469,129.946284653554)) ;
#145625 = CARTESIAN_POINT('Ctrl Pts',(-22.6695641165245,14.5722583544091,
130.232518171332)) ;
#145626 = CARTESIAN_POINT('Ctrl Pts',(-22.7598804555675,14.5801736799871,
130.529336653199)) ;
#145627 = CARTESIAN_POINT('Ctrl Pts',(-22.8480258383558,14.5050113517495,
130.820095830851)) ;
#145628 = CARTESIAN_POINT('Ctrl Pts',(-22.9257917436902,14.3522164750112,
131.080392384164)) ;
#145629 = CARTESIAN_POINT('Ctrl Pts',(-22.987136965067,14.1339602612738,131.292602674308)) ;
#145630 = CARTESIAN_POINT('Ctrl Pts',(-23.0274074755232,13.8641112712326,
131.443370465904)) ;
#145631 = CARTESIAN_POINT('Ctrl Pts',(-23.0426371790203,13.5616225014003,
131.521090320168)) ;
#145632 = CARTESIAN_POINT('Ctrl Pts',(-23.0309825577039,13.2502934236062,
131.520151201035)) ;
#145633 = CARTESIAN_POINT('Ctrl Pts',(-22.9925814825968,12.9509782560257,
131.441125269672)) ;
#145634 = CARTESIAN_POINT('Ctrl Pts',(-22.9297334436235,12.6863948819192,
131.290563314743)) ;
#145635 = CARTESIAN_POINT('Ctrl Pts',(-22.8457402853658,12.4734606146631,
131.078368259428)) ;
#145636 = CARTESIAN_POINT('Ctrl Pts',(-22.7459623009365,12.3287823734524,
130.820088867329)) ;
#145637 = CARTESIAN_POINT('Ctrl Pts',(-22.6373365168631,12.262963408062,130.535850196423)) ;
#145638 = CARTESIAN_POINT('Ctrl Pts',(-22.5266895904036,12.2798963364109,
130.245676252651)) ;
#145639 = CARTESIAN_POINT('Ctrl Pts',(-22.4207454828677,12.3786944152069,
129.96934005118)) ;
#145640 = CARTESIAN_POINT('Ctrl Pts',(-22.3265704318192,12.5532637477409,
129.727473762186)) ;
#145641 = CARTESIAN_POINT('Ctrl Pts',(-22.2510778917587,12.7879392173085,
129.539860818582)) ;
#145642 = CARTESIAN_POINT('Ctrl Pts',(-22.1975992748365,13.0695371613245,
129.416790381634)) ;
#145643 = CARTESIAN_POINT('Ctrl Pts',(-22.1699284873186,13.3764287313842,
129.369087812723)) ;
#145644 = CARTESIAN_POINT('Ctrl Pts',(-22.1693136310075,13.6873693944069,
129.400507755856)) ;
#145645 = CARTESIAN_POINT('Ctrl Pts',(-22.1949149197245,13.9780097537181,
129.508346847974)) ;
#145646 = CARTESIAN_POINT('Ctrl Pts',(-22.2445624596995,14.2303816916052,
129.686644518596)) ;
#145647 = CARTESIAN_POINT('Ctrl Pts',(-22.3130761042801,14.4229832275646,
129.919733582549)) ;
#145648 = CARTESIAN_POINT('Ctrl Pts',(-22.3960662366792,14.545607197334,130.195429870093)) ;
#145649 = CARTESIAN_POINT('Ctrl Pts',(-22.4857299738979,14.5869244372964,
130.490415745043)) ;
#145650 = CARTESIAN_POINT('Ctrl Pts',(-22.575453626079,14.545413999477,130.785606108546)) ;
#145651 = CARTESIAN_POINT('Ctrl Pts',(-22.6582120497049,14.4231615318539,
131.060527548057)) ;
#145652 = CARTESIAN_POINT('Ctrl Pts',(-22.7269164368304,14.2299646003197,
131.294274065008)) ;
#145653 = CARTESIAN_POINT('Ctrl Pts',(-22.7764175593052,13.9782380349311,
131.47205027609)) ;
#145654 = CARTESIAN_POINT('Ctrl Pts',(-22.8020622548463,13.6869896701315,
131.58008886622)) ;
#145655 = CARTESIAN_POINT('Ctrl Pts',(-22.8014560080435,13.3772462280803,
131.611403153323)) ;
#145656 = CARTESIAN_POINT('Ctrl Pts',(-22.7738460874784,13.0701026348063,
131.563905722585)) ;
#145657 = CARTESIAN_POINT('Ctrl Pts',(-22.7204413399783,12.7883757721948,
131.441047603048)) ;
#145658 = CARTESIAN_POINT('Ctrl Pts',(-22.6444900848234,12.5524788061311,
131.252281571094)) ;
#145659 = CARTESIAN_POINT('Ctrl Pts',(-22.5505848182462,12.3787205922408,
131.011087248236)) ;
#145660 = CARTESIAN_POINT('Ctrl Pts',(-22.4446658828603,12.2799428361804,
130.734823347179)) ;
#145661 = CARTESIAN_POINT('Ctrl Pts',(-22.3341711628268,12.26278144672,130.445043220403)) ;
#145662 = CARTESIAN_POINT('Ctrl Pts',(-22.2246631880983,12.3295044441556,
130.158507007516)) ;
#145663 = CARTESIAN_POINT('Ctrl Pts',(-22.1257254050998,12.4735104762095,
129.902424684196)) ;
#145664 = CARTESIAN_POINT('Ctrl Pts',(-22.0417569838295,12.6859036202202,
129.690264837747)) ;
#145665 = CARTESIAN_POINT('Ctrl Pts',(-21.9787385701834,12.9511128750471,
129.539283902845)) ;
#145666 = CARTESIAN_POINT('Ctrl Pts',(-21.9403107768235,13.2510042881428,
129.460237929327)) ;
#145667 = CARTESIAN_POINT('Ctrl Pts',(-21.9287596101754,13.5624349033162,
129.459612610358)) ;
#145668 = CARTESIAN_POINT('Ctrl Pts',(-21.9439314898076,13.8634351893562,
129.537002871099)) ;
#145669 = CARTESIAN_POINT('Ctrl Pts',(-21.9840596405432,14.1332614315187,
129.687330392558)) ;
#145670 = CARTESIAN_POINT('Ctrl Pts',(-22.0456493591576,14.3526410215066,
129.900400764091)) ;
#145671 = CARTESIAN_POINT('Ctrl Pts',(-22.1237356790095,14.5054039917793,
130.161735495758)) ;
#145672 = CARTESIAN_POINT('Ctrl Pts',(-22.2111275537692,14.5799567731311,
130.450008897407)) ;
#145673 = CARTESIAN_POINT('Ctrl Pts',(-22.3018824052644,14.572371407252,130.74826980151)) ;
#145674 = CARTESIAN_POINT('Ctrl Pts',(-22.3885019784228,14.4818104179813,
131.034516812178)) ;
#145675 = CARTESIAN_POINT('Ctrl Pts',(-22.4634673589328,14.3163442533983,
131.286522423217)) ;
#145676 = CARTESIAN_POINT('Ctrl Pts',(-22.5214998076607,14.0859120132609,
131.489249238818)) ;
#145677 = CARTESIAN_POINT('Ctrl Pts',(-22.5571587027642,13.8088757639041,
131.62648715997)) ;
#145678 = CARTESIAN_POINT('Ctrl Pts',(-22.5673836208744,13.5028415696086,
131.68958577917)) ;
#145679 = CARTESIAN_POINT('Ctrl Pts',(-22.5507152273552,13.1931030740132,
131.673896265537)) ;
#145680 = CARTESIAN_POINT('Ctrl Pts',(-22.5074512192622,12.8979592088334,
131.58072405734)) ;
#145681 = CARTESIAN_POINT('Ctrl Pts',(-22.4401878872421,12.6415806575113,
131.417320263901)) ;
#145682 = CARTESIAN_POINT('Ctrl Pts',(-22.3529978608748,12.4408172036161,
131.195714780762)) ;
#145683 = CARTESIAN_POINT('Ctrl Pts',(-22.2507185667645,12.3100401552364,
130.930208877523)) ;
#145684 = CARTESIAN_POINT('Ctrl Pts',(-22.1415541397393,12.2598615756175,
130.644270647017)) ;
#145685 = CARTESIAN_POINT('Ctrl Pts',(-22.0311013361464,12.2922205464447,
130.354723425766)) ;
#145686 = CARTESIAN_POINT('Ctrl Pts',(-21.9267303945298,12.40624849515,130.083044294425)) ;
#145687 = CARTESIAN_POINT('Ctrl Pts',(-21.8359058461118,12.5927140641391,
129.850810997993)) ;
#145688 = CARTESIAN_POINT('Ctrl Pts',(-21.7640101840432,12.8381488954601,
129.673838643522)) ;
#145689 = CARTESIAN_POINT('Ctrl Pts',(-21.7152207007081,13.1260095358548,
129.564442600056)) ;
#145690 = CARTESIAN_POINT('Ctrl Pts',(-21.6925855604333,13.4367097241923,
129.531608400982)) ;
#145691 = CARTESIAN_POINT('Ctrl Pts',(-21.6970872221281,13.7438376773702,
129.577766848317)) ;
#145692 = CARTESIAN_POINT('Ctrl Pts',(-21.7273689275802,14.0287736558089,
129.699306891545)) ;
#145693 = CARTESIAN_POINT('Ctrl Pts',(-21.7808528667027,14.2709621799374,
129.888711102644)) ;
#145694 = CARTESIAN_POINT('Ctrl Pts',(-21.8527753379124,14.4520608011874,
130.131934341161)) ;
#145695 = CARTESIAN_POINT('Ctrl Pts',(-21.937338148521,14.5594794464979,130.412094195668)) ;
#145696 = CARTESIAN_POINT('Ctrl Pts',(-22.0275873885439,14.5855261750269,
130.708811093224)) ;
#145697 = CARTESIAN_POINT('Ctrl Pts',(-22.1167126461185,14.5283738687936,
131.002328490394)) ;
#145698 = CARTESIAN_POINT('Ctrl Pts',(-22.1973624162769,14.3916536122689,
131.271100689726)) ;
#145699 = CARTESIAN_POINT('Ctrl Pts',(-22.2627919222655,14.1863632945959,
131.495280692911)) ;
#145700 = CARTESIAN_POINT('Ctrl Pts',(-22.3080735207915,13.9255968041967,
131.660732394034)) ;
#145701 = CARTESIAN_POINT('Ctrl Pts',(-22.3288933669282,13.6292800303555,
131.754659669598)) ;
#145702 = CARTESIAN_POINT('Ctrl Pts',(-22.3231642846892,13.3179689166563,
131.771059850504)) ;
#145703 = CARTESIAN_POINT('Ctrl Pts',(-22.2905466843428,13.0144328238462,
131.70888463353)) ;
#145704 = CARTESIAN_POINT('Ctrl Pts',(-22.232699413988,12.7401667038842,131.573002097289)) ;
#145705 = CARTESIAN_POINT('Ctrl Pts',(-22.1528576217879,12.5144106692782,
131.37292430167)) ;
#145706 = CARTESIAN_POINT('Ctrl Pts',(-22.0561564026532,12.3540784251448,
131.123573481352)) ;
#145707 = CARTESIAN_POINT('Ctrl Pts',(-21.9491234057288,12.2704506674806,
130.843940985009)) ;
#145708 = CARTESIAN_POINT('Ctrl Pts',(-21.8379492349739,12.2689821034606,
130.552336500549)) ;
#145709 = CARTESIAN_POINT('Ctrl Pts',(-21.7301340097967,12.350850990926,130.270599037869)) ;
#145710 = CARTESIAN_POINT('Ctrl Pts',(-21.6334302854589,12.5086055972373,
130.02111108677)) ;
#145711 = CARTESIAN_POINT('Ctrl Pts',(-21.5528038582257,12.7330677829212,
129.818816445627)) ;
#145712 = CARTESIAN_POINT('Ctrl Pts',(-21.4942939691824,13.0066124889692,
129.68103187895)) ;
#145713 = CARTESIAN_POINT('Ctrl Pts',(-21.4610544217535,13.308272601369,129.616896850597)) ;
#145714 = CARTESIAN_POINT('Ctrl Pts',(-21.4544299431771,13.6201713325224,
129.630731872719)) ;
#145715 = CARTESIAN_POINT('Ctrl Pts',(-21.474644249058,13.9183341039009,129.72301929693)) ;
#145716 = CARTESIAN_POINT('Ctrl Pts',(-21.5192529028078,14.1797388278147,
129.886437479066)) ;
#145717 = CARTESIAN_POINT('Ctrl Pts',(-21.5840569958028,14.3864987369051,
130.108738684431)) ;
#145718 = CARTESIAN_POINT('Ctrl Pts',(-21.6642121862485,14.5252641755352,
130.376013710086)) ;
#145719 = CARTESIAN_POINT('Ctrl Pts',(-21.7532842228128,14.5851721038055,
130.669413027174)) ;
#145720 = CARTESIAN_POINT('Ctrl Pts',(-21.8440338817864,14.5610669162746,
130.967758566311)) ;
#145721 = CARTESIAN_POINT('Ctrl Pts',(-21.9282251617535,14.4566509798001,
131.246584092179)) ;
#145722 = CARTESIAN_POINT('Ctrl Pts',(-22.0009339264215,14.2771545198569,
131.492228959747)) ;
#145723 = CARTESIAN_POINT('Ctrl Pts',(-22.0549712796414,14.0362065305465,
131.683263448546)) ;
#145724 = CARTESIAN_POINT('Ctrl Pts',(-22.0859468214144,13.753398715095,131.806709045245)) ;
#145725 = CARTESIAN_POINT('Ctrl Pts',(-22.0912337993049,13.4441283585126,
131.855429678035)) ;
#145726 = CARTESIAN_POINT('Ctrl Pts',(-22.0692970894306,13.1346408966579,
131.824482173486)) ;
#145727 = CARTESIAN_POINT('Ctrl Pts',(-22.0215845589901,12.8470251737848,
131.718082264569)) ;
#145728 = CARTESIAN_POINT('Ctrl Pts',(-21.9498823449809,12.5984937869307,
131.541883011935)) ;
#145729 = CARTESIAN_POINT('Ctrl Pts',(-21.859706635381,12.4108688278635,131.311455950053)) ;
#145730 = CARTESIAN_POINT('Ctrl Pts',(-21.7559998278931,12.2946081096869,
131.041613650211)) ;
#145731 = CARTESIAN_POINT('Ctrl Pts',(-21.6449281923886,12.2594450533974,
130.750468031976)) ;
#145732 = CARTESIAN_POINT('Ctrl Pts',(-21.5353149765672,12.30804814686,130.463325529376)) ;
#145733 = CARTESIAN_POINT('Ctrl Pts',(-21.433409422968,12.4360760991486,130.198700529688)) ;
#145734 = CARTESIAN_POINT('Ctrl Pts',(-21.3457569994458,12.634525822386,129.975706345904)) ;
#145735 = CARTESIAN_POINT('Ctrl Pts',(-21.2777014430076,12.8902137015407,
129.810072152823)) ;
#145736 = CARTESIAN_POINT('Ctrl Pts',(-21.2338043784698,13.1836915440523,
129.714952668352)) ;
#145737 = CARTESIAN_POINT('Ctrl Pts',(-21.2162760126707,13.4943234250401,
129.69686779882)) ;
#145738 = CARTESIAN_POINT('Ctrl Pts',(-21.2257767207619,13.8008444914087,
129.757847499092)) ;
#145739 = CARTESIAN_POINT('Ctrl Pts',(-21.260918305411,14.0793170573489,129.893644297111)) ;
#145740 = CARTESIAN_POINT('Ctrl Pts',(-21.3179351568953,14.3098745304063,
130.093168310721)) ;
#145741 = CARTESIAN_POINT('Ctrl Pts',(-21.393135043171,14.4788324739109,130.346151975855)) ;
#145742 = CARTESIAN_POINT('Ctrl Pts',(-21.4791104654225,14.5706780118123,
130.630335180623)) ;
#145743 = CARTESIAN_POINT('Ctrl Pts',(-21.569587551734,14.5811216563982,130.92769514245)) ;
#145744 = CARTESIAN_POINT('Ctrl Pts',(-21.6577489493399,14.5082991498853,
131.218439893283)) ;
#145745 = CARTESIAN_POINT('Ctrl Pts',(-21.7358456781333,14.3580057871193,
131.479665882624)) ;
#145746 = CARTESIAN_POINT('Ctrl Pts',(-21.798001885849,14.1405256903455,131.694385206399)) ;
#145747 = CARTESIAN_POINT('Ctrl Pts',(-21.8387940212521,13.8719961113424,
131.846641739039)) ;
#145748 = CARTESIAN_POINT('Ctrl Pts',(-21.8547791588512,13.5716289607196,
131.926408611645)) ;
#145749 = CARTESIAN_POINT('Ctrl Pts',(-21.8439115520657,13.2591262832754,
131.927893832288)) ;
#145750 = CARTESIAN_POINT('Ctrl Pts',(-21.8063818672718,12.9599151059205,
131.851322214392)) ;
#145751 = CARTESIAN_POINT('Ctrl Pts',(-21.7440145809282,12.6930800437845,
131.702283019861)) ;
#145752 = CARTESIAN_POINT('Ctrl Pts',(-21.660626104627,12.4788237616548,131.491808094147)) ;
#145753 = CARTESIAN_POINT('Ctrl Pts',(-21.5615327330444,12.332247898292,131.235434874409)) ;
#145754 = CARTESIAN_POINT('Ctrl Pts',(-21.4529505571654,12.2636849567094,
130.951367917164)) ;
#145755 = CARTESIAN_POINT('Ctrl Pts',(-21.3419633703332,12.2782423804387,
130.660286988405)) ;
#145756 = CARTESIAN_POINT('Ctrl Pts',(-21.2358893379918,12.3748788763276,
130.383546024411)) ;
#145757 = CARTESIAN_POINT('Ctrl Pts',(-21.141622326909,12.5463735135204,130.141264334557)) ;
#145758 = CARTESIAN_POINT('Ctrl Pts',(-21.0649842164547,12.7810696956234,
129.950540111674)) ;
#145759 = CARTESIAN_POINT('Ctrl Pts',(-21.0110514658407,13.0608633683861,
129.82603487308)) ;
#145760 = CARTESIAN_POINT('Ctrl Pts',(-20.9825739767851,13.3671883117348,
129.775968871056)) ;
#145761 = CARTESIAN_POINT('Ctrl Pts',(-20.9811465718423,13.6783221132163,
129.805007108354)) ;
#145762 = CARTESIAN_POINT('Ctrl Pts',(-21.0060732680338,13.9701100820096,
129.910918322944)) ;
#145763 = CARTESIAN_POINT('Ctrl Pts',(-21.0548192698872,14.2230345342298,
130.086443323896)) ;
#145764 = CARTESIAN_POINT('Ctrl Pts',(-21.1231998537938,14.4186168912711,
130.319327093341)) ;
#145765 = CARTESIAN_POINT('Ctrl Pts',(-21.2055023955591,14.5428705870382,
130.592855887077)) ;
#145766 = CARTESIAN_POINT('Ctrl Pts',(-21.2952349104155,14.5869069845901,
130.888119007957)) ;
#145767 = CARTESIAN_POINT('Ctrl Pts',(-21.3849839588049,14.5480013185182,
131.183345676982)) ;
#145768 = CARTESIAN_POINT('Ctrl Pts',(-21.4685154515025,14.4271740783889,
131.460720849614)) ;
#145769 = CARTESIAN_POINT('Ctrl Pts',(-21.5373912518205,14.2362638793065,
131.694850358935)) ;
#145770 = CARTESIAN_POINT('Ctrl Pts',(-21.5875113438075,13.9863048350813,
131.874404129707)) ;
#145771 = CARTESIAN_POINT('Ctrl Pts',(-21.6138800887913,13.6957298115947,
131.984578993146)) ;
#145772 = CARTESIAN_POINT('Ctrl Pts',(-21.614125788485,13.3866515588876,132.018333297806)) ;
#145773 = CARTESIAN_POINT('Ctrl Pts',(-21.5870104977058,13.0771469470951,
131.972501741679)) ;
#145774 = CARTESIAN_POINT('Ctrl Pts',(-21.5346173255377,12.7963920748989,
131.852368075822)) ;
#145775 = CARTESIAN_POINT('Ctrl Pts',(-21.4589507416269,12.5578779077828,
131.664580333898)) ;
#145776 = CARTESIAN_POINT('Ctrl Pts',(-21.3658400631902,12.3830735450268,
131.425564438929)) ;
#145777 = CARTESIAN_POINT('Ctrl Pts',(-21.2601690090166,12.2815115080033,
131.150038104503)) ;
#145778 = CARTESIAN_POINT('Ctrl Pts',(-21.1489223139169,12.262368243914,130.858300208979)) ;
#145779 = CARTESIAN_POINT('Ctrl Pts',(-21.0406225843969,12.3259184462842,
130.574873351895)) ;
#145780 = CARTESIAN_POINT('Ctrl Pts',(-20.940603983949,12.4680809705656,130.315844332064)) ;
#145781 = CARTESIAN_POINT('Ctrl Pts',(-20.8559583287252,12.6795623808911,
130.101791361904)) ;
#145782 = CARTESIAN_POINT('Ctrl Pts',(-20.7925168040744,12.9425895546652,
129.949458890712)) ;
#145783 = CARTESIAN_POINT('Ctrl Pts',(-20.7532890269665,13.2417283918,129.868075591736)) ;
#145784 = CARTESIAN_POINT('Ctrl Pts',(-20.7409116210845,13.5531903661268,
129.865041638529)) ;
#145785 = CARTESIAN_POINT('Ctrl Pts',(-20.7553800380265,13.8554129193782,
129.940450687303)) ;
#145786 = CARTESIAN_POINT('Ctrl Pts',(-20.7947745520951,14.1261609524352,
130.088592371087)) ;
#145787 = CARTESIAN_POINT('Ctrl Pts',(-20.8561230143057,14.3478085326463,
130.30108906054)) ;
#145788 = CARTESIAN_POINT('Ctrl Pts',(-20.9330819717435,14.5013887047212,
130.558818467068)) ;
#145789 = CARTESIAN_POINT('Ctrl Pts',(-21.0209925763894,14.5792263128841,
130.848889090578)) ;
#145790 = CARTESIAN_POINT('Ctrl Pts',(-21.1115720077452,14.5735423168914,
131.146566451509)) ;
#145791 = CARTESIAN_POINT('Ctrl Pts',(-21.1981832466757,14.4859391814988,
131.432684871179)) ;
#145792 = CARTESIAN_POINT('Ctrl Pts',(-21.2740827223277,14.3210239309704,
131.687674997692)) ;
#145793 = CARTESIAN_POINT('Ctrl Pts',(-21.3322242178944,14.0938128758495,
131.890466779621)) ;
#145794 = CARTESIAN_POINT('Ctrl Pts',(-21.3687438781438,13.8165579042321,
132.030389390382)) ;
#145795 = CARTESIAN_POINT('Ctrl Pts',(-21.3797138200489,13.5127263915299,
132.095468544481)) ;
#145796 = CARTESIAN_POINT('Ctrl Pts',(-21.3636004734543,13.2000971209204,
132.081705722308)) ;
#145797 = CARTESIAN_POINT('Ctrl Pts',(-21.3214813309677,12.907342662141,131.991518108208)) ;
#145798 = CARTESIAN_POINT('Ctrl Pts',(-21.2545834330948,12.6479572241649,
131.829377280071)) ;
#145799 = CARTESIAN_POINT('Ctrl Pts',(-21.1681470865365,12.4461100173765,
131.609861160652)) ;
#145800 = CARTESIAN_POINT('Ctrl Pts',(-21.0661478275666,12.3127706189861,
131.345206807129)) ;
#145801 = CARTESIAN_POINT('Ctrl Pts',(-20.9570001828304,12.2601401087974,
131.059348447915)) ;
#145802 = CARTESIAN_POINT('Ctrl Pts',(-20.8464455495092,12.2901733256143,
130.769514283601)) ;
#145803 = CARTESIAN_POINT('Ctrl Pts',(-20.7419747378729,12.4015833067204,
130.497476657603)) ;
#145804 = CARTESIAN_POINT('Ctrl Pts',(-20.6504205693361,12.5866483791686,
130.263212545272)) ;
#145805 = CARTESIAN_POINT('Ctrl Pts',(-20.5779605821059,12.8302723289068,
130.084547548889)) ;
#145806 = CARTESIAN_POINT('Ctrl Pts',(-20.5282977949781,13.1192440261277,
129.97282099279)) ;
#145807 = CARTESIAN_POINT('Ctrl Pts',(-20.5051826159402,13.4254781915307,
129.938132734578)) ;
#145808 = CARTESIAN_POINT('Ctrl Pts',(-20.5087491589204,13.7353596810941,
129.981818058974)) ;
#145809 = CARTESIAN_POINT('Ctrl Pts',(-20.538377675736,14.0210482002996,130.10142777843)) ;
#145810 = CARTESIAN_POINT('Ctrl Pts',(-20.5913066213589,14.2649914716046,
130.289249347501)) ;
#145811 = CARTESIAN_POINT('Ctrl Pts',(-20.66265561167,14.4476747030691,130.53073518382)) ;
#145812 = CARTESIAN_POINT('Ctrl Pts',(-20.7469069028372,14.5574100040251,
130.809977995015)) ;
#145813 = CARTESIAN_POINT('Ctrl Pts',(-20.8371160932442,14.5860647514156,
131.106584787319)) ;
#145814 = CARTESIAN_POINT('Ctrl Pts',(-20.9267472282309,14.5307819261163,
131.401725854825)) ;
#145815 = CARTESIAN_POINT('Ctrl Pts',(-21.0072764966253,14.3969445095406,
131.669955377324)) ;
#145816 = CARTESIAN_POINT('Ctrl Pts',(-21.0734887878382,14.1927448984532,
131.896554788733)) ;
#145817 = CARTESIAN_POINT('Ctrl Pts',(-21.1192566993192,13.93401239778,132.063324626172)) ;
#145818 = CARTESIAN_POINT('Ctrl Pts',(-21.1408827040485,13.6381121003486,
132.159652000683)) ;
#145819 = CARTESIAN_POINT('Ctrl Pts',(-21.1359298836086,13.3270742285028,
132.178300987423)) ;
#145820 = CARTESIAN_POINT('Ctrl Pts',(-21.1040417699142,13.0225106106699,
132.118308686489)) ;
#145821 = CARTESIAN_POINT('Ctrl Pts',(-21.046696839129,12.7468019660475,131.983949585715)) ;
#145822 = CARTESIAN_POINT('Ctrl Pts',(-20.9678162020651,12.5205887293237,
131.786510382128)) ;
#145823 = CARTESIAN_POINT('Ctrl Pts',(-20.8715310603488,12.3578209293796,
131.538392523229)) ;
#145824 = CARTESIAN_POINT('Ctrl Pts',(-20.7644175602374,12.2716454717833,
131.258612557137)) ;
#145825 = CARTESIAN_POINT('Ctrl Pts',(-20.6533664144399,12.2679543097138,
130.967335036085)) ;
#145826 = CARTESIAN_POINT('Ctrl Pts',(-20.5457061292773,12.3469222200597,
130.685931563992)) ;
#145827 = CARTESIAN_POINT('Ctrl Pts',(-20.4482108374109,12.503089881748,130.434261150502)) ;
#145828 = CARTESIAN_POINT('Ctrl Pts',(-20.3673275506228,12.7250182855012,
130.231090321485)) ;
#145829 = CARTESIAN_POINT('Ctrl Pts',(-20.3079802630187,12.9971829063299,
130.090864398519)) ;
#145830 = CARTESIAN_POINT('Ctrl Pts',(-20.2738118580622,13.2997829333183,
130.024178485513)) ;
#145831 = CARTESIAN_POINT('Ctrl Pts',(-20.2664947685224,13.6108911186927,
130.035899919689)) ;
#145832 = CARTESIAN_POINT('Ctrl Pts',(-20.2857578508788,13.9087324272285,
130.125281467885)) ;
#145833 = CARTESIAN_POINT('Ctrl Pts',(-20.3297556724829,14.1725576742086,
130.287029545329)) ;
#145834 = CARTESIAN_POINT('Ctrl Pts',(-20.3941998282761,14.3815588265502,
130.508353654678)) ;
#145835 = CARTESIAN_POINT('Ctrl Pts',(-20.474005477433,14.5223296073452,130.774601426749)) ;
#145836 = CARTESIAN_POINT('Ctrl Pts',(-20.5626590610956,14.5844939687617,
131.066682489216)) ;
#145837 = CARTESIAN_POINT('Ctrl Pts',(-20.6534515210062,14.5631534202887,
131.365145687928)) ;
#145838 = CARTESIAN_POINT('Ctrl Pts',(-20.7382600278816,14.4606750911625,
131.645905123897)) ;
#145839 = CARTESIAN_POINT('Ctrl Pts',(-20.8114033440883,14.2826953933965,
131.892850174446)) ;
#145840 = CARTESIAN_POINT('Ctrl Pts',(-20.8657920624794,14.0447463333177,
132.084724481994)) ;
#145841 = CARTESIAN_POINT('Ctrl Pts',(-20.8976628106915,13.7613771036905,
132.21097302955)) ;
#145842 = CARTESIAN_POINT('Ctrl Pts',(-20.9036617211628,13.4542323232824,
132.261581459296)) ;
#145843 = CARTESIAN_POINT('Ctrl Pts',(-20.8826279491425,13.143799460901,132.233338652764)) ;
#145844 = CARTESIAN_POINT('Ctrl Pts',(-20.8352934217348,12.8538469192422,
132.128218778633)) ;
#145845 = CARTESIAN_POINT('Ctrl Pts',(-20.7645944475466,12.6054873495862,
131.954751852928)) ;
#145846 = CARTESIAN_POINT('Ctrl Pts',(-20.6749066761871,12.4153273206803,
131.725780854323)) ;
#145847 = CARTESIAN_POINT('Ctrl Pts',(-20.5706090003662,12.2964112458501,
131.454476537484)) ;
#145848 = CARTESIAN_POINT('Ctrl Pts',(-20.4608420339056,12.2594155900217,
131.166772800409)) ;
#145849 = CARTESIAN_POINT('Ctrl Pts',(-20.3506734795636,12.3053349442499,
130.878138641754)) ;
#145850 = CARTESIAN_POINT('Ctrl Pts',(-20.2484737854587,12.4312259098382,
130.612644740711)) ;
#145851 = CARTESIAN_POINT('Ctrl Pts',(-20.1602130981831,12.6279597260861,
130.387910852536)) ;
#145852 = CARTESIAN_POINT('Ctrl Pts',(-20.0915104002888,12.8824933120028,
130.220406199881)) ;
#145853 = CARTESIAN_POINT('Ctrl Pts',(-20.0469681651641,13.1745455822002,
130.123334294232)) ;
#145854 = CARTESIAN_POINT('Ctrl Pts',(-20.0286034664188,13.485175620818,130.102825718079)) ;
#145855 = CARTESIAN_POINT('Ctrl Pts',(-20.0373664825325,13.7921379938219,
130.161654025936)) ;
#145856 = CARTESIAN_POINT('Ctrl Pts',(-20.0715995929942,14.0710148384314,
130.294692145833)) ;
#145857 = CARTESIAN_POINT('Ctrl Pts',(-20.1284301538696,14.3045452555015,
130.493888748158)) ;
#145858 = CARTESIAN_POINT('Ctrl Pts',(-20.2024927177133,14.4740866338348,
130.743236807604)) ;
#145859 = CARTESIAN_POINT('Ctrl Pts',(-20.2887543569043,14.5693022561264,
131.028482394559)) ;
#145860 = CARTESIAN_POINT('Ctrl Pts',(-20.3791881951362,14.582012624519,131.325700094759)) ;
#145861 = CARTESIAN_POINT('Ctrl Pts',(-20.4677451846558,14.5112270801159,
131.617691378033)) ;
#145862 = CARTESIAN_POINT('Ctrl Pts',(-20.5458784428509,14.3635590913307,
131.878885598879)) ;
#145863 = CARTESIAN_POINT('Ctrl Pts',(-20.6086278771025,14.1479538826623,
132.095344152089)) ;
#145864 = CARTESIAN_POINT('Ctrl Pts',(-20.6501541988264,13.8806546187411,
132.249752133656)) ;
#145865 = CARTESIAN_POINT('Ctrl Pts',(-20.6669329941746,13.5796272829373,
132.331977408768)) ;
#145866 = CARTESIAN_POINT('Ctrl Pts',(-20.6567504793002,13.2675901061276,
132.335413489308)) ;
#145867 = CARTESIAN_POINT('Ctrl Pts',(-20.6200953900451,12.9685391977506,
132.261306783387)) ;
#145868 = CARTESIAN_POINT('Ctrl Pts',(-20.5583590983708,12.7001826766663,
132.114143420094)) ;
#145869 = CARTESIAN_POINT('Ctrl Pts',(-20.4756221157238,12.4843513272629,
131.905532471069)) ;
#145870 = CARTESIAN_POINT('Ctrl Pts',(-20.3767435277783,12.3354377542164,
131.649841765062)) ;
#145871 = CARTESIAN_POINT('Ctrl Pts',(-20.2686590300988,12.2645466478322,
131.367129971997)) ;
#145872 = CARTESIAN_POINT('Ctrl Pts',(-20.1571318808931,12.276740062036,131.074627014157)) ;
#145873 = CARTESIAN_POINT('Ctrl Pts',(-20.0512008838517,12.3708039289104,
130.79818158066)) ;
#145874 = CARTESIAN_POINT('Ctrl Pts',(-19.9563086255669,12.5405714665883,
130.554144914128)) ;
#145875 = CARTESIAN_POINT('Ctrl Pts',(-19.8793088986638,12.7727637010119,
130.362246811073)) ;
#145876 = CARTESIAN_POINT('Ctrl Pts',(-19.8242814025798,13.0532482908803,
130.234757689759)) ;
#145877 = CARTESIAN_POINT('Ctrl Pts',(-19.7952189624458,13.3594504233503,
130.183004684366)) ;
#145878 = CARTESIAN_POINT('Ctrl Pts',(-19.7930134578907,13.6687251009062,
130.209550970589)) ;
#145879 = CARTESIAN_POINT('Ctrl Pts',(-19.817213216908,13.9622484425501,130.313436084114)) ;
#145880 = CARTESIAN_POINT('Ctrl Pts',(-19.8653052839122,14.2163837439272,
130.487026316147)) ;
#145881 = CARTESIAN_POINT('Ctrl Pts',(-19.9333746488485,14.4143549492585,
130.719088100669)) ;
#145882 = CARTESIAN_POINT('Ctrl Pts',(-20.0153927997561,14.5404303849103,
130.991781249979)) ;
#145883 = CARTESIAN_POINT('Ctrl Pts',(-20.1046291781112,14.5868747911533,
131.285452132637)) ;
#145884 = CARTESIAN_POINT('Ctrl Pts',(-20.1949857625837,14.5499212467829,
131.582654306618)) ;
#145885 = CARTESIAN_POINT('Ctrl Pts',(-20.2781124905757,14.4324626312606,
131.858552426998)) ;
#145886 = CARTESIAN_POINT('Ctrl Pts',(-20.3481188112535,14.2419356966938,
132.096282760798)) ;
#145887 = CARTESIAN_POINT('Ctrl Pts',(-20.3985871619512,13.9939564791264,
132.276740859809)) ;
#145888 = CARTESIAN_POINT('Ctrl Pts',(-20.425720129423,13.7043181769273,132.389150470966)) ;
#145889 = CARTESIAN_POINT('Ctrl Pts',(-20.426667137121,13.395369790062,132.424965585476)) ;
#145890 = CARTESIAN_POINT('Ctrl Pts',(-20.4005199781611,13.086808383261,132.381812352242)) ;
#145891 = CARTESIAN_POINT('Ctrl Pts',(-20.3486042070597,12.8035341555048,
132.263245810191)) ;
#145892 = CARTESIAN_POINT('Ctrl Pts',(-20.2736098470821,12.5639567351557,
132.077367144187)) ;
#145893 = CARTESIAN_POINT('Ctrl Pts',(-20.1807645712942,12.3867441251715,
131.839192537053)) ;
#145894 = CARTESIAN_POINT('Ctrl Pts',(-20.0751360357646,12.2832559633923,
131.563844017608)) ;
#145895 = CARTESIAN_POINT('Ctrl Pts',(-19.964903232874,12.2616345665819,131.274777694618)) ;
#145896 = CARTESIAN_POINT('Ctrl Pts',(-19.8555629286285,12.3231638960011,
130.98858229832)) ;
#145897 = CARTESIAN_POINT('Ctrl Pts',(-19.7556644206763,12.4627500215576,
130.729750507701)) ;
#145898 = CARTESIAN_POINT('Ctrl Pts',(-19.6702402237526,12.6729053974916,
130.513517339829)) ;
#145899 = CARTESIAN_POINT('Ctrl Pts',(-19.6062148535559,12.9344260822497,
130.35944129945)) ;
#145900 = CARTESIAN_POINT('Ctrl Pts',(-19.5661559405149,13.234077565713,130.27576146091)) ;
#145901 = CARTESIAN_POINT('Ctrl Pts',(-19.5531448999268,13.5439039553039,
130.270706955932)) ;
#145902 = CARTESIAN_POINT('Ctrl Pts',(-19.5667543120863,13.8465582342306,
130.343585324908)) ;
#145903 = CARTESIAN_POINT('Ctrl Pts',(-19.6055060890507,14.1188040415087,
130.489887703278)) ;
#145904 = CARTESIAN_POINT('Ctrl Pts',(-19.6661894867969,14.3420291426398,
130.700400837048)) ;
#145905 = CARTESIAN_POINT('Ctrl Pts',(-19.7429904163147,14.4980360771653,
130.957766454984)) ;
#145906 = CARTESIAN_POINT('Ctrl Pts',(-19.8302733403421,14.5780642539032,
131.245841073644)) ;
#145907 = CARTESIAN_POINT('Ctrl Pts',(-19.921571119927,14.5747644514925,131.545879565233)) ;
#145908 = CARTESIAN_POINT('Ctrl Pts',(-20.007901843405,14.489550077403,131.830999188099)) ;
#145909 = CARTESIAN_POINT('Ctrl Pts',(-20.0841056157462,14.3274511232625,
132.086804079126)) ;
#145910 = CARTESIAN_POINT('Ctrl Pts',(-20.1430494283501,14.10121310871,132.292050722471)) ;
#145911 = CARTESIAN_POINT('Ctrl Pts',(-20.1802685099669,13.8249843797631,
132.434023249095)) ;
#145912 = CARTESIAN_POINT('Ctrl Pts',(-20.1919483927985,13.5214320860101,
132.501202568774)) ;
#145913 = CARTESIAN_POINT('Ctrl Pts',(-20.1767867112314,13.2103011439188,
132.490041780221)) ;
#145914 = CARTESIAN_POINT('Ctrl Pts',(-20.1352091335675,12.9148531024708,
132.401647345103)) ;
#145915 = CARTESIAN_POINT('Ctrl Pts',(-20.0688842605853,12.6543477240414,
132.24117051739)) ;
#145916 = CARTESIAN_POINT('Ctrl Pts',(-19.983093218714,12.4511188454898,132.023484182445)) ;
#145917 = CARTESIAN_POINT('Ctrl Pts',(-19.8816672758417,12.3156705346788,
131.760435661779)) ;
#145918 = CARTESIAN_POINT('Ctrl Pts',(-19.7721629217621,12.2603783289395,
131.473684187594)) ;
#145919 = CARTESIAN_POINT('Ctrl Pts',(-19.6616031715542,12.2883877322888,
131.183818528714)) ;
#145920 = CARTESIAN_POINT('Ctrl Pts',(-19.5572825092889,12.396958266653,130.912081314997)) ;
#145921 = CARTESIAN_POINT('Ctrl Pts',(-19.4649165468607,12.5805839766397,
130.675559335482)) ;
#145922 = CARTESIAN_POINT('Ctrl Pts',(-19.3920517907422,12.8225431268309,
130.49566490348)) ;
#145923 = CARTESIAN_POINT('Ctrl Pts',(-19.3417667776537,13.1085293602313,
130.381910274806)) ;
#145924 = CARTESIAN_POINT('Ctrl Pts',(-19.3176156777269,13.4184312820959,
130.344629887277)) ;
#145925 = CARTESIAN_POINT('Ctrl Pts',(-19.3204546895957,13.725396855158,130.38583576103)) ;
#145926 = CARTESIAN_POINT('Ctrl Pts',(-19.3494655025508,14.0140710233184,
130.503873246052)) ;
#145927 = CARTESIAN_POINT('Ctrl Pts',(-19.4017261950081,14.2586953082214,
130.689648250537)) ;
#145928 = CARTESIAN_POINT('Ctrl Pts',(-19.4726871937748,14.4435712393275,
130.930045601665)) ;
#145929 = CARTESIAN_POINT('Ctrl Pts',(-19.5566519911389,14.5554638081498,
131.208437931173)) ;
#145930 = CARTESIAN_POINT('Ctrl Pts',(-19.6468808266438,14.5862678501096,
131.505140126049)) ;
#145931 = CARTESIAN_POINT('Ctrl Pts',(-19.7360484351444,14.5339455279845,
131.798696701267)) ;
#145932 = CARTESIAN_POINT('Ctrl Pts',(-19.8173615669052,14.4019055584218,
132.069386773039)) ;
#145933 = CARTESIAN_POINT('Ctrl Pts',(-19.8839994555415,14.1996929308369,
132.297189223288)) ;
#145934 = CARTESIAN_POINT('Ctrl Pts',(-19.9305118128425,13.9418839763085,
132.466195135576)) ;
#145935 = CARTESIAN_POINT('Ctrl Pts',(-19.9528419276723,13.6467945517117,
132.56456832424)) ;
#145936 = CARTESIAN_POINT('Ctrl Pts',(-19.9486515206637,13.3358857358536,
132.585446635425)) ;
#145937 = CARTESIAN_POINT('Ctrl Pts',(-19.9175619038722,13.0311283359512,
132.527750633158)) ;
#145938 = CARTESIAN_POINT('Ctrl Pts',(-19.8609233985763,12.7543595067604,
132.395451902013)) ;
#145939 = CARTESIAN_POINT('Ctrl Pts',(-19.7827102679386,12.5263863833961,
132.199944643095)) ;
#145940 = CARTESIAN_POINT('Ctrl Pts',(-19.6860393622514,12.3607017684255,
131.950953906113)) ;
#145941 = CARTESIAN_POINT('Ctrl Pts',(-19.580104111669,12.2732420029804,131.674307412116)) ;
#145942 = CARTESIAN_POINT('Ctrl Pts',(-19.4686330724515,12.2668291294782,
131.381938905443)) ;
#145943 = CARTESIAN_POINT('Ctrl Pts',(-19.3608533291528,12.3436152480751,
131.100162840615)) ;
#145944 = CARTESIAN_POINT('Ctrl Pts',(-19.2628621236054,12.4979168003383,
130.84708500029)) ;
#145945 = CARTESIAN_POINT('Ctrl Pts',(-19.1815148595947,12.7181781437397,
130.642540710761)) ;
#145946 = CARTESIAN_POINT('Ctrl Pts',(-19.1215859229779,12.9887185054322,
130.500562129518)) ;
#145947 = CARTESIAN_POINT('Ctrl Pts',(-19.0866327913616,13.2908827967775,
130.431601676791)) ;
#145948 = CARTESIAN_POINT('Ctrl Pts',(-19.0785282040241,13.6021684785122,
130.441033599336)) ;
#145949 = CARTESIAN_POINT('Ctrl Pts',(-19.0971518047465,13.901537415506,130.52864407598)) ;
#145950 = CARTESIAN_POINT('Ctrl Pts',(-19.1405520283606,14.1661758295122,
130.6886143988)) ;
#145951 = CARTESIAN_POINT('Ctrl Pts',(-19.2042657866774,14.3763137224392,
130.907701859825)) ;
#145952 = CARTESIAN_POINT('Ctrl Pts',(-19.2839098721216,14.5195379343594,
131.173557478438)) ;
#145953 = CARTESIAN_POINT('Ctrl Pts',(-19.3721859569991,14.5837467777198,
131.464450468761)) ;
#145954 = CARTESIAN_POINT('Ctrl Pts',(-19.4629509428763,14.5651055472896,
131.762802835642)) ;
#145955 = CARTESIAN_POINT('Ctrl Pts',(-19.5482888539825,14.4645028537766,
132.045218992615)) ;
#145956 = CARTESIAN_POINT('Ctrl Pts',(-19.6216217472489,14.2890439615902,
132.292607820973)) ;
#145957 = CARTESIAN_POINT('Ctrl Pts',(-19.6766909799852,14.0526944517644,
132.486486401001)) ;
#145958 = CARTESIAN_POINT('Ctrl Pts',(-19.7093072750895,13.7699865640071,
132.6149543649)) ;
#145959 = CARTESIAN_POINT('Ctrl Pts',(-19.7161146198736,13.4631529119525,
132.667930442523)) ;
#145960 = CARTESIAN_POINT('Ctrl Pts',(-19.6956515836537,13.1513620896954,
132.641483995069)) ;
#145961 = CARTESIAN_POINT('Ctrl Pts',(-19.6494470974551,12.8627668245119,
132.539399272476)) ;
#145962 = CARTESIAN_POINT('Ctrl Pts',(-19.5788203474868,12.6109028721184,
132.366417950411)) ;
#145963 = CARTESIAN_POINT('Ctrl Pts',(-19.4899551594223,12.4200193080497,
132.139689682939)) ;
#145964 = CARTESIAN_POINT('Ctrl Pts',(-19.3859186787791,12.298694725006,131.869172924049)) ;
#145965 = CARTESIAN_POINT('Ctrl Pts',(-19.2763944386609,12.2592723921271,
131.582128978046)) ;
#145966 = CARTESIAN_POINT('Ctrl Pts',(-19.165779613809,12.3030853474822,131.29229953169)) ;
#145967 = CARTESIAN_POINT('Ctrl Pts',(-19.0638020603307,12.4259705793417,
131.027270360588)) ;
#145968 = CARTESIAN_POINT('Ctrl Pts',(-18.9744571168751,12.6220550039555,
130.799590383652)) ;
#145969 = CARTESIAN_POINT('Ctrl Pts',(-18.9054157982143,12.8744669424422,
130.630978711971)) ;
#145970 = CARTESIAN_POINT('Ctrl Pts',(-18.8600323634942,13.1663406139675,
130.531527387548)) ;
#145971 = CARTESIAN_POINT('Ctrl Pts',(-18.8410254999906,13.475878892664,130.509047923724)) ;
#145972 = CARTESIAN_POINT('Ctrl Pts',(-18.848828895151,13.7823953075606,130.564962887383)) ;
#145973 = CARTESIAN_POINT('Ctrl Pts',(-18.8826580153594,14.064418215805,130.69708049184)) ;
#145974 = CARTESIAN_POINT('Ctrl Pts',(-18.9384679926998,14.2977471414108,
130.893033181098)) ;
#145975 = CARTESIAN_POINT('Ctrl Pts',(-19.0125610674894,14.4706194179794,
131.142700487904)) ;
#145976 = CARTESIAN_POINT('Ctrl Pts',(-19.09833071192,14.5675955159237,131.426393987923)) ;
#145977 = CARTESIAN_POINT('Ctrl Pts',(-19.1887786220764,14.5827755983601,
131.723678445035)) ;
#145978 = CARTESIAN_POINT('Ctrl Pts',(-19.2771526394746,14.5148008413574,
132.014994755847)) ;
#145979 = CARTESIAN_POINT('Ctrl Pts',(-19.3559595938276,14.3692242855325,
132.278254867564)) ;
#145980 = CARTESIAN_POINT('Ctrl Pts',(-19.4195009826797,14.1540994204916,
132.497190285371)) ;
#145981 = CARTESIAN_POINT('Ctrl Pts',(-19.4614287947386,13.889194577701,132.652613367611)) ;
#145982 = CARTESIAN_POINT('Ctrl Pts',(-19.479026321897,13.5894848313417,132.737169180434)) ;
#145983 = CARTESIAN_POINT('Ctrl Pts',(-19.469691253169,13.2771021698192,132.743118485761)) ;
#145984 = CARTESIAN_POINT('Ctrl Pts',(-19.4337533195738,12.9767128859996,
132.67117726944)) ;
#145985 = CARTESIAN_POINT('Ctrl Pts',(-19.3723820364147,12.7063601582146,
132.525197848911)) ;
#145986 = CARTESIAN_POINT('Ctrl Pts',(-19.2906337460424,12.4901609157503,
132.319283266615)) ;
#145987 = CARTESIAN_POINT('Ctrl Pts',(-19.1920848992532,12.338688213011,132.064589679679)) ;
#145988 = CARTESIAN_POINT('Ctrl Pts',(-19.0839647079271,12.2654833215425,
131.781836975828)) ;
#145989 = CARTESIAN_POINT('Ctrl Pts',(-18.9727805931348,12.2750423939134,
131.490221782582)) ;
#145990 = CARTESIAN_POINT('Ctrl Pts',(-18.8660747623374,12.3673309477628,
131.211686629903)) ;
#145991 = CARTESIAN_POINT('Ctrl Pts',(-18.771239184174,12.5343469793072,130.96765150365)) ;
#145992 = CARTESIAN_POINT('Ctrl Pts',(-18.693437502563,12.7652871615339,130.773485647564)) ;
#145993 = CARTESIAN_POINT('Ctrl Pts',(-18.6378021901779,13.0444119641298,
130.644182284215)) ;
#145994 = CARTESIAN_POINT('Ctrl Pts',(-18.6078827874849,13.3498617711502,
130.58989899629)) ;
#145995 = CARTESIAN_POINT('Ctrl Pts',(-18.6049643640782,13.6613615410962,
130.614584854872)) ;
#145996 = CARTESIAN_POINT('Ctrl Pts',(-18.6283610363628,13.9537822456917,
130.715914869578)) ;
#145997 = CARTESIAN_POINT('Ctrl Pts',(-18.6757830396079,14.2096141723503,
130.887574922432)) ;
#145998 = CARTESIAN_POINT('Ctrl Pts',(-18.7432084588704,14.4090573352496,
131.117688224262)) ;
#145999 = CARTESIAN_POINT('Ctrl Pts',(-18.8248444961312,14.5378227777349,
131.389262062474)) ;
#146000 = CARTESIAN_POINT('Ctrl Pts',(-18.9146615446444,14.5866410232384,
131.684888368504)) ;
#146001 = CARTESIAN_POINT('Ctrl Pts',(-19.0042448193372,14.5524956968184,
131.979503816669)) ;
#146002 = CARTESIAN_POINT('Ctrl Pts',(-19.0884275166112,14.4363359787846,
132.258795156506)) ;
#146003 = CARTESIAN_POINT('Ctrl Pts',(-19.158384232285,14.2487612531945,132.496149660261)) ;
#146004 = CARTESIAN_POINT('Ctrl Pts',(-19.2096369480705,14.0019963672536,
132.678965768853)) ;
#146005 = CARTESIAN_POINT('Ctrl Pts',(-19.2375262292726,13.7133413750086,
132.793570526747)) ;
#146006 = CARTESIAN_POINT('Ctrl Pts',(-19.2391685265025,13.4034231078491,
132.831554039307)) ;
#146007 = CARTESIAN_POINT('Ctrl Pts',(-19.2140103146631,13.0966156009071,
132.791052370135)) ;
#146008 = CARTESIAN_POINT('Ctrl Pts',(-19.1625096709922,12.8104956204696,
132.673916665319)) ;
#146009 = CARTESIAN_POINT('Ctrl Pts',(-19.08847519723,12.5707042349948,132.490662999038)) ;
#146010 = CARTESIAN_POINT('Ctrl Pts',(-18.9959730199521,12.3910193657153,
132.253550999424)) ;
#146011 = CARTESIAN_POINT('Ctrl Pts',(-18.8908542141825,12.285328864528,131.979615249099)) ;
#146012 = CARTESIAN_POINT('Ctrl Pts',(-18.7803139240097,12.2609818529467,
131.6897631227)) ;
#146013 = CARTESIAN_POINT('Ctrl Pts',(-18.6705377025057,12.3204757590526,
131.402379707675)) ;
#146014 = CARTESIAN_POINT('Ctrl Pts',(-18.5703346082798,12.4582515921679,
131.14266448369)) ;
#146015 = CARTESIAN_POINT('Ctrl Pts',(-18.4846714167296,12.6658998652864,
130.92561853516)) ;
#146016 = CARTESIAN_POINT('Ctrl Pts',(-18.4198906462997,12.9268096194457,
130.769416613743)) ;
#146017 = CARTESIAN_POINT('Ctrl Pts',(-18.3793353527382,13.2233761882574,
130.684026781784)) ;
#146018 = CARTESIAN_POINT('Ctrl Pts',(-18.3653039385833,13.5346577028184,
130.67616016624)) ;
#146019 = CARTESIAN_POINT('Ctrl Pts',(-18.37825174114,13.8387961550216,130.747205171599)) ;
#146020 = CARTESIAN_POINT('Ctrl Pts',(-18.416436223305,14.1123018093557,130.891880637841)) ;
#146021 = CARTESIAN_POINT('Ctrl Pts',(-18.4764360525695,14.3364687446635,
131.100308420715)) ;
#146022 = CARTESIAN_POINT('Ctrl Pts',(-18.5528414616942,14.494770833943,131.356525814744)) ;
#146023 = CARTESIAN_POINT('Ctrl Pts',(-18.6403171302965,14.5769227995843,
131.645303937294)) ;
#146024 = CARTESIAN_POINT('Ctrl Pts',(-18.7305714826929,14.5762675412157,
131.941905078074)) ;
#146025 = CARTESIAN_POINT('Ctrl Pts',(-18.8178911875836,14.4930554177443,
132.23020487892)) ;
#146026 = CARTESIAN_POINT('Ctrl Pts',(-18.8942971692305,14.3331650364545,
132.4865191295)) ;
#146027 = CARTESIAN_POINT('Ctrl Pts',(-18.9539181012747,14.1081176093321,
132.693817778015)) ;
#146028 = CARTESIAN_POINT('Ctrl Pts',(-18.9916963349415,13.8340178637995,
132.837300403657)) ;
#146029 = CARTESIAN_POINT('Ctrl Pts',(-19.0042096670202,13.5302898798933,
132.90699864193)) ;
#146030 = CARTESIAN_POINT('Ctrl Pts',(-18.989829242128,13.2194241455141,132.898077222158)) ;
#146031 = CARTESIAN_POINT('Ctrl Pts',(-18.949020417078,12.9232187981691,132.811930535479)) ;
#146032 = CARTESIAN_POINT('Ctrl Pts',(-18.8834324422067,12.6614612454166,
132.653582726297)) ;
#146033 = CARTESIAN_POINT('Ctrl Pts',(-18.7979851633379,12.4560560128417,
132.436966453739)) ;
#146034 = CARTESIAN_POINT('Ctrl Pts',(-18.6972333502297,12.3187614460116,
132.17577996401)) ;
#146035 = CARTESIAN_POINT('Ctrl Pts',(-18.5877188076482,12.2608758912203,
131.889053743613)) ;
#146036 = CARTESIAN_POINT('Ctrl Pts',(-18.4772617072998,12.2860567579314,
131.599425070931)) ;
#146037 = CARTESIAN_POINT('Ctrl Pts',(-18.3717678028048,12.3936760882031,
131.324566267309)) ;
#146038 = CARTESIAN_POINT('Ctrl Pts',(-18.2799662634484,12.5734427246259,
131.08932574441)) ;
#146039 = CARTESIAN_POINT('Ctrl Pts',(-18.205832390456,12.8155556850103,130.905988455816)) ;
#146040 = CARTESIAN_POINT('Ctrl Pts',(-18.1551033037978,13.1001458972495,
130.790857619227)) ;
#146041 = CARTESIAN_POINT('Ctrl Pts',(-18.1301831955087,13.4082451879306,
130.751183187586)) ;
#146042 = CARTESIAN_POINT('Ctrl Pts',(-18.1321866015327,13.7170001803432,
130.790102685016)) ;
#146043 = CARTESIAN_POINT('Ctrl Pts',(-18.160608589631,14.0068803402206,130.906464225431)) ;
#146044 = CARTESIAN_POINT('Ctrl Pts',(-18.2120937054126,14.2520830293328,
131.089860423946)) ;
#146045 = CARTESIAN_POINT('Ctrl Pts',(-18.2824550721689,14.4388654830233,
131.328466488959)) ;
#146046 = CARTESIAN_POINT('Ctrl Pts',(-18.3662181188831,14.5532758732377,
131.606309319578)) ;
#146047 = CARTESIAN_POINT('Ctrl Pts',(-18.4564381360141,14.5866372920254,
131.903009380992)) ;
#146048 = CARTESIAN_POINT('Ctrl Pts',(-18.5459782715731,14.5363254176441,
132.197752354425)) ;
#146049 = CARTESIAN_POINT('Ctrl Pts',(-18.6272540069243,14.4070821621483,
132.46818035341)) ;
#146050 = CARTESIAN_POINT('Ctrl Pts',(-18.6947300760767,14.2058492083664,
132.698587728027)) ;
#146051 = CARTESIAN_POINT('Ctrl Pts',(-18.7417516398663,13.9493209948446,
132.869059993674)) ;
#146052 = CARTESIAN_POINT('Ctrl Pts',(-18.7647488489571,13.6560816427411,
132.969264870124)) ;
#146053 = CARTESIAN_POINT('Ctrl Pts',(-18.7613810278091,13.3454213686902,
132.992539638917)) ;
#146054 = CARTESIAN_POINT('Ctrl Pts',(-18.7312094393375,13.0405957785926,
132.937469885673)) ;
#146055 = CARTESIAN_POINT('Ctrl Pts',(-18.6749590606351,12.761020315257,132.806501464058)) ;
#146056 = CARTESIAN_POINT('Ctrl Pts',(-18.5973111868101,12.5320804704421,
132.612600975859)) ;
#146057 = CARTESIAN_POINT('Ctrl Pts',(-18.5017869925786,12.3651153247515,
132.366732593609)) ;
#146058 = CARTESIAN_POINT('Ctrl Pts',(-18.3951993341836,12.2743249868604,
132.08846016447)) ;
#146059 = CARTESIAN_POINT('Ctrl Pts',(-18.2836787398034,12.2660445265336,
131.795962720769)) ;
#146060 = CARTESIAN_POINT('Ctrl Pts',(-18.1761286055653,12.3402671637665,
131.514732867287)) ;
#146061 = CARTESIAN_POINT('Ctrl Pts',(-18.0777202181115,12.492431210345,131.260444160921)) ;
#146062 = CARTESIAN_POINT('Ctrl Pts',(-17.9959153741565,12.7106681794057,
131.054521630885)) ;
#146063 = CARTESIAN_POINT('Ctrl Pts',(-17.9351451797697,12.9803450583886,
130.910137294443)) ;
#146064 = CARTESIAN_POINT('Ctrl Pts',(-17.8994023316142,13.2833171432177,
130.83901653828)) ;
#146065 = CARTESIAN_POINT('Ctrl Pts',(-17.8906094381936,13.5926828813481,
130.846226131332)) ;
#146066 = CARTESIAN_POINT('Ctrl Pts',(-17.9084948671421,13.8936498651441,
130.931784173422)) ;
#146067 = CARTESIAN_POINT('Ctrl Pts',(-17.9511483769507,14.1589431067745,
131.089492755246)) ;
#146068 = CARTESIAN_POINT('Ctrl Pts',(-18.0144302964997,14.3711507970921,
131.307375688141)) ;
#146069 = CARTESIAN_POINT('Ctrl Pts',(-18.0934259365928,14.5162610816314,
131.571225045128)) ;
#146070 = CARTESIAN_POINT('Ctrl Pts',(-18.182269930839,14.583306350133,131.864052397872)) ;
#146071 = CARTESIAN_POINT('Ctrl Pts',(-18.272835722527,14.5665129586633,132.161733104664)) ;
#146072 = CARTESIAN_POINT('Ctrl Pts',(-18.3581065810839,14.4685223967189,
132.443839852237)) ;
#146073 = CARTESIAN_POINT('Ctrl Pts',(-18.4318404880964,14.2954966012034,
132.692357198206)) ;
#146074 = CARTESIAN_POINT('Ctrl Pts',(-18.4877063256743,14.0596946296019,
132.888702759001)) ;
#146075 = CARTESIAN_POINT('Ctrl Pts',(-18.5209832839551,13.7784555956093,
133.019039209871)) ;
#146076 = CARTESIAN_POINT('Ctrl Pts',(-18.5284065230371,13.4704205391721,
133.073991147064)) ;
#146077 = CARTESIAN_POINT('Ctrl Pts',(-18.5091035543004,13.1626906793203,
133.050459846182)) ;
#146078 = CARTESIAN_POINT('Ctrl Pts',(-18.4631732366913,12.8697533216184,
132.949576875133)) ;
#146079 = CARTESIAN_POINT('Ctrl Pts',(-18.3938110455771,12.6186668370347,
132.77997790901)) ;
#146080 = CARTESIAN_POINT('Ctrl Pts',(-18.3046231204081,12.4240570551779,
132.552627422137)) ;
#146081 = CARTESIAN_POINT('Ctrl Pts',(-18.2019920844373,12.301712902155,132.285853012118)) ;
#146082 = CARTESIAN_POINT('Ctrl Pts',(-18.0917742767469,12.2592124433866,
131.997041312157)) ;
#146083 = CARTESIAN_POINT('Ctrl Pts',(-17.9815995706875,12.3002004237818,
131.708316187743)) ;
#146084 = CARTESIAN_POINT('Ctrl Pts',(-17.8782460339929,12.4222100081088,
131.439623337485)) ;
#146085 = CARTESIAN_POINT('Ctrl Pts',(-17.7891702075967,12.6151763804986,
131.212464661044)) ;
#146086 = CARTESIAN_POINT('Ctrl Pts',(-17.7192518879757,12.866763553233,131.041393055734)) ;
#146087 = CARTESIAN_POINT('Ctrl Pts',(-17.6733163828393,13.1566083036236,
130.940190964357)) ;
#146088 = CARTESIAN_POINT('Ctrl Pts',(-17.6533605413985,13.4669635155183,
130.91505403219)) ;
#146089 = CARTESIAN_POINT('Ctrl Pts',(-17.660526594431,13.7743605860558,130.969164445883)) ;
#146090 = CARTESIAN_POINT('Ctrl Pts',(-17.6933658448605,14.0556835712851,
131.098173550433)) ;
#146091 = CARTESIAN_POINT('Ctrl Pts',(-17.7488867045143,14.2923698679386,
131.293503308698)) ;
#146092 = CARTESIAN_POINT('Ctrl Pts',(-17.8227133439083,14.4669398360514,
131.54242287109)) ;
#146093 = CARTESIAN_POINT('Ctrl Pts',(-17.9077423757333,14.5658237204842,
131.823764797856)) ;
#146094 = CARTESIAN_POINT('Ctrl Pts',(-17.9986684570008,14.5834030750835,
132.122644069035)) ;
#146095 = CARTESIAN_POINT('Ctrl Pts',(-18.0867233838671,14.5182209369221,
132.412831774384)) ;
#146096 = CARTESIAN_POINT('Ctrl Pts',(-18.1665697451038,14.3732472228341,
132.679438010564)) ;
#146097 = CARTESIAN_POINT('Ctrl Pts',(-18.2299692526917,14.161734042983,132.897630258977)) ;
#146098 = CARTESIAN_POINT('Ctrl Pts',(-18.2728829473476,13.8968738672396,
133.056114256463)) ;
#146099 = CARTESIAN_POINT('Ctrl Pts',(-18.2911187814473,13.5970560174392,
133.142599500408)) ;
#146100 = CARTESIAN_POINT('Ctrl Pts',(-18.2824786204777,13.285349771455,133.150512015157)) ;
#146101 = CARTESIAN_POINT('Ctrl Pts',(-18.2473862581819,12.9854213227035,
133.080929265439)) ;
#146102 = CARTESIAN_POINT('Ctrl Pts',(-18.1869883996118,12.7145025865389,
132.937690581817)) ;
#146103 = CARTESIAN_POINT('Ctrl Pts',(-18.1054391959301,12.4953422149561,
132.732519305131)) ;
#146104 = CARTESIAN_POINT('Ctrl Pts',(-18.0070761592923,12.3417857538749,
132.478417504927)) ;
#146105 = CARTESIAN_POINT('Ctrl Pts',(-17.8994483905022,12.2665368093941,
132.197008614467)) ;
#146106 = CARTESIAN_POINT('Ctrl Pts',(-17.7883645178934,12.2735361740405,
131.905651880035)) ;
#146107 = CARTESIAN_POINT('Ctrl Pts',(-17.6814644389021,12.3632299565235,
131.626530218229)) ;
#146108 = CARTESIAN_POINT('Ctrl Pts',(-17.5858934658356,12.5286847950401,
131.380452412425)) ;
#146109 = CARTESIAN_POINT('Ctrl Pts',(-17.5076122654555,12.7579694730324,
131.18486375994)) ;
#146110 = CARTESIAN_POINT('Ctrl Pts',(-17.4513694267864,13.0352202971202,
131.053701691009)) ;
#146111 = CARTESIAN_POINT('Ctrl Pts',(-17.4206145070061,13.3405829184085,
130.99702547713)) ;
#146112 = CARTESIAN_POINT('Ctrl Pts',(-17.4168444194452,13.6512271972451,
131.019110996205)) ;
#146113 = CARTESIAN_POINT('Ctrl Pts',(-17.4395135787806,13.9458587168303,
131.118464332761)) ;
#146114 = CARTESIAN_POINT('Ctrl Pts',(-17.4864529506928,14.2033946727232,
131.288774833455)) ;
#146115 = CARTESIAN_POINT('Ctrl Pts',(-17.5532007112171,14.4040391264647,
131.51681448999)) ;
#146116 = CARTESIAN_POINT('Ctrl Pts',(-17.6343956033889,14.5350227428464,
131.787065599792)) ;
#146117 = CARTESIAN_POINT('Ctrl Pts',(-17.7242162985725,14.5864958766325,
132.082749953862)) ;
#146118 = CARTESIAN_POINT('Ctrl Pts',(-17.8140541710382,14.5544169233344,
132.37817969897)) ;
#146119 = CARTESIAN_POINT('Ctrl Pts',(-17.8980266225735,14.4414134366696,
132.656647056367)) ;
#146120 = CARTESIAN_POINT('Ctrl Pts',(-17.968839016247,14.2551029691134,132.896663337422)) ;
#146121 = CARTESIAN_POINT('Ctrl Pts',(-18.0206609436882,14.0100365412081,
133.081103390275)) ;
#146122 = CARTESIAN_POINT('Ctrl Pts',(-18.0493014678381,13.7214335751914,
133.198003238596)) ;
#146123 = CARTESIAN_POINT('Ctrl Pts',(-18.051767121632,13.4135493095884,133.23819933318)) ;
#146124 = CARTESIAN_POINT('Ctrl Pts',(-18.0272159345045,13.1045553543373,
133.199678527869)) ;
#146125 = CARTESIAN_POINT('Ctrl Pts',(-17.9769019731203,12.819735905808,133.085728232042)) ;
#146126 = CARTESIAN_POINT('Ctrl Pts',(-17.9029324475278,12.5762135123813,
132.902947309471)) ;
#146127 = CARTESIAN_POINT('Ctrl Pts',(-17.8110109172599,12.3952019865551,
132.66745603075)) ;
#146128 = CARTESIAN_POINT('Ctrl Pts',(-17.7060493534379,12.2871509096393,
132.394018600026)) ;
#146129 = CARTESIAN_POINT('Ctrl Pts',(-17.5958228629102,12.2605661260812,
132.105006344478)) ;
#146130 = CARTESIAN_POINT('Ctrl Pts',(-17.4859053807389,12.3174696156297,
131.817205208931)) ;
#146131 = CARTESIAN_POINT('Ctrl Pts',(-17.385124499541,12.4535095799729,131.555883884411)) ;
#146132 = CARTESIAN_POINT('Ctrl Pts',(-17.2991717616446,12.6588731415835,
131.337907662609)) ;
#146133 = CARTESIAN_POINT('Ctrl Pts',(-17.2336625509736,12.9185733098552,
131.179601474472)) ;
#146134 = CARTESIAN_POINT('Ctrl Pts',(-17.1923625242315,13.2144047799764,
131.09203406909)) ;
#146135 = CARTESIAN_POINT('Ctrl Pts',(-17.1775577739653,13.5255442513147,
131.081906877128)) ;
#146136 = CARTESIAN_POINT('Ctrl Pts',(-17.18966249855,13.8297540824603,131.150429396587)) ;
#146137 = CARTESIAN_POINT('Ctrl Pts',(-17.227235954351,14.1049218673864,131.293388869168)) ;
#146138 = CARTESIAN_POINT('Ctrl Pts',(-17.2862925400434,14.3298724417038,
131.498889388524)) ;
#146139 = CARTESIAN_POINT('Ctrl Pts',(-17.3628237983981,14.4915528402348,
131.755720653574)) ;
#146140 = CARTESIAN_POINT('Ctrl Pts',(-17.449818689308,14.5755974614276,132.042977501466)) ;
#146141 = CARTESIAN_POINT('Ctrl Pts',(-17.5402166301667,14.5774288175943,
132.340058427624)) ;
#146142 = CARTESIAN_POINT('Ctrl Pts',(-17.6275292470889,14.4968431022692,
132.628248586778)) ;
#146143 = CARTESIAN_POINT('Ctrl Pts',(-17.7046127069172,14.3385595023236,
132.886659534106)) ;
#146144 = CARTESIAN_POINT('Ctrl Pts',(-17.7647314828476,14.1152209980979,
133.095389388544)) ;
#146145 = CARTESIAN_POINT('Ctrl Pts',(-17.8031897569592,13.8419813754815,
133.240889834337)) ;
#146146 = CARTESIAN_POINT('Ctrl Pts',(-17.8164226854489,13.5398084238246,
133.3125803987)) ;
#146147 = CARTESIAN_POINT('Ctrl Pts',(-17.8028647743182,13.2280435028726,
133.306145228451)) ;
#146148 = CARTESIAN_POINT('Ctrl Pts',(-17.762509518981,12.9300590292135,133.221455259361)) ;
#146149 = CARTESIAN_POINT('Ctrl Pts',(-17.6978430232198,12.6684083848218,
133.065633233242)) ;
#146150 = CARTESIAN_POINT('Ctrl Pts',(-17.6127910105085,12.4608091208846,
132.850228765349)) ;
#146151 = CARTESIAN_POINT('Ctrl Pts',(-17.5122972473823,12.3214093347923,
132.589814453629)) ;
#146152 = CARTESIAN_POINT('Ctrl Pts',(-17.4027531001663,12.2613302981185,
132.303050991841)) ;
#146153 = CARTESIAN_POINT('Ctrl Pts',(-17.2926710306357,12.2843255086961,
132.014392933773)) ;
#146154 = CARTESIAN_POINT('Ctrl Pts',(-17.187376124559,12.3887269891781,131.73995348577)) ;
#146155 = CARTESIAN_POINT('Ctrl Pts',(-17.094528490589,12.567362762576,131.501852203403)) ;
#146156 = CARTESIAN_POINT('Ctrl Pts',(-17.0198679665341,12.8080166965812,
131.316965273115)) ;
#146157 = CARTESIAN_POINT('Ctrl Pts',(-16.9684023291972,13.0914774469774,
131.199671601539)) ;
#146158 = CARTESIAN_POINT('Ctrl Pts',(-16.9426807542661,13.4005589719555,
131.157796261443)) ;
#146159 = CARTESIAN_POINT('Ctrl Pts',(-16.9440165303375,13.7083911607305,
131.194641100135)) ;
#146160 = CARTESIAN_POINT('Ctrl Pts',(-16.9715883950981,13.9985991355892,
131.308446049961)) ;
#146161 = CARTESIAN_POINT('Ctrl Pts',(-17.0225241829903,14.2457812535683,
131.490297397422)) ;
#146162 = CARTESIAN_POINT('Ctrl Pts',(-17.0924768410808,14.434573414283,131.727731486366)) ;
#146163 = CARTESIAN_POINT('Ctrl Pts',(-17.1759989243048,14.5511370884747,
132.004883776446)) ;
#146164 = CARTESIAN_POINT('Ctrl Pts',(-17.2658532219854,14.5867802191552,
132.300414745677)) ;
#146165 = CARTESIAN_POINT('Ctrl Pts',(-17.3555337669737,14.5391948457713,
132.595565619242)) ;
#146166 = CARTESIAN_POINT('Ctrl Pts',(-17.4374124666097,14.4115345320068,
132.867878527861)) ;
#146167 = CARTESIAN_POINT('Ctrl Pts',(-17.5049786238165,14.2134355726879,
133.098342340037)) ;
#146168 = CARTESIAN_POINT('Ctrl Pts',(-17.5528570162914,13.958237750451,133.271366129121)) ;
#146169 = CARTESIAN_POINT('Ctrl Pts',(-17.5766815250463,13.6646542433851,
133.374114982498)) ;
#146170 = CARTESIAN_POINT('Ctrl Pts',(-17.5740742648385,13.3541836423797,
133.399606053148)) ;
#146171 = CARTESIAN_POINT('Ctrl Pts',(-17.5445387474705,13.0484268899304,
133.346452700391)) ;
#146172 = CARTESIAN_POINT('Ctrl Pts',(-17.4893307298857,12.769439556936,133.218328729894)) ;
#146173 = CARTESIAN_POINT('Ctrl Pts',(-17.4122024226174,12.538041732005,133.026020671942)) ;
#146174 = CARTESIAN_POINT('Ctrl Pts',(-17.3165197740753,12.3683285737822,
132.77987187364)) ;
#146175 = CARTESIAN_POINT('Ctrl Pts',(-17.2106392056921,12.2760420146323,
132.503507847891)) ;
#146176 = CARTESIAN_POINT('Ctrl Pts',(-17.0996526659154,12.2649172046645,
132.212420970085)) ;
#146177 = CARTESIAN_POINT('Ctrl Pts',(-16.9913739789809,12.3368690960139,
131.929222871054)) ;
#146178 = CARTESIAN_POINT('Ctrl Pts',(-16.8925201645751,12.4871143046054,
131.67365659481)) ;
#146179 = CARTESIAN_POINT('Ctrl Pts',(-16.8100266244737,12.7041606562746,
131.465789941374)) ;
#146180 = CARTESIAN_POINT('Ctrl Pts',(-16.7488144744473,12.9721743226057,
131.320042358429)) ;
#146181 = CARTESIAN_POINT('Ctrl Pts',(-16.7123802766638,13.2726903984431,
131.246711119902)) ;
#146182 = CARTESIAN_POINT('Ctrl Pts',(-16.7026684240063,13.5844635777056,
131.251490845653)) ;
#146183 = CARTESIAN_POINT('Ctrl Pts',(-16.7198723144853,13.8852371899129,
131.334971985811)) ;
#146184 = CARTESIAN_POINT('Ctrl Pts',(-16.7615944094477,14.1508961258859,
131.489831947096)) ;
#146185 = CARTESIAN_POINT('Ctrl Pts',(-16.8244978834266,14.3659570919706,
131.706731651083)) ;
#146186 = CARTESIAN_POINT('Ctrl Pts',(-16.903483751971,14.5133844766524,131.970678602505)) ;
#146187 = CARTESIAN_POINT('Ctrl Pts',(-16.9914123716409,14.5822824975676,
132.26055324515)) ;
#146188 = CARTESIAN_POINT('Ctrl Pts',(-17.0822412219883,14.5684017551043,
132.559086977075)) ;
#146189 = CARTESIAN_POINT('Ctrl Pts',(-17.1679464043999,14.4726240030268,
132.842523268284)) ;
#146190 = CARTESIAN_POINT('Ctrl Pts',(-17.2423050049178,14.3009017831871,
133.092973244359)) ;
#146191 = CARTESIAN_POINT('Ctrl Pts',(-17.2985250729578,14.0676661547484,
133.290210100475)) ;
#146192 = CARTESIAN_POINT('Ctrl Pts',(-17.3325852755681,13.7867922981234,
133.422922252114)) ;
#146193 = CARTESIAN_POINT('Ctrl Pts',(-17.340812658842,13.4808115386222,133.480046696113)) ;
#146194 = CARTESIAN_POINT('Ctrl Pts',(-17.322213176098,13.1706177086878,133.458812233851)) ;
#146195 = CARTESIAN_POINT('Ctrl Pts',(-17.2768978369704,12.877048394192,133.35971302766)) ;
#146196 = CARTESIAN_POINT('Ctrl Pts',(-17.2082784989992,12.6251910446387,
133.192217667791)) ;
#146197 = CARTESIAN_POINT('Ctrl Pts',(-17.1198239714151,12.4289584730978,
132.966933197476)) ;
#146198 = CARTESIAN_POINT('Ctrl Pts',(-17.016947151482,12.3038002385442,132.699618788606)) ;
#146199 = CARTESIAN_POINT('Ctrl Pts',(-16.9070593349269,12.2593442702032,
132.411696671294)) ;
#146200 = CARTESIAN_POINT('Ctrl Pts',(-16.7970423402235,12.2978898762746,
132.123361876262)) ;
#146201 = CARTESIAN_POINT('Ctrl Pts',(-16.6936288501025,12.4169444265874,
131.854394739963)) ;
#146202 = CARTESIAN_POINT('Ctrl Pts',(-16.6034534816505,12.6093773192219,
131.624257767718)) ;
#146203 = CARTESIAN_POINT('Ctrl Pts',(-16.5333014451683,12.8583734151229,
131.452333124793)) ;
#146204 = CARTESIAN_POINT('Ctrl Pts',(-16.4864482413194,13.1480449796925,
131.348541807378)) ;
#146205 = CARTESIAN_POINT('Ctrl Pts',(-16.4657803621371,13.4582418088587,
131.321329051345)) ;
#146206 = CARTESIAN_POINT('Ctrl Pts',(-16.4721450959125,13.7655079341762,
131.373040893652)) ;
#146207 = CARTESIAN_POINT('Ctrl Pts',(-16.5043240159691,14.048316994012,131.500173624113)) ;
#146208 = CARTESIAN_POINT('Ctrl Pts',(-16.55917049357,14.2859990299988,131.693469739828)) ;
#146209 = CARTESIAN_POINT('Ctrl Pts',(-16.6322772804353,14.4624790722787,
131.940192970349)) ;
#146210 = CARTESIAN_POINT('Ctrl Pts',(-16.7176228652551,14.5642184031824,
132.222682879556)) ;
#146211 = CARTESIAN_POINT('Ctrl Pts',(-16.8079333251705,14.584160945988,132.519546694171)) ;
#146212 = CARTESIAN_POINT('Ctrl Pts',(-16.8967026449305,14.5209707107522,
132.812037468598)) ;
#146213 = CARTESIAN_POINT('Ctrl Pts',(-16.9763340125269,14.3791778899535,
133.077768668898)) ;
#146214 = CARTESIAN_POINT('Ctrl Pts',(-17.0406340695259,14.1688150689694,
133.298742386899)) ;
#146215 = CARTESIAN_POINT('Ctrl Pts',(-17.0841510266317,13.9051956236196,
133.458976239671)) ;
#146216 = CARTESIAN_POINT('Ctrl Pts',(-17.1031304829445,13.6071499712881,
133.547524781534)) ;
#146217 = CARTESIAN_POINT('Ctrl Pts',(-17.095445226368,13.2953842790605,133.55823520747)) ;
#146218 = CARTESIAN_POINT('Ctrl Pts',(-17.0608564828447,12.9930168542047,
133.49033126729)) ;
#146219 = CARTESIAN_POINT('Ctrl Pts',(-17.0014002167995,12.722227284065,133.349682917051)) ;
#146220 = CARTESIAN_POINT('Ctrl Pts',(-16.920181788314,12.5005440271994,133.145587035709)) ;
#146221 = CARTESIAN_POINT('Ctrl Pts',(-16.822238500183,12.3451352919228,132.892688097985)) ;
#146222 = CARTESIAN_POINT('Ctrl Pts',(-16.7147807681509,12.2674914162103,
132.611784861536)) ;
#146223 = CARTESIAN_POINT('Ctrl Pts',(-16.603381855895,12.2722652816386,132.319595696845)) ;
#146224 = CARTESIAN_POINT('Ctrl Pts',(-16.4963775783064,12.3599738875374,
132.040146264629)) ;
#146225 = CARTESIAN_POINT('Ctrl Pts',(-16.40080748811,12.522637910065,131.793927324611)) ;
#146226 = CARTESIAN_POINT('Ctrl Pts',(-16.321682629452,12.7508223350777,131.595969665067)) ;
#146227 = CARTESIAN_POINT('Ctrl Pts',(-16.2646694657802,13.0279566235447,
131.462655335791)) ;
#146228 = CARTESIAN_POINT('Ctrl Pts',(-16.2333313099527,13.3323088318152,
131.40421290911)) ;
#146229 = CARTESIAN_POINT('Ctrl Pts',(-16.2287969756995,13.6420774787073,
131.423958328797)) ;
#146230 = CARTESIAN_POINT('Ctrl Pts',(-16.2506794474225,13.9374078863426,
131.521003414245)) ;
#146231 = CARTESIAN_POINT('Ctrl Pts',(-16.2969248519444,14.1965319765984,
131.68929487346)) ;
#146232 = CARTESIAN_POINT('Ctrl Pts',(-16.3636006492136,14.3999725992787,
131.917314329854)) ;
#146233 = CARTESIAN_POINT('Ctrl Pts',(-16.4440741066575,14.5320840225921,
132.185279118148)) ;
#146234 = CARTESIAN_POINT('Ctrl Pts',(-16.5336015824952,14.5862914481746,
132.480055865257)) ;
#146235 = CARTESIAN_POINT('Ctrl Pts',(-16.6240180686935,14.5562373139742,
132.777363371128)) ;
#146236 = CARTESIAN_POINT('Ctrl Pts',(-16.7077455074844,14.446076002877,133.054911135565)) ;
#146237 = CARTESIAN_POINT('Ctrl Pts',(-16.7793513256384,14.2613118658137,
133.29736654614)) ;
#146238 = CARTESIAN_POINT('Ctrl Pts',(-16.8317784891826,14.0168342944467,
133.483655477492)) ;
#146239 = CARTESIAN_POINT('Ctrl Pts',(-16.8609906465943,13.7314084945653,
133.601972817066)) ;
#146240 = CARTESIAN_POINT('Ctrl Pts',(-16.8642673995017,13.4213927806631,
133.644806850243)) ;
#146241 = CARTESIAN_POINT('Ctrl Pts',(-16.8405564164842,13.1138964829047,
133.608540738459)) ;
#146242 = CARTESIAN_POINT('Ctrl Pts',(-16.7909211560091,12.8273574952535,
133.496655651129)) ;
#146243 = CARTESIAN_POINT('Ctrl Pts',(-16.7174808384362,12.5821904217373,
133.315441011606)) ;
#146244 = CARTESIAN_POINT('Ctrl Pts',(-16.6259022245879,12.3992406566731,
133.080982325427)) ;
#146245 = CARTESIAN_POINT('Ctrl Pts',(-16.5215735406818,12.2892635320147,
132.809278724701)) ;
#146246 = CARTESIAN_POINT('Ctrl Pts',(-16.4111844090626,12.2601882735182,
132.519864635604)) ;
#146247 = CARTESIAN_POINT('Ctrl Pts',(-16.3015215656193,12.3144490437337,
132.232684612256)) ;
#146248 = CARTESIAN_POINT('Ctrl Pts',(-16.200280314493,12.4481500552587,131.970047674196)) ;
#146249 = CARTESIAN_POINT('Ctrl Pts',(-16.113745113496,12.6515765738091,131.750375686591)) ;
#146250 = CARTESIAN_POINT('Ctrl Pts',(-16.047245764908,12.911209097722,131.589339229255)) ;
#146251 = CARTESIAN_POINT('Ctrl Pts',(-16.0053029062974,13.2069681338802,
131.499952091212)) ;
#146252 = CARTESIAN_POINT('Ctrl Pts',(-15.9898149035429,13.5165271467016,
131.487670352965)) ;
#146253 = CARTESIAN_POINT('Ctrl Pts',(-16.0012609274539,13.8224961920609,
131.554412215482)) ;
#146254 = CARTESIAN_POINT('Ctrl Pts',(-16.0380155767778,14.0973150821475,
131.694808594853)) ;
#146255 = CARTESIAN_POINT('Ctrl Pts',(-16.0966000359878,14.3244518569206,
131.899001803462)) ;
#146256 = CARTESIAN_POINT('Ctrl Pts',(-16.1726120215274,14.4877799967397,
132.15425492571)) ;
#146257 = CARTESIAN_POINT('Ctrl Pts',(-16.2592709157759,14.5742905029568,
132.440493252649)) ;
#146258 = CARTESIAN_POINT('Ctrl Pts',(-16.3500516483461,14.5785355282753,
132.738832343294)) ;
#146259 = CARTESIAN_POINT('Ctrl Pts',(-16.4374337885806,14.4999982805016,
133.02719053569)) ;
#146260 = CARTESIAN_POINT('Ctrl Pts',(-16.5145794309264,14.344757358462,133.28562333112)) ;
#146261 = CARTESIAN_POINT('Ctrl Pts',(-16.5755120854339,14.1223923332962,
133.49685600228)) ;
#146262 = CARTESIAN_POINT('Ctrl Pts',(-16.6145706090846,13.8510685521418,
133.644018688014)) ;
#146263 = CARTESIAN_POINT('Ctrl Pts',(-16.6286485860927,13.5484335086258,
133.718296216895)) ;
#146264 = CARTESIAN_POINT('Ctrl Pts',(-16.6158251047736,13.2370240609784,
133.713960203863)) ;
#146265 = CARTESIAN_POINT('Ctrl Pts',(-16.5763969172709,12.9391310692164,
133.631884681932)) ;
#146266 = CARTESIAN_POINT('Ctrl Pts',(-16.5123859500824,12.6756659712694,
133.478021949865)) ;
#146267 = CARTESIAN_POINT('Ctrl Pts',(-16.427629899397,12.4657027471288,133.263569069972)) ;
#146268 = CARTESIAN_POINT('Ctrl Pts',(-16.3275418282825,12.3244745287068,
133.004314673347)) ;
#146269 = CARTESIAN_POINT('Ctrl Pts',(-16.2186503349576,12.2619232724697,
132.719311023849)) ;
#146270 = CARTESIAN_POINT('Ctrl Pts',(-16.1077327239437,12.2825882461712,
132.428447362504)) ;
#146271 = CARTESIAN_POINT('Ctrl Pts',(-16.0025399530748,12.3846501373822,
132.154198120639)) ;
#146272 = CARTESIAN_POINT('Ctrl Pts',(-15.9092526009268,12.5611187376007,
131.914805460089)) ;
#146273 = CARTESIAN_POINT('Ctrl Pts',(-15.8339742586128,12.8001289118654,
131.72810568261)) ;
#146274 = CARTESIAN_POINT('Ctrl Pts',(-15.7817650558556,13.0829558583446,
131.608682645535)) ;
#146275 = CARTESIAN_POINT('Ctrl Pts',(-15.7552921984508,13.3903655570018,
131.564473572041)) ;
#146276 = CARTESIAN_POINT('Ctrl Pts',(-15.7558344968402,13.7001366244489,
131.599183864421)) ;
#146277 = CARTESIAN_POINT('Ctrl Pts',(-15.7825612660351,13.9898881879969,
131.710361207101)) ;
#146278 = CARTESIAN_POINT('Ctrl Pts',(-15.8329158030238,14.2391934604651,
131.890590896131)) ;
#146279 = CARTESIAN_POINT('Ctrl Pts',(-15.902293018607,14.4298567276207,132.126306082656)) ;
#146280 = CARTESIAN_POINT('Ctrl Pts',(-15.9860173892895,14.5492471456149,
132.404244702619)) ;
#146281 = CARTESIAN_POINT('Ctrl Pts',(-16.0754794895065,14.5868020959289,
132.698512209234)) ;
#146282 = CARTESIAN_POINT('Ctrl Pts',(-16.1651952894194,14.5417975153692,
132.99373545863)) ;
#146283 = CARTESIAN_POINT('Ctrl Pts',(-16.2474295569201,14.4162088209851,
133.26710820894)) ;
#146284 = CARTESIAN_POINT('Ctrl Pts',(-16.3154498224604,14.2204083214859,
133.498849848744)) ;
#146285 = CARTESIAN_POINT('Ctrl Pts',(-16.364198904732,13.9647701024183,133.674638082656)) ;
#146286 = CARTESIAN_POINT('Ctrl Pts',(-16.3885363920283,13.6739288437871,
133.77865485733)) ;
#146287 = CARTESIAN_POINT('Ctrl Pts',(-16.3867167940381,13.362328471029,133.806593586957)) ;
#146288 = CARTESIAN_POINT('Ctrl Pts',(-16.3579953894516,13.0574724209015,
133.755675698701)) ;
#146289 = CARTESIAN_POINT('Ctrl Pts',(-16.3035992847228,12.7770676806865,
133.629936979636)) ;
#146290 = CARTESIAN_POINT('Ctrl Pts',(-16.2263721109659,12.5427864739332,
133.437579054895)) ;
#146291 = CARTESIAN_POINT('Ctrl Pts',(-16.1323081173652,12.3731888111629,
133.195738527186)) ;
#146292 = CARTESIAN_POINT('Ctrl Pts',(-16.0260671047681,12.2773794230824,
132.918532204642)) ;
#146293 = CARTESIAN_POINT('Ctrl Pts',(-15.9148031459185,12.2641879723106,
132.626720167564)) ;
#146294 = CARTESIAN_POINT('Ctrl Pts',(-15.8067357439252,12.3335960858358,
132.34402376968)) ;
#146295 = CARTESIAN_POINT('Ctrl Pts',(-15.7074889808104,12.4815617101667,
132.087309224399)) ;
#146296 = CARTESIAN_POINT('Ctrl Pts',(-15.6244038386482,12.6968288003286,
131.87771937363)) ;
#146297 = CARTESIAN_POINT('Ctrl Pts',(-15.5624078276461,12.9642191171328,
131.729755714177)) ;
#146298 = CARTESIAN_POINT('Ctrl Pts',(-15.5252477520953,13.2637556030546,
131.654261303762)) ;
#146299 = CARTESIAN_POINT('Ctrl Pts',(-15.51483397363,13.5766924952844,131.657121610923)) ;
#146300 = CARTESIAN_POINT('Ctrl Pts',(-15.5310818707384,13.8753723119149,
131.737498039997)) ;
#146301 = CARTESIAN_POINT('Ctrl Pts',(-15.5723926579611,14.1446746282912,
131.891438338589)) ;
#146302 = CARTESIAN_POINT('Ctrl Pts',(-15.6347429021983,14.3606486732163,
132.106650818172)) ;
#146303 = CARTESIAN_POINT('Ctrl Pts',(-15.7130545539066,14.510078619128,132.368523960334)) ;
#146304 = CARTESIAN_POINT('Ctrl Pts',(-15.8014941644787,14.5815775918547,
132.66014711967)) ;
#146305 = CARTESIAN_POINT('Ctrl Pts',(-15.8916848447273,14.5700419701179,
132.956563000691)) ;
#146306 = CARTESIAN_POINT('Ctrl Pts',(-15.9780332182577,14.4761037327312,
133.242048390542)) ;
#146307 = CARTESIAN_POINT('Ctrl Pts',(-16.0524313118317,14.3074346005472,
133.492417860637)) ;
#146308 = CARTESIAN_POINT('Ctrl Pts',(-16.1096785706815,14.073572566118,133.6929606647)) ;
#146309 = CARTESIAN_POINT('Ctrl Pts',(-16.1440328164937,13.7966474057212,
133.82617193438)) ;
#146310 = CARTESIAN_POINT('Ctrl Pts',(-16.1531898468542,13.4894704941488,
133.886207558095)) ;
#146311 = CARTESIAN_POINT('Ctrl Pts',(-16.1353814446473,13.1800818047294,
133.867171716919)) ;
#146312 = CARTESIAN_POINT('Ctrl Pts',(-16.0908480942642,12.8853355952022,
133.770390398962)) ;
#146313 = CARTESIAN_POINT('Ctrl Pts',(-16.0227996234303,12.6318025855322,
133.604593537981)) ;
#146314 = CARTESIAN_POINT('Ctrl Pts',(-15.9348050473155,12.4337108442548,
133.380663235259)) ;
#146315 = CARTESIAN_POINT('Ctrl Pts',(-15.8324634579182,12.3064394695167,
133.114845627519)) ;
#146316 = CARTESIAN_POINT('Ctrl Pts',(-15.7223718021778,12.259467253753,132.826428638725)) ;
#146317 = CARTESIAN_POINT('Ctrl Pts',(-15.61237482116,12.2954707770716,132.538108209265)) ;
#146318 = CARTESIAN_POINT('Ctrl Pts',(-15.5080697165881,12.4135506736779,
132.266757070083)) ;
#146319 = CARTESIAN_POINT('Ctrl Pts',(-15.4186188949712,12.6014761688176,
132.038284950102)) ;
#146320 = CARTESIAN_POINT('Ctrl Pts',(-15.3471518246755,12.8505488617132,
131.862777352297)) ;
#146321 = CARTESIAN_POINT('Ctrl Pts',(-15.2996665374583,13.1393106642719,
131.75711736515)) ;
#146322 = CARTESIAN_POINT('Ctrl Pts',(-15.2782008897368,13.4495612707078,
131.727612757336)) ;
#146323 = CARTESIAN_POINT('Ctrl Pts',(-15.2838028221544,13.7566531065693,
131.777034142582)) ;
#146324 = CARTESIAN_POINT('Ctrl Pts',(-15.3152314145327,14.0404143617275,
131.901967955441)) ;
#146325 = CARTESIAN_POINT('Ctrl Pts',(-15.369451427365,14.2798568103851,132.093440892985)) ;
#146326 = CARTESIAN_POINT('Ctrl Pts',(-15.4424743213,14.4588607973601,132.34006491953)) ;
#146327 = CARTESIAN_POINT('Ctrl Pts',(-15.5270913631344,14.5622468207321,
132.620235903549)) ;
#146328 = CARTESIAN_POINT('Ctrl Pts',(-15.6176932560271,14.5847589284177,
132.918083757224)) ;
#146329 = CARTESIAN_POINT('Ctrl Pts',(-15.7063494799737,14.5239999294188,
133.210141637278)) ;
#146330 = CARTESIAN_POINT('Ctrl Pts',(-15.7864511470471,14.3842925756614,
133.4772918037)) ;
#146331 = CARTESIAN_POINT('Ctrl Pts',(-15.8512389369364,14.1758058754008,
133.699671458692)) ;
#146332 = CARTESIAN_POINT('Ctrl Pts',(-15.8955022373477,13.9130883833925,
133.862137470225)) ;
#146333 = CARTESIAN_POINT('Ctrl Pts',(-15.9151622120142,13.6151579335754,
133.952729954653)) ;
#146334 = CARTESIAN_POINT('Ctrl Pts',(-15.9082762302878,13.3050553518441,
133.965606077722)) ;
#146335 = CARTESIAN_POINT('Ctrl Pts',(-15.8745380140857,13.0018870987347,
133.900204241411)) ;
#146336 = CARTESIAN_POINT('Ctrl Pts',(-15.8156006902136,12.7291797299788,
133.761159559006)) ;
#146337 = CARTESIAN_POINT('Ctrl Pts',(-15.7349813594489,12.5061726224373,
133.558781374846)) ;
#146338 = CARTESIAN_POINT('Ctrl Pts',(-15.6378228988285,12.3489725905771,
133.308056494779)) ;
#146339 = CARTESIAN_POINT('Ctrl Pts',(-15.530157628843,12.2685649990364,133.026676899959)) ;
#146340 = CARTESIAN_POINT('Ctrl Pts',(-15.4191690111872,12.2709027590492,
132.735560480177)) ;
#146341 = CARTESIAN_POINT('Ctrl Pts',(-15.3118886403359,12.3558100715775,
132.455309412101)) ;
#146342 = CARTESIAN_POINT('Ctrl Pts',(-15.2154321019517,12.5172182560686,
132.206663476268)) ;
#146343 = CARTESIAN_POINT('Ctrl Pts',(-15.1360069622019,12.743270611073,132.007738327536)) ;
#146344 = CARTESIAN_POINT('Ctrl Pts',(-15.0784065694775,13.0180148278647,
131.872581445848)) ;
#146345 = CARTESIAN_POINT('Ctrl Pts',(-15.0460718420616,13.3228200342207,
131.811342068092)) ;
#146346 = CARTESIAN_POINT('Ctrl Pts',(-15.0407629253236,13.6334362897112,
131.828899103818)) ;
#146347 = CARTESIAN_POINT('Ctrl Pts',(-15.0619394460524,13.929416387864,131.923875769177)) ;
#146348 = CARTESIAN_POINT('Ctrl Pts',(-15.1073807241388,14.1891570751448,
132.089722319927)) ;
#146349 = CARTESIAN_POINT('Ctrl Pts',(-15.173454010653,14.3946402332245,132.315974310693)) ;
#146350 = CARTESIAN_POINT('Ctrl Pts',(-15.2539080167936,14.5295569095383,
132.584013104552)) ;
#146351 = CARTESIAN_POINT('Ctrl Pts',(-15.3433923457211,14.5858061320267,
132.878694551811)) ;
#146352 = CARTESIAN_POINT('Ctrl Pts',(-15.4333868311324,14.5585141684262,
133.174582671032)) ;
#146353 = CARTESIAN_POINT('Ctrl Pts',(-15.5178587338625,14.4500372102403,
133.45449302783)) ;
#146354 = CARTESIAN_POINT('Ctrl Pts',(-15.5894979700118,14.268202012558,133.696854115771)) ;
#146355 = CARTESIAN_POINT('Ctrl Pts',(-15.6427738964284,14.0250734119471,
133.885689485768)) ;
#146356 = CARTESIAN_POINT('Ctrl Pts',(-15.6727728261184,13.7389393518604,
134.006480982623)) ;
#146357 = CARTESIAN_POINT('Ctrl Pts',(-15.6767371037588,13.4311037036194,
134.051125055907)) ;
#146358 = CARTESIAN_POINT('Ctrl Pts',(-15.6539490538312,13.1229020321195,
134.017585741783)) ;
#146359 = CARTESIAN_POINT('Ctrl Pts',(-15.6044808421572,12.8333723855065,
133.906452712776)) ;
#146360 = CARTESIAN_POINT('Ctrl Pts',(-15.5324157004818,12.5895126789185,
133.72888592348)) ;
#146361 = CARTESIAN_POINT('Ctrl Pts',(-15.4410477383866,12.4035404975601,
133.495173240331)) ;
#146362 = CARTESIAN_POINT('Ctrl Pts',(-15.3370016478281,12.2914040477839,
133.224285529547)) ;
#146363 = CARTESIAN_POINT('Ctrl Pts',(-15.2265724109178,12.259812265838,132.934791476383)) ;
#146364 = CARTESIAN_POINT('Ctrl Pts',(-15.1167148533907,12.3118570241587,
132.647062652829)) ;
#146365 = CARTESIAN_POINT('Ctrl Pts',(-15.0153503169405,12.4430958843788,
132.383997857726)) ;
#146366 = CARTESIAN_POINT('Ctrl Pts',(-14.9282226918438,12.6447072746916,
132.162614685402)) ;
#146367 = CARTESIAN_POINT('Ctrl Pts',(-14.8611005268562,12.9030427397014,
131.999762417432)) ;
#146368 = CARTESIAN_POINT('Ctrl Pts',(-14.8184323691343,13.1970329557463,
131.90815170385)) ;
#146369 = CARTESIAN_POINT('Ctrl Pts',(-14.8021120725842,13.5084313502234,
131.893655409077)) ;
#146370 = CARTESIAN_POINT('Ctrl Pts',(-14.8126487298977,13.8121188302543,
131.957427584863)) ;
#146371 = CARTESIAN_POINT('Ctrl Pts',(-14.8488131994512,14.0900962513971,
132.096326161093)) ;
#146372 = CARTESIAN_POINT('Ctrl Pts',(-14.906849179233,14.31872996458,132.298901194403)) ;
#146373 = CARTESIAN_POINT('Ctrl Pts',(-14.9826658905836,14.484422730659,132.553674773777)) ;
#146374 = CARTESIAN_POINT('Ctrl Pts',(-15.0687615290781,14.5727758927101,
132.838129202005)) ;
#146375 = CARTESIAN_POINT('Ctrl Pts',(-15.1595314097221,14.5796460422286,
133.136442849992)) ;
#146376 = CARTESIAN_POINT('Ctrl Pts',(-15.2471499676657,14.5035865487986,
133.425498378262)) ;
#146377 = CARTESIAN_POINT('Ctrl Pts',(-15.3249952354103,14.3497062950072,
133.686114882967)) ;
#146378 = CARTESIAN_POINT('Ctrl Pts',(-15.3863099770745,14.1291329679128,
133.898413257429)) ;
#146379 = CARTESIAN_POINT('Ctrl Pts',(-15.4259580102792,13.8597726326946,
134.047208043984)) ;
#146380 = CARTESIAN_POINT('Ctrl Pts',(-15.4408276270026,13.557462341525,134.123830690541)) ;
#146381 = CARTESIAN_POINT('Ctrl Pts',(-15.4288290015519,13.2463365194833,
134.121865090828)) ;
#146382 = CARTESIAN_POINT('Ctrl Pts',(-15.3900832769036,12.9472973154242,
134.041838296647)) ;
#146383 = CARTESIAN_POINT('Ctrl Pts',(-15.3269663434198,12.6832077780023,
133.890488587454)) ;
#146384 = CARTESIAN_POINT('Ctrl Pts',(-15.2423563366193,12.4704982394892,
133.676617683217)) ;
#146385 = CARTESIAN_POINT('Ctrl Pts',(-15.1429697800888,12.3276823235439,
133.419290281986)) ;
#146386 = CARTESIAN_POINT('Ctrl Pts',(-15.034025656949,12.2625925201889,133.13420442183)) ;
#146387 = CARTESIAN_POINT('Ctrl Pts',(-14.9234367169736,12.280619224966,132.844183391634)) ;
#146388 = CARTESIAN_POINT('Ctrl Pts',(-14.8172926653969,12.3809214756921,
132.567369365397)) ;
#146389 = CARTESIAN_POINT('Ctrl Pts',(-14.7236180638936,12.556040128184,132.326867240074)) ;
#146390 = CARTESIAN_POINT('Ctrl Pts',(-14.6482354062739,12.7918901581632,
132.13964381325)) ;
#146391 = CARTESIAN_POINT('Ctrl Pts',(-14.5951060569914,13.0744209862709,
132.017630257796)) ;
#146392 = CARTESIAN_POINT('Ctrl Pts',(-14.5678958064568,13.3812416833702,
131.971242619165)) ;
#146393 = CARTESIAN_POINT('Ctrl Pts',(-14.5676629123474,13.6920797161949,
132.003775510376)) ;
#146394 = CARTESIAN_POINT('Ctrl Pts',(-14.5937720069054,13.9824941766623,
132.113143701743)) ;
#146395 = CARTESIAN_POINT('Ctrl Pts',(-14.6432359699896,14.2323227471641,
132.290628513848)) ;
#146396 = CARTESIAN_POINT('Ctrl Pts',(-14.7125811656434,14.4258243482768,
132.526452324439)) ;
#146397 = CARTESIAN_POINT('Ctrl Pts',(-14.795259617687,14.5465247223938,132.801035574304)) ;
#146398 = CARTESIAN_POINT('Ctrl Pts',(-14.8854602664183,14.5869806833893,
133.097778776266)) ;
#146399 = CARTESIAN_POINT('Ctrl Pts',(-14.9747767120066,14.5442058476213,
133.391648023159)) ;
#146400 = CARTESIAN_POINT('Ctrl Pts',(-15.0575087952615,14.4209679586328,
133.666531321112)) ;
#146401 = CARTESIAN_POINT('Ctrl Pts',(-15.126197252713,14.2257906516459,133.900366785556)) ;
#146402 = CARTESIAN_POINT('Ctrl Pts',(-15.1751094293477,13.9741287595616,
134.0762978741)) ;
#146403 = CARTESIAN_POINT('Ctrl Pts',(-15.2004336399251,13.6829512293512,
134.183353995983)) ;
#146404 = CARTESIAN_POINT('Ctrl Pts',(-15.1993756323757,13.37146650651,134.213520518934)) ;
#146405 = CARTESIAN_POINT('Ctrl Pts',(-15.1713543841638,13.0656058260286,
134.164711854186)) ;
#146406 = CARTESIAN_POINT('Ctrl Pts',(-15.1177667999354,12.7850334229127,
134.041241823021)) ;
#146407 = CARTESIAN_POINT('Ctrl Pts',(-15.0415227466297,12.5496672671412,
133.851637015263)) ;
#146408 = CARTESIAN_POINT('Ctrl Pts',(-14.9472330050277,12.3766688304073,
133.6093776058)) ;
#146409 = CARTESIAN_POINT('Ctrl Pts',(-14.8412230464008,12.2789529109886,
133.332834468204)) ;
#146410 = CARTESIAN_POINT('Ctrl Pts',(-14.7301884575418,12.2634413575716,
133.041638140652)) ;
#146411 = CARTESIAN_POINT('Ctrl Pts',(-14.6219272251922,12.3304157181155,
132.758377292415)) ;
#146412 = CARTESIAN_POINT('Ctrl Pts',(-14.5219985404227,12.4770344340702,
132.499791442207)) ;
#146413 = CARTESIAN_POINT('Ctrl Pts',(-14.438846216414,12.6896430839443,132.289838653687)) ;
#146414 = CARTESIAN_POINT('Ctrl Pts',(-14.3761485768327,12.9554492280344,
132.139803286405)) ;
#146415 = CARTESIAN_POINT('Ctrl Pts',(-14.3381869562118,13.2546656267019,
132.062005855799)) ;
#146416 = CARTESIAN_POINT('Ctrl Pts',(-14.3269455293927,13.5672375771819,
132.062407602021)) ;
#146417 = CARTESIAN_POINT('Ctrl Pts',(-14.3425168856217,13.8673528503954,
132.140905544475)) ;
#146418 = CARTESIAN_POINT('Ctrl Pts',(-14.3828967515057,14.1367236573279,
132.29196398836)) ;
#146419 = CARTESIAN_POINT('Ctrl Pts',(-14.4451848472743,14.3561277006207,
132.507257563492)) ;
#146420 = CARTESIAN_POINT('Ctrl Pts',(-14.5227670474163,14.5065131900063,
132.766820448084)) ;
#146421 = CARTESIAN_POINT('Ctrl Pts',(-14.6107831313521,14.5806176996537,
133.05713220862)) ;
#146422 = CARTESIAN_POINT('Ctrl Pts',(-14.7013079495486,14.5715966835969,
133.354635276761)) ;
#146423 = CARTESIAN_POINT('Ctrl Pts',(-14.7879149238724,14.4799160450286,
133.640882829627)) ;
#146424 = CARTESIAN_POINT('Ctrl Pts',(-14.8627484547883,14.3130125765193,
133.892550568111)) ;
#146425 = CARTESIAN_POINT('Ctrl Pts',(-14.9203410309572,14.0821691302311,
134.093924104667)) ;
#146426 = CARTESIAN_POINT('Ctrl Pts',(-14.9556762161135,13.8046644835193,
134.230212081773)) ;
#146427 = CARTESIAN_POINT('Ctrl Pts',(-14.9654957367169,13.4979410489725,
134.292173058157)) ;
#146428 = CARTESIAN_POINT('Ctrl Pts',(-14.9484649563509,13.1889483563346,
134.275353533116)) ;
#146429 = CARTESIAN_POINT('Ctrl Pts',(-14.9048261853835,12.8939178220345,
134.181116548468)) ;
#146430 = CARTESIAN_POINT('Ctrl Pts',(-14.8371220940663,12.6378239154038,
134.016474615887)) ;
#146431 = CARTESIAN_POINT('Ctrl Pts',(-14.7495889434489,12.4382802078468,
133.793875792288)) ;
#146432 = CARTESIAN_POINT('Ctrl Pts',(-14.6480169552468,12.3092349638881,
133.530167877536)) ;
#146433 = CARTESIAN_POINT('Ctrl Pts',(-14.5376692614152,12.2595575251469,
133.241117653867)) ;
#146434 = CARTESIAN_POINT('Ctrl Pts',(-14.427778786874,12.2934341319413,132.953057165944)) ;
#146435 = CARTESIAN_POINT('Ctrl Pts',(-14.3237109603852,12.4080333826879,
132.68220443888)) ;
#146436 = CARTESIAN_POINT('Ctrl Pts',(-14.2327451779127,12.5960960403323,
132.449682391364)) ;
#146437 = CARTESIAN_POINT('Ctrl Pts',(-14.1611034981059,12.843083593107,132.27352851092)) ;
#146438 = CARTESIAN_POINT('Ctrl Pts',(-14.1129483862029,13.1299282656209,
132.165812124441)) ;
#146439 = CARTESIAN_POINT('Ctrl Pts',(-14.0906153604259,13.4413370847319,
132.133926329516)) ;
#146440 = CARTESIAN_POINT('Ctrl Pts',(-14.095508888872,13.7480777848253,132.181202614268)) ;
#146441 = CARTESIAN_POINT('Ctrl Pts',(-14.1262007162312,14.0327532963684,
132.303976693101)) ;
#146442 = CARTESIAN_POINT('Ctrl Pts',(-14.1797772693749,14.2736050959338,
132.493548029621)) ;
#146443 = CARTESIAN_POINT('Ctrl Pts',(-14.2524010625293,14.4547314296563,
132.739031944661)) ;
#146444 = CARTESIAN_POINT('Ctrl Pts',(-14.336638830989,14.5602675742185,133.018049943511)) ;
#146445 = CARTESIAN_POINT('Ctrl Pts',(-14.4272467643914,14.5853381801731,
133.315940718168)) ;
#146446 = CARTESIAN_POINT('Ctrl Pts',(-14.5161472798392,14.5268295873478,
133.608748133879)) ;
#146447 = CARTESIAN_POINT('Ctrl Pts',(-14.5965447904337,14.3893357497607,
133.876742386898)) ;
#146448 = CARTESIAN_POINT('Ctrl Pts',(-14.6618705056622,14.1825586684621,
134.100706056936)) ;
#146449 = CARTESIAN_POINT('Ctrl Pts',(-14.7067541737627,13.9213687845982,
134.264954864919)) ;
#146450 = CARTESIAN_POINT('Ctrl Pts',(-14.7271543963702,13.6242447212575,
134.357704685103)) ;
#146451 = CARTESIAN_POINT('Ctrl Pts',(-14.7211456285122,13.3143403284212,
134.373125855975)) ;
#146452 = CARTESIAN_POINT('Ctrl Pts',(-14.6877800682829,13.0084389968774,
134.309066553768)) ;
#146453 = CARTESIAN_POINT('Ctrl Pts',(-14.6299975192762,12.7371908431784,
134.173086803152)) ;
#146454 = CARTESIAN_POINT('Ctrl Pts',(-14.5496928088176,12.5114337629303,
133.971763331707)) ;
#146455 = CARTESIAN_POINT('Ctrl Pts',(-14.4529519278489,12.3524149247727,
133.722234690091)) ;
#146456 = CARTESIAN_POINT('Ctrl Pts',(-14.3453600058295,12.2696327934899,
133.441110630772)) ;
#146457 = CARTESIAN_POINT('Ctrl Pts',(-14.234427034219,12.2697667408868,133.150138706916)) ;
#146458 = CARTESIAN_POINT('Ctrl Pts',(-14.1271125200423,12.3522197325102,
132.869734388649)) ;
#146459 = CARTESIAN_POINT('Ctrl Pts',(-14.0301995863744,12.5116177862274,
132.619773055426)) ;
#146460 = CARTESIAN_POINT('Ctrl Pts',(-13.9501762091569,12.736082772034,132.419111274269)) ;
#146461 = CARTESIAN_POINT('Ctrl Pts',(-13.8917651248445,13.0105747690242,
132.281683171717)) ;
#146462 = CARTESIAN_POINT('Ctrl Pts',(-13.8588245965078,13.3146279151312,
132.218642076419)) ;
#146463 = CARTESIAN_POINT('Ctrl Pts',(-13.8527482583037,13.6243832359542,
132.233854307006)) ;
#146464 = CARTESIAN_POINT('Ctrl Pts',(-13.8732412974156,13.9217978697246,
132.326914159419)) ;
#146465 = CARTESIAN_POINT('Ctrl Pts',(-13.9179550084861,14.1821018677862,
132.49054999663)) ;
#146466 = CARTESIAN_POINT('Ctrl Pts',(-13.9833931661554,14.3894123612741,
132.714916036037)) ;
#146467 = CARTESIAN_POINT('Ctrl Pts',(-14.0637817030373,14.5268848445949,
132.982873768876)) ;
#146468 = CARTESIAN_POINT('Ctrl Pts',(-14.1528323479007,14.585256166508,133.276178284537)) ;
#146469 = CARTESIAN_POINT('Ctrl Pts',(-14.2429398570225,14.5605921317333,
133.572412885749)) ;
#146470 = CARTESIAN_POINT('Ctrl Pts',(-14.327783437094,14.4542388415829,133.853450491557)) ;
#146471 = CARTESIAN_POINT('Ctrl Pts',(-14.3999222529145,14.2743936202259,
134.0972769669)) ;
#146472 = CARTESIAN_POINT('Ctrl Pts',(-14.4539010120162,14.0316377152924,
134.288294641039)) ;
#146473 = CARTESIAN_POINT('Ctrl Pts',(-14.4844118562612,13.7487556087195,
134.410315372432)) ;
#146474 = CARTESIAN_POINT('Ctrl Pts',(-14.4892042813141,13.4387761357976,
134.457654070306)) ;
#146475 = CARTESIAN_POINT('Ctrl Pts',(-14.4671820256302,13.131784657343,134.426188716179)) ;
#146476 = CARTESIAN_POINT('Ctrl Pts',(-14.4184322168324,12.8410201909971,
134.317189600133)) ;
#146477 = CARTESIAN_POINT('Ctrl Pts',(-14.3471581146507,12.5963886012332,
134.141844320016)) ;
#146478 = CARTESIAN_POINT('Ctrl Pts',(-14.2564618620465,12.4083250161853,
133.910052273587)) ;
#146479 = CARTESIAN_POINT('Ctrl Pts',(-14.1520011623539,12.2932606214,133.638173291436)) ;
#146480 = CARTESIAN_POINT('Ctrl Pts',(-14.0421766856827,12.2596773190563,
133.350284976464)) ;
#146481 = CARTESIAN_POINT('Ctrl Pts',(-13.9322527165775,12.3089369873083,
133.062341698944)) ;
#146482 = CARTESIAN_POINT('Ctrl Pts',(-13.8301386015647,12.4384179192494,
132.797214281908)) ;
#146483 = CARTESIAN_POINT('Ctrl Pts',(-13.7424630213586,12.6389284665683,
132.574292676507)) ;
#146484 = CARTESIAN_POINT('Ctrl Pts',(-13.6751976177911,12.8936369055523,
132.410742884719)) ;
#146485 = CARTESIAN_POINT('Ctrl Pts',(-13.6313872780528,13.1890353554826,
132.316056077679)) ;
#146486 = CARTESIAN_POINT('Ctrl Pts',(-13.6144296986492,13.4997524264947,
132.299631910272)) ;
#146487 = CARTESIAN_POINT('Ctrl Pts',(-13.6242379968661,13.8039809535807,
132.36129191884)) ;
#146488 = CARTESIAN_POINT('Ctrl Pts',(-13.6595439406371,14.0820722250227,
132.497554900109)) ;
#146489 = CARTESIAN_POINT('Ctrl Pts',(-13.7171465091326,14.3130041304952,
132.698959363541)) ;
#146490 = CARTESIAN_POINT('Ctrl Pts',(-13.7921690834901,14.4800545558914,
132.951253870289)) ;
#146491 = CARTESIAN_POINT('Ctrl Pts',(-13.8782618612207,14.5714592047604,
133.235802806482)) ;
#146492 = CARTESIAN_POINT('Ctrl Pts',(-13.9694643431118,14.580498376248,133.535542208868)) ;
#146493 = CARTESIAN_POINT('Ctrl Pts',(-14.0568328810788,14.5069052062207,
133.823709965073)) ;
#146494 = CARTESIAN_POINT('Ctrl Pts',(-14.1349602526621,14.355702929433,134.085089279489)) ;
#146495 = CARTESIAN_POINT('Ctrl Pts',(-14.1969497713178,14.1367618967332,
134.299396492582)) ;
#146496 = CARTESIAN_POINT('Ctrl Pts',(-14.237404970337,13.8680692745211,134.450619705146)) ;
#146497 = CARTESIAN_POINT('Ctrl Pts',(-14.2529793616564,13.5652241802336,
134.529418842422)) ;
#146498 = CARTESIAN_POINT('Ctrl Pts',(-14.2417810472862,13.2558695648544,
134.529599297919)) ;
#146499 = CARTESIAN_POINT('Ctrl Pts',(-14.2038516719789,12.9557645621013,
134.451991133453)) ;
#146500 = CARTESIAN_POINT('Ctrl Pts',(-14.1412339441975,12.6900041384903,
134.302163095143)) ;
#146501 = CARTESIAN_POINT('Ctrl Pts',(-14.0574802284815,12.4761054960812,
134.090679313259)) ;
#146502 = CARTESIAN_POINT('Ctrl Pts',(-13.9579371786143,12.330458638013,133.833068527865)) ;
#146503 = CARTESIAN_POINT('Ctrl Pts',(-13.8496782688255,12.2634381555471,
133.54982031889)) ;
#146504 = CARTESIAN_POINT('Ctrl Pts',(-13.7388026570335,12.2788783725225,
133.259036812535)) ;
#146505 = CARTESIAN_POINT('Ctrl Pts',(-13.6325440380496,12.3768660101259,
132.981849454036)) ;
#146506 = CARTESIAN_POINT('Ctrl Pts',(-13.5384385408213,12.5495630530058,
132.740061699469)) ;
#146507 = CARTESIAN_POINT('Ctrl Pts',(-13.4620222411141,12.7855771799242,
132.550040928112)) ;
#146508 = CARTESIAN_POINT('Ctrl Pts',(-13.4085967067531,13.0654345443907,
132.426953066734)) ;
#146509 = CARTESIAN_POINT('Ctrl Pts',(-13.3805216983346,13.3720089515071,
132.378066496838)) ;
#146510 = CARTESIAN_POINT('Ctrl Pts',(-13.3795024819761,13.6824357040732,
132.408234983439)) ;
#146511 = CARTESIAN_POINT('Ctrl Pts',(-13.4047254545112,13.9739144872618,
132.515011531949)) ;
#146512 = CARTESIAN_POINT('Ctrl Pts',(-13.4540326672827,14.2268633761364,
132.692297533583)) ;
#146513 = CARTESIAN_POINT('Ctrl Pts',(-13.5222172871231,14.4204385567601,
132.924403441781)) ;
#146514 = CARTESIAN_POINT('Ctrl Pts',(-13.6053169565128,14.5445800980489,
133.200525150877)) ;
#146515 = CARTESIAN_POINT('Ctrl Pts',(-13.69482615905,14.5868220517618,133.495019337852)) ;
#146516 = CARTESIAN_POINT('Ctrl Pts',(-13.7844155042831,14.5468039115563,
133.789745744027)) ;
#146517 = CARTESIAN_POINT('Ctrl Pts',(-13.8677245925165,14.4251034056979,
134.066432113054)) ;
#146518 = CARTESIAN_POINT('Ctrl Pts',(-13.9365735484581,14.2325286559051,
134.300597292436)) ;
#146519 = CARTESIAN_POINT('Ctrl Pts',(-13.9862491962028,13.9823226082249,
134.478779895998)) ;
#146520 = CARTESIAN_POINT('Ctrl Pts',(-14.0123354158408,13.6900857614276,
134.588264981185)) ;
#146521 = CARTESIAN_POINT('Ctrl Pts',(-14.0119899662679,13.3811329933267,
134.620262334553)) ;
#146522 = CARTESIAN_POINT('Ctrl Pts',(-13.9847818385877,13.0742211924304,
134.573896287318)) ;
#146523 = CARTESIAN_POINT('Ctrl Pts',(-13.9317957915014,12.7922255681548,
134.452228797447)) ;
#146524 = CARTESIAN_POINT('Ctrl Pts',(-13.8559061607881,12.5548593941868,
134.263739840746)) ;
#146525 = CARTESIAN_POINT('Ctrl Pts',(-13.7621081879575,12.3804086208566,
134.022872111731)) ;
#146526 = CARTESIAN_POINT('Ctrl Pts',(-13.6568430418593,12.2809059673708,
133.748352658593)) ;
#146527 = CARTESIAN_POINT('Ctrl Pts',(-13.5459745763591,12.2624888540407,
133.457603489706)) ;
#146528 = CARTESIAN_POINT('Ctrl Pts',(-13.4369161855102,12.3276777325191,
133.172213886062)) ;
#146529 = CARTESIAN_POINT('Ctrl Pts',(-13.3374729301959,12.4707929525642,
132.914754251539)) ;
#146530 = CARTESIAN_POINT('Ctrl Pts',(-13.2532224546344,12.6823314867526,
132.701770694391)) ;
#146531 = CARTESIAN_POINT('Ctrl Pts',(-13.1897158468007,12.9478032750239,
132.549469198639)) ;
#146532 = CARTESIAN_POINT('Ctrl Pts',(-13.1510598607848,13.2466924677811,
132.469674263269)) ;
#146533 = CARTESIAN_POINT('Ctrl Pts',(-13.1391280106543,13.5583773879723,
132.467970469312)) ;
#146534 = CARTESIAN_POINT('Ctrl Pts',(-13.1538931724907,13.8592557726353,
132.544120545162)) ;
#146535 = CARTESIAN_POINT('Ctrl Pts',(-13.1939100913278,14.1306426193177,
132.69425915972)) ;
#146536 = CARTESIAN_POINT('Ctrl Pts',(-13.2548897709125,14.3493760513521,
132.905341284647)) ;
#146537 = CARTESIAN_POINT('Ctrl Pts',(-13.3326860582841,14.5035317935641,
133.165820676624)) ;
#146538 = CARTESIAN_POINT('Ctrl Pts',(-13.4203463467915,14.5795845166173,
133.455011718327)) ;
#146539 = CARTESIAN_POINT('Ctrl Pts',(-13.5110703082225,14.5729335427119,
133.753170497346)) ;
#146540 = CARTESIAN_POINT('Ctrl Pts',(-13.5975957735246,14.4838964505683,
134.039056609727)) ;
#146541 = CARTESIAN_POINT('Ctrl Pts',(-13.6730510545671,14.3187457002778,
134.292624837989)) ;
#146542 = CARTESIAN_POINT('Ctrl Pts',(-13.7311388935659,14.0897675242826,
134.495402280048)) ;
#146543 = CARTESIAN_POINT('Ctrl Pts',(-13.7671907435101,13.8134082052382,
134.633785843446)) ;
#146544 = CARTESIAN_POINT('Ctrl Pts',(-13.7778201049083,13.5073935686165,
134.698088922778)) ;
#146545 = CARTESIAN_POINT('Ctrl Pts',(-13.7615250080495,13.1976576575877,
134.683484364323)) ;
#146546 = CARTESIAN_POINT('Ctrl Pts',(-13.7187953498613,12.902722923634,134.591795852928)) ;
#146547 = CARTESIAN_POINT('Ctrl Pts',(-13.6516732615037,12.6448108187769,
134.428909139399)) ;
#146548 = CARTESIAN_POINT('Ctrl Pts',(-13.5648664921481,12.4434495534872,
134.208369317472)) ;
#146549 = CARTESIAN_POINT('Ctrl Pts',(-13.4626553121334,12.3113759719957,
133.943100168444)) ;
#146550 = CARTESIAN_POINT('Ctrl Pts',(-13.3536253569139,12.2599503304337,
133.65753108676)) ;
#146551 = CARTESIAN_POINT('Ctrl Pts',(-13.2427727916244,12.291369325937,133.366928182391)) ;
#146552 = CARTESIAN_POINT('Ctrl Pts',(-13.1387408123296,12.4038516063155,
133.096088025424)) ;
#146553 = CARTESIAN_POINT('Ctrl Pts',(-13.0475728337221,12.5892626492753,
132.862876992473)) ;
#146554 = CARTESIAN_POINT('Ctrl Pts',(-12.9752337296433,12.8342966688913,
132.684656592976)) ;
#146555 = CARTESIAN_POINT('Ctrl Pts',(-12.9260719761757,13.122430564087,132.574248236609)) ;
#146556 = CARTESIAN_POINT('Ctrl Pts',(-12.903169430825,13.4307504301952,132.540394077624)) ;
#146557 = CARTESIAN_POINT('Ctrl Pts',(-12.9071698221294,13.7394115406098,
132.585230287027)) ;
#146558 = CARTESIAN_POINT('Ctrl Pts',(-12.9371825249084,14.0250582572476,
132.70601678198)) ;
#146559 = CARTESIAN_POINT('Ctrl Pts',(-12.9902636541603,14.2676857637035,
132.894194946137)) ;
#146560 = CARTESIAN_POINT('Ctrl Pts',(-13.0621016867333,14.4501343866895,
133.137238551309)) ;
#146561 = CARTESIAN_POINT('Ctrl Pts',(-13.1464951100618,14.5585281733049,
133.416884073386)) ;
#146562 = CARTESIAN_POINT('Ctrl Pts',(-13.2367905862396,14.5857500263022,
133.713765250072)) ;
#146563 = CARTESIAN_POINT('Ctrl Pts',(-13.3259831356628,14.5296138137444,
134.00748135074)) ;
#146564 = CARTESIAN_POINT('Ctrl Pts',(-13.4067107227604,14.3940563365778,
134.276446490129)) ;
#146565 = CARTESIAN_POINT('Ctrl Pts',(-13.4723758800565,14.1896705870724,
134.501311639645)) ;
#146566 = CARTESIAN_POINT('Ctrl Pts',(-13.5180007326056,13.929679500594,134.667754972924)) ;
#146567 = CARTESIAN_POINT('Ctrl Pts',(-13.5391833761276,13.6325613008054,
134.762866814829)) ;
#146568 = CARTESIAN_POINT('Ctrl Pts',(-13.5338310344752,13.3229079041448,
134.780193273664)) ;
#146569 = CARTESIAN_POINT('Ctrl Pts',(-13.5015813505085,13.0185266052724,
134.719157623872)) ;
#146570 = CARTESIAN_POINT('Ctrl Pts',(-13.4440778905347,12.7436673209471,
134.584275396389)) ;
#146571 = CARTESIAN_POINT('Ctrl Pts',(-13.364164023709,12.5164978313935,134.384108889428)) ;
#146572 = CARTESIAN_POINT('Ctrl Pts',(-13.2681841114513,12.3560839841268,
134.136678866392)) ;
#146573 = CARTESIAN_POINT('Ctrl Pts',(-13.1607863258833,12.2708854639731,
133.856129718307)) ;
#146574 = CARTESIAN_POINT('Ctrl Pts',(-13.0499975081774,12.2685612257957,
133.565537388716)) ;
#146575 = CARTESIAN_POINT('Ctrl Pts',(-12.9422815963831,12.3486010166685,
133.28401225927)) ;
#146576 = CARTESIAN_POINT('Ctrl Pts',(-12.8446122552014,12.5069431442139,
133.031987927892)) ;
#146577 = CARTESIAN_POINT('Ctrl Pts',(-12.7645613027564,12.7284060361604,
132.831033985649)) ;
#146578 = CARTESIAN_POINT('Ctrl Pts',(-12.705253017919,13.0024846524795,132.691088883789)) ;
#146579 = CARTESIAN_POINT('Ctrl Pts',(-12.6716419222305,13.3053157268251,
132.6260084913)) ;
#146580 = CARTESIAN_POINT('Ctrl Pts',(-12.6647810266749,13.6156287863426,
132.638985809996)) ;
#146581 = CARTESIAN_POINT('Ctrl Pts',(-12.6843936920298,13.9128850712382,
132.729361876897)) ;
#146582 = CARTESIAN_POINT('Ctrl Pts',(-12.7288341766348,14.1766185876755,
132.892474897501)) ;
#146583 = CARTESIAN_POINT('Ctrl Pts',(-12.7937162436498,14.3847399014371,
133.115126688338)) ;
#146584 = CARTESIAN_POINT('Ctrl Pts',(-12.8734691079153,14.5238361204557,
133.381113923067)) ;
#146585 = CARTESIAN_POINT('Ctrl Pts',(-12.9622495766178,14.5847743037998,
133.673586233755)) ;
#146586 = CARTESIAN_POINT('Ctrl Pts',(-13.0527820859063,14.562330930931,133.971202261872)) ;
#146587 = CARTESIAN_POINT('Ctrl Pts',(-13.1377615990323,14.4584177990408,
134.252575475658)) ;
#146588 = CARTESIAN_POINT('Ctrl Pts',(-13.2105950760868,14.2791868588028,
134.498607925464)) ;
#146589 = CARTESIAN_POINT('Ctrl Pts',(-13.2645059669396,14.0415186925473,
134.688953563355)) ;
#146590 = CARTESIAN_POINT('Ctrl Pts',(-13.2961690615346,13.7564325224017,
134.814741376284)) ;
#146591 = CARTESIAN_POINT('Ctrl Pts',(-13.3017064519511,13.4495648486799,
134.863943731619)) ;
#146592 = CARTESIAN_POINT('Ctrl Pts',(-13.2802760759038,13.1394167822153,
134.83453108885)) ;
#146593 = CARTESIAN_POINT('Ctrl Pts',(-13.2328043241826,12.8508801279426,
134.728890639548)) ;
#146594 = CARTESIAN_POINT('Ctrl Pts',(-13.1616530962339,12.6022770183791,
134.554205749892)) ;
#146595 = CARTESIAN_POINT('Ctrl Pts',(-13.0714541468405,12.4127865792607,
134.323823666599)) ;
#146596 = CARTESIAN_POINT('Ctrl Pts',(-12.9673285301535,12.2953916608247,
134.052917908426)) ;
#146597 = CARTESIAN_POINT('Ctrl Pts',(-12.8573500994989,12.2594835078991,
133.764648208685)) ;
#146598 = CARTESIAN_POINT('Ctrl Pts',(-12.7475293975293,12.3065006928956,
133.476944904768)) ;
#146599 = CARTESIAN_POINT('Ctrl Pts',(-12.6453580244396,12.4331949975966,
133.211553226454)) ;
#146600 = CARTESIAN_POINT('Ctrl Pts',(-12.5568504774939,12.6325251245457,
132.986323708861)) ;
#146601 = CARTESIAN_POINT('Ctrl Pts',(-12.4890879876667,12.8854154202419,
132.821256063685)) ;
#146602 = CARTESIAN_POINT('Ctrl Pts',(-12.4444998174266,13.1803567120122,
132.724340428263)) ;
#146603 = CARTESIAN_POINT('Ctrl Pts',(-12.4267857836901,13.4893561619414,
132.705540842095)) ;
#146604 = CARTESIAN_POINT('Ctrl Pts',(-12.4357494783633,13.7954471105094,
132.764878099224)) ;
#146605 = CARTESIAN_POINT('Ctrl Pts',(-12.470514760125,14.0751705649909,132.899636718351)) ;
#146606 = CARTESIAN_POINT('Ctrl Pts',(-12.5273949578635,14.3069080842483,
133.098834382941)) ;
#146607 = CARTESIAN_POINT('Ctrl Pts',(-12.6018932112712,14.4762413340772,
133.349575995276)) ;
#146608 = CARTESIAN_POINT('Ctrl Pts',(-12.6884680140324,14.5702449830263,
133.635795840671)) ;
#146609 = CARTESIAN_POINT('Ctrl Pts',(-12.7787954726246,14.5813885604022,
133.932662954814)) ;
#146610 = CARTESIAN_POINT('Ctrl Pts',(-12.8668280999648,14.5100796553899,
134.222948212301)) ;
#146611 = CARTESIAN_POINT('Ctrl Pts',(-12.9454272270282,14.3602444697485,
134.48577132055)) ;
#146612 = CARTESIAN_POINT('Ctrl Pts',(-13.0077584665022,14.1432531479422,
134.701009749057)) ;
#146613 = CARTESIAN_POINT('Ctrl Pts',(-13.04871586247,13.8766589305714,134.853588406275)) ;
#146614 = CARTESIAN_POINT('Ctrl Pts',(-13.0651171404783,13.575471110015,134.934700187327)) ;
#146615 = CARTESIAN_POINT('Ctrl Pts',(-13.0547234569409,13.2645667872771,
134.937392906819)) ;
#146616 = CARTESIAN_POINT('Ctrl Pts',(-13.0173984270287,12.9634276879521,
134.861599179382)) ;
#146617 = CARTESIAN_POINT('Ctrl Pts',(-12.9556055647511,12.6972348288673,
134.714086108156)) ;
#146618 = CARTESIAN_POINT('Ctrl Pts',(-12.8725122568232,12.4817230037899,
134.504497176081)) ;
#146619 = CARTESIAN_POINT('Ctrl Pts',(-12.773428134007,12.3338051645045,134.248207978296)) ;
#146620 = CARTESIAN_POINT('Ctrl Pts',(-12.664997671945,12.2641455947444,133.964564222402)) ;
#146621 = CARTESIAN_POINT('Ctrl Pts',(-12.5541644274789,12.2773535863406,
133.673882486229)) ;
#146622 = CARTESIAN_POINT('Ctrl Pts',(-12.4479133266097,12.3726335000392,
133.396633128579)) ;
#146623 = CARTESIAN_POINT('Ctrl Pts',(-12.3532329844408,12.5434758841393,
133.153213940141)) ;
#146624 = CARTESIAN_POINT('Ctrl Pts',(-12.2764208543176,12.7769498129424,
132.961924438896)) ;
#146625 = CARTESIAN_POINT('Ctrl Pts',(-12.2219612543097,13.0568800238177,
132.835964380683)) ;
#146626 = CARTESIAN_POINT('Ctrl Pts',(-12.1931492705949,13.3636449854545,
132.784985244105)) ;
#146627 = CARTESIAN_POINT('Ctrl Pts',(-12.1913843931622,13.6733774781512,
132.812881465914)) ;
#146628 = CARTESIAN_POINT('Ctrl Pts',(-12.2157901192583,13.9654381108949,
132.917236471078)) ;
#146629 = CARTESIAN_POINT('Ctrl Pts',(-12.2644884683387,14.2203012801684,
133.092791679479)) ;
#146630 = CARTESIAN_POINT('Ctrl Pts',(-12.3323691648357,14.4159470499748,
133.324078571007)) ;
#146631 = CARTESIAN_POINT('Ctrl Pts',(-12.4146312012186,14.541694367896,133.597549977849)) ;
#146632 = CARTESIAN_POINT('Ctrl Pts',(-12.504384005875,14.5869018897487,133.892893860253)) ;
#146633 = CARTESIAN_POINT('Ctrl Pts',(-12.5942025143602,14.5489491309812,
134.188340585277)) ;
#146634 = CARTESIAN_POINT('Ctrl Pts',(-12.6775333194475,14.4300240468882,
134.464972796832)) ;
#146635 = CARTESIAN_POINT('Ctrl Pts',(-12.7471511772361,14.2387296194583,
134.701508328912)) ;
#146636 = CARTESIAN_POINT('Ctrl Pts',(-12.7973346677689,13.9899468992174,
134.881150877303)) ;
#146637 = CARTESIAN_POINT('Ctrl Pts',(-12.8240718619797,13.7002922296482,
134.992355286073)) ;
#146638 = CARTESIAN_POINT('Ctrl Pts',(-12.8246776599493,13.3909003011237,
135.027208892331)) ;
#146639 = CARTESIAN_POINT('Ctrl Pts',(-12.7980515837342,13.0819914193172,
134.982715951971)) ;
#146640 = CARTESIAN_POINT('Ctrl Pts',(-12.7458845974443,12.8000707089261,
134.863325630578)) ;
#146641 = CARTESIAN_POINT('Ctrl Pts',(-12.6708702798026,12.561613461146,134.677305827493)) ;
#146642 = CARTESIAN_POINT('Ctrl Pts',(-12.5773543002011,12.3844498728761,
134.437337291221)) ;
#146643 = CARTESIAN_POINT('Ctrl Pts',(-12.471806174944,12.2824628123426,134.162150550627)) ;
#146644 = CARTESIAN_POINT('Ctrl Pts',(-12.3615665234835,12.2618989630133,
133.873062538303)) ;
#146645 = CARTESIAN_POINT('Ctrl Pts',(-12.2522093017518,12.3245801672036,
133.586841008912)) ;
#146646 = CARTESIAN_POINT('Ctrl Pts',(-12.1524030524764,12.4655890286878,
133.328320986593)) ;
#146647 = CARTESIAN_POINT('Ctrl Pts',(-12.0676400812886,12.6753258983896,
133.113838294116)) ;
#146648 = CARTESIAN_POINT('Ctrl Pts',(-12.0035262345311,12.9389696147355,
132.959703405746)) ;
#146649 = CARTESIAN_POINT('Ctrl Pts',(-11.9640514725537,13.2377442398154,
132.877585546536)) ;
#146650 = CARTESIAN_POINT('Ctrl Pts',(-11.951288825654,13.5478078732814,132.87328298619)) ;
#146651 = CARTESIAN_POINT('Ctrl Pts',(-11.9653467927663,13.8515136096922,
132.947613389739)) ;
#146652 = CARTESIAN_POINT('Ctrl Pts',(-12.0046007635559,14.1231097969316,
133.095406436556)) ;
#146653 = CARTESIAN_POINT('Ctrl Pts',(-12.0651067843966,14.3439547255393,
133.305165205202)) ;
#146654 = CARTESIAN_POINT('Ctrl Pts',(-12.1423042997912,14.4998917409251,
133.563806490907)) ;
#146655 = CARTESIAN_POINT('Ctrl Pts',(-12.2300647068386,14.5786386561727,
133.853407609955)) ;
#146656 = CARTESIAN_POINT('Ctrl Pts',(-12.3207510678068,14.574267489829,134.151433421108)) ;
#146657 = CARTESIAN_POINT('Ctrl Pts',(-12.4075572935563,14.4873446647109,
134.438170951734)) ;
#146658 = CARTESIAN_POINT('Ctrl Pts',(-12.4831747499324,14.3247913257021,
134.692103132489)) ;
#146659 = CARTESIAN_POINT('Ctrl Pts',(-12.542042439971,14.0970301472897,134.897242195035)) ;
#146660 = CARTESIAN_POINT('Ctrl Pts',(-12.5788106537289,13.820492300365,135.037850166732)) ;
#146661 = CARTESIAN_POINT('Ctrl Pts',(-12.5900817230675,13.5164548784845,
135.103861743899)) ;
#146662 = CARTESIAN_POINT('Ctrl Pts',(-12.5745635456089,13.2060699162722,
135.091583899804)) ;
#146663 = CARTESIAN_POINT('Ctrl Pts',(-12.5324969640781,12.9102232065258,
135.001850755175)) ;
#146664 = CARTESIAN_POINT('Ctrl Pts',(-12.4658520839193,12.6507291243944,
134.840407336644)) ;
#146665 = CARTESIAN_POINT('Ctrl Pts',(-12.3798223962499,12.4485585440169,
134.622012614771)) ;
#146666 = CARTESIAN_POINT('Ctrl Pts',(-12.2785035906128,12.3145373722517,
134.359188397339)) ;
#146667 = CARTESIAN_POINT('Ctrl Pts',(-12.1689761661125,12.2601564021124,
134.072361071585)) ;
#146668 = CARTESIAN_POINT('Ctrl Pts',(-12.0580855205296,12.2893926148143,
133.781636394683)) ;
#146669 = CARTESIAN_POINT('Ctrl Pts',(-11.9537967692143,12.3994366791386,
133.510032588238)) ;
#146670 = CARTESIAN_POINT('Ctrl Pts',(-11.8618106924454,12.5839727255082,
133.274581017316)) ;
#146671 = CARTESIAN_POINT('Ctrl Pts',(-11.7892711806775,12.8264920327129,
133.095617229562)) ;
#146672 = CARTESIAN_POINT('Ctrl Pts',(-11.7392658398382,13.1141225858941,
132.982797082773)) ;
#146673 = CARTESIAN_POINT('Ctrl Pts',(-11.7235540209465,13.3194871424456,
132.958938670686)) ;
#146674 = CARTESIAN_POINT('Ctrl Pts',(-11.7201408679865,13.4222384841719,
132.959988719826)) ;
#146675 = CARTESIAN_POINT('Ctrl Pts',(-33.3012851433477,13.1368456608817,
127.965137779698)) ;
#146676 = CARTESIAN_POINT('Ctrl Pts',(-33.3005108918432,13.1302434176427,
127.963606955475)) ;
#146677 = CARTESIAN_POINT('Ctrl Pts',(-33.2878768464891,13.0249710001428,
127.93838217985)) ;
#146678 = CARTESIAN_POINT('Ctrl Pts',(-33.253359927881,12.826301888656,127.860524464141)) ;
#146679 = CARTESIAN_POINT('Ctrl Pts',(-33.180558749092,12.5833995163819,127.680876334219)) ;
#146680 = CARTESIAN_POINT('Ctrl Pts',(-33.0890149852688,12.3996267668574,
127.446559868317)) ;
#146681 = CARTESIAN_POINT('Ctrl Pts',(-32.9840141902935,12.289073168245,127.173099510327)) ;
#146682 = CARTESIAN_POINT('Ctrl Pts',(-32.8740536137075,12.2602312941192,
126.884806111823)) ;
#146683 = CARTESIAN_POINT('Ctrl Pts',(-32.7642172899274,12.3144254424815,
126.597172510079)) ;
#146684 = CARTESIAN_POINT('Ctrl Pts',(-32.6630373208337,12.4480642715863,
126.334692293817)) ;
#146685 = CARTESIAN_POINT('Ctrl Pts',(-32.576446271887,12.6516399513856,126.114881618259)) ;
#146686 = CARTESIAN_POINT('Ctrl Pts',(-32.5101373823508,12.9104452496318,
125.954300029618)) ;
#146687 = CARTESIAN_POINT('Ctrl Pts',(-32.4680947198103,13.2058492015505,
125.864596954978)) ;
#146688 = CARTESIAN_POINT('Ctrl Pts',(-32.4525008094708,13.5166184921212,
125.852133747766)) ;
#146689 = CARTESIAN_POINT('Ctrl Pts',(-32.4639876735504,13.8224100223415,
125.918979463408)) ;
#146690 = CARTESIAN_POINT('Ctrl Pts',(-32.5006141983944,14.0967865008827,
126.058936460803)) ;
#146691 = CARTESIAN_POINT('Ctrl Pts',(-32.5593185399482,14.3244562986112,
126.263555841175)) ;
#146692 = CARTESIAN_POINT('Ctrl Pts',(-32.6351145538659,14.4874741997871,
126.518089823437)) ;
#146693 = CARTESIAN_POINT('Ctrl Pts',(-32.7220896777706,14.5744204937736,
126.805378368018)) ;
#146694 = CARTESIAN_POINT('Ctrl Pts',(-32.8128052621322,14.5784621737365,
127.10350123506)) ;
#146695 = CARTESIAN_POINT('Ctrl Pts',(-32.900132936634,14.5000469778991,127.391677525357)) ;
#146696 = CARTESIAN_POINT('Ctrl Pts',(-32.977330701875,14.3445727249932,127.650295149581)) ;
#146697 = CARTESIAN_POINT('Ctrl Pts',(-33.0381556098337,14.122833835347,127.861131305989)) ;
#146698 = CARTESIAN_POINT('Ctrl Pts',(-33.0773675715877,13.8501516984393,
128.008903812172)) ;
#146699 = CARTESIAN_POINT('Ctrl Pts',(-33.0913163097499,13.5490423779197,
128.082630492233)) ;
#146700 = CARTESIAN_POINT('Ctrl Pts',(-33.0786099195809,13.2374717045801,
128.078653893675)) ;
#146701 = CARTESIAN_POINT('Ctrl Pts',(-33.0390139547928,12.9386844676289,
127.996192116606)) ;
#146702 = CARTESIAN_POINT('Ctrl Pts',(-32.975229814111,12.6761377246457,127.842873877758)) ;
#146703 = CARTESIAN_POINT('Ctrl Pts',(-32.8903638726636,12.4657586790897,
127.628156905795)) ;
#146704 = CARTESIAN_POINT('Ctrl Pts',(-32.7904652117052,12.3246285674056,
127.369395546857)) ;
#146705 = CARTESIAN_POINT('Ctrl Pts',(-32.6811498208371,12.2619062239342,
127.083285478092)) ;
#146706 = CARTESIAN_POINT('Ctrl Pts',(-32.5707291608164,12.282438835861,126.793720932159)) ;
#146707 = CARTESIAN_POINT('Ctrl Pts',(-32.4649957249968,12.3848777571664,
126.518059092902)) ;
#146708 = CARTESIAN_POINT('Ctrl Pts',(-32.3718774118045,12.5614991790326,
126.279126097839)) ;
#146709 = CARTESIAN_POINT('Ctrl Pts',(-32.2967868140066,12.7995868191894,
126.092866229788)) ;
#146710 = CARTESIAN_POINT('Ctrl Pts',(-32.2443216753795,13.084029998422,125.972880573089)) ;
#146711 = CARTESIAN_POINT('Ctrl Pts',(-32.2180641227937,13.3899587273314,
125.929135151855)) ;
#146712 = CARTESIAN_POINT('Ctrl Pts',(-32.2184913394978,13.6996411393276,
125.963497562112)) ;
#146713 = CARTESIAN_POINT('Ctrl Pts',(-32.2453325092191,13.9903747350237,
126.075123804051)) ;
#146714 = CARTESIAN_POINT('Ctrl Pts',(-32.2956569729903,14.2393240390192,
126.255222855766)) ;
#146715 = CARTESIAN_POINT('Ctrl Pts',(-32.3650841831038,14.429840029191,126.4910956906)) ;
#146716 = CARTESIAN_POINT('Ctrl Pts',(-32.448163738453,14.5487685207819,126.766909226846)) ;
#146717 = CARTESIAN_POINT('Ctrl Pts',(-32.5383659554756,14.5869290462078,
127.063619096291)) ;
#146718 = CARTESIAN_POINT('Ctrl Pts',(-32.6278128226021,14.5417666879112,
127.357958778643)) ;
#146719 = CARTESIAN_POINT('Ctrl Pts',(-32.7101561099796,14.4163781206347,
127.631674948744)) ;
#146720 = CARTESIAN_POINT('Ctrl Pts',(-32.7783498364979,14.2194053236093,
127.864061771658)) ;
#146721 = CARTESIAN_POINT('Ctrl Pts',(-32.8266393254659,13.9666437025949,
128.038144830637)) ;
#146722 = CARTESIAN_POINT('Ctrl Pts',(-32.851292510915,13.6737230311142,128.143343661379)) ;
#146723 = CARTESIAN_POINT('Ctrl Pts',(-32.8494473020655,13.3629183159293,
128.171112807256)) ;
#146724 = CARTESIAN_POINT('Ctrl Pts',(-32.8206607882665,13.0570541461369,
128.120117610136)) ;
#146725 = CARTESIAN_POINT('Ctrl Pts',(-32.7663361849904,12.7772474401736,
127.994519431102)) ;
#146726 = CARTESIAN_POINT('Ctrl Pts',(-32.6890886758744,12.542768054334,127.802123885512)) ;
#146727 = CARTESIAN_POINT('Ctrl Pts',(-32.5949608164813,12.3730788461159,
127.560114935571)) ;
#146728 = CARTESIAN_POINT('Ctrl Pts',(-32.4886545346452,12.2773830517675,
127.282736009967)) ;
#146729 = CARTESIAN_POINT('Ctrl Pts',(-32.3777178343667,12.2641121727855,
126.991780273813)) ;
#146730 = CARTESIAN_POINT('Ctrl Pts',(-32.269276455156,12.3337583329821,126.708108351852)) ;
#146731 = CARTESIAN_POINT('Ctrl Pts',(-32.1703548633399,12.4813160749921,
126.452235712459)) ;
#146732 = CARTESIAN_POINT('Ctrl Pts',(-32.0871433542004,12.6966779854676,
126.242314410242)) ;
#146733 = CARTESIAN_POINT('Ctrl Pts',(-32.0251441770006,12.964058481658,126.094337296347)) ;
#146734 = CARTESIAN_POINT('Ctrl Pts',(-31.9880271005956,13.2633621106785,
126.01894761863)) ;
#146735 = CARTESIAN_POINT('Ctrl Pts',(-31.9774841904215,13.5752568041736,
126.021313511474)) ;
#146736 = CARTESIAN_POINT('Ctrl Pts',(-31.9939116345013,13.8766502651513,
126.102521569776)) ;
#146737 = CARTESIAN_POINT('Ctrl Pts',(-32.0349700208106,14.1438626179913,
126.255472982178)) ;
#146738 = CARTESIAN_POINT('Ctrl Pts',(-32.0975480361989,14.3611558339141,
126.471516188421)) ;
#146739 = CARTESIAN_POINT('Ctrl Pts',(-32.1760316525525,14.5102070990302,
126.733925687538)) ;
#146740 = CARTESIAN_POINT('Ctrl Pts',(-32.2636499274558,14.5813677878946,
127.022848150248)) ;
#146741 = CARTESIAN_POINT('Ctrl Pts',(-32.3544916008583,14.5701315008181,
127.321407441068)) ;
#146742 = CARTESIAN_POINT('Ctrl Pts',(-32.4408443777509,14.4759919036324,
127.606902737038)) ;
#146743 = CARTESIAN_POINT('Ctrl Pts',(-32.5153098957686,14.3066892752371,
127.857540673623)) ;
#146744 = CARTESIAN_POINT('Ctrl Pts',(-32.572093511354,14.0751878826871,128.056411954729)) ;
#146745 = CARTESIAN_POINT('Ctrl Pts',(-32.606801906154,13.7962286869884,128.19092493514)) ;
#146746 = CARTESIAN_POINT('Ctrl Pts',(-32.6159392974398,13.4897393053989,
128.250814127221)) ;
#146747 = CARTESIAN_POINT('Ctrl Pts',(-32.5978520725212,13.1781056984616,
128.231218495251)) ;
#146748 = CARTESIAN_POINT('Ctrl Pts',(-32.5538717207945,12.8871394706553,
128.135620981617)) ;
#146749 = CARTESIAN_POINT('Ctrl Pts',(-32.4854748637565,12.6313543123433,
127.969059162825)) ;
#146750 = CARTESIAN_POINT('Ctrl Pts',(-32.3972131808472,12.4333423882355,
127.744400910633)) ;
#146751 = CARTESIAN_POINT('Ctrl Pts',(-32.2954852260653,12.3067788270204,
127.480184029957)) ;
#146752 = CARTESIAN_POINT('Ctrl Pts',(-32.1851063871179,12.2592790115486,
127.191016833271)) ;
#146753 = CARTESIAN_POINT('Ctrl Pts',(-32.0747522042955,12.2958890743791,
126.901769496605)) ;
#146754 = CARTESIAN_POINT('Ctrl Pts',(-31.9714548460177,12.412515962942,126.633025776648)) ;
#146755 = CARTESIAN_POINT('Ctrl Pts',(-31.8811186931709,12.6017795206287,
126.402264650772)) ;
#146756 = CARTESIAN_POINT('Ctrl Pts',(-31.8098352699652,12.850882040149,126.227256401551)) ;
#146757 = CARTESIAN_POINT('Ctrl Pts',(-31.762405072303,13.1389626258658,126.121689692541)) ;
#146758 = CARTESIAN_POINT('Ctrl Pts',(-31.7408679606482,13.4502019142914,
126.092079042597)) ;
#146759 = CARTESIAN_POINT('Ctrl Pts',(-31.7465832117125,13.7571545177325,
126.141825730537)) ;
#146760 = CARTESIAN_POINT('Ctrl Pts',(-31.7778345667064,14.0399279671086,
126.266112338252)) ;
#146761 = CARTESIAN_POINT('Ctrl Pts',(-31.832377419942,14.2804627439869,126.458703858811)) ;
#146762 = CARTESIAN_POINT('Ctrl Pts',(-31.9047636968708,14.4580430421026,
126.703179136283)) ;
#146763 = CARTESIAN_POINT('Ctrl Pts',(-31.9898069250853,14.5623041816762,
126.984785548002)) ;
#146764 = CARTESIAN_POINT('Ctrl Pts',(-32.0801395493773,14.5848738304735,
127.281737987156)) ;
#146765 = CARTESIAN_POINT('Ctrl Pts',(-32.1694325535098,14.5236285286568,
127.575900885035)) ;
#146766 = CARTESIAN_POINT('Ctrl Pts',(-32.2490892414091,14.3842858734187,
127.841584547318)) ;
#146767 = CARTESIAN_POINT('Ctrl Pts',(-32.3139443197535,14.176003666528,128.064165461533)) ;
#146768 = CARTESIAN_POINT('Ctrl Pts',(-32.3582858943054,13.9123645540699,
128.226961175517)) ;
#146769 = CARTESIAN_POINT('Ctrl Pts',(-32.3778469050749,13.6155079184588,
128.317141856664)) ;
#146770 = CARTESIAN_POINT('Ctrl Pts',(-32.3710005417205,13.3048786639477,
128.330191354686)) ;
#146771 = CARTESIAN_POINT('Ctrl Pts',(-32.337151787263,13.0013158611206,128.264513177756)) ;
#146772 = CARTESIAN_POINT('Ctrl Pts',(-32.2782558550222,12.7290184859203,
128.125547347738)) ;
#146773 = CARTESIAN_POINT('Ctrl Pts',(-32.1975975430178,12.5059453059748,
127.923067950598)) ;
#146774 = CARTESIAN_POINT('Ctrl Pts',(-32.1004419981188,12.3489356704195,
127.672343005709)) ;
#146775 = CARTESIAN_POINT('Ctrl Pts',(-31.9930053142448,12.2685725679141,
127.391562275537)) ;
#146776 = CARTESIAN_POINT('Ctrl Pts',(-31.8816137190197,12.2709800275436,
127.099390481669)) ;
#146777 = CARTESIAN_POINT('Ctrl Pts',(-31.7746039123214,12.3558597307768,
126.819849151034)) ;
#146778 = CARTESIAN_POINT('Ctrl Pts',(-31.6780754812207,12.5173148963124,
126.571016266393)) ;
#146779 = CARTESIAN_POINT('Ctrl Pts',(-31.5986036870283,12.7436533200346,
126.371982999436)) ;
#146780 = CARTESIAN_POINT('Ctrl Pts',(-31.5410722847427,13.018439069694,126.237023225013)) ;
#146781 = CARTESIAN_POINT('Ctrl Pts',(-31.5088077865552,13.3224259013371,
126.175900279904)) ;
#146782 = CARTESIAN_POINT('Ctrl Pts',(-31.5034619367311,13.6337496474671,
126.193425485829)) ;
#146783 = CARTESIAN_POINT('Ctrl Pts',(-31.5246981020183,13.9298381651934,
126.288591098426)) ;
#146784 = CARTESIAN_POINT('Ctrl Pts',(-31.5701771718773,14.1894306031692,
126.454544471721)) ;
#146785 = CARTESIAN_POINT('Ctrl Pts',(-31.6360906022642,14.3944757405405,
126.680250797952)) ;
#146786 = CARTESIAN_POINT('Ctrl Pts',(-31.7166218889976,14.5294751420936,
126.948550384764)) ;
#146787 = CARTESIAN_POINT('Ctrl Pts',(-31.8056980992989,14.5857784683659,
127.241889657182)) ;
#146788 = CARTESIAN_POINT('Ctrl Pts',(-31.8962806353445,14.5584757984426,
127.539713151438)) ;
#146789 = CARTESIAN_POINT('Ctrl Pts',(-31.9806081664582,14.4499269528594,
127.819149771317)) ;
#146790 = CARTESIAN_POINT('Ctrl Pts',(-32.0523166133892,14.2678362445854,
128.061754335213)) ;
#146791 = CARTESIAN_POINT('Ctrl Pts',(-32.1054370338036,14.0251814638135,
128.250058329836)) ;
#146792 = CARTESIAN_POINT('Ctrl Pts',(-32.1354437565122,13.7395989389894,
128.370820351111)) ;
#146793 = CARTESIAN_POINT('Ctrl Pts',(-32.1394815178705,13.4312396305714,
128.415735091465)) ;
#146794 = CARTESIAN_POINT('Ctrl Pts',(-32.1165830014567,13.122549732562,128.38193137299)) ;
#146795 = CARTESIAN_POINT('Ctrl Pts',(-32.0674362918147,12.8344723669187,
128.271558952154)) ;
#146796 = CARTESIAN_POINT('Ctrl Pts',(-31.9951154000811,12.5894057801397,
128.093391835837)) ;
#146797 = CARTESIAN_POINT('Ctrl Pts',(-31.9039296777277,12.403866957567,127.860139162014)) ;
#146798 = CARTESIAN_POINT('Ctrl Pts',(-31.7997673665532,12.2913271425025,
127.588958580803)) ;
#146799 = CARTESIAN_POINT('Ctrl Pts',(-31.6890195332233,12.2598830910493,
127.298627363114)) ;
#146800 = CARTESIAN_POINT('Ctrl Pts',(-31.5796091120672,12.3117248733074,
127.012068699769)) ;
#146801 = CARTESIAN_POINT('Ctrl Pts',(-31.4779216841838,12.443258179484,126.748161772403)) ;
#146802 = CARTESIAN_POINT('Ctrl Pts',(-31.3909668215143,12.6447768173015,
126.527237872634)) ;
#146803 = CARTESIAN_POINT('Ctrl Pts',(-31.3239965485428,12.9020426575426,
126.364712331942)) ;
#146804 = CARTESIAN_POINT('Ctrl Pts',(-31.2811636319815,13.1969220375029,
126.272729427645)) ;
#146805 = CARTESIAN_POINT('Ctrl Pts',(-31.2647925939637,13.5073633530841,
126.257975466901)) ;
#146806 = CARTESIAN_POINT('Ctrl Pts',(-31.2754796646211,13.8135027955519,
126.322467658605)) ;
#146807 = CARTESIAN_POINT('Ctrl Pts',(-31.3113409517686,14.0890634485619,
126.460181362196)) ;
#146808 = CARTESIAN_POINT('Ctrl Pts',(-31.3697525249587,14.3192684868255,
126.664089287873)) ;
#146809 = CARTESIAN_POINT('Ctrl Pts',(-31.444870150607,14.4835637589644,126.916510315013)) ;
#146810 = CARTESIAN_POINT('Ctrl Pts',(-31.5316044126137,14.5730188127273,
127.203099079401)) ;
#146811 = CARTESIAN_POINT('Ctrl Pts',(-31.6223288461193,14.57959678794,127.50125169877)) ;
#146812 = CARTESIAN_POINT('Ctrl Pts',(-31.7100305460252,14.5032854042053,
127.79059470504)) ;
#146813 = CARTESIAN_POINT('Ctrl Pts',(-31.7875405915815,14.3501151902807,
128.050081809365)) ;
#146814 = CARTESIAN_POINT('Ctrl Pts',(-31.8490600583958,14.1289952661381,
128.2630780679)) ;
#146815 = CARTESIAN_POINT('Ctrl Pts',(-31.8886334301929,13.8600884343622,
128.411594339113)) ;
#146816 = CARTESIAN_POINT('Ctrl Pts',(-31.9035590805538,13.5571076942101,
128.48845671365)) ;
#146817 = CARTESIAN_POINT('Ctrl Pts',(-31.891490451461,13.2461441401465,128.486272087745)) ;
#146818 = CARTESIAN_POINT('Ctrl Pts',(-31.8528844195338,12.9474784920459,
128.406597920553)) ;
#146819 = CARTESIAN_POINT('Ctrl Pts',(-31.7891993797209,12.6818050518092,
128.253824959229)) ;
#146820 = CARTESIAN_POINT('Ctrl Pts',(-31.7054543493643,12.4713262054323,
128.042128875258)) ;
#146821 = CARTESIAN_POINT('Ctrl Pts',(-31.6054318541548,12.3273775325765,
127.783175932083)) ;
#146822 = CARTESIAN_POINT('Ctrl Pts',(-31.4968892175325,12.2625380449618,
127.499127406172)) ;
#146823 = CARTESIAN_POINT('Ctrl Pts',(-31.3854381872944,12.2810707567545,
127.206858131135)) ;
#146824 = CARTESIAN_POINT('Ctrl Pts',(-31.2805878990866,12.3803129183538,
126.933416339024)) ;
#146825 = CARTESIAN_POINT('Ctrl Pts',(-31.1864354677024,12.5556239144648,
126.691657848135)) ;
#146826 = CARTESIAN_POINT('Ctrl Pts',(-31.111027629603,12.7914917134663,126.504358906648)) ;
#146827 = CARTESIAN_POINT('Ctrl Pts',(-31.0577220690262,13.0750409894439,
126.381951641574)) ;
#146828 = CARTESIAN_POINT('Ctrl Pts',(-31.0306610295189,13.3808908591526,
126.335889900064)) ;
#146829 = CARTESIAN_POINT('Ctrl Pts',(-31.0303315381077,13.6908804953288,
126.368052181132)) ;
#146830 = CARTESIAN_POINT('Ctrl Pts',(-31.0563466589472,13.9819858786258,
126.477198994722)) ;
#146831 = CARTESIAN_POINT('Ctrl Pts',(-31.1061826731212,14.2331023151693,
126.655970164011)) ;
#146832 = CARTESIAN_POINT('Ctrl Pts',(-31.1750550140311,14.4253737390559,
126.890183910735)) ;
#146833 = CARTESIAN_POINT('Ctrl Pts',(-31.2583620135867,14.5469025476726,
127.166860376023)) ;
#146834 = CARTESIAN_POINT('Ctrl Pts',(-31.347862049284,14.5868798001592,127.46128776363)) ;
#146835 = CARTESIAN_POINT('Ctrl Pts',(-31.4375362474262,14.5442430115436,
127.756337185626)) ;
#146836 = CARTESIAN_POINT('Ctrl Pts',(-31.520090798019,14.4211466691175,128.030630534762)) ;
#146837 = CARTESIAN_POINT('Ctrl Pts',(-31.5887855970849,14.2262607722871,
128.26447035042)) ;
#146838 = CARTESIAN_POINT('Ctrl Pts',(-31.637813480413,13.9744157563079,128.440774331866)) ;
#146839 = CARTESIAN_POINT('Ctrl Pts',(-31.6631297576241,13.6824770169396,
128.547890122591)) ;
#146840 = CARTESIAN_POINT('Ctrl Pts',(-31.6621601735374,13.3726811372132,
128.578131369071)) ;
#146841 = CARTESIAN_POINT('Ctrl Pts',(-31.6339298075738,13.0644553037201,
128.528972432263)) ;
#146842 = CARTESIAN_POINT('Ctrl Pts',(-31.5804815129814,12.7851437851833,
128.405767102733)) ;
#146843 = CARTESIAN_POINT('Ctrl Pts',(-31.5040909563557,12.5493640401518,
128.215802779888)) ;
#146844 = CARTESIAN_POINT('Ctrl Pts',(-31.4101685419032,12.3769707551736,
127.974484791043)) ;
#146845 = CARTESIAN_POINT('Ctrl Pts',(-31.3038113686885,12.2789143084507,
127.697043035198)) ;
#146846 = CARTESIAN_POINT('Ctrl Pts',(-31.1932340122808,12.2633331273902,
127.407040069204)) ;
#146847 = CARTESIAN_POINT('Ctrl Pts',(-31.0843720330517,12.3306602572705,
127.12221228676)) ;
#146848 = CARTESIAN_POINT('Ctrl Pts',(-30.9849847014499,12.476620286477,126.865029460424)) ;
#146849 = CARTESIAN_POINT('Ctrl Pts',(-30.9016709973712,12.6891736358698,
126.654641927599)) ;
#146850 = CARTESIAN_POINT('Ctrl Pts',(-30.8388786394785,12.9552555089657,
126.504364811448)) ;
#146851 = CARTESIAN_POINT('Ctrl Pts',(-30.8009092568263,13.2547270236638,
126.426573132103)) ;
#146852 = CARTESIAN_POINT('Ctrl Pts',(-30.7896564473616,13.5662746405731,
126.426832768617)) ;
#146853 = CARTESIAN_POINT('Ctrl Pts',(-30.8051805713809,13.8673046435887,
126.505283369193)) ;
#146854 = CARTESIAN_POINT('Ctrl Pts',(-30.8456859021479,14.1368396800883,
126.656749073381)) ;
#146855 = CARTESIAN_POINT('Ctrl Pts',(-30.9074821394584,14.3550474216671,
126.87038266722)) ;
#146856 = CARTESIAN_POINT('Ctrl Pts',(-30.9855180716348,14.5066809592571,
127.13148926813)) ;
#146857 = CARTESIAN_POINT('Ctrl Pts',(-31.0733917700147,14.5805549920085,
127.421320442569)) ;
#146858 = CARTESIAN_POINT('Ctrl Pts',(-31.1640057518086,14.5715434315125,
127.719124297166)) ;
#146859 = CARTESIAN_POINT('Ctrl Pts',(-31.250294290685,14.480461463905,128.004304835114)) ;
#146860 = CARTESIAN_POINT('Ctrl Pts',(-31.325509255673,14.3129344866538,128.257246400145)) ;
#146861 = CARTESIAN_POINT('Ctrl Pts',(-31.3829962643348,14.0824719984918,
128.458246852631)) ;
#146862 = CARTESIAN_POINT('Ctrl Pts',(-31.4183563386291,13.8045960176135,
128.59465740896)) ;
#146863 = CARTESIAN_POINT('Ctrl Pts',(-31.4282543053624,13.4994872434927,
128.656672597553)) ;
#146864 = CARTESIAN_POINT('Ctrl Pts',(-31.4110646719943,13.1877258858405,
128.639691696467)) ;
#146865 = CARTESIAN_POINT('Ctrl Pts',(-31.3676711726817,12.8947281848912,
128.545939349583)) ;
#146866 = CARTESIAN_POINT('Ctrl Pts',(-31.2997556078703,12.6375710521211,
128.380814298397)) ;
#146867 = CARTESIAN_POINT('Ctrl Pts',(-31.2125224650725,12.4386468746083,
128.158973911426)) ;
#146868 = CARTESIAN_POINT('Ctrl Pts',(-31.110552826707,12.3091461004709,127.89423942265)) ;
#146869 = CARTESIAN_POINT('Ctrl Pts',(-31.0009258819824,12.259612482053,127.607074537605)) ;
#146870 = CARTESIAN_POINT('Ctrl Pts',(-30.8902243931203,12.2934287591009,
127.316887906934)) ;
#146871 = CARTESIAN_POINT('Ctrl Pts',(-30.7861895858125,12.4085128322788,
127.046134719561)) ;
#146872 = CARTESIAN_POINT('Ctrl Pts',(-30.6956941591112,12.5956557303843,
126.814825506304)) ;
#146873 = CARTESIAN_POINT('Ctrl Pts',(-30.6240074889673,12.8419007256208,
126.638483909041)) ;
#146874 = CARTESIAN_POINT('Ctrl Pts',(-30.5755559223467,13.1310174981793,
126.530158612128)) ;
#146875 = CARTESIAN_POINT('Ctrl Pts',(-30.5533896865543,13.4394174350743,
126.498431840003)) ;
#146876 = CARTESIAN_POINT('Ctrl Pts',(-30.558221598687,13.7489280848763,126.545829231152)) ;
#146877 = CARTESIAN_POINT('Ctrl Pts',(-30.588915578463,14.0326636274873,126.668504298489)) ;
#146878 = CARTESIAN_POINT('Ctrl Pts',(-30.6425884547498,14.2739040718616,
126.858421059732)) ;
#146879 = CARTESIAN_POINT('Ctrl Pts',(-30.7148915412408,14.4542739063911,
127.102819520797)) ;
#146880 = CARTESIAN_POINT('Ctrl Pts',(-30.7992997459529,14.5602989647872,
127.382416465165)) ;
#146881 = CARTESIAN_POINT('Ctrl Pts',(-30.8898956705548,14.5853165165248,
127.680264564623)) ;
#146882 = CARTESIAN_POINT('Ctrl Pts',(-30.9787713220706,14.5269567135038,
127.97298882425)) ;
#146883 = CARTESIAN_POINT('Ctrl Pts',(-31.059371853488,14.3891797896351,128.24165329551)) ;
#146884 = CARTESIAN_POINT('Ctrl Pts',(-31.1247308236064,14.1817903074031,
128.465771041066)) ;
#146885 = CARTESIAN_POINT('Ctrl Pts',(-31.1693676067746,13.9219442128278,
128.629125974528)) ;
#146886 = CARTESIAN_POINT('Ctrl Pts',(-31.1898960969392,13.6244333194243,
128.722303903431)) ;
#146887 = CARTESIAN_POINT('Ctrl Pts',(-31.1838033289645,13.3138308436316,
128.737553741756)) ;
#146888 = CARTESIAN_POINT('Ctrl Pts',(-31.1505821290089,13.0089907399567,
128.673795751988)) ;
#146889 = CARTESIAN_POINT('Ctrl Pts',(-31.0925799521882,12.7367005360714,
128.537303399666)) ;
#146890 = CARTESIAN_POINT('Ctrl Pts',(-31.0125260998317,12.5117902877451,
128.336595761873)) ;
#146891 = CARTESIAN_POINT('Ctrl Pts',(-30.9157663468451,12.3525056138097,
128.087033803185)) ;
#146892 = CARTESIAN_POINT('Ctrl Pts',(-30.8080721736054,12.2695603566645,
127.80564077783)) ;
#146893 = CARTESIAN_POINT('Ctrl Pts',(-30.6968461827106,12.2698997440141,
127.513902289464)) ;
#146894 = CARTESIAN_POINT('Ctrl Pts',(-30.5899150674534,12.352163996818,127.234500824101)) ;
#146895 = CARTESIAN_POINT('Ctrl Pts',(-30.4928833175223,12.5116414977634,
126.984230142973)) ;
#146896 = CARTESIAN_POINT('Ctrl Pts',(-30.4129128244218,12.7360068873482,
126.783700837563)) ;
#146897 = CARTESIAN_POINT('Ctrl Pts',(-30.3546072212312,13.0100795378332,
126.646534492897)) ;
#146898 = CARTESIAN_POINT('Ctrl Pts',(-30.3216185057163,13.3126252447019,
126.583197233705)) ;
#146899 = CARTESIAN_POINT('Ctrl Pts',(-30.315459892126,13.6254714681501,126.598503485917)) ;
#146900 = CARTESIAN_POINT('Ctrl Pts',(-30.3359002449836,13.921236470121,126.691222007845)) ;
#146901 = CARTESIAN_POINT('Ctrl Pts',(-30.3807986094703,14.1826934134292,
126.855550522785)) ;
#146902 = CARTESIAN_POINT('Ctrl Pts',(-30.4459374684072,14.3889686231296,
127.07887661895)) ;
#146903 = CARTESIAN_POINT('Ctrl Pts',(-30.5266278674902,14.5271449992224,
127.347855170467)) ;
#146904 = CARTESIAN_POINT('Ctrl Pts',(-30.6156581605218,14.5852339330884,
127.641082103165)) ;
#146905 = CARTESIAN_POINT('Ctrl Pts',(-30.7057064852132,14.5605427750385,
127.9371260928)) ;
#146906 = CARTESIAN_POINT('Ctrl Pts',(-30.7905667310835,14.4541441679249,
128.218216443374)) ;
#146907 = CARTESIAN_POINT('Ctrl Pts',(-30.862675831402,14.2740963431477,128.461966754846)) ;
#146908 = CARTESIAN_POINT('Ctrl Pts',(-30.9165420426013,14.0323113034301,
128.6525373636)) ;
#146909 = CARTESIAN_POINT('Ctrl Pts',(-30.9471458928728,13.7476340175603,
128.775035918765)) ;
#146910 = CARTESIAN_POINT('Ctrl Pts',(-30.9519877933255,13.4408490970619,
128.822167947952)) ;
#146911 = CARTESIAN_POINT('Ctrl Pts',(-30.9297341148964,13.1304291613817,
128.790407351982)) ;
#146912 = CARTESIAN_POINT('Ctrl Pts',(-30.8814901893038,12.8426172804035,
128.682531897237)) ;
#146913 = CARTESIAN_POINT('Ctrl Pts',(-30.8094718054732,12.5951022421241,
128.505390632872)) ;
#146914 = CARTESIAN_POINT('Ctrl Pts',(-30.7191980384741,12.4086451366849,
128.274629627039)) ;
#146915 = CARTESIAN_POINT('Ctrl Pts',(-30.6150556663668,12.2933533540089,
128.003603482979)) ;
#146916 = CARTESIAN_POINT('Ctrl Pts',(-30.5044178921979,12.259635664544,127.713579852543)) ;
#146917 = CARTESIAN_POINT('Ctrl Pts',(-30.3949358707502,12.3091205538474,
127.426799822407)) ;
#146918 = CARTESIAN_POINT('Ctrl Pts',(-30.2931032152827,12.4379929301553,
127.162397289569)) ;
#146919 = CARTESIAN_POINT('Ctrl Pts',(-30.2052137326913,12.6386444970783,
126.938906232635)) ;
#146920 = CARTESIAN_POINT('Ctrl Pts',(-30.137812185091,12.8942394959608,126.775057354265)) ;
#146921 = CARTESIAN_POINT('Ctrl Pts',(-30.0942843746289,13.1876523538433,
126.680974568525)) ;
#146922 = CARTESIAN_POINT('Ctrl Pts',(-30.0771111354794,13.4984174777635,
126.663931147677)) ;
#146923 = CARTESIAN_POINT('Ctrl Pts',(-30.0869464816408,13.804322914882,126.725848509996)) ;
#146924 = CARTESIAN_POINT('Ctrl Pts',(-30.1223210460623,14.0825044071424,
126.862326755857)) ;
#146925 = CARTESIAN_POINT('Ctrl Pts',(-30.1800394723012,14.3134151405244,
127.064102376406)) ;
#146926 = CARTESIAN_POINT('Ctrl Pts',(-30.2547445132516,14.4799820056889,
127.315334142319)) ;
#146927 = CARTESIAN_POINT('Ctrl Pts',(-30.3415883631799,14.5717628953294,
127.602359997053)) ;
#146928 = CARTESIAN_POINT('Ctrl Pts',(-30.4318402066912,14.5804902446719,
127.898966396358)) ;
#146929 = CARTESIAN_POINT('Ctrl Pts',(-30.5196878520343,14.5068426391239,
128.188713407741)) ;
#146930 = CARTESIAN_POINT('Ctrl Pts',(-30.5976721590961,14.3556215775595,
128.449624531829)) ;
#146931 = CARTESIAN_POINT('Ctrl Pts',(-30.6597155605127,14.1365916181852,
128.664110539127)) ;
#146932 = CARTESIAN_POINT('Ctrl Pts',(-30.7000450417134,13.8680780332019,
128.814933477325)) ;
#146933 = CARTESIAN_POINT('Ctrl Pts',(-30.7157305313142,13.5671869080058,
128.893853152154)) ;
#146934 = CARTESIAN_POINT('Ctrl Pts',(-30.7043528399412,13.2537546109161,
128.893949585034)) ;
#146935 = CARTESIAN_POINT('Ctrl Pts',(-30.6665757156128,12.9561225351469,
128.816517537223)) ;
#146936 = CARTESIAN_POINT('Ctrl Pts',(-30.6038252448511,12.6895770541959,
128.666400531881)) ;
#146937 = CARTESIAN_POINT('Ctrl Pts',(-30.5203605300861,12.4765149005577,
128.45563440576)) ;
#146938 = CARTESIAN_POINT('Ctrl Pts',(-30.4206676847351,12.3303993150384,
128.197651178616)) ;
#146939 = CARTESIAN_POINT('Ctrl Pts',(-30.3122067645033,12.2633426661684,
127.913867609128)) ;
#146940 = CARTESIAN_POINT('Ctrl Pts',(-30.2012947046513,12.2791039677748,
127.622994778204)) ;
#146941 = CARTESIAN_POINT('Ctrl Pts',(-30.0955067911406,12.3764767274057,
127.34702506124)) ;
#146942 = CARTESIAN_POINT('Ctrl Pts',(-30.0009941671484,12.5500288715812,
127.104204398368)) ;
#146943 = CARTESIAN_POINT('Ctrl Pts',(-29.9251551979687,12.78395781333,126.915590684127)) ;
#146944 = CARTESIAN_POINT('Ctrl Pts',(-29.871187296773,13.0658040836913,126.791179592973)) ;
#146945 = CARTESIAN_POINT('Ctrl Pts',(-29.8432186865559,13.3726170327576,
126.742615453226)) ;
#146946 = CARTESIAN_POINT('Ctrl Pts',(-29.8422395429821,13.6826397298667,
126.772863652498)) ;
#146947 = CARTESIAN_POINT('Ctrl Pts',(-29.8673746353157,13.9734160140871,
126.879300450678)) ;
#146948 = CARTESIAN_POINT('Ctrl Pts',(-29.9167203821773,14.2269288316592,
127.056756775125)) ;
#146949 = CARTESIAN_POINT('Ctrl Pts',(-29.9850311185671,14.4205112254327,
127.289268900708)) ;
#146950 = CARTESIAN_POINT('Ctrl Pts',(-30.0675752554345,14.5441065975964,
127.563558807458)) ;
#146951 = CARTESIAN_POINT('Ctrl Pts',(-30.1576125359038,14.5870792666042,
127.859794320208)) ;
#146952 = CARTESIAN_POINT('Ctrl Pts',(-30.2474849888597,14.5462510454972,
128.155465708352)) ;
#146953 = CARTESIAN_POINT('Ctrl Pts',(-30.3299319014001,14.4261089753038,
128.429272190537)) ;
#146954 = CARTESIAN_POINT('Ctrl Pts',(-30.3995036371057,14.2320089308133,
128.665864379733)) ;
#146955 = CARTESIAN_POINT('Ctrl Pts',(-30.4489243649137,13.9821034957132,
128.843216326838)) ;
#146956 = CARTESIAN_POINT('Ctrl Pts',(-30.4749610643755,13.6914861079863,
128.952391552536)) ;
#146957 = CARTESIAN_POINT('Ctrl Pts',(-30.4747999900052,13.3820427102498,
128.98498114324)) ;
#146958 = CARTESIAN_POINT('Ctrl Pts',(-30.4473515216857,13.0731824784138,
128.938127658199)) ;
#146959 = CARTESIAN_POINT('Ctrl Pts',(-30.3945986181408,12.7927891532511,
128.816959868306)) ;
#146960 = CARTESIAN_POINT('Ctrl Pts',(-30.3187955084458,12.555308710761,128.628720211139)) ;
#146961 = CARTESIAN_POINT('Ctrl Pts',(-30.2251379780315,12.3807971567645,
128.388227552432)) ;
#146962 = CARTESIAN_POINT('Ctrl Pts',(-30.1194247642222,12.2807361442519,
128.112543422468)) ;
#146963 = CARTESIAN_POINT('Ctrl Pts',(-30.0085407368298,12.2625961499198,
127.821752081797)) ;
#146964 = CARTESIAN_POINT('Ctrl Pts',(-29.8996873404426,12.3275534579407,
127.536894483403)) ;
#146965 = CARTESIAN_POINT('Ctrl Pts',(-29.7999406635735,12.4713199935408,
127.278663605204)) ;
#146966 = CARTESIAN_POINT('Ctrl Pts',(-29.7160662663461,12.6818353825156,
127.066618789895)) ;
#146967 = CARTESIAN_POINT('Ctrl Pts',(-29.6522505230359,12.9488695805188,
126.913606492894)) ;
#146968 = CARTESIAN_POINT('Ctrl Pts',(-29.6139590229148,13.2449964341876,
126.834565223254)) ;
#146969 = CARTESIAN_POINT('Ctrl Pts',(-29.6017834508264,13.5577146897345,
126.832264886568)) ;
#146970 = CARTESIAN_POINT('Ctrl Pts',(-29.6166083435889,13.8591379588549,
126.90864921774)) ;
#146971 = CARTESIAN_POINT('Ctrl Pts',(-29.6564971042397,14.1301669170847,
127.058355027748)) ;
#146972 = CARTESIAN_POINT('Ctrl Pts',(-29.7177594105147,14.3498259232659,
127.270410807092)) ;
#146973 = CARTESIAN_POINT('Ctrl Pts',(-29.7952862533984,14.5033075535996,
127.529976715887)) ;
#146974 = CARTESIAN_POINT('Ctrl Pts',(-29.8830140909099,14.5795880895815,
127.819399645601)) ;
#146975 = CARTESIAN_POINT('Ctrl Pts',(-29.9736829293594,14.5729975204269,
128.11737472752)) ;
#146976 = CARTESIAN_POINT('Ctrl Pts',(-30.0604370601336,14.4837968438998,
128.404012404392)) ;
#146977 = CARTESIAN_POINT('Ctrl Pts',(-30.1359257622124,14.3181445860539,
128.65772161378)) ;
#146978 = CARTESIAN_POINT('Ctrl Pts',(-30.1938131883798,14.0900336842333,
128.859788825961)) ;
#146979 = CARTESIAN_POINT('Ctrl Pts',(-30.2299435215445,13.8125787469842,
128.998529327741)) ;
#146980 = CARTESIAN_POINT('Ctrl Pts',(-30.2405301452034,13.5087143541534,
129.062470965387)) ;
#146981 = CARTESIAN_POINT('Ctrl Pts',(-30.2242241360838,13.1970642256003,
129.048040790549)) ;
#146982 = CARTESIAN_POINT('Ctrl Pts',(-30.1814038042651,12.9023258693894,
128.956073007442)) ;
#146983 = CARTESIAN_POINT('Ctrl Pts',(-30.1143382086823,12.6446851573858,
128.793320917903)) ;
#146984 = CARTESIAN_POINT('Ctrl Pts',(-30.0276174900689,12.4436426796563,
128.572993750691)) ;
#146985 = CARTESIAN_POINT('Ctrl Pts',(-29.9258485365255,12.3118006099846,
128.308887056809)) ;
#146986 = CARTESIAN_POINT('Ctrl Pts',(-29.8163200649129,12.259762671147,128.022015597421)) ;
#146987 = CARTESIAN_POINT('Ctrl Pts',(-29.7051375050554,12.2917039149137,
127.730553612688)) ;
#146988 = CARTESIAN_POINT('Ctrl Pts',(-29.6016270677381,12.4035190243102,
127.461062925927)) ;
#146989 = CARTESIAN_POINT('Ctrl Pts',(-29.5098964515148,12.5902948826821,
127.22643242955)) ;
#146990 = CARTESIAN_POINT('Ctrl Pts',(-29.4380833187018,12.8337324578526,
127.049514825685)) ;
#146991 = CARTESIAN_POINT('Ctrl Pts',(-29.3886219255085,13.1235886478701,
126.938436984437)) ;
#146992 = CARTESIAN_POINT('Ctrl Pts',(-29.3659461445248,13.4302519439914,
126.905060184476)) ;
#146993 = CARTESIAN_POINT('Ctrl Pts',(-29.3698075336204,13.7390104771059,
126.949495883131)) ;
#146994 = CARTESIAN_POINT('Ctrl Pts',(-29.4000452910278,14.0260062251914,
127.071106527012)) ;
#146995 = CARTESIAN_POINT('Ctrl Pts',(-29.4528929037883,14.267226894927,127.258426176664)) ;
#146996 = CARTESIAN_POINT('Ctrl Pts',(-29.5246326985309,14.4498458863908,
127.501170540554)) ;
#146997 = CARTESIAN_POINT('Ctrl Pts',(-29.6091872255536,14.5586319287784,
127.781351330665)) ;
#146998 = CARTESIAN_POINT('Ctrl Pts',(-29.6997471862202,14.5856242099091,
128.07910262556)) ;
#146999 = CARTESIAN_POINT('Ctrl Pts',(-29.7883807533192,14.5299078303726,
128.370974736792)) ;
#147000 = CARTESIAN_POINT('Ctrl Pts',(-29.8695306978399,14.3940107888909,
128.641329791261)) ;
#147001 = CARTESIAN_POINT('Ctrl Pts',(-29.9352642647434,14.1888420918384,
128.866468214376)) ;
#147002 = CARTESIAN_POINT('Ctrl Pts',(-29.9806165337135,13.9299824930108,
129.031961511465)) ;
#147003 = CARTESIAN_POINT('Ctrl Pts',(-30.0018750942867,13.6339609144374,
129.127188391206)) ;
#147004 = CARTESIAN_POINT('Ctrl Pts',(-29.9965569305934,13.3227159368467,
129.144784844423)) ;
#147005 = CARTESIAN_POINT('Ctrl Pts',(-29.9642939595592,13.0187244434426,
129.083670051289)) ;
#147006 = CARTESIAN_POINT('Ctrl Pts',(-29.9069372408107,12.7442184480219,
128.949165273436)) ;
#147007 = CARTESIAN_POINT('Ctrl Pts',(-29.826988446716,12.516718909921,128.748926776798)) ;
#147008 = CARTESIAN_POINT('Ctrl Pts',(-29.7310520871085,12.3563386228632,
128.50161270827)) ;
#147009 = CARTESIAN_POINT('Ctrl Pts',(-29.6238026629605,12.2709228353889,
128.22145763842)) ;
#147010 = CARTESIAN_POINT('Ctrl Pts',(-29.5124524449978,12.2686101077704,
127.929393883299)) ;
#147011 = CARTESIAN_POINT('Ctrl Pts',(-29.4050655842839,12.3485946341444,
127.648731549074)) ;
#147012 = CARTESIAN_POINT('Ctrl Pts',(-29.307350900322,12.5068356453483,127.396583496414)) ;
#147013 = CARTESIAN_POINT('Ctrl Pts',(-29.2273191764511,12.728330138996,127.195683455919)) ;
#147014 = CARTESIAN_POINT('Ctrl Pts',(-29.1681740607996,13.0013550169445,
127.056098533042)) ;
#147015 = CARTESIAN_POINT('Ctrl Pts',(-29.134416586331,13.303953158046,126.990578886437)) ;
#147016 = CARTESIAN_POINT('Ctrl Pts',(-29.1274395375994,13.6158508355622,
127.003379945153)) ;
#147017 = CARTESIAN_POINT('Ctrl Pts',(-29.1472523538254,13.9138455338492,
127.094439041545)) ;
#147018 = CARTESIAN_POINT('Ctrl Pts',(-29.1913098510349,14.1752852419692,
127.256147124711)) ;
#147019 = CARTESIAN_POINT('Ctrl Pts',(-29.2560209697753,14.3839668801463,
127.47829864687)) ;
#147020 = CARTESIAN_POINT('Ctrl Pts',(-29.3362834013603,14.5240578429112,
127.745988342019)) ;
#147021 = CARTESIAN_POINT('Ctrl Pts',(-29.4250790846387,14.584818932524,128.038503048431)) ;
#147022 = CARTESIAN_POINT('Ctrl Pts',(-29.5157805659722,14.5621167369362,
128.33667727634)) ;
#147023 = CARTESIAN_POINT('Ctrl Pts',(-29.6003485790494,14.4583966415937,
128.616704866655)) ;
#147024 = CARTESIAN_POINT('Ctrl Pts',(-29.672999428089,14.2803903963779,128.862065022642)) ;
#147025 = CARTESIAN_POINT('Ctrl Pts',(-29.7273636308734,14.0406559571458,
129.054023045337)) ;
#147026 = CARTESIAN_POINT('Ctrl Pts',(-29.7588399368944,13.7571590252373,
129.179067225918)) ;
#147027 = CARTESIAN_POINT('Ctrl Pts',(-29.7643708007054,13.4483332658606,
129.228470996735)) ;
#147028 = CARTESIAN_POINT('Ctrl Pts',(-29.7431271902945,13.1406103959238,
129.199333519999)) ;
#147029 = CARTESIAN_POINT('Ctrl Pts',(-29.6952107620917,12.849237718573,129.092722743839)) ;
#147030 = CARTESIAN_POINT('Ctrl Pts',(-29.6242103407272,12.6021186040621,
128.918326096847)) ;
#147031 = CARTESIAN_POINT('Ctrl Pts',(-29.534342376669,12.4130744428075,128.688810495785)) ;
#147032 = CARTESIAN_POINT('Ctrl Pts',(-29.4300815144381,12.295357536539,128.417555698654)) ;
#147033 = CARTESIAN_POINT('Ctrl Pts',(-29.3199980857374,12.2595400049776,
128.129012313781)) ;
#147034 = CARTESIAN_POINT('Ctrl Pts',(-29.2102972783543,12.3063152833776,
127.841614367448)) ;
#147035 = CARTESIAN_POINT('Ctrl Pts',(-29.1075765805156,12.4341408238282,
127.57482056363)) ;
#147036 = CARTESIAN_POINT('Ctrl Pts',(-29.0198927916179,12.6316134700122,
127.351679653212)) ;
#147037 = CARTESIAN_POINT('Ctrl Pts',(-28.9516398841463,12.8861350192124,
127.185411007251)) ;
#147038 = CARTESIAN_POINT('Ctrl Pts',(-28.9073369484727,13.1792139028364,
127.089109169935)) ;
#147039 = CARTESIAN_POINT('Ctrl Pts',(-28.8894132390635,13.490568739432,127.069953917477)) ;
#147040 = CARTESIAN_POINT('Ctrl Pts',(-28.8985917369534,13.7964603979055,
127.129907547714)) ;
#147041 = CARTESIAN_POINT('Ctrl Pts',(-28.933109908976,14.0743848180785,127.263731937239)) ;
#147042 = CARTESIAN_POINT('Ctrl Pts',(-28.9900661981856,14.3070162611111,
127.463243023677)) ;
#147043 = CARTESIAN_POINT('Ctrl Pts',(-29.0648227386281,14.476451846962,127.714825187418)) ;
#147044 = CARTESIAN_POINT('Ctrl Pts',(-29.1506744032719,14.569850177848,127.998660756491)) ;
#147045 = CARTESIAN_POINT('Ctrl Pts',(-29.2413663721334,14.5816111241078,
128.296730098651)) ;
#147046 = CARTESIAN_POINT('Ctrl Pts',(-29.3296595746276,14.5098991717079,
128.587875780273)) ;
#147047 = CARTESIAN_POINT('Ctrl Pts',(-29.4080445514393,14.360403037698,128.849988285308)) ;
#147048 = CARTESIAN_POINT('Ctrl Pts',(-29.4704203779367,14.143565690272,129.065356761645)) ;
#147049 = CARTESIAN_POINT('Ctrl Pts',(-29.5114914499604,13.8762646142661,
129.218353321002)) ;
#147050 = CARTESIAN_POINT('Ctrl Pts',(-29.527821482954,13.5746434283165,129.299296311103)) ;
#147051 = CARTESIAN_POINT('Ctrl Pts',(-29.5174206340191,13.2647986868619,
129.301857135357)) ;
#147052 = CARTESIAN_POINT('Ctrl Pts',(-29.4802017636136,12.9638356585252,
129.226346996376)) ;
#147053 = CARTESIAN_POINT('Ctrl Pts',(-29.4181913382434,12.696740713892,129.0783105115)) ;
#147054 = CARTESIAN_POINT('Ctrl Pts',(-29.3350888977121,12.4815167402667,
128.868676644818)) ;
#147055 = CARTESIAN_POINT('Ctrl Pts',(-29.2361228630141,12.3337893595149,
128.61269329159)) ;
#147056 = CARTESIAN_POINT('Ctrl Pts',(-29.1275784391396,12.2640797923872,
128.3287499801)) ;
#147057 = CARTESIAN_POINT('Ctrl Pts',(-29.0167646928416,12.2774691483239,
128.038121461427)) ;
#147058 = CARTESIAN_POINT('Ctrl Pts',(-28.9107301726355,12.3724670418659,
127.761433361359)) ;
#147059 = CARTESIAN_POINT('Ctrl Pts',(-28.8158185730082,12.543767432119,127.517423530661)) ;
#147060 = CARTESIAN_POINT('Ctrl Pts',(-28.7392542408097,12.7765746874498,
127.32675668177)) ;
#147061 = CARTESIAN_POINT('Ctrl Pts',(-28.6847206547343,13.056442699504,127.200585791957)) ;
#147062 = CARTESIAN_POINT('Ctrl Pts',(-28.6558953247287,13.3632374383365,
127.149573983655)) ;
#147063 = CARTESIAN_POINT('Ctrl Pts',(-28.6540191244132,13.6730055112077,
127.177138695141)) ;
#147064 = CARTESIAN_POINT('Ctrl Pts',(-28.6787541261639,13.9671153301203,
127.282712736634)) ;
#147065 = CARTESIAN_POINT('Ctrl Pts',(-28.726959761685,14.2192391105439,127.456470176809)) ;
#147066 = CARTESIAN_POINT('Ctrl Pts',(-28.7952494116795,14.4164802327196,
127.689188807195)) ;
#147067 = CARTESIAN_POINT('Ctrl Pts',(-28.8773322714303,14.5415580388922,
127.96203905316)) ;
#147068 = CARTESIAN_POINT('Ctrl Pts',(-28.966957796165,14.5869148382087,128.25697340176)) ;
#147069 = CARTESIAN_POINT('Ctrl Pts',(-29.056892610989,14.5490099529441,128.55279780603)) ;
#147070 = CARTESIAN_POINT('Ctrl Pts',(-29.1402169930976,14.4299835692337,
128.829416302567)) ;
#147071 = CARTESIAN_POINT('Ctrl Pts',(-29.2096450513186,14.2395160261302,
129.065284124465)) ;
#147072 = CARTESIAN_POINT('Ctrl Pts',(-29.2600489235632,13.9900850961344,
129.245677108272)) ;
#147073 = CARTESIAN_POINT('Ctrl Pts',(-29.2867905400275,13.7002631156838,
129.356907899631)) ;
#147074 = CARTESIAN_POINT('Ctrl Pts',(-29.2873580451206,13.3906063492619,
129.391679953749)) ;
#147075 = CARTESIAN_POINT('Ctrl Pts',(-29.2608441995176,13.0826197535591,
129.347411851006)) ;
#147076 = CARTESIAN_POINT('Ctrl Pts',(-29.2085441327409,12.7997481172877,
129.227739730843)) ;
#147077 = CARTESIAN_POINT('Ctrl Pts',(-29.1335049130153,12.5614902971475,
129.041634768994)) ;
#147078 = CARTESIAN_POINT('Ctrl Pts',(-29.0401540366399,12.3846250273346,
128.802093504295)) ;
#147079 = CARTESIAN_POINT('Ctrl Pts',(-28.9346464367386,12.2824687909252,
128.527016672722)) ;
#147080 = CARTESIAN_POINT('Ctrl Pts',(-28.824116083048,12.2619556332192,128.237168385874)) ;
#147081 = CARTESIAN_POINT('Ctrl Pts',(-28.7149966519967,12.3244285143439,
127.951562960797)) ;
#147082 = CARTESIAN_POINT('Ctrl Pts',(-28.6146573164258,12.4664340119557,
127.691677135041)) ;
#147083 = CARTESIAN_POINT('Ctrl Pts',(-28.5303819440555,12.675348720281,127.478448660203)) ;
#147084 = CARTESIAN_POINT('Ctrl Pts',(-28.4662472388225,12.9390314346698,
127.32426847584)) ;
#147085 = CARTESIAN_POINT('Ctrl Pts',(-28.426784584346,13.2369183007794,127.242088186904)) ;
#147086 = CARTESIAN_POINT('Ctrl Pts',(-28.414001297498,13.549774387286,127.238027762963)) ;
#147087 = CARTESIAN_POINT('Ctrl Pts',(-28.4280334218581,13.850609448165,127.311971837892)) ;
#147088 = CARTESIAN_POINT('Ctrl Pts',(-28.4672280424493,14.1229209827014,
127.459657669781)) ;
#147089 = CARTESIAN_POINT('Ctrl Pts',(-28.5278478480601,14.3440340746158,
127.669795018464)) ;
#147090 = CARTESIAN_POINT('Ctrl Pts',(-28.6050799543434,14.5000650496519,
127.928551700968)) ;
#147091 = CARTESIAN_POINT('Ctrl Pts',(-28.6930251647457,14.578644462167,128.218756301245)) ;
#147092 = CARTESIAN_POINT('Ctrl Pts',(-28.7831377408782,14.5743811633841,
128.514894788016)) ;
#147093 = CARTESIAN_POINT('Ctrl Pts',(-28.8703782343565,14.4873598726622,
128.803057217724)) ;
#147094 = CARTESIAN_POINT('Ctrl Pts',(-28.9461043703451,14.3240886770746,
129.057379640458)) ;
#147095 = CARTESIAN_POINT('Ctrl Pts',(-29.0046450639296,14.0972553014586,
129.261412205121)) ;
#147096 = CARTESIAN_POINT('Ctrl Pts',(-29.041421187763,13.8219067372358,129.401927249139)) ;
#147097 = CARTESIAN_POINT('Ctrl Pts',(-29.0528414560578,13.5160256526642,
129.468579531831)) ;
#147098 = CARTESIAN_POINT('Ctrl Pts',(-29.0371616190134,13.2050737641674,
129.455888808854)) ;
#147099 = CARTESIAN_POINT('Ctrl Pts',(-28.9952221551934,12.9106474096039,
129.366380741704)) ;
#147100 = CARTESIAN_POINT('Ctrl Pts',(-28.9289573583744,12.6518068441283,
129.205925046669)) ;
#147101 = CARTESIAN_POINT('Ctrl Pts',(-28.8423703172031,12.4481718520534,
128.986128276051)) ;
#147102 = CARTESIAN_POINT('Ctrl Pts',(-28.7410953233907,12.3143466124611,
128.723403080249)) ;
#147103 = CARTESIAN_POINT('Ctrl Pts',(-28.6311229647181,12.2602411287431,
128.435411596259)) ;
#147104 = CARTESIAN_POINT('Ctrl Pts',(-28.521399927036,12.289044216294,128.147739484492)) ;
#147105 = CARTESIAN_POINT('Ctrl Pts',(-28.4163596339001,12.3996399053781,
127.874180741612)) ;
#147106 = CARTESIAN_POINT('Ctrl Pts',(-28.3249767341809,12.5827969083002,
127.64025343428)) ;
#147107 = CARTESIAN_POINT('Ctrl Pts',(-28.2518532145278,12.826962989628,127.459831520999)) ;
#147108 = CARTESIAN_POINT('Ctrl Pts',(-28.2021925015218,13.1127056207623,
127.34779653997)) ;
#147109 = CARTESIAN_POINT('Ctrl Pts',(-28.178363709681,13.421711878802,127.311352934498)) ;
#147110 = CARTESIAN_POINT('Ctrl Pts',(-28.1815690515954,13.7304251120726,
127.353829356402)) ;
#147111 = CARTESIAN_POINT('Ctrl Pts',(-28.211039530244,14.018344311728,127.473192935567)) ;
#147112 = CARTESIAN_POINT('Ctrl Pts',(-28.2634287201407,14.2615012017521,
127.659241766758)) ;
#147113 = CARTESIAN_POINT('Ctrl Pts',(-28.3346148571528,14.4455241651706,
127.900307053913)) ;
#147114 = CARTESIAN_POINT('Ctrl Pts',(-28.418623430654,14.5564730529287,128.178795974798)) ;
#147115 = CARTESIAN_POINT('Ctrl Pts',(-28.5094384562439,14.58603325722,128.477414862936)) ;
#147116 = CARTESIAN_POINT('Ctrl Pts',(-28.5980426291786,14.5327319880778,
128.769135372419)) ;
#147117 = CARTESIAN_POINT('Ctrl Pts',(-28.6796160846217,14.3988255152791,
129.040771032821)) ;
#147118 = CARTESIAN_POINT('Ctrl Pts',(-28.745579180709,14.1966329622431,129.266414354394)) ;
#147119 = CARTESIAN_POINT('Ctrl Pts',(-28.7918797647502,13.9381994545952,
129.434822486951)) ;
#147120 = CARTESIAN_POINT('Ctrl Pts',(-28.8138551442112,13.6421507642692,
129.532218437035)) ;
#147121 = CARTESIAN_POINT('Ctrl Pts',(-28.8092832638101,13.3319747880892,
129.551898416221)) ;
#147122 = CARTESIAN_POINT('Ctrl Pts',(-28.7779247190653,13.0275241495644,
129.493404475197)) ;
#147123 = CARTESIAN_POINT('Ctrl Pts',(-28.7206834966505,12.7499513139427,
129.359499879805)) ;
#147124 = CARTESIAN_POINT('Ctrl Pts',(-28.6420010050341,12.5230805952481,
129.162644470801)) ;
#147125 = CARTESIAN_POINT('Ctrl Pts',(-28.5460238731504,12.3595163479197,
128.915388817262)) ;
#147126 = CARTESIAN_POINT('Ctrl Pts',(-28.4387186631021,12.2720601072795,
128.6351364541)) ;
#147127 = CARTESIAN_POINT('Ctrl Pts',(-28.3276074338221,12.2676665398888,
128.343703806802)) ;
#147128 = CARTESIAN_POINT('Ctrl Pts',(-28.2204032567713,12.3451448289758,
128.063463534875)) ;
#147129 = CARTESIAN_POINT('Ctrl Pts',(-28.1225359120705,12.5004782540512,
127.810766610281)) ;
#147130 = CARTESIAN_POINT('Ctrl Pts',(-28.0414953870407,12.7212077587515,
127.607081321906)) ;
#147131 = CARTESIAN_POINT('Ctrl Pts',(-27.9816602120392,12.9936145319541,
127.4655295393)) ;
#147132 = CARTESIAN_POINT('Ctrl Pts',(-27.9472693123842,13.2947837203187,
127.398064809065)) ;
#147133 = CARTESIAN_POINT('Ctrl Pts',(-27.9394737059955,13.6064068032795,
127.408440270478)) ;
#147134 = CARTESIAN_POINT('Ctrl Pts',(-27.9584521870025,13.9050217412781,
127.497042995191)) ;
#147135 = CARTESIAN_POINT('Ctrl Pts',(-28.0019723652954,14.1686336677941,
127.657287030857)) ;
#147136 = CARTESIAN_POINT('Ctrl Pts',(-28.0661545150661,14.3788182698461,
127.877871299589)) ;
#147137 = CARTESIAN_POINT('Ctrl Pts',(-28.1458363458335,14.5208662743525,
128.14378094547)) ;
#147138 = CARTESIAN_POINT('Ctrl Pts',(-28.2345899026998,14.5841619964858,
128.436220428999)) ;
#147139 = CARTESIAN_POINT('Ctrl Pts',(-28.3250495930938,14.5641966212731,
128.733575916725)) ;
#147140 = CARTESIAN_POINT('Ctrl Pts',(-28.4102887222356,14.4625802031817,
129.01571259501)) ;
#147141 = CARTESIAN_POINT('Ctrl Pts',(-28.4834734306057,14.286005519678,129.262692624796)) ;
#147142 = CARTESIAN_POINT('Ctrl Pts',(-28.5382560423696,14.0484511766116,
129.455778944107)) ;
#147143 = CARTESIAN_POINT('Ctrl Pts',(-28.5704620543408,13.7663469641466,
129.58292061169)) ;
#147144 = CARTESIAN_POINT('Ctrl Pts',(-28.5768364910779,13.4574607862846,
129.634836630178)) ;
#147145 = CARTESIAN_POINT('Ctrl Pts',(-28.5562466562937,13.1488899343714,
129.607677485992)) ;
#147146 = CARTESIAN_POINT('Ctrl Pts',(-28.5093930101883,12.8583365038161,
129.503969294116)) ;
#147147 = CARTESIAN_POINT('Ctrl Pts',(-28.4388409420063,12.6085157642258,
129.331015719234)) ;
#147148 = CARTESIAN_POINT('Ctrl Pts',(-28.349200703581,12.417394689709,129.102233983392)) ;
#147149 = CARTESIAN_POINT('Ctrl Pts',(-28.2458285984717,12.2980452519264,
128.833391652384)) ;
#147150 = CARTESIAN_POINT('Ctrl Pts',(-28.1357470146788,12.2592457780577,
128.544885828624)) ;
#147151 = CARTESIAN_POINT('Ctrl Pts',(-28.0254127094965,12.304020860261,128.255796572371)) ;
#147152 = CARTESIAN_POINT('Ctrl Pts',(-27.9230809162868,12.4286939335528,
127.989907508623)) ;
#147153 = CARTESIAN_POINT('Ctrl Pts',(-27.8345386835555,12.6243589997422,
127.764349398266)) ;
#147154 = CARTESIAN_POINT('Ctrl Pts',(-27.7653382579701,12.878908332841,127.595482065447)) ;
#147155 = CARTESIAN_POINT('Ctrl Pts',(-27.7205297869088,13.1702261034011,
127.497588845532)) ;
#147156 = CARTESIAN_POINT('Ctrl Pts',(-27.7017835873121,13.4805036941569,
127.475942764132)) ;
#147157 = CARTESIAN_POINT('Ctrl Pts',(-27.710102323973,13.7876511360062,127.533460289688)) ;
#147158 = CARTESIAN_POINT('Ctrl Pts',(-27.7441693729637,14.0678452510403,
127.666126181136)) ;
#147159 = CARTESIAN_POINT('Ctrl Pts',(-27.8002814506919,14.3007432572347,
127.862995333965)) ;
#147160 = CARTESIAN_POINT('Ctrl Pts',(-27.8746546477273,14.4725786347777,
128.113498687342)) ;
#147161 = CARTESIAN_POINT('Ctrl Pts',(-27.9602816443766,14.5682598851549,
128.396677955504)) ;
#147162 = CARTESIAN_POINT('Ctrl Pts',(-28.0509255421651,14.5824152929646,
128.69460486853)) ;
#147163 = CARTESIAN_POINT('Ctrl Pts',(-28.1392618095582,14.5133614701989,
128.98581686609)) ;
#147164 = CARTESIAN_POINT('Ctrl Pts',(-28.2181642812926,14.3656855427812,
129.249510046041)) ;
#147165 = CARTESIAN_POINT('Ctrl Pts',(-28.2808475403188,14.1519223371762,
129.465604823184)) ;
#147166 = CARTESIAN_POINT('Ctrl Pts',(-28.3229370821972,13.8839965789022,
129.621822830416)) ;
#147167 = CARTESIAN_POINT('Ctrl Pts',(-28.3399163611,13.5839686018203,129.704545642806)) ;
#147168 = CARTESIAN_POINT('Ctrl Pts',(-28.3303022079607,13.2736211027787,
129.709464937928)) ;
#147169 = CARTESIAN_POINT('Ctrl Pts',(-28.2939612293933,12.9727616409807,
129.636430416121)) ;
#147170 = CARTESIAN_POINT('Ctrl Pts',(-28.2324344840821,12.7034620887289,
129.489924492685)) ;
#147171 = CARTESIAN_POINT('Ctrl Pts',(-28.1498921349049,12.4867212109574,
129.281903673158)) ;
#147172 = CARTESIAN_POINT('Ctrl Pts',(-28.0511944467291,12.3368637166341,
129.026735473833)) ;
#147173 = CARTESIAN_POINT('Ctrl Pts',(-27.9431866501433,12.265034692949,128.744249987499)) ;
#147174 = CARTESIAN_POINT('Ctrl Pts',(-27.8320553152906,12.2758062586622,
128.45277717957)) ;
#147175 = CARTESIAN_POINT('Ctrl Pts',(-27.725403769765,12.3692807185403,128.174418307397)) ;
#147176 = CARTESIAN_POINT('Ctrl Pts',(-27.6305768731226,12.5378929203228,
127.930489816518)) ;
#147177 = CARTESIAN_POINT('Ctrl Pts',(-27.5532840737938,12.7694277251572,
127.737752051998)) ;
#147178 = CARTESIAN_POINT('Ctrl Pts',(-27.4980628041724,13.0484835802669,
127.609590602882)) ;
#147179 = CARTESIAN_POINT('Ctrl Pts',(-27.468512009568,13.3553251834758,127.556508766541)) ;
#147180 = CARTESIAN_POINT('Ctrl Pts',(-27.4659658852971,13.664055596243,127.581991492348)) ;
#147181 = CARTESIAN_POINT('Ctrl Pts',(-27.4897083326271,13.9577070332473,
127.684504096901)) ;
#147182 = CARTESIAN_POINT('Ctrl Pts',(-27.537488419938,14.2128779767414,127.857213382513)) ;
#147183 = CARTESIAN_POINT('Ctrl Pts',(-27.6053110365793,14.4117544181439,
128.088557180992)) ;
#147184 = CARTESIAN_POINT('Ctrl Pts',(-27.6870263113948,14.539128300591,128.360320009239)) ;
#147185 = CARTESIAN_POINT('Ctrl Pts',(-27.776949692643,14.5867879384206,128.656273925629)) ;
#147186 = CARTESIAN_POINT('Ctrl Pts',(-27.866542120589,14.5512051552351,128.950939963951)) ;
#147187 = CARTESIAN_POINT('Ctrl Pts',(-27.9503029825462,14.4343419878625,
129.228886623273)) ;
#147188 = CARTESIAN_POINT('Ctrl Pts',(-28.0201765415202,14.2455278913779,
129.466064406398)) ;
#147189 = CARTESIAN_POINT('Ctrl Pts',(-28.071089607046,13.9981929136205,129.647863070259)) ;
#147190 = CARTESIAN_POINT('Ctrl Pts',(-28.0986318176994,13.7085066706188,
129.76151901077)) ;
#147191 = CARTESIAN_POINT('Ctrl Pts',(-28.099895689668,13.3995793923712,129.798274390018)) ;
#147192 = CARTESIAN_POINT('Ctrl Pts',(-28.0743169746615,13.0919774693214,
129.756648462602)) ;
#147193 = CARTESIAN_POINT('Ctrl Pts',(-28.0224473100631,12.8067303773131,
129.638400985545)) ;
#147194 = CARTESIAN_POINT('Ctrl Pts',(-27.9483787106709,12.5682008824759,
129.454956724157)) ;
#147195 = CARTESIAN_POINT('Ctrl Pts',(-27.8553471386476,12.3888212214355,
129.216414429093)) ;
#147196 = CARTESIAN_POINT('Ctrl Pts',(-27.7502434316432,12.2844119471438,
128.942471886976)) ;
#147197 = CARTESIAN_POINT('Ctrl Pts',(-27.6394225717743,12.2613333945147,
128.651879574797)) ;
#147198 = CARTESIAN_POINT('Ctrl Pts',(-27.5302844551379,12.3215794553672,
128.366182543468)) ;
#147199 = CARTESIAN_POINT('Ctrl Pts',(-27.4299126178422,12.4606919099578,
128.106084606762)) ;
#147200 = CARTESIAN_POINT('Ctrl Pts',(-27.3447157997432,12.6684213928488,
127.890292996441)) ;
#147201 = CARTESIAN_POINT('Ctrl Pts',(-27.2797816216191,12.9319195354802,
127.733892745092)) ;
#147202 = CARTESIAN_POINT('Ctrl Pts',(-27.2398427283627,13.2279082414743,
127.650182015427)) ;
#147203 = CARTESIAN_POINT('Ctrl Pts',(-27.226194121743,13.5392233230321,127.643439401524)) ;
#147204 = CARTESIAN_POINT('Ctrl Pts',(-27.2394396068356,13.8421683173594,
127.715246834978)) ;
#147205 = CARTESIAN_POINT('Ctrl Pts',(-27.2780066999911,14.1158320229517,
127.861122787859)) ;
#147206 = CARTESIAN_POINT('Ctrl Pts',(-27.3382205711599,14.3390093108208,
128.070142127096)) ;
#147207 = CARTESIAN_POINT('Ctrl Pts',(-27.4149366221091,14.4964745631391,
128.327319073576)) ;
#147208 = CARTESIAN_POINT('Ctrl Pts',(-27.5021455833055,14.5773715751741,
128.615182034661)) ;
#147209 = CARTESIAN_POINT('Ctrl Pts',(-27.5929606140918,14.5757025299613,
128.913627228843)) ;
#147210 = CARTESIAN_POINT('Ctrl Pts',(-27.6801654786792,14.4908671144554,
129.201599628883)) ;
#147211 = CARTESIAN_POINT('Ctrl Pts',(-27.7560500937159,14.3305923177535,
129.456257297716)) ;
#147212 = CARTESIAN_POINT('Ctrl Pts',(-27.8154777130251,14.1048090701634,
129.663003115917)) ;
#147213 = CARTESIAN_POINT('Ctrl Pts',(-27.8529655928213,13.8293691647795,
129.805723526022)) ;
#147214 = CARTESIAN_POINT('Ctrl Pts',(-27.8650722307394,13.5265763718341,
129.874102214767)) ;
#147215 = CARTESIAN_POINT('Ctrl Pts',(-27.8503095252252,13.2147295079812,
129.864175235836)) ;
#147216 = CARTESIAN_POINT('Ctrl Pts',(-27.8090676741835,12.9189025307067,
129.776765848521)) ;
#147217 = CARTESIAN_POINT('Ctrl Pts',(-27.7431914354456,12.6580299583616,
129.617552969924)) ;
#147218 = CARTESIAN_POINT('Ctrl Pts',(-27.6574792309469,12.4534345786707,
129.400168322233)) ;
#147219 = CARTESIAN_POINT('Ctrl Pts',(-27.5562948938853,12.3171076737635,
129.137795596999)) ;
#147220 = CARTESIAN_POINT('Ctrl Pts',(-27.4470412666183,12.2606844029487,
128.851727105467)) ;
#147221 = CARTESIAN_POINT('Ctrl Pts',(-27.3364454227257,12.2870889528383,
128.561747072364)) ;
#147222 = CARTESIAN_POINT('Ctrl Pts',(-27.2312037738575,12.3957983082861,
128.28758735162)) ;
#147223 = CARTESIAN_POINT('Ctrl Pts',(-27.1395909727778,12.5767257036487,
128.05292203751)) ;
#147224 = CARTESIAN_POINT('Ctrl Pts',(-27.0659643781722,12.818699316301,127.870953859959)) ;
#147225 = CARTESIAN_POINT('Ctrl Pts',(-27.0153388797732,13.105041814552,127.756279306161)) ;
#147226 = CARTESIAN_POINT('Ctrl Pts',(-26.9908956643554,13.4130762761878,
127.717963345236)) ;
#147227 = CARTESIAN_POINT('Ctrl Pts',(-26.9933449092516,13.7214651892491,
127.758172020665)) ;
#147228 = CARTESIAN_POINT('Ctrl Pts',(-27.0218385472917,14.0093161776234,
127.8745403043)) ;
#147229 = CARTESIAN_POINT('Ctrl Pts',(-27.074036131509,14.2560736746046,128.060312178445)) ;
#147230 = CARTESIAN_POINT('Ctrl Pts',(-27.1446201324908,14.4412184345139,
128.299514522)) ;
#147231 = CARTESIAN_POINT('Ctrl Pts',(-27.2283338792895,14.5543182512014,
128.577143613464)) ;
#147232 = CARTESIAN_POINT('Ctrl Pts',(-27.3186446732475,14.5864671227743,
128.874128754955)) ;
#147233 = CARTESIAN_POINT('Ctrl Pts',(-27.4079946957503,14.5351930421584,
129.16826245517)) ;
#147234 = CARTESIAN_POINT('Ctrl Pts',(-27.4893963387798,14.4042256673591,
129.439187707624)) ;
#147235 = CARTESIAN_POINT('Ctrl Pts',(-27.556178276305,14.2033620088234,129.667350441437)) ;
#147236 = CARTESIAN_POINT('Ctrl Pts',(-27.6030960151028,13.9460943123355,
129.837568573444)) ;
#147237 = CARTESIAN_POINT('Ctrl Pts',(-27.625791925615,13.651094014162,129.937042303808)) ;
#147238 = CARTESIAN_POINT('Ctrl Pts',(-27.6220316760032,13.340963258282,129.959100830306)) ;
#147239 = CARTESIAN_POINT('Ctrl Pts',(-27.5913092970485,13.0355469071403,
129.902524920128)) ;
#147240 = CARTESIAN_POINT('Ctrl Pts',(-27.5351586679639,12.7584810147084,
129.771601190251)) ;
#147241 = CARTESIAN_POINT('Ctrl Pts',(-27.456805832877,12.5287898592304,129.575848285187)) ;
#147242 = CARTESIAN_POINT('Ctrl Pts',(-27.3612326647653,12.3633457050948,
129.329763294114)) ;
#147243 = CARTESIAN_POINT('Ctrl Pts',(-27.2545344495649,12.2737023356338,
129.051174297588)) ;
#147244 = CARTESIAN_POINT('Ctrl Pts',(-27.1434004213349,12.2663504555484,
128.759683649007)) ;
#147245 = CARTESIAN_POINT('Ctrl Pts',(-27.0353422164726,12.3420801358765,
128.477156085888)) ;
#147246 = CARTESIAN_POINT('Ctrl Pts',(-26.9375649820687,12.4946576254463,
128.224562106625)) ;
#147247 = CARTESIAN_POINT('Ctrl Pts',(-26.8556736032525,12.7142649717312,
128.018500360345)) ;
#147248 = CARTESIAN_POINT('Ctrl Pts',(-26.7952452994607,12.9853994961716,
127.875192560308)) ;
#147249 = CARTESIAN_POINT('Ctrl Pts',(-26.7600758607061,13.2860374615536,
127.805462444181)) ;
#147250 = CARTESIAN_POINT('Ctrl Pts',(-26.7515328287848,13.5985522242575,
127.813742362503)) ;
#147251 = CARTESIAN_POINT('Ctrl Pts',(-26.7698756432365,13.8975128735152,
127.900464759074)) ;
#147252 = CARTESIAN_POINT('Ctrl Pts',(-26.8125360422085,14.1612606569833,
128.058053439872)) ;
#147253 = CARTESIAN_POINT('Ctrl Pts',(-26.8763333439844,14.3739608476098,
128.277609007069)) ;
#147254 = CARTESIAN_POINT('Ctrl Pts',(-26.9559480791001,14.518294704107,128.543420710541)) ;
#147255 = CARTESIAN_POINT('Ctrl Pts',(-27.0443940887923,14.5834512840226,
128.834899340936)) ;
#147256 = CARTESIAN_POINT('Ctrl Pts',(-27.1346038864515,14.5659482192211,
129.131417292674)) ;
#147257 = CARTESIAN_POINT('Ctrl Pts',(-27.2200732093609,14.4667697740707,
129.414216297154)) ;
#147258 = CARTESIAN_POINT('Ctrl Pts',(-27.2937703844988,14.2923285700355,
129.662701599611)) ;
#147259 = CARTESIAN_POINT('Ctrl Pts',(-27.3494004042238,14.0548140486651,
129.858453434174)) ;
#147260 = CARTESIAN_POINT('Ctrl Pts',(-27.3820270800496,13.7751054294997,
129.986645187117)) ;
#147261 = CARTESIAN_POINT('Ctrl Pts',(-27.3893034306534,13.4671706932676,
130.041144761007)) ;
#147262 = CARTESIAN_POINT('Ctrl Pts',(-27.3693096962278,13.1566326789877,
130.015914968687)) ;
#147263 = CARTESIAN_POINT('Ctrl Pts',(-27.3234453767361,12.8670308674408,
129.91489111767)) ;
#147264 = CARTESIAN_POINT('Ctrl Pts',(-27.2533334364548,12.6146257445343,
129.743351676563)) ;
#147265 = CARTESIAN_POINT('Ctrl Pts',(-27.1639433566548,12.4216271707414,
129.515355134645)) ;
#147266 = CARTESIAN_POINT('Ctrl Pts',(-27.0613606146514,12.3004936343569,
129.248664903975)) ;
#147267 = CARTESIAN_POINT('Ctrl Pts',(-26.9507521852777,12.2591976943178,
128.958810361861)) ;
#147268 = CARTESIAN_POINT('Ctrl Pts',(-26.8410653311802,12.3014766465694,
128.671386114435)) ;
#147269 = CARTESIAN_POINT('Ctrl Pts',(-26.7381556212626,12.4236752423031,
128.403872346275)) ;
#147270 = CARTESIAN_POINT('Ctrl Pts',(-26.6486024466278,12.6191375568078,
128.175587812738)) ;
#147271 = CARTESIAN_POINT('Ctrl Pts',(-26.5792953547801,12.8707902400354,
128.006190100915)) ;
#147272 = CARTESIAN_POINT('Ctrl Pts',(-26.5336332509194,13.1617413268143,
127.905867012926)) ;
#147273 = CARTESIAN_POINT('Ctrl Pts',(-26.5141802488474,13.4713352737269,
127.882101279265)) ;
#147274 = CARTESIAN_POINT('Ctrl Pts',(-26.5216819221517,13.7785022138413,
127.937189629823)) ;
#147275 = CARTESIAN_POINT('Ctrl Pts',(-26.5549217794985,14.0596469368124,
128.067407385282)) ;
#147276 = CARTESIAN_POINT('Ctrl Pts',(-26.610728225856,14.2953142567661,128.263552793007)) ;
#147277 = CARTESIAN_POINT('Ctrl Pts',(-26.684686815018,14.4689647332084,128.512830919732)) ;
#147278 = CARTESIAN_POINT('Ctrl Pts',(-26.7703491580962,14.5668407340065,
128.796212142762)) ;
#147279 = CARTESIAN_POINT('Ctrl Pts',(-26.8605101017941,14.5831863615057,
129.092558768383)) ;
#147280 = CARTESIAN_POINT('Ctrl Pts',(-26.9493781611684,14.5160479174659,
129.385470762593)) ;
#147281 = CARTESIAN_POINT('Ctrl Pts',(-27.0282194316067,14.3710573530436,
129.648813233255)) ;
#147282 = CARTESIAN_POINT('Ctrl Pts',(-27.0915895135471,14.1586832186318,
129.866986504732)) ;
#147283 = CARTESIAN_POINT('Ctrl Pts',(-27.1342318596262,13.8924168097658,
130.02475813213)) ;
#147284 = CARTESIAN_POINT('Ctrl Pts',(-27.1520214448119,13.5934590630732,
130.109811091012)) ;
#147285 = CARTESIAN_POINT('Ctrl Pts',(-27.1431457178143,13.2817949508325,
130.117027448321)) ;
#147286 = CARTESIAN_POINT('Ctrl Pts',(-27.107478861766,12.9807520838768,130.045927154159)) ;
#147287 = CARTESIAN_POINT('Ctrl Pts',(-27.0469864938312,12.7114088692144,
129.902283115458)) ;
#147288 = CARTESIAN_POINT('Ctrl Pts',(-26.9647202422579,12.4920355710748,
129.695194113043)) ;
#147289 = CARTESIAN_POINT('Ctrl Pts',(-26.8666704559515,12.3404092306431,
129.441827358629)) ;
#147290 = CARTESIAN_POINT('Ctrl Pts',(-26.7584759114317,12.2658594230555,
129.158914687965)) ;
#147291 = CARTESIAN_POINT('Ctrl Pts',(-26.647473216562,12.2744067792623,128.867771365807)) ;
#147292 = CARTESIAN_POINT('Ctrl Pts',(-26.5408791869932,12.3651073701196,
128.58948675102)) ;
#147293 = CARTESIAN_POINT('Ctrl Pts',(-26.4454504393884,12.5316552741645,
128.343844417814)) ;
#147294 = CARTESIAN_POINT('Ctrl Pts',(-26.3673650678726,12.7621961418758,
128.148878346518)) ;
#147295 = CARTESIAN_POINT('Ctrl Pts',(-26.3115589819965,13.0400249210017,
128.018983277286)) ;
#147296 = CARTESIAN_POINT('Ctrl Pts',(-26.2812519148647,13.3449925039121,
127.963545408573)) ;
#147297 = CARTESIAN_POINT('Ctrl Pts',(-26.2778797392448,13.6560824350963,
127.986850254171)) ;
#147298 = CARTESIAN_POINT('Ctrl Pts',(-26.3008975455134,13.9495230290834,
128.087137834312)) ;
#147299 = CARTESIAN_POINT('Ctrl Pts',(-26.3479782652609,14.2060602053469,
128.257797236022)) ;
#147300 = CARTESIAN_POINT('Ctrl Pts',(-26.415271572287,14.4068533701998,128.487586750175)) ;
#147301 = CARTESIAN_POINT('Ctrl Pts',(-26.4967691286776,14.5364834485285,
128.758756328545)) ;
#147302 = CARTESIAN_POINT('Ctrl Pts',(-26.586194501111,14.5865952297017,129.053116471795)) ;
#147303 = CARTESIAN_POINT('Ctrl Pts',(-26.6763590123459,14.553289693682,129.349636823295)) ;
#147304 = CARTESIAN_POINT('Ctrl Pts',(-26.7600228764154,14.4391769973074,
129.627142397581)) ;
#147305 = CARTESIAN_POINT('Ctrl Pts',(-26.8305563269227,14.2521193924325,
129.866320001124)) ;
#147306 = CARTESIAN_POINT('Ctrl Pts',(-26.8821056983442,14.0064610013992,
130.049955365184)) ;
#147307 = CARTESIAN_POINT('Ctrl Pts',(-26.9104630889835,13.7162751839027,
130.166152471987)) ;
#147308 = CARTESIAN_POINT('Ctrl Pts',(-26.9124439133158,13.4088590372776,
130.204864159524)) ;
#147309 = CARTESIAN_POINT('Ctrl Pts',(-26.8876203324447,13.1005339015723,
130.165487747714)) ;
#147310 = CARTESIAN_POINT('Ctrl Pts',(-26.8367036547029,12.8153801442626,
130.049891561204)) ;
#147311 = CARTESIAN_POINT('Ctrl Pts',(-26.7630941930023,12.5742829419459,
129.867895511603)) ;
#147312 = CARTESIAN_POINT('Ctrl Pts',(-26.6700181781098,12.3924207775489,
129.62937532917)) ;
#147313 = CARTESIAN_POINT('Ctrl Pts',(-26.5657046350372,12.2864008537638,
129.357568602088)) ;
#147314 = CARTESIAN_POINT('Ctrl Pts',(-26.4545900751574,12.2608494079679,
129.066227997659)) ;
#147315 = CARTESIAN_POINT('Ctrl Pts',(-26.345767615669,12.3186106579848,128.781313857206)) ;
#147316 = CARTESIAN_POINT('Ctrl Pts',(-26.2448324759386,12.4554523175926,
128.519622374665)) ;
#147317 = CARTESIAN_POINT('Ctrl Pts',(-26.1588332332188,12.6626735352652,
128.301638928963)) ;
#147318 = CARTESIAN_POINT('Ctrl Pts',(-26.0938900095568,12.9221025997255,
128.144867830553)) ;
#147319 = CARTESIAN_POINT('Ctrl Pts',(-26.0527924934696,13.2188658748081,
128.057962797512)) ;
#147320 = CARTESIAN_POINT('Ctrl Pts',(-26.0384362022978,13.5309969609299,
128.049243549581)) ;
#147321 = CARTESIAN_POINT('Ctrl Pts',(-26.0508964161626,13.8333910291505,
128.118640022779)) ;
#147322 = CARTESIAN_POINT('Ctrl Pts',(-26.0887248099249,14.1082732516314,
128.262358068777)) ;
#147323 = CARTESIAN_POINT('Ctrl Pts',(-26.1483616887784,14.3332733930533,
128.469696784862)) ;
#147324 = CARTESIAN_POINT('Ctrl Pts',(-26.2248538967359,14.4930899265818,
128.726293642741)) ;
#147325 = CARTESIAN_POINT('Ctrl Pts',(-26.3117593915966,14.5762694731203,
129.013227399328)) ;
#147326 = CARTESIAN_POINT('Ctrl Pts',(-26.4029117585351,14.5766426477847,
129.3127891345)) ;
#147327 = CARTESIAN_POINT('Ctrl Pts',(-26.4895350988602,14.4950561808568,
129.598750745687)) ;
#147328 = CARTESIAN_POINT('Ctrl Pts',(-26.5665136204875,14.3357812745788,
129.856885878982)) ;
#147329 = CARTESIAN_POINT('Ctrl Pts',(-26.6262592796755,14.1117726317635,
130.064489680492)) ;
#147330 = CARTESIAN_POINT('Ctrl Pts',(-26.664428327791,13.8385112435954,130.209095717924)) ;
#147331 = CARTESIAN_POINT('Ctrl Pts',(-26.6772984039839,13.5338962434735,
130.27996038854)) ;
#147332 = CARTESIAN_POINT('Ctrl Pts',(-26.6633735809435,13.2242575692473,
130.272227496551)) ;
#147333 = CARTESIAN_POINT('Ctrl Pts',(-26.6226746960282,12.9262819012927,
130.18657442431)) ;
#147334 = CARTESIAN_POINT('Ctrl Pts',(-26.5578472919816,12.6654698435916,
130.03022959216)) ;
#147335 = CARTESIAN_POINT('Ctrl Pts',(-26.4718376309163,12.4574146101121,
129.812281248977)) ;
#147336 = CARTESIAN_POINT('Ctrl Pts',(-26.3720422424379,12.3205165550688,
129.553606148421)) ;
#147337 = CARTESIAN_POINT('Ctrl Pts',(-26.2623404084189,12.2610390468186,
129.266423763094)) ;
#147338 = CARTESIAN_POINT('Ctrl Pts',(-26.1520390344193,12.2851065141721,
128.97719162075)) ;
#147339 = CARTESIAN_POINT('Ctrl Pts',(-26.0464052214175,12.3913707511119,
128.701919778819)) ;
#147340 = CARTESIAN_POINT('Ctrl Pts',(-25.9542397322552,12.5705078775683,
128.465670763245)) ;
#147341 = CARTESIAN_POINT('Ctrl Pts',(-25.8800073520596,12.8110530886845,
128.281943454991)) ;
#147342 = CARTESIAN_POINT('Ctrl Pts',(-25.8287174453691,13.0958080980136,
128.16526124174)) ;
#147343 = CARTESIAN_POINT('Ctrl Pts',(-25.8034286370072,13.4043791366155,
128.124575677788)) ;
#147344 = CARTESIAN_POINT('Ctrl Pts',(-25.8050680904062,13.7127503618814,
128.162374639568)) ;
#147345 = CARTESIAN_POINT('Ctrl Pts',(-25.8331792366338,14.0031465413693,
128.277846201473)) ;
#147346 = CARTESIAN_POINT('Ctrl Pts',(-25.8840548911354,14.2480984891944,
128.459304631545)) ;
#147347 = CARTESIAN_POINT('Ctrl Pts',(-25.9545856190801,14.4370589148149,
128.698609955357)) ;
#147348 = CARTESIAN_POINT('Ctrl Pts',(-26.0380121218444,14.5521322470153,
128.975377743495)) ;
#147349 = CARTESIAN_POINT('Ctrl Pts',(-26.1283292300662,14.5867077632741,
129.272419970589)) ;
#147350 = CARTESIAN_POINT('Ctrl Pts',(-26.2176425716056,14.5378478961583,
129.566384402424)) ;
#147351 = CARTESIAN_POINT('Ctrl Pts',(-26.2993554539816,14.4092030329905,
129.838211853804)) ;
#147352 = CARTESIAN_POINT('Ctrl Pts',(-26.3667060054575,14.2102655256447,
130.068042548754)) ;
#147353 = CARTESIAN_POINT('Ctrl Pts',(-26.4143965075339,13.953116489833,130.240663994916)) ;
#147354 = CARTESIAN_POINT('Ctrl Pts',(-26.4376848856322,13.6605445363077,
130.341677819469)) ;
#147355 = CARTESIAN_POINT('Ctrl Pts',(-26.4347158653785,13.3493859858442,
130.366180421727)) ;
#147356 = CARTESIAN_POINT('Ctrl Pts',(-26.4048124301675,13.0444135456855,
130.311894349898)) ;
#147357 = CARTESIAN_POINT('Ctrl Pts',(-26.3493229430599,12.7658508988887,
130.182947087287)) ;
#147358 = CARTESIAN_POINT('Ctrl Pts',(-26.2715830488278,12.5346698659633,
129.988965884616)) ;
#147359 = CARTESIAN_POINT('Ctrl Pts',(-26.1762853786461,12.3668713025773,
129.743737589104)) ;
#147360 = CARTESIAN_POINT('Ctrl Pts',(-26.069606670302,12.2750736510529,129.465261546678)) ;
#147361 = CARTESIAN_POINT('Ctrl Pts',(-25.9590624120991,12.2654123837922,
129.175324576531)) ;
#147362 = CARTESIAN_POINT('Ctrl Pts',(-25.8507386841537,12.3385001121927,
128.89203884047)) ;
#147363 = CARTESIAN_POINT('Ctrl Pts',(-25.7523129533691,12.4893940977294,
128.637638133927)) ;
#147364 = CARTESIAN_POINT('Ctrl Pts',(-25.6700022058392,12.7071835395625,
128.430318876464)) ;
#147365 = CARTESIAN_POINT('Ctrl Pts',(-25.6090294076232,12.9760086815988,
128.285301835029)) ;
#147366 = CARTESIAN_POINT('Ctrl Pts',(-25.5729252411528,13.2771671350434,
128.212971047945)) ;
#147367 = CARTESIAN_POINT('Ctrl Pts',(-25.5636314421838,13.5885363726329,
128.218931944683)) ;
#147368 = CARTESIAN_POINT('Ctrl Pts',(-25.5810657627957,13.8883474938027,
128.303005296954)) ;
#147369 = CARTESIAN_POINT('Ctrl Pts',(-25.6232704125892,14.1546797324028,
128.45942516704)) ;
#147370 = CARTESIAN_POINT('Ctrl Pts',(-25.6864051786995,14.3683945164845,
128.676955004146)) ;
#147371 = CARTESIAN_POINT('Ctrl Pts',(-25.7652853789973,14.5146640414989,
128.940493836316)) ;
#147372 = CARTESIAN_POINT('Ctrl Pts',(-25.8538439793988,14.5827891573481,
129.232415670476)) ;
#147373 = CARTESIAN_POINT('Ctrl Pts',(-25.9443062053087,14.5676065967762,
129.52974540677)) ;
#147374 = CARTESIAN_POINT('Ctrl Pts',(-26.0299884903879,14.4706131159399,
129.813160378237)) ;
#147375 = CARTESIAN_POINT('Ctrl Pts',(-26.1039155103848,14.2987449000821,
130.062221274369)) ;
#147376 = CARTESIAN_POINT('Ctrl Pts',(-26.1602098677861,14.063095802434,130.259906440819)) ;
#147377 = CARTESIAN_POINT('Ctrl Pts',(-26.1937049681925,13.7833208359645,
130.390765918343)) ;
#147378 = CARTESIAN_POINT('Ctrl Pts',(-26.2016332025184,13.4754883225496,
130.447200559689)) ;
#147379 = CARTESIAN_POINT('Ctrl Pts',(-26.182591675332,13.1664272763286,130.424565803854)) ;
#147380 = CARTESIAN_POINT('Ctrl Pts',(-26.1372145619655,12.8743475214726,
130.325153027451)) ;
#147381 = CARTESIAN_POINT('Ctrl Pts',(-26.0681100485298,12.6220180673462,
130.156364599778)) ;
#147382 = CARTESIAN_POINT('Ctrl Pts',(-25.9791355180504,12.4263341483682,
129.929648965762)) ;
#147383 = CARTESIAN_POINT('Ctrl Pts',(-25.8762687412122,12.302605659073,129.662304783115)) ;
#147384 = CARTESIAN_POINT('Ctrl Pts',(-25.7664265682515,12.2593725247806,
129.374490277057)) ;
#147385 = CARTESIAN_POINT('Ctrl Pts',(-25.6565009947126,12.2987734021689,
129.086399334671)) ;
#147386 = CARTESIAN_POINT('Ctrl Pts',(-25.5525415623039,12.4202091773167,
128.816083115814)) ;
#147387 = CARTESIAN_POINT('Ctrl Pts',(-25.463523806087,12.6117736562181,128.588993280005)) ;
#147388 = CARTESIAN_POINT('Ctrl Pts',(-25.3931975895658,12.8626551569237,
128.416749070774)) ;
#147389 = CARTESIAN_POINT('Ctrl Pts',(-25.3468388426278,13.1527448320073,
128.314381265538)) ;
#147390 = CARTESIAN_POINT('Ctrl Pts',(-25.3265594515291,13.4624297819909,
128.288238626184)) ;
#147391 = CARTESIAN_POINT('Ctrl Pts',(-25.333337476772,13.7701810821573,128.34123302125)) ;
#147392 = CARTESIAN_POINT('Ctrl Pts',(-25.3658008060248,14.0517728376964,
128.469114625698)) ;
#147393 = CARTESIAN_POINT('Ctrl Pts',(-25.4210139847123,14.2892526795151,
128.663546384413)) ;
#147394 = CARTESIAN_POINT('Ctrl Pts',(-25.4945519789554,14.4648240216747,
128.911599442644)) ;
#147395 = CARTESIAN_POINT('Ctrl Pts',(-25.579674277019,14.5650403080843,129.193298266083)) ;
#147396 = CARTESIAN_POINT('Ctrl Pts',(-25.67036522595,14.5837489578772,129.491409968998)) ;
#147397 = CARTESIAN_POINT('Ctrl Pts',(-25.7585912679521,14.519716790758,129.782133273891)) ;
#147398 = CARTESIAN_POINT('Ctrl Pts',(-25.8383866398907,14.3763314788885,
130.04848919323)) ;
#147399 = CARTESIAN_POINT('Ctrl Pts',(-25.9022469285143,14.1656645339802,
130.26807856477)) ;
#147400 = CARTESIAN_POINT('Ctrl Pts',(-25.9456274021111,13.8999128484359,
130.428097361213)) ;
#147401 = CARTESIAN_POINT('Ctrl Pts',(-25.9640567630253,13.6028235446839,
130.514880792807)) ;
#147402 = CARTESIAN_POINT('Ctrl Pts',(-25.9560293185912,13.291184558806,130.5245814653)) ;
#147403 = CARTESIAN_POINT('Ctrl Pts',(-25.9211626506794,12.9894030516706,
130.455825428731)) ;
#147404 = CARTESIAN_POINT('Ctrl Pts',(-25.8610673900144,12.7177659651588,
130.313481364272)) ;
#147405 = CARTESIAN_POINT('Ctrl Pts',(-25.7793965335319,12.49725897855,130.108081193746)) ;
#147406 = CARTESIAN_POINT('Ctrl Pts',(-25.6820096977712,12.3438957408669,
129.856561080609)) ;
#147407 = CARTESIAN_POINT('Ctrl Pts',(-25.5739096114305,12.2668705214432,
129.573956876957)) ;
#147408 = CARTESIAN_POINT('Ctrl Pts',(-25.4630100257819,12.2729078136877,
129.283075556305)) ;
#147409 = CARTESIAN_POINT('Ctrl Pts',(-25.356027244478,12.3614501444855,129.003710369665)) ;
#147410 = CARTESIAN_POINT('Ctrl Pts',(-25.2604256897816,12.5253315069565,
128.757464536731)) ;
#147411 = CARTESIAN_POINT('Ctrl Pts',(-25.1814030954091,12.75527704082,128.559915933982)) ;
#147412 = CARTESIAN_POINT('Ctrl Pts',(-25.1251196612894,13.0310569738766,
128.428504091722)) ;
#147413 = CARTESIAN_POINT('Ctrl Pts',(-25.0939685502416,13.336121760913,128.370672083575)) ;
#147414 = CARTESIAN_POINT('Ctrl Pts',(-25.089777654312,13.6463105031288,128.39146772838)) ;
#147415 = CARTESIAN_POINT('Ctrl Pts',(-25.1121607797936,13.942487386476,128.490115395761)) ;
#147416 = CARTESIAN_POINT('Ctrl Pts',(-25.1587979741093,14.2002009126819,
128.659500935617)) ;
#147417 = CARTESIAN_POINT('Ctrl Pts',(-25.2251350521265,14.4015262560108,
128.886278135871)) ;
#147418 = CARTESIAN_POINT('Ctrl Pts',(-25.3065076717985,14.5339054968789,
129.157180214865)) ;
#147419 = CARTESIAN_POINT('Ctrl Pts',(-25.3957504816741,14.5863178640126,
129.450982591655)) ;
#147420 = CARTESIAN_POINT('Ctrl Pts',(-25.4862345240099,14.5553221759541,
129.748523545111)) ;
#147421 = CARTESIAN_POINT('Ctrl Pts',(-25.5701152155034,14.4431215041297,
130.026657665419)) ;
#147422 = CARTESIAN_POINT('Ctrl Pts',(-25.6408625622055,14.2589451929284,
130.266317223022)) ;
#147423 = CARTESIAN_POINT('Ctrl Pts',(-25.6932705534346,14.0132050920919,
130.452661573645)) ;
#147424 = CARTESIAN_POINT('Ctrl Pts',(-25.7221401451884,13.7264814749198,
130.570060326567)) ;
#147425 = CARTESIAN_POINT('Ctrl Pts',(-25.7249810058714,13.4166671234753,
130.611582683641)) ;
#147426 = CARTESIAN_POINT('Ctrl Pts',(-25.7008673309746,13.1090562116308,
130.57416706686)) ;
#147427 = CARTESIAN_POINT('Ctrl Pts',(-25.650705201746,12.82289367226,130.460777367842)) ;
#147428 = CARTESIAN_POINT('Ctrl Pts',(-25.5776200733177,12.5803482566307,
130.280325138346)) ;
#147429 = CARTESIAN_POINT('Ctrl Pts',(-25.4854578756859,12.3971382864686,
130.044324611692)) ;
#147430 = CARTESIAN_POINT('Ctrl Pts',(-25.3808890229052,12.2881794770673,
129.771944567501)) ;
#147431 = CARTESIAN_POINT('Ctrl Pts',(-25.2700108769558,12.2604447735571,
129.481239923333)) ;
#147432 = CARTESIAN_POINT('Ctrl Pts',(-25.1608183013244,12.3158800471475,
129.195310553149)) ;
#147433 = CARTESIAN_POINT('Ctrl Pts',(-25.0594670901994,12.4512316162553,
128.932457223453)) ;
#147434 = CARTESIAN_POINT('Ctrl Pts',(-24.9736427412008,12.6546809483565,
128.714694415)) ;
#147435 = CARTESIAN_POINT('Ctrl Pts',(-24.9074766800191,12.9147731293523,
128.554622339809)) ;
#147436 = CARTESIAN_POINT('Ctrl Pts',(-24.8658875479562,13.2095559485039,
128.466127574624)) ;
#147437 = CARTESIAN_POINT('Ctrl Pts',(-24.850668730366,13.5223874270332,128.454982787526)) ;
#147438 = CARTESIAN_POINT('Ctrl Pts',(-24.862374550478,13.825017500004,128.522137475361)) ;
#147439 = CARTESIAN_POINT('Ctrl Pts',(-24.899721165262,14.1019895669497,128.66457954536)) ;
#147440 = CARTESIAN_POINT('Ctrl Pts',(-24.9585507005245,14.3273312659445,
128.869390260325)) ;
#147441 = CARTESIAN_POINT('Ctrl Pts',(-25.0345366141788,14.4893435493457,
129.124486798499)) ;
#147442 = CARTESIAN_POINT('Ctrl Pts',(-25.1213275613785,14.5749600096558,
129.411124229977)) ;
#147443 = CARTESIAN_POINT('Ctrl Pts',(-25.2123749716485,14.5779281254001,
129.710338631677)) ;
#147444 = CARTESIAN_POINT('Ctrl Pts',(-25.2994338403886,14.4983365281884,
129.997670388463)) ;
#147445 = CARTESIAN_POINT('Ctrl Pts',(-25.3764852172115,14.3420896185929,
130.255855966299)) ;
#147446 = CARTESIAN_POINT('Ctrl Pts',(-25.4372612466155,14.1180211548404,
130.466732396769)) ;
#147447 = CARTESIAN_POINT('Ctrl Pts',(-25.4757954504626,13.8471808602615,
130.612225812772)) ;
#147448 = CARTESIAN_POINT('Ctrl Pts',(-25.4895325193993,13.5439413026185,
130.685549031096)) ;
#147449 = CARTESIAN_POINT('Ctrl Pts',(-25.4763877137705,13.2331634650753,
130.680205857451)) ;
#147450 = CARTESIAN_POINT('Ctrl Pts',(-25.436417688245,12.9343808446189,130.59668869728)) ;
#147451 = CARTESIAN_POINT('Ctrl Pts',(-25.3721536694258,12.672197812707,130.442015902959)) ;
#147452 = CARTESIAN_POINT('Ctrl Pts',(-25.2871759098898,12.4632419540624,
130.226903985326)) ;
#147453 = CARTESIAN_POINT('Ctrl Pts',(-25.1871271731951,12.3231158661213,
129.96769991366)) ;
#147454 = CARTESIAN_POINT('Ctrl Pts',(-25.0775746371766,12.2616017897263,
129.680943711049)) ;
#147455 = CARTESIAN_POINT('Ctrl Pts',(-24.9674177556154,12.2833201820527,
129.392078348861)) ;
#147456 = CARTESIAN_POINT('Ctrl Pts',(-24.8617121590519,12.3868877345153,
129.116527833986)) ;
#147457 = CARTESIAN_POINT('Ctrl Pts',(-24.7686713370083,12.5648231371291,
128.877870667661)) ;
#147458 = CARTESIAN_POINT('Ctrl Pts',(-24.6939731377639,12.8039602179339,
128.692766032637)) ;
#147459 = CARTESIAN_POINT('Ctrl Pts',(-24.6421512068702,13.0864729050957,
128.57439142321)) ;
#147460 = CARTESIAN_POINT('Ctrl Pts',(-24.6159486541681,13.3957238460679,
128.531150167993)) ;
#147461 = CARTESIAN_POINT('Ctrl Pts',(-24.6169248165692,13.7038340446914,
128.566964483066)) ;
#147462 = CARTESIAN_POINT('Ctrl Pts',(-24.6439310731031,13.9936201440332,
128.678997984667)) ;
#147463 = CARTESIAN_POINT('Ctrl Pts',(-24.694875907643,14.2431366555827,128.861092575931)) ;
#147464 = CARTESIAN_POINT('Ctrl Pts',(-24.7642561700479,14.4318623927357,
129.096682946381)) ;
#147465 = CARTESIAN_POINT('Ctrl Pts',(-24.847909290222,14.5502397441639,129.374344984616)) ;
#147466 = CARTESIAN_POINT('Ctrl Pts',(-24.9379186092033,14.5868194745111,
129.670393657069)) ;
#147467 = CARTESIAN_POINT('Ctrl Pts',(-25.0274560736447,14.5403267792944,
129.96505775103)) ;
#147468 = CARTESIAN_POINT('Ctrl Pts',(-25.1094619526943,14.4138414926087,
130.237727564842)) ;
#147469 = CARTESIAN_POINT('Ctrl Pts',(-25.1773154114334,14.2163546967306,
130.469065398273)) ;
#147470 = CARTESIAN_POINT('Ctrl Pts',(-25.2253773054646,13.962464783628,130.642541368542)) ;
#147471 = CARTESIAN_POINT('Ctrl Pts',(-25.24961618706,13.6693367580008,130.746502542024)) ;
#147472 = CARTESIAN_POINT('Ctrl Pts',(-25.2474068337107,13.3586798418074,
130.773184087954)) ;
#147473 = CARTESIAN_POINT('Ctrl Pts',(-25.2182356406182,13.0526929530247,
130.721098440752)) ;
#147474 = CARTESIAN_POINT('Ctrl Pts',(-25.1634305798166,12.7731728077457,
130.594139490751)) ;
#147475 = CARTESIAN_POINT('Ctrl Pts',(-25.0862589189529,12.5404162023862,
130.401820361483)) ;
#147476 = CARTESIAN_POINT('Ctrl Pts',(-24.9914844710839,12.3707607989948,
130.158084215147)) ;
#147477 = CARTESIAN_POINT('Ctrl Pts',(-24.8850624365054,12.2766729601255,
129.880354699258)) ;
#147478 = CARTESIAN_POINT('Ctrl Pts',(-24.7745883557454,12.2643218460961,
129.59060471869)) ;
#147479 = CARTESIAN_POINT('Ctrl Pts',(-24.665300865596,12.3360206522436,129.304757619663)) ;
#147480 = CARTESIAN_POINT('Ctrl Pts',(-24.5674413550508,12.4836397048973,
129.051702486663)) ;
#147481 = CARTESIAN_POINT('Ctrl Pts',(-24.4841980631826,12.7003319185399,
128.841794655393)) ;
#147482 = CARTESIAN_POINT('Ctrl Pts',(-24.4226430737707,12.9678917727225,
128.695053256231)) ;
#147483 = CARTESIAN_POINT('Ctrl Pts',(-24.3857571441025,13.2687869300656,
128.62048000068)) ;
#147484 = CARTESIAN_POINT('Ctrl Pts',(-24.3757550894969,13.5800035034693,
128.624353835401)) ;
#147485 = CARTESIAN_POINT('Ctrl Pts',(-24.3924109780588,13.8799729722643,
128.706099674378)) ;
#147486 = CARTESIAN_POINT('Ctrl Pts',(-24.4339595637666,14.14769940646,128.860620861967)) ;
#147487 = CARTESIAN_POINT('Ctrl Pts',(-24.4965774264268,14.3632524598664,
129.076651664713)) ;
#147488 = CARTESIAN_POINT('Ctrl Pts',(-24.5753469438563,14.511933585639,129.339964185627)) ;
#147489 = CARTESIAN_POINT('Ctrl Pts',(-24.6636723624433,14.5819602156047,
129.631172820673)) ;
#147490 = CARTESIAN_POINT('Ctrl Pts',(-24.7538880579223,14.5692454320411,
129.927679411565)) ;
#147491 = CARTESIAN_POINT('Ctrl Pts',(-24.8400111036722,14.4742854665662,
130.212461777541)) ;
#147492 = CARTESIAN_POINT('Ctrl Pts',(-24.9141474049248,14.3047439211162,
130.462048740383)) ;
#147493 = CARTESIAN_POINT('Ctrl Pts',(-24.9710435495452,14.0710831127117,
130.66146131265)) ;
#147494 = CARTESIAN_POINT('Ctrl Pts',(-25.0053326588705,13.7914036460412,
130.794750491077)) ;
#147495 = CARTESIAN_POINT('Ctrl Pts',(-25.0139823256091,13.4850123175133,
130.853182599625)) ;
#147496 = CARTESIAN_POINT('Ctrl Pts',(-24.9957867875723,13.1755843986706,
130.833035511702)) ;
#147497 = CARTESIAN_POINT('Ctrl Pts',(-24.9510844064904,12.8823157698566,
130.735635283545)) ;
#147498 = CARTESIAN_POINT('Ctrl Pts',(-24.8826220204888,12.628436297888,130.568728677609)) ;
#147499 = CARTESIAN_POINT('Ctrl Pts',(-24.7937281426364,12.4304595196238,
130.342377740803)) ;
#147500 = CARTESIAN_POINT('Ctrl Pts',(-24.6919949244802,12.3053999531995,
130.078078985158)) ;
#147501 = CARTESIAN_POINT('Ctrl Pts',(-24.5813762118716,12.2593484395974,
129.788270620212)) ;
#147502 = CARTESIAN_POINT('Ctrl Pts',(-24.4718806439112,12.2965483924972,
129.501275586179)) ;
#147503 = CARTESIAN_POINT('Ctrl Pts',(-24.3675517835472,12.4156949312687,
129.229904709214)) ;
#147504 = CARTESIAN_POINT('Ctrl Pts',(-24.2781540160857,12.6050470802083,
129.001655484171)) ;
#147505 = CARTESIAN_POINT('Ctrl Pts',(-24.2070200380848,12.8553420969347,
128.827159977025)) ;
#147506 = CARTESIAN_POINT('Ctrl Pts',(-24.1601461823753,13.14294545291,128.723103202303)) ;
#147507 = CARTESIAN_POINT('Ctrl Pts',(-24.1389317962829,13.4543916932758,
128.694450505378)) ;
#147508 = CARTESIAN_POINT('Ctrl Pts',(-24.1449949752851,13.7614619882681,
128.745238827839)) ;
#147509 = CARTESIAN_POINT('Ctrl Pts',(-24.1768158430516,14.0447128123048,
128.871321579809)) ;
#147510 = CARTESIAN_POINT('Ctrl Pts',(-24.231333547993,14.2828872878416,129.063626721277)) ;
#147511 = CARTESIAN_POINT('Ctrl Pts',(-24.3041010172989,14.4603132279032,
129.309318834514)) ;
#147512 = CARTESIAN_POINT('Ctrl Pts',(-24.3896352702838,14.5634617408265,
129.592480733006)) ;
#147513 = CARTESIAN_POINT('Ctrl Pts',(-24.4795823186102,14.5844329912441,
129.888156786475)) ;
#147514 = CARTESIAN_POINT('Ctrl Pts',(-24.5685724115342,14.5225343527704,
130.181342201958)) ;
#147515 = CARTESIAN_POINT('Ctrl Pts',(-24.6484337252993,14.3815448492318,
130.447775913898)) ;
#147516 = CARTESIAN_POINT('Ctrl Pts',(-24.7128675060765,14.172575531033,130.669066255997)) ;
#147517 = CARTESIAN_POINT('Ctrl Pts',(-24.7567752762927,13.9093041266096,
130.830484961807)) ;
#147518 = CARTESIAN_POINT('Ctrl Pts',(-24.7761511782523,13.6121559231782,
130.920131335962)) ;
#147519 = CARTESIAN_POINT('Ctrl Pts',(-24.7687788447022,13.2990171970743,
130.93190911656)) ;
#147520 = CARTESIAN_POINT('Ctrl Pts',(-24.7347587150341,12.998156604328,130.865468282676)) ;
#147521 = CARTESIAN_POINT('Ctrl Pts',(-24.6755494930383,12.7257033246492,
130.725651376967)) ;
#147522 = CARTESIAN_POINT('Ctrl Pts',(-24.5943950553872,12.5030758718665,
130.521797413364)) ;
#147523 = CARTESIAN_POINT('Ctrl Pts',(-24.4972021110052,12.3471530104355,
130.270914197217)) ;
#147524 = CARTESIAN_POINT('Ctrl Pts',(-24.3888920694182,12.2678408684918,
129.987814315935)) ;
#147525 = CARTESIAN_POINT('Ctrl Pts',(-24.2786242157361,12.2715869144481,
129.698586587052)) ;
#147526 = CARTESIAN_POINT('Ctrl Pts',(-24.1712851072626,12.3575775842601,
129.41821433343)) ;
#147527 = CARTESIAN_POINT('Ctrl Pts',(-24.075122506587,12.5198591790598,129.170392897351)) ;
#147528 = CARTESIAN_POINT('Ctrl Pts',(-23.9957490620432,12.7472700388984,
128.971705039795)) ;
#147529 = CARTESIAN_POINT('Ctrl Pts',(-23.9384956276451,13.0233714187906,
128.837633345603)) ;
#147530 = CARTESIAN_POINT('Ctrl Pts',(-23.906768899648,13.3264774895314,128.777955771663)) ;
#147531 = CARTESIAN_POINT('Ctrl Pts',(-23.9017175998981,13.6374828806093,
128.796312918205)) ;
#147532 = CARTESIAN_POINT('Ctrl Pts',(-23.9233630582439,13.9340522489258,
128.892767015105)) ;
#147533 = CARTESIAN_POINT('Ctrl Pts',(-23.9692246158357,14.1931239362593,
129.059859846587)) ;
#147534 = CARTESIAN_POINT('Ctrl Pts',(-24.0355476616512,14.3974304653898,
129.286818250949)) ;
#147535 = CARTESIAN_POINT('Ctrl Pts',(-24.1161188310183,14.5309245418109,
129.55517001156)) ;
#147536 = CARTESIAN_POINT('Ctrl Pts',(-24.2052743323323,14.5859814534191,
129.848744590398)) ;
#147537 = CARTESIAN_POINT('Ctrl Pts',(-24.2956465504689,14.5574777864012,
130.145891527965)) ;
#147538 = CARTESIAN_POINT('Ctrl Pts',(-24.3798737732299,14.448015060185,130.425034900643)) ;
#147539 = CARTESIAN_POINT('Ctrl Pts',(-24.4515521270911,14.2640746959558,
130.667673308155)) ;
#147540 = CARTESIAN_POINT('Ctrl Pts',(-24.504086412636,14.0222278715719,130.854058913168)) ;
#147541 = CARTESIAN_POINT('Ctrl Pts',(-24.5339722227007,13.733909228241,130.974734762504)) ;
#147542 = CARTESIAN_POINT('Ctrl Pts',(-24.5374751707681,13.4264443346404,
131.017960330213)) ;
#147543 = CARTESIAN_POINT('Ctrl Pts',(-24.5141880982397,13.1179337320863,
130.98302610922)) ;
#147544 = CARTESIAN_POINT('Ctrl Pts',(-24.4647870843601,12.8308236550973,
130.87184558373)) ;
#147545 = CARTESIAN_POINT('Ctrl Pts',(-24.3919588197093,12.5859821218942,
130.692280995326)) ;
#147546 = CARTESIAN_POINT('Ctrl Pts',(-24.3009187620074,12.4020104650746,
130.459321123967)) ;
#147547 = CARTESIAN_POINT('Ctrl Pts',(-24.1959717032129,12.289987565929,130.186054381331)) ;
#147548 = CARTESIAN_POINT('Ctrl Pts',(-24.0857390473135,12.2601247779834,
129.897056302984)) ;
#147549 = CARTESIAN_POINT('Ctrl Pts',(-23.9762171103296,12.3130229005744,
129.610225108169)) ;
#147550 = CARTESIAN_POINT('Ctrl Pts',(-23.8747284259677,12.4457555473525,
129.34689389739)) ;
#147551 = CARTESIAN_POINT('Ctrl Pts',(-23.7880521676098,12.6478748794645,
129.12675488543)) ;
#147552 = CARTESIAN_POINT('Ctrl Pts',(-23.721103989264,12.9074235012635,128.964483450518)) ;
#147553 = CARTESIAN_POINT('Ctrl Pts',(-23.6788842464701,13.2015879263547,
128.874152848765)) ;
#147554 = CARTESIAN_POINT('Ctrl Pts',(-23.6629323939292,13.5132462059268,
128.860752059264)) ;
#147555 = CARTESIAN_POINT('Ctrl Pts',(-23.6739570788282,13.8170404321959,
128.925997813721)) ;
#147556 = CARTESIAN_POINT('Ctrl Pts',(-23.7102694152644,14.0930904001558,
129.065158549252)) ;
#147557 = CARTESIAN_POINT('Ctrl Pts',(-23.7686960140215,14.3215764972773,
129.268960849726)) ;
#147558 = CARTESIAN_POINT('Ctrl Pts',(-23.8445454380153,14.4860164278212,
129.523758037768)) ;
#147559 = CARTESIAN_POINT('Ctrl Pts',(-23.9312213636041,14.573742198897,129.810089766075)) ;
#147560 = CARTESIAN_POINT('Ctrl Pts',(-24.0220093823538,14.5789283396522,
130.108457949363)) ;
#147561 = CARTESIAN_POINT('Ctrl Pts',(-24.109313917463,14.5018180377366,130.396514557441)) ;
#147562 = CARTESIAN_POINT('Ctrl Pts',(-24.1869754969046,14.346557147794,130.656623143926)) ;
#147563 = CARTESIAN_POINT('Ctrl Pts',(-24.2476549364385,14.1268974997841,
130.866828184463)) ;
#147564 = CARTESIAN_POINT('Ctrl Pts',(-24.2873207213174,13.8551172342444,
131.015918349445)) ;
#147565 = CARTESIAN_POINT('Ctrl Pts',(-24.3017140358187,13.5530513946411,
131.091077286669)) ;
#147566 = CARTESIAN_POINT('Ctrl Pts',(-24.2893139396289,13.2415864711832,
131.087983566359)) ;
#147567 = CARTESIAN_POINT('Ctrl Pts',(-24.250237975428,12.9431697313624,131.006954863297)) ;
#147568 = CARTESIAN_POINT('Ctrl Pts',(-24.1865152004602,12.6789856337564,
130.853947378745)) ;
#147569 = CARTESIAN_POINT('Ctrl Pts',(-24.1021542313126,12.4685393883903,
130.640594380605)) ;
#147570 = CARTESIAN_POINT('Ctrl Pts',(-24.0024751379339,12.3261974816525,
130.382472154133)) ;
#147571 = CARTESIAN_POINT('Ctrl Pts',(-23.8931586555059,12.2622045903834,
130.09638187146)) ;
#147572 = CARTESIAN_POINT('Ctrl Pts',(-23.7827401832175,12.2815898228841,
129.806818174174)) ;
#147573 = CARTESIAN_POINT('Ctrl Pts',(-23.6770976764349,12.3824517560788,
129.53134468171)) ;
#147574 = CARTESIAN_POINT('Ctrl Pts',(-23.5834505310389,12.5585396734663,
129.290971302459)) ;
#147575 = CARTESIAN_POINT('Ctrl Pts',(-23.508182467316,12.7954954768117,129.104139062345)) ;
#147576 = CARTESIAN_POINT('Ctrl Pts',(-23.455285908669,13.0796939956766,128.982930941838)) ;
#147577 = CARTESIAN_POINT('Ctrl Pts',(-23.4286311064434,13.3852304275537,
128.938001175148)) ;
#147578 = CARTESIAN_POINT('Ctrl Pts',(-23.4287217575004,13.6960444491442,
128.971493246291)) ;
#147579 = CARTESIAN_POINT('Ctrl Pts',(-23.4551013960019,13.9858667293059,
129.081617279581)) ;
#147580 = CARTESIAN_POINT('Ctrl Pts',(-23.5051029609528,14.2358877355362,
129.26080876385)) ;
#147581 = CARTESIAN_POINT('Ctrl Pts',(-23.5742887287595,14.4275999351318,
129.495985612575)) ;
#147582 = CARTESIAN_POINT('Ctrl Pts',(-23.6577980269704,14.5480862866817,
129.773271676715)) ;
#147583 = CARTESIAN_POINT('Ctrl Pts',(-23.7474018757379,14.5868446716621,
130.068022721532)) ;
#147584 = CARTESIAN_POINT('Ctrl Pts',(-23.8369559093925,14.5430357669594,
130.362695615245)) ;
#147585 = CARTESIAN_POINT('Ctrl Pts',(-23.9193924881052,14.4187440206734,
130.6366634839)) ;
#147586 = CARTESIAN_POINT('Ctrl Pts',(-23.9878235278518,14.2230681613756,
130.869712210717)) ;
#147587 = CARTESIAN_POINT('Ctrl Pts',(-24.0366005220974,13.9697197628044,
131.045375325504)) ;
#147588 = CARTESIAN_POINT('Ctrl Pts',(-24.0614674762417,13.6787523584359,
131.15101843608)) ;
#147589 = CARTESIAN_POINT('Ctrl Pts',(-24.0600609361775,13.3668523124778,
131.180201589393)) ;
#147590 = CARTESIAN_POINT('Ctrl Pts',(-24.0315449778296,13.0606725090592,
131.130008882499)) ;
#147591 = CARTESIAN_POINT('Ctrl Pts',(-23.9776458019882,12.7810811423454,
131.005579190731)) ;
#147592 = CARTESIAN_POINT('Ctrl Pts',(-23.9011130557165,12.5467077639777,
130.815119966979)) ;
#147593 = CARTESIAN_POINT('Ctrl Pts',(-23.8069768149252,12.3750360607571,
130.573192638211)) ;
#147594 = CARTESIAN_POINT('Ctrl Pts',(-23.7001683995269,12.2779852511976,
130.29453089196)) ;
#147595 = CARTESIAN_POINT('Ctrl Pts',(-23.5898763343155,12.2637459485192,
130.005268133567)) ;
#147596 = CARTESIAN_POINT('Ctrl Pts',(-23.4811263606614,12.3321871592446,
129.720763770541)) ;
#147597 = CARTESIAN_POINT('Ctrl Pts',(-23.3820175069721,12.4786899759448,
129.46433889727)) ;
#147598 = CARTESIAN_POINT('Ctrl Pts',(-23.2983098747109,12.6941598777831,
129.253090432204)) ;
#147599 = CARTESIAN_POINT('Ctrl Pts',(-23.2363410217116,12.9594897352697,
129.105015491517)) ;
#147600 = CARTESIAN_POINT('Ctrl Pts',(-23.1986697974538,13.2597801817525,
129.028156015944)) ;
#147601 = CARTESIAN_POINT('Ctrl Pts',(-23.1878842508862,13.5705932837916,
129.029699535421)) ;
#147602 = CARTESIAN_POINT('Ctrl Pts',(-23.2037430688038,13.8717554022753,
129.109168701418)) ;
#147603 = CARTESIAN_POINT('Ctrl Pts',(-23.2449054031129,14.1416796116284,
129.262708213378)) ;
#147604 = CARTESIAN_POINT('Ctrl Pts',(-23.3066159094202,14.3575208228019,
129.475876783172)) ;
#147605 = CARTESIAN_POINT('Ctrl Pts',(-23.3852205028398,14.5088742490897,
129.738811477045)) ;
#147606 = CARTESIAN_POINT('Ctrl Pts',(-23.4731754167806,14.5810485839828,
130.028857377012)) ;
#147607 = CARTESIAN_POINT('Ctrl Pts',(-23.5635550033295,14.57070182657,130.325899723339)) ;
#147608 = CARTESIAN_POINT('Ctrl Pts',(-23.6496619348552,14.4785662715794,
130.610523033247)) ;
#147609 = CARTESIAN_POINT('Ctrl Pts',(-23.7248247529453,14.3096046389662,
130.863384071564)) ;
#147610 = CARTESIAN_POINT('Ctrl Pts',(-23.7820115470691,14.0777450263891,
131.063555946023)) ;
#147611 = CARTESIAN_POINT('Ctrl Pts',(-23.8168619482178,13.8001342055984,
131.198371274251)) ;
#147612 = CARTESIAN_POINT('Ctrl Pts',(-23.8263563634216,13.4946153250832,
131.25922816625)) ;
#147613 = CARTESIAN_POINT('Ctrl Pts',(-23.8088367280898,13.1837407036183,
131.241195456402)) ;
#147614 = CARTESIAN_POINT('Ctrl Pts',(-23.7649433507423,12.8901082598339,
131.146097057007)) ;
#147615 = CARTESIAN_POINT('Ctrl Pts',(-23.6966251290329,12.6339160902113,
130.979788263205)) ;
#147616 = CARTESIAN_POINT('Ctrl Pts',(-23.6095241543669,12.4365925755612,
130.758201152529)) ;
#147617 = CARTESIAN_POINT('Ctrl Pts',(-23.5069538528283,12.3075969620248,
130.4918578891)) ;
#147618 = CARTESIAN_POINT('Ctrl Pts',(-23.3974350400682,12.2595413696365,
130.204950867827)) ;
#147619 = CARTESIAN_POINT('Ctrl Pts',(-23.2868288278412,12.294598124244,129.915031930311)) ;
#147620 = CARTESIAN_POINT('Ctrl Pts',(-23.1832923441451,12.4101972582257,
129.645612469305)) ;
#147621 = CARTESIAN_POINT('Ctrl Pts',(-23.0926759195256,12.5987159467278,
129.414061565499)) ;
#147622 = CARTESIAN_POINT('Ctrl Pts',(-23.0212220550139,12.8461743732165,
129.238450204882)) ;
#147623 = CARTESIAN_POINT('Ctrl Pts',(-22.9731430841991,13.1359262373299,
129.131228901704)) ;
#147624 = CARTESIAN_POINT('Ctrl Pts',(-22.9514283043162,13.4447581486374,
129.100849561658)) ;
#147625 = CARTESIAN_POINT('Ctrl Pts',(-22.9566735082346,13.7530929107791,
129.149350380603)) ;
#147626 = CARTESIAN_POINT('Ctrl Pts',(-22.9876517295182,14.0362080368137,
129.27283351649)) ;
#147627 = CARTESIAN_POINT('Ctrl Pts',(-23.0416755840538,14.2769559920641,
129.463810736857)) ;
#147628 = CARTESIAN_POINT('Ctrl Pts',(-23.1141892209063,14.4563581826417,
129.708818632771)) ;
#147629 = CARTESIAN_POINT('Ctrl Pts',(-23.1988829773585,14.5613193473425,
129.989308389901)) ;
#147630 = CARTESIAN_POINT('Ctrl Pts',(-23.2893749967103,14.5851466761501,
130.286798104915)) ;
#147631 = CARTESIAN_POINT('Ctrl Pts',(-23.3785630002914,14.5250094388502,
130.580592252952)) ;
#147632 = CARTESIAN_POINT('Ctrl Pts',(-23.4583548680528,14.3871119239881,
130.846635045836)) ;
#147633 = CARTESIAN_POINT('Ctrl Pts',(-23.5236585342063,14.1786613718342,
131.070664502412)) ;
#147634 = CARTESIAN_POINT('Ctrl Pts',(-23.5679982643713,13.9181922141156,
131.233148618779)) ;
#147635 = CARTESIAN_POINT('Ctrl Pts',(-23.5882190837167,13.6189923508217,
131.325572962413)) ;
#147636 = CARTESIAN_POINT('Ctrl Pts',(-23.5816035000313,13.3089361907061,
131.339232711532)) ;
#147637 = CARTESIAN_POINT('Ctrl Pts',(-23.5482741486513,13.0058325903369,
131.274990715579)) ;
#147638 = CARTESIAN_POINT('Ctrl Pts',(-23.4894854786624,12.7318652754408,
131.136467121549)) ;
#147639 = CARTESIAN_POINT('Ctrl Pts',(-23.4089831642771,12.5082426893396,
130.93445138261)) ;
#147640 = CARTESIAN_POINT('Ctrl Pts',(-23.3125034670551,12.3508732586718,
130.685540079445)) ;
#147641 = CARTESIAN_POINT('Ctrl Pts',(-23.2047609813718,12.269103649341,130.403995285876)) ;
#147642 = CARTESIAN_POINT('Ctrl Pts',(-23.0939408644455,12.2702137268432,
130.113315971798)) ;
#147643 = CARTESIAN_POINT('Ctrl Pts',(-22.98625125803,12.3542929865281,129.831968807891)) ;
#147644 = CARTESIAN_POINT('Ctrl Pts',(-22.8899768708341,12.5141176451976,
129.583726131609)) ;
#147645 = CARTESIAN_POINT('Ctrl Pts',(-22.8100908927799,12.739523408871,129.383506653874)) ;
#147646 = CARTESIAN_POINT('Ctrl Pts',(-22.7521073762579,13.0142279275944,
129.247283138693)) ;
#147647 = CARTESIAN_POINT('Ctrl Pts',(-22.7194937058142,13.3177662597612,
129.185120174962)) ;
#147648 = CARTESIAN_POINT('Ctrl Pts',(-22.7137261666825,13.6286637364164,
129.201363001925)) ;
#147649 = CARTESIAN_POINT('Ctrl Pts',(-22.7345204242546,13.925291864832,129.295246555959)) ;
#147650 = CARTESIAN_POINT('Ctrl Pts',(-22.7797671843805,14.1860949701751,
129.460591241563)) ;
#147651 = CARTESIAN_POINT('Ctrl Pts',(-22.8453023863681,14.39173242129,129.685135742378)) ;
#147652 = CARTESIAN_POINT('Ctrl Pts',(-22.9258525518916,14.5282787439252,
129.953574723786)) ;
#147653 = CARTESIAN_POINT('Ctrl Pts',(-23.0150519408169,14.5855538698207,
130.247337850803)) ;
#147654 = CARTESIAN_POINT('Ctrl Pts',(-23.1052288897223,14.5594424200451,
130.54382032972)) ;
#147655 = CARTESIAN_POINT('Ctrl Pts',(-23.1896555995475,14.4525338341733,
130.823512429026)) ;
#147656 = CARTESIAN_POINT('Ctrl Pts',(-23.2619405515289,14.2704301925612,
131.067970264371)) ;
#147657 = CARTESIAN_POINT('Ctrl Pts',(-23.3151218822301,14.029440480781,131.25631660837)) ;
#147658 = CARTESIAN_POINT('Ctrl Pts',(-23.3456010904319,13.743952252976,131.378516130427)) ;
#147659 = CARTESIAN_POINT('Ctrl Pts',(-23.3499839073277,13.4354033018238,
131.424474143209)) ;
#147660 = CARTESIAN_POINT('Ctrl Pts',(-23.3274917765377,13.1268757888795,
131.391823283427)) ;
#147661 = CARTESIAN_POINT('Ctrl Pts',(-23.2786246114809,12.8380942338867,
131.28230278294)) ;
#147662 = CARTESIAN_POINT('Ctrl Pts',(-23.20686160686,12.5930207357232,131.105657440217)) ;
#147663 = CARTESIAN_POINT('Ctrl Pts',(-23.1157309768258,12.406038862873,130.872640568249)) ;
#147664 = CARTESIAN_POINT('Ctrl Pts',(-23.0119458727502,12.2925312371157,
130.602486998872)) ;
#147665 = CARTESIAN_POINT('Ctrl Pts',(-22.9008788581356,12.2597001754449,
130.311334552258)) ;
#147666 = CARTESIAN_POINT('Ctrl Pts',(-22.7914701328309,12.3104428537015,
130.024758576775)) ;
#147667 = CARTESIAN_POINT('Ctrl Pts',(-22.6895482353747,12.4411375499462,
129.760200811099)) ;
#147668 = CARTESIAN_POINT('Ctrl Pts',(-22.6025879552657,12.6410412531594,
129.539155276432)) ;
#147669 = CARTESIAN_POINT('Ctrl Pts',(-22.5349468862704,12.8990709835383,
129.374854664712)) ;
#147670 = CARTESIAN_POINT('Ctrl Pts',(-22.4919137164626,13.1932158971754,
129.282229595877)) ;
#147671 = CARTESIAN_POINT('Ctrl Pts',(-22.4752413419626,13.5039483796779,
129.266639539968)) ;
#147672 = CARTESIAN_POINT('Ctrl Pts',(-22.4854719189725,13.8084630012421,
129.32958919523)) ;
#147673 = CARTESIAN_POINT('Ctrl Pts',(-22.5210896546395,14.0856215177356,
129.4667188073)) ;
#147674 = CARTESIAN_POINT('Ctrl Pts',(-22.5789372654531,14.3156974280267,
129.668828273479)) ;
#147675 = CARTESIAN_POINT('Ctrl Pts',(-22.6542125348602,14.4820692905758,
129.92188857157)) ;
#147676 = CARTESIAN_POINT('Ctrl Pts',(-22.7408312256979,14.5722583385509,
130.208122077193)) ;
#147677 = CARTESIAN_POINT('Ctrl Pts',(-22.8311475633563,14.5801736907429,
130.504940555016)) ;
#147678 = CARTESIAN_POINT('Ctrl Pts',(-22.919292947113,14.5050113905237,130.795699735496)) ;
#147679 = CARTESIAN_POINT('Ctrl Pts',(-22.9970588564607,14.3522165397239,
131.055996300533)) ;
#147680 = CARTESIAN_POINT('Ctrl Pts',(-23.0584040842159,14.1339603470577,
131.26820660931)) ;
#147681 = CARTESIAN_POINT('Ctrl Pts',(-23.0986746028439,13.8641113715177,
131.418974424778)) ;
#147682 = CARTESIAN_POINT('Ctrl Pts',(-23.1139043155525,13.5616226074544,
131.496694305952)) ;
#147683 = CARTESIAN_POINT('Ctrl Pts',(-23.1022497033995,13.2502935266874,
131.495755213587)) ;
#147684 = CARTESIAN_POINT('Ctrl Pts',(-23.0638486364948,12.9509783477542,
131.416729306186)) ;
#147685 = CARTESIAN_POINT('Ctrl Pts',(-23.0010006040838,12.686394956267,131.266167370427)) ;
#147686 = CARTESIAN_POINT('Ctrl Pts',(-22.9170074500105,12.4734606665479,
131.053972327335)) ;
#147687 = CARTESIAN_POINT('Ctrl Pts',(-22.8172294670306,12.3287824012662,
130.79569293947)) ;
#147688 = CARTESIAN_POINT('Ctrl Pts',(-22.7086036821982,12.2629634134795,
130.511454266347)) ;
#147689 = CARTESIAN_POINT('Ctrl Pts',(-22.5979567530543,12.2798963226628,
130.221280314733)) ;
#147690 = CARTESIAN_POINT('Ctrl Pts',(-22.4920126410245,12.3786943874465,
129.944944100135)) ;
#147691 = CARTESIAN_POINT('Ctrl Pts',(-22.3978375846003,12.5532637132079,
129.703077795437)) ;
#147692 = CARTESIAN_POINT('Ctrl Pts',(-22.3223450400085,12.7879391796142,
129.515464838595)) ;
#147693 = CARTESIAN_POINT('Ctrl Pts',(-22.2688664186441,13.0695371271683,
129.392394388671)) ;
#147694 = CARTESIAN_POINT('Ctrl Pts',(-22.2411956279741,13.3764287043337,
129.344691810552)) ;
#147695 = CARTESIAN_POINT('Ctrl Pts',(-22.2405807700061,13.6873693766845,
129.376111748844)) ;
#147696 = CARTESIAN_POINT('Ctrl Pts',(-22.266182058288,13.9780097436375,129.483950839692)) ;
#147697 = CARTESIAN_POINT('Ctrl Pts',(-22.3158295990549,14.2303816884254,
129.662248512627)) ;
#147698 = CARTESIAN_POINT('Ctrl Pts',(-22.3843432444658,14.4229832272402,
129.895337579006)) ;
#147699 = CARTESIAN_POINT('Ctrl Pts',(-22.467333378006,14.5456071982134,130.171033869882)) ;
#147700 = CARTESIAN_POINT('Ctrl Pts',(-22.5569971155474,14.5869244372791,
130.466019745775)) ;
#147701 = CARTESIAN_POINT('Ctrl Pts',(-22.6467207673819,14.5454139986495,
130.761210108266)) ;
#147702 = CARTESIAN_POINT('Ctrl Pts',(-22.7294791899913,14.423161531977,131.036131544807)) ;
#147703 = CARTESIAN_POINT('Ctrl Pts',(-22.7981835761643,14.2299646036066,
131.269878058976)) ;
#147704 = CARTESIAN_POINT('Ctrl Pts',(-22.8476846979566,13.9782380445369,
131.447654268064)) ;
#147705 = CARTESIAN_POINT('Ctrl Pts',(-22.8733293938664,13.6869896878631,
131.555692859271)) ;
#147706 = CARTESIAN_POINT('Ctrl Pts',(-22.8727231487113,13.3772462538757,
131.587007151188)) ;
#147707 = CARTESIAN_POINT('Ctrl Pts',(-22.8451132311897,13.0701026679002,
131.539509729341)) ;
#147708 = CARTESIAN_POINT('Ctrl Pts',(-22.7917084880126,12.7883758090077,
131.416651622432)) ;
#147709 = CARTESIAN_POINT('Ctrl Pts',(-22.715757237827,12.5524788411572,131.227885604995)) ;
#147710 = CARTESIAN_POINT('Ctrl Pts',(-22.6218519763286,12.3787206196838,
130.986691296974)) ;
#147711 = CARTESIAN_POINT('Ctrl Pts',(-22.5159330453895,12.2799428497071,
130.710427408907)) ;
#147712 = CARTESIAN_POINT('Ctrl Pts',(-22.4054383279324,12.262781441409,130.420647289657)) ;
#147713 = CARTESIAN_POINT('Ctrl Pts',(-22.2959303546471,12.3295044155471,
130.134111080986)) ;
#147714 = CARTESIAN_POINT('Ctrl Pts',(-22.1969925695421,12.4735104244077,
129.878028751513)) ;
#147715 = CARTESIAN_POINT('Ctrl Pts',(-22.1130241441533,12.6859035463297,
129.665868893032)) ;
#147716 = CARTESIAN_POINT('Ctrl Pts',(-22.0500057240316,12.9511127833356,
129.514887939214)) ;
#147717 = CARTESIAN_POINT('Ctrl Pts',(-22.0115779224571,13.2510041848706,
129.435841941698)) ;
#147718 = CARTESIAN_POINT('Ctrl Pts',(-22.0000267466205,13.5624347972365,
129.435216595887)) ;
#147719 = CARTESIAN_POINT('Ctrl Pts',(-22.0151986171199,13.8634350892771,
129.512606829949)) ;
#147720 = CARTESIAN_POINT('Ctrl Pts',(-22.0553267596581,14.1332613456827,
129.662934327461)) ;
#147721 = CARTESIAN_POINT('Ctrl Pts',(-22.1169164718532,14.352640956948,129.876004680242)) ;
#147722 = CARTESIAN_POINT('Ctrl Pts',(-22.1950027878672,14.5054039533886,
130.137339400697)) ;
#147723 = CARTESIAN_POINT('Ctrl Pts',(-22.2823946613197,14.5799567622948,
130.425612798528)) ;
#147724 = CARTESIAN_POINT('Ctrl Pts',(-22.3731495143974,14.5723714233898,
130.723873707253)) ;
#147725 = CARTESIAN_POINT('Ctrl Pts',(-22.4597690917796,14.4818104569399,
131.010120730261)) ;
#147726 = CARTESIAN_POINT('Ctrl Pts',(-22.5347344779201,14.3163443098713,
131.262126357748)) ;
#147727 = CARTESIAN_POINT('Ctrl Pts',(-22.5927669336754,14.085912079338,131.464853193877)) ;
#147728 = CARTESIAN_POINT('Ctrl Pts',(-22.6284258357542,13.8088758328653,
131.602091135406)) ;
#147729 = CARTESIAN_POINT('Ctrl Pts',(-22.6386507602744,13.502841633218,131.66518977333)) ;
#147730 = CARTESIAN_POINT('Ctrl Pts',(-22.6219823717775,13.1931031291703,
131.649500274369)) ;
#147731 = CARTESIAN_POINT('Ctrl Pts',(-22.5787183669213,12.8979592502217,
131.556328075628)) ;
#147732 = CARTESIAN_POINT('Ctrl Pts',(-22.5114550363443,12.6415806855276,
131.392924286405)) ;
#147733 = CARTESIAN_POINT('Ctrl Pts',(-22.4242650098309,12.4408172190554,
131.171318802838)) ;
#147734 = CARTESIAN_POINT('Ctrl Pts',(-22.3219857137763,12.3100401605785,
130.90581289392)) ;
#147735 = CARTESIAN_POINT('Ctrl Pts',(-22.2128212850724,12.2598615755304,
130.61987465851)) ;
#147736 = CARTESIAN_POINT('Ctrl Pts',(-22.1023684792295,12.2922205439251,
130.330327430686)) ;
#147737 = CARTESIAN_POINT('Ctrl Pts',(-21.9979975356662,12.4062484936796,
130.058648293658)) ;
#147738 = CARTESIAN_POINT('Ctrl Pts',(-21.9071729863386,12.5927140648452,
129.826414994569)) ;
#147739 = CARTESIAN_POINT('Ctrl Pts',(-21.8352773240707,12.8381488980971,
129.649442639516)) ;
#147740 = CARTESIAN_POINT('Ctrl Pts',(-21.7864878410526,13.1260095389923,
129.540046596977)) ;
#147741 = CARTESIAN_POINT('Ctrl Pts',(-21.763852701103,13.4367097243977,129.507212398852)) ;
#147742 = CARTESIAN_POINT('Ctrl Pts',(-21.7683543624926,13.7438376738668,
129.553370845295)) ;
#147743 = CARTESIAN_POINT('Ctrl Pts',(-21.7986360668358,14.0287736481255,
129.674910885284)) ;
#147744 = CARTESIAN_POINT('Ctrl Pts',(-21.8521200037136,14.2709621687312,
129.864315089826)) ;
#147745 = CARTESIAN_POINT('Ctrl Pts',(-21.9240424719339,14.4520607897228,
130.10753831961)) ;
#147746 = CARTESIAN_POINT('Ctrl Pts',(-22.0086052791843,14.5594794390157,
130.387698164307)) ;
#147747 = CARTESIAN_POINT('Ctrl Pts',(-22.0988545163125,14.5855261762896,
130.684415053406)) ;
#147748 = CARTESIAN_POINT('Ctrl Pts',(-22.1879797716456,14.5283738832722,
130.977932444029)) ;
#147749 = CARTESIAN_POINT('Ctrl Pts',(-22.268629541142,14.391653643749,131.246704641427)) ;
#147750 = CARTESIAN_POINT('Ctrl Pts',(-22.3340590487769,14.1863633435458,
131.470884649421)) ;
#147751 = CARTESIAN_POINT('Ctrl Pts',(-22.3793406508304,13.9255968705726,
131.636336360849)) ;
#147752 = CARTESIAN_POINT('Ctrl Pts',(-22.4001605026576,13.6292801101744,
131.730263653037)) ;
#147753 = CARTESIAN_POINT('Ctrl Pts',(-22.3944314276688,13.3179690043923,
131.746663855123)) ;
#147754 = CARTESIAN_POINT('Ctrl Pts',(-22.3618138354626,13.0144329118731,
131.684488661927)) ;
#147755 = CARTESIAN_POINT('Ctrl Pts',(-22.3039665732409,12.7401667840787,
131.548606149446)) ;
#147756 = CARTESIAN_POINT('Ctrl Pts',(-22.2241247883536,12.5144107338462,
131.34852837519)) ;
#147757 = CARTESIAN_POINT('Ctrl Pts',(-22.1274235747229,12.3540784671315,
131.09917757095)) ;
#147758 = CARTESIAN_POINT('Ctrl Pts',(-22.0203905808136,12.2704506823876,
130.819545083415)) ;
#147759 = CARTESIAN_POINT('Ctrl Pts',(-21.9092164103805,12.2689820893059,
130.527940599895)) ;
#147760 = CARTESIAN_POINT('Ctrl Pts',(-21.8014011825293,12.3508509488233,
130.246203129404)) ;
#147761 = CARTESIAN_POINT('Ctrl Pts',(-21.7046974530704,12.5086055311564,
129.996715163344)) ;
#147762 = CARTESIAN_POINT('Ctrl Pts',(-21.6240710185452,12.7330676993537,
129.7944205009)) ;
#147763 = CARTESIAN_POINT('Ctrl Pts',(-21.5655611211422,13.0066123960221,
129.656635909801)) ;
#147764 = CARTESIAN_POINT('Ctrl Pts',(-21.5323215652133,13.3082725062707,
129.592500856618)) ;
#147765 = CARTESIAN_POINT('Ctrl Pts',(-21.5256970786124,13.6201712444572,
129.606335855298)) ;
#147766 = CARTESIAN_POINT('Ctrl Pts',(-21.5459113781207,13.9183340301052,
129.698623260894)) ;
#147767 = CARTESIAN_POINT('Ctrl Pts',(-21.5905200274983,14.1797387715242,
129.862041430257)) ;
#147768 = CARTESIAN_POINT('Ctrl Pts',(-21.6553241180103,14.3864986993276,
130.084342628369)) ;
#147769 = CARTESIAN_POINT('Ctrl Pts',(-21.7354793084019,14.5252641571149,
130.351617653865)) ;
#147770 = CARTESIAN_POINT('Ctrl Pts',(-21.8245513470897,14.5851721018435,
130.645016977157)) ;
#147771 = CARTESIAN_POINT('Ctrl Pts',(-21.9153010096144,14.5610669254243,
130.943362526667)) ;
#147772 = CARTESIAN_POINT('Ctrl Pts',(-21.9994922925595,14.4566509961662,
131.222188061234)) ;
#147773 = CARTESIAN_POINT('Ctrl Pts',(-22.0722010613077,14.2771545373181,
131.467832940722)) ;
#147774 = CARTESIAN_POINT('Ctrl Pts',(-22.1262384175291,14.0362065449594,
131.658867438289)) ;
#147775 = CARTESIAN_POINT('Ctrl Pts',(-22.1572139611432,13.7533987258428,
131.782313040366)) ;
#147776 = CARTESIAN_POINT('Ctrl Pts',(-22.1625009400224,13.4441283625548,
131.831033676045)) ;
#147777 = CARTESIAN_POINT('Ctrl Pts',(-22.140564230066,13.1346408964387,131.800086171256)) ;
#147778 = CARTESIAN_POINT('Ctrl Pts',(-22.0928516991892,12.8470251714903,
131.693686261064)) ;
#147779 = CARTESIAN_POINT('Ctrl Pts',(-22.0211494847611,12.5984937845751,
131.517487007206)) ;
#147780 = CARTESIAN_POINT('Ctrl Pts',(-21.9309737753859,12.4108688271007,
131.287059945981)) ;
#147781 = CARTESIAN_POINT('Ctrl Pts',(-21.8272669687951,12.2946081104034,
131.01721764876)) ;
#147782 = CARTESIAN_POINT('Ctrl Pts',(-21.7161953353961,12.2594450538074,
130.726072036675)) ;
#147783 = CARTESIAN_POINT('Ctrl Pts',(-21.60658212141,12.308048143484,130.438929539437)) ;
#147784 = CARTESIAN_POINT('Ctrl Pts',(-21.5046765692389,12.4360760888544,
130.174304543921)) ;
#147785 = CARTESIAN_POINT('Ctrl Pts',(-21.4170241462741,12.6345258024436,
129.951310361765)) ;
#147786 = CARTESIAN_POINT('Ctrl Pts',(-21.3489685892398,12.8902136692482,
129.785676166942)) ;
#147787 = CARTESIAN_POINT('Ctrl Pts',(-21.3050715222795,13.1836914998379,
129.690556675395)) ;
#147788 = CARTESIAN_POINT('Ctrl Pts',(-21.2875431524177,13.4943233710872,
129.672471793995)) ;
#147789 = CARTESIAN_POINT('Ctrl Pts',(-21.2970438548803,13.8008444309758,
129.733451477825)) ;
#147790 = CARTESIAN_POINT('Ctrl Pts',(-21.3321854329995,14.0793169977329,
129.869248256768)) ;
#147791 = CARTESIAN_POINT('Ctrl Pts',(-21.3892022783264,14.3098744793808,
130.06877225239)) ;
#147792 = CARTESIAN_POINT('Ctrl Pts',(-21.4644021583777,14.4788324369104,
130.321755899341)) ;
#147793 = CARTESIAN_POINT('Ctrl Pts',(-21.5503775766376,14.5706779961945,
130.605939092449)) ;
#147794 = CARTESIAN_POINT('Ctrl Pts',(-21.6408546610516,14.5811216657767,
130.903299048732)) ;
#147795 = CARTESIAN_POINT('Ctrl Pts',(-21.7290160591459,14.508299186415,131.194043800993)) ;
#147796 = CARTESIAN_POINT('Ctrl Pts',(-21.8071127913757,14.3580058494818,
131.455269800372)) ;
#147797 = CARTESIAN_POINT('Ctrl Pts',(-21.8692690049898,14.1405257747425,
131.669989141378)) ;
#147798 = CARTESIAN_POINT('Ctrl Pts',(-21.9100611483019,13.8719962112454,
131.822245697122)) ;
#147799 = CARTESIAN_POINT('Ctrl Pts',(-21.9260462949812,13.571629068225,131.902012596254)) ;
#147800 = CARTESIAN_POINT('Ctrl Pts',(-21.9151786975918,13.2591263892434,
131.903497844346)) ;
#147801 = CARTESIAN_POINT('Ctrl Pts',(-21.8776490214524,12.9599152020145,
131.826926251731)) ;
#147802 = CARTESIAN_POINT('Ctrl Pts',(-21.8152817422074,12.693080122514,131.677887077937)) ;
#147803 = CARTESIAN_POINT('Ctrl Pts',(-21.7318932707648,12.478823817929,131.467412166417)) ;
#147804 = CARTESIAN_POINT('Ctrl Pts',(-21.6327999015098,12.3322479297148,
131.211038953478)) ;
#147805 = CARTESIAN_POINT('Ctrl Pts',(-21.5242177252989,12.2636849635138,
130.926971995263)) ;
#147806 = CARTESIAN_POINT('Ctrl Pts',(-21.4132305357613,12.2782423656434,
130.635891058601)) ;
#147807 = CARTESIAN_POINT('Ctrl Pts',(-21.3071564989926,12.3748788450642,
130.359150081673)) ;
#147808 = CARTESIAN_POINT('Ctrl Pts',(-21.2128894825434,12.5463734718221,
130.116868376143)) ;
#147809 = CARTESIAN_POINT('Ctrl Pts',(-21.1362513663819,12.7810696504838,
129.926144136588)) ;
#147810 = CARTESIAN_POINT('Ctrl Pts',(-21.0823186107827,13.0608633247241,
129.80163888343)) ;
#147811 = CARTESIAN_POINT('Ctrl Pts',(-21.053841117646,13.3671882747387,129.751572869485)) ;
#147812 = CARTESIAN_POINT('Ctrl Pts',(-21.052413710193,13.6783220863787,129.78061109945)) ;
#147813 = CARTESIAN_POINT('Ctrl Pts',(-21.0773404053595,13.970110064652,129.886522311045)) ;
#147814 = CARTESIAN_POINT('Ctrl Pts',(-21.1260864074651,14.223034525395,130.062047312734)) ;
#147815 = CARTESIAN_POINT('Ctrl Pts',(-21.1944669924731,14.4186168883369,
130.294931085397)) ;
#147816 = CARTESIAN_POINT('Ctrl Pts',(-21.2767695355892,14.5428705869547,
130.568459883078)) ;
#147817 = CARTESIAN_POINT('Ctrl Pts',(-21.3665020515511,14.5869069848455,
130.863723007188)) ;
#147818 = CARTESIAN_POINT('Ctrl Pts',(-21.4562511004557,14.5480013176435,
131.158949677718)) ;
#147819 = CARTESIAN_POINT('Ctrl Pts',(-21.5397825926928,14.4271740770577,
131.436324849005)) ;
#147820 = CARTESIAN_POINT('Ctrl Pts',(-21.6086583923119,14.2362638791343,
131.670454356284)) ;
#147821 = CARTESIAN_POINT('Ctrl Pts',(-21.6587784835505,13.9863048386446,
131.85000812487)) ;
#147822 = CARTESIAN_POINT('Ctrl Pts',(-21.6851472284161,13.6957298215624,
131.960182987964)) ;
#147823 = CARTESIAN_POINT('Ctrl Pts',(-21.6853929289674,13.3866515753752,
131.993937295129)) ;
#147824 = CARTESIAN_POINT('Ctrl Pts',(-21.6582776406114,13.0771469727204,
131.948105746081)) ;
#147825 = CARTESIAN_POINT('Ctrl Pts',(-21.605884471671,12.796392103063,131.827972089653)) ;
#147826 = CARTESIAN_POINT('Ctrl Pts',(-21.5302178923545,12.5578779370545,
131.640184361149)) ;
#147827 = CARTESIAN_POINT('Ctrl Pts',(-21.4371072181925,12.383073568111,131.401168478668)) ;
#147828 = CARTESIAN_POINT('Ctrl Pts',(-21.3314361683633,12.2815115204251,
131.125642156933)) ;
#147829 = CARTESIAN_POINT('Ctrl Pts',(-21.220189476718,12.2623682395224,130.833904271501)) ;
#147830 = CARTESIAN_POINT('Ctrl Pts',(-21.111889747899,12.3259184217804,130.550477416465)) ;
#147831 = CARTESIAN_POINT('Ctrl Pts',(-21.0118711465864,12.4680809238775,
130.291448394108)) ;
#147832 = CARTESIAN_POINT('Ctrl Pts',(-20.9272254879945,12.6795623120404,
130.077395414109)) ;
#147833 = CARTESIAN_POINT('Ctrl Pts',(-20.8637839574138,12.9425894685416,
129.925062925594)) ;
#147834 = CARTESIAN_POINT('Ctrl Pts',(-20.8245561726934,13.2417282929866,
129.843679604379)) ;
#147835 = CARTESIAN_POINT('Ctrl Pts',(-20.8121787579524,13.5531902629317,
129.840645625293)) ;
#147836 = CARTESIAN_POINT('Ctrl Pts',(-20.826647165812,13.8554128204607,129.916054647535)) ;
#147837 = CARTESIAN_POINT('Ctrl Pts',(-20.8660416715249,14.1261608663375,
130.06419630691)) ;
#147838 = CARTESIAN_POINT('Ctrl Pts',(-20.9273901269622,14.3478084668955,
130.276692976576)) ;
#147839 = CARTESIAN_POINT('Ctrl Pts',(-21.0043490799319,14.5013886643306,
130.534422370052)) ;
#147840 = CARTESIAN_POINT('Ctrl Pts',(-21.0922596829206,14.5792263009218,
130.82449298872)) ;
#147841 = CARTESIAN_POINT('Ctrl Pts',(-21.1828391154011,14.5735423327803,
131.122170352937)) ;
#147842 = CARTESIAN_POINT('Ctrl Pts',(-21.2694503580301,14.4859392223761,
131.408288783411)) ;
#147843 = CARTESIAN_POINT('Ctrl Pts',(-21.345349839766,14.32102399054,131.663278927697)) ;
#147844 = CARTESIAN_POINT('Ctrl Pts',(-21.4034913421488,14.0938129483377,
131.866070729537)) ;
#147845 = CARTESIAN_POINT('Ctrl Pts',(-21.4400110100887,13.8165579803482,
132.005993362765)) ;
#147846 = CARTESIAN_POINT('Ctrl Pts',(-21.4509809590389,13.5127264652926,
132.071072537445)) ;
#147847 = CARTESIAN_POINT('Ctrl Pts',(-21.4348676182243,13.2000971837,132.057309732157)) ;
#147848 = CARTESIAN_POINT('Ctrl Pts',(-21.3927484801215,12.9073427141145,
131.967122130863)) ;
#147849 = CARTESIAN_POINT('Ctrl Pts',(-21.3258505842354,12.6479572594797,
131.804981308529)) ;
#147850 = CARTESIAN_POINT('Ctrl Pts',(-21.2394142383129,12.4461100388149,
131.585465190968)) ;
#147851 = CARTESIAN_POINT('Ctrl Pts',(-21.1374149775603,12.3127706272653,
131.320810832237)) ;
#147852 = CARTESIAN_POINT('Ctrl Pts',(-21.0282673309725,12.2601401090579,
131.034952467614)) ;
#147853 = CARTESIAN_POINT('Ctrl Pts',(-20.9177126950044,12.2901733213181,
130.745118295567)) ;
#147854 = CARTESIAN_POINT('Ctrl Pts',(-20.8132418808532,12.4015833019759,
130.473080662222)) ;
#147855 = CARTESIAN_POINT('Ctrl Pts',(-20.7216877105118,12.586648376757,130.238816544621)) ;
#147856 = CARTESIAN_POINT('Ctrl Pts',(-20.6492277224844,12.8302723293176,
130.060151545908)) ;
#147857 = CARTESIAN_POINT('Ctrl Pts',(-20.5995649352274,13.1192440292328,
129.948424989432)) ;
#147858 = CARTESIAN_POINT('Ctrl Pts',(-20.5764497565438,13.4254781947616,
129.913736732255)) ;
#147859 = CARTESIAN_POINT('Ctrl Pts',(-20.5800162996611,13.73535968212,129.957422057051)) ;
#147860 = CARTESIAN_POINT('Ctrl Pts',(-20.6096448160032,14.0210481979202,
130.077031775124)) ;
#147861 = CARTESIAN_POINT('Ctrl Pts',(-20.6625737600944,14.2649914654817,
130.264853339721)) ;
#147862 = CARTESIAN_POINT('Ctrl Pts',(-20.7339227482206,14.4476746957159,
130.506339169657)) ;
#147863 = CARTESIAN_POINT('Ctrl Pts',(-20.8181740365747,14.5574099985375,
130.785581972635)) ;
#147864 = CARTESIAN_POINT('Ctrl Pts',(-20.9083832242606,14.5860647518339,
131.082188756989)) ;
#147865 = CARTESIAN_POINT('Ctrl Pts',(-20.9980143564362,14.5307819376324,
131.377329816283)) ;
#147866 = CARTESIAN_POINT('Ctrl Pts',(-21.0785436243018,14.3969445347875,
131.645559337238)) ;
#147867 = CARTESIAN_POINT('Ctrl Pts',(-21.144755916161,14.1927449402103,131.872158750535)) ;
#147868 = CARTESIAN_POINT('Ctrl Pts',(-21.1905238305556,13.9340124552338,
132.038928596485)) ;
#147869 = CARTESIAN_POINT('Ctrl Pts',(-21.2121498400583,13.638112171606,132.135255984941)) ;
#147870 = CARTESIAN_POINT('Ctrl Pts',(-21.2071970261272,13.3270743083993,
132.153904990694)) ;
#147871 = CARTESIAN_POINT('Ctrl Pts',(-21.1753089200448,13.0225106928389,
132.093912711997)) ;
#147872 = CARTESIAN_POINT('Ctrl Pts',(-21.1179639971965,12.7468020423806,
131.959553634409)) ;
#147873 = CARTESIAN_POINT('Ctrl Pts',(-21.0390833671459,12.520588791344,131.76211445131)) ;
#147874 = CARTESIAN_POINT('Ctrl Pts',(-20.9427982312011,12.3578209708367,
131.51399660927)) ;
#147875 = CARTESIAN_POINT('Ctrl Pts',(-20.8356847345824,12.2716454872787,
131.234216653382)) ;
#147876 = CARTESIAN_POINT('Ctrl Pts',(-20.7246335895613,12.26795429664,130.942939134598)) ;
#147877 = CARTESIAN_POINT('Ctrl Pts',(-20.616973302296,12.3469221787347,130.661535656363)) ;
#147878 = CARTESIAN_POINT('Ctrl Pts',(-20.5194780056374,12.5030898153774,
130.409865228873)) ;
#147879 = CARTESIAN_POINT('Ctrl Pts',(-20.4385947118709,12.725018199882,130.20669437947)) ;
#147880 = CARTESIAN_POINT('Ctrl Pts',(-20.3792474158337,12.997182809166,130.066468431869)) ;
#147881 = CARTESIAN_POINT('Ctrl Pts',(-20.3450790019387,13.2997828332168,
129.999782492752)) ;
#147882 = CARTESIAN_POINT('Ctrl Pts',(-20.3377619039051,13.6108910238796,
130.011503902114)) ;
#147883 = CARTESIAN_POINT('Ctrl Pts',(-20.3570249789921,13.9087323450299,
130.100885429075)) ;
#147884 = CARTESIAN_POINT('Ctrl Pts',(-20.4010227954552,14.1725576107312,
130.2626334915)) ;
#147885 = CARTESIAN_POINT('Ctrl Pts',(-20.4654669482324,14.3815587835512,
130.483957592039)) ;
#147886 = CARTESIAN_POINT('Ctrl Pts',(-20.5452725967779,14.522329585323,130.750205362324)) ;
#147887 = CARTESIAN_POINT('Ctrl Pts',(-20.6339261819108,14.5844939655697,
131.042286429086)) ;
#147888 = CARTESIAN_POINT('Ctrl Pts',(-20.7247186453383,14.5631534313931,
131.340749638072)) ;
#147889 = CARTESIAN_POINT('Ctrl Pts',(-20.809527155941,14.4606751117259,131.62150908493)) ;
#147890 = CARTESIAN_POINT('Ctrl Pts',(-20.8826704768018,14.2826954166288,
131.868454149074)) ;
#147891 = CARTESIAN_POINT('Ctrl Pts',(-20.9370591986332,14.0447463561046,
132.060328466672)) ;
#147892 = CARTESIAN_POINT('Ctrl Pts',(-20.9689299497297,13.7613771216005,
132.186577022654)) ;
#147893 = CARTESIAN_POINT('Ctrl Pts',(-20.9749288618211,13.4542323350155,
132.237185457133)) ;
#147894 = CARTESIAN_POINT('Ctrl Pts',(-20.9538950902724,13.1437994657192,
132.208942651979)) ;
#147895 = CARTESIAN_POINT('Ctrl Pts',(-20.9065605624444,12.8538469194028,
132.103822776619)) ;
#147896 = CARTESIAN_POINT('Ctrl Pts',(-20.8358615876408,12.6054873478473,
131.930355849117)) ;
#147897 = CARTESIAN_POINT('Ctrl Pts',(-20.7461738157483,12.4153273189239,
131.701384848955)) ;
#147898 = CARTESIAN_POINT('Ctrl Pts',(-20.6418761403516,12.2964112456076,
131.430080533355)) ;
#147899 = CARTESIAN_POINT('Ctrl Pts',(-20.5321091748032,12.2594155903617,
131.142376798945)) ;
#147900 = CARTESIAN_POINT('Ctrl Pts',(-20.4219406220952,12.3053349430094,
130.853742645064)) ;
#147901 = CARTESIAN_POINT('Ctrl Pts',(-20.3197409294041,12.431225904051,130.58824874815)) ;
#147902 = CARTESIAN_POINT('Ctrl Pts',(-20.2314802430667,12.6279597128561,
130.363514862716)) ;
#147903 = CARTESIAN_POINT('Ctrl Pts',(-20.162777545172,12.8824932881055,130.19601021006)) ;
#147904 = CARTESIAN_POINT('Ctrl Pts',(-20.1182353083601,13.1745455481659,
130.098938299482)) ;
#147905 = CARTESIAN_POINT('Ctrl Pts',(-20.0998706065,13.4851755770177,130.078429714229)) ;
#147906 = CARTESIAN_POINT('Ctrl Pts',(-20.1086336178108,13.7921379427258,
130.137258008057)) ;
#147907 = CARTESIAN_POINT('Ctrl Pts',(-20.14286672269,14.0710147871215,130.270296111646)) ;
#147908 = CARTESIAN_POINT('Ctrl Pts',(-20.1996972773832,14.3045452092941,
130.469492695911)) ;
#147909 = CARTESIAN_POINT('Ctrl Pts',(-20.273759835946,14.4740866003594,130.71884073993)) ;
#147910 = CARTESIAN_POINT('Ctrl Pts',(-20.3600214704323,14.5693022408221,
131.004086313141)) ;
#147911 = CARTESIAN_POINT('Ctrl Pts',(-20.4504553064572,14.5820126324711,
131.301304006894)) ;
#147912 = CARTESIAN_POINT('Ctrl Pts',(-20.5390122957554,14.5112271142504,
131.593295289522)) ;
#147913 = CARTESIAN_POINT('Ctrl Pts',(-20.617145557028,14.3635591504594,131.854489519357)) ;
#147914 = CARTESIAN_POINT('Ctrl Pts',(-20.6798949965578,14.147953964214,132.070948087986)) ;
#147915 = CARTESIAN_POINT('Ctrl Pts',(-20.7214213257657,13.88065471692,132.225356091417)) ;
#147916 = CARTESIAN_POINT('Ctrl Pts',(-20.7382001300279,13.5796273902736,
132.307581392569)) ;
#147917 = CARTESIAN_POINT('Ctrl Pts',(-20.72801762459,13.2675902134212,132.311017500675)) ;
#147918 = CARTESIAN_POINT('Ctrl Pts',(-20.6913625442672,12.9685392965924,
132.236910820847)) ;
#147919 = CARTESIAN_POINT('Ctrl Pts',(-20.6296262601908,12.7001827589766,
132.08974747975)) ;
#147920 = CARTESIAN_POINT('Ctrl Pts',(-20.5468892830631,12.4843513873254,
131.881136546848)) ;
#147921 = CARTESIAN_POINT('Ctrl Pts',(-20.4480106979793,12.3354377885734,
131.625445849201)) ;
#147922 = CARTESIAN_POINT('Ctrl Pts',(-20.3399262007123,12.2645466561417,
131.342734057341)) ;
#147923 = CARTESIAN_POINT('Ctrl Pts',(-20.2283990487693,12.2767400465521,
131.050231091505)) ;
#147924 = CARTESIAN_POINT('Ctrl Pts',(-20.122468047658,12.3708038942679,130.773785646118)) ;
#147925 = CARTESIAN_POINT('Ctrl Pts',(-20.0275757835949,12.540571419273,130.529748962707)) ;
#147926 = CARTESIAN_POINT('Ctrl Pts',(-19.9505760506739,12.7727636471261,
130.337850842071)) ;
#147927 = CARTESIAN_POINT('Ctrl Pts',(-19.895548548468,13.0532482388654,130.210361702874)) ;
#147928 = CARTESIAN_POINT('Ctrl Pts',(-19.8664861035887,13.3594503778047,
130.158608683618)) ;
#147929 = CARTESIAN_POINT('Ctrl Pts',(-19.8642805955961,13.6687250636368,
130.185154959799)) ;
#147930 = CARTESIAN_POINT('Ctrl Pts',(-19.8884803528754,13.9622484171183,
130.289040068247)) ;
#147931 = CARTESIAN_POINT('Ctrl Pts',(-19.9365724196129,14.2163837288721,
130.462630299501)) ;
#147932 = CARTESIAN_POINT('Ctrl Pts',(-20.004641785684,14.4143549429609,130.694692087338)) ;
#147933 = CARTESIAN_POINT('Ctrl Pts',(-20.0866599380791,14.5404303833534,
130.967385240993)) ;
#147934 = CARTESIAN_POINT('Ctrl Pts',(-20.1758963178231,14.5868747915152,
131.261056127709)) ;
#147935 = CARTESIAN_POINT('Ctrl Pts',(-20.2662529036822,14.5499212466532,
131.558258305741)) ;
#147936 = CARTESIAN_POINT('Ctrl Pts',(-20.3493796320755,14.4324626296397,
131.834156427293)) ;
#147937 = CARTESIAN_POINT('Ctrl Pts',(-20.4193859524165,14.2419356946445,
132.071886760109)) ;
#147938 = CARTESIAN_POINT('Ctrl Pts',(-20.4698543024917,13.9939564786199,
132.252344857302)) ;
#147939 = CARTESIAN_POINT('Ctrl Pts',(-20.4969872695557,13.7043181806052,
132.364754467268)) ;
#147940 = CARTESIAN_POINT('Ctrl Pts',(-20.497934277569,13.3953697990708,132.400569582699)) ;
#147941 = CARTESIAN_POINT('Ctrl Pts',(-20.4717871200725,13.0868083993376,
132.35741635374)) ;
#147942 = CARTESIAN_POINT('Ctrl Pts',(-20.4198713515675,12.8035341762303,
132.238849819273)) ;
#147943 = CARTESIAN_POINT('Ctrl Pts',(-20.3448769953812,12.5639567579486,
132.052971164344)) ;
#147944 = CARTESIAN_POINT('Ctrl Pts',(-20.2520317235411,12.3867441444795,
131.814796568743)) ;
#147945 = CARTESIAN_POINT('Ctrl Pts',(-20.1464031923312,12.2832559742793,
131.539448061917)) ;
#147946 = CARTESIAN_POINT('Ctrl Pts',(-20.0361703920393,12.2616345635869,
131.250381746518)) ;
#147947 = CARTESIAN_POINT('Ctrl Pts',(-19.926830089703,12.3231638748032,130.964186355798)) ;
#147948 = CARTESIAN_POINT('Ctrl Pts',(-19.8269315810433,12.4627499804897,
130.705354563112)) ;
#147949 = CARTESIAN_POINT('Ctrl Pts',(-19.7415073817147,12.6729053346686,
130.489121388215)) ;
#147950 = CARTESIAN_POINT('Ctrl Pts',(-19.6774820062394,12.9344260025205,
130.335045332416)) ;
#147951 = CARTESIAN_POINT('Ctrl Pts',(-19.6374230862404,13.2340774716611,
130.25136547355)) ;
#147952 = CARTESIAN_POINT('Ctrl Pts',(-19.6244120372296,13.5439038566318,
130.246310943966)) ;
#147953 = CARTESIAN_POINT('Ctrl Pts',(-19.6380214405693,13.8465581380597,
130.319189287178)) ;
#147954 = CARTESIAN_POINT('Ctrl Pts',(-19.6767732091256,14.1188039564303,
130.465491640985)) ;
#147955 = CARTESIAN_POINT('Ctrl Pts',(-19.7374565997598,14.3420290763671,
130.67600475398)) ;
#147956 = CARTESIAN_POINT('Ctrl Pts',(-19.8142575244507,14.4980360356998,
130.933370357815)) ;
#147957 = CARTESIAN_POINT('Ctrl Pts',(-19.9015404461652,14.5780642406309,
131.221444969718)) ;
#147958 = CARTESIAN_POINT('Ctrl Pts',(-19.9928382265916,14.574764467068,131.521483463765)) ;
#147959 = CARTESIAN_POINT('Ctrl Pts',(-20.0791689532746,14.4895501192037,
131.806603095994)) ;
#147960 = CARTESIAN_POINT('Ctrl Pts',(-20.1553727313655,14.3274511862454,
132.062408003817)) ;
#147961 = CARTESIAN_POINT('Ctrl Pts',(-20.2143165511384,14.1012131862614,
132.267654668105)) ;
#147962 = CARTESIAN_POINT('Ctrl Pts',(-20.251535640847,13.8249844629114,132.409627218368)) ;
#147963 = CARTESIAN_POINT('Ctrl Pts',(-20.2632155313294,13.5214321679055,
132.476806560396)) ;
#147964 = CARTESIAN_POINT('Ctrl Pts',(-20.2480538564404,13.2103012172843,
132.465645791352)) ;
#147965 = CARTESIAN_POINT('Ctrl Pts',(-20.2064762839106,12.914853162699,132.377251371231)) ;
#147966 = CARTESIAN_POINT('Ctrl Pts',(-20.140151413628,12.6543477666719,132.216774551405)) ;
#147967 = CARTESIAN_POINT('Ctrl Pts',(-20.0543603731437,12.4511188727926,
131.999088220512)) ;
#147968 = CARTESIAN_POINT('Ctrl Pts',(-19.9529344290796,12.3156705463735,
131.736039696364)) ;
#147969 = CARTESIAN_POINT('Ctrl Pts',(-19.8434300726974,12.2603783295909,
131.449288215452)) ;
#147970 = CARTESIAN_POINT('Ctrl Pts',(-19.7328703196566,12.2883877263298,
131.159422548297)) ;
#147971 = CARTESIAN_POINT('Ctrl Pts',(-19.6285496546779,12.396958257867,130.887685326654)) ;
#147972 = CARTESIAN_POINT('Ctrl Pts',(-19.5361836894076,12.5805839699868,
130.651163338837)) ;
#147973 = CARTESIAN_POINT('Ctrl Pts',(-19.4633189319576,12.8225431227576,
130.471268902944)) ;
#147974 = CARTESIAN_POINT('Ctrl Pts',(-19.4130339180868,13.1085293602937,
130.357514271986)) ;
#147975 = CARTESIAN_POINT('Ctrl Pts',(-19.3888828182431,13.4184312850536,
130.320233884699)) ;
#147976 = CARTESIAN_POINT('Ctrl Pts',(-19.391721830465,13.725396858395,130.361439759483)) ;
#147977 = CARTESIAN_POINT('Ctrl Pts',(-19.4207326434381,14.0140710244904,
130.479477244557)) ;
#147978 = CARTESIAN_POINT('Ctrl Pts',(-19.472993335133,14.2586953063536,130.665252246815)) ;
#147979 = CARTESIAN_POINT('Ctrl Pts',(-19.5439543323498,14.4435712353924,
130.905649593416)) ;
#147980 = CARTESIAN_POINT('Ctrl Pts',(-19.6279191274748,14.5554638044199,
131.184041916383)) ;
#147981 = CARTESIAN_POINT('Ctrl Pts',(-19.718147960445,14.5862678502014,131.480744103854)) ;
#147982 = CARTESIAN_POINT('Ctrl Pts',(-19.807315566859,14.5339455357937,131.774300672977)) ;
#147983 = CARTESIAN_POINT('Ctrl Pts',(-19.8886286972119,14.4019055778879,
132.044990740636)) ;
#147984 = CARTESIAN_POINT('Ctrl Pts',(-19.9552665859861,14.1996929646046,
132.272793191288)) ;
#147985 = CARTESIAN_POINT('Ctrl Pts',(-20.0017789452845,13.9418840250199,
132.441799109411)) ;
#147986 = CARTESIAN_POINT('Ctrl Pts',(-20.0241090640634,13.6467946138759,
132.540172309611)) ;
#147987 = CARTESIAN_POINT('Ctrl Pts',(-20.0199186627607,13.3358858072713,
132.561050637465)) ;
#147988 = CARTESIAN_POINT('Ctrl Pts',(-19.9888290528914,13.0311284107843,
132.503354655419)) ;
#147989 = CARTESIAN_POINT('Ctrl Pts',(-19.9321905550994,12.7543595776973,
132.371055946195)) ;
#147990 = CARTESIAN_POINT('Ctrl Pts',(-19.8539774312581,12.5263864421984,
132.175548707132)) ;
#147991 = CARTESIAN_POINT('Ctrl Pts',(-19.7573065319154,12.360701809008,131.926557988683)) ;
#147992 = CARTESIAN_POINT('Ctrl Pts',(-19.6513712846264,12.2732420187478,
131.649911504307)) ;
#147993 = CARTESIAN_POINT('Ctrl Pts',(-19.5399002468881,12.2668291176247,
131.357543001955)) ;
#147994 = CARTESIAN_POINT('Ctrl Pts',(-19.4321205019427,12.3436152080196,
131.075766932317)) ;
#147995 = CARTESIAN_POINT('Ctrl Pts',(-19.3341292920677,12.4979167345461,
130.82268907935)) ;
#147996 = CARTESIAN_POINT('Ctrl Pts',(-19.2527820213521,12.7181780575431,
130.618144770234)) ;
#147997 = CARTESIAN_POINT('Ctrl Pts',(-19.1928530764132,12.9887184060059,
130.47616616468)) ;
#147998 = CARTESIAN_POINT('Ctrl Pts',(-19.1578999356697,13.2908826927602,
130.40720568529)) ;
#147999 = CARTESIAN_POINT('Ctrl Pts',(-19.1497953394028,13.6021683784905,
130.416637581749)) ;
#148000 = CARTESIAN_POINT('Ctrl Pts',(-19.1684189323087,13.9015373279121,
130.50424803556)) ;
#148001 = CARTESIAN_POINT('Ctrl Pts',(-19.2118191501217,14.1661757603649,
130.664218341433)) ;
#148002 = CARTESIAN_POINT('Ctrl Pts',(-19.275532904537,14.3763136740977,130.883305791061)) ;
#148003 = CARTESIAN_POINT('Ctrl Pts',(-19.3551769889654,14.519537909018,131.149161406706)) ;
#148004 = CARTESIAN_POINT('Ctrl Pts',(-19.4434530746954,14.5837467731856,
131.44005439952)) ;
#148005 = CARTESIAN_POINT('Ctrl Pts',(-19.5342180638581,14.5651055600629,
131.738406775999)) ;
#148006 = CARTESIAN_POINT('Ctrl Pts',(-19.6195559792533,14.4645028782859,
132.020822945501)) ;
#148007 = CARTESIAN_POINT('Ctrl Pts',(-19.6928888773536,14.2890439916082,
132.26821178798)) ;
#148008 = CARTESIAN_POINT('Ctrl Pts',(-19.7479581143454,14.0526944829589,
132.46209038044)) ;
#148009 = CARTESIAN_POINT('Ctrl Pts',(-19.7805744132292,13.7699865905546,
132.59055835538)) ;
#148010 = CARTESIAN_POINT('Ctrl Pts',(-19.7873817604731,13.4631529317897,
132.643534440188)) ;
#148011 = CARTESIAN_POINT('Ctrl Pts',(-19.7669187252397,13.1513621002968,
132.617087995616)) ;
#148012 = CARTESIAN_POINT('Ctrl Pts',(-19.7207142391698,12.8627668300252,
132.515003273399)) ;
#148013 = CARTESIAN_POINT('Ctrl Pts',(-19.65008748828,12.6109028722605,132.342021948642)) ;
#148014 = CARTESIAN_POINT('Ctrl Pts',(-19.561222299513,12.4200193070119,132.115293679117)) ;
#148015 = CARTESIAN_POINT('Ctrl Pts',(-19.4571858182592,12.2986947240349,
131.844776918444)) ;
#148016 = CARTESIAN_POINT('Ctrl Pts',(-19.3476615783916,12.2592723923921,
131.557732973173)) ;
#148017 = CARTESIAN_POINT('Ctrl Pts',(-19.2370467547134,12.3030853474788,
131.267903530246)) ;
#148018 = CARTESIAN_POINT('Ctrl Pts',(-19.1350692021642,12.4259705775221,
131.002874361858)) ;
#148019 = CARTESIAN_POINT('Ctrl Pts',(-19.0457242601456,12.6220549960923,
130.77519438912)) ;
#148020 = CARTESIAN_POINT('Ctrl Pts',(-18.9766829417426,12.8744669266435,
130.606582718191)) ;
#148021 = CARTESIAN_POINT('Ctrl Pts',(-18.9312995061322,13.1663405887179,
130.507131391168)) ;
#148022 = CARTESIAN_POINT('Ctrl Pts',(-18.9122926402712,13.4758788590996,
130.484651920458)) ;
#148023 = CARTESIAN_POINT('Ctrl Pts',(-18.9200960317738,13.7823952671727,
130.540566873431)) ;
#148024 = CARTESIAN_POINT('Ctrl Pts',(-18.9539251467135,14.0644181714752,
130.672684462497)) ;
#148025 = CARTESIAN_POINT('Ctrl Pts',(-19.0097351190021,14.2977471019388,
130.868637136998)) ;
#148026 = CARTESIAN_POINT('Ctrl Pts',(-19.0838281882075,14.4706193874242,
131.11830442749)) ;
#148027 = CARTESIAN_POINT('Ctrl Pts',(-19.1695978281786,14.5675955014972,
131.401997914482)) ;
#148028 = CARTESIAN_POINT('Ctrl Pts',(-19.2600457357947,14.5827756049051,
131.699282364173)) ;
#148029 = CARTESIAN_POINT('Ctrl Pts',(-19.3484197526924,14.5148008720864,
131.990598673523)) ;
#148030 = CARTESIAN_POINT('Ctrl Pts',(-19.4272267092737,14.3692243405837,
132.253858791749)) ;
#148031 = CARTESIAN_POINT('Ctrl Pts',(-19.4907681026563,14.1540994987709,
132.472794222791)) ;
#148032 = CARTESIAN_POINT('Ctrl Pts',(-19.5326959218197,13.8891946725912,
132.628217325786)) ;
#148033 = CARTESIAN_POINT('Ctrl Pts',(-19.5502934574863,13.5894849367596,
132.712773163463)) ;
#148034 = CARTESIAN_POINT('Ctrl Pts',(-19.5409583981256,13.2771022770821,
132.718722496154)) ;
#148035 = CARTESIAN_POINT('Ctrl Pts',(-19.5050204736514,12.9767129861419,
132.646781306479)) ;
#148036 = CARTESIAN_POINT('Ctrl Pts',(-19.4436491984434,12.7063602426885,
132.500801909177)) ;
#148037 = CARTESIAN_POINT('Ctrl Pts',(-19.3619009141506,12.490160978819,132.294887344641)) ;
#148038 = CARTESIAN_POINT('Ctrl Pts',(-19.2633520708704,12.3386882499648,
132.040193767955)) ;
#148039 = CARTESIAN_POINT('Ctrl Pts',(-19.1552318803299,12.2654833312748,
131.757441066399)) ;
#148040 = CARTESIAN_POINT('Ctrl Pts',(-19.0440477635001,12.2750423779192,
131.465825867201)) ;
#148041 = CARTESIAN_POINT('Ctrl Pts',(-18.937341928339,12.3673309106593,131.187290701774)) ;
#148042 = CARTESIAN_POINT('Ctrl Pts',(-18.8425063446484,12.534346926541,130.943255559375)) ;
#148043 = CARTESIAN_POINT('Ctrl Pts',(-18.7647046564001,12.7652871002756,
130.749089683899)) ;
#148044 = CARTESIAN_POINT('Ctrl Pts',(-18.709069337308,13.0444119027006,130.619786300958)) ;
#148045 = CARTESIAN_POINT('Ctrl Pts',(-18.6791499289154,13.3498617149792,
130.565502996383)) ;
#148046 = CARTESIAN_POINT('Ctrl Pts',(-18.6762315013032,13.6613614956128,
130.590188842679)) ;
#148047 = CARTESIAN_POINT('Ctrl Pts',(-18.6996281709069,13.9537822109427,
130.691518849554)) ;
#148048 = CARTESIAN_POINT('Ctrl Pts',(-18.7470501732347,14.2096141501914,
130.863178899728)) ;
#148049 = CARTESIAN_POINT('Ctrl Pts',(-18.8144755931522,14.409057323901,131.093292203471)) ;
#148050 = CARTESIAN_POINT('Ctrl Pts',(-18.8961116319339,14.5378227740497,
131.364866046126)) ;
#148051 = CARTESIAN_POINT('Ctrl Pts',(-18.9859286827012,14.5866410235712,
131.660492358741)) ;
#148052 = CARTESIAN_POINT('Ctrl Pts',(-19.0755119588269,14.5524956980778,
131.955107811092)) ;
#148053 = CARTESIAN_POINT('Ctrl Pts',(-19.1596946576678,14.436335978299,132.234399155507)) ;
#148054 = CARTESIAN_POINT('Ctrl Pts',(-19.229651373559,14.2487612510743,132.471753659897)) ;
#148055 = CARTESIAN_POINT('Ctrl Pts',(-19.2809040891234,14.0019963644833,
132.654569767843)) ;
#148056 = CARTESIAN_POINT('Ctrl Pts',(-19.3087933698156,13.7133413739479,
132.769174524247)) ;
#148057 = CARTESIAN_POINT('Ctrl Pts',(-19.3104356669662,13.4034231112183,
132.807158036576)) ;
#148058 = CARTESIAN_POINT('Ctrl Pts',(-19.2852774557655,13.0966156086416,
132.766656369269)) ;
#148059 = CARTESIAN_POINT('Ctrl Pts',(-19.2337768140943,12.8104956344232,
132.649520670295)) ;
#148060 = CARTESIAN_POINT('Ctrl Pts',(-19.1597423430483,12.5707042508866,
132.466267011948)) ;
#148061 = CARTESIAN_POINT('Ctrl Pts',(-19.0672401692143,12.3910193805736,
132.229155022395)) ;
#148062 = CARTESIAN_POINT('Ctrl Pts',(-18.9621213671864,12.2853288734926,
131.955219283)) ;
#148063 = CARTESIAN_POINT('Ctrl Pts',(-18.8515810799726,12.2609818511097,
131.665367165245)) ;
#148064 = CARTESIAN_POINT('Ctrl Pts',(-18.7418048609671,12.3204757411683,
131.377983757519)) ;
#148065 = CARTESIAN_POINT('Ctrl Pts',(-18.6416017664951,12.4582515561699,
131.118268532816)) ;
#148066 = CARTESIAN_POINT('Ctrl Pts',(-18.5559385730554,12.665899809485,130.901222578766)) ;
#148067 = CARTESIAN_POINT('Ctrl Pts',(-18.491157798158,12.926809546633,130.745020644298)) ;
#148068 = CARTESIAN_POINT('Ctrl Pts',(-18.4506024983066,13.2233761024273,
130.659630793965)) ;
#148069 = CARTESIAN_POINT('Ctrl Pts',(-18.4365710763997,13.5346576099115,
130.651764155775)) ;
#148070 = CARTESIAN_POINT('Ctrl Pts',(-18.4495188703671,13.8387960624651,
130.722809136042)) ;
#148071 = CARTESIAN_POINT('Ctrl Pts',(-18.4877033441777,14.1123017262305,
130.867484577879)) ;
#148072 = CARTESIAN_POINT('Ctrl Pts',(-18.5477031662279,14.3364686788982,
131.075912339679)) ;
#148073 = CARTESIAN_POINT('Ctrl Pts',(-18.6241085701617,14.4947707919197,
131.332129718544)) ;
#148074 = CARTESIAN_POINT('Ctrl Pts',(-18.711584236043,14.5769227854228,131.620907833145)) ;
#148075 = CARTESIAN_POINT('Ctrl Pts',(-18.8018385885695,14.5762675559882,
131.917508974305)) ;
#148076 = CARTESIAN_POINT('Ctrl Pts',(-18.8891582964534,14.4930554599536,
132.205808783895)) ;
#148077 = CARTESIAN_POINT('Ctrl Pts',(-18.965564283553,14.3331651015145,132.462123050403)) ;
#148078 = CARTESIAN_POINT('Ctrl Pts',(-19.0251852228589,14.1081176905962,
132.669421720131)) ;
#148079 = CARTESIAN_POINT('Ctrl Pts',(-19.0629634647551,13.8340179533061,
132.812904369814)) ;
#148080 = CARTESIAN_POINT('Ctrl Pts',(-19.0754768051102,13.5302899691965,
132.882602632264)) ;
#148081 = CARTESIAN_POINT('Ctrl Pts',(-19.0610963876099,13.2194242274908,
132.873681234086)) ;
#148082 = CARTESIAN_POINT('Ctrl Pts',(-19.0202875685388,12.9232188670747,
132.787534564873)) ;
#148083 = CARTESIAN_POINT('Ctrl Pts',(-18.9546995972872,12.661461296016,132.629186766265)) ;
#148084 = CARTESIAN_POINT('Ctrl Pts',(-18.8692523203122,12.4560560459253,
132.41257049924)) ;
#148085 = CARTESIAN_POINT('Ctrl Pts',(-18.7685005068051,12.3187614615208,
132.151384008345)) ;
#148086 = CARTESIAN_POINT('Ctrl Pts',(-18.6589859619205,12.2608758926762,
131.86465778122)) ;
#148087 = CARTESIAN_POINT('Ctrl Pts',(-18.5485288587057,12.2860567497161,
131.575029100165)) ;
#148088 = CARTESIAN_POINT('Ctrl Pts',(-18.4430349502106,12.3936760762178,
131.300170284857)) ;
#148089 = CARTESIAN_POINT('Ctrl Pts',(-18.3512334081958,12.5734427117125,
131.064929754193)) ;
#148090 = CARTESIAN_POINT('Ctrl Pts',(-18.2770995326014,12.8155556757963,
130.881592457997)) ;
#148091 = CARTESIAN_POINT('Ctrl Pts',(-18.2263704446761,13.1001458923633,
130.766461617706)) ;
#148092 = CARTESIAN_POINT('Ctrl Pts',(-18.2014503359618,13.4082451874709,
130.726787184823)) ;
#148093 = CARTESIAN_POINT('Ctrl Pts',(-18.2034537422446,13.7170001828003,
130.765706683009)) ;
#148094 = CARTESIAN_POINT('Ctrl Pts',(-18.2318757307596,14.0068803431456,
130.882068224642)) ;
#148095 = CARTESIAN_POINT('Ctrl Pts',(-18.2833608464469,14.2520830304775,
131.065464422881)) ;
#148096 = CARTESIAN_POINT('Ctrl Pts',(-18.3537222124873,14.4388654821964,
131.304070485803)) ;
#148097 = CARTESIAN_POINT('Ctrl Pts',(-18.437485257584,14.5532758713035,131.581913311696)) ;
#148098 = CARTESIAN_POINT('Ctrl Pts',(-18.5277052725611,14.5866372917137,
131.878613366819)) ;
#148099 = CARTESIAN_POINT('Ctrl Pts',(-18.6172454058676,14.5363254229255,
132.173356333672)) ;
#148100 = CARTESIAN_POINT('Ctrl Pts',(-18.698521140024,14.4070821758454,132.443784329166)) ;
#148101 = CARTESIAN_POINT('Ctrl Pts',(-18.7659972083928,14.2058492351143,
132.674191701494)) ;
#148102 = CARTESIAN_POINT('Ctrl Pts',(-18.8130187735829,13.9493210351354,
132.844663971232)) ;
#148103 = CARTESIAN_POINT('Ctrl Pts',(-18.8360159858587,13.6560816946818,
132.944868856986)) ;
#148104 = CARTESIAN_POINT('Ctrl Pts',(-18.8326481694973,13.345421430163,132.968143639762)) ;
#148105 = CARTESIAN_POINT('Ctrl Pts',(-18.802476587049,13.040595844376,132.913073904114)) ;
#148106 = CARTESIAN_POINT('Ctrl Pts',(-18.746226215621,12.7610203807177,132.782105503749)) ;
#148107 = CARTESIAN_POINT('Ctrl Pts',(-18.66857834825,12.5320805251594,132.588205034405)) ;
#148108 = CARTESIAN_POINT('Ctrl Pts',(-18.5730541599684,12.3651153632671,
132.342336669536)) ;
#148109 = CARTESIAN_POINT('Ctrl Pts',(-18.4664665056406,12.2743250028136,
132.064064252278)) ;
#148110 = CARTESIAN_POINT('Ctrl Pts',(-18.3549459131847,12.2660445158075,
131.771566814198)) ;
#148111 = CARTESIAN_POINT('Ctrl Pts',(-18.2473957776497,12.3402671255805,
131.490336956928)) ;
#148112 = CARTESIAN_POINT('Ctrl Pts',(-18.1489873864352,12.4924311460887,
131.236048239576)) ;
#148113 = CARTESIAN_POINT('Ctrl Pts',(-18.0671825361654,12.7106680938423,
131.030125691093)) ;
#148114 = CARTESIAN_POINT('Ctrl Pts',(-18.0064123336501,12.9803449580317,
130.885741330905)) ;
#148115 = CARTESIAN_POINT('Ctrl Pts',(-17.9706694762708,13.2833170370261,
130.814620547797)) ;
#148116 = CARTESIAN_POINT('Ctrl Pts',(-17.9618765736868,13.5926827772034,
130.82183011408)) ;
#148117 = CARTESIAN_POINT('Ctrl Pts',(-17.9797619942938,13.8936497726217,
130.907388131803)) ;
#148118 = CARTESIAN_POINT('Ctrl Pts',(-18.0224154975657,14.1589430320387,
131.065096694531)) ;
#148119 = CARTESIAN_POINT('Ctrl Pts',(-18.0856974126482,14.3711507440271,
131.282979614378)) ;
#148120 = CARTESIAN_POINT('Ctrl Pts',(-18.1646930507973,14.5162610526243,
131.546828965686)) ;
#148121 = CARTESIAN_POINT('Ctrl Pts',(-18.2535370462115,14.5833063446483,
131.839656321843)) ;
#148122 = CARTESIAN_POINT('Ctrl Pts',(-18.3441028407741,14.566512972423,132.137337037032)) ;
#148123 = CARTESIAN_POINT('Ctrl Pts',(-18.4293737033493,14.4685224251672,
132.419443796344)) ;
#148124 = CARTESIAN_POINT('Ctrl Pts',(-18.503107615546,14.295496638092,132.667961157457)) ;
#148125 = CARTESIAN_POINT('Ctrl Pts',(-18.5589734583344,14.0596946684097,
132.864306733473)) ;
#148126 = CARTESIAN_POINT('Ctrl Pts',(-18.5922504211388,13.7784556311811,
132.994643197558)) ;
#148127 = CARTESIAN_POINT('Ctrl Pts',(-18.5996736634581,13.4704205664196,
133.049595144208)) ;
#148128 = CARTESIAN_POINT('Ctrl Pts',(-18.5803706966428,13.1626907003778,
133.026063848939)) ;
#148129 = CARTESIAN_POINT('Ctrl Pts',(-18.5344403794479,12.8697533326654,
132.9251808791)) ;
#148130 = CARTESIAN_POINT('Ctrl Pts',(-18.4650781878909,12.6186668419938,
132.755581911683)) ;
#148131 = CARTESIAN_POINT('Ctrl Pts',(-18.3758902615424,12.4240570557475,
132.528231421364)) ;
#148132 = CARTESIAN_POINT('Ctrl Pts',(-18.2732592245776,12.3017129015635,
132.261457008441)) ;
#148133 = CARTESIAN_POINT('Ctrl Pts',(-18.1630414162269,12.259212443294,131.972645306552)) ;
#148134 = CARTESIAN_POINT('Ctrl Pts',(-18.0528667103631,12.3002004247184,
131.683920182709)) ;
#148135 = CARTESIAN_POINT('Ctrl Pts',(-17.9495131746608,12.4222100082891,
131.41522733535)) ;
#148136 = CARTESIAN_POINT('Ctrl Pts',(-17.8604373492352,12.6151763777399,
131.188068661744)) ;
#148137 = CARTESIAN_POINT('Ctrl Pts',(-17.7905190303083,12.8667635442981,
131.016997058462)) ;
#148138 = CARTESIAN_POINT('Ctrl Pts',(-17.7445835247863,13.156608287975,130.915794965958)) ;
#148139 = CARTESIAN_POINT('Ctrl Pts',(-17.7246276819165,13.4669634913823,
130.890658029617)) ;
#148140 = CARTESIAN_POINT('Ctrl Pts',(-17.7317937319993,13.7743605544172,
130.944768434693)) ;
#148141 = CARTESIAN_POINT('Ctrl Pts',(-17.7646329783859,14.0556835364492,
131.073777527433)) ;
#148142 = CARTESIAN_POINT('Ctrl Pts',(-17.8201538331759,14.2923698340539,
131.269107271489)) ;
#148143 = CARTESIAN_POINT('Ctrl Pts',(-17.8939804671672,14.4669398089711,
131.518026818099)) ;
#148144 = CARTESIAN_POINT('Ctrl Pts',(-17.9790094951731,14.5658237072004,
131.799368733708)) ;
#148145 = CARTESIAN_POINT('Ctrl Pts',(-18.0699355731019,14.5834030804103,
132.098247995134)) ;
#148146 = CARTESIAN_POINT('Ctrl Pts',(-18.1579904994827,14.5182209640518,
132.388435699064)) ;
#148147 = CARTESIAN_POINT('Ctrl Pts',(-18.2378368617494,14.3732472744243,
132.655041938253)) ;
#148148 = CARTESIAN_POINT('Ctrl Pts',(-18.3012363737009,14.1617341160313,
132.873234199414)) ;
#148149 = CARTESIAN_POINT('Ctrl Pts',(-18.3441500746653,13.8968739581495,
133.031718215328)) ;
#148150 = CARTESIAN_POINT('Ctrl Pts',(-18.36238591691,13.5970561201623,133.118203483067)) ;
#148151 = CARTESIAN_POINT('Ctrl Pts',(-18.353745765101,13.2853498772371,133.126116024577)) ;
#148152 = CARTESIAN_POINT('Ctrl Pts',(-18.3186534118777,12.9854214225964,
133.056533301362)) ;
#148153 = CARTESIAN_POINT('Ctrl Pts',(-18.2582555615791,12.7145026725385,
132.913294641903)) ;
#148154 = CARTESIAN_POINT('Ctrl Pts',(-18.1767063643979,12.4953422799607,
132.708123384207)) ;
#148155 = CARTESIAN_POINT('Ctrl Pts',(-18.0783433317562,12.341785792788,132.454021595677)) ;
#148156 = CARTESIAN_POINT('Ctrl Pts',(-17.9707155643602,12.2665368205457,
132.172612709289)) ;
#148157 = CARTESIAN_POINT('Ctrl Pts',(-17.8596316902576,12.2735361579836,
131.881255970493)) ;
#148158 = CARTESIAN_POINT('Ctrl Pts',(-17.7527316072051,12.3632299170458,
131.602134296824)) ;
#148159 = CARTESIAN_POINT('Ctrl Pts',(-17.6571606283092,12.5286847379392,
131.356056473991)) ;
#148160 = CARTESIAN_POINT('Ctrl Pts',(-17.5788794210432,12.7579694052531,
131.16046780139)) ;
#148161 = CARTESIAN_POINT('Ctrl Pts',(-17.5226365751704,13.0352202264865,
131.029305711414)) ;
#148162 = CARTESIAN_POINT('Ctrl Pts',(-17.4918816488371,13.3405828522819,
130.972629478393)) ;
#148163 = CARTESIAN_POINT('Ctrl Pts',(-17.4881115560766,13.6512271404406,
130.994714982278)) ;
#148164 = CARTESIAN_POINT('Ctrl Pts',(-17.5107807119142,13.945858673121,131.094068308616)) ;
#148165 = CARTESIAN_POINT('Ctrl Pts',(-17.5577200823908,14.2033946436315,
131.264378805117)) ;
#148166 = CARTESIAN_POINT('Ctrl Pts',(-17.6244678428917,14.4040391097263,
131.492418461584)) ;
#148167 = CARTESIAN_POINT('Ctrl Pts',(-17.7056627363047,14.5350227363909,
131.762669575012)) ;
#148168 = CARTESIAN_POINT('Ctrl Pts',(-17.7954834341729,14.5864958768454,
132.058353936923)) ;
#148169 = CARTESIAN_POINT('Ctrl Pts',(-17.885321308586,14.554416926093,132.353783687721)) ;
#148170 = CARTESIAN_POINT('Ctrl Pts',(-17.9692937621649,14.4414134388981,
132.632251051087)) ;
#148171 = CARTESIAN_POINT('Ctrl Pts',(-18.0401061570019,14.2551029689439,
132.872267335541)) ;
#148172 = CARTESIAN_POINT('Ctrl Pts',(-18.0919280847591,14.0100365387615,
133.056707389317)) ;
#148173 = CARTESIAN_POINT('Ctrl Pts',(-18.120568608652,13.7214335720741,133.173607236888)) ;
#148174 = CARTESIAN_POINT('Ctrl Pts',(-18.1230342621043,13.4135493080175,
133.213803330473)) ;
#148175 = CARTESIAN_POINT('Ctrl Pts',(-18.0984830751662,13.1045553567054,
133.175282525716)) ;
#148176 = CARTESIAN_POINT('Ctrl Pts',(-18.0481691146944,12.8197359120567,
133.061332232554)) ;
#148177 = CARTESIAN_POINT('Ctrl Pts',(-17.9741995914314,12.576213522993,132.878551316788)) ;
#148178 = CARTESIAN_POINT('Ctrl Pts',(-17.882278063881,12.3952019972504,132.643060046006)) ;
#148179 = CARTESIAN_POINT('Ctrl Pts',(-17.7773165034846,12.2871509168402,
132.369622625289)) ;
#148180 = CARTESIAN_POINT('Ctrl Pts',(-17.6670900155522,12.2605661250461,
132.080610377323)) ;
#148181 = CARTESIAN_POINT('Ctrl Pts',(-17.5571725360923,12.3174696014915,
131.792809249696)) ;
#148182 = CARTESIAN_POINT('Ctrl Pts',(-17.4563916553665,12.45350954949,131.531487926555)) ;
#148183 = CARTESIAN_POINT('Ctrl Pts',(-17.3704389160813,12.6588730933983,
131.313511700696)) ;
#148184 = CARTESIAN_POINT('Ctrl Pts',(-17.3049297018148,12.9185732452431,
131.155205502056)) ;
#148185 = CARTESIAN_POINT('Ctrl Pts',(-17.2636296695763,13.2144047021654,
131.067638080618)) ;
#148186 = CARTESIAN_POINT('Ctrl Pts',(-17.2488249122446,13.5255441654578,
131.057510868015)) ;
#148187 = CARTESIAN_POINT('Ctrl Pts',(-17.2609296287798,13.8297539954917,
131.126033363959)) ;
#148188 = CARTESIAN_POINT('Ctrl Pts',(-17.2985030763623,14.1049217876101,
131.268992812532)) ;
#148189 = CARTESIAN_POINT('Ctrl Pts',(-17.3575596549785,14.329872377713,131.474493311217)) ;
#148190 = CARTESIAN_POINT('Ctrl Pts',(-17.4340909075981,14.491552798162,131.731324559513)) ;
#148191 = CARTESIAN_POINT('Ctrl Pts',(-17.5210857954015,14.5755974464537,
132.01858139833)) ;
#148192 = CARTESIAN_POINT('Ctrl Pts',(-17.6114837359406,14.5774288314458,
132.315662323554)) ;
#148193 = CARTESIAN_POINT('Ctrl Pts',(-17.698796355316,14.4968431442199,132.603852489875)) ;
#148194 = CARTESIAN_POINT('Ctrl Pts',(-17.775879820333,14.3385595684728,132.862263452361)) ;
#148195 = CARTESIAN_POINT('Ctrl Pts',(-17.835998603421,14.1152210821619,133.070993327708)) ;
#148196 = CARTESIAN_POINT('Ctrl Pts',(-17.874456885931,13.8419814694385,133.216493798034)) ;
#148197 = CARTESIAN_POINT('Ctrl Pts',(-17.8876898230409,13.5398085198315,
133.28818438758)) ;
#148198 = CARTESIAN_POINT('Ctrl Pts',(-17.8741319200142,13.2280435921434,
133.281749241004)) ;
#148199 = CARTESIAN_POINT('Ctrl Pts',(-17.8337766712165,12.9300591046375,
133.197059291018)) ;
#148200 = CARTESIAN_POINT('Ctrl Pts',(-17.7691101800502,12.6684084427586,
133.041237278321)) ;
#148201 = CARTESIAN_POINT('Ctrl Pts',(-17.6840581698328,12.4608091594121,
132.825832817714)) ;
#148202 = CARTESIAN_POINT('Ctrl Pts',(-17.5835644067408,12.3214093535999,
132.565418506094)) ;
#148203 = CARTESIAN_POINT('Ctrl Pts',(-17.4740202572772,12.261330300397,132.27865503774)) ;
#148204 = CARTESIAN_POINT('Ctrl Pts',(-17.3639381852683,12.2843254988424,
131.989996972432)) ;
#148205 = CARTESIAN_POINT('Ctrl Pts',(-17.2586432752413,12.3887269721217,
131.71555751289)) ;
#148206 = CARTESIAN_POINT('Ctrl Pts',(-17.1657956374155,12.5673627436567,
131.477456219259)) ;
#148207 = CARTESIAN_POINT('Ctrl Pts',(-17.0911351100522,12.8080166806353,
131.292569279306)) ;
#148208 = CARTESIAN_POINT('Ctrl Pts',(-17.0396694706571,13.0914774354823,
131.175275601717)) ;
#148209 = CARTESIAN_POINT('Ctrl Pts',(-17.0139478947046,13.4005589670674,
131.133400258637)) ;
#148210 = CARTESIAN_POINT('Ctrl Pts',(-17.0152836707085,13.7083911596742,
131.170245097133)) ;
#148211 = CARTESIAN_POINT('Ctrl Pts',(-17.0428555359998,13.9985991378762,
131.284050048509)) ;
#148212 = CARTESIAN_POINT('Ctrl Pts',(-17.0937913243256,14.2457812559265,
131.465901397237)) ;
#148213 = CARTESIAN_POINT('Ctrl Pts',(-17.1637439823567,14.4345734153115,
131.703335486007)) ;
#148214 = CARTESIAN_POINT('Ctrl Pts',(-17.2472660646445,14.5511370879547,
131.980487773352)) ;
#148215 = CARTESIAN_POINT('Ctrl Pts',(-17.337120360927,14.5867802187907,132.276018738499)) ;
#148216 = CARTESIAN_POINT('Ctrl Pts',(-17.4268009039852,14.5391948483821,
132.571169606425)) ;
#148217 = CARTESIAN_POINT('Ctrl Pts',(-17.50867960202,14.411534541166,132.843482510367)) ;
#148218 = CARTESIAN_POINT('Ctrl Pts',(-17.5762457585438,14.2134355911455,
133.073946320548)) ;
#148219 = CARTESIAN_POINT('Ctrl Pts',(-17.6241241514975,13.9582377807151,
133.246970111031)) ;
#148220 = CARTESIAN_POINT('Ctrl Pts',(-17.6479486624558,13.6646542857207,
133.349718970844)) ;
#148221 = CARTESIAN_POINT('Ctrl Pts',(-17.6453414061695,13.354183694307,133.375210052951)) ;
#148222 = CARTESIAN_POINT('Ctrl Pts',(-17.6158058941285,13.0484269475921,
133.322056715755)) ;
#148223 = CARTESIAN_POINT('Ctrl Pts',(-17.560597882875,12.7694396144753,133.193932763753)) ;
#148224 = CARTESIAN_POINT('Ctrl Pts',(-17.4834695817437,12.5380417818578,
133.001624723729)) ;
#148225 = CARTESIAN_POINT('Ctrl Pts',(-17.3877869395594,12.3683286103215,
132.755475944)) ;
#148226 = CARTESIAN_POINT('Ctrl Pts',(-17.2819063750014,12.2760420301782,
132.479111929425)) ;
#148227 = CARTESIAN_POINT('Ctrl Pts',(-17.1709198373748,12.2649171956023,
132.1880250579)) ;
#148228 = CARTESIAN_POINT('Ctrl Pts',(-17.0626411499466,12.3368690602114,
131.904826957427)) ;
#148229 = CARTESIAN_POINT('Ctrl Pts',(-16.9637873323835,12.4871142426883,
131.64926067196)) ;
#148230 = CARTESIAN_POINT('Ctrl Pts',(-16.8812937864313,12.7041605723025,
131.441394001432)) ;
#148231 = CARTESIAN_POINT('Ctrl Pts',(-16.8200816285751,12.9721742229255,
131.295646395614)) ;
#148232 = CARTESIAN_POINT('Ctrl Pts',(-16.7836474217345,13.2726902909237,
131.222315130629)) ;
#148233 = CARTESIAN_POINT('Ctrl Pts',(-16.773935559665,13.5844634712024,131.227094828885)) ;
#148234 = CARTESIAN_POINT('Ctrl Pts',(-16.7911394414361,13.8852370935213,
131.310575943605)) ;
#148235 = CARTESIAN_POINT('Ctrl Pts',(-16.8328615291614,14.1508960461137,
131.465435883749)) ;
#148236 = CARTESIAN_POINT('Ctrl Pts',(-16.8957649980785,14.3659570347197,
131.682335572948)) ;
#148237 = CARTESIAN_POINT('Ctrl Pts',(-16.9747508643797,14.513384444757,131.946282517817)) ;
#148238 = CARTESIAN_POINT('Ctrl Pts',(-17.0626794840163,14.58228249035,132.236157160365)) ;
#148239 = CARTESIAN_POINT('Ctrl Pts',(-17.1535083371299,14.5684017700248,
132.534690900371)) ;
#148240 = CARTESIAN_POINT('Ctrl Pts',(-17.2392135238107,14.4726240352221,
132.818127204052)) ;
#148241 = CARTESIAN_POINT('Ctrl Pts',(-17.3135721300852,14.3009018256013,
133.068577196943)) ;
#148242 = CARTESIAN_POINT('Ctrl Pts',(-17.3697922036115,14.0676662021592,
133.265814069086)) ;
#148243 = CARTESIAN_POINT('Ctrl Pts',(-17.4038524116641,13.7867923428731,
133.398526236623)) ;
#148244 = CARTESIAN_POINT('Ctrl Pts',(-17.4120797990217,13.4808115770732,
133.455650692552)) ;
#148245 = CARTESIAN_POINT('Ctrl Pts',(-17.393480319056,13.1706177379304,133.434416238406)) ;
#148246 = CARTESIAN_POINT('Ctrl Pts',(-17.3481649808676,12.8770484120512,
133.335317034958)) ;
#148247 = CARTESIAN_POINT('Ctrl Pts',(-17.2795456429539,12.6251910549939,
133.167821675258)) ;
#148248 = CARTESIAN_POINT('Ctrl Pts',(-17.191091114337,12.4289584768191,132.942537201925)) ;
#148249 = CARTESIAN_POINT('Ctrl Pts',(-17.0882142927875,12.3038002387545,
132.675222788334)) ;
#148250 = CARTESIAN_POINT('Ctrl Pts',(-16.978326475091,12.2593442699651,132.387300667687)) ;
#148251 = CARTESIAN_POINT('Ctrl Pts',(-16.8683094798042,12.2978898769658,
132.098965870951)) ;
#148252 = CARTESIAN_POINT('Ctrl Pts',(-16.7648959897926,12.4169444283248,
131.829998734971)) ;
#148253 = CARTESIAN_POINT('Ctrl Pts',(-16.6747206222422,12.6093773195972,
131.599861765361)) ;
#148254 = CARTESIAN_POINT('Ctrl Pts',(-16.6045685863941,12.8583734122104,
131.427937124288)) ;
#148255 = CARTESIAN_POINT('Ctrl Pts',(-16.5577153827191,13.1480449714035,
131.324145807381)) ;
#148256 = CARTESIAN_POINT('Ctrl Pts',(-16.5370475027575,13.4582417931766,
131.296933049071)) ;
#148257 = CARTESIAN_POINT('Ctrl Pts',(-16.5434122344791,13.7655079117814,
131.348644885379)) ;
#148258 = CARTESIAN_POINT('Ctrl Pts',(-16.57559115125,14.0483169670967,131.475777606241)) ;
#148259 = CARTESIAN_POINT('Ctrl Pts',(-16.6304376248013,14.285999002941,131.669073710126)) ;
#148260 = CARTESIAN_POINT('Ctrl Pts',(-16.7035444070544,14.4624790496655,
131.915796927174)) ;
#148261 = CARTESIAN_POINT('Ctrl Pts',(-16.788889987511,14.5642183911393,132.198286823634)) ;
#148262 = CARTESIAN_POINT('Ctrl Pts',(-16.8792004445873,14.5841609498882,
132.495150629956)) ;
#148263 = CARTESIAN_POINT('Ctrl Pts',(-16.9679697628479,14.520970734674,132.787641400003)) ;
#148264 = CARTESIAN_POINT('Ctrl Pts',(-17.0476011313862,14.3791779358065,
133.053372603054)) ;
#148265 = CARTESIAN_POINT('Ctrl Pts',(-17.1119011916955,14.1688151362551,
133.274346330725)) ;
#148266 = CARTESIAN_POINT('Ctrl Pts',(-17.1554181544879,13.9051957088918,
133.43458020011)) ;
#148267 = CARTESIAN_POINT('Ctrl Pts',(-17.1743976183435,13.60715006879,133.523128764007)) ;
#148268 = CARTESIAN_POINT('Ctrl Pts',(-17.1667123705159,13.2953843814918,
133.533839215501)) ;
#148269 = CARTESIAN_POINT('Ctrl Pts',(-17.1321236360563,12.9930169526984,
133.465935301798)) ;
#148270 = CARTESIAN_POINT('Ctrl Pts',(-17.0726673783466,12.7222273700058,
133.325286975909)) ;
#148271 = CARTESIAN_POINT('Ctrl Pts',(-16.991448956747,12.500544093303,133.121191114684)) ;
#148272 = CARTESIAN_POINT('Ctrl Pts',(-16.8935056731294,12.3451353324325,
132.868292190144)) ;
#148273 = CARTESIAN_POINT('Ctrl Pts',(-16.7860479429717,12.2674914285865,
132.587388959171)) ;
#148274 = CARTESIAN_POINT('Ctrl Pts',(-16.6746490295685,12.2722652657277,
132.295199791128)) ;
#148275 = CARTESIAN_POINT('Ctrl Pts',(-16.5676447482205,12.3599738467364,
132.01575034793)) ;
#148276 = CARTESIAN_POINT('Ctrl Pts',(-16.4720746525094,12.5226378491769,
131.769531391802)) ;
#148277 = CARTESIAN_POINT('Ctrl Pts',(-16.3929497865683,12.7508222616319,
131.571573710982)) ;
#148278 = CARTESIAN_POINT('Ctrl Pts',(-16.3359366151232,13.0279565462644,
131.438259358999)) ;
#148279 = CARTESIAN_POINT('Ctrl Pts',(-16.3045984521949,13.3323087573567,
131.379816911574)) ;
#148280 = CARTESIAN_POINT('Ctrl Pts',(-16.3000641118992,13.6420774120511,
131.399562313609)) ;
#148281 = CARTESIAN_POINT('Ctrl Pts',(-16.3219465791947,13.9374078331077,
131.496607386123)) ;
#148282 = CARTESIAN_POINT('Ctrl Pts',(-16.3681919814467,14.1965319396346,
131.664898838707)) ;
#148283 = CARTESIAN_POINT('Ctrl Pts',(-16.4348677786798,14.3999725779251,
131.892918294996)) ;
#148284 = CARTESIAN_POINT('Ctrl Pts',(-16.5153412365751,14.5320840128439,
132.160883084608)) ;
#148285 = CARTESIAN_POINT('Ctrl Pts',(-16.6048687150457,14.5862914481129,
132.455659839408)) ;
#148286 = CARTESIAN_POINT('Ctrl Pts',(-16.6952852040637,14.5562373183141,
132.752967353517)) ;
#148287 = CARTESIAN_POINT('Ctrl Pts',(-16.7790126449957,14.4460760086482,
133.030515124208)) ;
#148288 = CARTESIAN_POINT('Ctrl Pts',(-16.8506184653848,14.2613118690052,
133.272970541313)) ;
#148289 = CARTESIAN_POINT('Ctrl Pts',(-16.9030456298473,14.0168342944471,
133.459259475347)) ;
#148290 = CARTESIAN_POINT('Ctrl Pts',(-16.9322577874261,13.7314084921459,
133.57757681541)) ;
#148291 = CARTESIAN_POINT('Ctrl Pts',(-16.9355345400515,13.4213927772855,
133.620410847763)) ;
#148292 = CARTESIAN_POINT('Ctrl Pts',(-16.9118235568279,13.1138964811438,
133.584144735377)) ;
#148293 = CARTESIAN_POINT('Ctrl Pts',(-16.8621882966479,12.8273574964974,
133.472259648909)) ;
#148294 = CARTESIAN_POINT('Ctrl Pts',(-16.7887479806333,12.5821904273637,
133.291045013938)) ;
#148295 = CARTESIAN_POINT('Ctrl Pts',(-16.6971693689497,12.3992406636329,
133.056586334083)) ;
#148296 = CARTESIAN_POINT('Ctrl Pts',(-16.592840687638,12.2892635372044,132.784882740936)) ;
#148297 = CARTESIAN_POINT('Ctrl Pts',(-16.4824515586233,12.2601882731061,
132.495468659447)) ;
#148298 = CARTESIAN_POINT('Ctrl Pts',(-16.3727887175883,12.3144490332909,
132.208288643135)) ;
#148299 = CARTESIAN_POINT('Ctrl Pts',(-16.2715474674814,12.4481500310982,
131.945651708052)) ;
#148300 = CARTESIAN_POINT('Ctrl Pts',(-16.1850122658441,12.6515765338915,
131.725979718577)) ;
#148301 = CARTESIAN_POINT('Ctrl Pts',(-16.1185129147627,12.9112090409297,
131.564943253957)) ;
#148302 = CARTESIAN_POINT('Ctrl Pts',(-16.0765700513496,13.2069680634014,
131.475556101884)) ;
#148303 = CARTESIAN_POINT('Ctrl Pts',(-16.0610820422751,13.5165270688446,
131.463274345175)) ;
#148304 = CARTESIAN_POINT('Ctrl Pts',(-16.0725280585734,13.8224961105202,
131.530016185453)) ;
#148305 = CARTESIAN_POINT('Ctrl Pts',(-16.1092827001771,14.0973150070006,
131.670412542272)) ;
#148306 = CARTESIAN_POINT('Ctrl Pts',(-16.1678671523189,14.3244517952957,
131.874605730233)) ;
#148307 = CARTESIAN_POINT('Ctrl Pts',(-16.2438791319829,14.4877799553715,
132.129858835317)) ;
#148308 = CARTESIAN_POINT('Ctrl Pts',(-16.3305380227414,14.5742904873528,
132.416097152061)) ;
#148309 = CARTESIAN_POINT('Ctrl Pts',(-16.4213187544321,14.5785355411289,
132.714436240136)) ;
#148310 = CARTESIAN_POINT('Ctrl Pts',(-16.5087008967038,14.4999983215905,
133.002794438483)) ;
#148311 = CARTESIAN_POINT('Ctrl Pts',(-16.5858465437254,14.3447574247582,
133.261227247573)) ;
#148312 = CARTESIAN_POINT('Ctrl Pts',(-16.6467792052261,14.1223924190304,
133.472459939162)) ;
#148313 = CARTESIAN_POINT('Ctrl Pts',(-16.6858377372559,13.8510686498015,
133.619622649373)) ;
#148314 = CARTESIAN_POINT('Ctrl Pts',(-16.6999157232596,13.5484336095185,
133.693900204533)) ;
#148315 = CARTESIAN_POINT('Ctrl Pts',(-16.6870922505193,13.2370241566132,
133.689564216562)) ;
#148316 = CARTESIAN_POINT('Ctrl Pts',(-16.6476640703555,12.9391311523709,
133.60748871607)) ;
#148317 = CARTESIAN_POINT('Ctrl Pts',(-16.5836531085729,12.6756660362993,
133.453625999795)) ;
#148318 = CARTESIAN_POINT('Ctrl Pts',(-16.4988970609242,12.4657027909829,
133.239173128773)) ;
#148319 = CARTESIAN_POINT('Ctrl Pts',(-16.3988089904537,12.324474551251,132.979918734029)) ;
#148320 = CARTESIAN_POINT('Ctrl Pts',(-16.2899174957269,12.2619232759168,
132.694915080436)) ;
#148321 = CARTESIAN_POINT('Ctrl Pts',(-16.1789998814677,12.2825882347195,
132.40405140961)) ;
#148322 = CARTESIAN_POINT('Ctrl Pts',(-16.0738071067368,12.3846501160854,
132.129802156463)) ;
#148323 = CARTESIAN_POINT('Ctrl Pts',(-15.9805197501771,12.5611187121008,
131.890409483026)) ;
#148324 = CARTESIAN_POINT('Ctrl Pts',(-15.9052414037615,12.800128888062,131.703709693564)) ;
#148325 = CARTESIAN_POINT('Ctrl Pts',(-15.8530321981078,13.0829558390025,
131.584286648028)) ;
#148326 = CARTESIAN_POINT('Ctrl Pts',(-15.8265593389286,13.3903655442342,
131.540077569351)) ;
#148327 = CARTESIAN_POINT('Ctrl Pts',(-15.8271016367445,13.7001366182577,
131.574787860055)) ;
#148328 = CARTESIAN_POINT('Ctrl Pts',(-15.853828406241,13.9898881867711,131.685965203616)) ;
#148329 = CARTESIAN_POINT('Ctrl Pts',(-15.9041829439333,14.2391934618933,
131.866194894701)) ;
#148330 = CARTESIAN_POINT('Ctrl Pts',(-15.9735601601396,14.4298567293758,
132.101910083047)) ;
#148331 = CARTESIAN_POINT('Ctrl Pts',(-16.0572845306013,14.5492471460414,
132.379848702365)) ;
#148332 = CARTESIAN_POINT('Ctrl Pts',(-16.1467466300587,14.5868020956478,
132.674116206761)) ;
#148333 = CARTESIAN_POINT('Ctrl Pts',(-16.2364624285869,14.5417975160937,
132.969339452112)) ;
#148334 = CARTESIAN_POINT('Ctrl Pts',(-16.3186966945366,14.416208825978,133.242712197891)) ;
#148335 = CARTESIAN_POINT('Ctrl Pts',(-16.3867169591892,14.22040833296,133.474453835102)) ;
#148336 = CARTESIAN_POINT('Ctrl Pts',(-16.4354660410799,13.9647701256438,
133.650242067901)) ;
#148337 = CARTESIAN_POINT('Ctrl Pts',(-16.4598035300757,13.6739288758575,
133.75425884754)) ;
#148338 = CARTESIAN_POINT('Ctrl Pts',(-16.4579839350789,13.3623285139176,
133.782197585911)) ;
#148339 = CARTESIAN_POINT('Ctrl Pts',(-16.4292625349313,13.0574724687543,
133.731279710622)) ;
#148340 = CARTESIAN_POINT('Ctrl Pts',(-16.374866435716,12.7770677304932,133.605541007664)) ;
#148341 = CARTESIAN_POINT('Ctrl Pts',(-16.2976392682529,12.5427865194022,
133.413183101308)) ;
#148342 = CARTESIAN_POINT('Ctrl Pts',(-16.2035752797556,12.3731888439483,
133.171342588508)) ;
#148343 = CARTESIAN_POINT('Ctrl Pts',(-16.0973342716302,12.2773794382998,
132.894136279027)) ;
#148344 = CARTESIAN_POINT('Ctrl Pts',(-15.9860703154779,12.2641879645069,
132.602324249829)) ;
#148345 = CARTESIAN_POINT('Ctrl Pts',(-15.8780029132509,12.3335960528712,
132.319627851263)) ;
#148346 = CARTESIAN_POINT('Ctrl Pts',(-15.7787561476632,12.4815616516049,
132.062913298757)) ;
#148347 = CARTESIAN_POINT('Ctrl Pts',(-15.6956710002437,12.6968287193189,
131.85332343263)) ;
#148348 = CARTESIAN_POINT('Ctrl Pts',(-15.6336749818423,12.9642190193072,
131.705359751562)) ;
#148349 = CARTESIAN_POINT('Ctrl Pts',(-15.5965148974486,13.2637554960381,
131.629865315315)) ;
#148350 = CARTESIAN_POINT('Ctrl Pts',(-15.5861011095343,13.5766923878532,
131.632725594872)) ;
#148351 = CARTESIAN_POINT('Ctrl Pts',(-15.6023489976743,13.875372212648,131.713101997748)) ;
#148352 = CARTESIAN_POINT('Ctrl Pts',(-15.6436597772124,14.1446745454968,
131.86704227389)) ;
#148353 = CARTESIAN_POINT('Ctrl Pts',(-15.7060100158634,14.3606486125631,
132.082254737154)) ;
#148354 = CARTESIAN_POINT('Ctrl Pts',(-15.7843216644605,14.5100785842148,
132.344127870228)) ;
#148355 = CARTESIAN_POINT('Ctrl Pts',(-15.8727612750498,14.581577583442,132.635751029614)) ;
#148356 = CARTESIAN_POINT('Ctrl Pts',(-15.9629519571558,14.5700419857243,
132.932166916061)) ;
#148357 = CARTESIAN_POINT('Ctrl Pts',(-16.0493003352905,14.4761037677004,
133.217652319363)) ;
#148358 = CARTESIAN_POINT('Ctrl Pts',(-16.1236984343831,14.3074346492421,
133.468021805579)) ;
#148359 = CARTESIAN_POINT('Ctrl Pts',(-16.1809456998344,14.0735726196759,
133.668564628927)) ;
#148360 = CARTESIAN_POINT('Ctrl Pts',(-16.2152999512208,13.7966474612173,
133.801775914891)) ;
#148361 = CARTESIAN_POINT('Ctrl Pts',(-16.2244569868023,13.4894705422107,
133.861811553858)) ;
#148362 = CARTESIAN_POINT('Ctrl Pts',(-16.2066485882241,13.1800818443726,
133.842775723282)) ;
#148363 = CARTESIAN_POINT('Ctrl Pts',(-16.1621152395961,12.8853356216509,
133.745994410451)) ;
#148364 = CARTESIAN_POINT('Ctrl Pts',(-16.0940667692907,12.6318026022688,
133.580197551014)) ;
#148365 = CARTESIAN_POINT('Ctrl Pts',(-16.0060721923492,12.4337108519891,
133.356267245877)) ;
#148366 = CARTESIAN_POINT('Ctrl Pts',(-15.903730601277,12.3064394714406,133.090449633245)) ;
#148367 = CARTESIAN_POINT('Ctrl Pts',(-15.7936389437268,12.2594672533841,
132.802032639163)) ;
#148368 = CARTESIAN_POINT('Ctrl Pts',(-15.6836419614988,12.2954707769561,
132.513712206169)) ;
#148369 = CARTESIAN_POINT('Ctrl Pts',(-15.5793368562183,12.4135506751844,
132.242361064916)) ;
#148370 = CARTESIAN_POINT('Ctrl Pts',(-15.489886034823,12.6014761711869,132.013888945583)) ;
#148371 = CARTESIAN_POINT('Ctrl Pts',(-15.4184189651294,12.8505488628237,
131.838381349536)) ;
#148372 = CARTESIAN_POINT('Ctrl Pts',(-15.3709336783578,13.1393106619413,
131.732721363692)) ;
#148373 = CARTESIAN_POINT('Ctrl Pts',(-15.3494680304114,13.4495612623856,
131.70321675522)) ;
#148374 = CARTESIAN_POINT('Ctrl Pts',(-15.3550699615667,13.756653092605,131.752638136779)) ;
#148375 = CARTESIAN_POINT('Ctrl Pts',(-15.3864985515293,14.0404143429371,
131.877571942581)) ;
#148376 = CARTESIAN_POINT('Ctrl Pts',(-15.4407185610853,14.279856789825,132.069044870554)) ;
#148377 = CARTESIAN_POINT('Ctrl Pts',(-15.5137414504908,14.458860778503,132.315668883867)) ;
#148378 = CARTESIAN_POINT('Ctrl Pts',(-15.5983584888055,14.5622468104248,
132.595839857605)) ;
#148379 = CARTESIAN_POINT('Ctrl Pts',(-15.6889603783722,14.5847589311911,
132.893687701564)) ;
#148380 = CARTESIAN_POINT('Ctrl Pts',(-15.7776166007816,14.5239999496504,
133.185745577127)) ;
#148381 = CARTESIAN_POINT('Ctrl Pts',(-15.8577182680662,14.3842926160759,
133.452895744165)) ;
#148382 = CARTESIAN_POINT('Ctrl Pts',(-15.9225060605763,14.1758059361387,
133.675275406814)) ;
#148383 = CARTESIAN_POINT('Ctrl Pts',(-15.9667693658469,13.9130884623637,
133.837741432542)) ;
#148384 = CARTESIAN_POINT('Ctrl Pts',(-15.9864293474601,13.6151580257587,
133.928333937263)) ;
#148385 = CARTESIAN_POINT('Ctrl Pts',(-15.9795433739699,13.3050554492312,
133.941210084392)) ;
#148386 = CARTESIAN_POINT('Ctrl Pts',(-15.9458051665583,13.0018871941951,
133.87580827376)) ;
#148387 = CARTESIAN_POINT('Ctrl Pts',(-15.886867851103,12.7291798147193,133.736763615943)) ;
#148388 = CARTESIAN_POINT('Ctrl Pts',(-15.8062485274327,12.5061726886818,
133.534385452508)) ;
#148389 = CARTESIAN_POINT('Ctrl Pts',(-15.709090071799,12.3489726322612,133.283660587009)) ;
#148390 = CARTESIAN_POINT('Ctrl Pts',(-15.6014248041649,12.2685650125514,
133.002280999057)) ;
#148391 = CARTESIAN_POINT('Ctrl Pts',(-15.4904361859871,12.2709027437165,
132.711164577751)) ;
#148392 = CARTESIAN_POINT('Ctrl Pts',(-15.3831558118205,12.3558100296643,
132.43091349999)) ;
#148393 = CARTESIAN_POINT('Ctrl Pts',(-15.2866992677918,12.5172181925544,
132.182267547668)) ;
#148394 = CARTESIAN_POINT('Ctrl Pts',(-15.2072741208272,12.7432705327431,
131.983342377859)) ;
#148395 = CARTESIAN_POINT('Ctrl Pts',(-15.1496737200748,13.0180147425716,
131.848185472719)) ;
#148396 = CARTESIAN_POINT('Ctrl Pts',(-15.117338984736,13.3228199509295,131.786946071819)) ;
#148397 = CARTESIAN_POINT('Ctrl Pts',(-15.1120300611744,13.6334362143055,
131.804503087611)) ;
#148398 = CARTESIAN_POINT('Ctrl Pts',(-15.133206576665,13.9294163259488,131.899479737668)) ;
#148399 = CARTESIAN_POINT('Ctrl Pts',(-15.1786478514763,14.18915702975,132.06532627885)) ;
#148400 = CARTESIAN_POINT('Ctrl Pts',(-15.2447211372006,14.3946402056162,
132.291578267309)) ;
#148401 = CARTESIAN_POINT('Ctrl Pts',(-15.3251751438084,14.5295568967571,
132.559617062532)) ;
#148402 = CARTESIAN_POINT('Ctrl Pts',(-15.4146594754138,14.5858061312981,
132.854298517614)) ;
#148403 = CARTESIAN_POINT('Ctrl Pts',(-15.5046539633587,14.5585141748975,
133.150186644236)) ;
#148404 = CARTESIAN_POINT('Ctrl Pts',(-15.5891258692447,14.4500372195652,
133.430097010254)) ;
#148405 = CARTESIAN_POINT('Ctrl Pts',(-15.6607651079543,14.268202021056,133.672458105674)) ;
#148406 = CARTESIAN_POINT('Ctrl Pts',(-15.7140410362885,14.0250734165881,
133.861293481273)) ;
#148407 = CARTESIAN_POINT('Ctrl Pts',(-15.7440399667486,13.7389393522913,
133.982084980378)) ;
#148408 = CARTESIAN_POINT('Ctrl Pts',(-15.7480042443892,13.4311037013635,
134.026729053662)) ;
#148409 = CARTESIAN_POINT('Ctrl Pts',(-15.725216194089,13.1229020286871,133.99318973845)) ;
#148410 = CARTESIAN_POINT('Ctrl Pts',(-15.6757479823679,12.8333723840705,
133.882056709305)) ;
#148411 = CARTESIAN_POINT('Ctrl Pts',(-15.6036828412038,12.5895126798869,
133.704489921503)) ;
#148412 = CARTESIAN_POINT('Ctrl Pts',(-15.5123148806256,12.4035405009807,
133.470777242786)) ;
#148413 = CARTESIAN_POINT('Ctrl Pts',(-15.4082687921079,12.2914040510789,
133.199889537963)) ;
#148414 = CARTESIAN_POINT('Ctrl Pts',(-15.2978395575661,12.2598122659222,
132.910395491718)) ;
#148415 = CARTESIAN_POINT('Ctrl Pts',(-15.1879820024828,12.3118570167027,
132.622666675303)) ;
#148416 = CARTESIAN_POINT('Ctrl Pts',(-15.0866174671626,12.4430958660728,
132.359601883501)) ;
#148417 = CARTESIAN_POINT('Ctrl Pts',(-14.9994898421019,12.6447072426792,
132.138218711282)) ;
#148418 = CARTESIAN_POINT('Ctrl Pts',(-14.9323676753914,12.9030426920416,
131.97536643828)) ;
#148419 = CARTESIAN_POINT('Ctrl Pts',(-14.889699513773,13.1970328957413,131.883755713314)) ;
#148420 = CARTESIAN_POINT('Ctrl Pts',(-14.8733792116843,13.5084312803207,
131.869259402362)) ;
#148421 = CARTESIAN_POINT('Ctrl Pts',(-14.8839158623484,13.8121187578149,
131.933031558723)) ;
#148422 = CARTESIAN_POINT('Ctrl Pts',(-14.9200803244134,14.0900961815241,
132.071930113077)) ;
#148423 = CARTESIAN_POINT('Ctrl Pts',(-14.9781162973069,14.318729906323,132.274505126265)) ;
#148424 = CARTESIAN_POINT('Ctrl Pts',(-15.0539330025022,14.4844226904234,
132.529278687657)) ;
#148425 = CARTESIAN_POINT('Ctrl Pts',(-15.1400286374453,14.5727758768623,
132.813733105511)) ;
#148426 = CARTESIAN_POINT('Ctrl Pts',(-15.2307985166822,14.5796460537581,
133.112046749388)) ;
#148427 = CARTESIAN_POINT('Ctrl Pts',(-15.3184170761058,14.5035865884274,
133.401102281981)) ;
#148428 = CARTESIAN_POINT('Ctrl Pts',(-15.3962623480525,14.3497063605797,
133.661718798962)) ;
#148429 = CARTESIAN_POINT('Ctrl Pts',(-15.4575770963959,14.1291330540675,
133.874017192935)) ;
#148430 = CARTESIAN_POINT('Ctrl Pts',(-15.4972251378502,13.8597727323871,
134.022812003589)) ;
#148431 = CARTESIAN_POINT('Ctrl Pts',(-15.5120947637313,13.5574624461298,
134.099434676898)) ;
#148432 = CARTESIAN_POINT('Ctrl Pts',(-15.5000961472788,13.2463366204199,
134.097469103472)) ;
#148433 = CARTESIAN_POINT('Ctrl Pts',(-15.4613504305426,12.9472974044437,
134.017442332404)) ;
#148434 = CARTESIAN_POINT('Ctrl Pts',(-15.3982335033183,12.6832078495132,
133.866092641497)) ;
#148435 = CARTESIAN_POINT('Ctrl Pts',(-15.3136235000347,12.4704982882043,
133.652221747533)) ;
#148436 = CARTESIAN_POINT('Ctrl Pts',(-15.214236945017,12.3276823498278,133.394894350722)) ;
#148437 = CARTESIAN_POINT('Ctrl Pts',(-15.1052928206969,12.2625925248945,
133.109808487118)) ;
#148438 = CARTESIAN_POINT('Ctrl Pts',(-14.9947038779737,12.2806192118825,
132.819787448895)) ;
#148439 = CARTESIAN_POINT('Ctrl Pts',(-14.8885598216415,12.3809214505585,
132.542973408766)) ;
#148440 = CARTESIAN_POINT('Ctrl Pts',(-14.7948852153021,12.5560400972574,
132.302471269315)) ;
#148441 = CARTESIAN_POINT('Ctrl Pts',(-14.7195025533567,12.7918901255773,
132.115247829854)) ;
#148442 = CARTESIAN_POINT('Ctrl Pts',(-14.6663732001335,13.0744209582552,
131.993234262889)) ;
#148443 = CARTESIAN_POINT('Ctrl Pts',(-14.6391629470329,13.3812416621058,
131.946846616762)) ;
#148444 = CARTESIAN_POINT('Ctrl Pts',(-14.6389300517192,13.6920797035989,
131.979379504455)) ;
#148445 = CARTESIAN_POINT('Ctrl Pts',(-14.6650391462422,13.9824941706661,
132.088747695719)) ;
#148446 = CARTESIAN_POINT('Ctrl Pts',(-14.7145031098689,14.2323227455577,
132.266232509409)) ;
#148447 = CARTESIAN_POINT('Ctrl Pts',(-14.7838483066136,14.4258243493526,
132.502056323187)) ;
#148448 = CARTESIAN_POINT('Ctrl Pts',(-14.866526759289,14.5465247232896,132.776639574897)) ;
#148449 = CARTESIAN_POINT('Ctrl Pts',(-14.9567274078562,14.5869806832562,
133.073382776381)) ;
#148450 = CARTESIAN_POINT('Ctrl Pts',(-15.0460438527412,14.5442058471831,
133.367252021219)) ;
#148451 = CARTESIAN_POINT('Ctrl Pts',(-15.1287759346931,14.4209679601538,
133.642135315366)) ;
#148452 = CARTESIAN_POINT('Ctrl Pts',(-15.1974643909208,14.2257906584797,
133.875970776234)) ;
#148453 = CARTESIAN_POINT('Ctrl Pts',(-15.2463765672829,13.9741287735189,
134.051901863982)) ;
#148454 = CARTESIAN_POINT('Ctrl Pts',(-15.2717007785664,13.6829512518686,
134.158957987928)) ;
#148455 = CARTESIAN_POINT('Ctrl Pts',(-15.2706427731617,13.3714665393579,
134.189124517144)) ;
#148456 = CARTESIAN_POINT('Ctrl Pts',(-15.2426215285773,13.0656058649526,
134.140315862993)) ;
#148457 = CARTESIAN_POINT('Ctrl Pts',(-15.1890339489811,12.7850334641615,
134.01684584536)) ;
#148458 = CARTESIAN_POINT('Ctrl Pts',(-15.1127899010191,12.5496673057456,
133.827241053212)) ;
#148459 = CARTESIAN_POINT('Ctrl Pts',(-15.0185001648777,12.3766688601944,
133.584981659701)) ;
#148460 = CARTESIAN_POINT('Ctrl Pts',(-14.912490210718,12.2789529253499,133.308438535154)) ;
#148461 = CARTESIAN_POINT('Ctrl Pts',(-14.8014556247031,12.2634413511376,
133.017242215912)) ;
#148462 = CARTESIAN_POINT('Ctrl Pts',(-14.6931943926143,12.330415688247,132.733981368436)) ;
#148463 = CARTESIAN_POINT('Ctrl Pts',(-14.5932657061769,12.4770343788681,
132.475395513356)) ;
#148464 = CARTESIAN_POINT('Ctrl Pts',(-14.5101133772823,12.6896430070817,
132.265442710562)) ;
#148465 = CARTESIAN_POINT('Ctrl Pts',(-14.4474157308921,12.9554491336733,
132.11540732339)) ;
#148466 = CARTESIAN_POINT('Ctrl Pts',(-14.4094541017876,13.2546655218149,
132.037609868002)) ;
#148467 = CARTESIAN_POINT('Ctrl Pts',(-14.3982126656332,13.5672374700513,
132.038011586952)) ;
#148468 = CARTESIAN_POINT('Ctrl Pts',(-14.4137840127669,13.8673527502542,
132.116509502837)) ;
#148469 = CARTESIAN_POINT('Ctrl Pts',(-14.4541638705567,14.1367235720608,
132.267567923076)) ;
#148470 = CARTESIAN_POINT('Ctrl Pts',(-14.5164519603104,14.3561276375805,
132.482861480637)) ;
#148471 = CARTESIAN_POINT('Ctrl Pts',(-14.5940341567091,14.5065131525026,
132.742424354294)) ;
#148472 = CARTESIAN_POINT('Ctrl Pts',(-14.6820502398555,14.58061768968,133.032736112524)) ;
#148473 = CARTESIAN_POINT('Ctrl Pts',(-14.772575059781,14.5715966995796,133.330239185716)) ;
#148474 = CARTESIAN_POINT('Ctrl Pts',(-14.8591820385415,14.4799160826423,
133.616486751543)) ;
#148475 = CARTESIAN_POINT('Ctrl Pts',(-14.9340155751519,14.3130126299592,
133.868154506662)) ;
#148476 = CARTESIAN_POINT('Ctrl Pts',(-14.991608157995,14.0821691922297,134.069528062715)) ;
#148477 = CARTESIAN_POINT('Ctrl Pts',(-15.0269433497899,13.8046645474474,
134.205816059215)) ;
#148478 = CARTESIAN_POINT('Ctrl Pts',(-15.0367628763332,13.4979411063597,
134.26777705295)) ;
#148479 = CARTESIAN_POINT('Ctrl Pts',(-15.0197321004595,13.1889484059184,
134.250957541032)) ;
#148480 = CARTESIAN_POINT('Ctrl Pts',(-14.9760933322257,12.8939178579835,
134.15672056437)) ;
#148481 = CARTESIAN_POINT('Ctrl Pts',(-14.9083892418113,12.637823938518,133.992078634426)) ;
#148482 = CARTESIAN_POINT('Ctrl Pts',(-14.8208560907062,12.4382802201008,
133.769479809402)) ;
#148483 = CARTESIAN_POINT('Ctrl Pts',(-14.7192841012341,12.3092349682175,
133.50577189094)) ;
#148484 = CARTESIAN_POINT('Ctrl Pts',(-14.6089364049052,12.2595575247746,
133.216721659976)) ;
#148485 = CARTESIAN_POINT('Ctrl Pts',(-14.4990459288312,12.2934341304884,
132.928661167576)) ;
#148486 = CARTESIAN_POINT('Ctrl Pts',(-14.3949781008443,12.4080333824313,
132.657808436135)) ;
#148487 = CARTESIAN_POINT('Ctrl Pts',(-14.3040123177586,12.5960960423707,
132.425286386828)) ;
#148488 = CARTESIAN_POINT('Ctrl Pts',(-14.2323706381693,12.8430835958632,
132.249132507019)) ;
#148489 = CARTESIAN_POINT('Ctrl Pts',(-14.1842155266943,13.1299282675871,
132.14141612179)) ;
#148490 = CARTESIAN_POINT('Ctrl Pts',(-14.1618825011132,13.4413370820985,
132.109530327437)) ;
#148491 = CARTESIAN_POINT('Ctrl Pts',(-14.1667760289367,13.7480777778484,
132.156806610371)) ;
#148492 = CARTESIAN_POINT('Ctrl Pts',(-14.1974678546853,14.0327532847483,
132.279580684498)) ;
#148493 = CARTESIAN_POINT('Ctrl Pts',(-14.2510444053685,14.2736050816731,
132.469152013831)) ;
#148494 = CARTESIAN_POINT('Ctrl Pts',(-14.323668194567,14.454731415087,132.714635917315)) ;
#148495 = CARTESIAN_POINT('Ctrl Pts',(-14.4079059599784,14.5602675657722,
132.99365390726)) ;
#148496 = CARTESIAN_POINT('Ctrl Pts',(-14.4985138900094,14.5853381818847,
133.291544672069)) ;
#148497 = CARTESIAN_POINT('Ctrl Pts',(-14.5874144035252,14.5268296040502,
133.584352082136)) ;
#148498 = CARTESIAN_POINT('Ctrl Pts',(-14.6678119138476,14.3893357844739,
133.852346334359)) ;
#148499 = CARTESIAN_POINT('Ctrl Pts',(-14.7331376309536,14.1825587222419,
134.076310009883)) ;
#148500 = CARTESIAN_POINT('Ctrl Pts',(-14.7780213031554,13.9213688559687,
134.240558829846)) ;
#148501 = CARTESIAN_POINT('Ctrl Pts',(-14.7984215319615,13.6242448062503,
134.333308668138)) ;
#148502 = CARTESIAN_POINT('Ctrl Pts',(-14.7924127716866,13.3143404196874,
134.348729861162)) ;
#148503 = CARTESIAN_POINT('Ctrl Pts',(-14.7590472201161,13.0084390891239,
134.28467058425)) ;
#148504 = CARTESIAN_POINT('Ctrl Pts',(-14.7012646791225,12.7371909250803,
134.148690857043)) ;
#148505 = CARTESIAN_POINT('Ctrl Pts',(-14.6209599760378,12.5114338285413,
133.947367407138)) ;
#148506 = CARTESIAN_POINT('Ctrl Pts',(-14.5242191003668,12.3524149668545,
133.697838780998)) ;
#148507 = CARTESIAN_POINT('Ctrl Pts',(-14.4166271811855,12.2696328079286,
133.416714729971)) ;
#148508 = CARTESIAN_POINT('Ctrl Pts',(-14.3056942095112,12.2697667262583,
133.125742805927)) ;
#148509 = CARTESIAN_POINT('Ctrl Pts',(-14.1983796924837,12.352219690353,132.845338479333)) ;
#148510 = CARTESIAN_POINT('Ctrl Pts',(-14.1014667534168,12.5116177208884,
132.595377130338)) ;
#148511 = CARTESIAN_POINT('Ctrl Pts',(-14.0214433689727,12.7360826900141,
132.39471532807)) ;
#148512 = CARTESIAN_POINT('Ctrl Pts',(-13.9630322762884,13.0105746787141,
132.257287201062)) ;
#148513 = CARTESIAN_POINT('Ctrl Pts',(-13.9300917396253,13.3146278251872,
132.194246081439)) ;
#148514 = CARTESIAN_POINT('Ctrl Pts',(-13.9240153938967,13.6243831521928,
132.209458290046)) ;
#148515 = CARTESIAN_POINT('Ctrl Pts',(-13.944508427021,13.9217978,132.302518124968)) ;
#148516 = CARTESIAN_POINT('Ctrl Pts',(-13.9892221339268,14.1821018146301,
132.466153950012)) ;
#148517 = CARTESIAN_POINT('Ctrl Pts',(-14.0546602899526,14.389412327527,132.690519984618)) ;
#148518 = CARTESIAN_POINT('Ctrl Pts',(-14.1350488271771,14.5268848285114,
132.958477718458)) ;
#148519 = CARTESIAN_POINT('Ctrl Pts',(-14.2240994741948,14.5852561648766,
133.251782240412)) ;
#148520 = CARTESIAN_POINT('Ctrl Pts',(-14.3142069860548,14.5605921402289,
133.548016849623)) ;
#148521 = CARTESIAN_POINT('Ctrl Pts',(-14.3990505698622,14.4542388550499,
133.829054466345)) ;
#148522 = CARTESIAN_POINT('Ctrl Pts',(-14.4711893889587,14.2743936343232,
134.072880951258)) ;
#148523 = CARTESIAN_POINT('Ctrl Pts',(-14.5251681508735,14.0316377250169,
134.263898633615)) ;
#148524 = CARTESIAN_POINT('Ctrl Pts',(-14.5556789963755,13.7487556151288,
134.38591936868)) ;
#148525 = CARTESIAN_POINT('Ctrl Pts',(-14.5604714220069,13.4387761363986,
134.433258068243)) ;
#148526 = CARTESIAN_POINT('Ctrl Pts',(-14.5384491661002,13.1317846555727,
134.401792713465)) ;
#148527 = CARTESIAN_POINT('Ctrl Pts',(-14.4896993568433,12.8410201879509,
134.292793596079)) ;
#148528 = CARTESIAN_POINT('Ctrl Pts',(-14.418425254601,12.5963885995688,134.117448315784)) ;
#148529 = CARTESIAN_POINT('Ctrl Pts',(-14.3277290025618,12.4083250165559,
133.885656271006)) ;
#148530 = CARTESIAN_POINT('Ctrl Pts',(-14.2232683046687,12.2932606232103,
133.613777294112)) ;
#148531 = CARTESIAN_POINT('Ctrl Pts',(-14.1134438296,12.2596773192959,133.325888983821)) ;
#148532 = CARTESIAN_POINT('Ctrl Pts',(-14.0035198626591,12.3089369828892,
133.037945712624)) ;
#148533 = CARTESIAN_POINT('Ctrl Pts',(-13.9014057493695,12.4384179061081,
132.772818300622)) ;
#148534 = CARTESIAN_POINT('Ctrl Pts',(-13.8137301697272,12.6389284410988,
132.549896696867)) ;
#148535 = CARTESIAN_POINT('Ctrl Pts',(-13.7464647647404,12.893636868565,132.386346900933)) ;
#148536 = CARTESIAN_POINT('Ctrl Pts',(-13.7026544223093,13.1890353043008,
132.291660086028)) ;
#148537 = CARTESIAN_POINT('Ctrl Pts',(-13.6856968381069,13.4997523656822,
132.275235904602)) ;
#148538 = CARTESIAN_POINT('Ctrl Pts',(-13.6955051304073,13.8039808891053,
132.336895895886)) ;
#148539 = CARTESIAN_POINT('Ctrl Pts',(-13.730811067449,14.0820721620834,132.473158857497)) ;
#148540 = CARTESIAN_POINT('Ctrl Pts',(-13.7884136291909,14.3130040763869,
132.6745633012)) ;
#148541 = CARTESIAN_POINT('Ctrl Pts',(-13.8634361976948,14.4800545179009,
132.926857790848)) ;
#148542 = CARTESIAN_POINT('Ctrl Pts',(-13.9495289714166,14.5714591887958,
133.211406715331)) ;
#148543 = CARTESIAN_POINT('Ctrl Pts',(-14.0407314511908,14.5804983866051,
133.511146111532)) ;
#148544 = CARTESIAN_POINT('Ctrl Pts',(-14.1280999903725,14.5069052438345,
133.799313871286)) ;
#148545 = CARTESIAN_POINT('Ctrl Pts',(-14.2062273655573,14.3557029930728,
134.060693196223)) ;
#148546 = CARTESIAN_POINT('Ctrl Pts',(-14.2682168904107,14.1367619821381,
134.275000427421)) ;
#148547 = CARTESIAN_POINT('Ctrl Pts',(-14.308672097508,13.868069374817,134.426223663583)) ;
#148548 = CARTESIAN_POINT('Ctrl Pts',(-14.3242464980369,13.5652242868234,
134.505022827762)) ;
#148549 = CARTESIAN_POINT('Ctrl Pts',(-14.3130481928678,13.2558696695954,
134.505203310138)) ;
#148550 = CARTESIAN_POINT('Ctrl Pts',(-14.2751188260239,12.9557646560496,
134.427595170396)) ;
#148551 = CARTESIAN_POINT('Ctrl Pts',(-14.2125011050347,12.6900042149153,
134.277767151928)) ;
#148552 = CARTESIAN_POINT('Ctrl Pts',(-14.1287473937729,12.4761055498728,
134.066283383056)) ;
#148553 = CARTESIAN_POINT('Ctrl Pts',(-14.0292043456581,12.3304586673531,
133.808672602781)) ;
#148554 = CARTESIAN_POINT('Ctrl Pts',(-13.9209454355513,12.2634381617438,
133.525424392877)) ;
#148555 = CARTESIAN_POINT('Ctrl Pts',(-13.8100698210139,12.278878358219,133.234640878502)) ;
#148556 = CARTESIAN_POINT('Ctrl Pts',(-13.7038111973288,12.3768659810513,
132.957453506269)) ;
#148557 = CARTESIAN_POINT('Ctrl Pts',(-13.6097056948675,12.5495630151977,
132.715665736416)) ;
#148558 = CARTESIAN_POINT('Ctrl Pts',(-13.5332893897392,12.7855771404834,
132.525644949222)) ;
#148559 = CARTESIAN_POINT('Ctrl Pts',(-13.4798638510241,13.0654345066809,
132.402557075124)) ;
#148560 = CARTESIAN_POINT('Ctrl Pts',(-13.4517888390726,13.3720089206918,
132.353670494908)) ;
#148561 = CARTESIAN_POINT('Ctrl Pts',(-13.4507696207002,13.682435682329,132.383838975626)) ;
#148562 = CARTESIAN_POINT('Ctrl Pts',(-13.4759925925544,13.9739144742565,
132.490615522146)) ;
#148563 = CARTESIAN_POINT('Ctrl Pts',(-13.5252998059987,14.2268633708939,
132.667901525746)) ;
#148564 = CARTESIAN_POINT('Ctrl Pts',(-13.5934844266385,14.4204385553042,
132.900007436279)) ;
#148565 = CARTESIAN_POINT('Ctrl Pts',(-13.6765840975396,14.5445800987763,
133.176129149791)) ;
#148566 = CARTESIAN_POINT('Ctrl Pts',(-13.7660933005895,14.5868220518321,
133.470623338263)) ;
#148567 = CARTESIAN_POINT('Ctrl Pts',(-13.8556826458728,14.5468039105965,
133.765349744584)) ;
#148568 = CARTESIAN_POINT('Ctrl Pts',(-13.9389917331868,14.4251034051228,
134.042036110926)) ;
#148569 = CARTESIAN_POINT('Ctrl Pts',(-14.0078406882011,14.2325286580178,
134.276201287599)) ;
#148570 = CARTESIAN_POINT('Ctrl Pts',(-14.0575163353173,13.9823226151408,
134.454383889325)) ;
#148571 = CARTESIAN_POINT('Ctrl Pts',(-14.0836025549971,13.6900857770298,
134.563868974634)) ;
#148572 = CARTESIAN_POINT('Ctrl Pts',(-14.0832571069024,13.3811330160851,
134.595866332321)) ;
#148573 = CARTESIAN_POINT('Ctrl Pts',(-14.0560489819167,13.0742212220075,
134.549500292957)) ;
#148574 = CARTESIAN_POINT('Ctrl Pts',(-14.0030629387518,12.7922256015956,
134.427832814541)) ;
#148575 = CARTESIAN_POINT('Ctrl Pts',(-13.9271733129843,12.5548594273492,
134.239343872288)) ;
#148576 = CARTESIAN_POINT('Ctrl Pts',(-13.8333753451746,12.3804086470547,
133.99847615794)) ;
#148577 = CARTESIAN_POINT('Ctrl Pts',(-13.7281102029634,12.2809059803651,
133.723956716157)) ;
#148578 = CARTESIAN_POINT('Ctrl Pts',(-13.617241740478,12.2624888492441,133.433207556077)) ;
#148579 = CARTESIAN_POINT('Ctrl Pts',(-13.5081833508386,12.3276777056696,
133.147817955966)) ;
#148580 = CARTESIAN_POINT('Ctrl Pts',(-13.4087400939355,12.4707929028479,
132.890358316802)) ;
#148581 = CARTESIAN_POINT('Ctrl Pts',(-13.3244896145502,12.6823314150819,
132.677374748484)) ;
#148582 = CARTESIAN_POINT('Ctrl Pts',(-13.2609830005564,12.9478031848441,
132.525073234737)) ;
#148583 = CARTESIAN_POINT('Ctrl Pts',(-13.2223270064774,13.2466923660168,
132.445278275813)) ;
#148584 = CARTESIAN_POINT('Ctrl Pts',(-13.2103951472699,13.5583772827196,
132.44357445534)) ;
#148585 = CARTESIAN_POINT('Ctrl Pts',(-13.2251602999981,13.8592556728242,
132.519724504582)) ;
#148586 = CARTESIAN_POINT('Ctrl Pts',(-13.2651772105284,14.1306425332548,
132.669863094874)) ;
#148587 = CARTESIAN_POINT('Ctrl Pts',(-13.3261568835758,14.3493759860233,
132.880945200703)) ;
#148588 = CARTESIAN_POINT('Ctrl Pts',(-13.4039531667767,14.5035317541652,
133.141424580497)) ;
#148589 = CARTESIAN_POINT('Ctrl Pts',(-13.4916134539024,14.5795845052791,
133.430615618163)) ;
#148590 = CARTESIAN_POINT('Ctrl Pts',(-13.5823374167532,14.5729335586883,
133.72877440133)) ;
#148591 = CARTESIAN_POINT('Ctrl Pts',(-13.6688628859832,14.4838964903463,
134.014660525185)) ;
#148592 = CARTESIAN_POINT('Ctrl Pts',(-13.7443181729218,14.3187457579905,
134.268228770671)) ;
#148593 = CARTESIAN_POINT('Ctrl Pts',(-13.8024060188236,14.0897675929633,
134.471006232896)) ;
#148594 = CARTESIAN_POINT('Ctrl Pts',(-13.8384578759884,13.8134082777409,
134.609389817387)) ;
#148595 = CARTESIAN_POINT('Ctrl Pts',(-13.8490872441391,13.5073936360873,
134.673692916445)) ;
#148596 = CARTESIAN_POINT('Ctrl Pts',(-13.832792152632,13.1976577168155,134.659088373623)) ;
#148597 = CARTESIAN_POINT('Ctrl Pts',(-13.7900624981885,12.9027229695694,
134.567399873167)) ;
#148598 = CARTESIAN_POINT('Ctrl Pts',(-13.7229404114228,12.6448108497487,
134.404513164289)) ;
#148599 = CARTESIAN_POINT('Ctrl Pts',(-13.6361336422572,12.4434495713625,
134.183973342917)) ;
#148600 = CARTESIAN_POINT('Ctrl Pts',(-13.5339224602791,12.311375978469,133.918704188154)) ;
#148601 = CARTESIAN_POINT('Ctrl Pts',(-13.4248925033934,12.2599503304442,
133.633135101603)) ;
#148602 = CARTESIAN_POINT('Ctrl Pts',(-13.3140399354172,12.2913693228783,
133.342532189384)) ;
#148603 = CARTESIAN_POINT('Ctrl Pts',(-13.2100079542354,12.4038516035479,
133.071692026905)) ;
#148604 = CARTESIAN_POINT('Ctrl Pts',(-13.1188399743127,12.5892626487071,
132.838480990112)) ;
#148605 = CARTESIAN_POINT('Ctrl Pts',(-13.0465008697508,12.8342966709516,
132.660260589203)) ;
#148606 = CARTESIAN_POINT('Ctrl Pts',(-12.9973391164619,13.122430567382,132.549852233358)) ;
#148607 = CARTESIAN_POINT('Ctrl Pts',(-12.9744365714638,13.4307504322514,
132.515998075404)) ;
#148608 = CARTESIAN_POINT('Ctrl Pts',(-12.9784369626985,13.7394115392885,
132.560834284604)) ;
#148609 = CARTESIAN_POINT('Ctrl Pts',(-13.0084496645794,14.0250582517609,
132.681620776933)) ;
#148610 = CARTESIAN_POINT('Ctrl Pts',(-13.0615307919976,14.2676857548662,
132.869798935733)) ;
#148611 = CARTESIAN_POINT('Ctrl Pts',(-13.1333688217039,14.4501343766899,
133.112842532531)) ;
#148612 = CARTESIAN_POINT('Ctrl Pts',(-13.2177622418928,14.5585281665325,
133.392488045436)) ;
#148613 = CARTESIAN_POINT('Ctrl Pts',(-13.3080577151419,14.5857500272389,
133.689369213566)) ;
#148614 = CARTESIAN_POINT('Ctrl Pts',(-13.3972502622619,14.5296138269876,
133.983085307506)) ;
#148615 = CARTESIAN_POINT('Ctrl Pts',(-13.4779778486236,14.3940563657681,
134.252050444746)) ;
#148616 = CARTESIAN_POINT('Ctrl Pts',(-13.5436430073141,14.1896706330216,
134.476915598335)) ;
#148617 = CARTESIAN_POINT('Ctrl Pts',(-13.5892678630379,13.9296795635546,
134.643358940888)) ;
#148618 = CARTESIAN_POINT('Ctrl Pts',(-13.6104505119164,13.6325613783442,
134.738470798441)) ;
#148619 = CARTESIAN_POINT('Ctrl Pts',(-13.6050981772493,13.3229079884786,
134.755797277682)) ;
#148620 = CARTESIAN_POINT('Ctrl Pts',(-13.5728485012099,13.018526691074,134.694761651048)) ;
#148621 = CARTESIAN_POINT('Ctrl Pts',(-13.5153450492774,12.7436673997071,
134.559879447056)) ;
#148622 = CARTESIAN_POINT('Ctrl Pts',(-13.4354311899252,12.5164978954953,
134.359712961926)) ;
#148623 = CARTESIAN_POINT('Ctrl Pts',(-13.3394512830422,12.3560840259889,
134.112282954591)) ;
#148624 = CARTESIAN_POINT('Ctrl Pts',(-13.2320535007894,12.2708854791944,
133.831733816191)) ;
#148625 = CARTESIAN_POINT('Ctrl Pts',(-13.1212646835022,12.2685612121641,
133.541141487823)) ;
#148626 = CARTESIAN_POINT('Ctrl Pts',(-13.0135487693522,12.3486009748257,
133.259616351496)) ;
#148627 = CARTESIAN_POINT('Ctrl Pts',(-12.9158794229883,12.5069430780995,
133.007592004978)) ;
#148628 = CARTESIAN_POINT('Ctrl Pts',(-12.8358284635978,12.7284059514765,
132.806638042446)) ;
#148629 = CARTESIAN_POINT('Ctrl Pts',(-12.7765201702019,13.0024845577893,
132.666692915585)) ;
#148630 = CARTESIAN_POINT('Ctrl Pts',(-12.7429090658184,13.3053156304276,
132.601612497695)) ;
#148631 = CARTESIAN_POINT('Ctrl Pts',(-12.7360481621408,13.6156286955051,
132.614589792664)) ;
#148632 = CARTESIAN_POINT('Ctrl Pts',(-12.7556608206096,13.9128849931579,
132.70496583945)) ;
#148633 = CARTESIAN_POINT('Ctrl Pts',(-12.8001013006508,14.1766185287715,
132.868078846721)) ;
#148634 = CARTESIAN_POINT('Ctrl Pts',(-12.8649833652883,14.3847398624139,
133.090730630613)) ;
#148635 = CARTESIAN_POINT('Ctrl Pts',(-12.9447362290285,14.5238361005913,
133.356717863807)) ;
#148636 = CARTESIAN_POINT('Ctrl Pts',(-13.0335166994612,14.5847743012247,
133.649190179549)) ;
#148637 = CARTESIAN_POINT('Ctrl Pts',(-13.1240492119926,14.5623309410939,
133.94680621714)) ;
#148638 = CARTESIAN_POINT('Ctrl Pts',(-13.2090287290572,14.4584178167976,
134.228179442432)) ;
#148639 = CARTESIAN_POINT('Ctrl Pts',(-13.281862210307,14.2791868777477,134.474211904493)) ;
#148640 = CARTESIAN_POINT('Ctrl Pts',(-13.335773103936,14.0415187113142,134.664557550494)) ;
#148641 = CARTESIAN_POINT('Ctrl Pts',(-13.3674362011174,13.7564325349983,
134.790345370979)) ;
#148642 = CARTESIAN_POINT('Ctrl Pts',(-13.3729735926156,13.4495648560064,
134.839547729474)) ;
#148643 = CARTESIAN_POINT('Ctrl Pts',(-13.3515432167407,13.1394167838631,
134.810135087209)) ;
#148644 = CARTESIAN_POINT('Ctrl Pts',(-13.3040714645819,12.8508801265976,
134.704494636628)) ;
#148645 = CARTESIAN_POINT('Ctrl Pts',(-13.2329202360563,12.6022770159485,
134.529809745286)) ;
#148646 = CARTESIAN_POINT('Ctrl Pts',(-13.1427212865503,12.4127865779696,
134.299427661665)) ;
#148647 = CARTESIAN_POINT('Ctrl Pts',(-13.0385956707939,12.2953916612225,
134.02852190621)) ;
#148648 = CARTESIAN_POINT('Ctrl Pts',(-12.9286172414397,12.2594835082488,
133.740252210268)) ;
#148649 = CARTESIAN_POINT('Ctrl Pts',(-12.8187965411872,12.3065006906036,
133.452548911367)) ;
#148650 = CARTESIAN_POINT('Ctrl Pts',(-12.7166251696081,12.4331949897075,
133.187157237466)) ;
#148651 = CARTESIAN_POINT('Ctrl Pts',(-12.6281176238896,12.6325251060339,
132.961927723459)) ;
#148652 = CARTESIAN_POINT('Ctrl Pts',(-12.5603551331913,12.8854153923965,
132.796860075738)) ;
#148653 = CARTESIAN_POINT('Ctrl Pts',(-12.5157669611184,13.1803566705807,
132.699944434962)) ;
#148654 = CARTESIAN_POINT('Ctrl Pts',(-12.498052923534,13.4893561125358,132.681144837552)) ;
#148655 = CARTESIAN_POINT('Ctrl Pts',(-12.5070166131313,13.7954470549273,
132.740482079854)) ;
#148656 = CARTESIAN_POINT('Ctrl Pts',(-12.5417818886109,14.0751705086754,
132.875240680629)) ;
#148657 = CARTESIAN_POINT('Ctrl Pts',(-12.5986620801991,14.3069080353192,
133.074438327252)) ;
#148658 = CARTESIAN_POINT('Ctrl Pts',(-12.673160327911,14.4762412985565,133.325179922949)) ;
#148659 = CARTESIAN_POINT('Ctrl Pts',(-12.7597351258917,14.5702449672957,
133.611399754379)) ;
#148660 = CARTESIAN_POINT('Ctrl Pts',(-12.8500625826259,14.5813885693018,
133.908266863094)) ;
#148661 = CARTESIAN_POINT('Ctrl Pts',(-12.9380952103393,14.5100796907114,
134.198552121671)) ;
#148662 = CARTESIAN_POINT('Ctrl Pts',(-13.0166943404508,14.3602445312062,
134.461375238824)) ;
#148663 = CARTESIAN_POINT('Ctrl Pts',(-13.079025585699,14.143253231573,134.676613684199)) ;
#148664 = CARTESIAN_POINT('Ctrl Pts',(-13.1199829894282,13.8766590298569,
134.82919236409)) ;
#148665 = CARTESIAN_POINT('Ctrl Pts',(-13.1363842764657,13.575471217549,134.910304171519)) ;
#148666 = CARTESIAN_POINT('Ctrl Pts',(-13.1259906023331,13.2645668941717,
134.912996918485)) ;
#148667 = CARTESIAN_POINT('Ctrl Pts',(-13.0886655812232,12.9634277851347,
134.837203216762)) ;
#148668 = CARTESIAN_POINT('Ctrl Pts',(-13.0268727262915,12.6972349094739,
134.689690166995)) ;
#148669 = CARTESIAN_POINT('Ctrl Pts',(-12.9437794235418,12.4817230619034,
134.480101250047)) ;
#148670 = CARTESIAN_POINT('Ctrl Pts',(-12.8446953032213,12.3338051971936,
134.223812059553)) ;
#148671 = CARTESIAN_POINT('Ctrl Pts',(-12.736264841077,12.2641456022445,133.940168303419)) ;
#148672 = CARTESIAN_POINT('Ctrl Pts',(-12.6254315941907,12.2773535712523,
133.649486560175)) ;
#148673 = CARTESIAN_POINT('Ctrl Pts',(-12.519180488884,12.3726334671979,133.372237189562)) ;
#148674 = CARTESIAN_POINT('Ctrl Pts',(-12.424500141051,12.5434758401697,133.128817984578)) ;
#148675 = CARTESIAN_POINT('Ctrl Pts',(-12.3476880051171,12.7769497642035,
132.937528466358)) ;
#148676 = CARTESIAN_POINT('Ctrl Pts',(-12.2932283996367,13.0568799766939,
132.811568392158)) ;
#148677 = CARTESIAN_POINT('Ctrl Pts',(-12.2644164115581,13.3636449455261,
132.760589242832)) ;
#148678 = CARTESIAN_POINT('Ctrl Pts',(-12.2626515312786,13.6733774469028,
132.788485456325)) ;
#148679 = CARTESIAN_POINT('Ctrl Pts',(-12.287057255896,13.9654380896254,132.892840457169)) ;
#148680 = CARTESIAN_POINT('Ctrl Pts',(-12.3357556053458,14.220301269476,133.06839566665)) ;
#148681 = CARTESIAN_POINT('Ctrl Pts',(-12.4036363026361,14.415947045335,133.299682560496)) ;
#148682 = CARTESIAN_POINT('Ctrl Pts',(-12.4858983405842,14.5416943673476,
133.573153971909)) ;
#148683 = CARTESIAN_POINT('Ctrl Pts',(-12.5756511466147,14.586901890039,133.868497858328)) ;
#148684 = CARTESIAN_POINT('Ctrl Pts',(-12.6654696558363,14.5489491303822,
134.163944585503)) ;
#148685 = CARTESIAN_POINT('Ctrl Pts',(-12.7488004609279,14.4300240451422,
134.44057679707)) ;
#148686 = CARTESIAN_POINT('Ctrl Pts',(-12.8184183179855,14.2387296185005,
134.677112327015)) ;
#148687 = CARTESIAN_POINT('Ctrl Pts',(-12.8686018078536,13.9899469010905,
134.856754873464)) ;
#148688 = CARTESIAN_POINT('Ctrl Pts',(-12.8953390018291,13.7002922366985,
134.967959281547)) ;
#148689 = CARTESIAN_POINT('Ctrl Pts',(-12.8959448004099,13.3909003145637,
135.00281288959)) ;
#148690 = CARTESIAN_POINT('Ctrl Pts',(-12.8693187261974,13.0819914408663,
134.95831995508)) ;
#148691 = CARTESIAN_POINT('Ctrl Pts',(-12.8171517429198,12.8000707339927,
134.838929642487)) ;
#148692 = CARTESIAN_POINT('Ctrl Pts',(-12.7421374292196,12.5616134870626,
134.652909850917)) ;
#148693 = CARTESIAN_POINT('Ctrl Pts',(-12.6486214543391,12.384449895012,134.412941328436)) ;
#148694 = CARTESIAN_POINT('Ctrl Pts',(-12.5430733333332,12.2824628240901,
134.137754600261)) ;
#148695 = CARTESIAN_POINT('Ctrl Pts',(-12.4328336844289,12.2618989594336,
133.848666595403)) ;
#148696 = CARTESIAN_POINT('Ctrl Pts',(-12.3234764644886,12.3245801439636,
133.562445071246)) ;
#148697 = CARTESIAN_POINT('Ctrl Pts',(-12.2236702142189,12.4655889841413,
133.303925046023)) ;
#148698 = CARTESIAN_POINT('Ctrl Pts',(-12.1389072399167,12.6753258327154,
133.089442344447)) ;
#148699 = CARTESIAN_POINT('Ctrl Pts',(-12.0747933877151,12.9389695306945,
132.935307440174)) ;
#148700 = CARTESIAN_POINT('Ctrl Pts',(-12.0353186182838,13.2377441429055,
132.853189559189)) ;
#148701 = CARTESIAN_POINT('Ctrl Pts',(-12.0225559627654,13.5478077720715,
132.848886973666)) ;
#148702 = CARTESIAN_POINT('Ctrl Pts',(-12.0366139208027,13.8515135114459,
132.923217350704)) ;
#148703 = CARTESIAN_POINT('Ctrl Pts',(-12.0758678831878,14.1231097110526,
133.07101037297)) ;
#148704 = CARTESIAN_POINT('Ctrl Pts',(-12.1363738971983,14.3439546593352,
133.280769121662)) ;
#148705 = CARTESIAN_POINT('Ctrl Pts',(-12.2135714078888,14.4998916999394,
133.539410393626)) ;
#148706 = CARTESIAN_POINT('Ctrl Pts',(-12.3013318130591,14.5786386436238,
133.82901150719)) ;
#148707 = CARTESIAN_POINT('Ctrl Pts',(-12.3920181749816,14.5742675055765,
134.127037321131)) ;
#148708 = CARTESIAN_POINT('Ctrl Pts',(-12.4788244044002,14.4873447057953,
134.413774862475)) ;
#148709 = CARTESIAN_POINT('Ctrl Pts',(-12.5544418663992,14.324791387065,134.667707059656)) ;
#148710 = CARTESIAN_POINT('Ctrl Pts',(-12.6133095637089,14.0970302215938,
134.872846143443)) ;
#148711 = CARTESIAN_POINT('Ctrl Pts',(-12.6500777852611,13.8204923791666,
135.013454137909)) ;
#148712 = CARTESIAN_POINT('Ctrl Pts',(-12.6613488618547,13.5164549549645,
135.07946573627)) ;
#148713 = CARTESIAN_POINT('Ctrl Pts',(-12.6458306906024,13.2060699844781,
135.067187910305)) ;
#148714 = CARTESIAN_POINT('Ctrl Pts',(-12.6037641136263,12.9102232608784,
134.977454778982)) ;
#148715 = CARTESIAN_POINT('Ctrl Pts',(-12.5371192356222,12.6507291621381,
134.816011366745)) ;
#148716 = CARTESIAN_POINT('Ctrl Pts',(-12.4510895491266,12.4485585677655,
134.597616648301)) ;
#148717 = CARTESIAN_POINT('Ctrl Pts',(-12.349770741895,12.3145373825205,134.334792426212)) ;
#148718 = CARTESIAN_POINT('Ctrl Pts',(-12.2402433163891,12.2601564012495,
134.047965097519)) ;
#148719 = CARTESIAN_POINT('Ctrl Pts',(-12.1293526644653,12.2893926145907,
133.757240402094)) ;
#148720 = CARTESIAN_POINT('Ctrl Pts',(-12.0250639181401,12.3994366582283,
133.485636610226)) ;
#148721 = CARTESIAN_POINT('Ctrl Pts',(-11.9330778249773,12.5839727611718,
133.250184991413)) ;
#148722 = CARTESIAN_POINT('Ctrl Pts',(-11.8605383338059,12.8264919442356,
133.071221263827)) ;
#148723 = CARTESIAN_POINT('Ctrl Pts',(-11.8105329668041,13.1141227557289,
132.958401040611)) ;
#148724 = CARTESIAN_POINT('Ctrl Pts',(-11.7948211693083,13.3194869799383,
132.934542691027)) ;
#148725 = CARTESIAN_POINT('Ctrl Pts',(-11.7914080085508,13.4222384087837,
132.935592717388)) ;
#148726 = CARTESIAN_POINT('Ctrl Pts',(-33.372552283912,13.1368456608817,127.94074177726)) ;
#148727 = CARTESIAN_POINT('Ctrl Pts',(-33.3717780316138,13.1302434100695,
127.939210950719)) ;
#148728 = CARTESIAN_POINT('Ctrl Pts',(-33.3591440063766,13.0249711622575,
127.91398623386)) ;
#148729 = CARTESIAN_POINT('Ctrl Pts',(-33.3246270598641,12.8263018173041,
127.836128436635)) ;
#148730 = CARTESIAN_POINT('Ctrl Pts',(-33.2518258931156,12.5833995397257,
127.656480341887)) ;
#148731 = CARTESIAN_POINT('Ctrl Pts',(-33.1602821282434,12.3996267675037,
127.42216387292)) ;
#148732 = CARTESIAN_POINT('Ctrl Pts',(-33.0552813371174,12.2890731746127,
127.148703526175)) ;
#148733 = CARTESIAN_POINT('Ctrl Pts',(-32.9453207624895,12.2602312933653,
126.860410133392)) ;
#148734 = CARTESIAN_POINT('Ctrl Pts',(-32.8354844413288,12.3144254327404,
126.5727765393)) ;
#148735 = CARTESIAN_POINT('Ctrl Pts',(-32.7343044732474,12.4480642485612,
126.310296325994)) ;
#148736 = CARTESIAN_POINT('Ctrl Pts',(-32.647713423827,12.6516399128533,126.090485649053)) ;
#148737 = CARTESIAN_POINT('Ctrl Pts',(-32.5814045317866,12.9104451953934,
125.929904053096)) ;
#148738 = CARTESIAN_POINT('Ctrl Pts',(-32.539361864737,13.2058491339696,125.840200965284)) ;
#148739 = CARTESIAN_POINT('Ctrl Pts',(-32.5237679482684,13.5166184158111,
125.827737740167)) ;
#148740 = CARTESIAN_POINT('Ctrl Pts',(-32.5352548048312,13.822409942281,125.89458343385)) ;
#148741 = CARTESIAN_POINT('Ctrl Pts',(-32.5718813221576,14.0967864271645,
126.034540409285)) ;
#148742 = CARTESIAN_POINT('Ctrl Pts',(-32.6305856565637,14.3244562376795,
126.239159768777)) ;
#148743 = CARTESIAN_POINT('Ctrl Pts',(-32.7063816647152,14.4874741588536,
126.493693734194)) ;
#148744 = CARTESIAN_POINT('Ctrl Pts',(-32.7933567848837,14.5744204782189,
126.78098226786)) ;
#148745 = CARTESIAN_POINT('Ctrl Pts',(-32.8840723683445,14.5784621865543,
127.079105132271)) ;
#148746 = CARTESIAN_POINT('Ctrl Pts',(-32.9714000447983,14.5000470189108,
127.367281428271)) ;
#148747 = CARTESIAN_POINT('Ctrl Pts',(-33.0485978146599,14.3445727913024,
127.625899065993)) ;
#148748 = CARTESIAN_POINT('Ctrl Pts',(-33.1094227295156,14.1228339214572,
127.836735242549)) ;
#148749 = CARTESIAN_POINT('Ctrl Pts',(-33.1486346997481,13.850151796375,127.9845077735)) ;
#148750 = CARTESIAN_POINT('Ctrl Pts',(-33.1625834468356,13.5490424798657,
128.058234479633)) ;
#148751 = CARTESIAN_POINT('Ctrl Pts',(-33.1498770654012,13.2374718016147,
128.054257906591)) ;
#148752 = CARTESIAN_POINT('Ctrl Pts',(-33.110281108,12.9386845516003,127.971796151102)) ;
#148753 = CARTESIAN_POINT('Ctrl Pts',(-33.0464969729853,12.6761377912153,
127.818477928809)) ;
#148754 = CARTESIAN_POINT('Ctrl Pts',(-32.9616310346417,12.4657587239521,
127.603760965913)) ;
#148755 = CARTESIAN_POINT('Ctrl Pts',(-32.8617323746109,12.3246285907277,
127.344999609685)) ;
#148756 = CARTESIAN_POINT('Ctrl Pts',(-32.7524169820034,12.2619062274696,
127.058889535839)) ;
#148757 = CARTESIAN_POINT('Ctrl Pts',(-32.6419963192406,12.2824388238971,
126.769324981895)) ;
#148758 = CARTESIAN_POINT('Ctrl Pts',(-32.5362628789588,12.3848777352211,
126.493663129602)) ;
#148759 = CARTESIAN_POINT('Ctrl Pts',(-32.4431445614343,12.5614991526439,
126.254730121884)) ;
#148760 = CARTESIAN_POINT('Ctrl Pts',(-32.3680539595633,12.7995867932639,
126.068470241934)) ;
#148761 = CARTESIAN_POINT('Ctrl Pts',(-32.3155888176679,13.0840299785093,
125.948484575688)) ;
#148762 = CARTESIAN_POINT('Ctrl Pts',(-32.2893312633254,13.3899587126068,
125.904739149321)) ;
#148763 = CARTESIAN_POINT('Ctrl Pts',(-32.2897584792436,13.6996411315525,
125.939101557284)) ;
#148764 = CARTESIAN_POINT('Ctrl Pts',(-32.3165996493069,13.9903747332587,
126.050727800221)) ;
#148765 = CARTESIAN_POINT('Ctrl Pts',(-32.3669241137826,14.2393240400609,
126.230826853994)) ;
#148766 = CARTESIAN_POINT('Ctrl Pts',(-32.4363513245266,14.4298400308443,
126.46669969067)) ;
#148767 = CARTESIAN_POINT('Ctrl Pts',(-32.519430880019,14.5487685214643,126.742513227334)) ;
#148768 = CARTESIAN_POINT('Ctrl Pts',(-32.6096330962241,14.5869290459119,
127.039223094392)) ;
#148769 = CARTESIAN_POINT('Ctrl Pts',(-32.6990799621577,14.5417666883846,
127.333562773258)) ;
#148770 = CARTESIAN_POINT('Ctrl Pts',(-32.7814232479936,14.4163781247343,
127.607278938856)) ;
#148771 = CARTESIAN_POINT('Ctrl Pts',(-32.8496169733658,14.2194053349132,
127.839665758422)) ;
#148772 = CARTESIAN_POINT('Ctrl Pts',(-32.8979064624203,13.9666437223108,
128.013748817654)) ;
#148773 = CARTESIAN_POINT('Ctrl Pts',(-32.9225596490422,13.6737230615468,
128.118947651821)) ;
#148774 = CARTESIAN_POINT('Ctrl Pts',(-32.9207144430641,13.3629183562335,
128.146716806087)) ;
#148775 = CARTESIAN_POINT('Ctrl Pts',(-32.8919279335873,13.0570541926124,
128.095721621593)) ;
#148776 = CARTESIAN_POINT('Ctrl Pts',(-32.8376033356132,12.7772474882028,
127.970123458047)) ;
#148777 = CARTESIAN_POINT('Ctrl Pts',(-32.7603558327083,12.5427680986525,
127.777727930602)) ;
#148778 = CARTESIAN_POINT('Ctrl Pts',(-32.6662279784257,12.3730788782687,
127.53571899559)) ;
#148779 = CARTESIAN_POINT('Ctrl Pts',(-32.5599217010986,12.2773830666973,
127.258340083159)) ;
#148780 = CARTESIAN_POINT('Ctrl Pts',(-32.4489850033344,12.2641121652248,
126.967384354349)) ;
#148781 = CARTESIAN_POINT('Ctrl Pts',(-32.3405436242218,12.3337583003129,
126.683712432675)) ;
#148782 = CARTESIAN_POINT('Ctrl Pts',(-32.2416220298584,12.481316017211,126.42783978584)) ;
#148783 = CARTESIAN_POINT('Ctrl Pts',(-32.1584105156519,12.6966779051232,
126.217918468821)) ;
#148784 = CARTESIAN_POINT('Ctrl Pts',(-32.0964113311334,12.96405838434,126.069941333546)) ;
#148785 = CARTESIAN_POINT('Ctrl Pts',(-32.0592942459553,13.2633620040759,
125.994551630201)) ;
#148786 = CARTESIAN_POINT('Ctrl Pts',(-32.0487513263688,13.5752566966047,
125.996917495549)) ;
#148787 = CARTESIAN_POINT('Ctrl Pts',(-32.0651787613996,13.8766501658651,
126.078125527416)) ;
#148788 = CARTESIAN_POINT('Ctrl Pts',(-32.106237139948,14.1438625345399,126.231076917147)) ;
#148789 = CARTESIAN_POINT('Ctrl Pts',(-32.1688151496798,14.3611557729943,
126.447120106865)) ;
#148790 = CARTESIAN_POINT('Ctrl Pts',(-32.2472987630035,14.5102070639316,
126.709529597132)) ;
#148791 = CARTESIAN_POINT('Ctrl Pts',(-32.3349170372181,14.5813677790431,
126.99845205783)) ;
#148792 = CARTESIAN_POINT('Ctrl Pts',(-32.4257587129059,14.5701315167375,
127.297011355326)) ;
#148793 = CARTESIAN_POINT('Ctrl Pts',(-32.5121114944259,14.4759919392145,
127.582506664814)) ;
#148794 = CARTESIAN_POINT('Ctrl Pts',(-32.586577018117,14.3066893243029,127.833144617972)) ;
#148795 = CARTESIAN_POINT('Ctrl Pts',(-32.6433606397653,14.075187939402,128.032015916789)) ;
#148796 = CARTESIAN_POINT('Ctrl Pts',(-32.6780690407698,13.7962287438528,
128.166528915326)) ;
#148797 = CARTESIAN_POINT('Ctrl Pts',(-32.6872064373839,13.4897393556908,
128.226418122972)) ;
#148798 = CARTESIAN_POINT('Ctrl Pts',(-32.6691192160608,13.1781057377786,
128.206822501505)) ;
#148799 = CARTESIAN_POINT('Ctrl Pts',(-32.6251388666684,12.8871395007703,
128.11122499469)) ;
#148800 = CARTESIAN_POINT('Ctrl Pts',(-32.5567420099813,12.6313543298591,
127.944663176923)) ;
#148801 = CARTESIAN_POINT('Ctrl Pts',(-32.468480326082,12.4333423964865,127.720004921838)) ;
#148802 = CARTESIAN_POINT('Ctrl Pts',(-32.3667523701111,12.3067788295905,
127.45578803769)) ;
#148803 = CARTESIAN_POINT('Ctrl Pts',(-32.2563735289916,12.2592790110699,
127.166620834658)) ;
#148804 = CARTESIAN_POINT('Ctrl Pts',(-32.1460193447871,12.2958890741667,
126.877373493955)) ;
#148805 = CARTESIAN_POINT('Ctrl Pts',(-32.0427219858457,12.412515964046,126.608629772059)) ;
#148806 = CARTESIAN_POINT('Ctrl Pts',(-31.9523858329491,12.6017795231482,
126.377868646038)) ;
#148807 = CARTESIAN_POINT('Ctrl Pts',(-31.8811024103402,12.8508820416093,
126.20286039856)) ;
#148808 = CARTESIAN_POINT('Ctrl Pts',(-31.8336722130978,13.1389626246921,
126.097293690777)) ;
#148809 = CARTESIAN_POINT('Ctrl Pts',(-31.8121351013455,13.4502019068506,
126.067683040548)) ;
#148810 = CARTESIAN_POINT('Ctrl Pts',(-31.8178503511759,13.7571545047615,
126.117429724884)) ;
#148811 = CARTESIAN_POINT('Ctrl Pts',(-31.8491017041277,14.0399279502617,
126.241716326633)) ;
#148812 = CARTESIAN_POINT('Ctrl Pts',(-31.9036445538269,14.2804627240583,
126.43430783686)) ;
#148813 = CARTESIAN_POINT('Ctrl Pts',(-31.976030827149,14.4580430249791,126.678783103797)) ;
#148814 = CARTESIAN_POINT('Ctrl Pts',(-32.0610740513668,14.5623041717052,
126.960389503841)) ;
#148815 = CARTESIAN_POINT('Ctrl Pts',(-32.1514066726644,14.5848738329504,
127.257341934247)) ;
#148816 = CARTESIAN_POINT('Ctrl Pts',(-32.2406996744394,14.5236285487513,
127.551504825239)) ;
#148817 = CARTESIAN_POINT('Ctrl Pts',(-32.3203563629849,14.3842859128116,
127.81718848941)) ;
#148818 = CARTESIAN_POINT('Ctrl Pts',(-32.3852114437279,14.1760037258481,
128.039769410632)) ;
#148819 = CARTESIAN_POINT('Ctrl Pts',(-32.4295530229322,13.9123646323485,
128.202565138207)) ;
#148820 = CARTESIAN_POINT('Ctrl Pts',(-32.4491140406027,13.6155080091082,
128.292745839514)) ;
#148821 = CARTESIAN_POINT('Ctrl Pts',(-32.442267685353,13.3048787604148,128.305795361212)) ;
#148822 = CARTESIAN_POINT('Ctrl Pts',(-32.4084189396864,13.0013159560589,
128.240117209961)) ;
#148823 = CARTESIAN_POINT('Ctrl Pts',(-32.3495230158094,12.7290185702227,
128.101151404377)) ;
#148824 = CARTESIAN_POINT('Ctrl Pts',(-32.2688647109356,12.5059453720444,
127.898672028067)) ;
#148825 = CARTESIAN_POINT('Ctrl Pts',(-32.171709171051,12.348935712054,127.647947097826)) ;
#148826 = CARTESIAN_POINT('Ctrl Pts',(-32.0642724896307,12.2685725815048,
127.367166374823)) ;
#148827 = CARTESIAN_POINT('Ctrl Pts',(-31.9528808938988,12.2709800121234,
127.074994579475)) ;
#148828 = CARTESIAN_POINT('Ctrl Pts',(-31.8458710839946,12.3558596886437,
126.795453239474)) ;
#148829 = CARTESIAN_POINT('Ctrl Pts',(-31.7493426472634,12.5173148322773,
126.546620338384)) ;
#148830 = CARTESIAN_POINT('Ctrl Pts',(-31.669870845794,12.7436532410187,126.347587050169)) ;
#148831 = CARTESIAN_POINT('Ctrl Pts',(-31.6123394354576,13.0184389835147,
126.212627252227)) ;
#148832 = CARTESIAN_POINT('Ctrl Pts',(-31.5800749292973,13.3224258162056,
126.151504283828)) ;
#148833 = CARTESIAN_POINT('Ctrl Pts',(-31.5747290724803,13.6337495707095,
126.169029469326)) ;
#148834 = CARTESIAN_POINT('Ctrl Pts',(-31.5959652324382,13.9298381021214,
126.264195066353)) ;
#148835 = CARTESIAN_POINT('Ctrl Pts',(-31.6414442989228,14.1894305566765,
126.430148429791)) ;
#148836 = CARTESIAN_POINT('Ctrl Pts',(-31.7073577282004,14.394475711673,126.655854752782)) ;
#148837 = CARTESIAN_POINT('Ctrl Pts',(-31.787889015417,14.5294751286176,126.924154341006)) ;
#148838 = CARTESIAN_POINT('Ctrl Pts',(-31.8769652278811,14.5857784674847,
127.217493619742)) ;
#148839 = CARTESIAN_POINT('Ctrl Pts',(-31.967547767219,14.5584758053027,127.515317123615)) ;
#148840 = CARTESIAN_POINT('Ctrl Pts',(-32.0518753014039,14.4499269628754,
127.794753752466)) ;
#148841 = CARTESIAN_POINT('Ctrl Pts',(-32.1235837510951,14.2678362538152,
128.037358324424)) ;
#148842 = CARTESIAN_POINT('Ctrl Pts',(-32.1767041734191,14.025181469635,128.225662324627)) ;
#148843 = CARTESIAN_POINT('Ctrl Pts',(-32.2067108970508,13.7395989406437,
128.346424348598)) ;
#148844 = CARTESIAN_POINT('Ctrl Pts',(-32.2107486585136,13.4312396287892,
128.391339089257)) ;
#148845 = CARTESIAN_POINT('Ctrl Pts',(-32.187850141749,13.1225497292761,128.357535369758)) ;
#148846 = CARTESIAN_POINT('Ctrl Pts',(-32.1387034319013,12.8344723647331,
128.247162948321)) ;
#148847 = CARTESIAN_POINT('Ctrl Pts',(-32.0663825406077,12.5894057804916,
128.068995833289)) ;
#148848 = CARTESIAN_POINT('Ctrl Pts',(-31.9751968195314,12.40386696018,127.835743163197)) ;
#148849 = CARTESIAN_POINT('Ctrl Pts',(-31.8710345103169,12.2913271454925,
127.564562587712)) ;
#148850 = CARTESIAN_POINT('Ctrl Pts',(-31.7602866795664,12.2598830910962,
127.274231377558)) ;
#148851 = CARTESIAN_POINT('Ctrl Pts',(-31.650876260428,12.3117248665292,126.987672720107)) ;
#148852 = CARTESIAN_POINT('Ctrl Pts',(-31.5491888340202,12.4432581620118,
126.723765797051)) ;
#148853 = CARTESIAN_POINT('Ctrl Pts',(-31.4622339713139,12.6447767866554,
126.502841897175)) ;
#148854 = CARTESIAN_POINT('Ctrl Pts',(-31.3952636966444,12.9020426127521,
126.340316351523)) ;
#148855 = CARTESIAN_POINT('Ctrl Pts',(-31.3524307764882,13.1969219794908,
126.248333436724)) ;
#148856 = CARTESIAN_POINT('Ctrl Pts',(-31.3360597331942,13.5073632860462,
126.233579460567)) ;
#148857 = CARTESIAN_POINT('Ctrl Pts',(-31.3467467970684,13.813502723387,126.298071632455)) ;
#148858 = CARTESIAN_POINT('Ctrl Pts',(-31.3826080772341,14.089063380816,126.435785315651)) ;
#148859 = CARTESIAN_POINT('Ctrl Pts',(-31.4410196431954,14.319268429037,126.639693220211)) ;
#148860 = CARTESIAN_POINT('Ctrl Pts',(-31.5161372632697,14.4835637196257,
126.892114231068)) ;
#148861 = CARTESIAN_POINT('Ctrl Pts',(-31.6028715211698,14.5730187968723,
127.178702983459)) ;
#148862 = CARTESIAN_POINT('Ctrl Pts',(-31.6935959532657,14.5795967994517,
127.47685559871)) ;
#148863 = CARTESIAN_POINT('Ctrl Pts',(-31.7812976545653,14.5032854437543,
127.766198609052)) ;
#148864 = CARTESIAN_POINT('Ctrl Pts',(-31.8588077042813,14.350115255618,128.025685725528)) ;
#148865 = CARTESIAN_POINT('Ctrl Pts',(-31.9203271776916,14.1289953523701,
128.238682003332)) ;
#148866 = CARTESIAN_POINT('Ctrl Pts',(-31.9599005577063,13.8600885343661,
128.38719829855)) ;
#148867 = CARTESIAN_POINT('Ctrl Pts',(-31.9748262172758,13.5571077993043,
128.464060699988)) ;
#148868 = CARTESIAN_POINT('Ctrl Pts',(-31.962757597202,13.2461442417419,128.46187610043)) ;
#148869 = CARTESIAN_POINT('Ctrl Pts',(-31.9241515733642,12.9474785821981,
128.382201956869)) ;
#148870 = CARTESIAN_POINT('Ctrl Pts',(-31.8604665395994,12.6818051231589,
128.229429013214)) ;
#148871 = CARTESIAN_POINT('Ctrl Pts',(-31.7767215134204,12.4713262557242,
128.017732941446)) ;
#148872 = CARTESIAN_POINT('Ctrl Pts',(-31.6766990193786,12.3273775591191,
127.758780001682)) ;
#148873 = CARTESIAN_POINT('Ctrl Pts',(-31.5681563819875,12.2625380497534,
127.474731473525)) ;
#148874 = CARTESIAN_POINT('Ctrl Pts',(-31.456705348187,12.2810707437097,127.182462188082)) ;
#148875 = CARTESIAN_POINT('Ctrl Pts',(-31.3518550564754,12.3803128917833,
126.909020385735)) ;
#148876 = CARTESIAN_POINT('Ctrl Pts',(-31.257702619694,12.5556238817755,126.66726187908)) ;
#148877 = CARTESIAN_POINT('Ctrl Pts',(-31.1822947771,12.7914916788268,126.479962924463)) ;
#148878 = CARTESIAN_POINT('Ctrl Pts',(-31.128989212263,13.075040960321,126.357555646944)) ;
#148879 = CARTESIAN_POINT('Ctrl Pts',(-31.1019281701604,13.3808908357546,
126.311493897852)) ;
#148880 = CARTESIAN_POINT('Ctrl Pts',(-31.101598677276,13.6908804801079,126.343656174616)) ;
#148881 = CARTESIAN_POINT('Ctrl Pts',(-31.1276137979724,13.9819858711707,
126.452802987788)) ;
#148882 = CARTESIAN_POINT('Ctrl Pts',(-31.1774498129048,14.2331023132834,
126.631574159292)) ;
#148883 = CARTESIAN_POINT('Ctrl Pts',(-31.2463221547252,14.4253737396298,
126.865787908676)) ;
#148884 = CARTESIAN_POINT('Ctrl Pts',(-31.3296291551697,14.54690254864,127.142464376561)) ;
#148885 = CARTESIAN_POINT('Ctrl Pts',(-31.4191291908472,14.5868798000434,
127.43689176411)) ;
#148886 = CARTESIAN_POINT('Ctrl Pts',(-31.5088033883795,14.5442430109602,
127.731941184325)) ;
#148887 = CARTESIAN_POINT('Ctrl Pts',(-31.5913579378226,14.4211466700167,
128.006234530102)) ;
#148888 = CARTESIAN_POINT('Ctrl Pts',(-31.6600527357246,14.2262607777735,
128.24007434236)) ;
#148889 = CARTESIAN_POINT('Ctrl Pts',(-31.7090806186089,13.9744157685803,
128.41637832251)) ;
#148890 = CARTESIAN_POINT('Ctrl Pts',(-31.7343968963979,13.6824770382547,
128.523494114923)) ;
#148891 = CARTESIAN_POINT('Ctrl Pts',(-31.733427314249,13.3726811668738,128.553735367064)) ;
#148892 = CARTESIAN_POINT('Ctrl Pts',(-31.7051969519129,13.06445534207,128.504576440852)) ;
#148893 = CARTESIAN_POINT('Ctrl Pts',(-31.6517486616812,12.7851438246932,
128.381371124061)) ;
#148894 = CARTESIAN_POINT('Ctrl Pts',(-31.5753581104184,12.5493640778092,
128.191406816883)) ;
#148895 = CARTESIAN_POINT('Ctrl Pts',(-31.4814357009972,12.3769707838731,
127.950088842735)) ;
#148896 = CARTESIAN_POINT('Ctrl Pts',(-31.3750785325616,12.2789143225366,
127.672647100852)) ;
#148897 = CARTESIAN_POINT('Ctrl Pts',(-31.2645011786584,12.2633331212568,
127.382644142174)) ;
#148898 = CARTESIAN_POINT('Ctrl Pts',(-31.1556392002351,12.3306602276622,
127.097816362084)) ;
#148899 = CARTESIAN_POINT('Ctrl Pts',(-31.0562518667152,12.4766202323596,
126.840633530145)) ;
#148900 = CARTESIAN_POINT('Ctrl Pts',(-30.972938158,12.6891735601127,126.630245983775)) ;
#148901 = CARTESIAN_POINT('Ctrl Pts',(-30.9101457934406,12.9552554154068,
126.479968848149)) ;
#148902 = CARTESIAN_POINT('Ctrl Pts',(-30.8721764023773,13.2547269193452,
126.402177144233)) ;
#148903 = CARTESIAN_POINT('Ctrl Pts',(-30.8609235836592,13.5662745338838,
126.402436753715)) ;
#148904 = CARTESIAN_POINT('Ctrl Pts',(-30.8764476985309,13.8673045434185,
126.480887327569)) ;
#148905 = CARTESIAN_POINT('Ctrl Pts',(-30.9169530211909,14.1368395947381,
126.632353008074)) ;
#148906 = CARTESIAN_POINT('Ctrl Pts',(-30.9787492522739,14.355047357882,126.845986583721)) ;
#148907 = CARTESIAN_POINT('Ctrl Pts',(-31.0567851807192,14.5066809215218,
127.107093173731)) ;
#148908 = CARTESIAN_POINT('Ctrl Pts',(-31.1446588781563,14.5805549818753,
127.396924345416)) ;
#148909 = CARTESIAN_POINT('Ctrl Pts',(-31.2352728616708,14.5715434476004,
127.69472820504)) ;
#148910 = CARTESIAN_POINT('Ctrl Pts',(-31.3215614046395,14.4804615024267,
127.979908754942)) ;
#148911 = CARTESIAN_POINT('Ctrl Pts',(-31.3967763756955,14.3129345410317,
128.232850337699)) ;
#148912 = CARTESIAN_POINT('Ctrl Pts',(-31.4542633909924,14.0824720621631,
128.433850809568)) ;
#148913 = CARTESIAN_POINT('Ctrl Pts',(-31.489623472081,13.8045960831527,128.570261385745)) ;
#148914 = CARTESIAN_POINT('Ctrl Pts',(-31.4995214449114,13.4994873044745,
128.632276592149)) ;
#148915 = CARTESIAN_POINT('Ctrl Pts',(-31.4823318161701,13.1877259359498,
128.615295704579)) ;
#148916 = CARTESIAN_POINT('Ctrl Pts',(-31.4389383199175,12.8947282234829,
128.521543366635)) ;
#148917 = CARTESIAN_POINT('Ctrl Pts',(-31.3710227559662,12.6375710763399,
128.35641831796)) ;
#148918 = CARTESIAN_POINT('Ctrl Pts',(-31.2837896130209,12.438646888205,128.134577930559)) ;
#148919 = CARTESIAN_POINT('Ctrl Pts',(-31.1818199730732,12.3091461051662,
127.869843437161)) ;
#148920 = CARTESIAN_POINT('Ctrl Pts',(-31.0721930263466,12.2596124817515,
127.582678546268)) ;
#148921 = CARTESIAN_POINT('Ctrl Pts',(-30.9614915352443,12.2934287573512,
127.292491909052)) ;
#148922 = CARTESIAN_POINT('Ctrl Pts',(-30.8574567264293,12.4085128318244,
127.021738717277)) ;
#148923 = CARTESIAN_POINT('Ctrl Pts',(-30.7669612991102,12.5956557318582,
126.790429502215)) ;
#148924 = CARTESIAN_POINT('Ctrl Pts',(-30.6952746289736,12.8419007286425,
126.614087904973)) ;
#148925 = CARTESIAN_POINT('Ctrl Pts',(-30.646823062796,13.131017500255,126.505762609354)) ;
#148926 = CARTESIAN_POINT('Ctrl Pts',(-30.6246568272436,13.4394174344068,
126.47403583793)) ;
#148927 = CARTESIAN_POINT('Ctrl Pts',(-30.6294887388324,13.7489280786131,
126.521433227491)) ;
#148928 = CARTESIAN_POINT('Ctrl Pts',(-30.6601827171697,14.0326636171821,
126.644108290625)) ;
#148929 = CARTESIAN_POINT('Ctrl Pts',(-30.7138555910178,14.2739040584896,
126.834025044744)) ;
#148930 = CARTESIAN_POINT('Ctrl Pts',(-30.7861586740712,14.4542738931404,
127.078423495766)) ;
#148931 = CARTESIAN_POINT('Ctrl Pts',(-30.8705668756073,14.5602989567159,
127.358020430857)) ;
#148932 = CARTESIAN_POINT('Ctrl Pts',(-30.9611627968773,14.5853165181453,
127.655868520581)) ;
#148933 = CARTESIAN_POINT('Ctrl Pts',(-31.050038446453,14.5269567294315,127.948592774541)) ;
#148934 = CARTESIAN_POINT('Ctrl Pts',(-31.1306389772583,14.3891798235028,
128.217257244013)) ;
#148935 = CARTESIAN_POINT('Ctrl Pts',(-31.1959979491023,14.1817903606507,
128.44137499461)) ;
#148936 = CARTESIAN_POINT('Ctrl Pts',(-31.2406347364941,13.9219442821041,
128.60472994041)) ;
#148937 = CARTESIAN_POINT('Ctrl Pts',(-31.2611632325786,13.6244334028394,
128.697907886607)) ;
#148938 = CARTESIAN_POINT('Ctrl Pts',(-31.2550704721298,13.313830933939,128.713157746917)) ;
#148939 = CARTESIAN_POINT('Ctrl Pts',(-31.2218492806563,13.0089908308966,
128.649399781927)) ;
#148940 = CARTESIAN_POINT('Ctrl Pts',(-31.1638471119269,12.7367006174924,
128.512907453242)) ;
#148941 = CARTESIAN_POINT('Ctrl Pts',(-31.0837932668277,12.511790352846,128.312199836649)) ;
#148942 = CARTESIAN_POINT('Ctrl Pts',(-30.9870335192191,12.3525056557872,
128.062637893671)) ;
#148943 = CARTESIAN_POINT('Ctrl Pts',(-30.8793393489368,12.2695603711095,
127.781244876956)) ;
#148944 = CARTESIAN_POINT('Ctrl Pts',(-30.7681133580193,12.2698997293224,
127.489506388524)) ;
#148945 = CARTESIAN_POINT('Ctrl Pts',(-30.6611822400165,12.3521639545542,
127.21010491514)) ;
#148946 = CARTESIAN_POINT('Ctrl Pts',(-30.5641504847242,12.5116414320552,
126.959834218351)) ;
#148947 = CARTESIAN_POINT('Ctrl Pts',(-30.4841799844132,12.7360068046191,
126.759304891877)) ;
#148948 = CARTESIAN_POINT('Ctrl Pts',(-30.4258743728948,13.0100794462922,
126.622138522883)) ;
#148949 = CARTESIAN_POINT('Ctrl Pts',(-30.3928856489435,13.3126251519116,
126.558801239046)) ;
#148950 = CARTESIAN_POINT('Ctrl Pts',(-30.3867270276499,13.6254713838339,
126.574107468755)) ;
#148951 = CARTESIAN_POINT('Ctrl Pts',(-30.4071673743065,13.9212363983898,
126.666825972568)) ;
#148952 = CARTESIAN_POINT('Ctrl Pts',(-30.4520657346943,14.182693359551,126.831154475535)) ;
#148953 = CARTESIAN_POINT('Ctrl Pts',(-30.5172045915089,14.388968587839,127.054480565499)) ;
#148954 = CARTESIAN_POINT('Ctrl Pts',(-30.5978949912035,14.5271449828327,
127.323459118803)) ;
#148955 = CARTESIAN_POINT('Ctrl Pts',(-30.6869252863348,14.5852339313446,
127.616686057635)) ;
#148956 = CARTESIAN_POINT('Ctrl Pts',(-30.7769736137098,14.5605427839008,
127.912730055109)) ;
#148957 = CARTESIAN_POINT('Ctrl Pts',(-30.8618338634156,14.4541441821425,
128.193820416888)) ;
#148958 = CARTESIAN_POINT('Ctrl Pts',(-30.933942967095,14.2740963581792,128.437570738178)) ;
#148959 = CARTESIAN_POINT('Ctrl Pts',(-30.9878091811295,14.0323113149494,
128.628141355214)) ;
#148960 = CARTESIAN_POINT('Ctrl Pts',(-31.0184130329351,13.7476340244825,
128.750639914861)) ;
#148961 = CARTESIAN_POINT('Ctrl Pts',(-31.0232549340075,13.4408490996929,
128.797771945858)) ;
#148962 = CARTESIAN_POINT('Ctrl Pts',(-31.0010012554192,13.1304291597349,
128.766011349424)) ;
#148963 = CARTESIAN_POINT('Ctrl Pts',(-30.9527573293382,12.8426172775068,
128.658135893252)) ;
#148964 = CARTESIAN_POINT('Ctrl Pts',(-30.8807389453885,12.5951022403137,
128.480994628538)) ;
#148965 = CARTESIAN_POINT('Ctrl Pts',(-30.7904651788176,12.4086451366238,
128.250233623956)) ;
#148966 = CARTESIAN_POINT('Ctrl Pts',(-30.6863228080809,12.2933533554013,
127.9792074839)) ;
#148967 = CARTESIAN_POINT('Ctrl Pts',(-30.5756850359936,12.2596356648428,
127.689183859545)) ;
#148968 = CARTESIAN_POINT('Ctrl Pts',(-30.466203016368,12.3091205496962,127.402403834731)) ;
#148969 = CARTESIAN_POINT('Ctrl Pts',(-30.3643703623581,12.4379929184033,
127.138001306152)) ;
#148970 = CARTESIAN_POINT('Ctrl Pts',(-30.2764808806105,12.6386444733354,
126.914510251683)) ;
#148971 = CARTESIAN_POINT('Ctrl Pts',(-30.2090793318311,12.8942394600066,
126.750661369868)) ;
#148972 = CARTESIAN_POINT('Ctrl Pts',(-30.1655515186205,13.1876523061434,
126.6565785761)) ;
#148973 = CARTESIAN_POINT('Ctrl Pts',(-30.1483782750824,13.4984174202856,
126.639535142431)) ;
#148974 = CARTESIAN_POINT('Ctrl Pts',(-30.1582136153607,13.804322851742,126.701452487564)) ;
#148975 = CARTESIAN_POINT('Ctrl Pts',(-30.1935881730914,14.0825043451859,
126.837930713879)) ;
#148976 = CARTESIAN_POINT('Ctrl Pts',(-30.2513065925607,14.3134150870924,
127.039706314653)) ;
#148977 = CARTESIAN_POINT('Ctrl Pts',(-30.3260116279673,14.4799819682822,
127.290938064371)) ;
#148978 = CARTESIAN_POINT('Ctrl Pts',(-30.4128554732831,14.5717628794977,
127.577963905631)) ;
#148979 = CARTESIAN_POINT('Ctrl Pts',(-30.5031073153007,14.5804902548306,
127.874570300572)) ;
#148980 = CARTESIAN_POINT('Ctrl Pts',(-30.5909549614635,14.5068426765183,
128.16431731435)) ;
#148981 = CARTESIAN_POINT('Ctrl Pts',(-30.6689392721254,14.3556216409034,
128.425228448955)) ;
#148982 = CARTESIAN_POINT('Ctrl Pts',(-30.7309826796393,14.1365917034713,
128.639714474064)) ;
#148983 = CARTESIAN_POINT('Ctrl Pts',(-30.7713121688787,13.8680781333687,
128.790537435745)) ;
#148984 = CARTESIAN_POINT('Ctrl Pts',(-30.7869976676125,13.5671870152877,
128.869457137254)) ;
#148985 = CARTESIAN_POINT('Ctrl Pts',(-30.7756199855816,13.253754715573,128.869553597425)) ;
#148986 = CARTESIAN_POINT('Ctrl Pts',(-30.7378428697437,12.9561226298826,
128.792121574417)) ;
#148987 = CARTESIAN_POINT('Ctrl Pts',(-30.6750924058368,12.689577131159,128.6420045891)) ;
#148988 = CARTESIAN_POINT('Ctrl Pts',(-30.5916276957833,12.4765149553713,
128.431238476743)) ;
#148989 = CARTESIAN_POINT('Ctrl Pts',(-30.4919348522374,12.330399344862,128.173255254871)) ;
#148990 = CARTESIAN_POINT('Ctrl Pts',(-30.3834739315927,12.2633426723701,
127.889471684178)) ;
#148991 = CARTESIAN_POINT('Ctrl Pts',(-30.2725618689719,12.2791039533646,
127.598598845165)) ;
#148992 = CARTESIAN_POINT('Ctrl Pts',(-30.1667739512017,12.3764766971553,
127.322629115757)) ;
#148993 = CARTESIAN_POINT('Ctrl Pts',(-30.0722613215076,12.5500288330121,
127.079808436229)) ;
#148994 = CARTESIAN_POINT('Ctrl Pts',(-29.9964223473625,12.7839577704924,
126.891194707482)) ;
#148995 = CARTESIAN_POINT('Ctrl Pts',(-29.942454441113,13.0658040445484,126.766783601565)) ;
#148996 = CARTESIAN_POINT('Ctrl Pts',(-29.9144858273214,13.3726170007347,
126.718219451376)) ;
#148997 = CARTESIAN_POINT('Ctrl Pts',(-29.9135066816094,13.6826397065971,
126.748467644402)) ;
#148998 = CARTESIAN_POINT('Ctrl Pts',(-29.93864177303,13.973415999198,126.854904439915)) ;
#148999 = CARTESIAN_POINT('Ctrl Pts',(-29.9879875205848,14.2269288255441,
127.032360766386)) ;
#149000 = CARTESIAN_POINT('Ctrl Pts',(-30.0562982578127,14.4205112234245,
127.264872894418)) ;
#149001 = CARTESIAN_POINT('Ctrl Pts',(-30.1388423960146,14.5441065980074,
127.539162805067)) ;
#149002 = CARTESIAN_POINT('Ctrl Pts',(-30.2288796774429,14.5870792667271,
127.835398320618)) ;
#149003 = CARTESIAN_POINT('Ctrl Pts',(-30.318752130409,14.5462510446376,128.131069708792)) ;
#149004 = CARTESIAN_POINT('Ctrl Pts',(-30.4011990424657,14.4261089740706,
128.404876189564)) ;
#149005 = CARTESIAN_POINT('Ctrl Pts',(-30.4707707769806,14.2320089324099,
128.641468375281)) ;
#149006 = CARTESIAN_POINT('Ctrl Pts',(-30.5201915042362,13.9821035017428,
128.818820320772)) ;
#149007 = CARTESIAN_POINT('Ctrl Pts',(-30.5462282037767,13.6914861208152,
128.927995546701)) ;
#149008 = CARTESIAN_POINT('Ctrl Pts',(-30.5460671305447,13.3820427303129,
128.96058514073)) ;
#149009 = CARTESIAN_POINT('Ctrl Pts',(-30.5186186649558,13.0731825073203,
128.913731663666)) ;
#149010 = CARTESIAN_POINT('Ctrl Pts',(-30.4658657649698,12.792789184468,128.792563884169)) ;
#149011 = CARTESIAN_POINT('Ctrl Pts',(-30.390062659985,12.5553087421356,128.604324240762)) ;
#149012 = CARTESIAN_POINT('Ctrl Pts',(-30.2964051343669,12.3807971817362,
128.363831596065)) ;
#149013 = CARTESIAN_POINT('Ctrl Pts',(-30.1906919248692,12.2807361570638,
128.088147478697)) ;
#149014 = CARTESIAN_POINT('Ctrl Pts',(-30.0798079005075,12.2625961451368,
127.797356146879)) ;
#149015 = CARTESIAN_POINT('Ctrl Pts',(-29.970954505239,12.32755343176,127.512498551753)) ;
#149016 = CARTESIAN_POINT('Ctrl Pts',(-29.8712078270959,12.4713199441997,
127.254267669833)) ;
#149017 = CARTESIAN_POINT('Ctrl Pts',(-29.7873334259334,12.6818353121991,
127.042222843029)) ;
#149018 = CARTESIAN_POINT('Ctrl Pts',(-29.7235176767161,12.9488694906299,
126.889210528772)) ;
#149019 = CARTESIAN_POINT('Ctrl Pts',(-29.6852261685552,13.2449963341531,
126.810169235645)) ;
#149020 = CARTESIAN_POINT('Ctrl Pts',(-29.6730505875199,13.5577145851588,
126.807868872823)) ;
#149021 = CARTESIAN_POINT('Ctrl Pts',(-29.6878754711503,13.8591378593898,
126.884253177317)) ;
#149022 = CARTESIAN_POINT('Ctrl Pts',(-29.7277642234698,14.130166831006,127.033958962988)) ;
#149023 = CARTESIAN_POINT('Ctrl Pts',(-29.7890265231427,14.349825857909,127.246014723046)) ;
#149024 = CARTESIAN_POINT('Ctrl Pts',(-29.8665533617496,14.5033075139511,
127.505580619346)) ;
#149025 = CARTESIAN_POINT('Ctrl Pts',(-29.9542811977828,14.5795880781192,
127.795003544742)) ;
#149026 = CARTESIAN_POINT('Ctrl Pts',(-30.0449500375347,14.5729975365321,
128.092978630465)) ;
#149027 = CARTESIAN_POINT('Ctrl Pts',(-30.1317041723412,14.4837968841282,
128.379616319117)) ;
#149028 = CARTESIAN_POINT('Ctrl Pts',(-30.2071928803997,14.3181446441766,
128.633325545973)) ;
#149029 = CARTESIAN_POINT('Ctrl Pts',(-30.2650803133091,14.0900337543834,
128.83539277785)) ;
#149030 = CARTESIAN_POINT('Ctrl Pts',(-30.3012106539237,13.8125788202494,
128.974133301393)) ;
#149031 = CARTESIAN_POINT('Ctrl Pts',(-30.3117972843206,13.5087144247666,
129.038074958722)) ;
#149032 = CARTESIAN_POINT('Ctrl Pts',(-30.2954912808033,13.1970642860529,
129.02364480025)) ;
#149033 = CARTESIAN_POINT('Ctrl Pts',(-30.2526709527815,12.9023259165876,
128.931677028235)) ;
#149034 = CARTESIAN_POINT('Ctrl Pts',(-30.1856053589782,12.6446851896536,
128.768924943894)) ;
#149035 = CARTESIAN_POINT('Ctrl Pts',(-30.0988846407419,12.4436426987833,
128.548597777783)) ;
#149036 = CARTESIAN_POINT('Ctrl Pts',(-29.9971156856899,12.311800617446,128.284491079494)) ;
#149037 = CARTESIAN_POINT('Ctrl Pts',(-29.8875872119017,12.2597626710197,
127.997619613751)) ;
#149038 = CARTESIAN_POINT('Ctrl Pts',(-29.7764046490522,12.2917039117493,
127.706157620277)) ;
#149039 = CARTESIAN_POINT('Ctrl Pts',(-29.6728942100867,12.4035190207528,
127.436666928702)) ;
#149040 = CARTESIAN_POINT('Ctrl Pts',(-29.5811635921256,12.5902948819765,
127.202036427248)) ;
#149041 = CARTESIAN_POINT('Ctrl Pts',(-29.5093504589281,12.8337324593119,
127.02511882226)) ;
#149042 = CARTESIAN_POINT('Ctrl Pts',(-29.459889065768,13.1235886512336,126.914040981108)) ;
#149043 = CARTESIAN_POINT('Ctrl Pts',(-29.4372132851433,13.4302519465087,
126.880664182196)) ;
#149044 = CARTESIAN_POINT('Ctrl Pts',(-29.4410746743041,13.7390104769504,
126.925099881042)) ;
#149045 = CARTESIAN_POINT('Ctrl Pts',(-29.4713124307665,14.026006220093,127.046710522163)) ;
#149046 = CARTESIAN_POINT('Ctrl Pts',(-29.5241600420331,14.267226887447,127.23403016745)) ;
#149047 = CARTESIAN_POINT('Ctrl Pts',(-29.5958998341777,14.4498458774909,
127.476774523752)) ;
#149048 = CARTESIAN_POINT('Ctrl Pts',(-29.6804543579856,14.5586319222976,
127.75695530447)) ;
#149049 = CARTESIAN_POINT('Ctrl Pts',(-29.7710143154337,14.5856242109288,
128.054706589964)) ;
#149050 = CARTESIAN_POINT('Ctrl Pts',(-29.8596478809037,14.5299078426425,
128.346578696437)) ;
#149051 = CARTESIAN_POINT('Ctrl Pts',(-29.940797824085,14.3940108170827,128.616933746993)) ;
#149052 = CARTESIAN_POINT('Ctrl Pts',(-30.0065313921842,14.1888421373124,
128.842072173602)) ;
#149053 = CARTESIAN_POINT('Ctrl Pts',(-30.0518836645061,13.9299825539778,
129.007565480482)) ;
#149054 = CARTESIAN_POINT('Ctrl Pts',(-30.0731422301956,13.6339609889882,
129.102792375169)) ;
#149055 = CARTESIAN_POINT('Ctrl Pts',(-30.0678240733041,13.322716019869,129.120388848256)) ;
#149056 = CARTESIAN_POINT('Ctrl Pts',(-30.0355611101008,13.0187245278142,
129.059274077997)) ;
#149057 = CARTESIAN_POINT('Ctrl Pts',(-29.9782043992279,12.7442185255371,
128.924769323151)) ;
#149058 = CARTESIAN_POINT('Ctrl Pts',(-29.8982556126516,12.5167189734132,
128.724530848476)) ;
#149059 = CARTESIAN_POINT('Ctrl Pts',(-29.8023192584172,12.3563386644065,
128.477216795645)) ;
#149060 = CARTESIAN_POINT('Ctrl Pts',(-29.6950698376708,12.2709228506509,
128.197061735731)) ;
#149061 = CARTESIAN_POINT('Ctrl Pts',(-29.5837196202969,12.268610094108,127.904997982331)) ;
#149062 = CARTESIAN_POINT('Ctrl Pts',(-29.4763327572683,12.3485945923255,
127.624335641344)) ;
#149063 = CARTESIAN_POINT('Ctrl Pts',(-29.3786180682244,12.5068355789937,
127.372187573838)) ;
#149064 = CARTESIAN_POINT('Ctrl Pts',(-29.2985863374153,12.7283300538896,
127.171287513075)) ;
#149065 = CARTESIAN_POINT('Ctrl Pts',(-29.2394412133029,13.0013549210284,
127.031702565481)) ;
#149066 = CARTESIAN_POINT('Ctrl Pts',(-29.2056837300174,13.3039530597295,
126.96618289312)) ;
#149067 = CARTESIAN_POINT('Ctrl Pts',(-29.1987066729557,13.615850743561,126.978983927502)) ;
#149068 = CARTESIAN_POINT('Ctrl Pts',(-29.2185194823492,13.9138454553417,
127.070043003934)) ;
#149069 = CARTESIAN_POINT('Ctrl Pts',(-29.2625769744912,14.1752851805425,
127.231751072296)) ;
#149070 = CARTESIAN_POINT('Ctrl Pts',(-29.3272880904875,14.3839668392215,
127.45390258644)) ;
#149071 = CARTESIAN_POINT('Ctrl Pts',(-29.4075505220235,14.5240578226957,
127.721592281445)) ;
#149072 = CARTESIAN_POINT('Ctrl Pts',(-29.4963462070103,14.584818929902,128.014106992847)) ;
#149073 = CARTESIAN_POINT('Ctrl Pts',(-29.587047691809,14.5621167472896,128.312281230879)) ;
#149074 = CARTESIAN_POINT('Ctrl Pts',(-29.6716157083653,14.4583966602146,
128.592308831358)) ;
#149075 = CARTESIAN_POINT('Ctrl Pts',(-29.7442665614833,14.2803904178195,
128.837668999258)) ;
#149076 = CARTESIAN_POINT('Ctrl Pts',(-29.7986307677681,14.0406559765549,
129.02962703218)) ;
#149077 = CARTESIAN_POINT('Ctrl Pts',(-29.8301070762697,13.7571590399429,
129.154671220007)) ;
#149078 = CARTESIAN_POINT('Ctrl Pts',(-29.8356379413796,13.4483332736025,
129.204074994619)) ;
#149079 = CARTESIAN_POINT('Ctrl Pts',(-29.8143943312686,13.1406103992417,
129.174937518758)) ;
#149080 = CARTESIAN_POINT('Ctrl Pts',(-29.7664779024948,12.8492377170497,
129.068326740931)) ;
#149081 = CARTESIAN_POINT('Ctrl Pts',(-29.695477480617,12.6021186018862,128.893930092439)) ;
#149082 = CARTESIAN_POINT('Ctrl Pts',(-29.6056095162878,12.4130744412516,
128.664414490585)) ;
#149083 = CARTESIAN_POINT('Ctrl Pts',(-29.5013486547958,12.2953575367152,
128.393159695613)) ;
#149084 = CARTESIAN_POINT('Ctrl Pts',(-29.3912652273664,12.2595400052722,
128.104616314454)) ;
#149085 = CARTESIAN_POINT('Ctrl Pts',(-29.2815644215268,12.3063152816415,
127.81721837263)) ;
#149086 = CARTESIAN_POINT('Ctrl Pts',(-29.1788437256449,12.4341408158502,
127.550424574528)) ;
#149087 = CARTESIAN_POINT('Ctrl Pts',(-29.0911599373369,12.6316134537437,
127.327283665833)) ;
#149088 = CARTESIAN_POINT('Ctrl Pts',(-29.0229070295168,12.8861349922411,
127.161015018853)) ;
#149089 = CARTESIAN_POINT('Ctrl Pts',(-28.97860409195,13.1792138645797,127.064713176007)) ;
#149090 = CARTESIAN_POINT('Ctrl Pts',(-28.960680378975,13.4905686905893,127.045557913132)) ;
#149091 = CARTESIAN_POINT('Ctrl Pts',(-28.9698588717169,13.7964603430473,
127.105511528331)) ;
#149092 = CARTESIAN_POINT('Ctrl Pts',(-29.0043770379677,14.0743847640953,
127.239335900994)) ;
#149093 = CARTESIAN_POINT('Ctrl Pts',(-29.0613333209739,14.3070162131528,
127.438846969311)) ;
#149094 = CARTESIAN_POINT('Ctrl Pts',(-29.1360898555168,14.4764518119822,
127.690429115817)) ;
#149095 = CARTESIAN_POINT('Ctrl Pts',(-29.2219415160562,14.5698501625241,
127.974264672901)) ;
#149096 = CARTESIAN_POINT('Ctrl Pts',(-29.3126334826048,14.5816111326668,
128.272334008304)) ;
#149097 = CARTESIAN_POINT('Ctrl Pts',(-29.400926685228,14.5098992068035,128.563479690303)) ;
#149098 = CARTESIAN_POINT('Ctrl Pts',(-29.4793116651,14.3604030985763,128.825592204278)) ;
#149099 = CARTESIAN_POINT('Ctrl Pts',(-29.541687497227,14.1435657734104,129.04096069706)) ;
#149100 = CARTESIAN_POINT('Ctrl Pts',(-29.5827585769447,13.8762647134096,
129.193957278894)) ;
#149101 = CARTESIAN_POINT('Ctrl Pts',(-29.5990886189644,13.5746435358358,
129.274900295363)) ;
#149102 = CARTESIAN_POINT('Ctrl Pts',(-29.5886877794002,13.2647987939523,
129.27746114699)) ;
#149103 = CARTESIAN_POINT('Ctrl Pts',(-29.5514689178778,12.9638357563477,
129.201951033959)) ;
#149104 = CARTESIAN_POINT('Ctrl Pts',(-29.489458499903,12.6967407948571,129.053914570688)) ;
#149105 = CARTESIAN_POINT('Ctrl Pts',(-29.4063560646129,12.481516798795,128.844280719317)) ;
#149106 = CARTESIAN_POINT('Ctrl Pts',(-29.3073900325767,12.3337893926253,
128.588297373864)) ;
#149107 = CARTESIAN_POINT('Ctrl Pts',(-29.1988456086286,12.264079799943,128.304354062159)) ;
#149108 = CARTESIAN_POINT('Ctrl Pts',(-29.0880318599508,12.2774691330631,
128.013725536534)) ;
#149109 = CARTESIAN_POINT('Ctrl Pts',(-28.9819973355058,12.3724670081561,
127.737037424083)) ;
#149110 = CARTESIAN_POINT('Ctrl Pts',(-28.8870857299463,12.5437673872502,
127.493027576055)) ;
#149111 = CARTESIAN_POINT('Ctrl Pts',(-28.8105213920732,12.7765746367498,
127.302360710588)) ;
#149112 = CARTESIAN_POINT('Ctrl Pts',(-28.7559878003064,13.056442650052,127.176189804149)) ;
#149113 = CARTESIAN_POINT('Ctrl Pts',(-28.7271624657516,13.3632373960093,
127.125177982557)) ;
#149114 = CARTESIAN_POINT('Ctrl Pts',(-28.7252862623066,13.6730054777402,
127.152742684901)) ;
#149115 = CARTESIAN_POINT('Ctrl Pts',(-28.7500212628402,13.9671153090071,
127.258316722838)) ;
#149116 = CARTESIAN_POINT('Ctrl Pts',(-28.7982268980631,14.2192390976399,
127.432074162142)) ;
#149117 = CARTESIAN_POINT('Ctrl Pts',(-28.8665165492583,14.4164802278466,
127.664792796035)) ;
#149118 = CARTESIAN_POINT('Ctrl Pts',(-28.9485994104117,14.5415580379271,
127.937643046099)) ;
#149119 = CARTESIAN_POINT('Ctrl Pts',(-29.0382249365808,14.5869148385537,
128.232577398888)) ;
#149120 = CARTESIAN_POINT('Ctrl Pts',(-29.1281597523479,14.5490099524811,
128.528401805914)) ;
#149121 = CARTESIAN_POINT('Ctrl Pts',(-29.2114841346123,14.4299835675068,
128.805020302905)) ;
#149122 = CARTESIAN_POINT('Ctrl Pts',(-29.2809121923004,14.2395160245118,
129.040888123246)) ;
#149123 = CARTESIAN_POINT('Ctrl Pts',(-29.331316063822,13.9900850970595,129.221281104942)) ;
#149124 = CARTESIAN_POINT('Ctrl Pts',(-29.3580576799696,13.7002631215164,
129.332511895375)) ;
#149125 = CARTESIAN_POINT('Ctrl Pts',(-29.3586251855949,13.3906063614652,
129.367283951049)) ;
#149126 = CARTESIAN_POINT('Ctrl Pts',(-29.332111341756,13.0826197728353,129.323015853458)) ;
#149127 = CARTESIAN_POINT('Ctrl Pts',(-29.2798112779405,12.799748141124,129.203343741946)) ;
#149128 = CARTESIAN_POINT('Ctrl Pts',(-29.2047720620516,12.5614903219102,
129.017238791305)) ;
#149129 = CARTESIAN_POINT('Ctrl Pts',(-29.1114211901215,12.3846250484045,
128.777697539592)) ;
#149130 = CARTESIAN_POINT('Ctrl Pts',(-29.0059135943882,12.2824688023076,
128.502620720195)) ;
#149131 = CARTESIAN_POINT('Ctrl Pts',(-28.8953832435428,12.2619556296945,
128.212772441659)) ;
#149132 = CARTESIAN_POINT('Ctrl Pts',(-28.7862638141337,12.3244284918516,
127.927167021378)) ;
#149133 = CARTESIAN_POINT('Ctrl Pts',(-28.6859244781036,12.4664339674621,
127.667281194282)) ;
#149134 = CARTESIAN_POINT('Ctrl Pts',(-28.601649102341,12.6753486557463,127.454052709534)) ;
#149135 = CARTESIAN_POINT('Ctrl Pts',(-28.5375143918303,12.9390313518122,
127.299872509753)) ;
#149136 = CARTESIAN_POINT('Ctrl Pts',(-28.4980517300494,13.2369182053758,
127.217692199479)) ;
#149137 = CARTESIAN_POINT('Ctrl Pts',(-28.4852684345572,13.5497742859679,
127.213631750286)) ;
#149138 = CARTESIAN_POINT('Ctrl Pts',(-28.4993005500257,13.8506093508767,
127.28757579924)) ;
#149139 = CARTESIAN_POINT('Ctrl Pts',(-28.5384951621769,14.1229208970494,
127.435261606474)) ;
#149140 = CARTESIAN_POINT('Ctrl Pts',(-28.599114960893,14.3440340084818,127.645398935015)) ;
#149141 = CARTESIAN_POINT('Ctrl Pts',(-28.6763470623928,14.5000650086301,
127.904155603546)) ;
#149142 = CARTESIAN_POINT('Ctrl Pts',(-28.7642922709141,14.5786444496306,
128.194360198328)) ;
#149143 = CARTESIAN_POINT('Ctrl Pts',(-28.8544048477181,14.5743811791395,
128.490498687061)) ;
#149144 = CARTESIAN_POINT('Ctrl Pts',(-28.9416453449683,14.4873599141627,
128.778661127787)) ;
#149145 = CARTESIAN_POINT('Ctrl Pts',(-29.0173714867235,14.3240887387416,
129.032983567367)) ;
#149146 = CARTESIAN_POINT('Ctrl Pts',(-29.0759121873307,14.0972553768965,
129.237016152545)) ;
#149147 = CARTESIAN_POINT('Ctrl Pts',(-29.1126883189575,13.8219068186535,
129.377531219329)) ;
#149148 = CARTESIAN_POINT('Ctrl Pts',(-29.1241085948694,13.5160257304535,
129.444183524273)) ;
#149149 = CARTESIAN_POINT('Ctrl Pts',(-29.1084287640549,13.2050738330625,
129.431492819495)) ;
#149150 = CARTESIAN_POINT('Ctrl Pts',(-29.0664893049883,12.9106474660782,
129.341984766231)) ;
#149151 = CARTESIAN_POINT('Ctrl Pts',(-29.000224510898,12.6518068845878,129.181529079168)) ;
#149152 = CARTESIAN_POINT('Ctrl Pts',(-28.9136374703434,12.4481718764226,
128.961732310351)) ;
#149153 = CARTESIAN_POINT('Ctrl Pts',(-28.8123624754787,12.314346622866,128.699007111475)) ;
#149154 = CARTESIAN_POINT('Ctrl Pts',(-28.7023901141071,12.2602411291599,
128.4110156196)) ;
#149155 = CARTESIAN_POINT('Ctrl Pts',(-28.5926670744185,12.289044210784,128.123343501971)) ;
#149156 = CARTESIAN_POINT('Ctrl Pts',(-28.4876267780401,12.3996398985986,
127.84978474962)) ;
#149157 = CARTESIAN_POINT('Ctrl Pts',(-28.3962438763497,12.5827969028938,
127.61585743653)) ;
#149158 = CARTESIAN_POINT('Ctrl Pts',(-28.3231203552759,12.8269629878668,
127.435435519098)) ;
#149159 = CARTESIAN_POINT('Ctrl Pts',(-28.2734596418954,13.1127056220744,
127.323400536975)) ;
#149160 = CARTESIAN_POINT('Ctrl Pts',(-28.2496308502148,13.4217118821407,
127.286956931971)) ;
#149161 = CARTESIAN_POINT('Ctrl Pts',(-28.2528361924696,13.73042511485,127.329433354869)) ;
#149162 = CARTESIAN_POINT('Ctrl Pts',(-28.2823066708455,14.0183443112805,
127.448796933238)) ;
#149163 = CARTESIAN_POINT('Ctrl Pts',(-28.3346958598102,14.2615011985034,
127.634845761707)) ;
#149164 = CARTESIAN_POINT('Ctrl Pts',(-28.4058819950025,14.4455241600489,
127.875911043545)) ;
#149165 = CARTESIAN_POINT('Ctrl Pts',(-28.4898905661539,14.5564730484766,
128.154399957566)) ;
#149166 = CARTESIAN_POINT('Ctrl Pts',(-28.5807055884456,14.5860332576142,
128.453018836069)) ;
#149167 = CARTESIAN_POINT('Ctrl Pts',(-28.6693097598626,14.5327319969804,
128.744739341118)) ;
#149168 = CARTESIAN_POINT('Ctrl Pts',(-28.7508832134965,14.3988255377981,
129.016374996236)) ;
#149169 = CARTESIAN_POINT('Ctrl Pts',(-28.8168463104849,14.1966329987979,
129.242018320441)) ;
#149170 = CARTESIAN_POINT('Ctrl Pts',(-28.8631468967079,13.9381995065902,
129.410426459371)) ;
#149171 = CARTESIAN_POINT('Ctrl Pts',(-28.8851222804496,13.64215083048,129.50782242196)) ;
#149172 = CARTESIAN_POINT('Ctrl Pts',(-28.8805504060926,13.3319748624789,
129.527502418803)) ;
#149173 = CARTESIAN_POINT('Ctrl Pts',(-28.8491918684474,13.0275242268779,
129.469008498518)) ;
#149174 = CARTESIAN_POINT('Ctrl Pts',(-28.7919506539434,12.7499513876655,
129.335103926236)) ;
#149175 = CARTESIAN_POINT('Ctrl Pts',(-28.7132681692753,12.5230806555812,
129.138248537529)) ;
#149176 = CARTESIAN_POINT('Ctrl Pts',(-28.6172910431696,12.3595163887299,
128.89099290087)) ;
#149177 = CARTESIAN_POINT('Ctrl Pts',(-28.5099858369398,12.2720601229367,
128.610740548863)) ;
#149178 = CARTESIAN_POINT('Ctrl Pts',(-28.3988746086419,12.2676665272562,
128.319307904433)) ;
#149179 = CARTESIAN_POINT('Ctrl Pts',(-28.2916704296753,12.3451447883363,
128.039067626911)) ;
#149180 = CARTESIAN_POINT('Ctrl Pts',(-28.1938030804671,12.5004781878849,
127.786370689149)) ;
#149181 = CARTESIAN_POINT('Ctrl Pts',(-28.1127625486316,12.7212076725333,
127.582685380892)) ;
#149182 = CARTESIAN_POINT('Ctrl Pts',(-28.0529273651762,12.9936144334216,
127.44113357359)) ;
#149183 = CARTESIAN_POINT('Ctrl Pts',(-28.0185364565288,13.2947836175078,
127.373668817087)) ;
#149184 = CARTESIAN_POINT('Ctrl Pts',(-28.0107408413296,13.6064067051063,
127.384044252762)) ;
#149185 = CARTESIAN_POINT('Ctrl Pts',(-28.0297193147551,13.9050216556666,
127.472646955327)) ;
#149186 = CARTESIAN_POINT('Ctrl Pts',(-28.073239487346,14.1686336001984,127.632890974336)) ;
#149187 = CARTESIAN_POINT('Ctrl Pts',(-28.1374216336648,14.378818223522,127.853475232984)) ;
#149188 = CARTESIAN_POINT('Ctrl Pts',(-28.2171034635145,14.520866250274,128.119384876184)) ;
#149189 = CARTESIAN_POINT('Ctrl Pts',(-28.3058570218466,14.5841619926364,
128.411824363996)) ;
#149190 = CARTESIAN_POINT('Ctrl Pts',(-28.3963167152646,14.5641966334699,
128.709179860555)) ;
#149191 = CARTESIAN_POINT('Ctrl Pts',(-28.4815558486508,14.4625802261662,
128.991316551239)) ;
#149192 = CARTESIAN_POINT('Ctrl Pts',(-28.5547405617564,14.2860055470816,
129.238296594858)) ;
#149193 = CARTESIAN_POINT('Ctrl Pts',(-28.6095231775212,14.0484512040757,
129.431382925857)) ;
#149194 = CARTESIAN_POINT('Ctrl Pts',(-28.6417291928216,13.7663469877686,
129.558524603165)) ;
#149195 = CARTESIAN_POINT('Ctrl Pts',(-28.6481036317158,13.4574608016115,
129.610440627955)) ;
#149196 = CARTESIAN_POINT('Ctrl Pts',(-28.6275137977541,13.1488899436826,
129.583281486172)) ;
#149197 = CARTESIAN_POINT('Ctrl Pts',(-28.5806601514756,12.8583365068185,
129.47957329379)) ;
#149198 = CARTESIAN_POINT('Ctrl Pts',(-28.5101080825143,12.6085157636358,
129.306619716631)) ;
#149199 = CARTESIAN_POINT('Ctrl Pts',(-28.4204678433571,12.4173946881525,
129.077837978652)) ;
#149200 = CARTESIAN_POINT('Ctrl Pts',(-28.3170957380088,12.2980452511377,
128.808995646945)) ;
#149201 = CARTESIAN_POINT('Ctrl Pts',(-28.2070141547135,12.2592457783441,
128.520489824639)) ;
#149202 = CARTESIAN_POINT('Ctrl Pts',(-28.0966798508768,12.3040208599772,
128.231400572317)) ;
#149203 = CARTESIAN_POINT('Ctrl Pts',(-27.9943480589568,12.42869393012,127.965511512337)) ;
#149204 = CARTESIAN_POINT('Ctrl Pts',(-27.9058058272702,12.6243589904513,
127.739953405032)) ;
#149205 = CARTESIAN_POINT('Ctrl Pts',(-27.8366054021169,12.8789083134422,
127.571086073474)) ;
#149206 = CARTESIAN_POINT('Ctrl Pts',(-27.7917969297281,13.1702260749438,
127.473192849682)) ;
#149207 = CARTESIAN_POINT('Ctrl Pts',(-27.7730507275345,13.4805036565043,
127.451546760695)) ;
#149208 = CARTESIAN_POINT('Ctrl Pts',(-27.7813694599879,13.7876510907378,
127.509064273961)) ;
#149209 = CARTESIAN_POINT('Ctrl Pts',(-27.8154365035927,14.0678452038592,
127.641730149674)) ;
#149210 = CARTESIAN_POINT('Ctrl Pts',(-27.8715485760057,14.3007432153336,
127.838599286977)) ;
#149211 = CARTESIAN_POINT('Ctrl Pts',(-27.9459217672765,14.4725786028925,
128.089102623514)) ;
#149212 = CARTESIAN_POINT('Ctrl Pts',(-28.0315487597573,14.5682598705244,
128.372281879499)) ;
#149213 = CARTESIAN_POINT('Ctrl Pts',(-28.1221926549195,14.582415300085,128.670208784852)) ;
#149214 = CARTESIAN_POINT('Ctrl Pts',(-28.2105289219673,14.5133615021942,
128.961420781404)) ;
#149215 = CARTESIAN_POINT('Ctrl Pts',(-28.2894313960368,14.3656856001402,
129.225113968176)) ;
#149216 = CARTESIAN_POINT('Ctrl Pts',(-28.3521146601827,14.1519224163712,
129.441208760275)) ;
#149217 = CARTESIAN_POINT('Ctrl Pts',(-28.3942042091648,13.8839966757843,
129.597426788259)) ;
#149218 = CARTESIAN_POINT('Ctrl Pts',(-28.411183496847,13.5839687082689,129.680149626296)) ;
#149219 = CARTESIAN_POINT('Ctrl Pts',(-28.4015693530436,13.2736212101871,
129.685068948691)) ;
#149220 = CARTESIAN_POINT('Ctrl Pts',(-28.3652283835743,12.972761740788,129.612034453461)) ;
#149221 = CARTESIAN_POINT('Ctrl Pts',(-28.3037016460954,12.7034621724925,
129.465528552906)) ;
#149222 = CARTESIAN_POINT('Ctrl Pts',(-28.2211593027135,12.4867212726039,
129.257507750308)) ;
#149223 = CARTESIAN_POINT('Ctrl Pts',(-28.1224616177338,12.33686375234,129.00233956032)) ;
#149224 = CARTESIAN_POINT('Ctrl Pts',(-28.0144538218038,12.2650347020363,
128.719854075902)) ;
#149225 = CARTESIAN_POINT('Ctrl Pts',(-27.903322484762,12.2758062427332,128.428381261578)) ;
#149226 = CARTESIAN_POINT('Ctrl Pts',(-27.7966709347457,12.3692806824326,
128.150022376286)) ;
#149227 = CARTESIAN_POINT('Ctrl Pts',(-27.7018440324355,12.5378928700438,
127.90609386885)) ;
#149228 = CARTESIAN_POINT('Ctrl Pts',(-27.6245512268183,12.7694276671961,
127.71335608596)) ;
#149229 = CARTESIAN_POINT('Ctrl Pts',(-27.5693299508102,13.0484835222186,
127.585194618187)) ;
#149230 = CARTESIAN_POINT('Ctrl Pts',(-27.5397791508547,13.3553251323831,
127.532112766213)) ;
#149231 = CARTESIAN_POINT('Ctrl Pts',(-27.5372330226569,13.6640555528138,
127.557595480549)) ;
#149232 = CARTESIAN_POINT('Ctrl Pts',(-27.5609754676578,13.9577070020221,
127.660108078298)) ;
#149233 = CARTESIAN_POINT('Ctrl Pts',(-27.6087555543691,14.2128779574234,
127.832817362159)) ;
#149234 = CARTESIAN_POINT('Ctrl Pts',(-27.6765781719764,14.4117544090383,
128.06416116346)) ;
#149235 = CARTESIAN_POINT('Ctrl Pts',(-27.7582934482354,14.5391282978367,
128.335923995923)) ;
#149236 = CARTESIAN_POINT('Ctrl Pts',(-27.8482168316244,14.5867879388137,
128.631877918567)) ;
#149237 = CARTESIAN_POINT('Ctrl Pts',(-27.9378092608112,14.5512051558335,
128.926543960514)) ;
#149238 = CARTESIAN_POINT('Ctrl Pts',(-28.0215701238513,14.4343419868163,
129.204490622999)) ;
#149239 = CARTESIAN_POINT('Ctrl Pts',(-28.0914436828456,14.2455278890041,
129.441668406184)) ;
#149240 = CARTESIAN_POINT('Ctrl Pts',(-28.14235674795,13.9981929113896,129.623467068814)) ;
#149241 = CARTESIAN_POINT('Ctrl Pts',(-28.1698989580778,13.7085066713852,
129.737123007789)) ;
#149242 = CARTESIAN_POINT('Ctrl Pts',(-28.1711628301339,13.399579397686,129.773878387293)) ;
#149243 = CARTESIAN_POINT('Ctrl Pts',(-28.1455841160295,13.0919774800644,
129.732252462512)) ;
#149244 = CARTESIAN_POINT('Ctrl Pts',(-28.093714453794,12.8067303941414,129.614004992358)) ;
#149245 = CARTESIAN_POINT('Ctrl Pts',(-28.019645857162,12.5682009002538,129.430560739033)) ;
#149246 = CARTESIAN_POINT('Ctrl Pts',(-27.9266142891176,12.3888212381261,
129.192018455593)) ;
#149247 = CARTESIAN_POINT('Ctrl Pts',(-27.821510585854,12.2844119567793,128.918075924403)) ;
#149248 = CARTESIAN_POINT('Ctrl Pts',(-27.7106897292081,12.2613333921228,
128.62748362164)) ;
#149249 = CARTESIAN_POINT('Ctrl Pts',(-27.6015516143989,12.3215794364131,
128.341786595649)) ;
#149250 = CARTESIAN_POINT('Ctrl Pts',(-27.5011797769738,12.460691871722,128.081688658565)) ;
#149251 = CARTESIAN_POINT('Ctrl Pts',(-27.4159829565428,12.6684213350559,
127.865897041431)) ;
#149252 = CARTESIAN_POINT('Ctrl Pts',(-27.3510487739651,12.9319194586172,
127.709496777072)) ;
#149253 = CARTESIAN_POINT('Ctrl Pts',(-27.3111098739424,13.227908152673,127.625786027641)) ;
#149254 = CARTESIAN_POINT('Ctrl Pts',(-27.2974612593413,13.5392232276546,
127.619043390422)) ;
#149255 = CARTESIAN_POINT('Ctrl Pts',(-27.3107067357766,13.842168223521,127.690850798586)) ;
#149256 = CARTESIAN_POINT('Ctrl Pts',(-27.3492738204767,14.115831938889,127.836726726766)) ;
#149257 = CARTESIAN_POINT('Ctrl Pts',(-27.4094876845083,14.3390092448437,
128.045746045153)) ;
#149258 = CARTESIAN_POINT('Ctrl Pts',(-27.4862037303775,14.4964745213525,
128.302922976793)) ;
#149259 = CARTESIAN_POINT('Ctrl Pts',(-27.5734126890435,14.5773715613601,
128.590785930487)) ;
#149260 = CARTESIAN_POINT('Ctrl Pts',(-27.6642277201677,14.5757025452078,
128.889231125655)) ;
#149261 = CARTESIAN_POINT('Ctrl Pts',(-27.7514325880381,14.4908671565799,
129.177203535286)) ;
#149262 = CARTESIAN_POINT('Ctrl Pts',(-27.8273172084641,14.3305923822081,
129.431861219863)) ;
#149263 = CARTESIAN_POINT('Ctrl Pts',(-27.8867448350719,14.104809150226,129.638607059385)) ;
#149264 = CARTESIAN_POINT('Ctrl Pts',(-27.924232723082,13.8293692517449,129.781327493485)) ;
#149265 = CARTESIAN_POINT('Ctrl Pts',(-27.9363393689926,13.5265764588792,
129.849706205578)) ;
#149266 = CARTESIAN_POINT('Ctrl Pts',(-27.9215766706455,13.2147295864641,
129.839779247584)) ;
#149267 = CARTESIAN_POINT('Ctrl Pts',(-27.8803348251946,12.9189025959915,
129.752369876601)) ;
#149268 = CARTESIAN_POINT('Ctrl Pts',(-27.8144585897609,12.6580300058624,
129.593157007656)) ;
#149269 = CARTESIAN_POINT('Ctrl Pts',(-27.7287463868753,12.4534346092271,
129.375772364678)) ;
#149270 = CARTESIAN_POINT('Ctrl Pts',(-27.6275620489468,12.3171076875182,
129.113399636911)) ;
#149271 = CARTESIAN_POINT('Ctrl Pts',(-27.518308419636,12.2606844041001,128.827331139409)) ;
#149272 = CARTESIAN_POINT('Ctrl Pts',(-27.4077125727585,12.28708894542,128.537351097586)) ;
#149273 = CARTESIAN_POINT('Ctrl Pts',(-27.3024709202027,12.3957982979784,
128.26319136607)) ;
#149274 = CARTESIAN_POINT('Ctrl Pts',(-27.2108581166926,12.5767256931705,
128.02852604486)) ;
#149275 = CARTESIAN_POINT('Ctrl Pts',(-27.1372315199395,12.8186993090181,
127.846557861036)) ;
#149276 = CARTESIAN_POINT('Ctrl Pts',(-27.0866060204049,13.1050418122632,
127.73188330392)) ;
#149277 = CARTESIAN_POINT('Ctrl Pts',(-27.062162804843,13.4130762774239,127.693567342574)) ;
#149278 = CARTESIAN_POINT('Ctrl Pts',(-27.0646120500407,13.7214651922854,
127.733776018884)) ;
#149279 = CARTESIAN_POINT('Ctrl Pts',(-27.0931056884195,14.0093161803211,
127.850144303508)) ;
#149280 = CARTESIAN_POINT('Ctrl Pts',(-27.1453032721948,14.2560736745197,
128.035916176362)) ;
#149281 = CARTESIAN_POINT('Ctrl Pts',(-27.2158872721112,14.4412184324741,
128.275118516804)) ;
#149282 = CARTESIAN_POINT('Ctrl Pts',(-27.2996010171685,14.5543182486296,
128.552747603182)) ;
#149283 = CARTESIAN_POINT('Ctrl Pts',(-27.3899118087328,14.5864671226158,
128.84973273768)) ;
#149284 = CARTESIAN_POINT('Ctrl Pts',(-27.4792618290635,14.5351930483474,
129.14386643155)) ;
#149285 = CARTESIAN_POINT('Ctrl Pts',(-27.560663470632,14.4042256836979,129.414791679736)) ;
#149286 = CARTESIAN_POINT('Ctrl Pts',(-27.6274454081149,14.2033620376663,
129.642954413426)) ;
#149287 = CARTESIAN_POINT('Ctrl Pts',(-27.6743631483564,13.9460943554148,
129.81317254965)) ;
#149288 = CARTESIAN_POINT('Ctrl Pts',(-27.697059062296,13.6510940707038,129.912646290026)) ;
#149289 = CARTESIAN_POINT('Ctrl Pts',(-27.6932988178505,13.340963323575,129.934704831616)) ;
#149290 = CARTESIAN_POINT('Ctrl Pts',(-27.6625764453814,13.0355469770442,
129.878128940385)) ;
#149291 = CARTESIAN_POINT('Ctrl Pts',(-27.6064258233987,12.7584810816834,
129.747205231254)) ;
#149292 = CARTESIAN_POINT('Ctrl Pts',(-27.5280729952501,12.5287899159639,
129.551452346458)) ;
#149293 = CARTESIAN_POINT('Ctrl Pts',(-27.4324998329583,12.3633457442531,
129.305367372387)) ;
#149294 = CARTESIAN_POINT('Ctrl Pts',(-27.3258016217117,12.2737023514909,
129.026778387411)) ;
#149295 = CARTESIAN_POINT('Ctrl Pts',(-27.21466759507,12.2663504443872,128.73528774347)) ;
#149296 = CARTESIAN_POINT('Ctrl Pts',(-27.1066093889239,12.3420800967331,
128.452760176601)) ;
#149297 = CARTESIAN_POINT('Ctrl Pts',(-27.0088321504467,12.4946575605773,
128.200166185438)) ;
#149298 = CARTESIAN_POINT('Ctrl Pts',(-26.9269407651993,12.7142648856192,
127.994104420372)) ;
#149299 = CARTESIAN_POINT('Ctrl Pts',(-26.8665124531143,12.9853993961476,
127.850796596108)) ;
#149300 = CARTESIAN_POINT('Ctrl Pts',(-26.8313430052465,13.2860373557687,
127.781066453358)) ;
#149301 = CARTESIAN_POINT('Ctrl Pts',(-26.8227999641649,13.5985521220417,
127.789346344921)) ;
#149302 = CARTESIAN_POINT('Ctrl Pts',(-26.8411427705591,13.8975127829307,
127.876068717954)) ;
#149303 = CARTESIAN_POINT('Ctrl Pts',(-26.8838031630307,14.1612605834451,
128.033657379763)) ;
#149304 = CARTESIAN_POINT('Ctrl Pts',(-26.9476004607464,14.3739607965711,
128.253212935099)) ;
#149305 = CARTESIAN_POINT('Ctrl Pts',(-27.0272151946275,14.5182946770733,
128.519024634964)) ;
#149306 = CARTESIAN_POINT('Ctrl Pts',(-27.1156612052403,14.5834512789115,
128.810503268048)) ;
#149307 = CARTESIAN_POINT('Ctrl Pts',(-27.2058710054321,14.5659482327596,
129.107021227185)) ;
#149308 = CARTESIAN_POINT('Ctrl Pts',(-27.2913403326924,14.4667698012676,
129.389820244375)) ;
#149309 = CARTESIAN_POINT('Ctrl Pts',(-27.365037513102,14.2923286042259,129.638305562232)) ;
#149310 = CARTESIAN_POINT('Ctrl Pts',(-27.4206675378827,14.0548140829524,
129.834057411563)) ;
#149311 = CARTESIAN_POINT('Ctrl Pts',(-27.4532942174668,13.7751054623822,
129.962249175486)) ;
#149312 = CARTESIAN_POINT('Ctrl Pts',(-27.4605705712052,13.4671707180117,
130.016748758532)) ;
#149313 = CARTESIAN_POINT('Ctrl Pts',(-27.4405768382025,13.1566326950211,
129.99151897037)) ;
#149314 = CARTESIAN_POINT('Ctrl Pts',(-27.3947125191724,12.867030876862,129.890495120701)) ;
#149315 = CARTESIAN_POINT('Ctrl Pts',(-27.3246005780535,12.6146257470566,
129.718955677147)) ;
#149316 = CARTESIAN_POINT('Ctrl Pts',(-27.2352104972191,12.4216271704312,
129.490959132207)) ;
#149317 = CARTESIAN_POINT('Ctrl Pts',(-27.1326277544319,12.300493633533,129.224268899247)) ;
#149318 = CARTESIAN_POINT('Ctrl Pts',(-27.0220193247481,12.2591976943658,
128.934414356228)) ;
#149319 = CARTESIAN_POINT('Ctrl Pts',(-26.9123324711744,12.3014766472521,
128.646990110332)) ;
#149320 = CARTESIAN_POINT('Ctrl Pts',(-26.8094227622297,12.4236752420719,
128.379476345014)) ;
#149321 = CARTESIAN_POINT('Ctrl Pts',(-26.7198695890128,12.619137551761,128.151191815619)) ;
#149322 = CARTESIAN_POINT('Ctrl Pts',(-26.6505624975948,12.8707902283033,
127.981794105051)) ;
#149323 = CARTESIAN_POINT('Ctrl Pts',(-26.6049003931584,13.1617413070734,
127.881471015381)) ;
#149324 = CARTESIAN_POINT('Ctrl Pts',(-26.5854473892697,13.4713352459494,
127.857705276412)) ;
#149325 = CARTESIAN_POINT('Ctrl Pts',(-26.5929490593232,13.778502178637,127.912793617474)) ;
#149326 = CARTESIAN_POINT('Ctrl Pts',(-26.6261889122264,14.0596468984735,
128.043011359952)) ;
#149327 = CARTESIAN_POINT('Ctrl Pts',(-26.6819953534812,14.2953142204187,
128.239156752771)) ;
#149328 = CARTESIAN_POINT('Ctrl Pts',(-26.7559539371804,14.4689647045759,
128.488434863537)) ;
#149329 = CARTESIAN_POINT('Ctrl Pts',(-26.8416162758305,14.5668407202151,
128.771816073632)) ;
#149330 = CARTESIAN_POINT('Ctrl Pts',(-26.9317772171447,14.5831863672356,
129.06816269229)) ;
#149331 = CARTESIAN_POINT('Ctrl Pts',(-27.0206452753331,14.5160479467046,
129.361074683035)) ;
#149332 = CARTESIAN_POINT('Ctrl Pts',(-27.0994865478493,14.371057406114,129.624417159767)) ;
#149333 = CARTESIAN_POINT('Ctrl Pts',(-27.1628566341757,14.1586832935138,
129.842590444057)) ;
#149334 = CARTESIAN_POINT('Ctrl Pts',(-27.2054989868208,13.8924169027706,
130.000362090636)) ;
#149335 = CARTESIAN_POINT('Ctrl Pts',(-27.223288580354,13.5934591668299,130.085415073904)) ;
#149336 = CARTESIAN_POINT('Ctrl Pts',(-27.2144128625738,13.2817950572783,
130.092631458139)) ;
#149337 = CARTESIAN_POINT('Ctrl Pts',(-27.1787460156679,12.9807521840059,
130.021531190684)) ;
#149338 = CARTESIAN_POINT('Ctrl Pts',(-27.1182536558926,12.7114089548823,
129.877887175819)) ;
#149339 = CARTESIAN_POINT('Ctrl Pts',(-27.0359874106081,12.4920356351317,
129.670798191775)) ;
#149340 = CARTESIAN_POINT('Ctrl Pts',(-26.9379376281562,12.3404092688171,
129.417431448621)) ;
#149341 = CARTESIAN_POINT('Ctrl Pts',(-26.829743084675,12.2658594334509,129.134518780991)) ;
#149342 = CARTESIAN_POINT('Ctrl Pts',(-26.7187403880943,12.2744067631739,
128.843375453836)) ;
#149343 = CARTESIAN_POINT('Ctrl Pts',(-26.6121463544767,12.3651073313828,
128.565090827221)) ;
#149344 = CARTESIAN_POINT('Ctrl Pts',(-26.5167176009969,12.5316552187529,
128.319448476852)) ;
#149345 = CARTESIAN_POINT('Ctrl Pts',(-26.4386322226201,12.7621960771077,
128.124482385513)) ;
#149346 = CARTESIAN_POINT('Ctrl Pts',(-26.3828261298418,13.0400248542652,
127.994587296118)) ;
#149347 = CARTESIAN_POINT('Ctrl Pts',(-26.3525190565265,13.3449924415224,
127.939149409341)) ;
#149348 = CARTESIAN_POINT('Ctrl Pts',(-26.3491468760843,13.6560823827408,
127.962454240853)) ;
#149349 = CARTESIAN_POINT('Ctrl Pts',(-26.372164679168,13.9495229886617,128.062741811689)) ;
#149350 = CARTESIAN_POINT('Ctrl Pts',(-26.4192453975585,14.2060601785511,
128.233401209434)) ;
#149351 = CARTESIAN_POINT('Ctrl Pts',(-26.4865387051378,14.406853356067,128.463190725204)) ;
#149352 = CARTESIAN_POINT('Ctrl Pts',(-26.568036262976,14.5364834433348,128.734360307803)) ;
#149353 = CARTESIAN_POINT('Ctrl Pts',(-26.6574616375403,14.5865952299809,
129.028720457278)) ;
#149354 = CARTESIAN_POINT('Ctrl Pts',(-26.7476261509057,14.5532896957255,
129.325240815001)) ;
#149355 = CARTESIAN_POINT('Ctrl Pts',(-26.831290016583,14.4391769984152,129.602746393984)) ;
#149356 = CARTESIAN_POINT('Ctrl Pts',(-26.9018234679493,14.2521193913653,
129.841924000037)) ;
#149357 = CARTESIAN_POINT('Ctrl Pts',(-26.953372839476,14.0064609984077,130.025559364404)) ;
#149358 = CARTESIAN_POINT('Ctrl Pts',(-26.9817302296853,13.7162751815943,
130.14175646995)) ;
#149359 = CARTESIAN_POINT('Ctrl Pts',(-26.9837110537891,13.4088590373153,
130.18046815682)) ;
#149360 = CARTESIAN_POINT('Ctrl Pts',(-26.9588874732449,13.1005339058846,
130.141091745965)) ;
#149361 = CARTESIAN_POINT('Ctrl Pts',(-26.907970796887,12.8153801533597,130.025495563498)) ;
#149362 = CARTESIAN_POINT('Ctrl Pts',(-26.8343613372862,12.5742829537778,
129.843499520031)) ;
#149363 = CARTESIAN_POINT('Ctrl Pts',(-26.7412853262,12.392420790546,129.604979348717)) ;
#149364 = CARTESIAN_POINT('Ctrl Pts',(-26.6369717859904,12.2864008615048,
129.333172629999)) ;
#149365 = CARTESIAN_POINT('Ctrl Pts',(-26.5258572296115,12.2608494064564,
129.041832035797)) ;
#149366 = CARTESIAN_POINT('Ctrl Pts',(-26.4170347717267,12.3186106427626,
128.756917900028)) ;
#149367 = CARTESIAN_POINT('Ctrl Pts',(-26.3160996326238,12.4554522853447,
128.495226419321)) ;
#149368 = CARTESIAN_POINT('Ctrl Pts',(-26.2301003884934,12.6626734835884,
128.277242969498)) ;
#149369 = CARTESIAN_POINT('Ctrl Pts',(-26.1651571607187,12.9221025323028,
128.120471859074)) ;
#149370 = CARTESIAN_POINT('Ctrl Pts',(-26.1240596389376,13.2188657935947,
128.033566809399)) ;
#149371 = CARTESIAN_POINT('Ctrl Pts',(-26.1097033403075,13.5309968714097,
128.024847539681)) ;
#149372 = CARTESIAN_POINT('Ctrl Pts',(-26.1221635460237,13.833390940375,128.094243989074)) ;
#149373 = CARTESIAN_POINT('Ctrl Pts',(-26.1599919314982,14.1082731705155,
128.237962010862)) ;
#149374 = CARTESIAN_POINT('Ctrl Pts',(-26.2196288030865,14.3332733281916,
128.445300705723)) ;
#149375 = CARTESIAN_POINT('Ctrl Pts',(-26.2961210056048,14.4930898845826,
128.701897547713)) ;
#149376 = CARTESIAN_POINT('Ctrl Pts',(-26.3830264974971,14.5762694584335,
128.988831295629)) ;
#149377 = CARTESIAN_POINT('Ctrl Pts',(-26.4741788643102,14.5766426622739,
129.288393030434)) ;
#149378 = CARTESIAN_POINT('Ctrl Pts',(-26.5608022072879,14.4950562230295,
129.57435464937)) ;
#149379 = CARTESIAN_POINT('Ctrl Pts',(-26.6377807342573,14.3357813404639,
129.832489798271)) ;
#149380 = CARTESIAN_POINT('Ctrl Pts',(-26.6975264006213,14.1117727148765,
130.040093620744)) ;
#149381 = CARTESIAN_POINT('Ctrl Pts',(-26.7356954570761,13.8385113362907,
130.184699682537)) ;
#149382 = CARTESIAN_POINT('Ctrl Pts',(-26.7485655418517,13.5338963360909,
130.255564378225)) ;
#149383 = CARTESIAN_POINT('Ctrl Pts',(-26.7346407265886,13.2242576561067,
130.247831508955)) ;
#149384 = CARTESIAN_POINT('Ctrl Pts',(-26.6939418479399,12.9262819739174,
130.162178455022)) ;
#149385 = CARTESIAN_POINT('Ctrl Pts',(-26.6291144483335,12.6654698991639,
130.005833635842)) ;
#149386 = CARTESIAN_POINT('Ctrl Pts',(-26.5431047888369,12.4574146452965,
129.787885297242)) ;
#149387 = CARTESIAN_POINT('Ctrl Pts',(-26.443309400981,12.3205165730399,129.529210198504)) ;
#149388 = CARTESIAN_POINT('Ctrl Pts',(-26.3336075645494,12.2610390486759,
129.242027806129)) ;
#149389 = CARTESIAN_POINT('Ctrl Pts',(-26.2233061878199,12.2851065048332,
128.952795655811)) ;
#149390 = CARTESIAN_POINT('Ctrl Pts',(-26.1176723705432,12.3913707363663,
128.677523801392)) ;
#149391 = CARTESIAN_POINT('Ctrl Pts',(-26.025506878235,12.5705078611999,128.441274776628)) ;
#149392 = CARTESIAN_POINT('Ctrl Pts',(-25.9512744951246,12.8110530748773,
128.257547459859)) ;
#149393 = CARTESIAN_POINT('Ctrl Pts',(-25.8999845865538,13.0958080893831,
128.140865241115)) ;
#149394 = CARTESIAN_POINT('Ctrl Pts',(-25.8746957774511,13.4043791335754,
128.100179674998)) ;
#149395 = CARTESIAN_POINT('Ctrl Pts',(-25.8763352309333,13.7127503625776,
128.137978637021)) ;
#149396 = CARTESIAN_POINT('Ctrl Pts',(-25.9044463776869,14.003146544252,128.253450200463)) ;
#149397 = CARTESIAN_POINT('Ctrl Pts',(-25.9553220324677,14.2480984913921,
128.434908631351)) ;
#149398 = CARTESIAN_POINT('Ctrl Pts',(-26.0258527600041,14.4370589151547,
128.67421395397)) ;
#149399 = CARTESIAN_POINT('Ctrl Pts',(-26.1092792616536,14.5521322459825,
128.950981738852)) ;
#149400 = CARTESIAN_POINT('Ctrl Pts',(-26.199596367935,14.5867077629414,129.248023960277)) ;
#149401 = CARTESIAN_POINT('Ctrl Pts',(-26.2889097076484,14.5378478997284,
129.541988386777)) ;
#149402 = CARTESIAN_POINT('Ctrl Pts',(-26.3706225884636,14.4092030440239,
129.813815833598)) ;
#149403 = CARTESIAN_POINT('Ctrl Pts',(-26.4379731393695,14.2102655467961,
130.043646526883)) ;
#149404 = CARTESIAN_POINT('Ctrl Pts',(-26.4856636420017,13.9531165249686,
130.216267974669)) ;
#149405 = CARTESIAN_POINT('Ctrl Pts',(-26.5089520228723,13.6605445823028,
130.31728180732)) ;
#149406 = CARTESIAN_POINT('Ctrl Pts',(-26.505983006858,13.3493860420966,130.341784421963)) ;
#149407 = CARTESIAN_POINT('Ctrl Pts',(-26.4760795773027,13.0444136066678,
130.287498366656)) ;
#149408 = CARTESIAN_POINT('Ctrl Pts',(-26.4205900967314,12.7658509592001,
130.158551123139)) ;
#149409 = CARTESIAN_POINT('Ctrl Pts',(-26.3428502090789,12.5346699181632,
129.964569939688)) ;
#149410 = CARTESIAN_POINT('Ctrl Pts',(-26.2475525447978,12.3668713397562,
129.719341661414)) ;
#149411 = CARTESIAN_POINT('Ctrl Pts',(-26.1408738407262,12.2750736667704,
129.440865631469)) ;
#149412 = CARTESIAN_POINT('Ctrl Pts',(-26.0303295842009,12.2654123740739,
129.150928666223)) ;
#149413 = CARTESIAN_POINT('Ctrl Pts',(-25.9220058556232,12.338500075334,128.867642928314)) ;
#149414 = CARTESIAN_POINT('Ctrl Pts',(-25.823580121359,12.4893940348924,128.613242211606)) ;
#149415 = CARTESIAN_POINT('Ctrl Pts',(-25.7412693678322,12.7071834548376,
128.405922936625)) ;
#149416 = CARTESIAN_POINT('Ctrl Pts',(-25.6802965616572,12.9760085814995,
128.26090587194)) ;
#149417 = CARTESIAN_POINT('Ctrl Pts',(-25.6441923860615,13.2771670277102,
128.188575058199)) ;
#149418 = CARTESIAN_POINT('Ctrl Pts',(-25.6348985777501,13.5885362669385,
128.194535927645)) ;
#149419 = CARTESIAN_POINT('Ctrl Pts',(-25.6523328897567,13.8883473983697,
128.278609254777)) ;
#149420 = CARTESIAN_POINT('Ctrl Pts',(-25.6945375325596,14.1546796544185,
128.435029104442)) ;
#149421 = CARTESIAN_POINT('Ctrl Pts',(-25.7576722938783,14.3683944607912,
128.652558927551)) ;
#149422 = CARTESIAN_POINT('Ctrl Pts',(-25.8365524919284,14.5146640106003,
128.916097753154)) ;
#149423 = CARTESIAN_POINT('Ctrl Pts',(-25.9251110929857,14.5827891509108,
129.208019589231)) ;
#149424 = CARTESIAN_POINT('Ctrl Pts',(-26.015573321456,14.5676066114005,129.505349333004)) ;
#149425 = CARTESIAN_POINT('Ctrl Pts',(-26.1012556109092,14.4706131467255,
129.788764317248)) ;
#149426 = CARTESIAN_POINT('Ctrl Pts',(-26.1751826362596,14.2987449409649,
130.037825229019)) ;
#149427 = CARTESIAN_POINT('Ctrl Pts',(-26.231476999422,14.063095845739,130.235510412299)) ;
#149428 = CARTESIAN_POINT('Ctrl Pts',(-26.2649721046301,13.783320877813,130.36636990385)) ;
#149429 = CARTESIAN_POINT('Ctrl Pts',(-26.2729003428569,13.4754883561184,
130.422804556592)) ;
#149430 = CARTESIAN_POINT('Ctrl Pts',(-26.2538588179999,13.1664273020677,
130.400169807561)) ;
#149431 = CARTESIAN_POINT('Ctrl Pts',(-26.2084817055547,12.8743475374644,
130.30075703385)) ;
#149432 = CARTESIAN_POINT('Ctrl Pts',(-26.1393771918487,12.6220180754337,
130.131968605388)) ;
#149433 = CARTESIAN_POINT('Ctrl Pts',(-26.0504026601184,12.4263341505379,
129.905252967717)) ;
#149434 = CARTESIAN_POINT('Ctrl Pts',(-25.947535881916,12.3026056588691,129.637908781085)) ;
#149435 = CARTESIAN_POINT('Ctrl Pts',(-25.8376937080852,12.2593725245785,
129.350094272485)) ;
#149436 = CARTESIAN_POINT('Ctrl Pts',(-25.7277681341655,12.2987734031186,
129.062003328986)) ;
#149437 = CARTESIAN_POINT('Ctrl Pts',(-25.6238087024035,12.4202091784099,
128.791687112019)) ;
#149438 = CARTESIAN_POINT('Ctrl Pts',(-25.5347909469648,12.6117736557302,
128.564597278483)) ;
#149439 = CARTESIAN_POINT('Ctrl Pts',(-25.4644647312364,12.8626551517495,
128.392353071568)) ;
#149440 = CARTESIAN_POINT('Ctrl Pts',(-25.4181059842558,13.1527448205317,
128.289985266207)) ;
#149441 = CARTESIAN_POINT('Ctrl Pts',(-25.3978265921149,13.4624297632054,
128.26384262381)) ;
#149442 = CARTESIAN_POINT('Ctrl Pts',(-25.4046046149136,13.7701810558333,
128.316837011734)) ;
#149443 = CARTESIAN_POINT('Ctrl Pts',(-25.4370679406513,14.0517728078933,
128.444718605914)) ;
#149444 = CARTESIAN_POINT('Ctrl Pts',(-25.4922811148997,14.2892526496134,
128.639150351661)) ;
#149445 = CARTESIAN_POINT('Ctrl Pts',(-25.5658191040767,14.4648239971076,
128.887203395093)) ;
#149446 = CARTESIAN_POINT('Ctrl Pts',(-25.6509413981458,14.5650402955601,
129.168902206863)) ;
#149447 = CARTESIAN_POINT('Ctrl Pts',(-25.7416323438765,14.5837489624633,
129.467013900429)) ;
#149448 = CARTESIAN_POINT('Ctrl Pts',(-25.8298583850632,14.5197168158782,
129.75773720294)) ;
#149449 = CARTESIAN_POINT('Ctrl Pts',(-25.9096537578399,14.3763315271282,
130.024093124728)) ;
#149450 = CARTESIAN_POINT('Ctrl Pts',(-25.973514050232,14.1656646034779,130.243682507277)) ;
#149451 = CARTESIAN_POINT('Ctrl Pts',(-26.0168945296712,13.8999129369224,
130.403701320786)) ;
#149452 = CARTESIAN_POINT('Ctrl Pts',(-26.0353238984872,13.6028236441132,
130.490484775464)) ;
#149453 = CARTESIAN_POINT('Ctrl Pts',(-26.0272964629209,13.291184662554,130.500185473863)) ;
#149454 = CARTESIAN_POINT('Ctrl Pts',(-25.9924298041082,12.9894031508225,
130.431429463874)) ;
#149455 = CARTESIAN_POINT('Ctrl Pts',(-25.9323345518416,12.7177660513116,
130.289085423949)) ;
#149456 = CARTESIAN_POINT('Ctrl Pts',(-25.8506637020188,12.4972590440602,
130.083685272878)) ;
#149457 = CARTESIAN_POINT('Ctrl Pts',(-25.7532768706347,12.3438957808923,
129.832165172526)) ;
#149458 = CARTESIAN_POINT('Ctrl Pts',(-25.6451767858764,12.2668705331881,
129.549560973497)) ;
#149459 = CARTESIAN_POINT('Ctrl Pts',(-25.5342771990314,12.2729077976525,
129.258679649349)) ;
#149460 = CARTESIAN_POINT('Ctrl Pts',(-25.4272944138605,12.3614501040313,
128.979314451413)) ;
#149461 = CARTESIAN_POINT('Ctrl Pts',(-25.3316928534878,12.5253314471916,
128.733068601897)) ;
#149462 = CARTESIAN_POINT('Ctrl Pts',(-25.2526702517292,12.7552769702176,
128.535519977571)) ;
#149463 = CARTESIAN_POINT('Ctrl Pts',(-25.1963868103433,13.0310568986237,
128.404108114085)) ;
#149464 = CARTESIAN_POINT('Ctrl Pts',(-25.1652356923081,13.3361216893249,
128.346276085526)) ;
#149465 = CARTESIAN_POINT('Ctrl Pts',(-25.1610447906198,13.6463104400421,
128.367071713508)) ;
#149466 = CARTESIAN_POINT('Ctrl Pts',(-25.1834279122032,13.9424873380838,
128.465719369502)) ;
#149467 = CARTESIAN_POINT('Ctrl Pts',(-25.2300651046473,14.2002008792275,
128.63510490389)) ;
#149468 = CARTESIAN_POINT('Ctrl Pts',(-25.2964021821312,14.4015262359145,
128.861882102586)) ;
#149469 = CARTESIAN_POINT('Ctrl Pts',(-25.377774803287,14.5339054889456,129.132784185914)) ;
#149470 = CARTESIAN_POINT('Ctrl Pts',(-25.4670176153515,14.5863178639959,
129.426586569099)) ;
#149471 = CARTESIAN_POINT('Ctrl Pts',(-25.5575016604959,14.5553221796482,
129.724127530759)) ;
#149472 = CARTESIAN_POINT('Ctrl Pts',(-25.6413823541268,14.4431215079252,
130.002261657312)) ;
#149473 = CARTESIAN_POINT('Ctrl Pts',(-25.7121297022502,14.2589451950462,
130.241921219066)) ;
#149474 = CARTESIAN_POINT('Ctrl Pts',(-25.7645376943468,14.0132050908334,
130.428265572224)) ;
#149475 = CARTESIAN_POINT('Ctrl Pts',(-25.7934072860426,13.7264814717307,
130.545664324976)) ;
#149476 = CARTESIAN_POINT('Ctrl Pts',(-25.7962481463893,13.4166671207193,
130.587186681068)) ;
#149477 = CARTESIAN_POINT('Ctrl Pts',(-25.7721344714061,13.1090562113246,
130.549771064034)) ;
#149478 = CARTESIAN_POINT('Ctrl Pts',(-25.721972342848,12.8228936758021,130.436381366975)) ;
#149479 = CARTESIAN_POINT('Ctrl Pts',(-25.648887215864,12.5803482632518,130.255929141698)) ;
#149480 = CARTESIAN_POINT('Ctrl Pts',(-25.5567250208858,12.3971382948885,
130.019928622796)) ;
#149481 = CARTESIAN_POINT('Ctrl Pts',(-25.4521561710051,12.2881794831016,
129.747548587076)) ;
#149482 = CARTESIAN_POINT('Ctrl Pts',(-25.341278028209,12.260444772771,129.45684395212)) ;
#149483 = CARTESIAN_POINT('Ctrl Pts',(-25.2320854545694,12.3158800352752,
129.170914587755)) ;
#149484 = CARTESIAN_POINT('Ctrl Pts',(-25.1307342445682,12.4512315889953,
128.908061261342)) ;
#149485 = CARTESIAN_POINT('Ctrl Pts',(-25.0449098942256,12.6546809056087,
128.690298448963)) ;
#149486 = CARTESIAN_POINT('Ctrl Pts',(-24.9787438302227,12.9147730695688,
128.53022636553)) ;
#149487 = CARTESIAN_POINT('Ctrl Pts',(-24.9371546931072,13.2095558762223,
128.441731585585)) ;
#149488 = CARTESIAN_POINT('Ctrl Pts',(-24.9219358688328,13.5223873446286,
128.430586778961)) ;
#149489 = CARTESIAN_POINT('Ctrl Pts',(-24.9336416813406,13.8250174171808,
128.497741444582)) ;
#149490 = CARTESIAN_POINT('Ctrl Pts',(-24.9709882879253,14.1019894892023,
128.640183490629)) ;
#149491 = CARTESIAN_POINT('Ctrl Pts',(-25.0298178161762,14.3273312033298,
128.844994185111)) ;
#149492 = CARTESIAN_POINT('Ctrl Pts',(-25.10580372417,14.4893435077641,129.10009070675)) ;
#149493 = CARTESIAN_POINT('Ctrl Pts',(-25.1925946679685,14.5749599942803,
129.386728128292)) ;
#149494 = CARTESIAN_POINT('Ctrl Pts',(-25.2836420775207,14.5779281388509,
129.685942527895)) ;
#149495 = CARTESIAN_POINT('Ctrl Pts',(-25.3707009485329,14.498336569716,129.973274291318)) ;
#149496 = CARTESIAN_POINT('Ctrl Pts',(-25.4477523301807,14.3420896850988,
130.231459883249)) ;
#149497 = CARTESIAN_POINT('Ctrl Pts',(-25.5085283667888,14.1180212398974,
130.442336334764)) ;
#149498 = CARTESIAN_POINT('Ctrl Pts',(-25.5470625789099,13.8471809568527,
130.587829774937)) ;
#149499 = CARTESIAN_POINT('Ctrl Pts',(-25.5607996567635,13.5439414016218,
130.66115301931)) ;
#149500 = CARTESIAN_POINT('Ctrl Pts',(-25.5476548595395,13.2331635587154,
130.655809870217)) ;
#149501 = CARTESIAN_POINT('Ctrl Pts',(-25.5076848410153,12.9343809245396,
130.5722927305)) ;
#149502 = CARTESIAN_POINT('Ctrl Pts',(-25.4434208273164,12.6721978750302,
130.417619951137)) ;
#149503 = CARTESIAN_POINT('Ctrl Pts',(-25.3584430705461,12.4632419957696,
130.202508041582)) ;
#149504 = CARTESIAN_POINT('Ctrl Pts',(-25.25839433447,12.3231158873288,129.943303971723)) ;
#149505 = CARTESIAN_POINT('Ctrl Pts',(-25.1488417963276,12.2616017925994,
129.656547762908)) ;
#149506 = CARTESIAN_POINT('Ctrl Pts',(-25.038684912235,12.2833201710628,129.367682393325)) ;
#149507 = CARTESIAN_POINT('Ctrl Pts',(-24.9329793112531,12.3868877150975,
129.092131865543)) ;
#149508 = CARTESIAN_POINT('Ctrl Pts',(-24.8399384850518,12.5648231149356,
128.853474687072)) ;
#149509 = CARTESIAN_POINT('Ctrl Pts',(-24.7652402822907,12.8039601972563,
128.668370041775)) ;
#149510 = CARTESIAN_POINT('Ctrl Pts',(-24.7134183488315,13.0864728883471,
128.549995424853)) ;
#149511 = CARTESIAN_POINT('Ctrl Pts',(-24.6872157946094,13.395723837035,128.506754165196)) ;
#149512 = CARTESIAN_POINT('Ctrl Pts',(-24.6881919566604,13.7038340403903,
128.542568479247)) ;
#149513 = CARTESIAN_POINT('Ctrl Pts',(-24.715198213589,13.9936201443638,128.654601982)) ;
#149514 = CARTESIAN_POINT('Ctrl Pts',(-24.766143048851,14.2431366577781,128.836696575373)) ;
#149515 = CARTESIAN_POINT('Ctrl Pts',(-24.8355233115694,14.4318623943572,
129.072286946739)) ;
#149516 = CARTESIAN_POINT('Ctrl Pts',(-24.9191764312831,14.5502397442867,
129.349948983629)) ;
#149517 = CARTESIAN_POINT('Ctrl Pts',(-25.009185749029,14.5868194741509,129.645997652474)) ;
#149518 = CARTESIAN_POINT('Ctrl Pts',(-25.0987232119014,14.5403267808585,
129.940661741851)) ;
#149519 = CARTESIAN_POINT('Ctrl Pts',(-25.1807290894155,14.4138414992085,
130.213331551178)) ;
#149520 = CARTESIAN_POINT('Ctrl Pts',(-25.2485825472388,14.2163547115684,
130.444669381933)) ;
#149521 = CARTESIAN_POINT('Ctrl Pts',(-25.2966444415633,13.9624648084783,
130.618145353059)) ;
#149522 = CARTESIAN_POINT('Ctrl Pts',(-25.3208833248344,13.6693367941651,
130.722106531436)) ;
#149523 = CARTESIAN_POINT('Ctrl Pts',(-25.3186739748594,13.3586798877786,
130.748788087223)) ;
#149524 = CARTESIAN_POINT('Ctrl Pts',(-25.2895027866024,13.0526930051948,
130.696702454147)) ;
#149525 = CARTESIAN_POINT('Ctrl Pts',(-25.2346977316742,12.7731728607976,
130.569743521304)) ;
#149526 = CARTESIAN_POINT('Ctrl Pts',(-25.1575260769634,12.5404162495143,
130.37742441001)) ;
#149527 = CARTESIAN_POINT('Ctrl Pts',(-25.0627516347693,12.3707608334166,
130.133688280252)) ;
#149528 = CARTESIAN_POINT('Ctrl Pts',(-24.9563296046017,12.2766729754023,
129.855958777249)) ;
#149529 = CARTESIAN_POINT('Ctrl Pts',(-24.8458555258651,12.2643218379507,
129.566208802592)) ;
#149530 = CARTESIAN_POINT('Ctrl Pts',(-24.7365680360254,12.3360206173623,
129.280361704469)) ;
#149531 = CARTESIAN_POINT('Ctrl Pts',(-24.6387085221223,12.4836396452835,
129.02730656166)) ;
#149532 = CARTESIAN_POINT('Ctrl Pts',(-24.5554652249711,12.7003318361734,
128.817398714957)) ;
#149533 = CARTESIAN_POINT('Ctrl Pts',(-24.4939102279339,12.9678916740203,
128.67065729352)) ;
#149534 = CARTESIAN_POINT('Ctrl Pts',(-24.4570242893103,13.2687868226262,
128.596084011808)) ;
#149535 = CARTESIAN_POINT('Ctrl Pts',(-24.4470222252909,13.5800033962545,
128.599957819028)) ;
#149536 = CARTESIAN_POINT('Ctrl Pts',(-24.4636781049398,13.8799728738773,
128.681703631968)) ;
#149537 = CARTESIAN_POINT('Ctrl Pts',(-24.5052266831448,14.1476993247652,
128.836224797639)) ;
#149538 = CARTESIAN_POINT('Ctrl Pts',(-24.5678445404094,14.3632524005006,
129.052255584623)) ;
#149539 = CARTESIAN_POINT('Ctrl Pts',(-24.6466140551618,14.5119335521308,
129.315568097717)) ;
#149540 = CARTESIAN_POINT('Ctrl Pts',(-24.7349394738753,14.5819602078055,
129.606776733132)) ;
#149541 = CARTESIAN_POINT('Ctrl Pts',(-24.8251551713637,14.5692454474693,
129.903283329894)) ;
#149542 = CARTESIAN_POINT('Ctrl Pts',(-24.9112782216652,14.4742855004693,
130.188065709167)) ;
#149543 = CARTESIAN_POINT('Ctrl Pts',(-24.9854145282877,14.3047439678629,
130.437652687695)) ;
#149544 = CARTESIAN_POINT('Ctrl Pts',(-25.0423106791957,14.0710831645145,
130.63706527833)) ;
#149545 = CARTESIAN_POINT('Ctrl Pts',(-25.0765997942413,13.7914036967699,
130.770354473467)) ;
#149546 = CARTESIAN_POINT('Ctrl Pts',(-25.0852494656584,13.4850123615767,
130.828786595683)) ;
#149547 = CARTESIAN_POINT('Ctrl Pts',(-25.0670539308989,13.1755844342699,
130.808639517333)) ;
#149548 = CARTESIAN_POINT('Ctrl Pts',(-25.0223515514235,12.8823157939158,
130.71123929387)) ;
#149549 = CARTESIAN_POINT('Ctrl Pts',(-24.953889165623,12.6284363118315,130.544332688521)) ;
#149550 = CARTESIAN_POINT('Ctrl Pts',(-24.8649952863517,12.430459524885,130.31798174757)) ;
#149551 = CARTESIAN_POINT('Ctrl Pts',(-24.7632620671208,12.3053999545834,
130.053682988785)) ;
#149552 = CARTESIAN_POINT('Ctrl Pts',(-24.6526433526302,12.259348439198,129.763874618342)) ;
#149553 = CARTESIAN_POINT('Ctrl Pts',(-24.543147783903,12.2965483927982,129.476879582069)) ;
#149554 = CARTESIAN_POINT('Ctrl Pts',(-24.4388189231228,12.4156949329505,
129.205508703888)) ;
#149555 = CARTESIAN_POINT('Ctrl Pts',(-24.3494211561216,12.6050470822163,
128.97725948019)) ;
#149556 = CARTESIAN_POINT('Ctrl Pts',(-24.2782871788887,12.8553420961893,
128.802763975287)) ;
#149557 = CARTESIAN_POINT('Ctrl Pts',(-24.2314133234197,13.1429454488516,
128.698707201268)) ;
#149558 = CARTESIAN_POINT('Ctrl Pts',(-24.2101989369583,13.454391681807,128.670054503265)) ;
#149559 = CARTESIAN_POINT('Ctrl Pts',(-24.2162621143245,13.7614619706277,
128.720842820947)) ;
#149560 = CARTESIAN_POINT('Ctrl Pts',(-24.2480829792965,14.0447127899292,
128.846925564753)) ;
#149561 = CARTESIAN_POINT('Ctrl Pts',(-24.3026006806666,14.2828872647388,
129.039230695789)) ;
#149562 = CARTESIAN_POINT('Ctrl Pts',(-24.3753681458238,14.4603132079677,
129.284922796906)) ;
#149563 = CARTESIAN_POINT('Ctrl Pts',(-24.4609023941818,14.5634617296136,
129.568084681882)) ;
#149564 = CARTESIAN_POINT('Ctrl Pts',(-24.5508494400508,14.5844329944993,
129.863760728172)) ;
#149565 = CARTESIAN_POINT('Ctrl Pts',(-24.639839531071,14.5225343745256,130.156946138094)) ;
#149566 = CARTESIAN_POINT('Ctrl Pts',(-24.7197008453795,14.3815448921276,
130.423379851621)) ;
#149567 = CARTESIAN_POINT('Ctrl Pts',(-24.7841346291663,14.1725755942996,
130.644670202512)) ;
#149568 = CARTESIAN_POINT('Ctrl Pts',(-24.8280424045697,13.9093042080622,
130.806088923475)) ;
#149569 = CARTESIAN_POINT('Ctrl Pts',(-24.8474183136767,13.6121560169538,
130.89573531851)) ;
#149570 = CARTESIAN_POINT('Ctrl Pts',(-24.8400459886506,13.2990172973707,
130.907513124008)) ;
#149571 = CARTESIAN_POINT('Ctrl Pts',(-24.8060258678097,12.9981567008458,
130.841072315911)) ;
#149572 = CARTESIAN_POINT('Ctrl Pts',(-24.7468166542393,12.7257034100229,
130.701255434815)) ;
#149573 = CARTESIAN_POINT('Ctrl Pts',(-24.6656622236315,12.503075938083,130.497401491787)) ;
#149574 = CARTESIAN_POINT('Ctrl Pts',(-24.5684692840645,12.3471530516957,
130.246518289706)) ;
#149575 = CARTESIAN_POINT('Ctrl Pts',(-24.4601592445073,12.2678408813101,
129.963418414353)) ;
#149576 = CARTESIAN_POINT('Ctrl Pts',(-24.3498913902178,12.2715868988579,
129.674190683696)) ;
#149577 = CARTESIAN_POINT('Ctrl Pts',(-24.2425522782409,12.3575775425478,
129.39381841984)) ;
#149578 = CARTESIAN_POINT('Ctrl Pts',(-24.1463896718838,12.519859116392,129.145996967163)) ;
#149579 = CARTESIAN_POINT('Ctrl Pts',(-24.0670162200056,12.7472699624983,
128.947309088182)) ;
#149580 = CARTESIAN_POINT('Ctrl Pts',(-24.0097627776868,13.0233713370029,
128.813237370851)) ;
#149581 = CARTESIAN_POINT('Ctrl Pts',(-23.9780360421946,13.3264774087469,
128.753559775016)) ;
#149582 = CARTESIAN_POINT('Ctrl Pts',(-23.972984735808,13.6374828083211,128.771916902171)) ;
#149583 = CARTESIAN_POINT('Ctrl Pts',(-23.9946301893743,13.9340521911672,
128.868370985109)) ;
#149584 = CARTESIAN_POINT('Ctrl Pts',(-24.0404917441425,14.193123894667,129.035463808342)) ;
#149585 = CARTESIAN_POINT('Ctrl Pts',(-24.1068147894344,14.3974304405376,
129.262422211174)) ;
#149586 = CARTESIAN_POINT('Ctrl Pts',(-24.1873859593662,14.5309245304013,
129.530773973435)) ;
#149587 = CARTESIAN_POINT('Ctrl Pts',(-24.2765414629164,14.5859814529116,
129.824348558805)) ;
#149588 = CARTESIAN_POINT('Ctrl Pts',(-24.3669136839927,14.5574777921035,
130.12149550496)) ;
#149589 = CARTESIAN_POINT('Ctrl Pts',(-24.4511409095846,14.4480150679812,
130.400638885907)) ;
#149590 = CARTESIAN_POINT('Ctrl Pts',(-24.5228192659594,14.2640747016683,
130.643277300762)) ;
#149591 = CARTESIAN_POINT('Ctrl Pts',(-24.5753535527293,14.0222278748094,
130.829662909355)) ;
#149592 = CARTESIAN_POINT('Ctrl Pts',(-24.6052393635017,13.7339092268223,
130.950338760758)) ;
#149593 = CARTESIAN_POINT('Ctrl Pts',(-24.6087423113482,13.4264443315917,
130.993564327821)) ;
#149594 = CARTESIAN_POINT('Ctrl Pts',(-24.5854552385146,13.117933729061,130.958630105936)) ;
#149595 = CARTESIAN_POINT('Ctrl Pts',(-24.5360542246663,12.8308236543942,
130.847449580538)) ;
#149596 = CARTESIAN_POINT('Ctrl Pts',(-24.4632259609744,12.5859821244952,
130.667884994936)) ;
#149597 = CARTESIAN_POINT('Ctrl Pts',(-24.3721859047241,12.4020104693658,
130.434925127817)) ;
#149598 = CARTESIAN_POINT('Ctrl Pts',(-24.2672388487678,12.2899875702474,
130.161658393472)) ;
#149599 = CARTESIAN_POINT('Ctrl Pts',(-24.1570061952322,12.2601247777389,
129.872660322031)) ;
#149600 = CARTESIAN_POINT('Ctrl Pts',(-24.0474842604457,12.3130228920766,
129.585829133635)) ;
#149601 = CARTESIAN_POINT('Ctrl Pts',(-23.9459955773779,12.4457555265159,
129.322497926636)) ;
#149602 = CARTESIAN_POINT('Ctrl Pts',(-23.8593193186365,12.6478748445304,
129.102358913556)) ;
#149603 = CARTESIAN_POINT('Ctrl Pts',(-23.7923711383799,12.90742344953,128.940087473062)) ;
#149604 = CARTESIAN_POINT('Ctrl Pts',(-23.7501513912619,13.2015878623563,
128.849756858677)) ;
#149605 = CARTESIAN_POINT('Ctrl Pts',(-23.7341995328484,13.513246132059,128.83635605202)) ;
#149606 = CARTESIAN_POINT('Ctrl Pts',(-23.7452242106922,13.8170403560637,
128.901601785867)) ;
#149607 = CARTESIAN_POINT('Ctrl Pts',(-23.7815365397005,14.0930903285622,
129.040762499699)) ;
#149608 = CARTESIAN_POINT('Ctrl Pts',(-23.8399631313571,14.3215764376153,
129.244564779432)) ;
#149609 = CARTESIAN_POINT('Ctrl Pts',(-23.9158125493605,14.4860163871687,
129.499361949974)) ;
#149610 = CARTESIAN_POINT('Ctrl Pts',(-24.0024884712054,14.5737421831593,
129.785693667344)) ;
#149611 = CARTESIAN_POINT('Ctrl Pts',(-24.0932764888338,14.5789283519424,
130.084061847356)) ;
#149612 = CARTESIAN_POINT('Ctrl Pts',(-24.1805810257139,14.5018180781457,
130.372118460608)) ;
#149613 = CARTESIAN_POINT('Ctrl Pts',(-24.2582426096159,14.3465572138388,
130.632227060123)) ;
#149614 = CARTESIAN_POINT('Ctrl Pts',(-24.318922055871,14.1268975859946,130.842432120294)) ;
#149615 = CARTESIAN_POINT('Ctrl Pts',(-24.3585878491517,13.8551173333083,
130.991522309819)) ;
#149616 = CARTESIAN_POINT('Ctrl Pts',(-24.3729811727422,13.5530514979448,
131.066681273596)) ;
#149617 = CARTESIAN_POINT('Ctrl Pts',(-24.3605810853974,13.2415865700778,
131.063587579124)) ;
#149618 = CARTESIAN_POINT('Ctrl Pts',(-24.3215051289014,12.9431698181064,
130.982558898571)) ;
#149619 = CARTESIAN_POINT('Ctrl Pts',(-24.2577823597366,12.6789857022783,
130.82955143097)) ;
#149620 = CARTESIAN_POINT('Ctrl Pts',(-24.1734213941347,12.4685394355876,
130.616198443188)) ;
#149621 = CARTESIAN_POINT('Ctrl Pts',(-24.073742301987,12.3261975065515,130.358076220312)) ;
#149622 = CARTESIAN_POINT('Ctrl Pts',(-23.964425817923,12.2622045944374,130.07198593286)) ;
#149623 = CARTESIAN_POINT('Ctrl Pts',(-23.85400734296,12.2815898104216,129.782422227761)) ;
#149624 = CARTESIAN_POINT('Ctrl Pts',(-23.7483648318689,12.3824517320663,
129.506948722711)) ;
#149625 = CARTESIAN_POINT('Ctrl Pts',(-23.6547176816251,12.5585396445524,
129.266575329298)) ;
#149626 = CARTESIAN_POINT('Ctrl Pts',(-23.5794496136605,12.7954954473237,
129.079743076793)) ;
#149627 = CARTESIAN_POINT('Ctrl Pts',(-23.5265530513227,13.0796939722615,
128.958534945504)) ;
#149628 = CARTESIAN_POINT('Ctrl Pts',(-23.4998982470055,13.3852304092896,
128.913605172704)) ;
#149629 = CARTESIAN_POINT('Ctrl Pts',(-23.4999888970711,13.6960444391784,
128.947097240951)) ;
#149630 = CARTESIAN_POINT('Ctrl Pts',(-23.5263685356686,13.9858667251667,
129.057221274521)) ;
#149631 = CARTESIAN_POINT('Ctrl Pts',(-23.5763701013332,14.2358877354541,
129.236412760875)) ;
#149632 = CARTESIAN_POINT('Ctrl Pts',(-23.6455558699911,14.427599936546,129.471589612086)) ;
#149633 = CARTESIAN_POINT('Ctrl Pts',(-23.7290651686037,14.5480862875162,
129.748875677401)) ;
#149634 = CARTESIAN_POINT('Ctrl Pts',(-23.8186690168967,14.5868446714445,
130.043626720831)) ;
#149635 = CARTESIAN_POINT('Ctrl Pts',(-23.9082230495936,14.543035766912,130.338299611746)) ;
#149636 = CARTESIAN_POINT('Ctrl Pts',(-23.9906596269093,14.4187440233768,
130.61226747632)) ;
#149637 = CARTESIAN_POINT('Ctrl Pts',(-24.0590906655054,14.2230681699305,
130.845316199776)) ;
#149638 = CARTESIAN_POINT('Ctrl Pts',(-24.1078676594404,13.9697197802327,
131.020979313656)) ;
#149639 = CARTESIAN_POINT('Ctrl Pts',(-24.1327346146683,13.678752384422,131.126622427397)) ;
#149640 = CARTESIAN_POINT('Ctrl Pts',(-24.1313280770406,13.3668523493994,
131.155805587828)) ;
#149641 = CARTESIAN_POINT('Ctrl Pts',(-24.1028121227854,13.0606725524935,
131.10561289289)) ;
#149642 = CARTESIAN_POINT('Ctrl Pts',(-24.0489129518643,12.7810811870564,
130.981183215495)) ;
#149643 = CARTESIAN_POINT('Ctrl Pts',(-23.9723802111595,12.5467078049701,
130.790724008006)) ;
#149644 = CARTESIAN_POINT('Ctrl Pts',(-23.878243975613,12.3750360916392,130.548796694559)) ;
#149645 = CARTESIAN_POINT('Ctrl Pts',(-23.7714355652821,12.2779852659618,
130.270134963112)) ;
#149646 = CARTESIAN_POINT('Ctrl Pts',(-23.6611435021707,12.2637459415924,
129.980872210853)) ;
#149647 = CARTESIAN_POINT('Ctrl Pts',(-23.5523935290098,12.3321871278704,
129.696367849268)) ;
#149648 = CARTESIAN_POINT('Ctrl Pts',(-23.4532846730256,12.4786899197398,
129.439942969293)) ;
#149649 = CARTESIAN_POINT('Ctrl Pts',(-23.369577036012,12.6941597985184,129.228694490344)) ;
#149650 = CARTESIAN_POINT('Ctrl Pts',(-23.3076081758044,12.95948963943,129.0806195286)) ;
#149651 = CARTESIAN_POINT('Ctrl Pts',(-23.2699369429155,13.2597800757016,
129.003760027813)) ;
#149652 = CARTESIAN_POINT('Ctrl Pts',(-23.259151387003,13.570593176475,129.005303519991)) ;
#149653 = CARTESIAN_POINT('Ctrl Pts',(-23.2750101957861,13.8717553022586,
129.084772659304)) ;
#149654 = CARTESIAN_POINT('Ctrl Pts',(-23.3161725222393,14.1416795276356,
129.238312148315)) ;
#149655 = CARTESIAN_POINT('Ctrl Pts',(-23.3778830225391,14.3575207602719,
129.451480700559)) ;
#149656 = CARTESIAN_POINT('Ctrl Pts',(-23.456487612726,14.5088742129947,129.714415384989)) ;
#149657 = CARTESIAN_POINT('Ctrl Pts',(-23.5444425261219,14.5810485747374,
130.004461283364)) ;
#149658 = CARTESIAN_POINT('Ctrl Pts',(-23.6348221144792,14.5707018423974,
130.301503634973)) ;
#149659 = CARTESIAN_POINT('Ctrl Pts',(-23.720929050143,14.4785663086567,130.58612695697)) ;
#149660 = CARTESIAN_POINT('Ctrl Pts',(-23.796091874448,14.3096046901172,130.838988013443)) ;
#149661 = CARTESIAN_POINT('Ctrl Pts',(-23.8532786750127,14.0777450848623,
131.039159906717)) ;
#149662 = CARTESIAN_POINT('Ctrl Pts',(-23.8881290823669,13.8001342656759,
131.173975253073)) ;
#149663 = CARTESIAN_POINT('Ctrl Pts',(-23.8976235031685,13.4946153798022,
131.234832161425)) ;
#149664 = CARTESIAN_POINT('Ctrl Pts',(-23.8801038719591,13.1837407483122,
131.216799463619)) ;
#149665 = CARTESIAN_POINT('Ctrl Pts',(-23.8362104970674,12.8901082923596,
131.121701071398)) ;
#149666 = CARTESIAN_POINT('Ctrl Pts',(-23.7678922757388,12.6339161097821,
130.955392278708)) ;
#149667 = CARTESIAN_POINT('Ctrl Pts',(-23.6807913010125,12.43659258656,130.733805167857)) ;
#149668 = CARTESIAN_POINT('Ctrl Pts',(-23.5782209974731,12.3075969650438,
130.467461898583)) ;
#149669 = CARTESIAN_POINT('Ctrl Pts',(-23.4687021830052,12.25954136932,130.18055487232)) ;
#149670 = CARTESIAN_POINT('Ctrl Pts',(-23.3580959689389,12.2945981234014,
129.890635929431)) ;
#149671 = CARTESIAN_POINT('Ctrl Pts',(-23.2545594842742,12.4101972587338,
129.621216465596)) ;
#149672 = CARTESIAN_POINT('Ctrl Pts',(-23.1639430593023,12.5987159490307,
129.38966556076)) ;
#149673 = CARTESIAN_POINT('Ctrl Pts',(-23.0924891951647,12.8461743758197,
129.214054201236)) ;
#149674 = CARTESIAN_POINT('Ctrl Pts',(-23.044410224878,13.135926237231,129.1068328996)) ;
#149675 = CARTESIAN_POINT('Ctrl Pts',(-23.0226954450076,13.4447581443412,
129.076453559591)) ;
#149676 = CARTESIAN_POINT('Ctrl Pts',(-23.0279406480016,13.7530929006016,
129.124954375836)) ;
#149677 = CARTESIAN_POINT('Ctrl Pts',(-23.0589188674744,14.0362080227333,
129.248437506434)) ;
#149678 = CARTESIAN_POINT('Ctrl Pts',(-23.1129427190555,14.2769559751065,
129.43941471817)) ;
#149679 = CARTESIAN_POINT('Ctrl Pts',(-23.1854563521041,14.4563581668246,
129.684422602972)) ;
#149680 = CARTESIAN_POINT('Ctrl Pts',(-23.2701501049664,14.5613193380967,
129.964912349614)) ;
#149681 = CARTESIAN_POINT('Ctrl Pts',(-23.3606421210985,14.5851466782009,
130.262402055223)) ;
#149682 = CARTESIAN_POINT('Ctrl Pts',(-23.4498301224202,14.5250094575114,
130.556196196659)) ;
#149683 = CARTESIAN_POINT('Ctrl Pts',(-23.5296219906433,14.3871119607425,
130.822238990892)) ;
#149684 = CARTESIAN_POINT('Ctrl Pts',(-23.594925658701,14.1786614290351,131.046268453031)) ;
#149685 = CARTESIAN_POINT('Ctrl Pts',(-23.6392653935183,13.9181922877867,
131.208752582989)) ;
#149686 = CARTESIAN_POINT('Ctrl Pts',(-23.659486219196,13.6189924395308,131.301176945121)) ;
#149687 = CARTESIAN_POINT('Ctrl Pts',(-23.6528706435111,13.3089362850498,
131.314836717611)) ;
#149688 = CARTESIAN_POINT('Ctrl Pts',(-23.6195413006821,13.0058326835249,
131.250594746638)) ;
#149689 = CARTESIAN_POINT('Ctrl Pts',(-23.5607526391566,12.7318653591864,
131.112071177331)) ;
#149690 = CARTESIAN_POINT('Ctrl Pts',(-23.4802503319466,12.5082427552374,
130.910055459354)) ;
#149691 = CARTESIAN_POINT('Ctrl Pts',(-23.3837706397875,12.3508733005898,
130.661144170979)) ;
#149692 = CARTESIAN_POINT('Ctrl Pts',(-23.2760281567671,12.269103663372,130.379599385189)) ;
#149693 = CARTESIAN_POINT('Ctrl Pts',(-23.1652080396249,12.2702137118359,
130.088920070481)) ;
#149694 = CARTESIAN_POINT('Ctrl Pts',(-23.0575184300557,12.3542929443511,
129.807572897361)) ;
#149695 = CARTESIAN_POINT('Ctrl Pts',(-22.9612440374846,12.5141175803543,
129.559330205376)) ;
#149696 = CARTESIAN_POINT('Ctrl Pts',(-22.8813580521407,12.7395233280602,
129.359110706345)) ;
#149697 = CARTESIAN_POINT('Ctrl Pts',(-22.8233745273822,13.0142278391015,
129.222887167103)) ;
#149698 = CARTESIAN_POINT('Ctrl Pts',(-22.7907608487807,13.3177661715459,
129.160724179542)) ;
#149699 = CARTESIAN_POINT('Ctrl Pts',(-22.7849933023356,13.6286636556953,
129.176966985141)) ;
#149700 = CARTESIAN_POINT('Ctrl Pts',(-22.8057875541623,13.925291797829,129.270850522391)) ;
#149701 = CARTESIAN_POINT('Ctrl Pts',(-22.8510343106894,14.1860949206715,
129.436195197481)) ;
#149702 = CARTESIAN_POINT('Ctrl Pts',(-22.9165695111379,14.3917323897328,
129.6607396938)) ;
#149703 = CARTESIAN_POINT('Ctrl Pts',(-22.9971196771895,14.5282787292637,
129.929178676751)) ;
#149704 = CARTESIAN_POINT('Ctrl Pts',(-23.0863190684493,14.5855538686264,
130.222941810588)) ;
#149705 = CARTESIAN_POINT('Ctrl Pts',(-23.1764960201686,14.5594424276329,
130.519424297724)) ;
#149706 = CARTESIAN_POINT('Ctrl Pts',(-23.260922733227,14.4525338463175,130.799116406476)) ;
#149707 = CARTESIAN_POINT('Ctrl Pts',(-23.3332076886336,14.2704302035547,
131.043574251826)) ;
#149708 = CARTESIAN_POINT('Ctrl Pts',(-23.3863890212945,14.0294404893197,
131.23192060155)) ;
#149709 = CARTESIAN_POINT('Ctrl Pts',(-23.4168682308191,13.7439522566763,
131.354120127472)) ;
#149710 = CARTESIAN_POINT('Ctrl Pts',(-23.4212510479879,13.4354033012877,
131.400078141052)) ;
#149711 = CARTESIAN_POINT('Ctrl Pts',(-23.3987589168995,13.1268757860435,
131.367427280398)) ;
#149712 = CARTESIAN_POINT('Ctrl Pts',(-23.3498917515074,12.8380942311381,
131.257906778931)) ;
#149713 = CARTESIAN_POINT('Ctrl Pts',(-23.2781287469993,12.593020734814,131.081261436538)) ;
#149714 = CARTESIAN_POINT('Ctrl Pts',(-23.1869981180015,12.406038864334,130.848244567597)) ;
#149715 = CARTESIAN_POINT('Ctrl Pts',(-23.0832130154599,12.2925312393263,
130.578091002702)) ;
#149716 = CARTESIAN_POINT('Ctrl Pts',(-22.9721460034913,12.2597001756507,
130.286938563817)) ;
#149717 = CARTESIAN_POINT('Ctrl Pts',(-22.8627372801265,12.3104428480306,
130.000362594001)) ;
#149718 = CARTESIAN_POINT('Ctrl Pts',(-22.7608153842907,12.4411375343228,
129.735804833059)) ;
#149719 = CARTESIAN_POINT('Ctrl Pts',(-22.6738551041291,12.6410412260459,
129.514759298238)) ;
#149720 = CARTESIAN_POINT('Ctrl Pts',(-22.6062140340479,12.8990709412412,
129.350458683346)) ;
#149721 = CARTESIAN_POINT('Ctrl Pts',(-22.563180860829,13.1932158422951,129.257833604546)) ;
#149722 = CARTESIAN_POINT('Ctrl Pts',(-22.5465084812916,13.5039483153196,
129.242243533921)) ;
#149723 = CARTESIAN_POINT('Ctrl Pts',(-22.5567390519965,13.8084629331276,
129.305193170766)) ;
#149724 = CARTESIAN_POINT('Ctrl Pts',(-22.5923567807548,14.0856214522983,
129.442322762653)) ;
#149725 = CARTESIAN_POINT('Ctrl Pts',(-22.6502043847312,14.3156973723363,
129.644432208859)) ;
#149726 = CARTESIAN_POINT('Ctrl Pts',(-22.7254796481943,14.4820692516826,
129.897492489586)) ;
#149727 = CARTESIAN_POINT('Ctrl Pts',(-22.8120983348714,14.5722583226928,
130.183725983055)) ;
#149728 = CARTESIAN_POINT('Ctrl Pts',(-22.9024146711451,14.5801737014987,
130.480544456833)) ;
#149729 = CARTESIAN_POINT('Ctrl Pts',(-22.9905600558702,14.5050114292979,
130.771303640142)) ;
#149730 = CARTESIAN_POINT('Ctrl Pts',(-23.0683259692311,14.3522166044366,
131.031600216903)) ;
#149731 = CARTESIAN_POINT('Ctrl Pts',(-23.1296712033648,14.1339604328417,
131.243810544313)) ;
#149732 = CARTESIAN_POINT('Ctrl Pts',(-23.1699417301646,13.8641114718027,
131.394578383652)) ;
#149733 = CARTESIAN_POINT('Ctrl Pts',(-23.1851714520848,13.5616227135085,
131.472298291736)) ;
#149734 = CARTESIAN_POINT('Ctrl Pts',(-23.1735168490952,13.2502936297686,
131.47135922614)) ;
#149735 = CARTESIAN_POINT('Ctrl Pts',(-23.1351157903928,12.9509784394827,
131.392333342699)) ;
#149736 = CARTESIAN_POINT('Ctrl Pts',(-23.0722677645441,12.6863950306147,
131.241771426111)) ;
#149737 = CARTESIAN_POINT('Ctrl Pts',(-22.9882746146552,12.4734607184327,
131.029576395243)) ;
#149738 = CARTESIAN_POINT('Ctrl Pts',(-22.8884966331246,12.3287824290801,
130.771297011611)) ;
#149739 = CARTESIAN_POINT('Ctrl Pts',(-22.7798708475332,12.2629634188969,
130.487058336271)) ;
#149740 = CARTESIAN_POINT('Ctrl Pts',(-22.6692239157049,12.2798963089147,
130.196884376816)) ;
#149741 = CARTESIAN_POINT('Ctrl Pts',(-22.5632797991812,12.3786943596861,
129.920548149089)) ;
#149742 = CARTESIAN_POINT('Ctrl Pts',(-22.4691047373813,12.5532636786749,
129.678681828688)) ;
#149743 = CARTESIAN_POINT('Ctrl Pts',(-22.3936121882583,12.7879391419199,
129.491068858609)) ;
#149744 = CARTESIAN_POINT('Ctrl Pts',(-22.3401335624516,13.0695370930121,
129.367998395707)) ;
#149745 = CARTESIAN_POINT('Ctrl Pts',(-22.3124627686297,13.3764286772832,
129.32029580838)) ;
#149746 = CARTESIAN_POINT('Ctrl Pts',(-22.3118479090046,13.6873693589622,
129.351715741832)) ;
#149747 = CARTESIAN_POINT('Ctrl Pts',(-22.3374491968515,13.9780097335569,
129.459554831409)) ;
#149748 = CARTESIAN_POINT('Ctrl Pts',(-22.3870967384103,14.2303816852456,
129.637852506658)) ;
#149749 = CARTESIAN_POINT('Ctrl Pts',(-22.4556103846514,14.4229832269157,
129.870941575462)) ;
#149750 = CARTESIAN_POINT('Ctrl Pts',(-22.5386005193327,14.5456071990929,
130.146637869672)) ;
#149751 = CARTESIAN_POINT('Ctrl Pts',(-22.6282642571968,14.5869244372619,
130.441623746508)) ;
#149752 = CARTESIAN_POINT('Ctrl Pts',(-22.7179879086847,14.545413997822,130.736814107986)) ;
#149753 = CARTESIAN_POINT('Ctrl Pts',(-22.8007463302778,14.4231615321001,
131.011735541558)) ;
#149754 = CARTESIAN_POINT('Ctrl Pts',(-22.8694507154982,14.2299646068936,
131.245482052944)) ;
#149755 = CARTESIAN_POINT('Ctrl Pts',(-22.918951836608,13.9782380541428,131.423258260038)) ;
#149756 = CARTESIAN_POINT('Ctrl Pts',(-22.9445965328865,13.6869897055948,
131.531296852322)) ;
#149757 = CARTESIAN_POINT('Ctrl Pts',(-22.943990289379,13.3772462796711,131.562611149052)) ;
#149758 = CARTESIAN_POINT('Ctrl Pts',(-22.9163803749009,13.0701027009942,
131.515113736096)) ;
#149759 = CARTESIAN_POINT('Ctrl Pts',(-22.8629756360469,12.7883758458207,
131.392255641816)) ;
#149760 = CARTESIAN_POINT('Ctrl Pts',(-22.7870243908306,12.5524788761833,
131.203489638896)) ;
#149761 = CARTESIAN_POINT('Ctrl Pts',(-22.693119134411,12.3787206471269,130.962295345711)) ;
#149762 = CARTESIAN_POINT('Ctrl Pts',(-22.5872002079186,12.2799428632339,
130.686031470634)) ;
#149763 = CARTESIAN_POINT('Ctrl Pts',(-22.4767054930379,12.262781436098,130.396251358911)) ;
#149764 = CARTESIAN_POINT('Ctrl Pts',(-22.3671975211959,12.3295043869385,
130.109715154456)) ;
#149765 = CARTESIAN_POINT('Ctrl Pts',(-22.2682597339845,12.473510372606,129.853632818829)) ;
#149766 = CARTESIAN_POINT('Ctrl Pts',(-22.1842913044772,12.6859034724392,
129.641472948318)) ;
#149767 = CARTESIAN_POINT('Ctrl Pts',(-22.1212728778799,12.9511126916242,
129.490491975582)) ;
#149768 = CARTESIAN_POINT('Ctrl Pts',(-22.0828450680906,13.2510040815984,
129.411445954069)) ;
#149769 = CARTESIAN_POINT('Ctrl Pts',(-22.0712938830656,13.5624346911567,
129.410820581416)) ;
#149770 = CARTESIAN_POINT('Ctrl Pts',(-22.0864657444321,13.863434989198,129.488210788799)) ;
#149771 = CARTESIAN_POINT('Ctrl Pts',(-22.126593878773,14.1332612598468,129.638538262364)) ;
#149772 = CARTESIAN_POINT('Ctrl Pts',(-22.1881835845486,14.3526408923895,
129.851608596392)) ;
#149773 = CARTESIAN_POINT('Ctrl Pts',(-22.2662698967249,14.5054039149979,
130.112943305636)) ;
#149774 = CARTESIAN_POINT('Ctrl Pts',(-22.3536617688702,14.5799567514586,
130.401216699648)) ;
#149775 = CARTESIAN_POINT('Ctrl Pts',(-22.4444166235303,14.5723714395277,
130.699477612996)) ;
#149776 = CARTESIAN_POINT('Ctrl Pts',(-22.5310362051364,14.4818104958985,
130.985724648343)) ;
#149777 = CARTESIAN_POINT('Ctrl Pts',(-22.6060015969075,14.3163443663444,
131.237730292278)) ;
#149778 = CARTESIAN_POINT('Ctrl Pts',(-22.6640340596901,14.0859121454152,
131.440457148936)) ;
#149779 = CARTESIAN_POINT('Ctrl Pts',(-22.6996929687443,13.8088759018265,
131.577695110842)) ;
#149780 = CARTESIAN_POINT('Ctrl Pts',(-22.7099178996743,13.5028416968273,
131.640793767491)) ;
#149781 = CARTESIAN_POINT('Ctrl Pts',(-22.6932495161997,13.1931031843273,
131.625104283202)) ;
#149782 = CARTESIAN_POINT('Ctrl Pts',(-22.6499855145804,12.89795929161,131.531932093916)) ;
#149783 = CARTESIAN_POINT('Ctrl Pts',(-22.5827221854466,12.6415807135438,
131.368528308909)) ;
#149784 = CARTESIAN_POINT('Ctrl Pts',(-22.4955321587869,12.4408172344946,
131.146922824915)) ;
#149785 = CARTESIAN_POINT('Ctrl Pts',(-22.393252860788,12.3100401659206,130.881416910317)) ;
#149786 = CARTESIAN_POINT('Ctrl Pts',(-22.2840884304056,12.2598615754433,
130.595478670003)) ;
#149787 = CARTESIAN_POINT('Ctrl Pts',(-22.1736356223127,12.2922205414055,
130.305931435607)) ;
#149788 = CARTESIAN_POINT('Ctrl Pts',(-22.0692646768025,12.4062484922091,
130.034252292892)) ;
#149789 = CARTESIAN_POINT('Ctrl Pts',(-21.9784401265655,12.5927140655513,
129.802018991146)) ;
#149790 = CARTESIAN_POINT('Ctrl Pts',(-21.9065444640982,12.8381489007341,
129.62504663551)) ;
#149791 = CARTESIAN_POINT('Ctrl Pts',(-21.857754981397,13.1260095421298,129.515650593897)) ;
#149792 = CARTESIAN_POINT('Ctrl Pts',(-21.8351198417726,13.4367097246031,
129.482816396722)) ;
#149793 = CARTESIAN_POINT('Ctrl Pts',(-21.8396215028571,13.7438376703634,
129.528974842274)) ;
#149794 = CARTESIAN_POINT('Ctrl Pts',(-21.8699032060914,14.0287736404421,
129.650514879023)) ;
#149795 = CARTESIAN_POINT('Ctrl Pts',(-21.9233871407245,14.270962157525,129.839919077007)) ;
#149796 = CARTESIAN_POINT('Ctrl Pts',(-21.9953096059553,14.4520607782582,
130.083142298059)) ;
#149797 = CARTESIAN_POINT('Ctrl Pts',(-22.0798724098477,14.5594794315335,
130.363302132946)) ;
#149798 = CARTESIAN_POINT('Ctrl Pts',(-22.170121644081,14.5855261775524,130.660019013588)) ;
#149799 = CARTESIAN_POINT('Ctrl Pts',(-22.2592468971728,14.5283738977508,
130.953536397664)) ;
#149800 = CARTESIAN_POINT('Ctrl Pts',(-22.3398966660071,14.391653675229,131.222308593128)) ;
#149801 = CARTESIAN_POINT('Ctrl Pts',(-22.4053261752883,14.1863633924956,
131.446488605931)) ;
#149802 = CARTESIAN_POINT('Ctrl Pts',(-22.4506077808692,13.9255969369485,
131.611940327664)) ;
#149803 = CARTESIAN_POINT('Ctrl Pts',(-22.4714276383869,13.6292801899933,
131.705867636475)) ;
#149804 = CARTESIAN_POINT('Ctrl Pts',(-22.4656985706484,13.3179690921283,
131.722267859741)) ;
#149805 = CARTESIAN_POINT('Ctrl Pts',(-22.4330809865824,13.0144329999001,
131.660092690325)) ;
#149806 = CARTESIAN_POINT('Ctrl Pts',(-22.3752337324937,12.7401668642732,
131.524210201602)) ;
#149807 = CARTESIAN_POINT('Ctrl Pts',(-22.2953919549194,12.5144107984142,
131.324132448709)) ;
#149808 = CARTESIAN_POINT('Ctrl Pts',(-22.1986907467925,12.3540785091182,
131.074781660547)) ;
#149809 = CARTESIAN_POINT('Ctrl Pts',(-22.0916577558985,12.2704506972946,
130.795149181821)) ;
#149810 = CARTESIAN_POINT('Ctrl Pts',(-21.9804835857871,12.2689820751512,
130.503544699241)) ;
#149811 = CARTESIAN_POINT('Ctrl Pts',(-21.8726683552619,12.3508509067205,
130.221807220938)) ;
#149812 = CARTESIAN_POINT('Ctrl Pts',(-21.7759646206819,12.5086054650755,
129.972319239919)) ;
#149813 = CARTESIAN_POINT('Ctrl Pts',(-21.6953381788648,12.7330676157862,
129.770024556173)) ;
#149814 = CARTESIAN_POINT('Ctrl Pts',(-21.6368282731019,13.0066123030749,
129.632239940653)) ;
#149815 = CARTESIAN_POINT('Ctrl Pts',(-21.6035887086732,13.3082724111724,
129.568104862639)) ;
#149816 = CARTESIAN_POINT('Ctrl Pts',(-21.5969642140476,13.6201711563921,
129.581939837877)) ;
#149817 = CARTESIAN_POINT('Ctrl Pts',(-21.6171785071835,13.9183339563094,
129.674227224857)) ;
#149818 = CARTESIAN_POINT('Ctrl Pts',(-21.6617871521888,14.1797387152336,
129.837645381447)) ;
#149819 = CARTESIAN_POINT('Ctrl Pts',(-21.7265912402179,14.3864986617501,
130.059946572306)) ;
#149820 = CARTESIAN_POINT('Ctrl Pts',(-21.8067464305552,14.5252641386946,
130.327221597644)) ;
#149821 = CARTESIAN_POINT('Ctrl Pts',(-21.8958184713667,14.5851720998815,
130.620620927139)) ;
#149822 = CARTESIAN_POINT('Ctrl Pts',(-21.9865681374424,14.561066934574,130.918966487023)) ;
#149823 = CARTESIAN_POINT('Ctrl Pts',(-22.0707594233655,14.4566510125324,
131.19779203029)) ;
#149824 = CARTESIAN_POINT('Ctrl Pts',(-22.1434681961939,14.2771545547794,
131.443436921697)) ;
#149825 = CARTESIAN_POINT('Ctrl Pts',(-22.1975055554167,14.0362065593723,
131.634471428032)) ;
#149826 = CARTESIAN_POINT('Ctrl Pts',(-22.228481100872,13.7533987365905,131.757917035488)) ;
#149827 = CARTESIAN_POINT('Ctrl Pts',(-22.2337680807398,13.444128366597,131.806637674055)) ;
#149828 = CARTESIAN_POINT('Ctrl Pts',(-22.2118313707014,13.1346408962195,
131.775690169026)) ;
#149829 = CARTESIAN_POINT('Ctrl Pts',(-22.1641188393883,12.8470251691959,
131.66929025756)) ;
#149830 = CARTESIAN_POINT('Ctrl Pts',(-22.0924166245413,12.5984937822196,
131.493091002478)) ;
#149831 = CARTESIAN_POINT('Ctrl Pts',(-22.0022409153909,12.4108688263379,
131.262663941909)) ;
#149832 = CARTESIAN_POINT('Ctrl Pts',(-21.898534109697,12.2946081111199,130.992821647308)) ;
#149833 = CARTESIAN_POINT('Ctrl Pts',(-21.7874624784035,12.2594450542174,
130.701676041375)) ;
#149834 = CARTESIAN_POINT('Ctrl Pts',(-21.6778492662529,12.3080481401079,
130.414533549498)) ;
#149835 = CARTESIAN_POINT('Ctrl Pts',(-21.5759437155099,12.4360760785603,
130.149908558154)) ;
#149836 = CARTESIAN_POINT('Ctrl Pts',(-21.4882912931024,12.6345257825012,
129.926914377626)) ;
#149837 = CARTESIAN_POINT('Ctrl Pts',(-21.420235735472,12.8902136369556,129.761280181062)) ;
#149838 = CARTESIAN_POINT('Ctrl Pts',(-21.3763386660893,13.1836914556234,
129.666160682438)) ;
#149839 = CARTESIAN_POINT('Ctrl Pts',(-21.3588102921648,13.4943233171344,
129.64807578917)) ;
#149840 = CARTESIAN_POINT('Ctrl Pts',(-21.3683109889988,13.800844370543,129.709055456557)) ;
#149841 = CARTESIAN_POINT('Ctrl Pts',(-21.4034525605879,14.0793169381169,
129.844852216424)) ;
#149842 = CARTESIAN_POINT('Ctrl Pts',(-21.4604693997575,14.3098744283553,
130.044376194059)) ;
#149843 = CARTESIAN_POINT('Ctrl Pts',(-21.5356692735843,14.4788323999099,
130.297359822827)) ;
#149844 = CARTESIAN_POINT('Ctrl Pts',(-21.6216446878527,14.5706779805767,
130.581543004274)) ;
#149845 = CARTESIAN_POINT('Ctrl Pts',(-21.7121217703692,14.5811216751553,
130.878902955014)) ;
#149846 = CARTESIAN_POINT('Ctrl Pts',(-21.8002831689519,14.5082992229446,
131.169647708702)) ;
#149847 = CARTESIAN_POINT('Ctrl Pts',(-21.8783799046181,14.3580059118444,
131.43087371812)) ;
#149848 = CARTESIAN_POINT('Ctrl Pts',(-21.9405361241306,14.1405258591395,
131.645593076356)) ;
#149849 = CARTESIAN_POINT('Ctrl Pts',(-21.9813282753517,13.8719963111484,
131.797849655205)) ;
#149850 = CARTESIAN_POINT('Ctrl Pts',(-21.9973134311112,13.5716291757303,
131.877616580862)) ;
#149851 = CARTESIAN_POINT('Ctrl Pts',(-21.986445843118,13.2591264952113,131.879101856403)) ;
#149852 = CARTESIAN_POINT('Ctrl Pts',(-21.9489161756331,12.9599152981085,
131.80253028907)) ;
#149853 = CARTESIAN_POINT('Ctrl Pts',(-21.8865489034867,12.6930802012435,
131.653491136013)) ;
#149854 = CARTESIAN_POINT('Ctrl Pts',(-21.8031604369027,12.4788238742032,
131.443016238686)) ;
#149855 = CARTESIAN_POINT('Ctrl Pts',(-21.7040670699751,12.3322479611375,
131.186643032547)) ;
#149856 = CARTESIAN_POINT('Ctrl Pts',(-21.5954848934324,12.2636849703181,
130.902576073362)) ;
#149857 = CARTESIAN_POINT('Ctrl Pts',(-21.4844977011893,12.2782423508481,
130.611495128797)) ;
#149858 = CARTESIAN_POINT('Ctrl Pts',(-21.3784236599933,12.3748788138008,
130.334754138936)) ;
#149859 = CARTESIAN_POINT('Ctrl Pts',(-21.2841566381779,12.5463734301239,
130.092472417729)) ;
#149860 = CARTESIAN_POINT('Ctrl Pts',(-21.2075185163092,12.7810696053441,
129.901748161502)) ;
#149861 = CARTESIAN_POINT('Ctrl Pts',(-21.1535857557247,13.0608632810621,
129.777242893781)) ;
#149862 = CARTESIAN_POINT('Ctrl Pts',(-21.1251082585069,13.3671882377426,
129.727176867914)) ;
#149863 = CARTESIAN_POINT('Ctrl Pts',(-21.1236808485437,13.6783220595412,
129.756215090546)) ;
#149864 = CARTESIAN_POINT('Ctrl Pts',(-21.1486075426851,13.9701100472944,
129.862126299147)) ;
#149865 = CARTESIAN_POINT('Ctrl Pts',(-21.1973535450429,14.2230345165602,
130.037651301572)) ;
#149866 = CARTESIAN_POINT('Ctrl Pts',(-21.2657341311525,14.4186168854027,
130.270535077452)) ;
#149867 = CARTESIAN_POINT('Ctrl Pts',(-21.3480366756193,14.5428705868712,
130.54406387908)) ;
#149868 = CARTESIAN_POINT('Ctrl Pts',(-21.4377691926866,14.5869069851008,
130.839327006419)) ;
#149869 = CARTESIAN_POINT('Ctrl Pts',(-21.5275182421065,14.5480013167689,
131.134553678454)) ;
#149870 = CARTESIAN_POINT('Ctrl Pts',(-21.6110497338832,14.4271740757264,
131.411928848396)) ;
#149871 = CARTESIAN_POINT('Ctrl Pts',(-21.6799255328032,14.2362638789622,
131.646058353633)) ;
#149872 = CARTESIAN_POINT('Ctrl Pts',(-21.7300456232936,13.9863048422078,
131.825612120033)) ;
#149873 = CARTESIAN_POINT('Ctrl Pts',(-21.7564143680409,13.6957298315302,
131.935786982782)) ;
#149874 = CARTESIAN_POINT('Ctrl Pts',(-21.7566600694498,13.3866515918627,
131.969541292452)) ;
#149875 = CARTESIAN_POINT('Ctrl Pts',(-21.729544783517,13.0771469983457,131.923709750482)) ;
#149876 = CARTESIAN_POINT('Ctrl Pts',(-21.6771516178043,12.7963921312271,
131.803576103484)) ;
#149877 = CARTESIAN_POINT('Ctrl Pts',(-21.601485043082,12.5578779663261,131.615788388401)) ;
#149878 = CARTESIAN_POINT('Ctrl Pts',(-21.5083743731948,12.3830735911952,
131.376772518408)) ;
#149879 = CARTESIAN_POINT('Ctrl Pts',(-21.4027033277101,12.2815115328469,
131.101246209364)) ;
#149880 = CARTESIAN_POINT('Ctrl Pts',(-21.2914566395192,12.2623682351307,
130.809508334023)) ;
#149881 = CARTESIAN_POINT('Ctrl Pts',(-21.183156911401,12.3259183972767,130.526081481035)) ;
#149882 = CARTESIAN_POINT('Ctrl Pts',(-21.0831383092239,12.4680808771893,
130.267052456152)) ;
#149883 = CARTESIAN_POINT('Ctrl Pts',(-20.9984926472638,12.6795622431896,
130.052999466313)) ;
#149884 = CARTESIAN_POINT('Ctrl Pts',(-20.9350511107532,12.942589382418,129.900666960476)) ;
#149885 = CARTESIAN_POINT('Ctrl Pts',(-20.8958233184202,13.2417281941733,
129.819283617023)) ;
#149886 = CARTESIAN_POINT('Ctrl Pts',(-20.8834458948203,13.5531901597367,
129.816249612058)) ;
#149887 = CARTESIAN_POINT('Ctrl Pts',(-20.8979142935974,13.8554127215433,
129.891658607767)) ;
#149888 = CARTESIAN_POINT('Ctrl Pts',(-20.9373087909547,14.1261607802399,
130.039800242733)) ;
#149889 = CARTESIAN_POINT('Ctrl Pts',(-20.9986572396186,14.3478084011447,
130.252296892612)) ;
#149890 = CARTESIAN_POINT('Ctrl Pts',(-21.0756161881204,14.5013886239399,
130.510026273036)) ;
#149891 = CARTESIAN_POINT('Ctrl Pts',(-21.1635267894519,14.5792262889595,
130.800096886863)) ;
#149892 = CARTESIAN_POINT('Ctrl Pts',(-21.2541062230571,14.5735423486693,
131.097774254365)) ;
#149893 = CARTESIAN_POINT('Ctrl Pts',(-21.3407174693846,14.4859392632534,
131.383892695644)) ;
#149894 = CARTESIAN_POINT('Ctrl Pts',(-21.4166169572043,14.3210240501096,
131.638882857702)) ;
#149895 = CARTESIAN_POINT('Ctrl Pts',(-21.4747584664031,14.0938130208259,
131.841674679454)) ;
#149896 = CARTESIAN_POINT('Ctrl Pts',(-21.5112781420335,13.8165580564643,
131.981597335147)) ;
#149897 = CARTESIAN_POINT('Ctrl Pts',(-21.5222480980289,13.5127265390552,
132.046676530408)) ;
#149898 = CARTESIAN_POINT('Ctrl Pts',(-21.5061347629943,13.2000972464797,
132.032913742005)) ;
#149899 = CARTESIAN_POINT('Ctrl Pts',(-21.4640156292753,12.9073427660881,
131.942726153517)) ;
#149900 = CARTESIAN_POINT('Ctrl Pts',(-21.397117735376,12.6479572947944,131.780585336987)) ;
#149901 = CARTESIAN_POINT('Ctrl Pts',(-21.3106813900893,12.4461100602533,
131.561069221284)) ;
#149902 = CARTESIAN_POINT('Ctrl Pts',(-21.2086821275541,12.3127706355445,
131.296414857345)) ;
#149903 = CARTESIAN_POINT('Ctrl Pts',(-21.0995344791146,12.2601401093184,
131.010556487313)) ;
#149904 = CARTESIAN_POINT('Ctrl Pts',(-20.9889798404996,12.2901733170219,
130.720722307534)) ;
#149905 = CARTESIAN_POINT('Ctrl Pts',(-20.8845090238334,12.4015832972313,
130.448684666842)) ;
#149906 = CARTESIAN_POINT('Ctrl Pts',(-20.7929548516875,12.5866483743453,
130.214420543969)) ;
#149907 = CARTESIAN_POINT('Ctrl Pts',(-20.720494862863,12.8302723297284,130.035755542928)) ;
#149908 = CARTESIAN_POINT('Ctrl Pts',(-20.6708320754766,13.1192440323379,
129.924028986074)) ;
#149909 = CARTESIAN_POINT('Ctrl Pts',(-20.6477168971474,13.4254781979924,
129.889340729932)) ;
#149910 = CARTESIAN_POINT('Ctrl Pts',(-20.6512834404018,13.735359683146,129.933026055129)) ;
#149911 = CARTESIAN_POINT('Ctrl Pts',(-20.6809119562705,14.0210481955409,
130.052635771819)) ;
#149912 = CARTESIAN_POINT('Ctrl Pts',(-20.7338408988299,14.2649914593589,
130.240457331941)) ;
#149913 = CARTESIAN_POINT('Ctrl Pts',(-20.8051898847713,14.4476746883627,
130.481943155495)) ;
#149914 = CARTESIAN_POINT('Ctrl Pts',(-20.8894411703123,14.5574099930499,
130.761185950254)) ;
#149915 = CARTESIAN_POINT('Ctrl Pts',(-20.9796503552771,14.5860647522522,
131.057792726659)) ;
#149916 = CARTESIAN_POINT('Ctrl Pts',(-21.0692814846415,14.5307819491484,
131.352933777741)) ;
#149917 = CARTESIAN_POINT('Ctrl Pts',(-21.1498107519784,14.3969445600344,
131.621163297151)) ;
#149918 = CARTESIAN_POINT('Ctrl Pts',(-21.2160230444839,14.1927449819674,
131.847762712336)) ;
#149919 = CARTESIAN_POINT('Ctrl Pts',(-21.2617909617919,13.9340125126876,
132.014532566798)) ;
#149920 = CARTESIAN_POINT('Ctrl Pts',(-21.2834169760681,13.6381122428634,
132.110859969198)) ;
#149921 = CARTESIAN_POINT('Ctrl Pts',(-21.2784641686458,13.3270743882958,
132.129508993966)) ;
#149922 = CARTESIAN_POINT('Ctrl Pts',(-21.2465760701754,13.022510775008,132.069516737505)) ;
#149923 = CARTESIAN_POINT('Ctrl Pts',(-21.1892311552638,12.7468021187138,
131.935157683102)) ;
#149924 = CARTESIAN_POINT('Ctrl Pts',(-21.1103505322267,12.5205888533643,
131.737718520491)) ;
#149925 = CARTESIAN_POINT('Ctrl Pts',(-21.0140654020534,12.3578210122937,
131.489600695312)) ;
#149926 = CARTESIAN_POINT('Ctrl Pts',(-20.9069519089274,12.2716455027741,
131.209820749627)) ;
#149927 = CARTESIAN_POINT('Ctrl Pts',(-20.7959007646827,12.2679542835663,
130.91854323311)) ;
#149928 = CARTESIAN_POINT('Ctrl Pts',(-20.6882404753147,12.3469221374096,
130.637139748733)) ;
#149929 = CARTESIAN_POINT('Ctrl Pts',(-20.590745173864,12.5030897490068,130.385469307244)) ;
#149930 = CARTESIAN_POINT('Ctrl Pts',(-20.5098618731191,12.7250181142628,
130.182298437456)) ;
#149931 = CARTESIAN_POINT('Ctrl Pts',(-20.4505145686487,12.997182712002,130.042072465219)) ;
#149932 = CARTESIAN_POINT('Ctrl Pts',(-20.4163461458151,13.2997827331154,
129.97538649999)) ;
#149933 = CARTESIAN_POINT('Ctrl Pts',(-20.4090290392878,13.6108909290664,
129.98710788454)) ;
#149934 = CARTESIAN_POINT('Ctrl Pts',(-20.4282921071053,13.9087322628313,
130.076489390265)) ;
#149935 = CARTESIAN_POINT('Ctrl Pts',(-20.4722899184275,14.1725575472539,
130.238237437672)) ;
#149936 = CARTESIAN_POINT('Ctrl Pts',(-20.5367340681886,14.3815587405522,
130.4595615294)) ;
#149937 = CARTESIAN_POINT('Ctrl Pts',(-20.6165397161228,14.5223295633007,
130.725809297898)) ;
#149938 = CARTESIAN_POINT('Ctrl Pts',(-20.7051933027261,14.5844939623778,
131.017890368957)) ;
#149939 = CARTESIAN_POINT('Ctrl Pts',(-20.7959857696704,14.5631534424975,
131.316353588216)) ;
#149940 = CARTESIAN_POINT('Ctrl Pts',(-20.8807942840004,14.4606751322893,
131.597113045962)) ;
#149941 = CARTESIAN_POINT('Ctrl Pts',(-20.9539376095154,14.2826954398612,
131.844058123702)) ;
#149942 = CARTESIAN_POINT('Ctrl Pts',(-21.0083263347871,14.0447463788915,
132.03593245135)) ;
#149943 = CARTESIAN_POINT('Ctrl Pts',(-21.040197088768,13.7613771395104,132.162181015758)) ;
#149944 = CARTESIAN_POINT('Ctrl Pts',(-21.0461960024793,13.4542323467487,
132.212789454969)) ;
#149945 = CARTESIAN_POINT('Ctrl Pts',(-21.0251622314024,13.1437994705374,
132.184546651193)) ;
#149946 = CARTESIAN_POINT('Ctrl Pts',(-20.977827703154,12.8538469195634,132.079426774606)) ;
#149947 = CARTESIAN_POINT('Ctrl Pts',(-20.907128727735,12.6054873461084,131.905959845305)) ;
#149948 = CARTESIAN_POINT('Ctrl Pts',(-20.8174409553095,12.4153273171675,
131.676988843587)) ;
#149949 = CARTESIAN_POINT('Ctrl Pts',(-20.713143280337,12.2964112453651,131.405684529226)) ;
#149950 = CARTESIAN_POINT('Ctrl Pts',(-20.6033763157009,12.2594155907016,
131.117980797481)) ;
#149951 = CARTESIAN_POINT('Ctrl Pts',(-20.4932077646269,12.3053349417689,
130.829346648373)) ;
#149952 = CARTESIAN_POINT('Ctrl Pts',(-20.3910080733494,12.4312258982637,
130.563852755589)) ;
#149953 = CARTESIAN_POINT('Ctrl Pts',(-20.3027473879503,12.627959699626,130.339118872896)) ;
#149954 = CARTESIAN_POINT('Ctrl Pts',(-20.2340446900552,12.8824932642082,
130.171614220239)) ;
#149955 = CARTESIAN_POINT('Ctrl Pts',(-20.1895024515561,13.1745455141317,
130.074542304732)) ;
#149956 = CARTESIAN_POINT('Ctrl Pts',(-20.1711377465811,13.4851755332174,
130.05403371038)) ;
#149957 = CARTESIAN_POINT('Ctrl Pts',(-20.1799007530891,13.7921378916297,
130.112861990177)) ;
#149958 = CARTESIAN_POINT('Ctrl Pts',(-20.2141338523858,14.0710147358115,
130.245900077458)) ;
#149959 = CARTESIAN_POINT('Ctrl Pts',(-20.2709644008969,14.3045451630866,
130.445096643664)) ;
#149960 = CARTESIAN_POINT('Ctrl Pts',(-20.3450269541787,14.4740865668841,
130.694444672256)) ;
#149961 = CARTESIAN_POINT('Ctrl Pts',(-20.4312885839604,14.5693022255178,
130.979690231724)) ;
#149962 = CARTESIAN_POINT('Ctrl Pts',(-20.5217224177781,14.5820126404232,
131.276907919029)) ;
#149963 = CARTESIAN_POINT('Ctrl Pts',(-20.6102794068549,14.511227148385,131.56889920101)) ;
#149964 = CARTESIAN_POINT('Ctrl Pts',(-20.6884126712052,14.3635592095882,
131.830093439836)) ;
#149965 = CARTESIAN_POINT('Ctrl Pts',(-20.751162116013,14.1479540457657,132.046552023884)) ;
#149966 = CARTESIAN_POINT('Ctrl Pts',(-20.7926884527049,13.8806548150988,
132.200960049177)) ;
#149967 = CARTESIAN_POINT('Ctrl Pts',(-20.8094672658813,13.5796274976099,
132.283185376369)) ;
#149968 = CARTESIAN_POINT('Ctrl Pts',(-20.7992847698798,13.2675903207149,
132.286621512042)) ;
#149969 = CARTESIAN_POINT('Ctrl Pts',(-20.7626296984893,12.9685393954342,
132.212514858308)) ;
#149970 = CARTESIAN_POINT('Ctrl Pts',(-20.7008934220108,12.7001828412868,
132.065351539406)) ;
#149971 = CARTESIAN_POINT('Ctrl Pts',(-20.6181564504024,12.484351447388,131.856740622627)) ;
#149972 = CARTESIAN_POINT('Ctrl Pts',(-20.5192778681803,12.3354378229303,
131.60104993334)) ;
#149973 = CARTESIAN_POINT('Ctrl Pts',(-20.4111933713258,12.2645466644513,
131.318338142685)) ;
#149974 = CARTESIAN_POINT('Ctrl Pts',(-20.2996662166456,12.2767400310682,
131.025835168853)) ;
#149975 = CARTESIAN_POINT('Ctrl Pts',(-20.1937352114642,12.3708038596253,
130.749389711576)) ;
#149976 = CARTESIAN_POINT('Ctrl Pts',(-20.0988429416229,12.5405713719576,
130.505353011285)) ;
#149977 = CARTESIAN_POINT('Ctrl Pts',(-20.021843202684,12.7727635932404,130.31345487307)) ;
#149978 = CARTESIAN_POINT('Ctrl Pts',(-19.9668156943562,13.0532481868504,
130.185965715989)) ;
#149979 = CARTESIAN_POINT('Ctrl Pts',(-19.9377532447316,13.3594503322591,
130.134212682871)) ;
#149980 = CARTESIAN_POINT('Ctrl Pts',(-19.9355477333015,13.6687250263673,
130.16075894901)) ;
#149981 = CARTESIAN_POINT('Ctrl Pts',(-19.9597474888427,13.9622483916866,
130.26464405238)) ;
#149982 = CARTESIAN_POINT('Ctrl Pts',(-20.0078395553135,14.216383713817,130.438234282855)) ;
#149983 = CARTESIAN_POINT('Ctrl Pts',(-20.0759089225194,14.4143549366633,
130.670296074007)) ;
#149984 = CARTESIAN_POINT('Ctrl Pts',(-20.157927076402,14.5404303817965,130.942989232008)) ;
#149985 = CARTESIAN_POINT('Ctrl Pts',(-20.2471634575349,14.5868747918771,
131.236660122781)) ;
#149986 = CARTESIAN_POINT('Ctrl Pts',(-20.3375200447807,14.5499212465235,
131.533862304864)) ;
#149987 = CARTESIAN_POINT('Ctrl Pts',(-20.4206467735753,14.4324626280189,
131.809760427588)) ;
#149988 = CARTESIAN_POINT('Ctrl Pts',(-20.4906530935794,14.2419356925952,
132.04749075942)) ;
#149989 = CARTESIAN_POINT('Ctrl Pts',(-20.5411214430323,13.9939564781135,
132.227948854795)) ;
#149990 = CARTESIAN_POINT('Ctrl Pts',(-20.5682544096884,13.704318184283,132.340358463569)) ;
#149991 = CARTESIAN_POINT('Ctrl Pts',(-20.5692014180171,13.3953698080797,
132.376173579921)) ;
#149992 = CARTESIAN_POINT('Ctrl Pts',(-20.543054261984,13.0868084154143,132.333020355237)) ;
#149993 = CARTESIAN_POINT('Ctrl Pts',(-20.4911384960752,12.8035341969557,
132.214453828355)) ;
#149994 = CARTESIAN_POINT('Ctrl Pts',(-20.4161441436802,12.5639567807414,
132.028575184502)) ;
#149995 = CARTESIAN_POINT('Ctrl Pts',(-20.323298875788,12.3867441637874,131.790400600433)) ;
#149996 = CARTESIAN_POINT('Ctrl Pts',(-20.2176703488979,12.2832559851663,
131.515052106227)) ;
#149997 = CARTESIAN_POINT('Ctrl Pts',(-20.1074375512045,12.2616345605918,
131.225985798419)) ;
#149998 = CARTESIAN_POINT('Ctrl Pts',(-19.9980972507774,12.3231638536054,
130.939790413276)) ;
#149999 = CARTESIAN_POINT('Ctrl Pts',(-19.8981987414102,12.4627499394219,
130.680958618524)) ;
#150000 = CARTESIAN_POINT('Ctrl Pts',(-19.8127745396768,12.6729052718455,
130.464725436601)) ;
#150001 = CARTESIAN_POINT('Ctrl Pts',(-19.7487491589229,12.9344259227914,
130.310649365382)) ;
#150002 = CARTESIAN_POINT('Ctrl Pts',(-19.7086902319659,13.2340773776093,
130.226969486189)) ;
#150003 = CARTESIAN_POINT('Ctrl Pts',(-19.6956791745323,13.5439037579597,
130.221914932001)) ;
#150004 = CARTESIAN_POINT('Ctrl Pts',(-19.7092885690522,13.8465580418888,
130.294793249448)) ;
#150005 = CARTESIAN_POINT('Ctrl Pts',(-19.7480403292005,14.1188038713519,
130.441095578693)) ;
#150006 = CARTESIAN_POINT('Ctrl Pts',(-19.8087237127228,14.3420290100945,
130.651608670912)) ;
#150007 = CARTESIAN_POINT('Ctrl Pts',(-19.8855246325867,14.4980359942342,
130.908974260646)) ;
#150008 = CARTESIAN_POINT('Ctrl Pts',(-19.9728075519884,14.5780642273586,
131.197048865793)) ;
#150009 = CARTESIAN_POINT('Ctrl Pts',(-20.0641053332561,14.5747644826435,
131.497087362298)) ;
#150010 = CARTESIAN_POINT('Ctrl Pts',(-20.1504360631443,14.4895501610045,
131.78220700389)) ;
#150011 = CARTESIAN_POINT('Ctrl Pts',(-20.2266398469847,14.3274512492284,
132.038011928508)) ;
#150012 = CARTESIAN_POINT('Ctrl Pts',(-20.2855836739268,14.1012132638127,
132.24325861374)) ;
#150013 = CARTESIAN_POINT('Ctrl Pts',(-20.322802771727,13.8249845460598,132.38523118764)) ;
#150014 = CARTESIAN_POINT('Ctrl Pts',(-20.3344826698602,13.5214322498008,
132.452410552018)) ;
#150015 = CARTESIAN_POINT('Ctrl Pts',(-20.3193210016494,13.2103012906498,
132.441249802482)) ;
#150016 = CARTESIAN_POINT('Ctrl Pts',(-20.2777434342537,12.9148532229271,
132.35285539736)) ;
#150017 = CARTESIAN_POINT('Ctrl Pts',(-20.2114185666706,12.6543478093024,
132.19237858542)) ;
#150018 = CARTESIAN_POINT('Ctrl Pts',(-20.1256275275734,12.4511189000955,
131.974692258579)) ;
#150019 = CARTESIAN_POINT('Ctrl Pts',(-20.0242015823174,12.3156705580683,
131.711643730949)) ;
#150020 = CARTESIAN_POINT('Ctrl Pts',(-19.9146972236327,12.2603783302423,
131.424892243311)) ;
#150021 = CARTESIAN_POINT('Ctrl Pts',(-19.804137467759,12.2883877203707,131.13502656788)) ;
#150022 = CARTESIAN_POINT('Ctrl Pts',(-19.699816800067,12.396958249081,130.86328933831)) ;
#150023 = CARTESIAN_POINT('Ctrl Pts',(-19.6074508319546,12.5805839633338,
130.626767342191)) ;
#150024 = CARTESIAN_POINT('Ctrl Pts',(-19.534586073173,12.8225431186843,130.446872902408)) ;
#150025 = CARTESIAN_POINT('Ctrl Pts',(-19.48430105852,13.1085293603561,130.333118269165)) ;
#150026 = CARTESIAN_POINT('Ctrl Pts',(-19.4601499587593,13.4184312880114,
130.29583788212)) ;
#150027 = CARTESIAN_POINT('Ctrl Pts',(-19.4629889713343,13.725396861632,130.337043757937)) ;
#150028 = CARTESIAN_POINT('Ctrl Pts',(-19.4919997843254,14.0140710256624,
130.455081243063)) ;
#150029 = CARTESIAN_POINT('Ctrl Pts',(-19.5442604752578,14.2586953044857,
130.640856243093)) ;
#150030 = CARTESIAN_POINT('Ctrl Pts',(-19.6152214709248,14.4435712314573,
130.881253585167)) ;
#150031 = CARTESIAN_POINT('Ctrl Pts',(-19.6991862638108,14.5554638006899,
131.159645901593)) ;
#150032 = CARTESIAN_POINT('Ctrl Pts',(-19.7894150942462,14.5862678502932,
131.45634808166)) ;
#150033 = CARTESIAN_POINT('Ctrl Pts',(-19.8785826985735,14.5339455436029,
131.749904644687)) ;
#150034 = CARTESIAN_POINT('Ctrl Pts',(-19.9598958275185,14.4019055973539,
132.020594708233)) ;
#150035 = CARTESIAN_POINT('Ctrl Pts',(-20.0265337164306,14.1996929983724,
132.248397159288)) ;
#150036 = CARTESIAN_POINT('Ctrl Pts',(-20.0730460777264,13.9418840737313,
132.417403083246)) ;
#150037 = CARTESIAN_POINT('Ctrl Pts',(-20.0953762004544,13.6467946760401,
132.515776294982)) ;
#150038 = CARTESIAN_POINT('Ctrl Pts',(-20.0911858048577,13.3358858786889,
132.536654639505)) ;
#150039 = CARTESIAN_POINT('Ctrl Pts',(-20.0600962019105,13.0311284856173,
132.47895867768)) ;
#150040 = CARTESIAN_POINT('Ctrl Pts',(-20.0034577116224,12.7543596486341,
132.346659990378)) ;
#150041 = CARTESIAN_POINT('Ctrl Pts',(-19.9252445945777,12.5263865010007,
132.151152771168)) ;
#150042 = CARTESIAN_POINT('Ctrl Pts',(-19.8285737015795,12.3607018495905,
131.902162071254)) ;
#150043 = CARTESIAN_POINT('Ctrl Pts',(-19.7226384575838,12.2732420345152,
131.625515596499)) ;
#150044 = CARTESIAN_POINT('Ctrl Pts',(-19.6111674213246,12.2668291057712,
131.333147098468)) ;
#150045 = CARTESIAN_POINT('Ctrl Pts',(-19.5033876747326,12.3436151679642,
131.051371024019)) ;
#150046 = CARTESIAN_POINT('Ctrl Pts',(-19.40539646053,12.4979166687538,130.79829315841)) ;
#150047 = CARTESIAN_POINT('Ctrl Pts',(-19.3240491831095,12.7181779713464,
130.593748829707)) ;
#150048 = CARTESIAN_POINT('Ctrl Pts',(-19.2641202298485,12.9887183065796,
130.451770199842)) ;
#150049 = CARTESIAN_POINT('Ctrl Pts',(-19.2291670799778,13.2908825887428,
130.382809693789)) ;
#150050 = CARTESIAN_POINT('Ctrl Pts',(-19.2210624747814,13.6021682784688,
130.392241564163)) ;
#150051 = CARTESIAN_POINT('Ctrl Pts',(-19.2396860598708,13.9015372403182,
130.47985199514)) ;
#150052 = CARTESIAN_POINT('Ctrl Pts',(-19.2830862718829,14.1661756912177,
130.639822284067)) ;
#150053 = CARTESIAN_POINT('Ctrl Pts',(-19.3468000223966,14.3763136257562,
130.858909722296)) ;
#150054 = CARTESIAN_POINT('Ctrl Pts',(-19.4264441058091,14.5195378836765,
131.124765334975)) ;
#150055 = CARTESIAN_POINT('Ctrl Pts',(-19.5147201923918,14.5837467686513,
131.415658330279)) ;
#150056 = CARTESIAN_POINT('Ctrl Pts',(-19.6054851848399,14.5651055728363,
131.714010716355)) ;
#150057 = CARTESIAN_POINT('Ctrl Pts',(-19.6908231045242,14.4645029027952,
131.996426898387)) ;
#150058 = CARTESIAN_POINT('Ctrl Pts',(-19.7641560074583,14.2890440216263,
132.243815754987)) ;
#150059 = CARTESIAN_POINT('Ctrl Pts',(-19.8192252487056,14.0526945141533,
132.437694359878)) ;
#150060 = CARTESIAN_POINT('Ctrl Pts',(-19.8518415513689,13.769986617102,132.566162345859)) ;
#150061 = CARTESIAN_POINT('Ctrl Pts',(-19.8586489010726,13.4631529516268,
132.619138437853)) ;
#150062 = CARTESIAN_POINT('Ctrl Pts',(-19.8381858668256,13.1513621108982,
132.592691996163)) ;
#150063 = CARTESIAN_POINT('Ctrl Pts',(-19.7919813808844,12.8627668355385,
132.490607274321)) ;
#150064 = CARTESIAN_POINT('Ctrl Pts',(-19.7213546290731,12.6109028724027,
132.317625946872)) ;
#150065 = CARTESIAN_POINT('Ctrl Pts',(-19.6324894396037,12.420019305974,132.090897675296)) ;
#150066 = CARTESIAN_POINT('Ctrl Pts',(-19.5284529577394,12.2986947230639,
131.820380912839)) ;
#150067 = CARTESIAN_POINT('Ctrl Pts',(-19.4189287181224,12.259272392657,131.5333369683)) ;
#150068 = CARTESIAN_POINT('Ctrl Pts',(-19.3083138956178,12.3030853474754,
131.243507528801)) ;
#150069 = CARTESIAN_POINT('Ctrl Pts',(-19.2063363439977,12.4259705757025,
130.978478363128)) ;
#150070 = CARTESIAN_POINT('Ctrl Pts',(-19.1169914034161,12.6220549882292,
130.750798394588)) ;
#150071 = CARTESIAN_POINT('Ctrl Pts',(-19.0479500852708,12.8744669108447,
130.582186724412)) ;
#150072 = CARTESIAN_POINT('Ctrl Pts',(-19.0025666487703,13.1663405634683,
130.482735394788)) ;
#150073 = CARTESIAN_POINT('Ctrl Pts',(-18.9835597805517,13.4758788255352,
130.460255917191)) ;
#150074 = CARTESIAN_POINT('Ctrl Pts',(-18.9913631683965,13.7823952267848,
130.516170859479)) ;
#150075 = CARTESIAN_POINT('Ctrl Pts',(-19.0251922780675,14.0644181271455,
130.648288433154)) ;
#150076 = CARTESIAN_POINT('Ctrl Pts',(-19.0810022453044,14.2977470624668,
130.844241092897)) ;
#150077 = CARTESIAN_POINT('Ctrl Pts',(-19.1550953089256,14.470619356869,131.093908367077)) ;
#150078 = CARTESIAN_POINT('Ctrl Pts',(-19.2408649444371,14.5675954870708,
131.37760184104)) ;
#150079 = CARTESIAN_POINT('Ctrl Pts',(-19.331312849513,14.5827756114501,131.674886283311)) ;
#150080 = CARTESIAN_POINT('Ctrl Pts',(-19.4196868659102,14.5148009028155,
131.966202591199)) ;
#150081 = CARTESIAN_POINT('Ctrl Pts',(-19.4984938247197,14.369224395635,132.229462715935)) ;
#150082 = CARTESIAN_POINT('Ctrl Pts',(-19.5620352226328,14.1540995770501,
132.448398160212)) ;
#150083 = CARTESIAN_POINT('Ctrl Pts',(-19.6039630489008,13.8891947674814,
132.60382128396)) ;
#150084 = CARTESIAN_POINT('Ctrl Pts',(-19.6215605930756,13.5894850421774,
132.688377146492)) ;
#150085 = CARTESIAN_POINT('Ctrl Pts',(-19.612225543082,13.2771023843451,132.694326506547)) ;
#150086 = CARTESIAN_POINT('Ctrl Pts',(-19.576287627729,12.9767130862842,132.622385343517)) ;
#150087 = CARTESIAN_POINT('Ctrl Pts',(-19.514916360472,12.7063603271624,132.476405969442)) ;
#150088 = CARTESIAN_POINT('Ctrl Pts',(-19.4331680822589,12.4901610418877,
132.270491422667)) ;
#150089 = CARTESIAN_POINT('Ctrl Pts',(-19.3346192424875,12.3386882869186,
132.015797856231)) ;
#150090 = CARTESIAN_POINT('Ctrl Pts',(-19.2264990527328,12.2654833410071,
131.73304515697)) ;
#150091 = CARTESIAN_POINT('Ctrl Pts',(-19.1153149338654,12.2750423619251,
131.44142995182)) ;
#150092 = CARTESIAN_POINT('Ctrl Pts',(-19.0086090943406,12.3673308735559,
131.162894773645)) ;
#150093 = CARTESIAN_POINT('Ctrl Pts',(-18.9137735051228,12.5343468737747,
130.9188596151)) ;
#150094 = CARTESIAN_POINT('Ctrl Pts',(-18.8359718102372,12.7652870390172,
130.724693720235)) ;
#150095 = CARTESIAN_POINT('Ctrl Pts',(-18.7803364844381,13.0444118412715,
130.5953903177)) ;
#150096 = CARTESIAN_POINT('Ctrl Pts',(-18.7504170703459,13.3498616588083,
130.541106996476)) ;
#150097 = CARTESIAN_POINT('Ctrl Pts',(-18.7474986385281,13.6613614501294,
130.565792830486)) ;
#150098 = CARTESIAN_POINT('Ctrl Pts',(-18.770895305451,13.9537821761938,130.667122829529)) ;
#150099 = CARTESIAN_POINT('Ctrl Pts',(-18.8183173068615,14.2096141280325,
130.838782877024)) ;
#150100 = CARTESIAN_POINT('Ctrl Pts',(-18.8857427274339,14.4090573125523,
131.06889618268)) ;
#150101 = CARTESIAN_POINT('Ctrl Pts',(-18.9673787677367,14.5378227703646,
131.340470029779)) ;
#150102 = CARTESIAN_POINT('Ctrl Pts',(-19.0571958207579,14.586641023904,131.636096348978)) ;
#150103 = CARTESIAN_POINT('Ctrl Pts',(-19.1467790983166,14.5524956993372,
131.930711805515)) ;
#150104 = CARTESIAN_POINT('Ctrl Pts',(-19.2309617987245,14.4363359778134,
132.210003154507)) ;
#150105 = CARTESIAN_POINT('Ctrl Pts',(-19.300918514833,14.2487612489542,132.447357659532)) ;
#150106 = CARTESIAN_POINT('Ctrl Pts',(-19.3521712301763,14.001996361713,132.630173766833)) ;
#150107 = CARTESIAN_POINT('Ctrl Pts',(-19.3800605103585,13.7133413728872,
132.744778521747)) ;
#150108 = CARTESIAN_POINT('Ctrl Pts',(-19.3817028074299,13.4034231145874,
132.782762033844)) ;
#150109 = CARTESIAN_POINT('Ctrl Pts',(-19.3565445968679,13.096615616376,132.742260368403)) ;
#150110 = CARTESIAN_POINT('Ctrl Pts',(-19.3050439571965,12.8104956483767,
132.625124675271)) ;
#150111 = CARTESIAN_POINT('Ctrl Pts',(-19.2310094888665,12.5707042667784,
132.441871024858)) ;
#150112 = CARTESIAN_POINT('Ctrl Pts',(-19.1385073184765,12.391019395432,132.204759045366)) ;
#150113 = CARTESIAN_POINT('Ctrl Pts',(-19.0333885201903,12.2853288824572,
131.930823316902)) ;
#150114 = CARTESIAN_POINT('Ctrl Pts',(-18.9228482359354,12.2609818492728,
131.640971207791)) ;
#150115 = CARTESIAN_POINT('Ctrl Pts',(-18.8130720194284,12.320475723284,131.353587807363)) ;
#150116 = CARTESIAN_POINT('Ctrl Pts',(-18.7128689247104,12.4582515201719,
131.093872581941)) ;
#150117 = CARTESIAN_POINT('Ctrl Pts',(-18.6272057293813,12.6658997536836,
130.876826622372)) ;
#150118 = CARTESIAN_POINT('Ctrl Pts',(-18.5624249500162,12.9268094738204,
130.720624674853)) ;
#150119 = CARTESIAN_POINT('Ctrl Pts',(-18.5218696438751,13.2233760165972,
130.635234806146)) ;
#150120 = CARTESIAN_POINT('Ctrl Pts',(-18.5078382142161,13.5346575170046,
130.62736814531)) ;
#150121 = CARTESIAN_POINT('Ctrl Pts',(-18.5207859995942,13.8387959699086,
130.698413100486)) ;
#150122 = CARTESIAN_POINT('Ctrl Pts',(-18.5589704650504,14.1123016431052,
130.843088517918)) ;
#150123 = CARTESIAN_POINT('Ctrl Pts',(-18.6189702798864,14.3364686131329,
131.051516258642)) ;
#150124 = CARTESIAN_POINT('Ctrl Pts',(-18.6953756786293,14.4947707498965,
131.307733622343)) ;
#150125 = CARTESIAN_POINT('Ctrl Pts',(-18.7828513417895,14.5769227712613,
131.596511728995)) ;
#150126 = CARTESIAN_POINT('Ctrl Pts',(-18.8731056944461,14.5762675707607,
131.893112870536)) ;
#150127 = CARTESIAN_POINT('Ctrl Pts',(-18.9604254053233,14.493055502163,132.181412688869)) ;
#150128 = CARTESIAN_POINT('Ctrl Pts',(-19.0368313978755,14.3331651665745,
132.437726971307)) ;
#150129 = CARTESIAN_POINT('Ctrl Pts',(-19.096452344443,14.1081177718604,132.645025662247)) ;
#150130 = CARTESIAN_POINT('Ctrl Pts',(-19.1342305945688,13.8340180428126,
132.788508335971)) ;
#150131 = CARTESIAN_POINT('Ctrl Pts',(-19.1467439432002,13.5302900584997,
132.858206622598)) ;
#150132 = CARTESIAN_POINT('Ctrl Pts',(-19.1323635330917,13.2194243094674,
132.849285246013)) ;
#150133 = CARTESIAN_POINT('Ctrl Pts',(-19.0915547199997,12.9232189359804,
132.763138594267)) ;
#150134 = CARTESIAN_POINT('Ctrl Pts',(-19.0259667523677,12.6614613466154,
132.604790806233)) ;
#150135 = CARTESIAN_POINT('Ctrl Pts',(-18.9405194772865,12.4560560790089,
132.38817454474)) ;
#150136 = CARTESIAN_POINT('Ctrl Pts',(-18.8397676633806,12.3187614770299,
132.12698805268)) ;
#150137 = CARTESIAN_POINT('Ctrl Pts',(-18.7302531161927,12.2608758941321,
131.840261818826)) ;
#150138 = CARTESIAN_POINT('Ctrl Pts',(-18.6197960101115,12.2860567415008,
131.550633129398)) ;
#150139 = CARTESIAN_POINT('Ctrl Pts',(-18.5143020976164,12.3936760642326,
131.275774302405)) ;
#150140 = CARTESIAN_POINT('Ctrl Pts',(-18.4225005529432,12.5734426987992,
131.040533763975)) ;
#150141 = CARTESIAN_POINT('Ctrl Pts',(-18.3483666747467,12.8155556665824,
130.857196460178)) ;
#150142 = CARTESIAN_POINT('Ctrl Pts',(-18.2976375855543,13.1001458874772,
130.742065616185)) ;
#150143 = CARTESIAN_POINT('Ctrl Pts',(-18.2727174764149,13.4082451870112,
130.70239118206)) ;
#150144 = CARTESIAN_POINT('Ctrl Pts',(-18.2747208829564,13.7170001852575,
130.741310681003)) ;
#150145 = CARTESIAN_POINT('Ctrl Pts',(-18.3031428718883,14.0068803460707,
130.857672223853)) ;
#150146 = CARTESIAN_POINT('Ctrl Pts',(-18.3546279874812,14.2520830316222,
131.041068421816)) ;
#150147 = CARTESIAN_POINT('Ctrl Pts',(-18.4249893528057,14.4388654813696,
131.279674482647)) ;
#150148 = CARTESIAN_POINT('Ctrl Pts',(-18.5087523962848,14.5532758693692,
131.557517303815)) ;
#150149 = CARTESIAN_POINT('Ctrl Pts',(-18.5989724091081,14.5866372914021,
131.854217352645)) ;
#150150 = CARTESIAN_POINT('Ctrl Pts',(-18.688512540162,14.536325428207,132.148960312918)) ;
#150151 = CARTESIAN_POINT('Ctrl Pts',(-18.7697882731236,14.4070821895425,
132.419388304922)) ;
#150152 = CARTESIAN_POINT('Ctrl Pts',(-18.837264340709,14.2058492618622,132.649795674961)) ;
#150153 = CARTESIAN_POINT('Ctrl Pts',(-18.8842859072995,13.9493210754263,
132.820267948791)) ;
#150154 = CARTESIAN_POINT('Ctrl Pts',(-18.9072831227603,13.6560817466226,
132.920472843849)) ;
#150155 = CARTESIAN_POINT('Ctrl Pts',(-18.9039153111855,13.3454214916358,
132.943747640608)) ;
#150156 = CARTESIAN_POINT('Ctrl Pts',(-18.8737437347605,13.0405959101595,
132.888677922555)) ;
#150157 = CARTESIAN_POINT('Ctrl Pts',(-18.8174933706068,12.7610204461784,
132.757709543441)) ;
#150158 = CARTESIAN_POINT('Ctrl Pts',(-18.7398455096899,12.5320805798767,
132.56380909295)) ;
#150159 = CARTESIAN_POINT('Ctrl Pts',(-18.6443213273581,12.3651154017827,
132.317940745462)) ;
#150160 = CARTESIAN_POINT('Ctrl Pts',(-18.5377336770975,12.2743250187668,
132.039668340086)) ;
#150161 = CARTESIAN_POINT('Ctrl Pts',(-18.426213086566,12.2660445050815,131.747170907628)) ;
#150162 = CARTESIAN_POINT('Ctrl Pts',(-18.318662949734,12.3402670873944,131.465941046569)) ;
#150163 = CARTESIAN_POINT('Ctrl Pts',(-18.2202545547588,12.4924310818324,
131.211652318231)) ;
#150164 = CARTESIAN_POINT('Ctrl Pts',(-18.1384496981742,12.7106680082788,
131.0057297513)) ;
#150165 = CARTESIAN_POINT('Ctrl Pts',(-18.0776794875304,12.9803448576749,
130.861345367367)) ;
#150166 = CARTESIAN_POINT('Ctrl Pts',(-18.0419366209274,13.2833169308344,
130.790224557314)) ;
#150167 = CARTESIAN_POINT('Ctrl Pts',(-18.0331437091799,13.5926826730587,
130.797434096829)) ;
#150168 = CARTESIAN_POINT('Ctrl Pts',(-18.0510291214455,13.8936496800992,
130.882992090183)) ;
#150169 = CARTESIAN_POINT('Ctrl Pts',(-18.0936826181807,14.1589429573028,
131.040700633816)) ;
#150170 = CARTESIAN_POINT('Ctrl Pts',(-18.1569645287966,14.371150690962,131.258583540615)) ;
#150171 = CARTESIAN_POINT('Ctrl Pts',(-18.2359601650018,14.5162610236172,
131.522432886244)) ;
#150172 = CARTESIAN_POINT('Ctrl Pts',(-18.324804161584,14.5833063391636,131.815260245813)) ;
#150173 = CARTESIAN_POINT('Ctrl Pts',(-18.4153699590213,14.5665129861826,
132.1129409694)) ;
#150174 = CARTESIAN_POINT('Ctrl Pts',(-18.5006408256147,14.4685224536154,
132.39504774045)) ;
#150175 = CARTESIAN_POINT('Ctrl Pts',(-18.5743747429956,14.2954966749806,
132.643565116707)) ;
#150176 = CARTESIAN_POINT('Ctrl Pts',(-18.6302405909945,14.0596947072176,
132.839910707945)) ;
#150177 = CARTESIAN_POINT('Ctrl Pts',(-18.6635175583225,13.7784556667528,
132.970247185244)) ;
#150178 = CARTESIAN_POINT('Ctrl Pts',(-18.6709408038792,13.4704205936671,
133.025199141352)) ;
#150179 = CARTESIAN_POINT('Ctrl Pts',(-18.6516378389852,13.1626907214352,
133.001667851695)) ;
#150180 = CARTESIAN_POINT('Ctrl Pts',(-18.6057075222045,12.8697533437124,
132.900784883066)) ;
#150181 = CARTESIAN_POINT('Ctrl Pts',(-18.5363453302047,12.618666846953,132.731185914356)) ;
#150182 = CARTESIAN_POINT('Ctrl Pts',(-18.4471574026767,12.424057056317,132.503835420592)) ;
#150183 = CARTESIAN_POINT('Ctrl Pts',(-18.3445263647179,12.301712900972,132.237061004765)) ;
#150184 = CARTESIAN_POINT('Ctrl Pts',(-18.234308555707,12.2592124432014,131.948249300947)) ;
#150185 = CARTESIAN_POINT('Ctrl Pts',(-18.1241338500386,12.300200425655,131.659524177675)) ;
#150186 = CARTESIAN_POINT('Ctrl Pts',(-18.0207803153287,12.4222100084694,
131.390831333215)) ;
#150187 = CARTESIAN_POINT('Ctrl Pts',(-17.9317044908737,12.6151763749812,
131.163672662444)) ;
#150188 = CARTESIAN_POINT('Ctrl Pts',(-17.8617861726409,12.8667635353633,
130.99260106119)) ;
#150189 = CARTESIAN_POINT('Ctrl Pts',(-17.8158506667333,13.1566082723263,
130.891398967559)) ;
#150190 = CARTESIAN_POINT('Ctrl Pts',(-17.7958948224345,13.4669634672463,
130.866262027044)) ;
#150191 = CARTESIAN_POINT('Ctrl Pts',(-17.8030608695675,13.7743605227785,
130.920372423503)) ;
#150192 = CARTESIAN_POINT('Ctrl Pts',(-17.8359001119113,14.0556835016132,
131.049381504432)) ;
#150193 = CARTESIAN_POINT('Ctrl Pts',(-17.8914209618374,14.2923698001693,
131.244711234281)) ;
#150194 = CARTESIAN_POINT('Ctrl Pts',(-17.9652475904261,14.4669397818909,
131.493630765107)) ;
#150195 = CARTESIAN_POINT('Ctrl Pts',(-18.050276614613,14.5658236939165,131.77497266956)) ;
#150196 = CARTESIAN_POINT('Ctrl Pts',(-18.1412026892029,14.5834030857371,
132.073851921233)) ;
#150197 = CARTESIAN_POINT('Ctrl Pts',(-18.2292576150982,14.5182209911816,
132.364039623745)) ;
#150198 = CARTESIAN_POINT('Ctrl Pts',(-18.309103978395,14.3732473260144,132.630645865943)) ;
#150199 = CARTESIAN_POINT('Ctrl Pts',(-18.3725034947101,14.1617341890797,
132.848838139851)) ;
#150200 = CARTESIAN_POINT('Ctrl Pts',(-18.4154172019829,13.8968740490593,
133.007322174194)) ;
#150201 = CARTESIAN_POINT('Ctrl Pts',(-18.4336530523727,13.5970562228853,
133.093807465727)) ;
#150202 = CARTESIAN_POINT('Ctrl Pts',(-18.4250129097242,13.2853499830191,
133.101720033997)) ;
#150203 = CARTESIAN_POINT('Ctrl Pts',(-18.3899205655734,12.9854215224893,
133.032137337284)) ;
#150204 = CARTESIAN_POINT('Ctrl Pts',(-18.3295227235463,12.7145027585382,
132.888898701989)) ;
#150205 = CARTESIAN_POINT('Ctrl Pts',(-18.2479735328657,12.4953423449653,
132.683727463283)) ;
#150206 = CARTESIAN_POINT('Ctrl Pts',(-18.1496105042201,12.3417858317011,
132.429625686426)) ;
#150207 = CARTESIAN_POINT('Ctrl Pts',(-18.0419827382182,12.2665368316973,
132.148216804111)) ;
#150208 = CARTESIAN_POINT('Ctrl Pts',(-17.9308988626219,12.2735361419267,
131.856860060952)) ;
#150209 = CARTESIAN_POINT('Ctrl Pts',(-17.8239987755081,12.363229877568,131.577738375418)) ;
#150210 = CARTESIAN_POINT('Ctrl Pts',(-17.7284277907829,12.5286846808382,
131.331660535556)) ;
#150211 = CARTESIAN_POINT('Ctrl Pts',(-17.650146576631,12.7579693374739,131.13607184284)) ;
#150212 = CARTESIAN_POINT('Ctrl Pts',(-17.5939037235543,13.0352201558529,
131.00490973182)) ;
#150213 = CARTESIAN_POINT('Ctrl Pts',(-17.5631487906681,13.3405827861553,
130.948233479656)) ;
#150214 = CARTESIAN_POINT('Ctrl Pts',(-17.5593786927079,13.6512270836361,
130.970318968351)) ;
#150215 = CARTESIAN_POINT('Ctrl Pts',(-17.5820478450478,13.9458586294117,
131.069672284471)) ;
#150216 = CARTESIAN_POINT('Ctrl Pts',(-17.6289872140888,14.2033946145398,
131.239982776778)) ;
#150217 = CARTESIAN_POINT('Ctrl Pts',(-17.6957349745663,14.4040390929878,
131.468022433177)) ;
#150218 = CARTESIAN_POINT('Ctrl Pts',(-17.7769298692206,14.5350227299355,
131.738273550231)) ;
#150219 = CARTESIAN_POINT('Ctrl Pts',(-17.8667505697732,14.5864958770583,
132.033957919984)) ;
#150220 = CARTESIAN_POINT('Ctrl Pts',(-17.9565884461338,14.5544169288515,
132.329387676471)) ;
#150221 = CARTESIAN_POINT('Ctrl Pts',(-18.0405609017563,14.4414134411267,
132.607855045807)) ;
#150222 = CARTESIAN_POINT('Ctrl Pts',(-18.1113732977568,14.2551029687745,
132.84787133366)) ;
#150223 = CARTESIAN_POINT('Ctrl Pts',(-18.16319522583,14.0100365363148,133.032311388359)) ;
#150224 = CARTESIAN_POINT('Ctrl Pts',(-18.191835749466,13.7214335689568,133.149211235179)) ;
#150225 = CARTESIAN_POINT('Ctrl Pts',(-18.1943014025765,13.4135493064467,
133.189407327766)) ;
#150226 = CARTESIAN_POINT('Ctrl Pts',(-18.1697502158279,13.1045553590735,
133.150886523563)) ;
#150227 = CARTESIAN_POINT('Ctrl Pts',(-18.1194362562685,12.8197359183053,
133.036936233067)) ;
#150228 = CARTESIAN_POINT('Ctrl Pts',(-18.045466735335,12.5762135336046,132.854155324105)) ;
#150229 = CARTESIAN_POINT('Ctrl Pts',(-17.9535452105021,12.3952020079458,
132.618664061262)) ;
#150230 = CARTESIAN_POINT('Ctrl Pts',(-17.8485836535312,12.2871509240411,
132.345226650551)) ;
#150231 = CARTESIAN_POINT('Ctrl Pts',(-17.7383571681942,12.260566124011,132.056214410167)) ;
#150232 = CARTESIAN_POINT('Ctrl Pts',(-17.6284396914457,12.3174695873532,
131.768413290461)) ;
#150233 = CARTESIAN_POINT('Ctrl Pts',(-17.5276588111919,12.453509519007,131.5070919687)) ;
#150234 = CARTESIAN_POINT('Ctrl Pts',(-17.441706070518,12.6588730452131,131.289115738783)) ;
#150235 = CARTESIAN_POINT('Ctrl Pts',(-17.376196852656,12.918573180631,131.13080952964)) ;
#150236 = CARTESIAN_POINT('Ctrl Pts',(-17.3348968149211,13.2144046243544,
131.043242092145)) ;
#150237 = CARTESIAN_POINT('Ctrl Pts',(-17.3200920505239,13.5255440796009,
131.033114858903)) ;
#150238 = CARTESIAN_POINT('Ctrl Pts',(-17.3321967590095,13.829753908523,131.101637331332)) ;
#150239 = CARTESIAN_POINT('Ctrl Pts',(-17.3697701983736,14.1049217078337,
131.244596755897)) ;
#150240 = CARTESIAN_POINT('Ctrl Pts',(-17.4288267699135,14.3298723137222,
131.450097233909)) ;
#150241 = CARTESIAN_POINT('Ctrl Pts',(-17.5053580167981,14.4915527560892,
131.706928465452)) ;
#150242 = CARTESIAN_POINT('Ctrl Pts',(-17.592352901495,14.5755974314799,131.994185295194)) ;
#150243 = CARTESIAN_POINT('Ctrl Pts',(-17.6827508417145,14.5774288452973,
132.291266219485)) ;
#150244 = CARTESIAN_POINT('Ctrl Pts',(-17.7700634635431,14.4968431861705,
132.579456392972)) ;
#150245 = CARTESIAN_POINT('Ctrl Pts',(-17.8471469337488,14.338559634622,132.837867370615)) ;
#150246 = CARTESIAN_POINT('Ctrl Pts',(-17.9072657239944,14.1152211662258,
133.046597266871)) ;
#150247 = CARTESIAN_POINT('Ctrl Pts',(-17.9457240149027,13.8419815633955,
133.192097761732)) ;
#150248 = CARTESIAN_POINT('Ctrl Pts',(-17.9589569606329,13.5398086158385,
133.263788376459)) ;
#150249 = CARTESIAN_POINT('Ctrl Pts',(-17.9453990657103,13.2280436814142,
133.257353253558)) ;
#150250 = CARTESIAN_POINT('Ctrl Pts',(-17.905043823452,12.9300591800615,133.172663322675)) ;
#150251 = CARTESIAN_POINT('Ctrl Pts',(-17.8403773368806,12.6684085006953,
133.016841323401)) ;
#150252 = CARTESIAN_POINT('Ctrl Pts',(-17.7553253291571,12.4608091979395,
132.801436870079)) ;
#150253 = CARTESIAN_POINT('Ctrl Pts',(-17.6548315660994,12.3214093724075,
132.541022558559)) ;
#150254 = CARTESIAN_POINT('Ctrl Pts',(-17.545287414388,12.2613303026755,132.25425908364)) ;
#150255 = CARTESIAN_POINT('Ctrl Pts',(-17.4352053399009,12.2843254889888,
131.965601011091)) ;
#150256 = CARTESIAN_POINT('Ctrl Pts',(-17.3299104259236,12.3887269550652,
131.691161540009)) ;
#150257 = CARTESIAN_POINT('Ctrl Pts',(-17.237062784242,12.5673627247375,131.453060235114)) ;
#150258 = CARTESIAN_POINT('Ctrl Pts',(-17.1624022535704,12.8080166646894,
131.268173285497)) ;
#150259 = CARTESIAN_POINT('Ctrl Pts',(-17.1109366121169,13.0914774239872,
131.150879601895)) ;
#150260 = CARTESIAN_POINT('Ctrl Pts',(-17.085215035143,13.4005589621793,131.109004255832)) ;
#150261 = CARTESIAN_POINT('Ctrl Pts',(-17.0865508110795,13.7083911586178,
131.14584909413)) ;
#150262 = CARTESIAN_POINT('Ctrl Pts',(-17.1141226769015,13.9985991401632,
131.259654047056)) ;
#150263 = CARTESIAN_POINT('Ctrl Pts',(-17.1650584656608,14.2457812582848,
131.441505397051)) ;
#150264 = CARTESIAN_POINT('Ctrl Pts',(-17.2350111236326,14.4345734163401,
131.678939485648)) ;
#150265 = CARTESIAN_POINT('Ctrl Pts',(-17.3185332049843,14.5511370874347,
131.956091770258)) ;
#150266 = CARTESIAN_POINT('Ctrl Pts',(-17.4083874998686,14.5867802184263,
132.251622731321)) ;
#150267 = CARTESIAN_POINT('Ctrl Pts',(-17.4980680409966,14.5391948509929,
132.546773593608)) ;
#150268 = CARTESIAN_POINT('Ctrl Pts',(-17.5799467374303,14.4115345503253,
132.819086492873)) ;
#150269 = CARTESIAN_POINT('Ctrl Pts',(-17.6475128932711,14.2134356096031,
133.049550301058)) ;
#150270 = CARTESIAN_POINT('Ctrl Pts',(-17.6953912867036,13.9582378109792,
133.22257409294)) ;
#150271 = CARTESIAN_POINT('Ctrl Pts',(-17.7192157998652,13.6646543280563,
133.32532295919)) ;
#150272 = CARTESIAN_POINT('Ctrl Pts',(-17.7166085475005,13.3541837462344,
133.350814052753)) ;
#150273 = CARTESIAN_POINT('Ctrl Pts',(-17.6870730407865,13.0484270052538,
133.297660731118)) ;
#150274 = CARTESIAN_POINT('Ctrl Pts',(-17.6318650358643,12.7694396720145,
133.169536797612)) ;
#150275 = CARTESIAN_POINT('Ctrl Pts',(-17.5547367408699,12.5380418317107,
132.977228775516)) ;
#150276 = CARTESIAN_POINT('Ctrl Pts',(-17.4590541050436,12.3683286468607,
132.73108001436)) ;
#150277 = CARTESIAN_POINT('Ctrl Pts',(-17.3531735443108,12.276042045724,132.454716010959)) ;
#150278 = CARTESIAN_POINT('Ctrl Pts',(-17.2421870088341,12.2649171865401,
132.163629145715)) ;
#150279 = CARTESIAN_POINT('Ctrl Pts',(-17.1339083209122,12.3368690244089,
131.8804310438)) ;
#150280 = CARTESIAN_POINT('Ctrl Pts',(-17.035054500192,12.4871141807711,131.624864749109)) ;
#150281 = CARTESIAN_POINT('Ctrl Pts',(-16.9525609483888,12.7041604883304,
131.41699806149)) ;
#150282 = CARTESIAN_POINT('Ctrl Pts',(-16.8913487827029,12.9721741232452,
131.271250432799)) ;
#150283 = CARTESIAN_POINT('Ctrl Pts',(-16.8549145668053,13.2726901834042,
131.197919141356)) ;
#150284 = CARTESIAN_POINT('Ctrl Pts',(-16.8452026953237,13.5844633646991,
131.202698812117)) ;
#150285 = CARTESIAN_POINT('Ctrl Pts',(-16.8624065683868,13.8852369971297,
131.286179901398)) ;
#150286 = CARTESIAN_POINT('Ctrl Pts',(-16.9041286488751,14.1508959663415,
131.441039820401)) ;
#150287 = CARTESIAN_POINT('Ctrl Pts',(-16.9670321127304,14.3659569774688,
131.657939494814)) ;
#150288 = CARTESIAN_POINT('Ctrl Pts',(-17.0460179767883,14.5133844128615,
131.92188643313)) ;
#150289 = CARTESIAN_POINT('Ctrl Pts',(-17.1339465963916,14.5822824831324,
132.21176107558)) ;
#150290 = CARTESIAN_POINT('Ctrl Pts',(-17.2247754522715,14.5684017849453,
132.510294823667)) ;
#150291 = CARTESIAN_POINT('Ctrl Pts',(-17.3104806432216,14.4726240674175,
132.793731139819)) ;
#150292 = CARTESIAN_POINT('Ctrl Pts',(-17.3848392552526,14.3009018680156,
133.044181149527)) ;
#150293 = CARTESIAN_POINT('Ctrl Pts',(-17.4410593342651,14.06766624957,133.241418037696)) ;
#150294 = CARTESIAN_POINT('Ctrl Pts',(-17.4751195477601,13.7867923876229,
133.374130221132)) ;
#150295 = CARTESIAN_POINT('Ctrl Pts',(-17.4833469392014,13.4808116155242,
133.431254688991)) ;
#150296 = CARTESIAN_POINT('Ctrl Pts',(-17.464747462014,13.170617767173,133.41002024296)) ;
#150297 = CARTESIAN_POINT('Ctrl Pts',(-17.4194321247648,12.8770484299103,
133.310921042257)) ;
#150298 = CARTESIAN_POINT('Ctrl Pts',(-17.3508127869087,12.6251910653491,
133.143425682724)) ;
#150299 = CARTESIAN_POINT('Ctrl Pts',(-17.2623582572588,12.4289584805404,
132.918141206375)) ;
#150300 = CARTESIAN_POINT('Ctrl Pts',(-17.159481434093,12.3038002389648,132.650826788061)) ;
#150301 = CARTESIAN_POINT('Ctrl Pts',(-17.049593615255,12.2593442697271,132.36290466408)) ;
#150302 = CARTESIAN_POINT('Ctrl Pts',(-16.9395766193849,12.297889877657,132.07456986564)) ;
#150303 = CARTESIAN_POINT('Ctrl Pts',(-16.8361631294826,12.4169444300621,
131.80560272998)) ;
#150304 = CARTESIAN_POINT('Ctrl Pts',(-16.7459877628339,12.6093773199724,
131.575465763003)) ;
#150305 = CARTESIAN_POINT('Ctrl Pts',(-16.6758357276199,12.858373409298,131.403541123782)) ;
#150306 = CARTESIAN_POINT('Ctrl Pts',(-16.6289825241189,13.1480449631144,
131.299749807383)) ;
#150307 = CARTESIAN_POINT('Ctrl Pts',(-16.6083146433778,13.4582417774946,
131.272537046797)) ;
#150308 = CARTESIAN_POINT('Ctrl Pts',(-16.6146793730458,13.7655078893865,
131.324248877105)) ;
#150309 = CARTESIAN_POINT('Ctrl Pts',(-16.6468582865308,14.0483169401814,
131.451381588369)) ;
#150310 = CARTESIAN_POINT('Ctrl Pts',(-16.7017047560325,14.2859989758831,
131.644677680424)) ;
#150311 = CARTESIAN_POINT('Ctrl Pts',(-16.7748115336735,14.4624790270523,
131.891400883999)) ;
#150312 = CARTESIAN_POINT('Ctrl Pts',(-16.8601571097669,14.5642183790962,
132.173890767713)) ;
#150313 = CARTESIAN_POINT('Ctrl Pts',(-16.9504675640042,14.5841609537885,
132.470754565741)) ;
#150314 = CARTESIAN_POINT('Ctrl Pts',(-17.0392368807652,14.5209707585958,
132.763245331408)) ;
#150315 = CARTESIAN_POINT('Ctrl Pts',(-17.1188682502455,14.3791779816594,
133.02897653721)) ;
#150316 = CARTESIAN_POINT('Ctrl Pts',(-17.1831683138652,14.1688152035408,
133.249950274552)) ;
#150317 = CARTESIAN_POINT('Ctrl Pts',(-17.2266852823441,13.905195794164,133.410184160549)) ;
#150318 = CARTESIAN_POINT('Ctrl Pts',(-17.2456647537425,13.6071501662918,
133.49873274648)) ;
#150319 = CARTESIAN_POINT('Ctrl Pts',(-17.2379795146638,13.2953844839231,
133.509443223532)) ;
#150320 = CARTESIAN_POINT('Ctrl Pts',(-17.2033907892679,12.9930170511922,
133.441539336307)) ;
#150321 = CARTESIAN_POINT('Ctrl Pts',(-17.1439345398936,12.7222274559466,
133.300891034768)) ;
#150322 = CARTESIAN_POINT('Ctrl Pts',(-17.0627161251801,12.5005441594065,
133.096795193658)) ;
#150323 = CARTESIAN_POINT('Ctrl Pts',(-16.9647728460759,12.3451353729422,
132.843896282304)) ;
#150324 = CARTESIAN_POINT('Ctrl Pts',(-16.8573151177925,12.2674914409628,
132.562993056805)) ;
#150325 = CARTESIAN_POINT('Ctrl Pts',(-16.745916203242,12.2722652498167,132.270803885411)) ;
#150326 = CARTESIAN_POINT('Ctrl Pts',(-16.6389119181345,12.3599738059354,
131.99135443123)) ;
#150327 = CARTESIAN_POINT('Ctrl Pts',(-16.5433418169087,12.5226377882888,
131.745135458993)) ;
#150328 = CARTESIAN_POINT('Ctrl Pts',(-16.4642169436847,12.7508221881861,
131.547177756897)) ;
#150329 = CARTESIAN_POINT('Ctrl Pts',(-16.4072037644663,13.0279564689842,
131.413863382206)) ;
#150330 = CARTESIAN_POINT('Ctrl Pts',(-16.375865594437,13.3323086828982,131.355420914037)) ;
#150331 = CARTESIAN_POINT('Ctrl Pts',(-16.3713312480991,13.6420773453948,
131.375166298422)) ;
#150332 = CARTESIAN_POINT('Ctrl Pts',(-16.393213710967,13.9374077798728,131.472211358002)) ;
#150333 = CARTESIAN_POINT('Ctrl Pts',(-16.4394591109491,14.1965319026708,
131.640502803954)) ;
#150334 = CARTESIAN_POINT('Ctrl Pts',(-16.506134908146,14.3999725565714,131.868522260138)) ;
#150335 = CARTESIAN_POINT('Ctrl Pts',(-16.5866083664928,14.5320840030957,
132.136487051069)) ;
#150336 = CARTESIAN_POINT('Ctrl Pts',(-16.6761358475962,14.5862914480512,
132.43126381356)) ;
#150337 = CARTESIAN_POINT('Ctrl Pts',(-16.766552339434,14.5562373226541,132.728571335906)) ;
#150338 = CARTESIAN_POINT('Ctrl Pts',(-16.850279782507,14.4460760144195,133.006119112852)) ;
#150339 = CARTESIAN_POINT('Ctrl Pts',(-16.9218856051312,14.2613118721967,
133.248574536486)) ;
#150340 = CARTESIAN_POINT('Ctrl Pts',(-16.9743127705121,14.0168342944474,
133.434863473203)) ;
#150341 = CARTESIAN_POINT('Ctrl Pts',(-17.003524928258,13.7314084897265,133.553180813754)) ;
#150342 = CARTESIAN_POINT('Ctrl Pts',(-17.0068016806013,13.421392773908,133.596014845283)) ;
#150343 = CARTESIAN_POINT('Ctrl Pts',(-16.9830906971717,13.1138964793829,
133.559748732295)) ;
#150344 = CARTESIAN_POINT('Ctrl Pts',(-16.9334554372867,12.8273574977414,
133.447863646689)) ;
#150345 = CARTESIAN_POINT('Ctrl Pts',(-16.8600151228304,12.5821904329902,
133.26664901627)) ;
#150346 = CARTESIAN_POINT('Ctrl Pts',(-16.7684365133115,12.3992406705926,
133.032190342738)) ;
#150347 = CARTESIAN_POINT('Ctrl Pts',(-16.6641078345942,12.289263542394,132.76048675717)) ;
#150348 = CARTESIAN_POINT('Ctrl Pts',(-16.553718708184,12.260188272694,132.47107268329)) ;
#150349 = CARTESIAN_POINT('Ctrl Pts',(-16.4440558695573,12.3144490228481,
132.183892674013)) ;
#150350 = CARTESIAN_POINT('Ctrl Pts',(-16.3428146204697,12.4481500069378,
131.921255741908)) ;
#150351 = CARTESIAN_POINT('Ctrl Pts',(-16.2562794181923,12.6515764939739,
131.701583750563)) ;
#150352 = CARTESIAN_POINT('Ctrl Pts',(-16.1897800646174,12.9112089841373,
131.540547278658)) ;
#150353 = CARTESIAN_POINT('Ctrl Pts',(-16.1478371964019,13.2069679929226,
131.451160112557)) ;
#150354 = CARTESIAN_POINT('Ctrl Pts',(-16.1323491810072,13.5165269909875,
131.438878337385)) ;
#150355 = CARTESIAN_POINT('Ctrl Pts',(-16.143795189693,13.8224960289794,131.505620155425)) ;
#150356 = CARTESIAN_POINT('Ctrl Pts',(-16.1805498235764,14.0973149318537,
131.646016489691)) ;
#150357 = CARTESIAN_POINT('Ctrl Pts',(-16.23913426865,14.3244517336708,131.850209657004)) ;
#150358 = CARTESIAN_POINT('Ctrl Pts',(-16.3151462424385,14.4877799140032,
132.105462744924)) ;
#150359 = CARTESIAN_POINT('Ctrl Pts',(-16.401805129707,14.5742904717488,132.391701051472)) ;
#150360 = CARTESIAN_POINT('Ctrl Pts',(-16.492585860518,14.5785355539825,132.690040136978)) ;
#150361 = CARTESIAN_POINT('Ctrl Pts',(-16.5799680048269,14.4999983626793,
132.978398341277)) ;
#150362 = CARTESIAN_POINT('Ctrl Pts',(-16.6571136565244,14.3447574910545,
133.236831164026)) ;
#150363 = CARTESIAN_POINT('Ctrl Pts',(-16.7180463250183,14.1223925047645,
133.448063876043)) ;
#150364 = CARTESIAN_POINT('Ctrl Pts',(-16.7571048654271,13.8510687474612,
133.595226610732)) ;
#150365 = CARTESIAN_POINT('Ctrl Pts',(-16.7711828604265,13.5484337104113,
133.66950419217)) ;
#150366 = CARTESIAN_POINT('Ctrl Pts',(-16.758359396265,13.237024252248,133.66516822926)) ;
#150367 = CARTESIAN_POINT('Ctrl Pts',(-16.7189312234401,12.9391312355254,
133.583092750207)) ;
#150368 = CARTESIAN_POINT('Ctrl Pts',(-16.6549202670634,12.6756661013292,
133.429230049725)) ;
#150369 = CARTESIAN_POINT('Ctrl Pts',(-16.5701642224514,12.465702834837,133.214777187573)) ;
#150370 = CARTESIAN_POINT('Ctrl Pts',(-16.4700761526249,12.3244745737951,
132.955522794711)) ;
#150371 = CARTESIAN_POINT('Ctrl Pts',(-16.3611846564961,12.261923279364,132.670519137022)) ;
#150372 = CARTESIAN_POINT('Ctrl Pts',(-16.2502670389918,12.2825882232678,
132.379655456716)) ;
#150373 = CARTESIAN_POINT('Ctrl Pts',(-16.1450742603988,12.3846500947886,
132.105406192287)) ;
#150374 = CARTESIAN_POINT('Ctrl Pts',(-16.0517868994275,12.5611186866008,
131.866013505962)) ;
#150375 = CARTESIAN_POINT('Ctrl Pts',(-15.9765085489102,12.8001288642586,
131.679313704519)) ;
#150376 = CARTESIAN_POINT('Ctrl Pts',(-15.9242993403601,13.0829558196603,
131.559890650521)) ;
#150377 = CARTESIAN_POINT('Ctrl Pts',(-15.8978264794063,13.3903655314665,
131.51568156666)) ;
#150378 = CARTESIAN_POINT('Ctrl Pts',(-15.8983687766488,13.7001366120665,
131.550391855689)) ;
#150379 = CARTESIAN_POINT('Ctrl Pts',(-15.9250955464469,13.9898881855453,
131.661569200131)) ;
#150380 = CARTESIAN_POINT('Ctrl Pts',(-15.9754500848428,14.2391934633215,
131.841798893272)) ;
#150381 = CARTESIAN_POINT('Ctrl Pts',(-16.0448273016722,14.4298567311308,
132.077514083438)) ;
#150382 = CARTESIAN_POINT('Ctrl Pts',(-16.1285516719131,14.549247146468,132.355452702111)) ;
#150383 = CARTESIAN_POINT('Ctrl Pts',(-16.2180137706109,14.5868020953667,
132.649720204288)) ;
#150384 = CARTESIAN_POINT('Ctrl Pts',(-16.3077295677544,14.5417975168182,
132.944943445594)) ;
#150385 = CARTESIAN_POINT('Ctrl Pts',(-16.3899638321532,14.4162088309709,
133.218316186842)) ;
#150386 = CARTESIAN_POINT('Ctrl Pts',(-16.4579840959181,14.2204083444341,
133.45005782146)) ;
#150387 = CARTESIAN_POINT('Ctrl Pts',(-16.5067331774277,13.9647701488693,
133.625846053146)) ;
#150388 = CARTESIAN_POINT('Ctrl Pts',(-16.5310706681232,13.6739289079279,
133.72986283775)) ;
#150389 = CARTESIAN_POINT('Ctrl Pts',(-16.5292510761197,13.3623285568061,
133.757801584865)) ;
#150390 = CARTESIAN_POINT('Ctrl Pts',(-16.500529680411,13.0574725166072,133.706883722544)) ;
#150391 = CARTESIAN_POINT('Ctrl Pts',(-16.4461335867092,12.7770677802999,
133.581145035692)) ;
#150392 = CARTESIAN_POINT('Ctrl Pts',(-16.3689064255398,12.5427865648713,
133.388787147722)) ;
#150393 = CARTESIAN_POINT('Ctrl Pts',(-16.274842442146,12.3731888767337,133.14694664983)) ;
#150394 = CARTESIAN_POINT('Ctrl Pts',(-16.1686014384922,12.2773794535172,
132.869740353412)) ;
#150395 = CARTESIAN_POINT('Ctrl Pts',(-16.0573374850372,12.2641879567031,
132.577928332093)) ;
#150396 = CARTESIAN_POINT('Ctrl Pts',(-15.9492700825767,12.3335960199066,
132.295231932845)) ;
#150397 = CARTESIAN_POINT('Ctrl Pts',(-15.850023314516,12.481561593043,132.038517373115)) ;
#150398 = CARTESIAN_POINT('Ctrl Pts',(-15.7669381618391,12.6968286383091,
131.82892749163)) ;
#150399 = CARTESIAN_POINT('Ctrl Pts',(-15.7049421360384,12.9642189214816,
131.680963788946)) ;
#150400 = CARTESIAN_POINT('Ctrl Pts',(-15.6677820428019,13.2637553890215,
131.605469326867)) ;
#150401 = CARTESIAN_POINT('Ctrl Pts',(-15.6573682454385,13.576692280422,131.608329578821)) ;
#150402 = CARTESIAN_POINT('Ctrl Pts',(-15.6736161246103,13.8753721133811,
131.688705955498)) ;
#150403 = CARTESIAN_POINT('Ctrl Pts',(-15.7149268964637,14.1446744627024,
131.842646209192)) ;
#150404 = CARTESIAN_POINT('Ctrl Pts',(-15.7772771295284,14.36064855191,132.057858656137)) ;
#150405 = CARTESIAN_POINT('Ctrl Pts',(-15.8555887750143,14.5100785493016,
132.319731780122)) ;
#150406 = CARTESIAN_POINT('Ctrl Pts',(-15.9440283856208,14.5815775750292,
132.611354939558)) ;
#150407 = CARTESIAN_POINT('Ctrl Pts',(-16.0342190695844,14.5700420013307,
132.907770831432)) ;
#150408 = CARTESIAN_POINT('Ctrl Pts',(-16.1205674523234,14.4761038026697,
133.193256248184)) ;
#150409 = CARTESIAN_POINT('Ctrl Pts',(-16.1949655569345,14.307434697937,133.443625750521)) ;
#150410 = CARTESIAN_POINT('Ctrl Pts',(-16.2522128289874,14.0735726732338,
133.644168593153)) ;
#150411 = CARTESIAN_POINT('Ctrl Pts',(-16.286567085948,13.7966475167134,133.777379895401)) ;
#150412 = CARTESIAN_POINT('Ctrl Pts',(-16.2957241267505,13.4894705902725,
133.83741554962)) ;
#150413 = CARTESIAN_POINT('Ctrl Pts',(-16.277915731801,13.1800818840159,133.818379729644)) ;
#150414 = CARTESIAN_POINT('Ctrl Pts',(-16.233382384928,12.8853356480997,133.721598421941)) ;
#150415 = CARTESIAN_POINT('Ctrl Pts',(-16.1653339151511,12.6318026190054,
133.555801564048)) ;
#150416 = CARTESIAN_POINT('Ctrl Pts',(-16.0773393373828,12.4337108597235,
133.331871256496)) ;
#150417 = CARTESIAN_POINT('Ctrl Pts',(-15.9749977446359,12.3064394733644,
133.066053638971)) ;
#150418 = CARTESIAN_POINT('Ctrl Pts',(-15.8649060852758,12.2594672530152,
132.777636639602)) ;
#150419 = CARTESIAN_POINT('Ctrl Pts',(-15.7549091018377,12.2954707768407,
132.489316203072)) ;
#150420 = CARTESIAN_POINT('Ctrl Pts',(-15.6506039958486,12.4135506766909,
132.21796505975)) ;
#150421 = CARTESIAN_POINT('Ctrl Pts',(-15.5611531746748,12.6014761735562,
131.989492941064)) ;
#150422 = CARTESIAN_POINT('Ctrl Pts',(-15.4896861055833,12.8505488639341,
131.813985346776)) ;
#150423 = CARTESIAN_POINT('Ctrl Pts',(-15.4422008192573,13.1393106596108,
131.708325362233)) ;
#150424 = CARTESIAN_POINT('Ctrl Pts',(-15.4207351710859,13.4495612540633,
131.678820753104)) ;
#150425 = CARTESIAN_POINT('Ctrl Pts',(-15.426337100979,13.7566530786408,131.728242130976)) ;
#150426 = CARTESIAN_POINT('Ctrl Pts',(-15.4577656885259,14.0404143241467,
131.853175929721)) ;
#150427 = CARTESIAN_POINT('Ctrl Pts',(-15.5119856948056,14.2798567692648,
132.044648848123)) ;
#150428 = CARTESIAN_POINT('Ctrl Pts',(-15.5850085796815,14.458860759646,132.291272848204)) ;
#150429 = CARTESIAN_POINT('Ctrl Pts',(-15.6696256144766,14.5622468001176,
132.57144381166)) ;
#150430 = CARTESIAN_POINT('Ctrl Pts',(-15.7602275007173,14.5847589339645,
132.869291645903)) ;
#150431 = CARTESIAN_POINT('Ctrl Pts',(-15.8488837215895,14.5239999698819,
133.161349516975)) ;
#150432 = CARTESIAN_POINT('Ctrl Pts',(-15.9289853890852,14.3842926564904,
133.428499684631)) ;
#150433 = CARTESIAN_POINT('Ctrl Pts',(-15.9937731842162,14.1758059968765,
133.650879354936)) ;
#150434 = CARTESIAN_POINT('Ctrl Pts',(-16.0380364943461,13.9130885413349,
133.813345394859)) ;
#150435 = CARTESIAN_POINT('Ctrl Pts',(-16.0576964829059,13.615158117942,133.903937919873)) ;
#150436 = CARTESIAN_POINT('Ctrl Pts',(-16.050810517652,13.3050555466183,133.916814091063)) ;
#150437 = CARTESIAN_POINT('Ctrl Pts',(-16.0170723190309,13.0018872896554,
133.85141230611)) ;
#150438 = CARTESIAN_POINT('Ctrl Pts',(-15.9581350119924,12.7291798994599,
133.71236767288)) ;
#150439 = CARTESIAN_POINT('Ctrl Pts',(-15.8775156954164,12.5061727549264,
133.50998953017)) ;
#150440 = CARTESIAN_POINT('Ctrl Pts',(-15.7803572447695,12.3489726739453,
133.259264679238)) ;
#150441 = CARTESIAN_POINT('Ctrl Pts',(-15.6726919794867,12.2685650260664,
132.977885098156)) ;
#150442 = CARTESIAN_POINT('Ctrl Pts',(-15.5617033607869,12.2709027283838,
132.686768675325)) ;
#150443 = CARTESIAN_POINT('Ctrl Pts',(-15.4544229833051,12.3558099877511,
132.406517587879)) ;
#150444 = CARTESIAN_POINT('Ctrl Pts',(-15.3579664336319,12.5172181290402,
132.157871619068)) ;
#150445 = CARTESIAN_POINT('Ctrl Pts',(-15.2785412794525,12.7432704544133,
131.958946428183)) ;
#150446 = CARTESIAN_POINT('Ctrl Pts',(-15.220940870672,13.0180146572784,131.823789499591)) ;
#150447 = CARTESIAN_POINT('Ctrl Pts',(-15.1886061274104,13.3228198676384,
131.762550075545)) ;
#150448 = CARTESIAN_POINT('Ctrl Pts',(-15.1832971970252,13.6334361388998,
131.780107071404)) ;
#150449 = CARTESIAN_POINT('Ctrl Pts',(-15.2044737072776,13.9294162640336,
131.875083706159)) ;
#150450 = CARTESIAN_POINT('Ctrl Pts',(-15.2499149788137,14.1891569843553,
132.040930237774)) ;
#150451 = CARTESIAN_POINT('Ctrl Pts',(-15.3159882637482,14.3946401780078,
132.267182223925)) ;
#150452 = CARTESIAN_POINT('Ctrl Pts',(-15.3964422708231,14.529556883976,132.535221020513)) ;
#150453 = CARTESIAN_POINT('Ctrl Pts',(-15.4859266051064,14.5858061305694,
132.829902483417)) ;
#150454 = CARTESIAN_POINT('Ctrl Pts',(-15.575921095585,14.5585141813688,133.125790617441)) ;
#150455 = CARTESIAN_POINT('Ctrl Pts',(-15.660393004627,14.4500372288901,133.405700992678)) ;
#150456 = CARTESIAN_POINT('Ctrl Pts',(-15.7320322458967,14.2682020295539,
133.648062095577)) ;
#150457 = CARTESIAN_POINT('Ctrl Pts',(-15.7853081761487,14.0250734212292,
133.836897476779)) ;
#150458 = CARTESIAN_POINT('Ctrl Pts',(-15.8153071073788,13.7389393527222,
133.957688978132)) ;
#150459 = CARTESIAN_POINT('Ctrl Pts',(-15.8192713850197,13.4311036991076,
134.002333051418)) ;
#150460 = CARTESIAN_POINT('Ctrl Pts',(-15.7964833343467,13.1229020252546,
133.968793735116)) ;
#150461 = CARTESIAN_POINT('Ctrl Pts',(-15.7470151225786,12.8333723826346,
133.857660705835)) ;
#150462 = CARTESIAN_POINT('Ctrl Pts',(-15.6749499819258,12.5895126808553,
133.680093919526)) ;
#150463 = CARTESIAN_POINT('Ctrl Pts',(-15.5835820228647,12.4035405044014,
133.44638124524)) ;
#150464 = CARTESIAN_POINT('Ctrl Pts',(-15.4795359363878,12.2914040543739,
133.175493546379)) ;
#150465 = CARTESIAN_POINT('Ctrl Pts',(-15.3691067042144,12.2598122660064,
132.885999507054)) ;
#150466 = CARTESIAN_POINT('Ctrl Pts',(-15.2592491515748,12.3118570092467,
132.598270697777)) ;
#150467 = CARTESIAN_POINT('Ctrl Pts',(-15.1578846173847,12.4430958477667,
132.335205909277)) ;
#150468 = CARTESIAN_POINT('Ctrl Pts',(-15.0707569923601,12.6447072106669,
132.113822737163)) ;
#150469 = CARTESIAN_POINT('Ctrl Pts',(-15.0036348239267,12.9030426443817,
131.950970459127)) ;
#150470 = CARTESIAN_POINT('Ctrl Pts',(-14.9609666584116,13.1970328357363,
131.859359722779)) ;
#150471 = CARTESIAN_POINT('Ctrl Pts',(-14.9446463507845,13.508431210418,131.844863395647)) ;
#150472 = CARTESIAN_POINT('Ctrl Pts',(-14.955182994799,13.8121186853756,131.908635532583)) ;
#150473 = CARTESIAN_POINT('Ctrl Pts',(-14.9913474493756,14.0900961116511,
132.047534065062)) ;
#150474 = CARTESIAN_POINT('Ctrl Pts',(-15.0493834153807,14.3187298480659,
132.250109058127)) ;
#150475 = CARTESIAN_POINT('Ctrl Pts',(-15.1252001144207,14.4844226501879,
132.504882601538)) ;
#150476 = CARTESIAN_POINT('Ctrl Pts',(-15.2112957458124,14.5727758610145,
132.789337009017)) ;
#150477 = CARTESIAN_POINT('Ctrl Pts',(-15.3020656236423,14.5796460652876,
133.087650648783)) ;
#150478 = CARTESIAN_POINT('Ctrl Pts',(-15.3896841845459,14.5035866280562,
133.3767061857)) ;
#150479 = CARTESIAN_POINT('Ctrl Pts',(-15.4675294606947,14.3497064261521,
133.637322714956)) ;
#150480 = CARTESIAN_POINT('Ctrl Pts',(-15.5288442157173,14.1291331402223,
133.849621128442)) ;
#150481 = CARTESIAN_POINT('Ctrl Pts',(-15.5684922654212,13.8597728320795,
133.998415963195)) ;
#150482 = CARTESIAN_POINT('Ctrl Pts',(-15.58336190046,13.5574625507345,134.075038663256)) ;
#150483 = CARTESIAN_POINT('Ctrl Pts',(-15.5713632930057,13.2463367213565,
134.073073116115)) ;
#150484 = CARTESIAN_POINT('Ctrl Pts',(-15.5326175841816,12.9472974934633,
133.993046368162)) ;
#150485 = CARTESIAN_POINT('Ctrl Pts',(-15.4695006632167,12.6832079210241,
133.841696695539)) ;
#150486 = CARTESIAN_POINT('Ctrl Pts',(-15.38489066345,12.4704983369195,133.62782581185)) ;
#150487 = CARTESIAN_POINT('Ctrl Pts',(-15.2855041099453,12.3276823761117,
133.370498419458)) ;
#150488 = CARTESIAN_POINT('Ctrl Pts',(-15.1765599844448,12.2625925296001,
133.085412552406)) ;
#150489 = CARTESIAN_POINT('Ctrl Pts',(-15.0659710389737,12.2806191987991,
132.795391506155)) ;
#150490 = CARTESIAN_POINT('Ctrl Pts',(-14.959826977886,12.3809214254249,132.518577452134)) ;
#150491 = CARTESIAN_POINT('Ctrl Pts',(-14.8661523667106,12.5560400663307,
132.278075298556)) ;
#150492 = CARTESIAN_POINT('Ctrl Pts',(-14.7907697004394,12.7918900929914,
132.090851846458)) ;
#150493 = CARTESIAN_POINT('Ctrl Pts',(-14.7376403432757,13.0744209302394,
131.968838267981)) ;
#150494 = CARTESIAN_POINT('Ctrl Pts',(-14.7104300876091,13.3812416408414,
131.922450614359)) ;
#150495 = CARTESIAN_POINT('Ctrl Pts',(-14.7101971910909,13.6920796910028,
131.954983498533)) ;
#150496 = CARTESIAN_POINT('Ctrl Pts',(-14.7363062855789,13.9824941646698,
132.064351689695)) ;
#150497 = CARTESIAN_POINT('Ctrl Pts',(-14.7857702497481,14.2323227439513,
132.24183650497)) ;
#150498 = CARTESIAN_POINT('Ctrl Pts',(-14.8551154475838,14.4258243504284,
132.477660321935)) ;
#150499 = CARTESIAN_POINT('Ctrl Pts',(-14.937793900891,14.5465247241855,132.752243575491)) ;
#150500 = CARTESIAN_POINT('Ctrl Pts',(-15.0279945492941,14.5869806831231,
133.048986776495)) ;
#150501 = CARTESIAN_POINT('Ctrl Pts',(-15.1173109934759,14.5442058467449,
133.342856019278)) ;
#150502 = CARTESIAN_POINT('Ctrl Pts',(-15.2000430741247,14.4209679616749,
133.617739309619)) ;
#150503 = CARTESIAN_POINT('Ctrl Pts',(-15.2687315291286,14.2257906653135,
133.851574766913)) ;
#150504 = CARTESIAN_POINT('Ctrl Pts',(-15.3176437052182,13.9741287874761,
134.027505853864)) ;
#150505 = CARTESIAN_POINT('Ctrl Pts',(-15.3429679172076,13.6829512743861,
134.134561979873)) ;
#150506 = CARTESIAN_POINT('Ctrl Pts',(-15.3419099139476,13.3714665722058,
134.164728515353)) ;
#150507 = CARTESIAN_POINT('Ctrl Pts',(-15.3138886729906,13.0656059038766,
134.115919871799)) ;
#150508 = CARTESIAN_POINT('Ctrl Pts',(-15.2603010980268,12.7850335054103,
133.992449867698)) ;
#150509 = CARTESIAN_POINT('Ctrl Pts',(-15.1840570554085,12.54966734435,133.802845091161)) ;
#150510 = CARTESIAN_POINT('Ctrl Pts',(-15.0897673247278,12.3766688899815,
133.560585713602)) ;
#150511 = CARTESIAN_POINT('Ctrl Pts',(-14.9837573750352,12.2789529397111,
133.284042602105)) ;
#150512 = CARTESIAN_POINT('Ctrl Pts',(-14.8727227918643,12.2634413447035,
132.992846291171)) ;
#150513 = CARTESIAN_POINT('Ctrl Pts',(-14.7644615600363,12.3304156583785,
132.709585444456)) ;
#150514 = CARTESIAN_POINT('Ctrl Pts',(-14.6645328719311,12.477034323666,132.450999584505)) ;
#150515 = CARTESIAN_POINT('Ctrl Pts',(-14.5813805381505,12.6896429302191,
132.241046767438)) ;
#150516 = CARTESIAN_POINT('Ctrl Pts',(-14.5186828849514,12.9554490393123,
132.091011360375)) ;
#150517 = CARTESIAN_POINT('Ctrl Pts',(-14.4807212473634,13.2546654169279,
132.013213880204)) ;
#150518 = CARTESIAN_POINT('Ctrl Pts',(-14.4694798018736,13.5672373629207,
132.013615571884)) ;
#150519 = CARTESIAN_POINT('Ctrl Pts',(-14.4850511399121,13.867352650113,132.092113461199)) ;
#150520 = CARTESIAN_POINT('Ctrl Pts',(-14.5254309896077,14.1367234867938,
132.243171857793)) ;
#150521 = CARTESIAN_POINT('Ctrl Pts',(-14.5877190733466,14.3561275745404,
132.458465397783)) ;
#150522 = CARTESIAN_POINT('Ctrl Pts',(-14.665301266002,14.5065131149989,132.718028260505)) ;
#150523 = CARTESIAN_POINT('Ctrl Pts',(-14.7533173483588,14.5806176797064,
133.008340016427)) ;
#150524 = CARTESIAN_POINT('Ctrl Pts',(-14.8438421700134,14.5715967155624,
133.305843094671)) ;
#150525 = CARTESIAN_POINT('Ctrl Pts',(-14.9304491532105,14.4799161202559,
133.592090673458)) ;
#150526 = CARTESIAN_POINT('Ctrl Pts',(-15.0052826955154,14.3130126833991,
133.843758445213)) ;
#150527 = CARTESIAN_POINT('Ctrl Pts',(-15.0628752850329,14.0821692542283,
134.045132020763)) ;
#150528 = CARTESIAN_POINT('Ctrl Pts',(-15.0982104834664,13.8046646113754,
134.181420036656)) ;
#150529 = CARTESIAN_POINT('Ctrl Pts',(-15.1080300159495,13.4979411637468,
134.243381047743)) ;
#150530 = CARTESIAN_POINT('Ctrl Pts',(-15.0909992445679,13.1889484555023,
134.226561548948)) ;
#150531 = CARTESIAN_POINT('Ctrl Pts',(-15.0473604790679,12.8939178939325,
134.132324580271)) ;
#150532 = CARTESIAN_POINT('Ctrl Pts',(-14.9796563895563,12.6378239616322,
133.967682652965)) ;
#150533 = CARTESIAN_POINT('Ctrl Pts',(-14.8921232379636,12.4382802323548,
133.745083826517)) ;
#150534 = CARTESIAN_POINT('Ctrl Pts',(-14.7905512472213,12.3092349725469,
133.481375904344)) ;
#150535 = CARTESIAN_POINT('Ctrl Pts',(-14.6802035483952,12.2595575244022,
133.192325666085)) ;
#150536 = CARTESIAN_POINT('Ctrl Pts',(-14.5703130707885,12.2934341290355,
132.904265169207)) ;
#150537 = CARTESIAN_POINT('Ctrl Pts',(-14.4662452413034,12.4080333821748,
132.63341243339)) ;
#150538 = CARTESIAN_POINT('Ctrl Pts',(-14.3752794576045,12.5960960444092,
132.400890382292)) ;
#150539 = CARTESIAN_POINT('Ctrl Pts',(-14.3036377782328,12.8430835986194,
132.224736503118)) ;
#150540 = CARTESIAN_POINT('Ctrl Pts',(-14.2554826671856,13.1299282695534,
132.117020119139)) ;
#150541 = CARTESIAN_POINT('Ctrl Pts',(-14.2331496418005,13.4413370794651,
132.085134325359)) ;
#150542 = CARTESIAN_POINT('Ctrl Pts',(-14.2380431690014,13.7480777708716,
132.132410606473)) ;
#150543 = CARTESIAN_POINT('Ctrl Pts',(-14.2687349931395,14.0327532731281,
132.255184675896)) ;
#150544 = CARTESIAN_POINT('Ctrl Pts',(-14.3223115413622,14.2736050674125,
132.444755998041)) ;
#150545 = CARTESIAN_POINT('Ctrl Pts',(-14.3949353266048,14.4547314005176,
132.690239889969)) ;
#150546 = CARTESIAN_POINT('Ctrl Pts',(-14.4791730889678,14.560267557326,132.969257871009)) ;
#150547 = CARTESIAN_POINT('Ctrl Pts',(-14.5697810156274,14.5853381835963,
133.267148625969)) ;
#150548 = CARTESIAN_POINT('Ctrl Pts',(-14.6586815272113,14.5268296207526,
133.559956030392)) ;
#150549 = CARTESIAN_POINT('Ctrl Pts',(-14.7390790372614,14.3893358191871,
133.827950281821)) ;
#150550 = CARTESIAN_POINT('Ctrl Pts',(-14.8044047562451,14.1825587760216,
134.051913962829)) ;
#150551 = CARTESIAN_POINT('Ctrl Pts',(-14.8492884325481,13.9213689273391,
134.216162794773)) ;
#150552 = CARTESIAN_POINT('Ctrl Pts',(-14.8696886675527,13.624244891243,134.308912651173)) ;
#150553 = CARTESIAN_POINT('Ctrl Pts',(-14.8636799148611,13.3143405109537,
134.32433386635)) ;
#150554 = CARTESIAN_POINT('Ctrl Pts',(-14.8303143719492,13.0084391813705,
134.260274614731)) ;
#150555 = CARTESIAN_POINT('Ctrl Pts',(-14.7725318389689,12.7371910069822,
134.124294910933)) ;
#150556 = CARTESIAN_POINT('Ctrl Pts',(-14.6922271432579,12.5114338941523,
133.92297148257)) ;
#150557 = CARTESIAN_POINT('Ctrl Pts',(-14.5954862728848,12.3524150089363,
133.673442871905)) ;
#150558 = CARTESIAN_POINT('Ctrl Pts',(-14.4878943565415,12.2696328223672,
133.392318829169)) ;
#150559 = CARTESIAN_POINT('Ctrl Pts',(-14.3769613848032,12.2697667116298,
133.101346904939)) ;
#150560 = CARTESIAN_POINT('Ctrl Pts',(-14.2696468649251,12.3522196481958,
132.820942570017)) ;
#150561 = CARTESIAN_POINT('Ctrl Pts',(-14.1727339204591,12.5116176555494,
132.57098120525)) ;
#150562 = CARTESIAN_POINT('Ctrl Pts',(-14.0927105287885,12.7360826079941,
132.370319381871)) ;
#150563 = CARTESIAN_POINT('Ctrl Pts',(-14.0342994277323,13.0105745884039,
132.232891230406)) ;
#150564 = CARTESIAN_POINT('Ctrl Pts',(-14.0013588827428,13.3146277352433,
132.16985008646)) ;
#150565 = CARTESIAN_POINT('Ctrl Pts',(-13.9952825294897,13.6243830684314,
132.185062273086)) ;
#150566 = CARTESIAN_POINT('Ctrl Pts',(-14.0157755566262,13.9217977302755,
132.278122090516)) ;
#150567 = CARTESIAN_POINT('Ctrl Pts',(-14.0604892593674,14.182101761474,132.441757903395)) ;
#150568 = CARTESIAN_POINT('Ctrl Pts',(-14.1259274137499,14.38941229378,132.6661239332)) ;
#150569 = CARTESIAN_POINT('Ctrl Pts',(-14.2063159513169,14.5268848124279,
132.93408166804)) ;
#150570 = CARTESIAN_POINT('Ctrl Pts',(-14.2953666004889,14.5852561632452,
133.227386196288)) ;
#150571 = CARTESIAN_POINT('Ctrl Pts',(-14.385474115087,14.5605921487245,133.523620813497)) ;
#150572 = CARTESIAN_POINT('Ctrl Pts',(-14.4703177026304,14.4542388685168,
133.804658441133)) ;
#150573 = CARTESIAN_POINT('Ctrl Pts',(-14.5424565250029,14.2743936484204,
134.048484935615)) ;
#150574 = CARTESIAN_POINT('Ctrl Pts',(-14.5964352897309,14.0316377347413,
134.239502626191)) ;
#150575 = CARTESIAN_POINT('Ctrl Pts',(-14.6269461364899,13.748755621538,134.361523364928)) ;
#150576 = CARTESIAN_POINT('Ctrl Pts',(-14.6317385626997,13.4387761369995,
134.408862066181)) ;
#150577 = CARTESIAN_POINT('Ctrl Pts',(-14.6097163065701,13.1317846538023,
134.377396710751)) ;
#150578 = CARTESIAN_POINT('Ctrl Pts',(-14.5609664968543,12.8410201849047,
134.268397592025)) ;
#150579 = CARTESIAN_POINT('Ctrl Pts',(-14.4896923945512,12.5963885979045,
134.093052311552)) ;
#150580 = CARTESIAN_POINT('Ctrl Pts',(-14.3989961430771,12.4083250169264,
133.861260268425)) ;
#150581 = CARTESIAN_POINT('Ctrl Pts',(-14.2945354469835,12.2932606250205,
133.589381296788)) ;
#150582 = CARTESIAN_POINT('Ctrl Pts',(-14.1847109735173,12.2596773195356,
133.301492991178)) ;
#150583 = CARTESIAN_POINT('Ctrl Pts',(-14.0747870087407,12.3089369784701,
133.013549726303)) ;
#150584 = CARTESIAN_POINT('Ctrl Pts',(-13.9726728971743,12.4384178929668,
132.748422319335)) ;
#150585 = CARTESIAN_POINT('Ctrl Pts',(-13.8849973180957,12.6389284156292,
132.525500717228)) ;
#150586 = CARTESIAN_POINT('Ctrl Pts',(-13.8177319116897,12.8936368315776,
132.361950917148)) ;
#150587 = CARTESIAN_POINT('Ctrl Pts',(-13.7739215665659,13.189035253119,132.267264094376)) ;
#150588 = CARTESIAN_POINT('Ctrl Pts',(-13.7569639775647,13.4997523048697,
132.250839898931)) ;
#150589 = CARTESIAN_POINT('Ctrl Pts',(-13.7667722639485,13.80398082463,132.312499872932)) ;
#150590 = CARTESIAN_POINT('Ctrl Pts',(-13.802078194261,14.0820720991441,132.448762814885)) ;
#150591 = CARTESIAN_POINT('Ctrl Pts',(-13.8596807492491,14.3130040222785,
132.650167238859)) ;
#150592 = CARTESIAN_POINT('Ctrl Pts',(-13.9347033118994,14.4800544799105,
132.902461711407)) ;
#150593 = CARTESIAN_POINT('Ctrl Pts',(-14.0207960816125,14.5714591728311,
133.187010624179)) ;
#150594 = CARTESIAN_POINT('Ctrl Pts',(-14.1119985592697,14.5804983969621,
133.486750014196)) ;
#150595 = CARTESIAN_POINT('Ctrl Pts',(-14.1993670996661,14.5069052814483,
133.774917777498)) ;
#150596 = CARTESIAN_POINT('Ctrl Pts',(-14.2774944784524,14.3557030567126,
134.036297112957)) ;
#150597 = CARTESIAN_POINT('Ctrl Pts',(-14.3394840095035,14.1367620675431,
134.250604362259)) ;
#150598 = CARTESIAN_POINT('Ctrl Pts',(-14.3799392246789,13.868069475113,134.40182762202)) ;
#150599 = CARTESIAN_POINT('Ctrl Pts',(-14.3955136344173,13.5652243934133,
134.480626813103)) ;
#150600 = CARTESIAN_POINT('Ctrl Pts',(-14.3843153384494,13.2558697743365,
134.480807322357)) ;
#150601 = CARTESIAN_POINT('Ctrl Pts',(-14.3463859800688,12.9557647499979,
134.403199207339)) ;
#150602 = CARTESIAN_POINT('Ctrl Pts',(-14.2837682658718,12.6900042913403,
134.253371208713)) ;
#150603 = CARTESIAN_POINT('Ctrl Pts',(-14.2000145590644,12.4761056036643,
134.041887452853)) ;
#150604 = CARTESIAN_POINT('Ctrl Pts',(-14.1004715127018,12.3304586966932,
133.784276677697)) ;
#150605 = CARTESIAN_POINT('Ctrl Pts',(-13.9922126022772,12.2634381679405,
133.501028466864)) ;
#150606 = CARTESIAN_POINT('Ctrl Pts',(-13.8813369849944,12.2788783439155,
133.210244944469)) ;
#150607 = CARTESIAN_POINT('Ctrl Pts',(-13.775078356608,12.3768659519767,132.933057558503)) ;
#150608 = CARTESIAN_POINT('Ctrl Pts',(-13.6809728489137,12.5495629773897,
132.691269773362)) ;
#150609 = CARTESIAN_POINT('Ctrl Pts',(-13.6045565383643,12.7855771010426,
132.501248970332)) ;
#150610 = CARTESIAN_POINT('Ctrl Pts',(-13.551130995295,13.0654344689711,132.378161083515)) ;
#150611 = CARTESIAN_POINT('Ctrl Pts',(-13.5230559798106,13.3720088898766,
132.329274492978)) ;
#150612 = CARTESIAN_POINT('Ctrl Pts',(-13.5220367594244,13.6824356605847,
132.359442967812)) ;
#150613 = CARTESIAN_POINT('Ctrl Pts',(-13.5472597305976,13.9739144612511,
132.466219512344)) ;
#150614 = CARTESIAN_POINT('Ctrl Pts',(-13.5965669447147,14.2268633656514,
132.643505517909)) ;
#150615 = CARTESIAN_POINT('Ctrl Pts',(-13.6647515661538,14.4204385538483,
132.875611430777)) ;
#150616 = CARTESIAN_POINT('Ctrl Pts',(-13.7478512385664,14.5445800995036,
133.151733148704)) ;
#150617 = CARTESIAN_POINT('Ctrl Pts',(-13.837360442129,14.5868220519023,133.446227338674)) ;
#150618 = CARTESIAN_POINT('Ctrl Pts',(-13.9269497874624,14.5468039096368,
133.740953745142)) ;
#150619 = CARTESIAN_POINT('Ctrl Pts',(-14.010258873857,14.4251034045477,134.017640108798)) ;
#150620 = CARTESIAN_POINT('Ctrl Pts',(-14.0791078279441,14.2325286601305,
134.251805282762)) ;
#150621 = CARTESIAN_POINT('Ctrl Pts',(-14.1287834744318,13.9823226220566,
134.429987882651)) ;
#150622 = CARTESIAN_POINT('Ctrl Pts',(-14.1548696941534,13.6900857926319,
134.539472968083)) ;
#150623 = CARTESIAN_POINT('Ctrl Pts',(-14.154524247537,13.3811330388435,134.571470330088)) ;
#150624 = CARTESIAN_POINT('Ctrl Pts',(-14.1273161252456,13.0742212515847,
134.525104298596)) ;
#150625 = CARTESIAN_POINT('Ctrl Pts',(-14.0743300860021,12.7922256350364,
134.403436831635)) ;
#150626 = CARTESIAN_POINT('Ctrl Pts',(-13.9984404651805,12.5548594605115,
134.21494790383)) ;
#150627 = CARTESIAN_POINT('Ctrl Pts',(-13.9046425023917,12.3804086732527,
133.97408020415)) ;
#150628 = CARTESIAN_POINT('Ctrl Pts',(-13.7993773640674,12.2809059933595,
133.699560773721)) ;
#150629 = CARTESIAN_POINT('Ctrl Pts',(-13.6885089045968,12.2624888444475,
133.408811622449)) ;
#150630 = CARTESIAN_POINT('Ctrl Pts',(-13.5794505161669,12.3276776788202,
133.123422025871)) ;
#150631 = CARTESIAN_POINT('Ctrl Pts',(-13.4800072576751,12.4707928531316,
132.865962382066)) ;
#150632 = CARTESIAN_POINT('Ctrl Pts',(-13.3957567744659,12.6823313434113,
132.652978802577)) ;
#150633 = CARTESIAN_POINT('Ctrl Pts',(-13.3322501543121,12.9478030946643,
132.500677270835)) ;
#150634 = CARTESIAN_POINT('Ctrl Pts',(-13.29359415217,13.2466922642525,132.420882288356)) ;
#150635 = CARTESIAN_POINT('Ctrl Pts',(-13.2816622838855,13.5583771774669,
132.419178441367)) ;
#150636 = CARTESIAN_POINT('Ctrl Pts',(-13.2964274275055,13.8592555730131,
132.495328464001)) ;
#150637 = CARTESIAN_POINT('Ctrl Pts',(-13.3364443297289,14.130642447192,132.645467030027)) ;
#150638 = CARTESIAN_POINT('Ctrl Pts',(-13.397423996239,14.3493759206944,132.856549116759)) ;
#150639 = CARTESIAN_POINT('Ctrl Pts',(-13.4752202752693,14.5035317147663,
133.117028484369)) ;
#150640 = CARTESIAN_POINT('Ctrl Pts',(-13.5628805610133,14.5795844939409,
133.406219517999)) ;
#150641 = CARTESIAN_POINT('Ctrl Pts',(-13.6536045252838,14.5729335746648,
133.704378305314)) ;
#150642 = CARTESIAN_POINT('Ctrl Pts',(-13.7401299984418,14.4838965301244,
133.990264440643)) ;
#150643 = CARTESIAN_POINT('Ctrl Pts',(-13.8155852912765,14.3187458157033,
134.243832703353)) ;
#150644 = CARTESIAN_POINT('Ctrl Pts',(-13.8736731440813,14.089767661644,134.446610185744)) ;
#150645 = CARTESIAN_POINT('Ctrl Pts',(-13.9097250084666,13.8134083502436,
134.584993791328)) ;
#150646 = CARTESIAN_POINT('Ctrl Pts',(-13.9203543833699,13.507393703558,134.649296910112)) ;
#150647 = CARTESIAN_POINT('Ctrl Pts',(-13.9040592972145,13.1976577760434,
134.634692382924)) ;
#150648 = CARTESIAN_POINT('Ctrl Pts',(-13.8613296465157,12.9027230155048,
134.543003893407)) ;
#150649 = CARTESIAN_POINT('Ctrl Pts',(-13.794207561342,12.6448108807206,134.380117189179)) ;
#150650 = CARTESIAN_POINT('Ctrl Pts',(-13.7074007923663,12.4434495892378,
134.159577368362)) ;
#150651 = CARTESIAN_POINT('Ctrl Pts',(-13.6051896084249,12.3113759849424,
133.894308207864)) ;
#150652 = CARTESIAN_POINT('Ctrl Pts',(-13.4961596498729,12.2599503304548,
133.608739116444)) ;
#150653 = CARTESIAN_POINT('Ctrl Pts',(-13.38530707921,12.2913693198197,133.318136196378)) ;
#150654 = CARTESIAN_POINT('Ctrl Pts',(-13.2812750961412,12.4038516007803,
133.047296028386)) ;
#150655 = CARTESIAN_POINT('Ctrl Pts',(-13.1901071149032,12.589262648139,132.814084987751)) ;
#150656 = CARTESIAN_POINT('Ctrl Pts',(-13.1177680098582,12.834296673012,132.635864585431)) ;
#150657 = CARTESIAN_POINT('Ctrl Pts',(-13.0686062567482,13.122430570677,132.525456230108)) ;
#150658 = CARTESIAN_POINT('Ctrl Pts',(-13.0457037121026,13.4307504343076,
132.491602073184)) ;
#150659 = CARTESIAN_POINT('Ctrl Pts',(-13.0497041032677,13.7394115379672,
132.53643828218)) ;
#150660 = CARTESIAN_POINT('Ctrl Pts',(-13.0797168042505,14.0250582462743,
132.657224771886)) ;
#150661 = CARTESIAN_POINT('Ctrl Pts',(-13.1327979298348,14.267685746029,132.845402925329)) ;
#150662 = CARTESIAN_POINT('Ctrl Pts',(-13.2046359566746,14.4501343666904,
133.088446513753)) ;
#150663 = CARTESIAN_POINT('Ctrl Pts',(-13.2890293737238,14.5585281597601,
133.368092017486)) ;
#150664 = CARTESIAN_POINT('Ctrl Pts',(-13.3793248440442,14.5857500281756,
133.664973177061)) ;
#150665 = CARTESIAN_POINT('Ctrl Pts',(-13.4685173888611,14.5296138402308,
133.958689264273)) ;
#150666 = CARTESIAN_POINT('Ctrl Pts',(-13.5492449744867,14.3940563949584,
134.227654399362)) ;
#150667 = CARTESIAN_POINT('Ctrl Pts',(-13.6149101345716,14.1896706789709,
134.452519557024)) ;
#150668 = CARTESIAN_POINT('Ctrl Pts',(-13.6605349934702,13.9296796265153,
134.618962908852)) ;
#150669 = CARTESIAN_POINT('Ctrl Pts',(-13.6817176477053,13.632561455883,134.714074782053)) ;
#150670 = CARTESIAN_POINT('Ctrl Pts',(-13.6763653200233,13.3229080728124,
134.731401281699)) ;
#150671 = CARTESIAN_POINT('Ctrl Pts',(-13.6441156519113,13.0185267768755,
134.670365678224)) ;
#150672 = CARTESIAN_POINT('Ctrl Pts',(-13.5866122080201,12.7436674784671,
134.535483497722)) ;
#150673 = CARTESIAN_POINT('Ctrl Pts',(-13.5066983561414,12.516497959597,134.335317034424)) ;
#150674 = CARTESIAN_POINT('Ctrl Pts',(-13.4107184546331,12.3560840678509,
134.08788704279)) ;
#150675 = CARTESIAN_POINT('Ctrl Pts',(-13.3033206756955,12.2708854944156,
133.807337914075)) ;
#150676 = CARTESIAN_POINT('Ctrl Pts',(-13.1925318588269,12.2685611985324,
133.51674558693)) ;
#150677 = CARTESIAN_POINT('Ctrl Pts',(-13.0848159423213,12.3486009329829,
133.235220443721)) ;
#150678 = CARTESIAN_POINT('Ctrl Pts',(-12.9871465907751,12.5069430119851,
132.983196082065)) ;
#150679 = CARTESIAN_POINT('Ctrl Pts',(-12.9070956244391,12.7284058667927,
132.782242099243)) ;
#150680 = CARTESIAN_POINT('Ctrl Pts',(-12.8477873224849,13.0024844630991,
132.642296947381)) ;
#150681 = CARTESIAN_POINT('Ctrl Pts',(-12.8141762094062,13.3053155340302,
132.57721650409)) ;
#150682 = CARTESIAN_POINT('Ctrl Pts',(-12.8073152976066,13.6156286046676,
132.590193775333)) ;
#150683 = CARTESIAN_POINT('Ctrl Pts',(-12.8269279491894,13.9128849150777,
132.680569802002)) ;
#150684 = CARTESIAN_POINT('Ctrl Pts',(-12.8713684246668,14.1766184698676,
132.843682795941)) ;
#150685 = CARTESIAN_POINT('Ctrl Pts',(-12.9362504869269,14.3847398233907,
133.066334572889)) ;
#150686 = CARTESIAN_POINT('Ctrl Pts',(-13.0160033501416,14.523836080727,133.332321804548)) ;
#150687 = CARTESIAN_POINT('Ctrl Pts',(-13.1047838223045,14.5847742986496,
133.624794125344)) ;
#150688 = CARTESIAN_POINT('Ctrl Pts',(-13.1953163380789,14.5623309512569,
133.922410172408)) ;
#150689 = CARTESIAN_POINT('Ctrl Pts',(-13.2802958590821,14.4584178345544,
134.203783409206)) ;
#150690 = CARTESIAN_POINT('Ctrl Pts',(-13.3531293445272,14.2791868966926,
134.449815883522)) ;
#150691 = CARTESIAN_POINT('Ctrl Pts',(-13.4070402409324,14.0415187300811,
134.640161537634)) ;
#150692 = CARTESIAN_POINT('Ctrl Pts',(-13.4387033407001,13.7564325475948,
134.765949365673)) ;
#150693 = CARTESIAN_POINT('Ctrl Pts',(-13.4442407332801,13.4495648633329,
134.815151727329)) ;
#150694 = CARTESIAN_POINT('Ctrl Pts',(-13.4228103575776,13.139416785511,134.785739085568)) ;
#150695 = CARTESIAN_POINT('Ctrl Pts',(-13.3753386049812,12.8508801252525,
134.680098633708)) ;
#150696 = CARTESIAN_POINT('Ctrl Pts',(-13.3041873758787,12.6022770135179,
134.505413740681)) ;
#150697 = CARTESIAN_POINT('Ctrl Pts',(-13.21398842626,12.4127865766784,134.275031656731)) ;
#150698 = CARTESIAN_POINT('Ctrl Pts',(-13.1098628114342,12.2953916616204,
134.004125903995)) ;
#150699 = CARTESIAN_POINT('Ctrl Pts',(-12.9998843833805,12.2594835085984,
133.715856211852)) ;
#150700 = CARTESIAN_POINT('Ctrl Pts',(-12.890063684845,12.3065006883116,133.428152917967)) ;
#150701 = CARTESIAN_POINT('Ctrl Pts',(-12.7878923147766,12.4331949818184,
133.162761248478)) ;
#150702 = CARTESIAN_POINT('Ctrl Pts',(-12.6993847702854,12.6325250875222,
132.937531738056)) ;
#150703 = CARTESIAN_POINT('Ctrl Pts',(-12.6316222787159,12.8854153645511,
132.77246408779)) ;
#150704 = CARTESIAN_POINT('Ctrl Pts',(-12.5870341048101,13.1803566291491,
132.67554844166)) ;
#150705 = CARTESIAN_POINT('Ctrl Pts',(-12.5693200633778,13.4893560631302,
132.65674883301)) ;
#150706 = CARTESIAN_POINT('Ctrl Pts',(-12.5782837478994,13.7954469993451,
132.716086060484)) ;
#150707 = CARTESIAN_POINT('Ctrl Pts',(-12.6130490170968,14.0751704523599,
132.850844642907)) ;
#150708 = CARTESIAN_POINT('Ctrl Pts',(-12.6699292025348,14.3069079863902,
133.050042271564)) ;
#150709 = CARTESIAN_POINT('Ctrl Pts',(-12.7444274445508,14.4762412630358,
133.300783850622)) ;
#150710 = CARTESIAN_POINT('Ctrl Pts',(-12.8310022377509,14.5702449515651,
133.587003668086)) ;
#150711 = CARTESIAN_POINT('Ctrl Pts',(-12.9213296926271,14.5813885782014,
133.883870771373)) ;
#150712 = CARTESIAN_POINT('Ctrl Pts',(-13.0093623207136,14.5100797260329,
134.174156031041)) ;
#150713 = CARTESIAN_POINT('Ctrl Pts',(-13.0879614538735,14.3602445926638,
134.436979157099)) ;
#150714 = CARTESIAN_POINT('Ctrl Pts',(-13.1502927048958,14.1432533152037,
134.652217619341)) ;
#150715 = CARTESIAN_POINT('Ctrl Pts',(-13.1912501163863,13.8766591291424,
134.804796321906)) ;
#150716 = CARTESIAN_POINT('Ctrl Pts',(-13.2076514124531,13.5754713250829,
134.885908155711)) ;
#150717 = CARTESIAN_POINT('Ctrl Pts',(-13.1972577477252,13.2645670010663,
134.888600930151)) ;
#150718 = CARTESIAN_POINT('Ctrl Pts',(-13.1599327354177,12.9634278823174,
134.812807254142)) ;
#150719 = CARTESIAN_POINT('Ctrl Pts',(-13.0981398878319,12.6972349900806,
134.665294225835)) ;
#150720 = CARTESIAN_POINT('Ctrl Pts',(-13.0150465902604,12.481723120017,134.455705324013)) ;
#150721 = CARTESIAN_POINT('Ctrl Pts',(-12.9159624724356,12.3338052298827,
134.199416140809)) ;
#150722 = CARTESIAN_POINT('Ctrl Pts',(-12.8075320102091,12.2641456097446,
133.915772384435)) ;
#150723 = CARTESIAN_POINT('Ctrl Pts',(-12.6966987609025,12.277353556164,133.625090634121)) ;
#150724 = CARTESIAN_POINT('Ctrl Pts',(-12.5904476511584,12.3726334343567,
133.347841250545)) ;
#150725 = CARTESIAN_POINT('Ctrl Pts',(-12.4957672976613,12.5434757962,133.104422029015)) ;
#150726 = CARTESIAN_POINT('Ctrl Pts',(-12.4189551559165,12.7769497154647,
132.913132493819)) ;
#150727 = CARTESIAN_POINT('Ctrl Pts',(-12.3644955449637,13.0568799295701,
132.787172403634)) ;
#150728 = CARTESIAN_POINT('Ctrl Pts',(-12.3356835525213,13.3636449055978,
132.73619324156)) ;
#150729 = CARTESIAN_POINT('Ctrl Pts',(-12.3339186693949,13.6733774156544,
132.764089446736)) ;
#150730 = CARTESIAN_POINT('Ctrl Pts',(-12.3583243925336,13.965438068356,132.86844444326)) ;
#150731 = CARTESIAN_POINT('Ctrl Pts',(-12.4070227423529,14.2203012587836,
133.043999653821)) ;
#150732 = CARTESIAN_POINT('Ctrl Pts',(-12.4749034404365,14.4159470406951,
133.275286549984)) ;
#150733 = CARTESIAN_POINT('Ctrl Pts',(-12.5571654799498,14.5416943667992,
133.54875796597)) ;
#150734 = CARTESIAN_POINT('Ctrl Pts',(-12.6469182873543,14.5869018903293,
133.844101856402)) ;
#150735 = CARTESIAN_POINT('Ctrl Pts',(-12.7367367973124,14.5489491297832,
134.139548585729)) ;
#150736 = CARTESIAN_POINT('Ctrl Pts',(-12.8200676024084,14.4300240433963,
134.416180797309)) ;
#150737 = CARTESIAN_POINT('Ctrl Pts',(-12.8896854587349,14.2387296175427,
134.652716325118)) ;
#150738 = CARTESIAN_POINT('Ctrl Pts',(-12.9398689479383,13.9899469029636,
134.832358869625)) ;
#150739 = CARTESIAN_POINT('Ctrl Pts',(-12.9666061416785,13.7002922437487,
134.943563277021)) ;
#150740 = CARTESIAN_POINT('Ctrl Pts',(-12.9672119408705,13.3909003280038,
134.978416886849)) ;
#150741 = CARTESIAN_POINT('Ctrl Pts',(-12.9405858686605,13.0819914624154,
134.933923958189)) ;
#150742 = CARTESIAN_POINT('Ctrl Pts',(-12.8884188883953,12.8000707590593,
134.814533654396)) ;
#150743 = CARTESIAN_POINT('Ctrl Pts',(-12.8134045786365,12.5616135129792,
134.62851387434)) ;
#150744 = CARTESIAN_POINT('Ctrl Pts',(-12.719888608477,12.3844499171478,134.38854536565)) ;
#150745 = CARTESIAN_POINT('Ctrl Pts',(-12.6143404917224,12.2824628358376,
134.113358649894)) ;
#150746 = CARTESIAN_POINT('Ctrl Pts',(-12.5041008453743,12.2618989558539,
133.824270652504)) ;
#150747 = CARTESIAN_POINT('Ctrl Pts',(-12.3947436272254,12.3245801207235,
133.53804913358)) ;
#150748 = CARTESIAN_POINT('Ctrl Pts',(-12.2949373759615,12.4655889395947,
133.279529105452)) ;
#150749 = CARTESIAN_POINT('Ctrl Pts',(-12.2101743985447,12.6753257670411,
133.065046394778)) ;
#150750 = CARTESIAN_POINT('Ctrl Pts',(-12.1460605408991,12.9389694466535,
132.910911474602)) ;
#150751 = CARTESIAN_POINT('Ctrl Pts',(-12.1065857640139,13.2377440459955,
132.828793571842)) ;
#150752 = CARTESIAN_POINT('Ctrl Pts',(-12.0938230998767,13.5478076708615,
132.824490961141)) ;
#150753 = CARTESIAN_POINT('Ctrl Pts',(-12.1078810488391,13.8515134131997,
132.898821311669)) ;
#150754 = CARTESIAN_POINT('Ctrl Pts',(-12.1471350028197,14.1231096251736,
133.046614309383)) ;
#150755 = CARTESIAN_POINT('Ctrl Pts',(-12.20764101,14.3439545931311,133.256373038123)) ;
#150756 = CARTESIAN_POINT('Ctrl Pts',(-12.2848385159864,14.4998916589537,
133.515014296344)) ;
#150757 = CARTESIAN_POINT('Ctrl Pts',(-12.3725989192797,14.5786386310749,
133.804615404426)) ;
#150758 = CARTESIAN_POINT('Ctrl Pts',(-12.4632852821564,14.5742675213239,
134.102641221154)) ;
#150759 = CARTESIAN_POINT('Ctrl Pts',(-12.550091515244,14.4873447468798,134.389378773216)) ;
#150760 = CARTESIAN_POINT('Ctrl Pts',(-12.6257089828659,14.3247914484279,
134.643310986823)) ;
#150761 = CARTESIAN_POINT('Ctrl Pts',(-12.6845766874469,14.0970302958978,
134.848450091851)) ;
#150762 = CARTESIAN_POINT('Ctrl Pts',(-12.7213449167932,13.8204924579681,
134.989058109086)) ;
#150763 = CARTESIAN_POINT('Ctrl Pts',(-12.7326160006419,13.5164550314446,
135.055069728641)) ;
#150764 = CARTESIAN_POINT('Ctrl Pts',(-12.7170978355958,13.2060700526839,
135.042791920806)) ;
#150765 = CARTESIAN_POINT('Ctrl Pts',(-12.6750312631745,12.9102233152311,
134.953058802789)) ;
#150766 = CARTESIAN_POINT('Ctrl Pts',(-12.6083863873251,12.6507291998818,
134.791615396846)) ;
#150767 = CARTESIAN_POINT('Ctrl Pts',(-12.5223567020033,12.448558591514,134.573220681831)) ;
#150768 = CARTESIAN_POINT('Ctrl Pts',(-12.4210378931773,12.3145373927892,
134.310396455084)) ;
#150769 = CARTESIAN_POINT('Ctrl Pts',(-12.3115104666657,12.2601564003865,
134.023569123454)) ;
#150770 = CARTESIAN_POINT('Ctrl Pts',(-12.200619808401,12.2893926143671,133.732844409505)) ;
#150771 = CARTESIAN_POINT('Ctrl Pts',(-12.0963310670659,12.399436637318,133.461240632214)) ;
#150772 = CARTESIAN_POINT('Ctrl Pts',(-12.0043449575091,12.5839727968354,
133.225788965511)) ;
#150773 = CARTESIAN_POINT('Ctrl Pts',(-11.9318054869342,12.8264918557582,
133.046825298092)) ;
#150774 = CARTESIAN_POINT('Ctrl Pts',(-11.88180009377,13.1141229255637,132.934004998449)) ;
#150775 = CARTESIAN_POINT('Ctrl Pts',(-11.8660883176702,13.3194868174309,
132.910146711368)) ;
#150776 = CARTESIAN_POINT('Ctrl Pts',(-11.862675149115,13.4222383333956,132.91119671495)) ;
#150777 = CARTESIAN_POINT('Ctrl Pts',(-33.3489959095147,13.1551399285885,
127.871927411069)) ;
#150778 = CARTESIAN_POINT('Ctrl Pts',(-33.3482570091173,13.1489709609094,
127.870499856875)) ;
#150779 = CARTESIAN_POINT('Ctrl Pts',(-33.3362031847492,13.0505878441039,
127.846970056077)) ;
#150780 = CARTESIAN_POINT('Ctrl Pts',(-33.303456104594,12.8648900473044,127.774282508598)) ;
#150781 = CARTESIAN_POINT('Ctrl Pts',(-33.2347176391245,12.6378996894465,
127.606502631126)) ;
#150782 = CARTESIAN_POINT('Ctrl Pts',(-33.1484631699894,12.4661938442505,
127.38763758675)) ;
#150783 = CARTESIAN_POINT('Ctrl Pts',(-33.0496339239794,12.3629468779938,
127.132205946451)) ;
#150784 = CARTESIAN_POINT('Ctrl Pts',(-32.9461836982222,12.3360866578135,
126.862930995212)) ;
#150785 = CARTESIAN_POINT('Ctrl Pts',(-32.8428524780797,12.3868467815327,
126.594300512203)) ;
#150786 = CARTESIAN_POINT('Ctrl Pts',(-32.7476240151848,12.5118616193735,
126.34920621096)) ;
#150787 = CARTESIAN_POINT('Ctrl Pts',(-32.6660393235339,12.7022376314793,
126.14402042184)) ;
#150788 = CARTESIAN_POINT('Ctrl Pts',(-32.6034202579729,12.9442211340136,
125.994217779495)) ;
#150789 = CARTESIAN_POINT('Ctrl Pts',(-32.5634889320909,13.2203922331636,
125.91068247448)) ;
#150790 = CARTESIAN_POINT('Ctrl Pts',(-32.5482836171183,13.5109001041669,
125.899354456419)) ;
#150791 = CARTESIAN_POINT('Ctrl Pts',(-32.5583885908025,13.7967277450532,
125.962163306551)) ;
#150792 = CARTESIAN_POINT('Ctrl Pts',(-32.5919970185865,14.0531634695327,
126.093303648423)) ;
#150793 = CARTESIAN_POINT('Ctrl Pts',(-32.6462352627175,14.2659161102292,
126.2848763833)) ;
#150794 = CARTESIAN_POINT('Ctrl Pts',(-32.7164440425069,14.4182155312585,
126.52308858485)) ;
#150795 = CARTESIAN_POINT('Ctrl Pts',(-32.7970929244734,14.4993926065239,
126.791896512519)) ;
#150796 = CARTESIAN_POINT('Ctrl Pts',(-32.8812312900771,14.5030674016304,
127.070805593369)) ;
#150797 = CARTESIAN_POINT('Ctrl Pts',(-32.9621947752627,14.4296658181567,
127.340390412531)) ;
#150798 = CARTESIAN_POINT('Ctrl Pts',(-33.0336799536047,14.2842405620309,
127.582320067705)) ;
#150799 = CARTESIAN_POINT('Ctrl Pts',(-33.0898518257578,14.0768885755418,
127.779563482544)) ;
#150800 = CARTESIAN_POINT('Ctrl Pts',(-33.1258131095785,13.821937566696,127.917839903426)) ;
#150801 = CARTESIAN_POINT('Ctrl Pts',(-33.1381603359796,13.5404397832619,
127.986888146398)) ;
#150802 = CARTESIAN_POINT('Ctrl Pts',(-33.1255862370588,13.2491903771815,
127.98329800545)) ;
#150803 = CARTESIAN_POINT('Ctrl Pts',(-33.0878760919221,12.9699188880577,
127.906345203758)) ;
#150804 = CARTESIAN_POINT('Ctrl Pts',(-33.0275630545352,12.7245502986717,
127.763166970814)) ;
#150805 = CARTESIAN_POINT('Ctrl Pts',(-32.9475449968705,12.5279694687298,
127.562611942766)) ;
#150806 = CARTESIAN_POINT('Ctrl Pts',(-32.853484832887,12.3961377043517,127.320906369453)) ;
#150807 = CARTESIAN_POINT('Ctrl Pts',(-32.7506275244767,12.3376103677892,
127.053662058531)) ;
#150808 = CARTESIAN_POINT('Ctrl Pts',(-32.6467508382538,12.3569098529355,
126.783214181605)) ;
#150809 = CARTESIAN_POINT('Ctrl Pts',(-32.5472606088073,12.452769019898,126.525790390631)) ;
#150810 = CARTESIAN_POINT('Ctrl Pts',(-32.4595735399336,12.6179593573441,
126.30272348908)) ;
#150811 = CARTESIAN_POINT('Ctrl Pts',(-32.388745121808,12.8405880377693,126.12891456918)) ;
#150812 = CARTESIAN_POINT('Ctrl Pts',(-32.3390681420419,13.1065246421439,
126.017073858121)) ;
#150813 = CARTESIAN_POINT('Ctrl Pts',(-32.313898204756,13.3925179674891,125.976505647384)) ;
#150814 = CARTESIAN_POINT('Ctrl Pts',(-32.3136699242009,13.6819916651313,
126.008953177836)) ;
#150815 = CARTESIAN_POINT('Ctrl Pts',(-32.3381285657715,13.9537242418059,
126.113619428421)) ;
#150816 = CARTESIAN_POINT('Ctrl Pts',(-32.384536696511,14.1863734291659,126.28227784121)) ;
#150817 = CARTESIAN_POINT('Ctrl Pts',(-32.4487957222161,14.3643807985693,
126.503053049914)) ;
#150818 = CARTESIAN_POINT('Ctrl Pts',(-32.5258074280907,14.4754559850244,
126.761140801679)) ;
#150819 = CARTESIAN_POINT('Ctrl Pts',(-32.6094667487868,14.5110246739577,
127.038737149779)) ;
#150820 = CARTESIAN_POINT('Ctrl Pts',(-32.6924145513944,14.4687063588107,
127.314091355005)) ;
#150821 = CARTESIAN_POINT('Ctrl Pts',(-32.7687110106265,14.3514018815055,
127.570143149353)) ;
#150822 = CARTESIAN_POINT('Ctrl Pts',(-32.8317732094795,14.1671964752596,
127.787539429963)) ;
#150823 = CARTESIAN_POINT('Ctrl Pts',(-32.8762267217076,13.9308608041133,
127.950416591701)) ;
#150824 = CARTESIAN_POINT('Ctrl Pts',(-32.8985780094168,13.6570089999716,
128.048890973466)) ;
#150825 = CARTESIAN_POINT('Ctrl Pts',(-32.896157678737,13.3664659574419,128.074980037028)) ;
#150826 = CARTESIAN_POINT('Ctrl Pts',(-32.8685548522265,13.0805681472547,
128.027442701697)) ;
#150827 = CARTESIAN_POINT('Ctrl Pts',(-32.8170821736547,12.8190539470386,
127.91017574478)) ;
#150828 = CARTESIAN_POINT('Ctrl Pts',(-32.7441829163896,12.5999338423892,
127.73048258649)) ;
#150829 = CARTESIAN_POINT('Ctrl Pts',(-32.6555170250936,12.4413957528131,
127.504429482033)) ;
#150830 = CARTESIAN_POINT('Ctrl Pts',(-32.5554705400289,12.3520378265489,
127.245337069314)) ;
#150831 = CARTESIAN_POINT('Ctrl Pts',(-32.4511053019089,12.339734386482,126.973578302647)) ;
#150832 = CARTESIAN_POINT('Ctrl Pts',(-32.3490815539954,12.4049383167358,
126.708653969777)) ;
#150833 = CARTESIAN_POINT('Ctrl Pts',(-32.2559652828001,12.5429634979505,
126.469740198936)) ;
#150834 = CARTESIAN_POINT('Ctrl Pts',(-32.1775406776191,12.7443553986761,
126.273802702315)) ;
#150835 = CARTESIAN_POINT('Ctrl Pts',(-32.1189511785612,12.9943521537239,
126.135786155147)) ;
#150836 = CARTESIAN_POINT('Ctrl Pts',(-32.0836266547703,13.2741647768729,
126.065632995122)) ;
#150837 = CARTESIAN_POINT('Ctrl Pts',(-32.0731422430725,13.565720269456,126.068169777388)) ;
#150838 = CARTESIAN_POINT('Ctrl Pts',(-32.0878672761987,13.8474315556546,
126.144404645481)) ;
#150839 = CARTESIAN_POINT('Ctrl Pts',(-32.1256175280986,14.0971649669908,
126.287692127083)) ;
#150840 = CARTESIAN_POINT('Ctrl Pts',(-32.1834742057281,14.3002122843455,
126.489943063825)) ;
#150841 = CARTESIAN_POINT('Ctrl Pts',(-32.2561937622249,14.4394509674979,
126.73551422792)) ;
#150842 = CARTESIAN_POINT('Ctrl Pts',(-32.3374471159419,14.5058688200503,
127.005843081603)) ;
#150843 = CARTESIAN_POINT('Ctrl Pts',(-32.4217002826958,14.4952594831202,
127.285155611484)) ;
#150844 = CARTESIAN_POINT('Ctrl Pts',(-32.5017471426193,14.4071576912799,
127.552229665334)) ;
#150845 = CARTESIAN_POINT('Ctrl Pts',(-32.5706761898774,14.2488070341169,
127.786694114575)) ;
#150846 = CARTESIAN_POINT('Ctrl Pts',(-32.6230717724866,14.032332595662,127.972746797191)) ;
#150847 = CARTESIAN_POINT('Ctrl Pts',(-32.6548239115267,13.7715185673777,
128.098623777025)) ;
#150848 = CARTESIAN_POINT('Ctrl Pts',(-32.6626680714647,13.4849968555095,
128.154735100321)) ;
#150849 = CARTESIAN_POINT('Ctrl Pts',(-32.6450616243189,13.1936954317484,
128.136543946875)) ;
#150850 = CARTESIAN_POINT('Ctrl Pts',(-32.6032602463952,12.9217410981826,
128.047311789015)) ;
#150851 = CARTESIAN_POINT('Ctrl Pts',(-32.5386314820962,12.6826993167214,
127.891757560495)) ;
#150852 = CARTESIAN_POINT('Ctrl Pts',(-32.4554412889622,12.4976839220085,
127.681914464153)) ;
#150853 = CARTESIAN_POINT('Ctrl Pts',(-32.3596753952525,12.3794711428103,
127.435114332308)) ;
#150854 = CARTESIAN_POINT('Ctrl Pts',(-32.2558253838943,12.3351744196322,
127.165019558565)) ;
#150855 = CARTESIAN_POINT('Ctrl Pts',(-32.1520107530796,12.3695012763354,
126.894875973638)) ;
#150856 = CARTESIAN_POINT('Ctrl Pts',(-32.0548036090535,12.4786183736045,
126.643923371603)) ;
#150857 = CARTESIAN_POINT('Ctrl Pts',(-31.9697179472944,12.6556201701116,
126.428500311369)) ;
#150858 = CARTESIAN_POINT('Ctrl Pts',(-31.9024466959007,12.8885376957079,
126.26521267139)) ;
#150859 = CARTESIAN_POINT('Ctrl Pts',(-31.8574815700017,13.1578672277872,
126.166847085394)) ;
#150860 = CARTESIAN_POINT('Ctrl Pts',(-31.8367167778053,13.4488181058444,
126.139492583638)) ;
#150861 = CARTESIAN_POINT('Ctrl Pts',(-31.8414313820349,13.7357351250712,
126.186316118843)) ;
#150862 = CARTESIAN_POINT('Ctrl Pts',(-31.8700151821842,14.0000244154435,
126.30281009704)) ;
#150863 = CARTESIAN_POINT('Ctrl Pts',(-31.9203616130848,14.2248063693443,
126.483142763909)) ;
#150864 = CARTESIAN_POINT('Ctrl Pts',(-31.9873859775564,14.3907221531774,
126.711954484493)) ;
#150865 = CARTESIAN_POINT('Ctrl Pts',(-32.0662309963865,14.4880878052934,
126.975454295977)) ;
#150866 = CARTESIAN_POINT('Ctrl Pts',(-32.1500140049146,14.5090844515927,
127.253273584441)) ;
#150867 = CARTESIAN_POINT('Ctrl Pts',(-32.2328114906108,14.4517331277302,
127.528461364111)) ;
#150868 = CARTESIAN_POINT('Ctrl Pts',(-32.306599429151,14.3213873494252,127.777000865602)) ;
#150869 = CARTESIAN_POINT('Ctrl Pts',(-32.3665410586647,14.1266126254878,
127.985228303146)) ;
#150870 = CARTESIAN_POINT('Ctrl Pts',(-32.4072983071001,13.8801113803002,
128.137553257528)) ;
#150871 = CARTESIAN_POINT('Ctrl Pts',(-32.4248919159062,13.6025840232108,
128.221986639911)) ;
#150872 = CARTESIAN_POINT('Ctrl Pts',(-32.4177985341224,13.3122088978665,
128.234314532032)) ;
#150873 = CARTESIAN_POINT('Ctrl Pts',(-32.3854612722872,13.0284665595888,
128.173051822567)) ;
#150874 = CARTESIAN_POINT('Ctrl Pts',(-32.3297158719588,12.7739765033465,
128.043289524966)) ;
#150875 = CARTESIAN_POINT('Ctrl Pts',(-32.2536312710535,12.5655228915478,
127.854171141032)) ;
#150876 = CARTESIAN_POINT('Ctrl Pts',(-32.1621333883639,12.4188418488155,
127.619973715704)) ;
#150877 = CARTESIAN_POINT('Ctrl Pts',(-32.0610335191924,12.3438198182334,
127.357704488195)) ;
#150878 = CARTESIAN_POINT('Ctrl Pts',(-31.9562422849269,12.3461749880073,
127.084814084959)) ;
#150879 = CARTESIAN_POINT('Ctrl Pts',(-31.8555595514267,12.4256199459212,
126.823755799531)) ;
#150880 = CARTESIAN_POINT('Ctrl Pts',(-31.7646812381954,12.5766359900473,
126.591428395529)) ;
#150881 = CARTESIAN_POINT('Ctrl Pts',(-31.6897549709183,12.7882864475543,
126.405673808487)) ;
#150882 = CARTESIAN_POINT('Ctrl Pts',(-31.6353440859288,13.0452019382586,
126.279829886042)) ;
#150883 = CARTESIAN_POINT('Ctrl Pts',(-31.6045551307125,13.3293877258915,
126.223017390213)) ;
#150884 = CARTESIAN_POINT('Ctrl Pts',(-31.598929994185,13.6204035856812,126.239726726341)) ;
#150885 = CARTESIAN_POINT('Ctrl Pts',(-31.6181519561243,13.8971496153171,
126.329008321255)) ;
#150886 = CARTESIAN_POINT('Ctrl Pts',(-31.660032440097,14.1397539052331,126.4844492787)) ;
#150887 = CARTESIAN_POINT('Ctrl Pts',(-31.7210074180807,14.3313464702874,
126.695729086547)) ;
#150888 = CARTESIAN_POINT('Ctrl Pts',(-31.7956413070931,14.4574458616527,
126.94680082343)) ;
#150889 = CARTESIAN_POINT('Ctrl Pts',(-31.8782525153513,14.5099723944026,
127.221254124399)) ;
#150890 = CARTESIAN_POINT('Ctrl Pts',(-31.9622607746967,14.4843439695083,
127.499872427198)) ;
#150891 = CARTESIAN_POINT('Ctrl Pts',(-32.0404152099778,14.3827749410654,
127.761275810437)) ;
#150892 = CARTESIAN_POINT('Ctrl Pts',(-32.1067647607671,14.2124739950545,
127.988225629159)) ;
#150893 = CARTESIAN_POINT('Ctrl Pts',(-32.1557319181306,13.9855789386979,
128.164396849995)) ;
#150894 = CARTESIAN_POINT('Ctrl Pts',(-32.1830886305706,13.7185805864342,
128.27741749427)) ;
#150895 = CARTESIAN_POINT('Ctrl Pts',(-32.1861674536437,13.4303185636673,
128.319530923703)) ;
#150896 = CARTESIAN_POINT('Ctrl Pts',(-32.164067606359,13.1417758325219,128.288060327875)) ;
#150897 = CARTESIAN_POINT('Ctrl Pts',(-32.1174319130124,12.8725286043858,
128.185023246156)) ;
#150898 = CARTESIAN_POINT('Ctrl Pts',(-32.0491401802662,12.6435096258014,
128.018626363072)) ;
#150899 = CARTESIAN_POINT('Ctrl Pts',(-31.9632199754991,12.4701546223289,
127.800755651149)) ;
#150900 = CARTESIAN_POINT('Ctrl Pts',(-31.8651776863348,12.3650501876111,
127.547453264018)) ;
#150901 = CARTESIAN_POINT('Ctrl Pts',(-31.7609862185599,12.3357586674927,
127.276274914652)) ;
#150902 = CARTESIAN_POINT('Ctrl Pts',(-31.6580563102104,12.3843195509594,
127.008647533804)) ;
#150903 = CARTESIAN_POINT('Ctrl Pts',(-31.5623522569141,12.5073666683789,
126.762219617398)) ;
#150904 = CARTESIAN_POINT('Ctrl Pts',(-31.4804283317136,12.6958200369819,
126.55599240923)) ;
#150905 = CARTESIAN_POINT('Ctrl Pts',(-31.4171911262104,12.9363649293222,
126.404372140452)) ;
#150906 = CARTESIAN_POINT('Ctrl Pts',(-31.3765204454803,13.212046231595,126.318705695641)) ;
#150907 = CARTESIAN_POINT('Ctrl Pts',(-31.3605890149829,13.5022481067603,
126.305235943963)) ;
#150908 = CARTESIAN_POINT('Ctrl Pts',(-31.3699466511949,13.7884016128943,
126.365844507772)) ;
#150909 = CARTESIAN_POINT('Ctrl Pts',(-31.402839929772,14.045945075732,126.494887877481)) ;
#150910 = CARTESIAN_POINT('Ctrl Pts',(-31.456801839307,14.2610680704969,126.685797164984)) ;
#150911 = CARTESIAN_POINT('Ctrl Pts',(-31.5263791105061,14.4145624165552,
126.922033359285)) ;
#150912 = CARTESIAN_POINT('Ctrl Pts',(-31.6068029650713,14.4980852125695,
127.190187763467)) ;
#150913 = CARTESIAN_POINT('Ctrl Pts',(-31.6909497784616,14.5041312739862,
127.469125424148)) ;
#150914 = CARTESIAN_POINT('Ctrl Pts',(-31.7722616933248,14.4326962339747,
127.739802187408)) ;
#150915 = CARTESIAN_POINT('Ctrl Pts',(-31.8440399327869,14.289424830309,127.982545178335)) ;
#150916 = CARTESIAN_POINT('Ctrl Pts',(-31.9008586342929,14.0826507854277,
128.181809264848)) ;
#150917 = CARTESIAN_POINT('Ctrl Pts',(-31.9371644477761,13.8312291814697,
128.320780138694)) ;
#150918 = CARTESIAN_POINT('Ctrl Pts',(-31.9504192122518,13.5479805821752,
128.392761416066)) ;
#150919 = CARTESIAN_POINT('Ctrl Pts',(-31.9384428607775,13.2572981016289,
128.390846357411)) ;
#150920 = CARTESIAN_POINT('Ctrl Pts',(-31.9016603090654,12.9781391944844,
128.316499055668)) ;
#150921 = CARTESIAN_POINT('Ctrl Pts',(-31.8414344653115,12.7298471383749,
128.173831316095)) ;
#150922 = CARTESIAN_POINT('Ctrl Pts',(-31.7624693619783,12.5331718510569,
127.976098656417)) ;
#150923 = CARTESIAN_POINT('Ctrl Pts',(-31.6682896816273,12.3987050488903,
127.734214112554)) ;
#150924 = CARTESIAN_POINT('Ctrl Pts',(-31.5661584069127,12.3381977133859,
127.468894861423)) ;
#150925 = CARTESIAN_POINT('Ctrl Pts',(-31.4613121151811,12.3556285786372,
127.195919765139)) ;
#150926 = CARTESIAN_POINT('Ctrl Pts',(-31.3626542471411,12.448498640132,126.940567661376)) ;
#150927 = CARTESIAN_POINT('Ctrl Pts',(-31.2739963638957,12.6124651727369,
126.714860191145)) ;
#150928 = CARTESIAN_POINT('Ctrl Pts',(-31.2028733579617,12.8330193864531,
126.540078371683)) ;
#150929 = CARTESIAN_POINT('Ctrl Pts',(-31.1524099899045,13.0981216515098,
126.425973898796)) ;
#150930 = CARTESIAN_POINT('Ctrl Pts',(-31.1264884036244,13.3840423616995,
126.383240800023)) ;
#150931 = CARTESIAN_POINT('Ctrl Pts',(-31.1255526905879,13.6738043197191,
126.413632148392)) ;
#150932 = CARTESIAN_POINT('Ctrl Pts',(-31.1492407119047,13.9458856450603,
126.515980892251)) ;
#150933 = CARTESIAN_POINT('Ctrl Pts',(-31.1951906788803,14.1805609741337,
126.683399895541)) ;
#150934 = CARTESIAN_POINT('Ctrl Pts',(-31.2589322113538,14.3602096703021,
126.902625201214)) ;
#150935 = CARTESIAN_POINT('Ctrl Pts',(-31.336152907064,14.4737146563849,127.161521971997)) ;
#150936 = CARTESIAN_POINT('Ctrl Pts',(-31.4191607366893,14.510981736058,127.436983917868)) ;
#150937 = CARTESIAN_POINT('Ctrl Pts',(-31.5023202222332,14.4710234538019,
127.713002150618)) ;
#150938 = CARTESIAN_POINT('Ctrl Pts',(-31.5788150531214,14.3558611755068,
127.9695934644)) ;
#150939 = CARTESIAN_POINT('Ctrl Pts',(-31.6423459010436,14.1736059642118,
128.188348020273)) ;
#150940 = CARTESIAN_POINT('Ctrl Pts',(-31.6874883180192,13.9381264816024,
128.353301532308)) ;
#150941 = CARTESIAN_POINT('Ctrl Pts',(-31.7104598612239,13.665192099168,128.453567738071)) ;
#150942 = CARTESIAN_POINT('Ctrl Pts',(-31.7088598170554,13.3755914984187,
128.481967244671)) ;
#150943 = CARTESIAN_POINT('Ctrl Pts',(-31.6817723867748,13.0874857506397,
128.436147123456)) ;
#150944 = CARTESIAN_POINT('Ctrl Pts',(-31.6311222896079,12.8264337657975,
128.32111606456)) ;
#150945 = CARTESIAN_POINT('Ctrl Pts',(-31.5590254861687,12.6060974389448,
128.143694924089)) ;
#150946 = CARTESIAN_POINT('Ctrl Pts',(-31.4705496041744,12.4450313389733,
127.91828768914)) ;
#150947 = CARTESIAN_POINT('Ctrl Pts',(-31.3704536339561,12.3534666197661,
127.659136554107)) ;
#150948 = CARTESIAN_POINT('Ctrl Pts',(-31.2664260741019,12.3390029903486,
127.388267266672)) ;
#150949 = CARTESIAN_POINT('Ctrl Pts',(-31.1640074542676,12.4020392430349,
127.122262231831)) ;
#150950 = CARTESIAN_POINT('Ctrl Pts',(-31.0704546098695,12.5385711173323,
126.882123477286)) ;
#150951 = CARTESIAN_POINT('Ctrl Pts',(-30.9919375233747,12.737337324062,126.685748126109)) ;
#150952 = CARTESIAN_POINT('Ctrl Pts',(-30.9326059877163,12.9861206892308,
126.545580982005)) ;
#150953 = CARTESIAN_POINT('Ctrl Pts',(-30.8964828802307,13.2660910782566,
126.473182758033)) ;
#150954 = CARTESIAN_POINT('Ctrl Pts',(-30.8853353619794,13.5573227840952,
126.473749977841)) ;
#150955 = CARTESIAN_POINT('Ctrl Pts',(-30.8992181639316,13.8386952169897,
126.547405844888)) ;
#150956 = CARTESIAN_POINT('Ctrl Pts',(-30.9364490028324,14.0906007554108,
126.689305896974)) ;
#150957 = CARTESIAN_POINT('Ctrl Pts',(-30.993577379338,14.2945039762926,126.889303441531)) ;
#150958 = CARTESIAN_POINT('Ctrl Pts',(-31.0658785833472,14.4361574187858,
127.133657392973)) ;
#150959 = CARTESIAN_POINT('Ctrl Pts',(-31.1473678175875,14.5051117570611,
127.404837868273)) ;
#150960 = CARTESIAN_POINT('Ctrl Pts',(-31.2314101845586,14.496582620466,127.68344430737)) ;
#150961 = CARTESIAN_POINT('Ctrl Pts',(-31.3113999047549,14.4113394819302,
127.950224339128)) ;
#150962 = CARTESIAN_POINT('Ctrl Pts',(-31.3810275644355,14.2546479447355,
128.186843915728)) ;
#150963 = CARTESIAN_POINT('Ctrl Pts',(-31.434079388976,14.039143877786,128.374888028828)) ;
#150964 = CARTESIAN_POINT('Ctrl Pts',(-31.4664410188237,13.7793416572316,
128.502539340318)) ;
#150965 = CARTESIAN_POINT('Ctrl Pts',(-31.4749982660917,13.4941095874199,
128.560637934817)) ;
#150966 = CARTESIAN_POINT('Ctrl Pts',(-31.4582310109701,13.2026874966814,
128.544890911873)) ;
#150967 = CARTESIAN_POINT('Ctrl Pts',(-31.4169753439866,12.928833346161,128.457383735722)) ;
#150968 = CARTESIAN_POINT('Ctrl Pts',(-31.3527956487623,12.6885083712283,
128.303172142516)) ;
#150969 = CARTESIAN_POINT('Ctrl Pts',(-31.2705703901443,12.5026390795781,
128.0959611027)) ;
#150970 = CARTESIAN_POINT('Ctrl Pts',(-31.1745744230575,12.3816810236162,
127.848677279268)) ;
#150971 = CARTESIAN_POINT('Ctrl Pts',(-31.0714307037018,12.3354826595071,
127.580451601079)) ;
#150972 = CARTESIAN_POINT('Ctrl Pts',(-30.9672895160686,12.3671988660942,
127.309429336125)) ;
#150973 = CARTESIAN_POINT('Ctrl Pts',(-30.8693900237751,12.4748749581507,
127.056599017908)) ;
#150974 = CARTESIAN_POINT('Ctrl Pts',(-30.7841568236753,12.6498955190515,
126.840662152846)) ;
#150975 = CARTESIAN_POINT('Ctrl Pts',(-30.7165115975955,12.8801431332148,
126.67612667683)) ;
#150976 = CARTESIAN_POINT('Ctrl Pts',(-30.6705876552176,13.1504415297617,
126.575185235204)) ;
#150977 = CARTESIAN_POINT('Ctrl Pts',(-30.6492401911973,13.438739202615,126.545850310757)) ;
#150978 = CARTESIAN_POINT('Ctrl Pts',(-30.6531248486497,13.7280473502378,
126.590480521703)) ;
#150979 = CARTESIAN_POINT('Ctrl Pts',(-30.6811874381857,13.9932362064335,
126.705468605857)) ;
#150980 = CARTESIAN_POINT('Ctrl Pts',(-30.7307233901376,14.2186783745982,
126.88330032276)) ;
#150981 = CARTESIAN_POINT('Ctrl Pts',(-30.7976668939673,14.3872014330787,
127.112042032862)) ;
#150982 = CARTESIAN_POINT('Ctrl Pts',(-30.8759215226086,14.486216521528,127.373662762679)) ;
#150983 = CARTESIAN_POINT('Ctrl Pts',(-30.9599483085192,14.5095010567365,
127.652320679818)) ;
#150984 = CARTESIAN_POINT('Ctrl Pts',(-31.0423602583126,14.4548476689191,
127.926162766265)) ;
#150985 = CARTESIAN_POINT('Ctrl Pts',(-31.1170261636548,14.3259646517619,
128.177490633467)) ;
#150986 = CARTESIAN_POINT('Ctrl Pts',(-31.1774376241067,14.1320240566172,
128.38715540167)) ;
#150987 = CARTESIAN_POINT('Ctrl Pts',(-31.2184772814882,13.8890687487633,
128.540002184362)) ;
#150988 = CARTESIAN_POINT('Ctrl Pts',(-31.2369718788586,13.6109288487181,
128.62723857725)) ;
#150989 = CARTESIAN_POINT('Ctrl Pts',(-31.2305830637653,13.3205780973656,
128.64162358396)) ;
#150990 = CARTESIAN_POINT('Ctrl Pts',(-31.1988306507602,13.0356410236252,
128.582156307125)) ;
#150991 = CARTESIAN_POINT('Ctrl Pts',(-31.1439236012217,12.7811568557338,
128.454705635715)) ;
#150992 = CARTESIAN_POINT('Ctrl Pts',(-31.0684038299569,12.5709851276515,
128.267243241426)) ;
#150993 = CARTESIAN_POINT('Ctrl Pts',(-30.9772756205,12.4221766619671,128.03413250274)) ;
#150994 = CARTESIAN_POINT('Ctrl Pts',(-30.8759319496152,12.3447406812541,
127.771290965256)) ;
#150995 = CARTESIAN_POINT('Ctrl Pts',(-30.7712963261735,12.3451621602759,
127.498804673837)) ;
#150996 = CARTESIAN_POINT('Ctrl Pts',(-30.6706886680026,12.4221617733591,
127.237875690043)) ;
#150997 = CARTESIAN_POINT('Ctrl Pts',(-30.5793389036692,12.5713293574021,
127.00420358355)) ;
#150998 = CARTESIAN_POINT('Ctrl Pts',(-30.5039469378259,12.7811357471148,
126.817049360709)) ;
#150999 = CARTESIAN_POINT('Ctrl Pts',(-30.4488110435835,13.037385413305,126.689142569762)) ;
#151000 = CARTESIAN_POINT('Ctrl Pts',(-30.4173468141487,13.3202247802994,
126.630258735514)) ;
#151001 = CARTESIAN_POINT('Ctrl Pts',(-30.4109588954888,13.6126649497902,
126.644895127432)) ;
#151002 = CARTESIAN_POINT('Ctrl Pts',(-30.4294392941911,13.889109539137,126.731888107809)) ;
#151003 = CARTESIAN_POINT('Ctrl Pts',(-30.47077570761,14.1334576219234,126.885811226843)) ;
#151004 = CARTESIAN_POINT('Ctrl Pts',(-30.53102912446,14.3262010857029,127.094865661672)) ;
#151005 = CARTESIAN_POINT('Ctrl Pts',(-30.6058078949067,14.4552702241494,
127.346574791049)) ;
#151006 = CARTESIAN_POINT('Ctrl Pts',(-30.6883760016807,14.5094659873619,
127.620923977953)) ;
#151007 = CARTESIAN_POINT('Ctrl Pts',(-30.7718896570381,14.48627928254,127.897878479629)) ;
#151008 = CARTESIAN_POINT('Ctrl Pts',(-30.8505404170833,14.3867194330965,
128.16082928885)) ;
#151009 = CARTESIAN_POINT('Ctrl Pts',(-30.9172652518935,14.2183273389604,
128.388850744567)) ;
#151010 = CARTESIAN_POINT('Ctrl Pts',(-30.966927867041,13.9922441011096,128.567141543632)) ;
#151011 = CARTESIAN_POINT('Ctrl Pts',(-30.9948429554227,13.7260908863955,
128.681785518138)) ;
#151012 = CARTESIAN_POINT('Ctrl Pts',(-30.9986761317404,13.4392990683917,
128.725970798859)) ;
#151013 = CARTESIAN_POINT('Ctrl Pts',(-30.9771754995003,13.1491383926391,
128.696410048975)) ;
#151014 = CARTESIAN_POINT('Ctrl Pts',(-30.9313862314932,12.880138144259,128.595705294773)) ;
#151015 = CARTESIAN_POINT('Ctrl Pts',(-30.8633741700187,12.6488312040692,
128.430267551873)) ;
#151016 = CARTESIAN_POINT('Ctrl Pts',(-30.7783096718615,12.4746173052797,
128.214724190605)) ;
#151017 = CARTESIAN_POINT('Ctrl Pts',(-30.6802839201009,12.3669410581914,
127.961566303494)) ;
#151018 = CARTESIAN_POINT('Ctrl Pts',(-30.5761954681339,12.3355244467329,
127.690674965918)) ;
#151019 = CARTESIAN_POINT('Ctrl Pts',(-30.4731987242308,12.3818824637266,
127.42284013735)) ;
#151020 = CARTESIAN_POINT('Ctrl Pts',(-30.3773601675738,12.502442440452,127.175947943775)) ;
#151021 = CARTESIAN_POINT('Ctrl Pts',(-30.2945593439143,12.6900860359651,
126.967322197996)) ;
#151022 = CARTESIAN_POINT('Ctrl Pts',(-30.2309201264915,12.9290693621117,
126.814464075625)) ;
#151023 = CARTESIAN_POINT('Ctrl Pts',(-30.1896011311781,13.2033802627449,
126.726833819823)) ;
#151024 = CARTESIAN_POINT('Ctrl Pts',(-30.1729187517655,13.493885424346,126.711224329232)) ;
#151025 = CARTESIAN_POINT('Ctrl Pts',(-30.1814818466642,13.7798208359641,
126.769425110779)) ;
#151026 = CARTESIAN_POINT('Ctrl Pts',(-30.2139166442141,14.0398147256928,
126.897315524147)) ;
#151027 = CARTESIAN_POINT('Ctrl Pts',(-30.2672327260932,14.2555980954836,
127.086230738633)) ;
#151028 = CARTESIAN_POINT('Ctrl Pts',(-30.3364241626342,14.4112165057251,
127.321355815591)) ;
#151029 = CARTESIAN_POINT('Ctrl Pts',(-30.4169483545396,14.4969135755094,
127.589920286704)) ;
#151030 = CARTESIAN_POINT('Ctrl Pts',(-30.5006568417281,14.5049696810031,
127.867411820872)) ;
#151031 = CARTESIAN_POINT('Ctrl Pts',(-30.5821059141925,14.4360249735447,
128.13846691764)) ;
#151032 = CARTESIAN_POINT('Ctrl Pts',(-30.6543269887437,14.2945754362065,
128.382542123477)) ;
#151033 = CARTESIAN_POINT('Ctrl Pts',(-30.7116365732865,14.0897548858671,
128.583199406406)) ;
#151034 = CARTESIAN_POINT('Ctrl Pts',(-30.7486474004249,13.8387001375239,
128.724327683098)) ;
#151035 = CARTESIAN_POINT('Ctrl Pts',(-30.7626160375506,13.5574044598577,
128.79823198023)) ;
#151036 = CARTESIAN_POINT('Ctrl Pts',(-30.751280169492,13.2644130009093,128.798450590054)) ;
#151037 = CARTESIAN_POINT('Ctrl Pts',(-30.7152762753897,12.9862195730077,
128.726198614227)) ;
#151038 = CARTESIAN_POINT('Ctrl Pts',(-30.6559255495121,12.7371111819008,
128.586013158079)) ;
#151039 = CARTESIAN_POINT('Ctrl Pts',(-30.5772199975952,12.5380203242925,
128.389149798631)) ;
#151040 = CARTESIAN_POINT('Ctrl Pts',(-30.4833480932253,12.4015272632005,
128.148171071429)) ;
#151041 = CARTESIAN_POINT('Ctrl Pts',(-30.3812924082162,12.3389470103484,
127.883098879055)) ;
#151042 = CARTESIAN_POINT('Ctrl Pts',(-30.2769531606877,12.3537864997403,
127.611426962061)) ;
#151043 = CARTESIAN_POINT('Ctrl Pts',(-30.1774142848297,12.4449099176858,
127.353712328041)) ;
#151044 = CARTESIAN_POINT('Ctrl Pts',(-30.0884196313121,12.6072327563546,
127.127011108624)) ;
#151045 = CARTESIAN_POINT('Ctrl Pts',(-30.0168944583603,12.8259751420657,
126.950999128042)) ;
#151046 = CARTESIAN_POINT('Ctrl Pts',(-29.9658131020968,13.0894865209779,
126.835020394129)) ;
#151047 = CARTESIAN_POINT('Ctrl Pts',(-29.9390402950618,13.3763086244584,
126.789949510195)) ;
#151048 = CARTESIAN_POINT('Ctrl Pts',(-29.9374976893148,13.666102426872,126.818551688385)) ;
#151049 = CARTESIAN_POINT('Ctrl Pts',(-29.9603659689101,13.9378774393092,
126.918366530385)) ;
#151050 = CARTESIAN_POINT('Ctrl Pts',(-30.0058557147277,14.174793298913,127.084558461599)) ;
#151051 = CARTESIAN_POINT('Ctrl Pts',(-30.0690738202602,14.355667987911,127.302193672896)) ;
#151052 = CARTESIAN_POINT('Ctrl Pts',(-30.1455851444044,14.4711053294092,
127.558860146817)) ;
#151053 = CARTESIAN_POINT('Ctrl Pts',(-30.2290907276294,14.511170979715,127.836014853784)) ;
#151054 = CARTESIAN_POINT('Ctrl Pts',(-30.3124346958538,14.4729025341711,
128.112614820692)) ;
#151055 = CARTESIAN_POINT('Ctrl Pts',(-30.3888326028229,14.3605014183323,
128.368750566373)) ;
#151056 = CARTESIAN_POINT('Ctrl Pts',(-30.4531791538599,14.1789799497678,
128.590078616567)) ;
#151057 = CARTESIAN_POINT('Ctrl Pts',(-30.4986908853725,13.9453130755044,
128.756011357139)) ;
#151058 = CARTESIAN_POINT('Ctrl Pts',(-30.5223367702664,13.673613297581,128.858202384461)) ;
#151059 = CARTESIAN_POINT('Ctrl Pts',(-30.5214927257582,13.3843416477693,
128.888796839614)) ;
#151060 = CARTESIAN_POINT('Ctrl Pts',(-30.4951356796959,13.0956424787648,
128.845131685907)) ;
#151061 = CARTESIAN_POINT('Ctrl Pts',(-30.4451353943437,12.8335787485534,
128.73200501772)) ;
#151062 = CARTESIAN_POINT('Ctrl Pts',(-30.3735874311193,12.6116522531053,
128.556195762552)) ;
#151063 = CARTESIAN_POINT('Ctrl Pts',(-30.2853579635812,12.4486058050818,
128.33155990322)) ;
#151064 = CARTESIAN_POINT('Ctrl Pts',(-30.1858663129506,12.3551665981467,
128.074050595748)) ;
#151065 = CARTESIAN_POINT('Ctrl Pts',(-30.0815496988783,12.3383111368361,
127.802444396815)) ;
#151066 = CARTESIAN_POINT('Ctrl Pts',(-29.9791399961725,12.3991318667188,
127.536410522558)) ;
#151067 = CARTESIAN_POINT('Ctrl Pts',(-29.885250975789,12.5336133546432,127.2952913997)) ;
#151068 = CARTESIAN_POINT('Ctrl Pts',(-29.8062098846917,12.7304747525644,
127.097365942919)) ;
#151069 = CARTESIAN_POINT('Ctrl Pts',(-29.7459166115697,12.9801493565206,
126.954643707808)) ;
#151070 = CARTESIAN_POINT('Ctrl Pts',(-29.7094981424688,13.2569930870622,
126.881074054437)) ;
#151071 = CARTESIAN_POINT('Ctrl Pts',(-29.697485321225,13.5493201067258,126.879249155707)) ;
#151072 = CARTESIAN_POINT('Ctrl Pts',(-29.7107148915496,13.8310609228274,
126.950973130347)) ;
#151073 = CARTESIAN_POINT('Ctrl Pts',(-29.7473686079901,14.0843638099265,
127.091228525209)) ;
#151074 = CARTESIAN_POINT('Ctrl Pts',(-29.8039983073089,14.2896244491401,
127.289751241016)) ;
#151075 = CARTESIAN_POINT('Ctrl Pts',(-29.8758248177242,14.4330063116879,
127.5326649792)) ;
#151076 = CARTESIAN_POINT('Ctrl Pts',(-29.9571776043441,14.5042107415309,
127.803464708327)) ;
#151077 = CARTESIAN_POINT('Ctrl Pts',(-30.0412713276901,14.4979449999679,
128.082232149485)) ;
#151078 = CARTESIAN_POINT('Ctrl Pts',(-30.121694639328,14.4144601779744,128.350375838408)) ;
#151079 = CARTESIAN_POINT('Ctrl Pts',(-30.1915790917938,14.2595209902124,
128.587713560571)) ;
#151080 = CARTESIAN_POINT('Ctrl Pts',(-30.2450076010872,14.046214919979,128.776755103724)) ;
#151081 = CARTESIAN_POINT('Ctrl Pts',(-30.2780878046331,13.7868053449528,
128.906585374679)) ;
#151082 = CARTESIAN_POINT('Ctrl Pts',(-30.2872906950602,13.5027357390144,
128.966484763682)) ;
#151083 = CARTESIAN_POINT('Ctrl Pts',(-30.2713500951273,13.2114164567146,
128.953122045362)) ;
#151084 = CARTESIAN_POINT('Ctrl Pts',(-30.230627814723,12.9359342983456,128.86728322249)) ;
#151085 = CARTESIAN_POINT('Ctrl Pts',(-30.1672447422047,12.6951562018299,
128.715288751686)) ;
#151086 = CARTESIAN_POINT('Ctrl Pts',(-30.0854978465419,12.5073061272103,
128.509491429827)) ;
#151087 = CARTESIAN_POINT('Ctrl Pts',(-29.9896882822811,12.3841592686752,
128.262793679839)) ;
#151088 = CARTESIAN_POINT('Ctrl Pts',(-29.8866361087517,12.3356200239572,
127.994841190901)) ;
#151089 = CARTESIAN_POINT('Ctrl Pts',(-29.7820423738734,12.3655842279676,
127.722626897302)) ;
#151090 = CARTESIAN_POINT('Ctrl Pts',(-29.6846378874882,12.4702048591763,
127.470973299483)) ;
#151091 = CARTESIAN_POINT('Ctrl Pts',(-29.5982444318826,12.6448837976238,
127.251934053335)) ;
#151092 = CARTESIAN_POINT('Ctrl Pts',(-29.530484788473,12.872508423284,127.086857758343)) ;
#151093 = CARTESIAN_POINT('Ctrl Pts',(-29.4836133061575,13.1434988331289,
126.983345728084)) ;
#151094 = CARTESIAN_POINT('Ctrl Pts',(-29.4617927517553,13.4301737780494,
126.952467269919)) ;
#151095 = CARTESIAN_POINT('Ctrl Pts',(-29.4647728375027,13.7187795914099,
126.994328449619)) ;
#151096 = CARTESIAN_POINT('Ctrl Pts',(-29.4924039666026,13.9870154433738,
127.108324446431)) ;
#151097 = CARTESIAN_POINT('Ctrl Pts',(-29.5411722729436,14.2124398345738,
127.283727368873)) ;
#151098 = CARTESIAN_POINT('Ctrl Pts',(-29.6075895922723,14.3830654461858,
127.510923381855)) ;
#151099 = CARTESIAN_POINT('Ctrl Pts',(-29.6859780654117,14.4846609541733,
127.773091506423)) ;
#151100 = CARTESIAN_POINT('Ctrl Pts',(-29.7699711987632,14.5097913616969,
128.051659371141)) ;
#151101 = CARTESIAN_POINT('Ctrl Pts',(-29.8521599614632,14.4576093080194,
128.324704513275)) ;
#151102 = CARTESIAN_POINT('Ctrl Pts',(-29.9273378651692,14.3304831317374,
128.57761366537)) ;
#151103 = CARTESIAN_POINT('Ctrl Pts',(-29.9881011678196,14.1386183822934,
128.788232639006)) ;
#151104 = CARTESIAN_POINT('Ctrl Pts',(-30.0298088081978,13.8965846856625,
128.943079017119)) ;
#151105 = CARTESIAN_POINT('Ctrl Pts',(-30.048987740085,13.6198365630073,129.032230754272)) ;
#151106 = CARTESIAN_POINT('Ctrl Pts',(-30.0433213484704,13.3288844737818,
129.048809941996)) ;
#151107 = CARTESIAN_POINT('Ctrl Pts',(-30.0124680035273,13.0447399832046,
128.991813037362)) ;
#151108 = CARTESIAN_POINT('Ctrl Pts',(-29.958162147996,12.7881836368688,128.866220633411)) ;
#151109 = CARTESIAN_POINT('Ctrl Pts',(-29.8827371039613,12.5755910115287,
128.67919720058)) ;
#151110 = CARTESIAN_POINT('Ctrl Pts',(-29.7923817501949,12.4257574465567,
128.448186718166)) ;
#151111 = CARTESIAN_POINT('Ctrl Pts',(-29.6914548654442,12.3460112405744,
128.186501449005)) ;
#151112 = CARTESIAN_POINT('Ctrl Pts',(-29.5867020660159,12.3439532504127,
127.913710488866)) ;
#151113 = CARTESIAN_POINT('Ctrl Pts',(-29.485666657119,12.4188218900739,127.651602416161)) ;
#151114 = CARTESIAN_POINT('Ctrl Pts',(-29.3936759004092,12.5668341062151,
127.416175460721)) ;
#151115 = CARTESIAN_POINT('Ctrl Pts',(-29.3182301931701,12.7739565310488,
127.2286723812)) ;
#151116 = CARTESIAN_POINT('Ctrl Pts',(-29.2623086088496,13.0292275295923,
127.098504241357)) ;
#151117 = CARTESIAN_POINT('Ctrl Pts',(-29.2301243830033,13.3121167714202,
127.037580467898)) ;
#151118 = CARTESIAN_POINT('Ctrl Pts',(-29.2229734795966,13.6036711588795,
127.049873651472)) ;
#151119 = CARTESIAN_POINT('Ctrl Pts',(-29.2408639834952,13.8822010088686,
127.135317168003)) ;
#151120 = CARTESIAN_POINT('Ctrl Pts',(-29.2814175857852,14.126534024312,127.286789452504)) ;
#151121 = CARTESIAN_POINT('Ctrl Pts',(-29.341269933413,14.3215277156221,127.494747226261)) ;
#151122 = CARTESIAN_POINT('Ctrl Pts',(-29.4156496701704,14.4523872469144,
127.745252022521)) ;
#151123 = CARTESIAN_POINT('Ctrl Pts',(-29.4979993749135,14.509081269933,128.018936330148)) ;
#151124 = CARTESIAN_POINT('Ctrl Pts',(-29.5821194390776,14.4877530584647,
128.297884507417)) ;
#151125 = CARTESIAN_POINT('Ctrl Pts',(-29.6605015766084,14.3906972492053,
128.559841528178)) ;
#151126 = CARTESIAN_POINT('Ctrl Pts',(-29.7277325620602,14.2242127265294,
128.789368837068)) ;
#151127 = CARTESIAN_POINT('Ctrl Pts',(-29.7778622908604,14.0000453961231,
128.968956847515)) ;
#151128 = CARTESIAN_POINT('Ctrl Pts',(-29.8065930602879,13.7349941187306,
129.085980593616)) ;
#151129 = CARTESIAN_POINT('Ctrl Pts',(-29.8110647581583,13.4462938086935,
129.132290262238)) ;
#151130 = CARTESIAN_POINT('Ctrl Pts',(-29.7905149481192,13.1586524064852,
129.105179558969)) ;
#151131 = CARTESIAN_POINT('Ctrl Pts',(-29.7450251194424,12.8863235925418,
129.005657518442)) ;
#151132 = CARTESIAN_POINT('Ctrl Pts',(-29.6779688870286,12.6553854575325,
128.842782884932)) ;
#151133 = CARTESIAN_POINT('Ctrl Pts',(-29.5932822353585,12.4787538591612,
128.628403260321)) ;
#151134 = CARTESIAN_POINT('Ctrl Pts',(-29.4951432611704,12.3688114822916,
128.375032108495)) ;
#151135 = CARTESIAN_POINT('Ctrl Pts',(-29.3915755638739,12.3354319136936,
128.105522888968)) ;
#151136 = CARTESIAN_POINT('Ctrl Pts',(-29.2883737439491,12.3792576310417,
127.83711019449)) ;
#151137 = CARTESIAN_POINT('Ctrl Pts',(-29.1917010872287,12.4988398999205,
127.587984309591)) ;
#151138 = CARTESIAN_POINT('Ctrl Pts',(-29.1090972687786,12.6835118512005,
127.379683329034)) ;
#151139 = CARTESIAN_POINT('Ctrl Pts',(-29.0446608613966,12.9214923912795,
127.224563683631)) ;
#151140 = CARTESIAN_POINT('Ctrl Pts',(-29.0026163941945,13.1954916424955,
127.134859426664)) ;
#151141 = CARTESIAN_POINT('Ctrl Pts',(-28.985230945197,13.4865485670219,127.117276574287)) ;
#151142 = CARTESIAN_POINT('Ctrl Pts',(-28.9931808891691,13.772471589557,127.173641275195)) ;
#151143 = CARTESIAN_POINT('Ctrl Pts',(-29.0248180797672,14.0322259092952,
127.299049560001)) ;
#151144 = CARTESIAN_POINT('Ctrl Pts',(-29.0774225647813,14.2496185339524,
127.485847881482)) ;
#151145 = CARTESIAN_POINT('Ctrl Pts',(-29.1466584272716,14.4079186586772,
127.721302692546)) ;
#151146 = CARTESIAN_POINT('Ctrl Pts',(-29.2262609733389,14.495128940057,127.986882942297)) ;
#151147 = CARTESIAN_POINT('Ctrl Pts',(-29.310377688868,14.5060206783235,128.265744239721)) ;
#151148 = CARTESIAN_POINT('Ctrl Pts',(-29.3922415681972,14.4388851972431,
128.538108177024)) ;
#151149 = CARTESIAN_POINT('Ctrl Pts',(-29.4648367940965,14.2990479598781,
128.783307296558)) ;
#151150 = CARTESIAN_POINT('Ctrl Pts',(-29.5224591681686,14.096277092635,128.984789687897)) ;
#151151 = CARTESIAN_POINT('Ctrl Pts',(-29.5601633246064,13.8463552274942,
129.12795060112)) ;
#151152 = CARTESIAN_POINT('Ctrl Pts',(-29.5747316968106,13.5643762793268,
129.203747316631)) ;
#151153 = CARTESIAN_POINT('Ctrl Pts',(-29.5643172687888,13.2747380866486,
129.206268472805)) ;
#151154 = CARTESIAN_POINT('Ctrl Pts',(-29.5288291438255,12.9934296976024,
129.135814296567)) ;
#151155 = CARTESIAN_POINT('Ctrl Pts',(-29.470171863856,12.7438068041656,128.99757323151)) ;
#151156 = CARTESIAN_POINT('Ctrl Pts',(-29.391803285665,12.5426943442427,128.801768222048)) ;
#151157 = CARTESIAN_POINT('Ctrl Pts',(-29.2986131391391,12.4046936236787,
128.56265775762)) ;
#151158 = CARTESIAN_POINT('Ctrl Pts',(-29.1964773761958,12.3396331759052,
128.297435830634)) ;
#151159 = CARTESIAN_POINT('Ctrl Pts',(-29.092230590555,12.3522550875064,128.025991131613)) ;
#151160 = CARTESIAN_POINT('Ctrl Pts',(-28.9924608185787,12.441158614988,127.767604009206)) ;
#151161 = CARTESIAN_POINT('Ctrl Pts',(-28.9030933450802,12.6013769713038,
127.539790029494)) ;
#151162 = CARTESIAN_POINT('Ctrl Pts',(-28.8308886096015,12.819071640269,127.361858709555)) ;
#151163 = CARTESIAN_POINT('Ctrl Pts',(-28.779280341327,13.0807346140254,127.244233442709)) ;
#151164 = CARTESIAN_POINT('Ctrl Pts',(-28.7517055757331,13.3675408612144,
127.196874862189)) ;
#151165 = CARTESIAN_POINT('Ctrl Pts',(-28.7493257047856,13.6570979280699,
127.222968219409)) ;
#151166 = CARTESIAN_POINT('Ctrl Pts',(-28.7718142821641,13.9319893911641,
127.321979864566)) ;
#151167 = CARTESIAN_POINT('Ctrl Pts',(-28.8162456944187,14.1676085258846,
127.484711805867)) ;
#151168 = CARTESIAN_POINT('Ctrl Pts',(-28.8794392120634,14.3519029604138,
127.702543293248)) ;
#151169 = CARTESIAN_POINT('Ctrl Pts',(-28.955521536148,14.4687263868581,127.957864396171)) ;
#151170 = CARTESIAN_POINT('Ctrl Pts',(-29.0386446837284,14.5110206744739,
128.233803590714)) ;
#151171 = CARTESIAN_POINT('Ctrl Pts',(-29.1220480184099,14.4754839101951,
128.510547823415)) ;
#151172 = CARTESIAN_POINT('Ctrl Pts',(-29.1992609632459,14.3641243881349,
128.769313204063)) ;
#151173 = CARTESIAN_POINT('Ctrl Pts',(-29.2634796257756,14.1859981150162,
128.989963010774)) ;
#151174 = CARTESIAN_POINT('Ctrl Pts',(-29.309906743687,13.9527739629267,129.158738849017)) ;
#151175 = CARTESIAN_POINT('Ctrl Pts',(-29.3342115703911,13.6818171869407,
129.262851136394)) ;
#151176 = CARTESIAN_POINT('Ctrl Pts',(-29.3340473631818,13.3923456599437,
129.295485666288)) ;
#151177 = CARTESIAN_POINT('Ctrl Pts',(-29.3085669103323,13.1044625348289,
129.254236375475)) ;
#151178 = CARTESIAN_POINT('Ctrl Pts',(-29.258986211392,12.8400820200563,129.142508243958)) ;
#151179 = CARTESIAN_POINT('Ctrl Pts',(-29.1881542029012,12.6174283224968,
128.968693652698)) ;
#151180 = CARTESIAN_POINT('Ctrl Pts',(-29.1002100971169,12.4521814963559,
128.744946986999)) ;
#151181 = CARTESIAN_POINT('Ctrl Pts',(-29.0009103649547,12.3567835155047,
128.48800496993)) ;
#151182 = CARTESIAN_POINT('Ctrl Pts',(-28.896925987083,12.3377092271658,128.21727920025)) ;
#151183 = CARTESIAN_POINT('Ctrl Pts',(-28.7942667965697,12.3962076032604,
127.950545837014)) ;
#151184 = CARTESIAN_POINT('Ctrl Pts',(-28.6998220504126,12.5290432373042,
127.70787965737)) ;
#151185 = CARTESIAN_POINT('Ctrl Pts',(-28.6204061898145,12.7244085230837,
127.508847094626)) ;
#151186 = CARTESIAN_POINT('Ctrl Pts',(-28.559819094265,12.9709500550387,127.365030411237)) ;
#151187 = CARTESIAN_POINT('Ctrl Pts',(-28.5223002592329,13.2494402817627,
127.288528530129)) ;
#151188 = CARTESIAN_POINT('Ctrl Pts',(-28.5097189788881,13.5418967084717,
127.285058220228)) ;
#151189 = CARTESIAN_POINT('Ctrl Pts',(-28.5222097719137,13.8230883914708,
127.354499660829)) ;
#151190 = CARTESIAN_POINT('Ctrl Pts',(-28.5582144837367,14.0775910910953,
127.492866930045)) ;
#151191 = CARTESIAN_POINT('Ctrl Pts',(-28.6142444612186,14.2842118886259,
127.689596183375)) ;
#151192 = CARTESIAN_POINT('Ctrl Pts',(-28.6857946550641,14.4299775435325,
127.931754504999)) ;
#151193 = CARTESIAN_POINT('Ctrl Pts',(-28.7673480084958,14.503331032243,128.203286809695)) ;
#151194 = CARTESIAN_POINT('Ctrl Pts',(-28.8509261449003,14.4992417837061,
128.480336479146)) ;
#151195 = CARTESIAN_POINT('Ctrl Pts',(-28.9318023648984,14.4177939822546,
128.749907191947)) ;
#151196 = CARTESIAN_POINT('Ctrl Pts',(-29.001910688641,14.2650806147523,128.987818507409)) ;
#151197 = CARTESIAN_POINT('Ctrl Pts',(-29.0559489688668,14.0529681509037,
129.178698338362)) ;
#151198 = CARTESIAN_POINT('Ctrl Pts',(-29.0896354038435,13.7955270319932,
129.310187588582)) ;
#151199 = CARTESIAN_POINT('Ctrl Pts',(-29.099611948193,13.5095709535078,129.372622374006)) ;
#151200 = CARTESIAN_POINT('Ctrl Pts',(-29.0842585907111,13.2189036520177,
129.360885383851)) ;
#151201 = CARTESIAN_POINT('Ctrl Pts',(-29.0443620584725,12.9437120966298,
129.277345257376)) ;
#151202 = CARTESIAN_POINT('Ctrl Pts',(-28.9817282559493,12.7018113312773,
129.127496651977)) ;
#151203 = CARTESIAN_POINT('Ctrl Pts',(-28.900103185758,12.5115374792667,128.922195104015)) ;
#151204 = CARTESIAN_POINT('Ctrl Pts',(-28.8047562754635,12.3865362509785,
128.676787399727)) ;
#151205 = CARTESIAN_POINT('Ctrl Pts',(-28.7012853562746,12.3360647683775,
128.40778833087)) ;
#151206 = CARTESIAN_POINT('Ctrl Pts',(-28.5980648305844,12.3630945002041,
128.139111767235)) ;
#151207 = CARTESIAN_POINT('Ctrl Pts',(-28.4992221941751,12.4665769548229,
127.883658010127)) ;
#151208 = CARTESIAN_POINT('Ctrl Pts',(-28.4131594840602,12.637873730405,127.665272376222)) ;
#151209 = CARTESIAN_POINT('Ctrl Pts',(-28.3441687124707,12.8661806742055,
127.496923307267)) ;
#151210 = CARTESIAN_POINT('Ctrl Pts',(-28.2971179753842,13.1333277515124,
127.392512752519)) ;
#151211 = CARTESIAN_POINT('Ctrl Pts',(-28.2742141661044,13.4221934836715,
127.358771264461)) ;
#151212 = CARTESIAN_POINT('Ctrl Pts',(-28.2765820238562,13.7107571318464,
127.398801174816)) ;
#151213 = CARTESIAN_POINT('Ctrl Pts',(-28.3034962448371,13.9798563780996,
127.510697252844)) ;
#151214 = CARTESIAN_POINT('Ctrl Pts',(-28.3518348917567,14.2070905580459,
127.684913382421)) ;
#151215 = CARTESIAN_POINT('Ctrl Pts',(-28.417736051092,14.3790287482914,127.910539859451)) ;
#151216 = CARTESIAN_POINT('Ctrl Pts',(-28.4956163030634,14.4826462514907,
128.171126340958)) ;
#151217 = CARTESIAN_POINT('Ctrl Pts',(-28.5798455524846,14.5101765749395,
128.450506444325)) ;
#151218 = CARTESIAN_POINT('Ctrl Pts',(-28.66200834704,14.4602521093363,128.723409993032)) ;
#151219 = CARTESIAN_POINT('Ctrl Pts',(-28.7375813833395,14.3349863303821,
128.977516850491)) ;
#151220 = CARTESIAN_POINT('Ctrl Pts',(-28.7985628235098,14.1459036519263,
129.188607444567)) ;
#151221 = CARTESIAN_POINT('Ctrl Pts',(-28.8411540818564,13.9042674567381,
129.346179660859)) ;
#151222 = CARTESIAN_POINT('Ctrl Pts',(-28.8610016097192,13.6274934121279,
129.437359596521)) ;
#151223 = CARTESIAN_POINT('Ctrl Pts',(-28.8560349310886,13.3375401227482,
129.455886266098)) ;
#151224 = CARTESIAN_POINT('Ctrl Pts',(-28.8260275084833,13.0529656397982,
129.401339308127)) ;
#151225 = CARTESIAN_POINT('Ctrl Pts',(-28.7718240751871,12.793542004979,129.276308893705)) ;
#151226 = CARTESIAN_POINT('Ctrl Pts',(-28.69758931411,12.5815361452067,129.09244647551)) ;
#151227 = CARTESIAN_POINT('Ctrl Pts',(-28.607191982818,12.4287258471182,128.861490887195)) ;
#151228 = CARTESIAN_POINT('Ctrl Pts',(-28.5062114306704,12.3470719994747,
128.599714513405)) ;
#151229 = CARTESIAN_POINT('Ctrl Pts',(-28.4016831964791,12.3430683223392,
128.327512526391)) ;
#151230 = CARTESIAN_POINT('Ctrl Pts',(-28.3008205475048,12.4155936091128,
128.065797526111)) ;
#151231 = CARTESIAN_POINT('Ctrl Pts',(-28.2086887982306,12.5608875783812,
127.829855784513)) ;
#151232 = CARTESIAN_POINT('Ctrl Pts',(-28.1322966051425,12.7672957855937,
127.639749496506)) ;
#151233 = CARTESIAN_POINT('Ctrl Pts',(-28.0757288054588,13.0219896288371,
127.507742576733)) ;
#151234 = CARTESIAN_POINT('Ctrl Pts',(-28.0429540969002,13.3035436342973,
127.44499916588)) ;
#151235 = CARTESIAN_POINT('Ctrl Pts',(-28.0350385580784,13.5948422510341,
127.455024273178)) ;
#151236 = CARTESIAN_POINT('Ctrl Pts',(-28.0521494910461,13.8739529691167,
127.538171398898)) ;
#151237 = CARTESIAN_POINT('Ctrl Pts',(-28.0921989061459,14.1203174233417,
127.688276422386)) ;
#151238 = CARTESIAN_POINT('Ctrl Pts',(-28.151557364416,14.3167168643634,127.894769419474)) ;
#151239 = CARTESIAN_POINT('Ctrl Pts',(-28.2253962663715,14.4494066861711,
128.14361033343)) ;
#151240 = CARTESIAN_POINT('Ctrl Pts',(-28.3077059790347,14.5084702688582,
128.41722565312)) ;
#151241 = CARTESIAN_POINT('Ctrl Pts',(-28.3916026412673,14.489700746972,128.695408809309)) ;
#151242 = CARTESIAN_POINT('Ctrl Pts',(-28.4706094716546,14.3946106074975,
128.959339303664)) ;
#151243 = CARTESIAN_POINT('Ctrl Pts',(-28.5383385063881,14.2294635345246,
129.190381875795)) ;
#151244 = CARTESIAN_POINT('Ctrl Pts',(-28.5888615094772,14.0073333887475,
129.371024757805)) ;
#151245 = CARTESIAN_POINT('Ctrl Pts',(-28.6182752167583,13.7435828448799,
129.490009369002)) ;
#151246 = CARTESIAN_POINT('Ctrl Pts',(-28.6235344183767,13.454824745877,129.538667492509)) ;
#151247 = CARTESIAN_POINT('Ctrl Pts',(-28.6035941708859,13.1663898496403,
129.513405963783)) ;
#151248 = CARTESIAN_POINT('Ctrl Pts',(-28.5591016772346,12.8948251888563,
129.416595319443)) ;
#151249 = CARTESIAN_POINT('Ctrl Pts',(-28.4924613979654,12.6613614393991,
129.255069109059)) ;
#151250 = CARTESIAN_POINT('Ctrl Pts',(-28.4079858158223,12.4827884864443,
129.041374692839)) ;
#151251 = CARTESIAN_POINT('Ctrl Pts',(-28.3106810095428,12.3713198999723,
128.790256537741)) ;
#151252 = CARTESIAN_POINT('Ctrl Pts',(-28.2071142233906,12.3351536539427,
128.520782151597)) ;
#151253 = CARTESIAN_POINT('Ctrl Pts',(-28.1033170651269,12.3771106003778,
128.250789621036)) ;
#151254 = CARTESIAN_POINT('Ctrl Pts',(-28.0070122936131,12.493746042562,128.002507073001)) ;
#151255 = CARTESIAN_POINT('Ctrl Pts',(-27.9236042223444,12.6767291405437,
127.791947198724)) ;
#151256 = CARTESIAN_POINT('Ctrl Pts',(-27.8582788554542,12.9147362953278,
127.634399931538)) ;
#151257 = CARTESIAN_POINT('Ctrl Pts',(-27.8157639814054,13.1870897175325,
127.543206911709)) ;
#151258 = CARTESIAN_POINT('Ctrl Pts',(-27.7976113632335,13.4771402294594,
127.523294837643)) ;
#151259 = CARTESIAN_POINT('Ctrl Pts',(-27.8047562191335,13.7642376991577,
127.577383148529)) ;
#151260 = CARTESIAN_POINT('Ctrl Pts',(-27.8359687279842,14.0261140050281,
127.701710177171)) ;
#151261 = CARTESIAN_POINT('Ctrl Pts',(-27.8877875139809,14.2437566095146,
127.886037495367)) ;
#151262 = CARTESIAN_POINT('Ctrl Pts',(-27.9566643830394,14.4043004510961,
128.12048462873)) ;
#151263 = CARTESIAN_POINT('Ctrl Pts',(-28.0360570915207,14.4936451763547,
128.385451901082)) ;
#151264 = CARTESIAN_POINT('Ctrl Pts',(-28.120129115805,14.5067755223083,128.664180642723)) ;
#151265 = CARTESIAN_POINT('Ctrl Pts',(-28.2020346856407,14.4421251633059,
128.936606880987)) ;
#151266 = CARTESIAN_POINT('Ctrl Pts',(-28.2751125216823,14.3039891726026,
129.183284767789)) ;
#151267 = CARTESIAN_POINT('Ctrl Pts',(-28.3330260630189,14.1040922169467,
129.385445944809)) ;
#151268 = CARTESIAN_POINT('Ctrl Pts',(-28.3716774412633,13.8535852347893,
129.531620171577)) ;
#151269 = CARTESIAN_POINT('Ctrl Pts',(-28.3868553207156,13.5730952435811,
129.609080622274)) ;
#151270 = CARTESIAN_POINT('Ctrl Pts',(-28.3771751540194,13.2829861782011,
129.613807074417)) ;
#151271 = CARTESIAN_POINT('Ctrl Pts',(-28.3425095932928,13.0017737284941,
129.545666888846)) ;
#151272 = CARTESIAN_POINT('Ctrl Pts',(-28.284301937165,12.7500890797144,129.408856898039)) ;
#151273 = CARTESIAN_POINT('Ctrl Pts',(-28.2064572920802,12.5475577998432,
129.214559307957)) ;
#151274 = CARTESIAN_POINT('Ctrl Pts',(-28.1135171544018,12.4075652478031,
128.976210428243)) ;
#151275 = CARTESIAN_POINT('Ctrl Pts',(-28.0118850220544,12.3405227377109,
128.712349934362)) ;
#151276 = CARTESIAN_POINT('Ctrl Pts',(-27.9073393263242,12.3506975715296,
128.440115510787)) ;
#151277 = CARTESIAN_POINT('Ctrl Pts',(-27.8069898708441,12.438177489278,128.180166701549)) ;
#151278 = CARTESIAN_POINT('Ctrl Pts',(-27.7177045614419,12.5958827964123,
127.952426644854)) ;
#151279 = CARTESIAN_POINT('Ctrl Pts',(-27.6448174995369,12.8123887822574,
127.772559198421)) ;
#151280 = CARTESIAN_POINT('Ctrl Pts',(-27.5925658802496,13.0732934241726,
127.653072879261)) ;
#151281 = CARTESIAN_POINT('Ctrl Pts',(-27.5643119574423,13.3601444544887,
127.603779546763)) ;
#151282 = CARTESIAN_POINT('Ctrl Pts',(-27.5613082454556,13.6487324697402,
127.627925538602)) ;
#151283 = CARTESIAN_POINT('Ctrl Pts',(-27.5828722691528,13.9231969052117,
127.724074394844)) ;
#151284 = CARTESIAN_POINT('Ctrl Pts',(-27.6269024064909,14.1616648845749,
127.885829090303)) ;
#151285 = CARTESIAN_POINT('Ctrl Pts',(-27.6896598747405,14.3474885130478,
128.102376258084)) ;
#151286 = CARTESIAN_POINT('Ctrl Pts',(-27.7653992680876,14.4664584587802,
128.356681964705)) ;
#151287 = CARTESIAN_POINT('Ctrl Pts',(-27.8487981620875,14.5109046603937,
128.633576137683)) ;
#151288 = CARTESIAN_POINT('Ctrl Pts',(-27.9318850392023,14.477538406395,128.909237750788)) ;
#151289 = CARTESIAN_POINT('Ctrl Pts',(-28.0095052256554,14.3681997132881,
129.169245881706)) ;
#151290 = CARTESIAN_POINT('Ctrl Pts',(-28.0741401659524,14.19161807787,129.391120281656)) ;
#151291 = CARTESIAN_POINT('Ctrl Pts',(-28.1210449004513,13.9603524956053,
129.561209556167)) ;
#151292 = CARTESIAN_POINT('Ctrl Pts',(-28.1460961632202,13.6895220911817,
129.667588782595)) ;
#151293 = CARTESIAN_POINT('Ctrl Pts',(-28.1465838645101,13.4007319641459,
129.702076763037)) ;
#151294 = CARTESIAN_POINT('Ctrl Pts',(-28.1219792750298,13.1132078283894,
129.663296512428)) ;
#151295 = CARTESIAN_POINT('Ctrl Pts',(-28.072797303837,12.8466068578935,129.552900494661)) ;
#151296 = CARTESIAN_POINT('Ctrl Pts',(-28.0028760663637,12.6236984730367,
129.381571768306)) ;
#151297 = CARTESIAN_POINT('Ctrl Pts',(-27.9152289217031,12.4561011970055,
129.15875880179)) ;
#151298 = CARTESIAN_POINT('Ctrl Pts',(-27.8163074914158,12.3585968124196,
128.902876316079)) ;
#151299 = CARTESIAN_POINT('Ctrl Pts',(-27.7120492591559,12.3371246735504,
128.631455165304)) ;
#151300 = CARTESIAN_POINT('Ctrl Pts',(-27.6093731664381,12.3935413485491,
128.364635405542)) ;
#151301 = CARTESIAN_POINT('Ctrl Pts',(-27.5149001295544,12.5236723848828,
128.121769416389)) ;
#151302 = CARTESIAN_POINT('Ctrl Pts',(-27.4346201824783,12.7179304240541,
127.920341279588)) ;
#151303 = CARTESIAN_POINT('Ctrl Pts',(-27.3732833708595,12.9643000603806,
127.774449881944)) ;
#151304 = CARTESIAN_POINT('Ctrl Pts',(-27.3353218805088,13.2410161239663,
127.696515666237)) ;
#151305 = CARTESIAN_POINT('Ctrl Pts',(-27.3219345106549,13.5320326358814,
127.690536193544)) ;
#151306 = CARTESIAN_POINT('Ctrl Pts',(-27.3336868555628,13.8151976332958,
127.757981771659)) ;
#151307 = CARTESIAN_POINT('Ctrl Pts',(-27.3691045396702,14.070965110173,127.894657472177)) ;
#151308 = CARTESIAN_POINT('Ctrl Pts',(-27.4247538548607,14.2795161854134,
128.090342542637)) ;
#151309 = CARTESIAN_POINT('Ctrl Pts',(-27.495823154164,14.4266233568165,128.331023842141)) ;
#151310 = CARTESIAN_POINT('Ctrl Pts',(-27.5766922115291,14.5021444966585,
128.600366276399)) ;
#151311 = CARTESIAN_POINT('Ctrl Pts',(-27.6609223179021,14.5004799279669,
128.8795751742)) ;
#151312 = CARTESIAN_POINT('Ctrl Pts',(-27.7417671934519,14.4210758361391,
129.14896837329)) ;
#151313 = CARTESIAN_POINT('Ctrl Pts',(-27.8120265768946,14.2711637356508,
129.38719326095)) ;
#151314 = CARTESIAN_POINT('Ctrl Pts',(-27.866891762874,14.0600320259714,129.580611011308)) ;
#151315 = CARTESIAN_POINT('Ctrl Pts',(-27.9012411174026,13.8025046463563,
129.714162963611)) ;
#151316 = CARTESIAN_POINT('Ctrl Pts',(-27.9118652501947,13.5194350300881,
129.778210865001)) ;
#151317 = CARTESIAN_POINT('Ctrl Pts',(-27.8973675127668,13.227929848522,129.769057927685)) ;
#151318 = CARTESIAN_POINT('Ctrl Pts',(-27.8581217638387,12.9514279979351,
129.687479679852)) ;
#151319 = CARTESIAN_POINT('Ctrl Pts',(-27.7958487933346,12.7076270254922,
129.538792895781)) ;
#151320 = CARTESIAN_POINT('Ctrl Pts',(-27.7150442368328,12.5164543914562,
129.335744778992)) ;
#151321 = CARTESIAN_POINT('Ctrl Pts',(-27.6197799723084,12.3891143889345,
129.090666143106)) ;
#151322 = CARTESIAN_POINT('Ctrl Pts',(-27.5169840616899,12.3364756158918,
128.823462340777)) ;
#151323 = CARTESIAN_POINT('Ctrl Pts',(-27.4129425204162,12.3612642231578,
128.552629149903)) ;
#151324 = CARTESIAN_POINT('Ctrl Pts',(-27.3139116309648,12.4629838840005,
128.296612691349)) ;
#151325 = CARTESIAN_POINT('Ctrl Pts',(-27.2276350555539,12.6321971699934,
128.077535896234)) ;
#151326 = CARTESIAN_POINT('Ctrl Pts',(-27.1581753164316,12.8584558798932,
127.907740199772)) ;
#151327 = CARTESIAN_POINT('Ctrl Pts',(-27.1102193532803,13.1261648647243,
127.800864060768)) ;
#151328 = CARTESIAN_POINT('Ctrl Pts',(-27.0867427780488,13.4141234552309,
127.765371910168)) ;
#151329 = CARTESIAN_POINT('Ctrl Pts',(-27.088405263082,13.7023852342343,127.803282253112)) ;
#151330 = CARTESIAN_POINT('Ctrl Pts',(-27.1144094066955,13.9714212012371,
127.912378068659)) ;
#151331 = CARTESIAN_POINT('Ctrl Pts',(-27.1625636190418,14.202020081249,128.086338189894)) ;
#151332 = CARTESIAN_POINT('Ctrl Pts',(-27.2279041571622,14.3750071736422,
128.310222999053)) ;
#151333 = CARTESIAN_POINT('Ctrl Pts',(-27.3055089641359,14.4806351346196,
128.570006270221)) ;
#151334 = CARTESIAN_POINT('Ctrl Pts',(-27.3892702869014,14.5105855297535,
128.847858683373)) ;
#151335 = CARTESIAN_POINT('Ctrl Pts',(-27.4721256647169,14.4625550657111,
129.123019817885)) ;
#151336 = CARTESIAN_POINT('Ctrl Pts',(-27.5475424958297,14.3400369417443,
129.376461860258)) ;
#151337 = CARTESIAN_POINT('Ctrl Pts',(-27.6092868870231,14.1521957535254,
129.589908595948)) ;
#151338 = CARTESIAN_POINT('Ctrl Pts',(-27.6524549950664,13.9116489154345,
129.749173070005)) ;
#151339 = CARTESIAN_POINT('Ctrl Pts',(-27.6729767158619,13.6358544266559,
129.842295420114)) ;
#151340 = CARTESIAN_POINT('Ctrl Pts',(-27.6687686357343,13.3459427675745,
129.863045715734)) ;
#151341 = CARTESIAN_POINT('Ctrl Pts',(-27.6393546558192,13.0604649745041,
129.810291983176)) ;
#151342 = CARTESIAN_POINT('Ctrl Pts',(-27.5861749748563,12.8015143832803,
129.688047174148)) ;
#151343 = CARTESIAN_POINT('Ctrl Pts',(-27.5122453552566,12.586871423154,129.505215644939)) ;
#151344 = CARTESIAN_POINT('Ctrl Pts',(-27.4222257102063,12.4323032180318,
129.275353955494)) ;
#151345 = CARTESIAN_POINT('Ctrl Pts',(-27.321814640165,12.348604012381,129.015131363742)) ;
#151346 = CARTESIAN_POINT('Ctrl Pts',(-27.2172646277251,12.3418345254331,
128.742874357153)) ;
#151347 = CARTESIAN_POINT('Ctrl Pts',(-27.1155991989799,12.4127257697425,
128.479021774659)) ;
#151348 = CARTESIAN_POINT('Ctrl Pts',(-27.0235546029965,12.5554430365515,
128.24317434018)) ;
#151349 = CARTESIAN_POINT('Ctrl Pts',(-26.946364611968,12.7608029240068,128.050846584327)) ;
#151350 = CARTESIAN_POINT('Ctrl Pts',(-26.8892425932522,13.0143079229722,
127.917197312737)) ;
#151351 = CARTESIAN_POINT('Ctrl Pts',(-26.8557397574038,13.2953661026702,
127.852335782128)) ;
#151352 = CARTESIAN_POINT('Ctrl Pts',(-26.8471237684322,13.587499191953,127.86040257377)) ;
#151353 = CARTESIAN_POINT('Ctrl Pts',(-26.8636409106043,13.8669338626205,
127.941791701437)) ;
#151354 = CARTESIAN_POINT('Ctrl Pts',(-26.9028894020443,14.1134263503453,
128.089413302891)) ;
#151355 = CARTESIAN_POINT('Ctrl Pts',(-26.9618864660315,14.3121780897716,
128.294946112899)) ;
#151356 = CARTESIAN_POINT('Ctrl Pts',(-27.0356609756341,14.4470050265316,
128.543696981495)) ;
#151357 = CARTESIAN_POINT('Ctrl Pts',(-27.1176846698481,14.5078086325279,
128.816414339099)) ;
#151358 = CARTESIAN_POINT('Ctrl Pts',(-27.2013501944063,14.4913412737729,
129.093814747738)) ;
#151359 = CARTESIAN_POINT('Ctrl Pts',(-27.2805727554514,14.3985299043882,
129.358365317732)) ;
#151360 = CARTESIAN_POINT('Ctrl Pts',(-27.3487809879748,14.2353764928408,
129.590815975098)) ;
#151361 = CARTESIAN_POINT('Ctrl Pts',(-27.4000923756535,14.0132824388172,
129.773951949604)) ;
#151362 = CARTESIAN_POINT('Ctrl Pts',(-27.4299031588905,13.751770584179,129.893917739675)) ;
#151363 = CARTESIAN_POINT('Ctrl Pts',(-27.4360065328396,13.4639004603942,
129.944990740374)) ;
#151364 = CARTESIAN_POINT('Ctrl Pts',(-27.4166194504997,13.1736259559936,
129.921533138526)) ;
#151365 = CARTESIAN_POINT('Ctrl Pts',(-27.3730557967721,12.9029494351804,
129.827230137503)) ;
#151366 = CARTESIAN_POINT('Ctrl Pts',(-27.3068239081708,12.6670694829694,
129.667025348139)) ;
#151367 = CARTESIAN_POINT('Ctrl Pts',(-27.2225807375648,12.4867414535482,
129.454064281963)) ;
#151368 = CARTESIAN_POINT('Ctrl Pts',(-27.1260163205075,12.3736046950475,
129.204955161642)) ;
#151369 = CARTESIAN_POINT('Ctrl Pts',(-27.0219531940928,12.3351061359291,
128.934221171249)) ;
#151370 = CARTESIAN_POINT('Ctrl Pts',(-26.9187654991147,12.3747297412366,
128.665782677207)) ;
#151371 = CARTESIAN_POINT('Ctrl Pts',(-26.8219192185406,12.4890530273647,
128.415981781108)) ;
#151372 = CARTESIAN_POINT('Ctrl Pts',(-26.7375618368722,12.6718473822343,
128.20287552548)) ;
#151373 = CARTESIAN_POINT('Ctrl Pts',(-26.6721408995713,12.9071471042355,
128.044830293244)) ;
#151374 = CARTESIAN_POINT('Ctrl Pts',(-26.6288268693924,13.1791583633753,
127.951366546025)) ;
#151375 = CARTESIAN_POINT('Ctrl Pts',(-26.6100146219695,13.4685703303894,
127.929472625113)) ;
#151376 = CARTESIAN_POINT('Ctrl Pts',(-26.6163965606096,13.7556865610863,
127.981289936006)) ;
#151377 = CARTESIAN_POINT('Ctrl Pts',(-26.6468365176563,14.0184520779736,
128.103328446011)) ;
#151378 = CARTESIAN_POINT('Ctrl Pts',(-26.6983664732469,14.2386835545227,
128.286981099105)) ;
#151379 = CARTESIAN_POINT('Ctrl Pts',(-26.7668561678463,14.4009245247973,
128.520283146029)) ;
#151380 = CARTESIAN_POINT('Ctrl Pts',(-26.8462801396179,14.4923209079493,
128.785440445302)) ;
#151381 = CARTESIAN_POINT('Ctrl Pts',(-26.9299042318789,14.5074993821674,
129.062691208225)) ;
#151382 = CARTESIAN_POINT('Ctrl Pts',(-27.0123042045344,14.4446391320812,
129.336708219525)) ;
#151383 = CARTESIAN_POINT('Ctrl Pts',(-27.0853285109314,14.309013886893,129.583057807955)) ;
#151384 = CARTESIAN_POINT('Ctrl Pts',(-27.1438828659143,14.1104149351794,
129.787163074108)) ;
#151385 = CARTESIAN_POINT('Ctrl Pts',(-27.1830524640317,13.8614588559076,
129.934789891105)) ;
#151386 = CARTESIAN_POINT('Ctrl Pts',(-27.1989887778394,13.5819687002437,
130.014428956727)) ;
#151387 = CARTESIAN_POINT('Ctrl Pts',(-27.1899960665713,13.2906279013141,
130.021303572167)) ;
#151388 = CARTESIAN_POINT('Ctrl Pts',(-27.1559614540415,13.009243305788,129.95497149067)) ;
#151389 = CARTESIAN_POINT('Ctrl Pts',(-27.0987240639522,12.7575168112921,
129.820836098485)) ;
#151390 = CARTESIAN_POINT('Ctrl Pts',(-27.0211347642334,12.5525240138587,
129.627409702748)) ;
#151391 = CARTESIAN_POINT('Ctrl Pts',(-26.9288019853003,12.4108770336832,
129.390743830787)) ;
#151392 = CARTESIAN_POINT('Ctrl Pts',(-26.8269925769389,12.3412909140522,
129.126483822534)) ;
#151393 = CARTESIAN_POINT('Ctrl Pts',(-26.7225678003105,12.3493861735078,
128.854556329981)) ;
#151394 = CARTESIAN_POINT('Ctrl Pts',(-26.6222736426069,12.4342727909203,
128.594675298208)) ;
#151395 = CARTESIAN_POINT('Ctrl Pts',(-26.5324245140866,12.5900489009072,
128.365332500197)) ;
#151396 = CARTESIAN_POINT('Ctrl Pts',(-26.4587946173494,12.8056265995217,
128.183382042886)) ;
#151397 = CARTESIAN_POINT('Ctrl Pts',(-26.4059966216722,13.0653848746049,
128.062274396553)) ;
#151398 = CARTESIAN_POINT('Ctrl Pts',(-26.3770384247468,13.3504851063388,
128.01077693268)) ;
#151399 = CARTESIAN_POINT('Ctrl Pts',(-26.3732580768289,13.6412798147236,
128.032889399786)) ;
#151400 = CARTESIAN_POINT('Ctrl Pts',(-26.3941468859038,13.915548156852,128.126957619226)) ;
#151401 = CARTESIAN_POINT('Ctrl Pts',(-26.4375236270793,14.1552942040558,
128.286796725341)) ;
#151402 = CARTESIAN_POINT('Ctrl Pts',(-26.499786802166,14.3429101935435,128.501891901076)) ;
#151403 = CARTESIAN_POINT('Ctrl Pts',(-26.5753221744753,14.4639893047867,
128.755644371512)) ;
#151404 = CARTESIAN_POINT('Ctrl Pts',(-26.658258796401,14.5107279953385,129.031049167775)) ;
#151405 = CARTESIAN_POINT('Ctrl Pts',(-26.7418770326506,14.4794893752074,
129.308446128137)) ;
#151406 = CARTESIAN_POINT('Ctrl Pts',(-26.819410154467,14.3727211578977,129.56804219168)) ;
#151407 = CARTESIAN_POINT('Ctrl Pts',(-26.884660652684,14.1977799584113,129.791786901947)) ;
#151408 = CARTESIAN_POINT('Ctrl Pts',(-26.9321606344241,13.9680803032242,
129.963592933574)) ;
#151409 = CARTESIAN_POINT('Ctrl Pts',(-26.9579703404882,13.6967826933105,
130.072347583536)) ;
#151410 = CARTESIAN_POINT('Ctrl Pts',(-26.9591310030642,13.4094043760888,
130.108663362794)) ;
#151411 = CARTESIAN_POINT('Ctrl Pts',(-26.935231210856,13.1212039321583,130.071985580596)) ;
#151412 = CARTESIAN_POINT('Ctrl Pts',(-26.8869426549206,12.8546896237207,
129.964066829109)) ;
#151413 = CARTESIAN_POINT('Ctrl Pts',(-26.8174482093006,12.6293810356165,
129.794091823838)) ;
#151414 = CARTESIAN_POINT('Ctrl Pts',(-26.7297563031988,12.4594635396626,
129.571300039305)) ;
#151415 = CARTESIAN_POINT('Ctrl Pts',(-26.6315768169788,12.3604529302704,
129.317412505758)) ;
#151416 = CARTESIAN_POINT('Ctrl Pts',(-26.527041677516,12.3366695079855,129.045292118923)) ;
#151417 = CARTESIAN_POINT('Ctrl Pts',(-26.4246632418904,12.3907630606801,
128.779202667163)) ;
#151418 = CARTESIAN_POINT('Ctrl Pts',(-26.3296624090555,12.5187717527639,
128.534846855937)) ;
#151419 = CARTESIAN_POINT('Ctrl Pts',(-26.2486292653153,12.7125553045139,
128.331370691531)) ;
#151420 = CARTESIAN_POINT('Ctrl Pts',(-26.187290463919,12.9551208485313,128.185129058602)) ;
#151421 = CARTESIAN_POINT('Ctrl Pts',(-26.1482420973643,13.2325620060974,
128.104210130242)) ;
#151422 = CARTESIAN_POINT('Ctrl Pts',(-26.1341913899476,13.5243419796884,
128.096383572714)) ;
#151423 = CARTESIAN_POINT('Ctrl Pts',(-26.1452118388481,13.8069926528057,
128.161574113629)) ;
#151424 = CARTESIAN_POINT('Ctrl Pts',(-26.1799390075941,14.0639000199269,
128.296232665471)) ;
#151425 = CARTESIAN_POINT('Ctrl Pts',(-26.2350489546991,14.2741558930926,
128.490347023028)) ;
#151426 = CARTESIAN_POINT('Ctrl Pts',(-26.3059077450582,14.4234615625839,
128.730487186166)) ;
#151427 = CARTESIAN_POINT('Ctrl Pts',(-26.386494169588,14.5011170686614,128.998961276038)) ;
#151428 = CARTESIAN_POINT('Ctrl Pts',(-26.4710372754606,14.5013614779113,
129.279215621043)) ;
#151429 = CARTESIAN_POINT('Ctrl Pts',(-26.5513450363698,14.4249956630962,
129.546727763435)) ;
#151430 = CARTESIAN_POINT('Ctrl Pts',(-26.6226216620681,14.2760171565871,
129.788206158856)) ;
#151431 = CARTESIAN_POINT('Ctrl Pts',(-26.6777858163634,14.0665442400002,
129.982426179449)) ;
#151432 = CARTESIAN_POINT('Ctrl Pts',(-26.7127743428566,13.8110528410318,
130.117741076645)) ;
#151433 = CARTESIAN_POINT('Ctrl Pts',(-26.7241069347589,13.5262786463887,
130.184114351317)) ;
#151434 = CARTESIAN_POINT('Ctrl Pts',(-26.7103978253846,13.2368369901033,
130.177011615775)) ;
#151435 = CARTESIAN_POINT('Ctrl Pts',(-26.6716560461567,12.9583255903659,
130.097075764209)) ;
#151436 = CARTESIAN_POINT('Ctrl Pts',(-26.6103674672222,12.7145800096232,
129.95106877123)) ;
#151437 = CARTESIAN_POINT('Ctrl Pts',(-26.5292783226885,12.5201730384604,
129.747494551372)) ;
#151438 = CARTESIAN_POINT('Ctrl Pts',(-26.4353195353877,12.392297716127,129.505869698294)) ;
#151439 = CARTESIAN_POINT('Ctrl Pts',(-26.3321003131888,12.3368042043637,
129.23762472755)) ;
#151440 = CARTESIAN_POINT('Ctrl Pts',(-26.2283359448761,12.3594079574846,
128.967488898529)) ;
#151441 = CARTESIAN_POINT('Ctrl Pts',(-26.1289374320057,12.4588426243277,
128.710432008687)) ;
#151442 = CARTESIAN_POINT('Ctrl Pts',(-26.0421433826271,12.6263832935465,
128.489874381818)) ;
#151443 = CARTESIAN_POINT('Ctrl Pts',(-25.9721170036289,12.8513078071139,
128.318433909601)) ;
#151444 = CARTESIAN_POINT('Ctrl Pts',(-25.9235411833855,13.1175341941134,
128.209680256936)) ;
#151445 = CARTESIAN_POINT('Ctrl Pts',(-25.8992723616796,13.4059954970849,
128.171974342421)) ;
#151446 = CARTESIAN_POINT('Ctrl Pts',(-25.9001789667653,13.6942419645787,
128.207632461566)) ;
#151447 = CARTESIAN_POINT('Ctrl Pts',(-25.9258216003677,13.9656571359195,
128.31589284879)) ;
#151448 = CARTESIAN_POINT('Ctrl Pts',(-25.9727492712161,14.1945698215837,
128.485818180082)) ;
#151449 = CARTESIAN_POINT('Ctrl Pts',(-26.0380351219601,14.3711224528334,
128.709801837872)) ;
#151450 = CARTESIAN_POINT('Ctrl Pts',(-26.115372034482,14.4785950091488,128.968780330961)) ;
#151451 = CARTESIAN_POINT('Ctrl Pts',(-26.1991386228248,14.5108133112394,
129.246686766249)) ;
#151452 = CARTESIAN_POINT('Ctrl Pts',(-26.281961118953,14.4650394200622,129.521689731091)) ;
#151453 = CARTESIAN_POINT('Ctrl Pts',(-26.3576691539897,14.3446919400874,
129.775975443665)) ;
#151454 = CARTESIAN_POINT('Ctrl Pts',(-26.4199450377268,14.1586507898245,
129.990981699106)) ;
#151455 = CARTESIAN_POINT('Ctrl Pts',(-26.4638325348643,13.9182142591253,
130.152493567261)) ;
#151456 = CARTESIAN_POINT('Ctrl Pts',(-26.4849121372087,13.6446894301756,
130.247054976681)) ;
#151457 = CARTESIAN_POINT('Ctrl Pts',(-26.4814409395297,13.3538163555555,
130.270090586414)) ;
#151458 = CARTESIAN_POINT('Ctrl Pts',(-26.4527946492839,13.0687529323482,
130.219476965581)) ;
#151459 = CARTESIAN_POINT('Ctrl Pts',(-26.4002320096581,12.8084025711039,
130.099079794229)) ;
#151460 = CARTESIAN_POINT('Ctrl Pts',(-26.3268756685072,12.5923662507696,
129.91790410308)) ;
#151461 = CARTESIAN_POINT('Ctrl Pts',(-26.2371123368209,12.4355966936421,
129.688843066008)) ;
#151462 = CARTESIAN_POINT('Ctrl Pts',(-26.1367181878628,12.3498834173245,
129.42872587461)) ;
#151463 = CARTESIAN_POINT('Ctrl Pts',(-26.032722719753,12.3409542808635,129.157919642926)) ;
#151464 = CARTESIAN_POINT('Ctrl Pts',(-25.9308084387583,12.4093757248112,
128.893357587352)) ;
#151465 = CARTESIAN_POINT('Ctrl Pts',(-25.838155620905,12.5505196315372,128.655821078007)) ;
#151466 = CARTESIAN_POINT('Ctrl Pts',(-25.7605740007468,12.7541803006072,
128.462316845571)) ;
#151467 = CARTESIAN_POINT('Ctrl Pts',(-25.7029450253967,13.0055267425044,
128.327067990315)) ;
#151468 = CARTESIAN_POINT('Ctrl Pts',(-25.6685657347824,13.2870724884799,
128.259776019344)) ;
#151469 = CARTESIAN_POINT('Ctrl Pts',(-25.6592502061655,13.5781354317469,
128.265673438089)) ;
#151470 = CARTESIAN_POINT('Ctrl Pts',(-25.6749179654199,13.8583662507443,
128.344586199981)) ;
#151471 = CARTESIAN_POINT('Ctrl Pts',(-25.7137374162889,14.1072755060793,
128.491117013587)) ;
#151472 = CARTESIAN_POINT('Ctrl Pts',(-25.7721169966564,14.3069765889331,
128.694755702354)) ;
#151473 = CARTESIAN_POINT('Ctrl Pts',(-25.845207577047,14.443614067786,128.941381531894)) ;
#151474 = CARTESIAN_POINT('Ctrl Pts',(-25.9273346325596,14.5071928082345,
129.214515131727)) ;
#151475 = CARTESIAN_POINT('Ctrl Pts',(-26.011234962119,14.4928945220509,129.492675842775)) ;
#151476 = CARTESIAN_POINT('Ctrl Pts',(-26.0906570279007,14.4021254936154,
129.757803067043)) ;
#151477 = CARTESIAN_POINT('Ctrl Pts',(-26.159082383682,14.2413770477371,129.990792154917)) ;
#151478 = CARTESIAN_POINT('Ctrl Pts',(-26.2110152100895,14.0210258594474,
130.175736142196)) ;
#151479 = CARTESIAN_POINT('Ctrl Pts',(-26.241635177827,13.7594508415378,130.298196601018)) ;
#151480 = CARTESIAN_POINT('Ctrl Pts',(-26.2483473113095,13.4716753030503,
130.351078692086)) ;
#151481 = CARTESIAN_POINT('Ctrl Pts',(-26.2298541426232,13.18278007244,130.330045835803)) ;
#151482 = CARTESIAN_POINT('Ctrl Pts',(-26.1867418068547,12.9097866347109,
130.237249070666)) ;
#151483 = CARTESIAN_POINT('Ctrl Pts',(-26.1214552754847,12.6739761120234,
130.079613973061)) ;
#151484 = CARTESIAN_POINT('Ctrl Pts',(-26.037598712626,12.4911376353209,129.867849268882)) ;
#151485 = CARTESIAN_POINT('Ctrl Pts',(-25.9407649580424,12.3755758788311,
129.618129131331)) ;
#151486 = CARTESIAN_POINT('Ctrl Pts',(-25.8374214950217,12.3352662329562,
129.34929906656)) ;
#151487 = CARTESIAN_POINT('Ctrl Pts',(-25.7340098362028,12.3722006143293,
129.0802369826)) ;
#151488 = CARTESIAN_POINT('Ctrl Pts',(-25.6361773432197,12.4858118722087,
128.827819165484)) ;
#151489 = CARTESIAN_POINT('Ctrl Pts',(-25.5523274084712,12.6649628027199,
128.615825895545)) ;
#151490 = CARTESIAN_POINT('Ctrl Pts',(-25.4859513870995,12.8995424291904,
128.455121245363)) ;
#151491 = CARTESIAN_POINT('Ctrl Pts',(-25.4419863750333,13.1707489990253,
128.359746169264)) ;
#151492 = CARTESIAN_POINT('Ctrl Pts',(-25.4224009992562,13.4602465419289,
128.335630931104)) ;
#151493 = CARTESIAN_POINT('Ctrl Pts',(-25.4281061795563,13.7479094104328,
128.385491263721)) ;
#151494 = CARTESIAN_POINT('Ctrl Pts',(-25.4578216450762,14.0110933638022,
128.505345635233)) ;
#151495 = CARTESIAN_POINT('Ctrl Pts',(-25.5087967768197,14.2330195298938,
128.687396943834)) ;
#151496 = CARTESIAN_POINT('Ctrl Pts',(-25.5768933622651,14.397056415232,128.919554215411)) ;
#151497 = CARTESIAN_POINT('Ctrl Pts',(-25.6558147544988,14.4906410938832,
129.183138561615)) ;
#151498 = CARTESIAN_POINT('Ctrl Pts',(-25.7399301950195,14.5080280130628,
129.462041474598)) ;
#151499 = CARTESIAN_POINT('Ctrl Pts',(-25.8217364878674,14.4480725424633,
129.734011003358)) ;
#151500 = CARTESIAN_POINT('Ctrl Pts',(-25.8956483813608,14.3139470607326,
129.983179734343)) ;
#151501 = CARTESIAN_POINT('Ctrl Pts',(-25.9546615112484,14.1169437524237,
130.188609280051)) ;
#151502 = CARTESIAN_POINT('Ctrl Pts',(-25.994519421204,13.8684682048696,130.338337741358)) ;
#151503 = CARTESIAN_POINT('Ctrl Pts',(-26.0110568377318,13.5907243651,130.419594305655)) ;
#151504 = CARTESIAN_POINT('Ctrl Pts',(-26.0028570943019,13.2994062522709,
130.428791647391)) ;
#151505 = CARTESIAN_POINT('Ctrl Pts',(-25.9695704025357,13.0173302811176,
130.364651136717)) ;
#151506 = CARTESIAN_POINT('Ctrl Pts',(-25.9127012517306,12.7634586998748,
130.23173138777)) ;
#151507 = CARTESIAN_POINT('Ctrl Pts',(-25.8356694959319,12.5574053612187,
130.039883250671)) ;
#151508 = CARTESIAN_POINT('Ctrl Pts',(-25.7439581375389,12.4141338116398,
129.804942699892)) ;
#151509 = CARTESIAN_POINT('Ctrl Pts',(-25.6422361078924,12.342233208706,129.540970477651)) ;
#151510 = CARTESIAN_POINT('Ctrl Pts',(-25.5379082160016,12.3479816385131,
129.269286803224)) ;
#151511 = CARTESIAN_POINT('Ctrl Pts',(-25.4372492426153,12.4308508598937,
129.00839512309)) ;
#151512 = CARTESIAN_POINT('Ctrl Pts',(-25.3472402005208,12.5841342714032,
128.778486490676)) ;
#151513 = CARTESIAN_POINT('Ctrl Pts',(-25.272730898508,12.7991564308112,128.594122402279)) ;
#151514 = CARTESIAN_POINT('Ctrl Pts',(-25.2194888387276,13.0569999610756,
128.471595214616)) ;
#151515 = CARTESIAN_POINT('Ctrl Pts',(-25.1897401476562,13.3421921034464,
128.417860044275)) ;
#151516 = CARTESIAN_POINT('Ctrl Pts',(-25.1851966857885,13.6321454574867,
128.437625751363)) ;
#151517 = CARTESIAN_POINT('Ctrl Pts',(-25.2054882351433,13.9089725412032,
128.530163374861)) ;
#151518 = CARTESIAN_POINT('Ctrl Pts',(-25.2484501051326,14.1498188340954,
128.688812325716)) ;
#151519 = CARTESIAN_POINT('Ctrl Pts',(-25.3098239459612,14.3379335225619,
128.901090604678)) ;
#151520 = CARTESIAN_POINT('Ctrl Pts',(-25.3852409841119,14.4615825769609,
129.154594863581)) ;
#151521 = CARTESIAN_POINT('Ctrl Pts',(-25.4680078103566,14.5104718339952,
129.429479188798)) ;
#151522 = CARTESIAN_POINT('Ctrl Pts',(-25.5519233175472,14.4813917081873,
129.707831723369)) ;
#151523 = CARTESIAN_POINT('Ctrl Pts',(-25.6296594879759,14.3764101476522,
129.968016081421)) ;
#151524 = CARTESIAN_POINT('Ctrl Pts',(-25.6951131634194,14.2041613001764,
130.192211432841)) ;
#151525 = CARTESIAN_POINT('Ctrl Pts',(-25.7434116042681,13.9743839791119,
130.36655070585)) ;
#151526 = CARTESIAN_POINT('Ctrl Pts',(-25.7697062526325,13.7063210401926,
130.476427371815)) ;
#151527 = CARTESIAN_POINT('Ctrl Pts',(-25.7716643333024,13.416701167449,130.515370896243)) ;
#151528 = CARTESIAN_POINT('Ctrl Pts',(-25.7484303453548,13.1291677758352,
130.480525076402)) ;
#151529 = CARTESIAN_POINT('Ctrl Pts',(-25.7008468729498,12.86171027905,130.374668312212)) ;
#151530 = CARTESIAN_POINT('Ctrl Pts',(-25.6318421414092,12.6350478480017,
130.206135995294)) ;
#151531 = CARTESIAN_POINT('Ctrl Pts',(-25.5450073178082,12.4638699665219,
129.985698129429)) ;
#151532 = CARTESIAN_POINT('Ctrl Pts',(-25.4465855133018,12.3621126869917,
129.731275230113)) ;
#151533 = CARTESIAN_POINT('Ctrl Pts',(-25.3422723144961,12.336288293437,129.459748523319)) ;
#151534 = CARTESIAN_POINT('Ctrl Pts',(-25.2395464146887,12.3882079133966,
129.192710014154)) ;
#151535 = CARTESIAN_POINT('Ctrl Pts',(-25.1441554739243,12.5148240028862,
128.947268201873)) ;
#151536 = CARTESIAN_POINT('Ctrl Pts',(-25.0632912716036,12.7050812653244,
128.743995286524)) ;
#151537 = CARTESIAN_POINT('Ctrl Pts',(-25.0008040035337,12.9482677220772,
128.594669933562)) ;
#151538 = CARTESIAN_POINT('Ctrl Pts',(-24.9612989083473,13.2238578222556,
128.512263188183)) ;
#151539 = CARTESIAN_POINT('Ctrl Pts',(-24.9464400414306,13.5162932448957,
128.502169911524)) ;
#151540 = CARTESIAN_POINT('Ctrl Pts',(-24.9567559801261,13.799165239793,128.565264390033)) ;
#151541 = CARTESIAN_POINT('Ctrl Pts',(-24.9910303138475,14.0580267764743,
128.698731518742)) ;
#151542 = CARTESIAN_POINT('Ctrl Pts',(-25.0453888541943,14.2686028129511,
128.890481281382)) ;
#151543 = CARTESIAN_POINT('Ctrl Pts',(-25.1157749327763,14.4199618502008,
129.129219228183)) ;
#151544 = CARTESIAN_POINT('Ctrl Pts',(-25.1962537469819,14.4998958219189,
129.397417258709)) ;
#151545 = CARTESIAN_POINT('Ctrl Pts',(-25.2806998076144,14.5025664794371,
129.677347381576)) ;
#151546 = CARTESIAN_POINT('Ctrl Pts',(-25.3614130293349,14.4280652825415,
129.946141834169)) ;
#151547 = CARTESIAN_POINT('Ctrl Pts',(-25.4327613411336,14.2819177513075,
130.187667258866)) ;
#151548 = CARTESIAN_POINT('Ctrl Pts',(-25.4888836010397,14.0723877227319,
130.384948804485)) ;
#151549 = CARTESIAN_POINT('Ctrl Pts',(-25.524217369076,13.8191595273478,130.52109290564)) ;
#151550 = CARTESIAN_POINT('Ctrl Pts',(-25.5363621720147,13.5356702848312,
130.589764696207)) ;
#151551 = CARTESIAN_POINT('Ctrl Pts',(-25.5233799731752,13.2451626614465,
130.584896539849)) ;
#151552 = CARTESIAN_POINT('Ctrl Pts',(-25.4853193673611,12.9658959397094,
130.506957297054)) ;
#151553 = CARTESIAN_POINT('Ctrl Pts',(-25.4245567948317,12.720867949973,130.362513148524)) ;
#151554 = CARTESIAN_POINT('Ctrl Pts',(-25.3444357384131,12.5256178596935,
130.161588938401)) ;
#151555 = CARTESIAN_POINT('Ctrl Pts',(-25.2502354927177,12.3947249390078,
129.91946984754)) ;
#151556 = CARTESIAN_POINT('Ctrl Pts',(-25.1471557384846,12.3373274128747,
129.651622343389)) ;
#151557 = CARTESIAN_POINT('Ctrl Pts',(-25.04352722843,12.3577351376061,129.3818280718)) ;
#151558 = CARTESIAN_POINT('Ctrl Pts',(-24.9440625937448,12.4546492514378,
129.124509048456)) ;
#151559 = CARTESIAN_POINT('Ctrl Pts',(-24.8564471604785,12.6210676591383,
128.901700870073)) ;
#151560 = CARTESIAN_POINT('Ctrl Pts',(-24.7859855036776,12.8446766854148,
128.728972290107)) ;
#151561 = CARTESIAN_POINT('Ctrl Pts',(-24.7369148940067,13.108808163257,128.618635013836)) ;
#151562 = CARTESIAN_POINT('Ctrl Pts',(-24.7117898455147,13.3979062620311,
128.578541432007)) ;
#151563 = CARTESIAN_POINT('Ctrl Pts',(-24.7120774707783,13.6859097607706,
128.612344349061)) ;
#151564 = CARTESIAN_POINT('Ctrl Pts',(-24.7366917620368,13.9567565280856,
128.717390290963)) ;
#151565 = CARTESIAN_POINT('Ctrl Pts',(-24.7836759760245,14.1899349125241,
128.887914867791)) ;
#151566 = CARTESIAN_POINT('Ctrl Pts',(-24.8478937377255,14.3662692626876,
129.10842421568)) ;
#151567 = CARTESIAN_POINT('Ctrl Pts',(-24.9254379812952,14.4768289979695,
129.368240618362)) ;
#151568 = CARTESIAN_POINT('Ctrl Pts',(-25.0089189154175,14.5109207090365,
129.645218161262)) ;
#151569 = CARTESIAN_POINT('Ctrl Pts',(-25.0919501200887,14.4673589954117,
129.920875758852)) ;
#151570 = CARTESIAN_POINT('Ctrl Pts',(-25.1679324131496,14.3490298117359,
130.175949093355)) ;
#151571 = CARTESIAN_POINT('Ctrl Pts',(-25.2306776791176,14.1643442573792,
130.392364551844)) ;
#151572 = CARTESIAN_POINT('Ctrl Pts',(-25.2749172208417,13.9269540764464,
130.554674425406)) ;
#151573 = CARTESIAN_POINT('Ctrl Pts',(-25.296881801977,13.6529087066834,130.651991768824)) ;
#151574 = CARTESIAN_POINT('Ctrl Pts',(-25.294121582554,13.3625040426011,130.677064089887)) ;
#151575 = CARTESIAN_POINT('Ctrl Pts',(-25.2661584777254,13.0764917625792,
130.628507586136)) ;
#151576 = CARTESIAN_POINT('Ctrl Pts',(-25.2142358128611,12.8152457852602,
130.509968872735)) ;
#151577 = CARTESIAN_POINT('Ctrl Pts',(-25.1414105163864,12.5977360848388,
130.330346617025)) ;
#151578 = CARTESIAN_POINT('Ctrl Pts',(-25.0521369052221,12.4392301767845,
130.102679861577)) ;
#151579 = CARTESIAN_POINT('Ctrl Pts',(-24.9519825847367,12.3513755992719,
129.843259987167)) ;
#151580 = CARTESIAN_POINT('Ctrl Pts',(-24.8480528333298,12.3399316332142,
129.572627714051)) ;
#151581 = CARTESIAN_POINT('Ctrl Pts',(-24.7452323261505,12.4070554351268,
129.305672373312)) ;
#151582 = CARTESIAN_POINT('Ctrl Pts',(-24.653114699296,12.5451369869361,129.069390792946)) ;
#151583 = CARTESIAN_POINT('Ctrl Pts',(-24.574658401759,12.7477726868892,128.873467031278)) ;
#151584 = CARTESIAN_POINT('Ctrl Pts',(-24.516485448288,12.9979367372735,128.736605448719)) ;
#151585 = CARTESIAN_POINT('Ctrl Pts',(-24.4813744014041,13.2792370978739,
128.667217092649)) ;
#151586 = CARTESIAN_POINT('Ctrl Pts',(-24.4713970354524,13.5701580555343,
128.671163049425)) ;
#151587 = CARTESIAN_POINT('Ctrl Pts',(-24.4863380916386,13.8505377724051,
128.747899411962)) ;
#151588 = CARTESIAN_POINT('Ctrl Pts',(-24.5245439679385,14.1007512372239,
128.892655666103)) ;
#151589 = CARTESIAN_POINT('Ctrl Pts',(-24.5824402788279,14.3021715583994,
129.094893574169)) ;
#151590 = CARTESIAN_POINT('Ctrl Pts',(-24.6554257346924,14.4410638226486,
129.341309329826)) ;
#151591 = CARTESIAN_POINT('Ctrl Pts',(-24.7373356695316,14.506420576945,129.613776649341)) ;
#151592 = CARTESIAN_POINT('Ctrl Pts',(-24.8210078848283,14.4944296739133,
129.89116801343)) ;
#151593 = CARTESIAN_POINT('Ctrl Pts',(-24.9008406879447,14.4055611915821,
130.157574926146)) ;
#151594 = CARTESIAN_POINT('Ctrl Pts',(-24.9694636925505,14.2469875620131,
130.391056099313)) ;
#151595 = CARTESIAN_POINT('Ctrl Pts',(-25.0219599711088,14.0284942715184,
130.577615505577)) ;
#151596 = CARTESIAN_POINT('Ctrl Pts',(-25.053320022464,13.7670074742828,130.70234813533)) ;
#151597 = CARTESIAN_POINT('Ctrl Pts',(-25.0607089051815,13.4805781215048,
130.757097162265)) ;
#151598 = CARTESIAN_POINT('Ctrl Pts',(-25.0430061476845,13.1913388058783,
130.73838961606)) ;
#151599 = CARTESIAN_POINT('Ctrl Pts',(-25.0005234997867,12.9172330933754,
130.647473812606)) ;
#151600 = CARTESIAN_POINT('Ctrl Pts',(-24.9358367964898,12.6799728703758,
130.491596969194)) ;
#151601 = CARTESIAN_POINT('Ctrl Pts',(-24.8520526958292,12.4949910418975,
130.280173035867)) ;
#151602 = CARTESIAN_POINT('Ctrl Pts',(-24.756283433586,12.3781840447206,130.033296564361)) ;
#151603 = CARTESIAN_POINT('Ctrl Pts',(-24.6522083130104,12.3352411023339,
129.762603753164)) ;
#151604 = CARTESIAN_POINT('Ctrl Pts',(-24.5492013359519,12.3701183957634,
129.494563600041)) ;
#151605 = CARTESIAN_POINT('Ctrl Pts',(-24.4510228781676,12.4815908370187,
129.241159666924)) ;
#151606 = CARTESIAN_POINT('Ctrl Pts',(-24.3668186999168,12.6586744463426,
129.02808228214)) ;
#151607 = CARTESIAN_POINT('Ctrl Pts',(-24.2996856218142,12.8927064505131,
128.86527445598)) ;
#151608 = CARTESIAN_POINT('Ctrl Pts',(-24.2552426505653,13.1615895986342,
128.768318934161)) ;
#151609 = CARTESIAN_POINT('Ctrl Pts',(-24.2347791741716,13.4527337961883,
128.741859841865)) ;
#151610 = CARTESIAN_POINT('Ctrl Pts',(-24.2398184692911,13.7397606263225,
128.789657130047)) ;
#151611 = CARTESIAN_POINT('Ctrl Pts',(-24.2689320023009,14.0044956878458,
128.907831044878)) ;
#151612 = CARTESIAN_POINT('Ctrl Pts',(-24.3192589693072,14.2270717047825,
129.087893938316)) ;
#151613 = CARTESIAN_POINT('Ctrl Pts',(-24.386637598686,14.3928428531141,129.31784383242)) ;
#151614 = CARTESIAN_POINT('Ctrl Pts',(-24.4659391407555,14.4891679896536,
129.582798342604)) ;
#151615 = CARTESIAN_POINT('Ctrl Pts',(-24.5493645856168,14.5086708936273,
129.859423076708)) ;
#151616 = CARTESIAN_POINT('Ctrl Pts',(-24.6318807172738,14.4507091204102,
130.133696348165)) ;
#151617 = CARTESIAN_POINT('Ctrl Pts',(-24.7058567597393,14.318823465338,130.382937634357)) ;
#151618 = CARTESIAN_POINT('Ctrl Pts',(-24.7654056750014,14.1234067424229,
130.589957999186)) ;
#151619 = CARTESIAN_POINT('Ctrl Pts',(-24.8057595992627,13.8772496577341,
130.740994985991)) ;
#151620 = CARTESIAN_POINT('Ctrl Pts',(-24.8231799857801,13.5994498547175,
130.82492878504)) ;
#151621 = CARTESIAN_POINT('Ctrl Pts',(-24.8155893045152,13.3067289539218,
130.836068714423)) ;
#151622 = CARTESIAN_POINT('Ctrl Pts',(-24.7830973206933,13.025513208076,130.774091996489)) ;
#151623 = CARTESIAN_POINT('Ctrl Pts',(-24.7270577046474,12.7708776887036,
130.643534343482)) ;
#151624 = CARTESIAN_POINT('Ctrl Pts',(-24.6505077984341,12.5628412979246,
130.453131427416)) ;
#151625 = CARTESIAN_POINT('Ctrl Pts',(-24.5589760348122,12.4171764122364,
130.218786009453)) ;
#151626 = CARTESIAN_POINT('Ctrl Pts',(-24.4570551071365,12.3431378359771,
129.954350410602)) ;
#151627 = CARTESIAN_POINT('Ctrl Pts',(-24.3533214115063,12.3467434972734,
129.684210676246)) ;
#151628 = CARTESIAN_POINT('Ctrl Pts',(-24.2523283182393,12.4272274658185,
129.422376802438)) ;
#151629 = CARTESIAN_POINT('Ctrl Pts',(-24.1617932807192,12.5790158149027,
129.190994958755)) ;
#151630 = CARTESIAN_POINT('Ctrl Pts',(-24.0869579392724,12.7916687829571,
129.005564094205)) ;
#151631 = CARTESIAN_POINT('Ctrl Pts',(-24.0328055760906,13.0498138992039,
128.8805514449)) ;
#151632 = CARTESIAN_POINT('Ctrl Pts',(-24.002521804032,13.3331756720239,128.825089124936)) ;
#151633 = CARTESIAN_POINT('Ctrl Pts',(-23.9971725769105,13.6238935345468,
128.842575947387)) ;
#151634 = CARTESIAN_POINT('Ctrl Pts',(-24.0167753636582,13.9010885274901,
128.933062863381)) ;
#151635 = CARTESIAN_POINT('Ctrl Pts',(-24.0590128945408,14.1432054793993,
129.089568959686)) ;
#151636 = CARTESIAN_POINT('Ctrl Pts',(-24.1203695555296,14.3341070280144,
129.302019247719)) ;
#151637 = CARTESIAN_POINT('Ctrl Pts',(-24.1950418049019,14.4587991787124,
129.553138711427)) ;
#151638 = CARTESIAN_POINT('Ctrl Pts',(-24.2777268658875,14.5101605081857,
129.827811432152)) ;
#151639 = CARTESIAN_POINT('Ctrl Pts',(-24.3615395865942,14.4834097576633,
130.105796352381)) ;
#151640 = CARTESIAN_POINT('Ctrl Pts',(-24.4396001237497,14.380986704451,130.366925214371)) ;
#151641 = CARTESIAN_POINT('Ctrl Pts',(-24.5059188478657,14.2089571607828,
130.593906733665)) ;
#151642 = CARTESIAN_POINT('Ctrl Pts',(-24.5543423873352,13.9828180453883,
130.768283768123)) ;
#151643 = CARTESIAN_POINT('Ctrl Pts',(-24.5815804292821,13.7132629209954,
130.881224790375)) ;
#151644 = CARTESIAN_POINT('Ctrl Pts',(-24.5841620980753,13.42583764063,130.921759059005)) ;
#151645 = CARTESIAN_POINT('Ctrl Pts',(-24.5616991302751,13.1374631065902,
130.889232264708)) ;
#151646 = CARTESIAN_POINT('Ctrl Pts',(-24.5148271925072,12.8691197006536,
130.785439835784)) ;
#151647 = CARTESIAN_POINT('Ctrl Pts',(-24.4460595852779,12.6403113443668,
130.617737495797)) ;
#151648 = CARTESIAN_POINT('Ctrl Pts',(-24.3602783070861,12.468420702256,130.400139902644)) ;
#151649 = CARTESIAN_POINT('Ctrl Pts',(-24.2614984282295,12.3638000217504,
130.144889114756)) ;
#151650 = CARTESIAN_POINT('Ctrl Pts',(-24.1577920148866,12.3359859144704,
129.874955907544)) ;
#151651 = CARTESIAN_POINT('Ctrl Pts',(-24.054756872384,12.3855342690204,129.607074345636)) ;
#151652 = CARTESIAN_POINT('Ctrl Pts',(-23.9592387590454,12.5097023136888,
129.361184743235)) ;
#151653 = CARTESIAN_POINT('Ctrl Pts',(-23.8775758716564,12.6987169895182,
129.155691106511)) ;
#151654 = CARTESIAN_POINT('Ctrl Pts',(-23.8143557456443,12.9413958856346,
129.004310292951)) ;
#151655 = CARTESIAN_POINT('Ctrl Pts',(-23.7742609530853,13.2164083911014,
128.920187229679)) ;
#151656 = CARTESIAN_POINT('Ctrl Pts',(-23.7587189631835,13.5077476116907,
128.907983756604)) ;
#151657 = CARTESIAN_POINT('Ctrl Pts',(-23.7683966260473,13.7917084995172,
128.969294505237)) ;
#151658 = CARTESIAN_POINT('Ctrl Pts',(-23.8017090745378,14.0497089633418,
129.099691778832)) ;
#151659 = CARTESIAN_POINT('Ctrl Pts',(-23.855687851068,14.2632250030891,129.290500820459)) ;
#151660 = CARTESIAN_POINT('Ctrl Pts',(-23.9259445764529,14.4168537708596,
129.528960264585)) ;
#151661 = CARTESIAN_POINT('Ctrl Pts',(-24.0063154571533,14.4987598986465,
129.796873298139)) ;
#151662 = CARTESIAN_POINT('Ctrl Pts',(-24.0905209887515,14.5035045718472,
130.07601230486)) ;
#151663 = CARTESIAN_POINT('Ctrl Pts',(-24.1714640122117,14.4313229997249,
130.345485263966)) ;
#151664 = CARTESIAN_POINT('Ctrl Pts',(-24.243380136318,14.286096674379,130.588809864043)) ;
#151665 = CARTESIAN_POINT('Ctrl Pts',(-24.2994203289572,14.0806888556304,
130.785462444038)) ;
#151666 = CARTESIAN_POINT('Ctrl Pts',(-24.3358061636431,13.8265805447723,
130.924971011733)) ;
#151667 = CARTESIAN_POINT('Ctrl Pts',(-24.3485662665821,13.5441879409374,
130.995358908411)) ;
#151668 = CARTESIAN_POINT('Ctrl Pts',(-24.3362787692544,13.2530370689606,
130.992594119063)) ;
#151669 = CARTESIAN_POINT('Ctrl Pts',(-24.2990565233592,12.9741114175935,
130.916980614884)) ;
#151670 = CARTESIAN_POINT('Ctrl Pts',(-24.2387980421576,12.7272119216586,
130.774093243821)) ;
#151671 = CARTESIAN_POINT('Ctrl Pts',(-24.1592542721153,12.5305677659782,
130.57481255156)) ;
#151672 = CARTESIAN_POINT('Ctrl Pts',(-24.0653992661587,12.3976028767503,
130.333704016612)) ;
#151673 = CARTESIAN_POINT('Ctrl Pts',(-23.9625403093089,12.3378877564715,
130.06647786499)) ;
#151674 = CARTESIAN_POINT('Ctrl Pts',(-23.8586656317476,12.3561146457162,
129.796030313594)) ;
#151675 = CARTESIAN_POINT('Ctrl Pts',(-23.7592617382335,12.4504996091204,
129.538781451731)) ;
#151676 = CARTESIAN_POINT('Ctrl Pts',(-23.6710781493093,12.6151918179393,
129.314368558311)) ;
#151677 = CARTESIAN_POINT('Ctrl Pts',(-23.6000847768971,12.8367627956422,
129.140023816127)) ;
#151678 = CARTESIAN_POINT('Ctrl Pts',(-23.5500037307086,13.102471284239,129.027040548326)) ;
#151679 = CARTESIAN_POINT('Ctrl Pts',(-23.5244629176484,13.388098474674,128.985365037134)) ;
#151680 = CARTESIAN_POINT('Ctrl Pts',(-23.5239179211507,13.6786302634614,
129.017000214703)) ;
#151681 = CARTESIAN_POINT('Ctrl Pts',(-23.5479482075075,13.9495118019851,
129.120261172471)) ;
#151682 = CARTESIAN_POINT('Ctrl Pts',(-23.5940539896427,14.1831630717315,
129.28807205042)) ;
#151683 = CARTESIAN_POINT('Ctrl Pts',(-23.658087369295,14.3622887251467,129.508197418047)) ;
#151684 = CARTESIAN_POINT('Ctrl Pts',(-23.7354964858561,14.4748192529362,
129.767663246934)) ;
#151685 = CARTESIAN_POINT('Ctrl Pts',(-23.8186008712506,14.5109473630978,
130.043427649505)) ;
#151686 = CARTESIAN_POINT('Ctrl Pts',(-23.9016485189198,14.46989386631,130.319093678178)) ;
#151687 = CARTESIAN_POINT('Ctrl Pts',(-23.9780326629865,14.3536144736526,
130.57538079303)) ;
#151688 = CARTESIAN_POINT('Ctrl Pts',(-24.041317392537,14.17062113719,130.793395793898)) ;
#151689 = CARTESIAN_POINT('Ctrl Pts',(-24.0862233608817,13.933736573907,130.957750623604)) ;
#151690 = CARTESIAN_POINT('Ctrl Pts',(-24.1087782693582,13.6617104442443,
131.056639640472)) ;
#151691 = CARTESIAN_POINT('Ctrl Pts',(-24.1067652069901,13.3701432171844,
131.084050982405)) ;
#151692 = CARTESIAN_POINT('Ctrl Pts',(-24.0794150200347,13.0839501475181,
131.037263800254)) ;
#151693 = CARTESIAN_POINT('Ctrl Pts',(-24.0283415442683,12.8226369063403,
130.921088721576)) ;
#151694 = CARTESIAN_POINT('Ctrl Pts',(-23.9561135287856,12.6036153158418,
130.74320474868)) ;
#151695 = CARTESIAN_POINT('Ctrl Pts',(-23.8674374985634,12.4432239429731,
130.517228131168)) ;
#151696 = CARTESIAN_POINT('Ctrl Pts',(-23.7669177824065,12.3525997513282,
130.256937329486)) ;
#151697 = CARTESIAN_POINT('Ctrl Pts',(-23.6631589097691,12.3393903655815,
129.986759745082)) ;
#151698 = CARTESIAN_POINT('Ctrl Pts',(-23.5608451726887,12.403468098602,129.721057322036)) ;
#151699 = CARTESIAN_POINT('Ctrl Pts',(-23.4675538333872,12.5405072085783,
129.481626938511)) ;
#151700 = CARTESIAN_POINT('Ctrl Pts',(-23.388662980097,12.7420005519616,129.284449551793)) ;
#151701 = CARTESIAN_POINT('Ctrl Pts',(-23.3301053404809,12.9900801149227,
129.146339662681)) ;
#151702 = CARTESIAN_POINT('Ctrl Pts',(-23.2942598700259,13.2708158721555,
129.07481369419)) ;
#151703 = CARTESIAN_POINT('Ctrl Pts',(-23.2835507653219,13.5613604134334,
129.07658052044)) ;
#151704 = CARTESIAN_POINT('Ctrl Pts',(-23.2977457009926,13.8428560081929,
129.151189048699)) ;
#151705 = CARTESIAN_POINT('Ctrl Pts',(-23.3355877732922,14.0951246502648,
129.295029201952)) ;
#151706 = CARTESIAN_POINT('Ctrl Pts',(-23.392640021767,14.2968154125605,129.494589775277)) ;
#151707 = CARTESIAN_POINT('Ctrl Pts',(-23.4654695271126,14.4382062812648,
129.740653917803)) ;
#151708 = CARTESIAN_POINT('Ctrl Pts',(-23.5470349400498,14.5055713938207,
130.012034404642)) ;
#151709 = CARTESIAN_POINT('Ctrl Pts',(-23.6308595315768,14.4957941932041,
130.289927886282)) ;
#151710 = CARTESIAN_POINT('Ctrl Pts',(-23.7106798599952,14.4095662340998,
130.556186374908)) ;
#151711 = CARTESIAN_POINT('Ctrl Pts',(-23.7802571461447,14.2515335127425,
130.792730605287)) ;
#151712 = CARTESIAN_POINT('Ctrl Pts',(-23.8330271584667,14.0347236874785,
130.979999898394)) ;
#151713 = CARTESIAN_POINT('Ctrl Pts',(-23.8649144470802,13.7751700114088,
131.106159195577)) ;
#151714 = CARTESIAN_POINT('Ctrl Pts',(-23.8730939748177,13.489555102194,131.163174955555)) ;
#151715 = CARTESIAN_POINT('Ctrl Pts',(-23.8560200827014,13.1989624545804,
131.146444379055)) ;
#151716 = CARTESIAN_POINT('Ctrl Pts',(-23.8142948031392,12.9245155762064,
131.057679563774)) ;
#151717 = CARTESIAN_POINT('Ctrl Pts',(-23.7497390288408,12.6850932088169,
130.90236186876)) ;
#151718 = CARTESIAN_POINT('Ctrl Pts',(-23.6676401734867,12.5007200500438,
130.695387264516)) ;
#151719 = CARTESIAN_POINT('Ctrl Pts',(-23.5710799792398,12.3802348015134,
130.446601105623)) ;
#151720 = CARTESIAN_POINT('Ctrl Pts',(-23.4680387193144,12.3354177830535,
130.178616720221)) ;
#151721 = CARTESIAN_POINT('Ctrl Pts',(-23.3639870057212,12.3682931650198,
129.907845197495)) ;
#151722 = CARTESIAN_POINT('Ctrl Pts',(-23.2665557781875,12.4764500222757,
129.656260795804)) ;
#151723 = CARTESIAN_POINT('Ctrl Pts',(-23.1812074615382,12.6527561756398,
129.440099421206)) ;
#151724 = CARTESIAN_POINT('Ctrl Pts',(-23.1137789148354,12.8841372675975,
129.276247072773)) ;
#151725 = CARTESIAN_POINT('Ctrl Pts',(-23.0682028417558,13.1550291136418,
129.176337392218)) ;
#151726 = CARTESIAN_POINT('Ctrl Pts',(-23.0472767378411,13.4437302360126,
129.148261982065)) ;
#151727 = CARTESIAN_POINT('Ctrl Pts',(-23.0515496084932,13.7319393007276,
129.193922359653)) ;
#151728 = CARTESIAN_POINT('Ctrl Pts',(-23.079878251099,13.9965481623833,129.309665379139)) ;
#151729 = CARTESIAN_POINT('Ctrl Pts',(-23.129741526764,14.2215298170475,129.488488454029)) ;
#151730 = CARTESIAN_POINT('Ctrl Pts',(-23.1968818888558,14.3891483272759,
129.717799600751)) ;
#151731 = CARTESIAN_POINT('Ctrl Pts',(-23.2754021964238,14.4871687024338,
129.980255089599)) ;
#151732 = CARTESIAN_POINT('Ctrl Pts',(-23.3593328759968,14.5093408079897,
130.258577404978)) ;
#151733 = CARTESIAN_POINT('Ctrl Pts',(-23.4420335332337,14.4530254583256,
130.533420307647)) ;
#151734 = CARTESIAN_POINT('Ctrl Pts',(-23.5159486858221,14.3240305585518,
130.782295669503)) ;
#151735 = CARTESIAN_POINT('Ctrl Pts',(-23.5763068870408,14.1290979717854,
130.991878121919)) ;
#151736 = CARTESIAN_POINT('Ctrl Pts',(-23.617068843589,13.8855604155571,131.143910620301)) ;
#151737 = CARTESIAN_POINT('Ctrl Pts',(-23.6352727286933,13.6058416707122,
131.230442968303)) ;
#151738 = CARTESIAN_POINT('Ctrl Pts',(-23.6283964341607,13.3160021377259,
131.243341112372)) ;
#151739 = CARTESIAN_POINT('Ctrl Pts',(-23.5965464340223,13.0326886676077,
131.183420690455)) ;
#151740 = CARTESIAN_POINT('Ctrl Pts',(-23.5408985622457,12.7766372190837,
131.054072194123)) ;
#151741 = CARTESIAN_POINT('Ctrl Pts',(-23.4649595861684,12.5676698161814,
130.865387166735)) ;
#151742 = CARTESIAN_POINT('Ctrl Pts',(-23.3740967453034,12.4206517790888,
130.632884178497)) ;
#151743 = CARTESIAN_POINT('Ctrl Pts',(-23.2727082372118,12.3443150505119,
130.369901024895)) ;
#151744 = CARTESIAN_POINT('Ctrl Pts',(-23.1684546893583,12.3454567433165,
130.098404386445)) ;
#151745 = CARTESIAN_POINT('Ctrl Pts',(-23.0671327036379,12.4241540146565,
129.835658717647)) ;
#151746 = CARTESIAN_POINT('Ctrl Pts',(-22.9764947583752,12.5736454649868,
129.60388157098)) ;
#151747 = CARTESIAN_POINT('Ctrl Pts',(-22.9011806814661,12.7844244258342,
129.417017819213)) ;
#151748 = CARTESIAN_POINT('Ctrl Pts',(-22.8463459628872,13.041264478038,129.289992771218)) ;
#151749 = CARTESIAN_POINT('Ctrl Pts',(-22.815230919969,13.3250313838274,129.232207692813)) ;
#151750 = CARTESIAN_POINT('Ctrl Pts',(-22.8092125202162,13.6156492492809,
129.247717690027)) ;
#151751 = CARTESIAN_POINT('Ctrl Pts',(-22.8280212526032,13.8929002803611,
129.335801002832)) ;
#151752 = CARTESIAN_POINT('Ctrl Pts',(-22.8696833153775,14.1366366428793,
129.490673844657)) ;
#151753 = CARTESIAN_POINT('Ctrl Pts',(-22.9303059421642,14.3287833833703,
129.70086742119)) ;
#151754 = CARTESIAN_POINT('Ctrl Pts',(-23.0049559964505,14.4563288342089,
129.952070625789)) ;
#151755 = CARTESIAN_POINT('Ctrl Pts',(-23.0876811988293,14.5097636463918,
130.226920951019)) ;
#151756 = CARTESIAN_POINT('Ctrl Pts',(-23.171313625943,14.4852491819093,130.504285160366)) ;
#151757 = CARTESIAN_POINT('Ctrl Pts',(-23.2495616828516,14.385213180382,130.765927789329)) ;
#151758 = CARTESIAN_POINT('Ctrl Pts',(-23.3164467304666,14.2148994362801,
130.994611083723)) ;
#151759 = CARTESIAN_POINT('Ctrl Pts',(-23.3654737459425,13.9895605141043,
131.170821580244)) ;
#151760 = CARTESIAN_POINT('Ctrl Pts',(-23.3932709418014,13.7226496289756,
131.285186238845)) ;
#151761 = CARTESIAN_POINT('Ctrl Pts',(-23.3966715321499,13.4342098859693,
131.328274909581)) ;
#151762 = CARTESIAN_POINT('Ctrl Pts',(-23.3749521692447,13.1458182759752,
131.297881508113)) ;
#151763 = CARTESIAN_POINT('Ctrl Pts',(-23.3285769346008,12.8759127132536,
131.195640591877)) ;
#151764 = CARTESIAN_POINT('Ctrl Pts',(-23.2608087751802,12.6468868556867,
131.030665242811)) ;
#151765 = CARTESIAN_POINT('Ctrl Pts',(-23.1749384545703,12.4721832296684,
130.81301511834)) ;
#151766 = CARTESIAN_POINT('Ctrl Pts',(-23.0772501521557,12.3661739274481,
130.560671910315)) ;
#151767 = CARTESIAN_POINT('Ctrl Pts',(-22.972758046801,12.3355863385396,130.288726503058)) ;
#151768 = CARTESIAN_POINT('Ctrl Pts',(-22.8698300820149,12.3831198658751,
130.021082533712)) ;
#151769 = CARTESIAN_POINT('Ctrl Pts',(-22.7739061268904,12.5053833023315,
129.774046335208)) ;
#151770 = CARTESIAN_POINT('Ctrl Pts',(-22.6919791045737,12.6923270702948,
129.567704270438)) ;
#151771 = CARTESIAN_POINT('Ctrl Pts',(-22.6281112723494,12.9335865705139,
129.414426275698)) ;
#151772 = CARTESIAN_POINT('Ctrl Pts',(-22.5872544610613,13.2085814539572,
129.328158922446)) ;
#151773 = CARTESIAN_POINT('Ctrl Pts',(-22.5710404902249,13.4990557588074,
129.313907984072)) ;
#151774 = CARTESIAN_POINT('Ctrl Pts',(-22.5799753665134,13.7836907462661,
129.373072556554)) ;
#151775 = CARTESIAN_POINT('Ctrl Pts',(-22.612638583778,14.0427281414566,129.501571243045)) ;
#151776 = CARTESIAN_POINT('Ctrl Pts',(-22.6660762367978,14.2577309750281,
129.69079806233)) ;
#151777 = CARTESIAN_POINT('Ctrl Pts',(-22.7357975374954,14.4131664617501,
129.927633756715)) ;
#151778 = CARTESIAN_POINT('Ctrl Pts',(-22.8161137666784,14.4973755702956,
130.195456113862)) ;
#151779 = CARTESIAN_POINT('Ctrl Pts',(-22.8998820017925,14.5046724130054,
130.47314586159)) ;
#151780 = CARTESIAN_POINT('Ctrl Pts',(-22.9816064513032,14.4343111747756,
130.745147804022)) ;
#151781 = CARTESIAN_POINT('Ctrl Pts',(-23.0536227051492,14.2913904033354,
130.98864811284)) ;
#151782 = CARTESIAN_POINT('Ctrl Pts',(-23.1102843211941,14.0872940403586,
131.187176359758)) ;
#151783 = CARTESIAN_POINT('Ctrl Pts',(-23.1472375329922,13.8349907742835,
131.328253449348)) ;
#151784 = CARTESIAN_POINT('Ctrl Pts',(-23.1607772342592,13.5522018199285,
131.401036362566)) ;
#151785 = CARTESIAN_POINT('Ctrl Pts',(-23.1491871925298,13.2611771320633,
131.400285897439)) ;
#151786 = CARTESIAN_POINT('Ctrl Pts',(-23.1125952006362,12.9814107201437,
131.326544774095)) ;
#151787 = CARTESIAN_POINT('Ctrl Pts',(-23.0531566614903,12.7341369610279,
131.185942865115)) ;
#151788 = CARTESIAN_POINT('Ctrl Pts',(-22.9739547949964,12.535166216503,130.98774443351)) ;
#151789 = CARTESIAN_POINT('Ctrl Pts',(-22.8800044204222,12.4000170891871,
130.746489022896)) ;
#151790 = CARTESIAN_POINT('Ctrl Pts',(-22.7777942394703,12.3385941106561,
130.480992016477)) ;
#151791 = CARTESIAN_POINT('Ctrl Pts',(-22.6737045237347,12.3545286685026,
130.209973410253)) ;
#151792 = CARTESIAN_POINT('Ctrl Pts',(-22.574018025731,12.4469846430608,129.951917332464)) ;
#151793 = CARTESIAN_POINT('Ctrl Pts',(-22.4853397321754,12.6102579412087,
129.726108518223)) ;
#151794 = CARTESIAN_POINT('Ctrl Pts',(-22.4141387274598,12.8296977311719,
129.551032278381)) ;
#151795 = CARTESIAN_POINT('Ctrl Pts',(-22.3635165048781,13.0929763552362,
129.436306120848)) ;
#151796 = CARTESIAN_POINT('Ctrl Pts',(-22.3370222640428,13.3798715107165,
129.392040554444)) ;
#151797 = CARTESIAN_POINT('Ctrl Pts',(-22.3358180956749,13.6705227535771,
129.421738962196)) ;
#151798 = CARTESIAN_POINT('Ctrl Pts',(-22.359121262081,13.9421700423004,129.522864634634)) ;
#151799 = CARTESIAN_POINT('Ctrl Pts',(-22.4048936915904,14.1780191011813,
129.689842088352)) ;
#151800 = CARTESIAN_POINT('Ctrl Pts',(-22.4683015911897,14.3579768124892,
129.908015928199)) ;
#151801 = CARTESIAN_POINT('Ctrl Pts',(-22.5452274463354,14.4725057553617,
130.165996866725)) ;
#151802 = CARTESIAN_POINT('Ctrl Pts',(-22.6283868280108,14.5110248787396,
130.441981808158)) ;
#151803 = CARTESIAN_POINT('Ctrl Pts',(-22.7115926468901,14.4721191969269,
130.718131866034)) ;
#151804 = CARTESIAN_POINT('Ctrl Pts',(-22.7882774144574,14.3577454336847,
130.975310558445)) ;
#151805 = CARTESIAN_POINT('Ctrl Pts',(-22.8518198048839,14.1770688666527,
131.193977525084)) ;
#151806 = CARTESIAN_POINT('Ctrl Pts',(-22.8974027115045,13.9416997327419,
131.360307596844)) ;
#151807 = CARTESIAN_POINT('Ctrl Pts',(-22.9206820190988,13.6694104353782,
131.461436266431)) ;
#151808 = CARTESIAN_POINT('Ctrl Pts',(-22.9194213574652,13.3798585935035,
131.490838835533)) ;
#151809 = CARTESIAN_POINT('Ctrl Pts',(-22.8929170330155,13.0927640382574,
131.446571141722)) ;
#151810 = CARTESIAN_POINT('Ctrl Pts',(-22.8423030043868,12.8294542733058,
131.331865445954)) ;
#151811 = CARTESIAN_POINT('Ctrl Pts',(-22.7706185679307,12.6090080043084,
131.155563913664)) ;
#151812 = CARTESIAN_POINT('Ctrl Pts',(-22.6821571255679,12.4466659582347,
130.930272433196)) ;
#151813 = CARTESIAN_POINT('Ctrl Pts',(-22.5824728331909,12.3544265354386,
130.672221564255)) ;
#151814 = CARTESIAN_POINT('Ctrl Pts',(-22.478522759517,12.338485550426,130.401560070963)) ;
#151815 = CARTESIAN_POINT('Ctrl Pts',(-22.3754966015088,12.4009576070215,
130.133958949611)) ;
#151816 = CARTESIAN_POINT('Ctrl Pts',(-22.2823680889779,12.5356622675021,
129.894847033385)) ;
#151817 = CARTESIAN_POINT('Ctrl Pts',(-22.2032360996956,12.7342792931547,
129.696815676907)) ;
#151818 = CARTESIAN_POINT('Ctrl Pts',(-22.1436939987442,12.9822470405306,
129.555989965758)) ;
#151819 = CARTESIAN_POINT('Ctrl Pts',(-22.1071406671597,13.2626104241267,
129.482419788097)) ;
#151820 = CARTESIAN_POINT('Ctrl Pts',(-22.0957144593787,13.5537330357078,
129.482159506806)) ;
#151821 = CARTESIAN_POINT('Ctrl Pts',(-22.1092685563454,13.8350780443648,
129.554823798795)) ;
#151822 = CARTESIAN_POINT('Ctrl Pts',(-22.1461475103679,14.0872562376869,
129.695659561939)) ;
#151823 = CARTESIAN_POINT('Ctrl Pts',(-22.2030821358645,14.2922552735091,
129.895131181954)) ;
#151824 = CARTESIAN_POINT('Ctrl Pts',(-22.2754289643042,14.4349645919609,
130.139699349458)) ;
#151825 = CARTESIAN_POINT('Ctrl Pts',(-22.3564708008619,14.5045540577175,
130.40942261917)) ;
#151826 = CARTESIAN_POINT('Ctrl Pts',(-22.4406441329642,14.4973581396257,
130.688457173911)) ;
#151827 = CARTESIAN_POINT('Ctrl Pts',(-22.5209414268602,14.4126016842873,
130.956235143864)) ;
#151828 = CARTESIAN_POINT('Ctrl Pts',(-22.5903401138937,14.2578370889756,
131.191978979017)) ;
#151829 = CARTESIAN_POINT('Ctrl Pts',(-22.643899231601,14.0423606370671,131.381638018117)) ;
#151830 = CARTESIAN_POINT('Ctrl Pts',(-22.676541227732,13.7833430848993,131.510062783894)) ;
#151831 = CARTESIAN_POINT('Ctrl Pts',(-22.6854014712124,13.4972454461382,
131.569174829683)) ;
#151832 = CARTESIAN_POINT('Ctrl Pts',(-22.6691263169549,13.2077137971034,
131.554634071507)) ;
#151833 = CARTESIAN_POINT('Ctrl Pts',(-22.6279874269016,12.9318531124,131.467669892297)) ;
#151834 = CARTESIAN_POINT('Ctrl Pts',(-22.5644211603477,12.6922552108513,
131.31506619976)) ;
#151835 = CARTESIAN_POINT('Ctrl Pts',(-22.4822337913331,12.504666487009,131.108074794862)) ;
#151836 = CARTESIAN_POINT('Ctrl Pts',(-22.3859455591042,12.3825157199122,
130.860070359518)) ;
#151837 = CARTESIAN_POINT('Ctrl Pts',(-22.283236535859,12.3357140444497,130.592990061673)) ;
#151838 = CARTESIAN_POINT('Ctrl Pts',(-22.1793293005588,12.3660679541908,
130.322564167356)) ;
#151839 = CARTESIAN_POINT('Ctrl Pts',(-22.0811143599576,12.4727573812884,
130.068868334442)) ;
#151840 = CARTESIAN_POINT('Ctrl Pts',(-21.995572717209,12.6471452986828,129.852067795218)) ;
#151841 = CARTESIAN_POINT('Ctrl Pts',(-21.9277324469771,12.8766362181276,
129.686942307119)) ;
#151842 = CARTESIAN_POINT('Ctrl Pts',(-21.88149427899,13.1457609561308,129.584999326918)) ;
#151843 = CARTESIAN_POINT('Ctrl Pts',(-21.8597035864534,13.436208516762,129.554631981768)) ;
#151844 = CARTESIAN_POINT('Ctrl Pts',(-21.8632848179525,13.7232902020091,
129.598101610311)) ;
#151845 = CARTESIAN_POINT('Ctrl Pts',(-21.8909607988816,13.9896012284326,
129.712029646671)) ;
#151846 = CARTESIAN_POINT('Ctrl Pts',(-21.9403194385609,14.2159296230216,
129.889382772798)) ;
#151847 = CARTESIAN_POINT('Ctrl Pts',(-22.0069084874016,14.3851342144556,
130.117025681466)) ;
#151848 = CARTESIAN_POINT('Ctrl Pts',(-22.0853055168022,14.4854516976048,
130.379173666988)) ;
#151849 = CARTESIAN_POINT('Ctrl Pts',(-22.1690106808166,14.5096986607512,
130.656773596937)) ;
#151850 = CARTESIAN_POINT('Ctrl Pts',(-22.2516547688815,14.4561737731647,
130.931357792915)) ;
#151851 = CARTESIAN_POINT('Ctrl Pts',(-22.3263675110369,14.3282785458503,
131.182786371531)) ;
#151852 = CARTESIAN_POINT('Ctrl Pts',(-22.3868479785871,14.1363003864466,
131.392508931439)) ;
#151853 = CARTESIAN_POINT('Ctrl Pts',(-22.4284860760948,13.8924839857025,
131.547317007501)) ;
#151854 = CARTESIAN_POINT('Ctrl Pts',(-22.44725520974,13.6154602436594,131.6352536123)) ;
#151855 = CARTESIAN_POINT('Ctrl Pts',(-22.4412045671012,13.3244466531158,
131.650714430567)) ;
#151856 = CARTESIAN_POINT('Ctrl Pts',(-22.4100202102661,13.0407282159145,
131.592726094803)) ;
#151857 = CARTESIAN_POINT('Ctrl Pts',(-22.3552546417009,12.7843965627726,
131.465846020052)) ;
#151858 = CARTESIAN_POINT('Ctrl Pts',(-22.2799328403175,12.5734338880589,
131.27897230653)) ;
#151859 = CARTESIAN_POINT('Ctrl Pts',(-22.1888584470267,12.4236459559127,
131.046058924602)) ;
#151860 = CARTESIAN_POINT('Ctrl Pts',(-22.0881362776665,12.3455712635568,
130.784862015627)) ;
#151861 = CARTESIAN_POINT('Ctrl Pts',(-21.9835492566618,12.3443023671055,
130.512500328341)) ;
#151862 = CARTESIAN_POINT('Ctrl Pts',(-21.8821100407858,12.420933178294,130.249388866071)) ;
#151863 = CARTESIAN_POINT('Ctrl Pts',(-21.7910702729597,12.5684896870098,
130.016446821888)) ;
#151864 = CARTESIAN_POINT('Ctrl Pts',(-21.7150620477299,12.7783872300958,
129.827643163685)) ;
#151865 = CARTESIAN_POINT('Ctrl Pts',(-21.6597355302853,13.0341435528073,
129.699158062916)) ;
#151866 = CARTESIAN_POINT('Ctrl Pts',(-21.6280379920894,13.3161552682329,
129.639527649233)) ;
#151867 = CARTESIAN_POINT('Ctrl Pts',(-21.6212166338096,13.6077102167408,
129.65278753406)) ;
#151868 = CARTESIAN_POINT('Ctrl Pts',(-21.6394813968357,13.8863966863271,
129.739379830896)) ;
#151869 = CARTESIAN_POINT('Ctrl Pts',(-21.6805482499846,14.1306963082603,
129.892451481926)) ;
#151870 = CARTESIAN_POINT('Ctrl Pts',(-21.7404897132441,14.3238933046915,
130.100547666824)) ;
#151871 = CARTESIAN_POINT('Ctrl Pts',(-21.8147710462659,14.4535137780173,
130.350663609957)) ;
#151872 = CARTESIAN_POINT('Ctrl Pts',(-21.8973774190617,14.5094099168095,
130.625175022534)) ;
#151873 = CARTESIAN_POINT('Ctrl Pts',(-21.9815416990517,14.4867701673882,
130.904282937535)) ;
#151874 = CARTESIAN_POINT('Ctrl Pts',(-22.0595736035611,14.3890643828725,
131.165115307558)) ;
#151875 = CARTESIAN_POINT('Ctrl Pts',(-22.1268562117523,14.2211869107964,
131.394908944864)) ;
#151876 = CARTESIAN_POINT('Ctrl Pts',(-22.1766796342833,13.9958858020985,
131.573633433779)) ;
#151877 = CARTESIAN_POINT('Ctrl Pts',(-22.2049451389284,13.7314793548645,
131.689162299244)) ;
#151878 = CARTESIAN_POINT('Ctrl Pts',(-22.2091882562906,13.4423639400344,
131.734833540967)) ;
#151879 = CARTESIAN_POINT('Ctrl Pts',(-22.187986226038,13.1530743203904,131.706032228928)) ;
#151880 = CARTESIAN_POINT('Ctrl Pts',(-22.1426951060036,12.8842566111771,
131.60670589681)) ;
#151881 = CARTESIAN_POINT('Ctrl Pts',(-22.0749780240027,12.6519995362001,
131.442148263088)) ;
#151882 = CARTESIAN_POINT('Ctrl Pts',(-21.9900041425516,12.4766942436469,
131.226917109559)) ;
#151883 = CARTESIAN_POINT('Ctrl Pts',(-21.8923871793902,12.3681120678918,
130.974864846892)) ;
#151884 = CARTESIAN_POINT('Ctrl Pts',(-21.787890239755,12.3353450096833,130.70292564467)) ;
#151885 = CARTESIAN_POINT('Ctrl Pts',(-21.6847703934588,12.3808789292608,
130.434751982444)) ;
#151886 = CARTESIAN_POINT('Ctrl Pts',(-21.5888638247786,12.5006496739186,
130.187651595634)) ;
#151887 = CARTESIAN_POINT('Ctrl Pts',(-21.5062882918341,12.6862348924807,
129.979488344586)) ;
#151888 = CARTESIAN_POINT('Ctrl Pts',(-21.4420352783819,12.9253055289241,
129.824962379676)) ;
#151889 = CARTESIAN_POINT('Ctrl Pts',(-21.4003702869002,13.1996774467986,
129.7363633676)) ;
#151890 = CARTESIAN_POINT('Ctrl Pts',(-21.3833560025974,13.4900583198245,
129.719780265193)) ;
#151891 = CARTESIAN_POINT('Ctrl Pts',(-21.3916055296796,13.7765694769724,
129.777104936438)) ;
#151892 = CARTESIAN_POINT('Ctrl Pts',(-21.4238225675142,14.036835662277,129.904358363752)) ;
#151893 = CARTESIAN_POINT('Ctrl Pts',(-21.4764867420294,14.2522894974628,
130.091167062838)) ;
#151894 = CARTESIAN_POINT('Ctrl Pts',(-21.5461349346789,14.410142650821,130.327932770345)) ;
#151895 = CARTESIAN_POINT('Ctrl Pts',(-21.6258533196047,14.4959011359271,
130.593837523055)) ;
#151896 = CARTESIAN_POINT('Ctrl Pts',(-21.7097706486653,14.5055615596735,
130.872034708298)) ;
#151897 = CARTESIAN_POINT('Ctrl Pts',(-21.7915115159255,14.4373879166647,
131.144023400965)) ;
#151898 = CARTESIAN_POINT('Ctrl Pts',(-21.8638380594977,14.2968056087925,
131.388393161352)) ;
#151899 = CARTESIAN_POINT('Ctrl Pts',(-21.9212551892473,14.0934340145334,
131.589268391717)) ;
#151900 = CARTESIAN_POINT('Ctrl Pts',(-21.9586969314941,13.8423638114029,
131.731737544598)) ;
#151901 = CARTESIAN_POINT('Ctrl Pts',(-21.9729463381941,13.5615577206812,
131.806433890657)) ;
#151902 = CARTESIAN_POINT('Ctrl Pts',(-21.9620894874447,13.2694348944804,
131.807950532534)) ;
#151903 = CARTESIAN_POINT('Ctrl Pts',(-21.9263140164209,12.9897647818979,
131.73650343455)) ;
#151904 = CARTESIAN_POINT('Ctrl Pts',(-21.8673223314263,12.7403852471457,
131.597325259585)) ;
#151905 = CARTESIAN_POINT('Ctrl Pts',(-21.7886865523693,12.5401778472151,
131.400734212814)) ;
#151906 = CARTESIAN_POINT('Ctrl Pts',(-21.6953778525397,12.4032538731495,
131.161259541037)) ;
#151907 = CARTESIAN_POINT('Ctrl Pts',(-21.5932072064287,12.3392654765734,
130.895922348931)) ;
#151908 = CARTESIAN_POINT('Ctrl Pts',(-21.4887973419696,12.3529795705707,
130.624055509138)) ;
#151909 = CARTESIAN_POINT('Ctrl Pts',(-21.3889895957889,12.44341496887,130.365620015526)) ;
#151910 = CARTESIAN_POINT('Ctrl Pts',(-21.3002278613015,12.6038142404483,
130.13942068693)) ;
#151911 = CARTESIAN_POINT('Ctrl Pts',(-21.2279512253468,12.8232746698558,
129.96143747852)) ;
#151912 = CARTESIAN_POINT('Ctrl Pts',(-21.1769064226059,13.0848674095602,
129.845368695489)) ;
#151913 = CARTESIAN_POINT('Ctrl Pts',(-21.149658170467,13.3712340427374,129.798893618011)) ;
#151914 = CARTESIAN_POINT('Ctrl Pts',(-21.1476946959762,13.6620670155129,
129.826365855313)) ;
#151915 = CARTESIAN_POINT('Ctrl Pts',(-21.1703666330339,13.9347879219274,
129.92569032549)) ;
#151916 = CARTESIAN_POINT('Ctrl Pts',(-21.2152993770454,14.1711547034761,
130.090075797328)) ;
#151917 = CARTESIAN_POINT('Ctrl Pts',(-21.2785796529392,14.3538985958079,
130.308060225528)) ;
#151918 = CARTESIAN_POINT('Ctrl Pts',(-21.3548663994536,14.4699515410886,
130.564015298951)) ;
#151919 = CARTESIAN_POINT('Ctrl Pts',(-21.4380889896721,14.511011729743,130.840261217569)) ;
#151920 = CARTESIAN_POINT('Ctrl Pts',(-21.5213196238039,14.4745400421894,
131.116445883889)) ;
#151921 = CARTESIAN_POINT('Ctrl Pts',(-21.5987228795245,14.3614974996119,
131.37591886424)) ;
#151922 = CARTESIAN_POINT('Ctrl Pts',(-21.6624280158677,14.1829580277845,
131.594943503888)) ;
#151923 = CARTESIAN_POINT('Ctrl Pts',(-21.7085901232024,13.9492404929465,
131.762934960253)) ;
#151924 = CARTESIAN_POINT('Ctrl Pts',(-21.7325457579653,13.6775800982586,
131.866060493852)) ;
#151925 = CARTESIAN_POINT('Ctrl Pts',(-21.7320824211323,13.3886494635436,
131.897743516193)) ;
#151926 = CARTESIAN_POINT('Ctrl Pts',(-21.7060357693068,13.0993478015478,
131.855033735375)) ;
#151927 = CARTESIAN_POINT('Ctrl Pts',(-21.6563720516456,12.8369458310676,
131.74287352401)) ;
#151928 = CARTESIAN_POINT('Ctrl Pts',(-21.5849505607058,12.6140529768099,
131.567486815159)) ;
#151929 = CARTESIAN_POINT('Ctrl Pts',(-21.4972346922135,12.4507323341902,
131.344230579028)) ;
#151930 = CARTESIAN_POINT('Ctrl Pts',(-21.3977816403119,12.3558899306528,
131.086868664739)) ;
#151931 = CARTESIAN_POINT('Ctrl Pts',(-21.2931236526698,12.3380969081111,
130.814378116707)) ;
#151932 = CARTESIAN_POINT('Ctrl Pts',(-21.1912351475806,12.3976016694818,
130.549680132567)) ;
#151933 = CARTESIAN_POINT('Ctrl Pts',(-21.0970918464179,12.530583824708,130.307814407326)) ;
#151934 = CARTESIAN_POINT('Ctrl Pts',(-21.0173249384038,12.7283490506027,
130.108013541003)) ;
#151935 = CARTESIAN_POINT('Ctrl Pts',(-20.9573893511929,12.9742771227128,
129.965922835233)) ;
#151936 = CARTESIAN_POINT('Ctrl Pts',(-20.9200880297606,13.2539376227601,
129.890167219948)) ;
#151937 = CARTESIAN_POINT('Ctrl Pts',(-20.907889243952,13.5450903335013,129.887655062896)) ;
#151938 = CARTESIAN_POINT('Ctrl Pts',(-20.920784302057,13.8275787514848,129.958467916581)) ;
#151939 = CARTESIAN_POINT('Ctrl Pts',(-20.9569782930972,14.080619519853,130.097260030665)) ;
#151940 = CARTESIAN_POINT('Ctrl Pts',(-21.0136849887986,14.2877392133105,
130.296196899106)) ;
#151941 = CARTESIAN_POINT('Ctrl Pts',(-21.0849841102122,14.431213841156,130.537392435781)) ;
#151942 = CARTESIAN_POINT('Ctrl Pts',(-21.1665056814218,14.5038738166411,
130.808799012005)) ;
#151943 = CARTESIAN_POINT('Ctrl Pts',(-21.2505166479721,14.4984557576167,
131.087288159437)) ;
#151944 = CARTESIAN_POINT('Ctrl Pts',(-21.3308085825838,14.4164646825051,
131.354946228948)) ;
#151945 = CARTESIAN_POINT('Ctrl Pts',(-21.4010755566249,14.2622140461571,
131.593482336718)) ;
#151946 = CARTESIAN_POINT('Ctrl Pts',(-21.4547420541191,14.0497489487789,
131.7832014722)) ;
#151947 = CARTESIAN_POINT('Ctrl Pts',(-21.4881853748102,13.7905258352839,
131.91413728601)) ;
#151948 = CARTESIAN_POINT('Ctrl Pts',(-21.4977462696728,13.506486494377,131.975100243164)) ;
#151949 = CARTESIAN_POINT('Ctrl Pts',(-21.4819835887124,13.2142515667239,
131.96236180773)) ;
#151950 = CARTESIAN_POINT('Ctrl Pts',(-21.4419223606185,12.9406232851689,
131.878185903014)) ;
#151951 = CARTESIAN_POINT('Ctrl Pts',(-21.3786934156362,12.6982138740687,
131.726763051586)) ;
#151952 = CARTESIAN_POINT('Ctrl Pts',(-21.2972126241658,12.5096112048297,
131.521723412285)) ;
#151953 = CARTESIAN_POINT('Ctrl Pts',(-21.2011850848722,12.3850648620669,
131.274514023005)) ;
#151954 = CARTESIAN_POINT('Ctrl Pts',(-21.0984907761846,12.3359713268051,
131.007507556083)) ;
#151955 = CARTESIAN_POINT('Ctrl Pts',(-20.9944877940312,12.3641515700291,
130.736812488399)) ;
#151956 = CARTESIAN_POINT('Ctrl Pts',(-20.8961804382662,12.4683944776065,
130.482779938443)) ;
#151957 = CARTESIAN_POINT('Ctrl Pts',(-20.8099546373725,12.6414744910879,
130.264081389746)) ;
#151958 = CARTESIAN_POINT('Ctrl Pts',(-20.7415876002801,12.8692739707259,
130.097372977444)) ;
#151959 = CARTESIAN_POINT('Ctrl Pts',(-20.6945289877427,13.1394382839076,
129.993253900407)) ;
#151960 = CARTESIAN_POINT('Ctrl Pts',(-20.672298328365,13.4257125423889,129.961149556797)) ;
#151961 = CARTESIAN_POINT('Ctrl Pts',(-20.6750007501078,13.7153678926771,
130.002310555712)) ;
#151962 = CARTESIAN_POINT('Ctrl Pts',(-20.7020667565521,13.9823826092166,
130.114434508231)) ;
#151963 = CARTESIAN_POINT('Ctrl Pts',(-20.7509060316579,14.210351268189,130.290309073817)) ;
#151964 = CARTESIAN_POINT('Ctrl Pts',(-20.8169604036749,14.3810373513132,
130.516327937223)) ;
#151965 = CARTESIAN_POINT('Ctrl Pts',(-20.8950665489886,14.4835203874639,
130.777619160747)) ;
#151966 = CARTESIAN_POINT('Ctrl Pts',(-20.9787343216663,14.5102051470099,
131.055116750985)) ;
#151967 = CARTESIAN_POINT('Ctrl Pts',(-21.0618484768981,14.4584272467564,
131.331220006128)) ;
#151968 = CARTESIAN_POINT('Ctrl Pts',(-21.1364526301434,14.3332271538461,
131.582140708526)) ;
#151969 = CARTESIAN_POINT('Ctrl Pts',(-21.1976622623504,14.1422679027751,
131.794126036847)) ;
#151970 = CARTESIAN_POINT('Ctrl Pts',(-21.23975721544,13.9003526545792,131.950166196499)) ;
#151971 = CARTESIAN_POINT('Ctrl Pts',(-21.2592791168289,13.6237176044633,
132.040346931511)) ;
#151972 = CARTESIAN_POINT('Ctrl Pts',(-21.2539545891703,13.3329588361478,
132.057910063551)) ;
#151973 = CARTESIAN_POINT('Ctrl Pts',(-21.2234510913761,13.0482791472687,
132.00196258976)) ;
#151974 = CARTESIAN_POINT('Ctrl Pts',(-21.1691539099102,12.7905984211716,
131.876506766355)) ;
#151975 = CARTESIAN_POINT('Ctrl Pts',(-21.0947340593749,12.5792074314873,
131.692098693563)) ;
#151976 = CARTESIAN_POINT('Ctrl Pts',(-21.0040480835755,12.4271420328258,
131.460337471105)) ;
#151977 = CARTESIAN_POINT('Ctrl Pts',(-20.9032486407606,12.3466854620337,
131.199002527252)) ;
#151978 = CARTESIAN_POINT('Ctrl Pts',(-20.7987770579087,12.3433384451733,
130.926945640301)) ;
#151979 = CARTESIAN_POINT('Ctrl Pts',(-20.6974847568586,12.417256873973,130.664144724903)) ;
#151980 = CARTESIAN_POINT('Ctrl Pts',(-20.6057021506296,12.5633304568432,
130.429162568903)) ;
#151981 = CARTESIAN_POINT('Ctrl Pts',(-20.5294560018403,12.7708593905581,
130.239538039818)) ;
#151982 = CARTESIAN_POINT('Ctrl Pts',(-20.4733463103174,13.025326349885,130.108769986711)) ;
#151983 = CARTESIAN_POINT('Ctrl Pts',(-20.4407772110818,13.3082178025067,
130.046756066484)) ;
#151984 = CARTESIAN_POINT('Ctrl Pts',(-20.4333100328866,13.5990344955289,
130.058039052296)) ;
#151985 = CARTESIAN_POINT('Ctrl Pts',(-20.4506880067864,13.8774216043795,
130.141913702905)) ;
#151986 = CARTESIAN_POINT('Ctrl Pts',(-20.4911818153333,14.1239848990119,
130.293425636597)) ;
#151987 = CARTESIAN_POINT('Ctrl Pts',(-20.5507855806424,14.3192776170792,
130.500609692184)) ;
#151988 = CARTESIAN_POINT('Ctrl Pts',(-20.6247405377758,14.4507732360595,
130.749766053951)) ;
#151989 = CARTESIAN_POINT('Ctrl Pts',(-20.7069579624013,14.5087792678555,
131.023045402965)) ;
#151990 = CARTESIAN_POINT('Ctrl Pts',(-20.7911628034135,14.4887238336712,
131.302264434157)) ;
#151991 = CARTESIAN_POINT('Ctrl Pts',(-20.8697693366433,14.3928285084541,
131.564906273796)) ;
#151992 = CARTESIAN_POINT('Ctrl Pts',(-20.9374577677181,14.2263682040696,
131.795916170133)) ;
#151993 = CARTESIAN_POINT('Ctrl Pts',(-20.9876137387477,14.0038696460673,
131.975425509327)) ;
#151994 = CARTESIAN_POINT('Ctrl Pts',(-21.0167121922335,13.7389372008462,
132.093575454873)) ;
#151995 = CARTESIAN_POINT('Ctrl Pts',(-21.021624803058,13.4518073715824,132.141010517718)) ;
#151996 = CARTESIAN_POINT('Ctrl Pts',(-21.001265184062,13.1616327439453,132.114737089628)) ;
#151997 = CARTESIAN_POINT('Ctrl Pts',(-20.9563235153239,12.8906304372966,
132.016607385205)) ;
#151998 = CARTESIAN_POINT('Ctrl Pts',(-20.8895478488704,12.6585325321797,
131.854601473478)) ;
#151999 = CARTESIAN_POINT('Ctrl Pts',(-20.8050290649649,12.4808578746759,
131.640730446969)) ;
#152000 = CARTESIAN_POINT('Ctrl Pts',(-20.706854482996,12.369794968941,131.387313297938)) ;
#152001 = CARTESIAN_POINT('Ctrl Pts',(-20.6035841518815,12.3353140243209,
131.118587941619)) ;
#152002 = CARTESIAN_POINT('Ctrl Pts',(-20.4999425243112,12.3783402005982,
130.849020652898)) ;
#152003 = CARTESIAN_POINT('Ctrl Pts',(-20.4037610912831,12.4961137906607,
130.601107675479)) ;
#152004 = CARTESIAN_POINT('Ctrl Pts',(-20.3206161817449,12.6800956082709,
130.391318319672)) ;
#152005 = CARTESIAN_POINT('Ctrl Pts',(-20.2557578107062,12.9180877152906,
130.235043956869)) ;
#152006 = CARTESIAN_POINT('Ctrl Pts',(-20.2134909793572,13.1911275173993,
130.144619104063)) ;
#152007 = CARTESIAN_POINT('Ctrl Pts',(-20.1956945315034,13.4815072415882,
130.125770538085)) ;
#152008 = CARTESIAN_POINT('Ctrl Pts',(-20.2032544219231,13.7684314308885,
130.181084199128)) ;
#152009 = CARTESIAN_POINT('Ctrl Pts',(-20.2346242895992,14.029076308477,130.305758033525)) ;
#152010 = CARTESIAN_POINT('Ctrl Pts',(-20.2871102678795,14.2473093926041,
130.492262967075)) ;
#152011 = CARTESIAN_POINT('Ctrl Pts',(-20.3557014691764,14.4057091519906,
130.725627737145)) ;
#152012 = CARTESIAN_POINT('Ctrl Pts',(-20.4356832288713,14.4946178708306,
130.992528144001)) ;
#152013 = CARTESIAN_POINT('Ctrl Pts',(-20.5195606513706,14.5063975208026,
131.270592829057)) ;
#152014 = CARTESIAN_POINT('Ctrl Pts',(-20.601669735203,14.4401278585609,131.543748083559)) ;
#152015 = CARTESIAN_POINT('Ctrl Pts',(-20.6740334559909,14.3020001323071,
131.788087967881)) ;
#152016 = CARTESIAN_POINT('Ctrl Pts',(-20.7320052756849,14.100380875427,131.990589852135)) ;
#152017 = CARTESIAN_POINT('Ctrl Pts',(-20.7701334334659,13.8504602239821,
132.135070902885)) ;
#152018 = CARTESIAN_POINT('Ctrl Pts',(-20.7851220054825,13.5690360496352,
132.212066464694)) ;
#152019 = CARTESIAN_POINT('Ctrl Pts',(-20.7749067351906,13.277347744237,132.215406858043)) ;
#152020 = CARTESIAN_POINT('Ctrl Pts',(-20.739950771466,12.9978265767653,132.146263744771)) ;
#152021 = CARTESIAN_POINT('Ctrl Pts',(-20.6815482067024,12.747023860199,132.008839074771)) ;
#152022 = CARTESIAN_POINT('Ctrl Pts',(-20.6035221230103,12.5453431667421,
131.813989900865)) ;
#152023 = CARTESIAN_POINT('Ctrl Pts',(-20.5104128505178,12.4062333259034,
131.575152883014)) ;
#152024 = CARTESIAN_POINT('Ctrl Pts',(-20.4087091658857,12.3400677949455,
131.311081123435)) ;
#152025 = CARTESIAN_POINT('Ctrl Pts',(-20.303791085454,12.3515722965719,131.037884994155)) ;
#152026 = CARTESIAN_POINT('Ctrl Pts',(-20.2041191745575,12.4396025465946,
130.779723997866)) ;
#152027 = CARTESIAN_POINT('Ctrl Pts',(-20.1147712529316,12.5983879462257,
130.551883797315)) ;
#152028 = CARTESIAN_POINT('Ctrl Pts',(-20.0421585923302,12.8155081778463,
130.372801469089)) ;
#152029 = CARTESIAN_POINT('Ctrl Pts',(-19.9900861703505,13.0777480891852,
130.253944896754)) ;
#152030 = CARTESIAN_POINT('Ctrl Pts',(-19.9622906553043,13.3640007134148,
130.205892912972)) ;
#152031 = CARTESIAN_POINT('Ctrl Pts',(-19.9596040305283,13.6530970190172,
130.231033720601)) ;
#152032 = CARTESIAN_POINT('Ctrl Pts',(-19.9815947583038,13.9274410550996,
130.328465672942)) ;
#152033 = CARTESIAN_POINT('Ctrl Pts',(-20.0259169621657,14.1649405448642,
130.491043143204)) ;
#152034 = CARTESIAN_POINT('Ctrl Pts',(-20.0889049637749,14.3499176915205,
130.708260928926)) ;
#152035 = CARTESIAN_POINT('Ctrl Pts',(-20.1649263048442,14.4676736740884,
130.963435819328)) ;
#152036 = CARTESIAN_POINT('Ctrl Pts',(-20.247688472556,14.5109849198275,131.238193829716)) ;
#152037 = CARTESIAN_POINT('Ctrl Pts',(-20.331483197017,14.4763368011369,131.516227084564)) ;
#152038 = CARTESIAN_POINT('Ctrl Pts',(-20.4085145537121,14.3664425274482,
131.774319022009)) ;
#152039 = CARTESIAN_POINT('Ctrl Pts',(-20.4732700628347,14.1882602546085,
131.996710354005)) ;
#152040 = CARTESIAN_POINT('Ctrl Pts',(-20.5197600667737,13.9563928712726,
132.165546655575)) ;
#152041 = CARTESIAN_POINT('Ctrl Pts',(-20.544429934519,13.6856075071528,132.270760904427)) ;
#152042 = CARTESIAN_POINT('Ctrl Pts',(-20.5446218153691,13.3967978155194,
132.304370094684)) ;
#152043 = CARTESIAN_POINT('Ctrl Pts',(-20.5194831662747,13.1083772147109,
132.264162983921)) ;
#152044 = CARTESIAN_POINT('Ctrl Pts',(-20.4702619913672,12.8436201216384,
132.15346806604)) ;
#152045 = CARTESIAN_POINT('Ctrl Pts',(-20.3994698940617,12.6197329650473,
131.979865314557)) ;
#152046 = CARTESIAN_POINT('Ctrl Pts',(-20.3120006020497,12.4541610182818,
131.75739537006)) ;
#152047 = CARTESIAN_POINT('Ctrl Pts',(-20.2125860830344,12.3575181073951,
131.500199627294)) ;
#152048 = CARTESIAN_POINT('Ctrl Pts',(-20.1088815096965,12.337407534574,131.230203979974)) ;
#152049 = CARTESIAN_POINT('Ctrl Pts',(-20.0060146641454,12.3950240477661,
130.962919259217)) ;
#152050 = CARTESIAN_POINT('Ctrl Pts',(-19.9119864658295,12.5255974682326,
130.721236187127)) ;
#152051 = CARTESIAN_POINT('Ctrl Pts',(-19.8314897395286,12.7221236513144,
130.519397456966)) ;
#152052 = CARTESIAN_POINT('Ctrl Pts',(-19.7710089279874,12.966643820031,130.375676004731)) ;
#152053 = CARTESIAN_POINT('Ctrl Pts',(-19.732928013481,13.2467842966359,130.297774420096)) ;
#152054 = CARTESIAN_POINT('Ctrl Pts',(-19.7201400299444,13.5364084867458,
130.293371523372)) ;
#152055 = CARTESIAN_POINT('Ctrl Pts',(-19.7322324408918,13.819301352246,130.361818332685)) ;
#152056 = CARTESIAN_POINT('Ctrl Pts',(-19.7678249009645,14.0737430594077,
130.498891515294)) ;
#152057 = CARTESIAN_POINT('Ctrl Pts',(-19.8239107737393,14.2823383256047,
130.695974069195)) ;
#152058 = CARTESIAN_POINT('Ctrl Pts',(-19.8950604586474,14.4280819786068,
130.936830915041)) ;
#152059 = CARTESIAN_POINT('Ctrl Pts',(-19.9759986631136,14.5027907188546,
131.20637093887)) ;
#152060 = CARTESIAN_POINT('Ctrl Pts',(-20.0606762821136,14.4996009182714,
131.487070199978)) ;
#152061 = CARTESIAN_POINT('Ctrl Pts',(-20.1407098011001,14.4198435135005,
131.753794032065)) ;
#152062 = CARTESIAN_POINT('Ctrl Pts',(-20.2112630859601,14.2682255575811,
131.993092362855)) ;
#152063 = CARTESIAN_POINT('Ctrl Pts',(-20.2656775957736,14.0566692320112,
132.185107721384)) ;
#152064 = CARTESIAN_POINT('Ctrl Pts',(-20.2997748055791,13.7984046917339,
132.317960439349)) ;
#152065 = CARTESIAN_POINT('Ctrl Pts',(-20.3099989318143,13.5146255183712,
132.38088711118)) ;
#152066 = CARTESIAN_POINT('Ctrl Pts',(-20.2951296394703,13.22379017507,132.370580468596)) ;
#152067 = CARTESIAN_POINT('Ctrl Pts',(-20.2555701663945,12.9476430099182,
132.288081447981)) ;
#152068 = CARTESIAN_POINT('Ctrl Pts',(-20.1928769291611,12.7041858709694,
132.138213583783)) ;
#152069 = CARTESIAN_POINT('Ctrl Pts',(-20.1120002752265,12.5142908380612,
131.934883468866)) ;
#152070 = CARTESIAN_POINT('Ctrl Pts',(-20.0165096996154,12.3877724329813,
131.689173717466)) ;
#152071 = CARTESIAN_POINT('Ctrl Pts',(-19.913478604829,12.3361912043238,131.421332336646)) ;
#152072 = CARTESIAN_POINT('Ctrl Pts',(-19.8094708653727,12.3624798224069,
131.150606824843)) ;
#152073 = CARTESIAN_POINT('Ctrl Pts',(-19.7113062006748,12.4640688022784,
130.896852899496)) ;
#152074 = CARTESIAN_POINT('Ctrl Pts',(-19.6243191332476,12.6358046245907,
130.676044087363)) ;
#152075 = CARTESIAN_POINT('Ctrl Pts',(-19.5555745074161,12.862048858162,130.508185639822)) ;
#152076 = CARTESIAN_POINT('Ctrl Pts',(-19.5079382213539,13.1294243703739,
130.402168639634)) ;
#152077 = CARTESIAN_POINT('Ctrl Pts',(-19.4847311841948,13.419127554444,130.367646107838)) ;
#152078 = CARTESIAN_POINT('Ctrl Pts',(-19.486760537507,13.7060585256719,130.406486755971)) ;
#152079 = CARTESIAN_POINT('Ctrl Pts',(-19.5132448910941,13.9758635071568,
130.517143788552)) ;
#152080 = CARTESIAN_POINT('Ctrl Pts',(-19.561461527867,14.2044690811379,130.691105042514)) ;
#152081 = CARTESIAN_POINT('Ctrl Pts',(-19.6271525262166,14.3772046466544,
130.916107336043)) ;
#152082 = CARTESIAN_POINT('Ctrl Pts',(-19.7049913038784,14.4817041640368,
131.17660395042)) ;
#152083 = CARTESIAN_POINT('Ctrl Pts',(-19.7886768197028,14.5103977605507,
131.454191387136)) ;
#152084 = CARTESIAN_POINT('Ctrl Pts',(-19.8713625246764,14.461387716176,131.728812616932)) ;
#152085 = CARTESIAN_POINT('Ctrl Pts',(-19.9466960883751,14.3378670523305,
131.982034797292)) ;
#152086 = CARTESIAN_POINT('Ctrl Pts',(-20.0083045176645,14.1487649480966,
132.195144873615)) ;
#152087 = CARTESIAN_POINT('Ctrl Pts',(-20.0510942154457,13.9077124472436,
132.35327591803)) ;
#152088 = CARTESIAN_POINT('Ctrl Pts',(-20.0712746305926,13.6318349091011,
132.445369268278)) ;
#152089 = CARTESIAN_POINT('Ctrl Pts',(-20.0666628175852,13.3411961915081,
132.465016541542)) ;
#152090 = CARTESIAN_POINT('Ctrl Pts',(-20.0369065317575,13.0563347009616,
132.411215549619)) ;
#152091 = CARTESIAN_POINT('Ctrl Pts',(-19.9832697572704,12.7976622253545,
132.287685663652)) ;
#152092 = CARTESIAN_POINT('Ctrl Pts',(-19.909474160919,12.584625305209,132.105083184337)) ;
#152093 = CARTESIAN_POINT('Ctrl Pts',(-19.8184221729735,12.429833286881,131.872506784025)) ;
#152094 = CARTESIAN_POINT('Ctrl Pts',(-19.7187303437125,12.3481748757021,
131.614098966012)) ;
#152095 = CARTESIAN_POINT('Ctrl Pts',(-19.6138632113487,12.3422836205948,
131.341022208364)) ;
#152096 = CARTESIAN_POINT('Ctrl Pts',(-19.5124594677726,12.414162317258,131.077872115915)) ;
#152097 = CARTESIAN_POINT('Ctrl Pts',(-19.420212188348,12.55849168118,130.841573794732)) ;
#152098 = CARTESIAN_POINT('Ctrl Pts',(-19.3435324232807,12.7644624942609,
130.65066449742)) ;
#152099 = CARTESIAN_POINT('Ctrl Pts',(-19.2868798087134,13.0174115077838,
130.518256914751)) ;
#152100 = CARTESIAN_POINT('Ctrl Pts',(-19.2535766304538,13.2998964348547,
130.454116409847)) ;
#152101 = CARTESIAN_POINT('Ctrl Pts',(-19.2453729976278,13.5908799629275,
130.463258994527)) ;
#152102 = CARTESIAN_POINT('Ctrl Pts',(-19.2621513468008,13.8706960081611,
130.545479006086)) ;
#152103 = CARTESIAN_POINT('Ctrl Pts',(-19.3020872042403,14.1180202656557,
130.695329004107)) ;
#152104 = CARTESIAN_POINT('Ctrl Pts',(-19.3610103361281,14.3143765894564,
130.900421785235)) ;
#152105 = CARTESIAN_POINT('Ctrl Pts',(-19.434812974818,14.4481660809184,131.149213001408)) ;
#152106 = CARTESIAN_POINT('Ctrl Pts',(-19.5166794707772,14.5080838606745,
131.421381896559)) ;
#152107 = CARTESIAN_POINT('Ctrl Pts',(-19.6008596180551,14.4905518531177,
131.700498217892)) ;
#152108 = CARTESIAN_POINT('Ctrl Pts',(-19.679959110775,14.3964092296967,131.964690313878)) ;
#152109 = CARTESIAN_POINT('Ctrl Pts',(-19.7478273039877,14.232304987228,132.196115316038)) ;
#152110 = CARTESIAN_POINT('Ctrl Pts',(-19.7986192880396,14.0113006854444,
132.37749892765)) ;
#152111 = CARTESIAN_POINT('Ctrl Pts',(-19.8284139029138,13.7469853282518,
132.497724021509)) ;
#152112 = CARTESIAN_POINT('Ctrl Pts',(-19.8340820683678,13.4601451324146,
132.547372256783)) ;
#152113 = CARTESIAN_POINT('Ctrl Pts',(-19.8142531422841,13.1687003200991,
132.522778212001)) ;
#152114 = CARTESIAN_POINT('Ctrl Pts',(-19.7703730343976,12.8989650919222,
132.427483609972)) ;
#152115 = CARTESIAN_POINT('Ctrl Pts',(-19.7036589079187,12.6635916504989,
132.265932090456)) ;
#152116 = CARTESIAN_POINT('Ctrl Pts',(-19.6199118535932,12.485239800862,132.054155238019)) ;
#152117 = CARTESIAN_POINT('Ctrl Pts',(-19.5219805853211,12.3719259500599,
131.801473410491)) ;
#152118 = CARTESIAN_POINT('Ctrl Pts',(-19.4189379680128,12.3351771032852,
131.53336398971)) ;
#152119 = CARTESIAN_POINT('Ctrl Pts',(-19.3148770024859,12.3762351050997,
131.26268009039)) ;
#152120 = CARTESIAN_POINT('Ctrl Pts',(-19.2189066435572,12.4911992435135,
131.01519951472)) ;
#152121 = CARTESIAN_POINT('Ctrl Pts',(-19.1347439547889,12.6745749260732,
130.802658266804)) ;
#152122 = CARTESIAN_POINT('Ctrl Pts',(-19.0695712650756,12.9105841176317,
130.64534787781)) ;
#152123 = CARTESIAN_POINT('Ctrl Pts',(-19.026516615279,13.1834575472762,130.552699546602)) ;
#152124 = CARTESIAN_POINT('Ctrl Pts',(-19.0081217007437,13.4728172007292,
130.532007746554)) ;
#152125 = CARTESIAN_POINT('Ctrl Pts',(-19.0147866964172,13.7593252111675,
130.584597145698)) ;
#152126 = CARTESIAN_POINT('Ctrl Pts',(-19.0457740324292,14.0229111380707,
130.708413150787)) ;
#152127 = CARTESIAN_POINT('Ctrl Pts',(-19.0973111190571,14.2409568530166,
130.891883602161)) ;
#152128 = CARTESIAN_POINT('Ctrl Pts',(-19.165926552844,14.4024702596202,131.125549278518)) ;
#152129 = CARTESIAN_POINT('Ctrl Pts',(-19.2454507888212,14.4930252918819,
131.390998297428)) ;
#152130 = CARTESIAN_POINT('Ctrl Pts',(-19.3293410740711,14.5071138077779,
131.669126207063)) ;
#152131 = CARTESIAN_POINT('Ctrl Pts',(-19.4112821511384,14.4434722304718,
131.941650206842)) ;
#152132 = CARTESIAN_POINT('Ctrl Pts',(-19.4842739640058,14.3072991508372,
132.187922760495)) ;
#152133 = CARTESIAN_POINT('Ctrl Pts',(-19.5429829781195,14.1061281755834,
132.392741540416)) ;
#152134 = CARTESIAN_POINT('Ctrl Pts',(-19.5814898983426,13.8584458365122,
132.538171297678)) ;
#152135 = CARTESIAN_POINT('Ctrl Pts',(-19.5972452937213,13.5782527615593,
132.617345758941)) ;
#152136 = CARTESIAN_POINT('Ctrl Pts',(-19.587821553024,13.2862405830432,132.623036030091)) ;
#152137 = CARTESIAN_POINT('Ctrl Pts',(-19.5535345414538,13.0054673407222,
132.55591759128)) ;
#152138 = CARTESIAN_POINT('Ctrl Pts',(-19.4954706738399,12.7527978446706,
132.419600001604)) ;
#152139 = CARTESIAN_POINT('Ctrl Pts',(-19.4183727349997,12.5507722085017,
132.227270319449)) ;
#152140 = CARTESIAN_POINT('Ctrl Pts',(-19.3255707730553,12.4092693590586,
131.989364894937)) ;
#152141 = CARTESIAN_POINT('Ctrl Pts',(-19.2238321783356,12.3409406073707,
131.725254513543)) ;
#152142 = CARTESIAN_POINT('Ctrl Pts',(-19.119236753858,12.3499819194409,131.452886617979)) ;
#152143 = CARTESIAN_POINT('Ctrl Pts',(-19.0188367516298,12.4363532158425,
131.192772449436)) ;
#152144 = CARTESIAN_POINT('Ctrl Pts',(-18.9295447538629,12.5925663631045,
130.964931579883)) ;
#152145 = CARTESIAN_POINT('Ctrl Pts',(-18.85618070133,12.8085170384963,130.783729205798)) ;
#152146 = CARTESIAN_POINT('Ctrl Pts',(-18.8035406576781,13.0694866152918,
130.663175810496)) ;
#152147 = CARTESIAN_POINT('Ctrl Pts',(-18.774944483164,13.3550371201656,130.612758020313)) ;
#152148 = CARTESIAN_POINT('Ctrl Pts',(-18.7715872372659,13.6462143005165,
130.636161963138)) ;
#152149 = CARTESIAN_POINT('Ctrl Pts',(-18.7928313609646,13.9195287631536,
130.73120381732)) ;
#152150 = CARTESIAN_POINT('Ctrl Pts',(-18.8365269344384,14.1586150899391,
130.891977988719)) ;
#152151 = CARTESIAN_POINT('Ctrl Pts',(-18.8989146423201,14.3449689837057,
131.10737481057)) ;
#152152 = CARTESIAN_POINT('Ctrl Pts',(-18.9745793166611,14.465239738532,131.36150472704)) ;
#152153 = CARTESIAN_POINT('Ctrl Pts',(-19.0578793507872,14.5107689866746,
131.638093119859)) ;
#152154 = CARTESIAN_POINT('Ctrl Pts',(-19.1409583613005,14.4787461978325,
131.913707901465)) ;
#152155 = CARTESIAN_POINT('Ctrl Pts',(-19.2189706552468,14.3700644324197,
132.17497387013)) ;
#152156 = CARTESIAN_POINT('Ctrl Pts',(-19.2836848317943,14.1946408166751,
132.397013538057)) ;
#152157 = CARTESIAN_POINT('Ctrl Pts',(-19.3309065027156,13.963907732595,132.568053904224)) ;
#152158 = CARTESIAN_POINT('Ctrl Pts',(-19.3562835215805,13.6940409321305,
132.675319682935)) ;
#152159 = CARTESIAN_POINT('Ctrl Pts',(-19.3571223286895,13.4043243937501,
132.710955989412)) ;
#152160 = CARTESIAN_POINT('Ctrl Pts',(-19.3329129352278,13.1175424358185,
132.673226068229)) ;
#152161 = CARTESIAN_POINT('Ctrl Pts',(-19.284075134649,12.8501254079525,132.563869228407)) ;
#152162 = CARTESIAN_POINT('Ctrl Pts',(-19.2141838640519,12.6260375389968,
132.392718948333)) ;
#152163 = CARTESIAN_POINT('Ctrl Pts',(-19.1270338823226,12.4581545252769,
132.171242119684)) ;
#152164 = CARTESIAN_POINT('Ctrl Pts',(-19.0280972219191,12.3594525497003,
131.915366042047)) ;
#152165 = CARTESIAN_POINT('Ctrl Pts',(-18.9241027514417,12.3367944069397,
131.644635976731)) ;
#152166 = CARTESIAN_POINT('Ctrl Pts',(-18.8208265565642,12.3925085409291,
131.376240849143)) ;
#152167 = CARTESIAN_POINT('Ctrl Pts',(-18.7265133411892,12.5213898755188,
131.133731510503)) ;
#152168 = CARTESIAN_POINT('Ctrl Pts',(-18.6457952560714,12.7155724021421,
130.931131518529)) ;
#152169 = CARTESIAN_POINT('Ctrl Pts',(-18.5846065804363,12.9595220676015,
130.785423050799)) ;
#152170 = CARTESIAN_POINT('Ctrl Pts',(-18.546066469657,13.2367788940881,130.70592009773)) ;
#152171 = CARTESIAN_POINT('Ctrl Pts',(-18.5323213213029,13.5277643625836,
130.698889739784)) ;
#152172 = CARTESIAN_POINT('Ctrl Pts',(-18.543793348028,13.8120453761231,130.765623615628)) ;
#152173 = CARTESIAN_POINT('Ctrl Pts',(-18.5788549474306,14.0676654739834,
130.901176319765)) ;
#152174 = CARTESIAN_POINT('Ctrl Pts',(-18.6343035780449,14.2771419928287,
131.096308854122)) ;
#152175 = CARTESIAN_POINT('Ctrl Pts',(-18.7050835708224,14.425031880978,131.336092927187)) ;
#152176 = CARTESIAN_POINT('Ctrl Pts',(-18.7861994089251,14.5017260060049,
131.60629231186)) ;
#152177 = CARTESIAN_POINT('Ctrl Pts',(-18.8699095303306,14.5010099059246,
131.883776032442)) ;
#152178 = CARTESIAN_POINT('Ctrl Pts',(-18.950862117856,14.4231233705973,132.153475808602)) ;
#152179 = CARTESIAN_POINT('Ctrl Pts',(-19.0216063325537,14.2735700722065,
132.393250548626)) ;
#152180 = CARTESIAN_POINT('Ctrl Pts',(-19.0766525736922,14.0631260843178,
132.587185321685)) ;
#152181 = CARTESIAN_POINT('Ctrl Pts',(-19.1112752517511,13.8068513237717,
132.721449739404)) ;
#152182 = CARTESIAN_POINT('Ctrl Pts',(-19.1222768851844,13.5229068768556,
132.786731908381)) ;
#152183 = CARTESIAN_POINT('Ctrl Pts',(-19.1081388609896,13.2323185296325,
132.778518604924)) ;
#152184 = CARTESIAN_POINT('Ctrl Pts',(-19.0692979350921,12.955462422634,132.698120669452)) ;
#152185 = CARTESIAN_POINT('Ctrl Pts',(-19.0072938758856,12.7108337306576,
132.550242420851)) ;
#152186 = CARTESIAN_POINT('Ctrl Pts',(-18.9267369862212,12.5189036902296,
132.347912261719)) ;
#152187 = CARTESIAN_POINT('Ctrl Pts',(-18.8318784493428,12.3906586207823,
132.103941582259)) ;
#152188 = CARTESIAN_POINT('Ctrl Pts',(-18.7288363533557,12.3366531336248,
131.836123081131)) ;
#152189 = CARTESIAN_POINT('Ctrl Pts',(-18.624925410328,12.360297772879,131.565617456112)) ;
#152190 = CARTESIAN_POINT('Ctrl Pts',(-18.5256578035359,12.4609988515391,
131.308947306111)) ;
#152191 = CARTESIAN_POINT('Ctrl Pts',(-18.4392051331275,12.6291274638668,
131.089332236554)) ;
#152192 = CARTESIAN_POINT('Ctrl Pts',(-18.3692689876453,12.8555169755094,
130.918257614385)) ;
#152193 = CARTESIAN_POINT('Ctrl Pts',(-18.3212190683975,13.1215885522129,
130.810953330662)) ;
#152194 = CARTESIAN_POINT('Ctrl Pts',(-18.2972960902934,13.4096083938423,
130.774191778671)) ;
#152195 = CARTESIAN_POINT('Ctrl Pts',(-18.2985416991129,13.698212942693,130.810897551179)) ;
#152196 = CARTESIAN_POINT('Ctrl Pts',(-18.3244750392328,13.9691452295141,
130.91998909622)) ;
#152197 = CARTESIAN_POINT('Ctrl Pts',(-18.3719691340465,14.1982918407705,
131.091726472608)) ;
#152198 = CARTESIAN_POINT('Ctrl Pts',(-18.437100638801,14.3728095621698,131.315054734931)) ;
#152199 = CARTESIAN_POINT('Ctrl Pts',(-18.5147502122421,14.479662285758,131.575038501861)) ;
#152200 = CARTESIAN_POINT('Ctrl Pts',(-18.5984271700058,14.5107460879228,
131.852624565577)) ;
#152201 = CARTESIAN_POINT('Ctrl Pts',(-18.6814592251425,14.4636147982726,
132.128355723987)) ;
#152202 = CARTESIAN_POINT('Ctrl Pts',(-18.7567611079911,14.3427084720644,
132.38133252825)) ;
#152203 = CARTESIAN_POINT('Ctrl Pts',(-18.8191499212685,14.1545214106307,
132.596878690056)) ;
#152204 = CARTESIAN_POINT('Ctrl Pts',(-18.8624161383915,13.914665784431,132.756380600079)) ;
#152205 = CARTESIAN_POINT('Ctrl Pts',(-18.8832226690577,13.6405172708492,
132.850185928448)) ;
#152206 = CARTESIAN_POINT('Ctrl Pts',(-18.879379985006,13.3501102818962,132.872073497633)) ;
#152207 = CARTESIAN_POINT('Ctrl Pts',(-18.8504830366193,13.0651843315454,
132.820727303234)) ;
#152208 = CARTESIAN_POINT('Ctrl Pts',(-18.7972049191449,12.80388772374,132.698441638351)) ;
#152209 = CARTESIAN_POINT('Ctrl Pts',(-18.723938579695,12.5899465270377,132.517340764542)) ;
#152210 = CARTESIAN_POINT('Ctrl Pts',(-18.6339631078438,12.4339563210189,
132.28768165985)) ;
#152211 = CARTESIAN_POINT('Ctrl Pts',(-18.533655418016,12.3491846989202,132.027754670765)) ;
#152212 = CARTESIAN_POINT('Ctrl Pts',(-18.4287414629348,12.3415474281895,
131.754556958259)) ;
#152213 = CARTESIAN_POINT('Ctrl Pts',(-18.3275546121177,12.4110292201394,
131.491915929484)) ;
#152214 = CARTESIAN_POINT('Ctrl Pts',(-18.2349169164515,12.5533605448057,
131.254484931781)) ;
#152215 = CARTESIAN_POINT('Ctrl Pts',(-18.1578099509812,12.7574391512257,
131.062286140571)) ;
#152216 = CARTESIAN_POINT('Ctrl Pts',(-18.1003696787992,13.0095817126533,
130.92762938283)) ;
#152217 = CARTESIAN_POINT('Ctrl Pts',(-18.0663253206741,13.2928226801242,
130.861470362866)) ;
#152218 = CARTESIAN_POINT('Ctrl Pts',(-18.0574821752941,13.5820119966617,
130.868533156755)) ;
#152219 = CARTESIAN_POINT('Ctrl Pts',(-18.0735684910089,13.8633229249982,
130.948835515899)) ;
#152220 = CARTESIAN_POINT('Ctrl Pts',(-18.1128079244624,14.1112602779132,
131.096570682687)) ;
#152221 = CARTESIAN_POINT('Ctrl Pts',(-18.1713264366975,14.3095521754014,
131.300538449874)) ;
#152222 = CARTESIAN_POINT('Ctrl Pts',(-18.2445253330056,14.4451057235358,
131.547453993518)) ;
#152223 = CARTESIAN_POINT('Ctrl Pts',(-18.3269176211252,14.5076745769451,
131.821434215678)) ;
#152224 = CARTESIAN_POINT('Ctrl Pts',(-18.4109135921778,14.4918702514085,
132.09992274832)) ;
#152225 = CARTESIAN_POINT('Ctrl Pts',(-18.4899530140776,14.4001695900989,
132.363825830347)) ;
#152226 = CARTESIAN_POINT('Ctrl Pts',(-18.5581972721776,14.238339270588,132.596306467926)) ;
#152227 = CARTESIAN_POINT('Ctrl Pts',(-18.6097312244741,14.0178457541506,
132.77999745246)) ;
#152228 = CARTESIAN_POINT('Ctrl Pts',(-18.6401448193709,13.7549024704848,
132.901969265826)) ;
#152229 = CARTESIAN_POINT('Ctrl Pts',(-18.6463850313128,13.4669383655623,
132.953465269722)) ;
#152230 = CARTESIAN_POINT('Ctrl Pts',(-18.6276503009215,13.1792878389568,
132.931593942622)) ;
#152231 = CARTESIAN_POINT('Ctrl Pts',(-18.5840179153444,12.9054935275296,
132.837423835677)) ;
#152232 = CARTESIAN_POINT('Ctrl Pts',(-18.5184918875895,12.6708451835732,
132.679031311941)) ;
#152233 = CARTESIAN_POINT('Ctrl Pts',(-18.4344363065144,12.4890109361581,
132.466673752346)) ;
#152234 = CARTESIAN_POINT('Ctrl Pts',(-18.3378254602386,12.3747427440592,
132.217485900113)) ;
#152235 = CARTESIAN_POINT('Ctrl Pts',(-18.2341291109171,12.335118127865,131.947725095572)) ;
#152236 = CARTESIAN_POINT('Ctrl Pts',(-18.1304829793124,12.3735357257966,
131.678071654494)) ;
#152237 = CARTESIAN_POINT('Ctrl Pts',(-18.0332195672274,12.4876827050984,
131.427169660191)) ;
#152238 = CARTESIAN_POINT('Ctrl Pts',(-17.9493134502573,12.668143871092,131.215113064817)) ;
#152239 = CARTESIAN_POINT('Ctrl Pts',(-17.8833190355393,12.9033827829949,
131.055504217813)) ;
#152240 = CARTESIAN_POINT('Ctrl Pts',(-17.8397509602161,13.1743601664502,
130.961218011576)) ;
#152241 = CARTESIAN_POINT('Ctrl Pts',(-17.8204668396867,13.4644840041335,
130.938043352746)) ;
#152242 = CARTESIAN_POINT('Ctrl Pts',(-17.8265350254978,13.7518155739233,
130.988946607329)) ;
#152243 = CARTESIAN_POINT('Ctrl Pts',(-17.8566012791567,14.0147480425275,
131.109855058721)) ;
#152244 = CARTESIAN_POINT('Ctrl Pts',(-17.90786398017,14.2359322469135,131.292745615315)) ;
#152245 = CARTESIAN_POINT('Ctrl Pts',(-17.9762298617494,14.3990328419962,
131.525712867481)) ;
#152246 = CARTESIAN_POINT('Ctrl Pts',(-18.055065638864,14.4913721211862,131.788962667964)) ;
#152247 = CARTESIAN_POINT('Ctrl Pts',(-18.1393991985355,14.5077030613306,
132.068583449212)) ;
#152248 = CARTESIAN_POINT('Ctrl Pts',(-18.2210461373333,14.4466726935246,
132.340051735665)) ;
#152249 = CARTESIAN_POINT('Ctrl Pts',(-18.2950035387414,14.3110620977678,
132.589454770925)) ;
#152250 = CARTESIAN_POINT('Ctrl Pts',(-18.3535868279914,14.1132680684101,
132.793577578567)) ;
#152251 = CARTESIAN_POINT('Ctrl Pts',(-18.393011856418,13.8656264960883,132.941870264204)) ;
#152252 = CARTESIAN_POINT('Ctrl Pts',(-18.4093627200831,13.5853317318957,
133.022849013586)) ;
#152253 = CARTESIAN_POINT('Ctrl Pts',(-18.4005900814448,13.2939513094312,
133.030374526169)) ;
#152254 = CARTESIAN_POINT('Ctrl Pts',(-18.3670959101891,13.0136081090702,
132.965460512865)) ;
#152255 = CARTESIAN_POINT('Ctrl Pts',(-18.3099441323283,12.7604084565328,
132.831704484875)) ;
#152256 = CARTESIAN_POINT('Ctrl Pts',(-18.2330287799136,12.5556140537718,
132.640069906698)) ;
#152257 = CARTESIAN_POINT('Ctrl Pts',(-18.1403993250708,12.412162783817,132.402717407191)) ;
#152258 = CARTESIAN_POINT('Ctrl Pts',(-18.039122761627,12.3419224833159,132.139862058296)) ;
#152259 = CARTESIAN_POINT('Ctrl Pts',(-17.9346214328855,12.3485705631489,
131.867734666129)) ;
#152260 = CARTESIAN_POINT('Ctrl Pts',(-17.8340398826189,12.4325162173742,
131.60707108893)) ;
#152261 = CARTESIAN_POINT('Ctrl Pts',(-17.7440580525167,12.5872706018155,
131.377320640071)) ;
#152262 = CARTESIAN_POINT('Ctrl Pts',(-17.6702459325862,12.8016741765326,
131.1947873473)) ;
#152263 = CARTESIAN_POINT('Ctrl Pts',(-17.6170393754709,13.0608926757193,
131.072495055625)) ;
#152264 = CARTESIAN_POINT('Ctrl Pts',(-17.5876611427528,13.3463627388947,
131.019840506949)) ;
#152265 = CARTESIAN_POINT('Ctrl Pts',(-17.5835099051843,13.6367413735624,
131.040812586735)) ;
#152266 = CARTESIAN_POINT('Ctrl Pts',(-17.6040712549613,13.912123441329,131.134008457263)) ;
#152267 = CARTESIAN_POINT('Ctrl Pts',(-17.6473147092117,14.1528033236638,
131.293522210415)) ;
#152268 = CARTESIAN_POINT('Ctrl Pts',(-17.7090710684674,14.3402810134416,
131.506980670982)) ;
#152269 = CARTESIAN_POINT('Ctrl Pts',(-17.784324421975,14.4626257099404,131.759874983544)) ;
#152270 = CARTESIAN_POINT('Ctrl Pts',(-17.8676273435361,14.5106364099982,
132.036519206507)) ;
#152271 = CARTESIAN_POINT('Ctrl Pts',(-17.9509431998974,14.4805445966973,
132.31289642704)) ;
#152272 = CARTESIAN_POINT('Ctrl Pts',(-18.0287637016259,14.3748126779467,
132.57339232087)) ;
#152273 = CARTESIAN_POINT('Ctrl Pts',(-18.0942745357637,14.2005693776624,
132.797921352006)) ;
#152274 = CARTESIAN_POINT('Ctrl Pts',(-18.1420291731984,13.9714224956824,
132.970479780879)) ;
#152275 = CARTESIAN_POINT('Ctrl Pts',(-18.1681061343277,13.7016038456452,
133.07989078727)) ;
#152276 = CARTESIAN_POINT('Ctrl Pts',(-18.1697184694213,13.4137877720204,
133.117594113432)) ;
#152277 = CARTESIAN_POINT('Ctrl Pts',(-18.1460719924332,13.1249621059971,
133.081716204354)) ;
#152278 = CARTESIAN_POINT('Ctrl Pts',(-18.098349112227,12.858759801946,132.975335138158)) ;
#152279 = CARTESIAN_POINT('Ctrl Pts',(-18.0285125557916,12.6311849064932,
132.804627705542)) ;
#152280 = CARTESIAN_POINT('Ctrl Pts',(-17.9419067380147,12.4620614418067,
132.584665021202)) ;
#152281 = CARTESIAN_POINT('Ctrl Pts',(-17.8431161137062,12.3611529243014,
132.329254527925)) ;
#152282 = CARTESIAN_POINT('Ctrl Pts',(-17.7394163400758,12.336402737043,132.059308529178)) ;
#152283 = CARTESIAN_POINT('Ctrl Pts',(-17.636008023939,12.3896954767389,131.790522379684)) ;
#152284 = CARTESIAN_POINT('Ctrl Pts',(-17.5411529235148,12.5169545730866,
131.54651181945)) ;
#152285 = CARTESIAN_POINT('Ctrl Pts',(-17.4601656512396,12.7090014500136,
131.343041028757)) ;
#152286 = CARTESIAN_POINT('Ctrl Pts',(-17.3982954159609,12.9518209129291,
131.195365244849)) ;
#152287 = CARTESIAN_POINT('Ctrl Pts',(-17.3590590475251,13.2283911259786,
131.113826328101)) ;
#152288 = CARTESIAN_POINT('Ctrl Pts',(-17.3445909288019,13.5192444476926,
131.104682525303)) ;
#152289 = CARTESIAN_POINT('Ctrl Pts',(-17.3552759397806,13.8035929406365,
131.169057687742)) ;
#152290 = CARTESIAN_POINT('Ctrl Pts',(-17.3897650651813,14.0607675161601,
131.30300701978)) ;
#152291 = CARTESIAN_POINT('Ctrl Pts',(-17.4443353177419,14.2709776513911,
131.49540177985)) ;
#152292 = CARTESIAN_POINT('Ctrl Pts',(-17.5152284115638,14.4220258151157,
131.735762483094)) ;
#152293 = CARTESIAN_POINT('Ctrl Pts',(-17.5958972727999,14.5004899933202,
132.004539334194)) ;
#152294 = CARTESIAN_POINT('Ctrl Pts',(-17.6797407048686,14.5020985766214,
132.282472815977)) ;
#152295 = CARTESIAN_POINT('Ctrl Pts',(-17.7606887259789,14.426667623352,132.552070316538)) ;
#152296 = CARTESIAN_POINT('Ctrl Pts',(-17.8320641853255,14.2786158189735,
132.79380669298)) ;
#152297 = CARTESIAN_POINT('Ctrl Pts',(-17.8875765378756,14.0697690186074,
132.989079973035)) ;
#152298 = CARTESIAN_POINT('Ctrl Pts',(-17.922834488677,13.8142976320865,133.125231432651)) ;
#152299 = CARTESIAN_POINT('Ctrl Pts',(-17.9345112522901,13.5318062075926,
133.19237603013)) ;
#152300 = CARTESIAN_POINT('Ctrl Pts',(-17.9211404368569,13.2403761874523,
133.186487415733)) ;
#152301 = CARTESIAN_POINT('Ctrl Pts',(-17.8827207165006,12.9618561593774,
133.107451653599)) ;
#152302 = CARTESIAN_POINT('Ctrl Pts',(-17.821581417852,12.7173263730279,132.96193349821)) ;
#152303 = CARTESIAN_POINT('Ctrl Pts',(-17.7413926221805,12.5233446886838,
132.760735766704)) ;
#152304 = CARTESIAN_POINT('Ctrl Pts',(-17.6467746618759,12.3931312315505,
132.517486220828)) ;
#152305 = CARTESIAN_POINT('Ctrl Pts',(-17.5437035922363,12.337075246258,132.249632321582)) ;
#152306 = CARTESIAN_POINT('Ctrl Pts',(-17.4401454160532,12.3586764449227,
131.98003227223)) ;
#152307 = CARTESIAN_POINT('Ctrl Pts',(-17.3410665934673,12.4563696314589,
131.723751639427)) ;
#152308 = CARTESIAN_POINT('Ctrl Pts',(-17.2536320179894,12.6234424170359,
131.50146332499)) ;
#152309 = CARTESIAN_POINT('Ctrl Pts',(-17.1832036195686,12.8484690314232,
131.32893954711)) ;
#152310 = CARTESIAN_POINT('Ctrl Pts',(-17.1344653483001,13.1134860607375,
131.219613229379)) ;
#152311 = CARTESIAN_POINT('Ctrl Pts',(-17.1097906021278,13.402425050447,131.180795951585)) ;
#152312 = CARTESIAN_POINT('Ctrl Pts',(-17.1104146704051,13.6901681944769,
131.215561704661)) ;
#152313 = CARTESIAN_POINT('Ctrl Pts',(-17.1355551568111,13.9614083380647,
131.322263958797)) ;
#152314 = CARTESIAN_POINT('Ctrl Pts',(-17.1825349214449,14.1924050674132,
131.492558721692)) ;
#152315 = CARTESIAN_POINT('Ctrl Pts',(-17.247284144374,14.3688010159201,131.714792207733)) ;
#152316 = CARTESIAN_POINT('Ctrl Pts',(-17.3247083783915,14.4776662097744,
131.974131076165)) ;
#152317 = CARTESIAN_POINT('Ctrl Pts',(-17.4080456851403,14.5108828480259,
132.250624200494)) ;
#152318 = CARTESIAN_POINT('Ctrl Pts',(-17.4912091781135,14.4662997711349,
132.526737050679)) ;
#152319 = CARTESIAN_POINT('Ctrl Pts',(-17.5670722488366,14.3468724358185,
132.781476724685)) ;
#152320 = CARTESIAN_POINT('Ctrl Pts',(-17.6295496572066,14.161614932188,132.997074962764)) ;
#152321 = CARTESIAN_POINT('Ctrl Pts',(-17.6736158962945,13.9230022753498,
133.158962448849)) ;
#152322 = CARTESIAN_POINT('Ctrl Pts',(-17.6951931588153,13.6485314062169,
133.25514650467)) ;
#152323 = CARTESIAN_POINT('Ctrl Pts',(-17.6920615738823,13.3583011743042,
133.279105884718)) ;
#152324 = CARTESIAN_POINT('Ctrl Pts',(-17.6637579865309,13.072504270402,133.229551323447)) ;
#152325 = CARTESIAN_POINT('Ctrl Pts',(-17.6114584214845,12.8117566735177,
133.109923707737)) ;
#152326 = CARTESIAN_POINT('Ctrl Pts',(-17.5386760935971,12.5955171582893,
132.930311398659)) ;
#152327 = CARTESIAN_POINT('Ctrl Pts',(-17.4485485923782,12.4369580568928,
132.700390646819)) ;
#152328 = CARTESIAN_POINT('Ctrl Pts',(-17.3489049682672,12.3507869630092,
132.442246375848)) ;
#152329 = CARTESIAN_POINT('Ctrl Pts',(-17.2444930320388,12.3404899643528,
132.170365644373)) ;
#152330 = CARTESIAN_POINT('Ctrl Pts',(-17.1426216271441,12.4078494476239,
131.905884901552)) ;
#152331 = CARTESIAN_POINT('Ctrl Pts',(-17.0495668256941,12.5483871977687,
131.667259067528)) ;
#152332 = CARTESIAN_POINT('Ctrl Pts',(-16.971814498006,12.7513533086917,131.473242742698)) ;
#152333 = CARTESIAN_POINT('Ctrl Pts',(-16.9139622836365,13.001941318222,131.337310415625)) ;
#152334 = CARTESIAN_POINT('Ctrl Pts',(-16.8792750897038,13.2828868274063,
131.269082634896)) ;
#152335 = CARTESIAN_POINT('Ctrl Pts',(-16.8695679518648,13.5743278631276,
131.273876133887)) ;
#152336 = CARTESIAN_POINT('Ctrl Pts',(-16.8850187674673,13.8554587804339,
131.352236081223)) ;
#152337 = CARTESIAN_POINT('Ctrl Pts',(-16.9233899892215,14.103739100914,131.497307260457)) ;
#152338 = CARTESIAN_POINT('Ctrl Pts',(-16.9815525794946,14.3046990175591,
131.70035759611)) ;
#152339 = CARTESIAN_POINT('Ctrl Pts',(-17.0547401043487,14.4424188711516,
131.947366060444)) ;
#152340 = CARTESIAN_POINT('Ctrl Pts',(-17.1362824190426,14.5067209234145,
132.218584626412)) ;
#152341 = CARTESIAN_POINT('Ctrl Pts',(-17.2205230150152,14.4936392684735,
132.497872334383)) ;
#152342 = CARTESIAN_POINT('Ctrl Pts',(-17.2999675507863,14.404006740505,132.76301963)) ;
#152343 = CARTESIAN_POINT('Ctrl Pts',(-17.3687938432936,14.2433942656814,
132.99730827925)) ;
#152344 = CARTESIAN_POINT('Ctrl Pts',(-17.4206621252372,14.0252993056693,
133.181832423558)) ;
#152345 = CARTESIAN_POINT('Ctrl Pts',(-17.4518062177166,13.7626963119846,
133.306025850587)) ;
#152346 = CARTESIAN_POINT('Ctrl Pts',(-17.4588018749284,13.4766513624265,
133.3595520989)) ;
#152347 = CARTESIAN_POINT('Ctrl Pts',(-17.4407196010973,13.1866966293381,
133.339828540076)) ;
#152348 = CARTESIAN_POINT('Ctrl Pts',(-17.3976621744542,12.9123106961637,
133.247325290375)) ;
#152349 = CARTESIAN_POINT('Ctrl Pts',(-17.3328316521718,12.6769408805555,
133.090898057899)) ;
#152350 = CARTESIAN_POINT('Ctrl Pts',(-17.2494627622651,12.4935889535621,
132.880470073151)) ;
#152351 = CARTESIAN_POINT('Ctrl Pts',(-17.152618226233,12.3766908568814,132.630777552473)) ;
#152352 = CARTESIAN_POINT('Ctrl Pts',(-17.049231423334,12.3352383862452,132.361846606225)) ;
#152353 = CARTESIAN_POINT('Ctrl Pts',(-16.9457336891591,12.3713736006973,
132.092556286143)) ;
#152354 = CARTESIAN_POINT('Ctrl Pts',(-16.8484161060952,12.4827590293817,
131.841396897906)) ;
#152355 = CARTESIAN_POINT('Ctrl Pts',(-16.7634777794498,12.6627224306716,
131.626558702344)) ;
#152356 = CARTESIAN_POINT('Ctrl Pts',(-16.6972681323854,12.8955397849013,
131.466150815898)) ;
#152357 = CARTESIAN_POINT('Ctrl Pts',(-16.652840547036,13.1663558963296,131.369445368094)) ;
#152358 = CARTESIAN_POINT('Ctrl Pts',(-16.6328908225603,13.4563321062043,
131.344330530745)) ;
#152359 = CARTESIAN_POINT('Ctrl Pts',(-16.6382111416064,13.74354179735,131.392991362756)) ;
#152360 = CARTESIAN_POINT('Ctrl Pts',(-16.6676592322395,14.007863745204,131.512146621969)) ;
#152361 = CARTESIAN_POINT('Ctrl Pts',(-16.7182928746253,14.2299792391956,
131.693135937676)) ;
#152362 = CARTESIAN_POINT('Ctrl Pts',(-16.7859878307255,14.3948659481182,
131.924049786769)) ;
#152363 = CARTESIAN_POINT('Ctrl Pts',(-16.8651153132331,14.4898740802148,
132.188374983265)) ;
#152364 = CARTESIAN_POINT('Ctrl Pts',(-16.9488778829896,14.5084149248409,
132.466110688147)) ;
#152365 = CARTESIAN_POINT('Ctrl Pts',(-17.0311885247318,14.4492459338564,
132.739733964955)) ;
#152366 = CARTESIAN_POINT('Ctrl Pts',(-17.104950151554,14.316609488643,132.988318108268)) ;
#152367 = CARTESIAN_POINT('Ctrl Pts',(-17.1643724443007,14.1198900556279,
133.195042593654)) ;
#152368 = CARTESIAN_POINT('Ctrl Pts',(-17.2043618345605,13.8734079349303,
133.344971495627)) ;
#152369 = CARTESIAN_POINT('Ctrl Pts',(-17.2214102827416,13.5947694158123,
133.42787905469)) ;
#152370 = CARTESIAN_POINT('Ctrl Pts',(-17.2135302438731,13.3033325180628,
133.438020470237)) ;
#152371 = CARTESIAN_POINT('Ctrl Pts',(-17.1805025277542,13.0207084742087,
133.374676701685)) ;
#152372 = CARTESIAN_POINT('Ctrl Pts',(-17.124234300538,12.767628690545,133.243341451459)) ;
#152373 = CARTESIAN_POINT('Ctrl Pts',(-17.0476257592213,12.5604751539345,
133.052712263167)) ;
#152374 = CARTESIAN_POINT('Ctrl Pts',(-16.9553890051503,12.4152916729436,
132.816483612565)) ;
#152375 = CARTESIAN_POINT('Ctrl Pts',(-16.8542709676215,12.3428120631862,
132.554100291461)) ;
#152376 = CARTESIAN_POINT('Ctrl Pts',(-16.7494730831066,12.3473797413046,
132.281194465277)) ;
#152377 = CARTESIAN_POINT('Ctrl Pts',(-16.6487943422117,12.4294695368143,
132.020223589768)) ;
#152378 = CARTESIAN_POINT('Ctrl Pts',(-16.5588158738871,12.5816148375682,
131.790339248201)) ;
#152379 = CARTESIAN_POINT('Ctrl Pts',(-16.4842129576639,12.7949907280796,
131.605591372129)) ;
#152380 = CARTESIAN_POINT('Ctrl Pts',(-16.4302842435271,13.054101177031,131.481287531456)) ;
#152381 = CARTESIAN_POINT('Ctrl Pts',(-16.4003618883851,13.3386274126212,
131.426981031138)) ;
#152382 = CARTESIAN_POINT('Ctrl Pts',(-16.3954982522069,13.6281884734652,
131.445764473398)) ;
#152383 = CARTESIAN_POINT('Ctrl Pts',(-16.4153244875857,13.9042249218154,
131.536802751734)) ;
#152384 = CARTESIAN_POINT('Ctrl Pts',(-16.4579192874622,14.1463903457502,
131.694429834647)) ;
#152385 = CARTESIAN_POINT('Ctrl Pts',(-16.519604946235,14.3364819716926,131.907871784003)) ;
#152386 = CARTESIAN_POINT('Ctrl Pts',(-16.5941877045133,14.4598817702337,
132.158628290576)) ;
#152387 = CARTESIAN_POINT('Ctrl Pts',(-16.6772180078865,14.5104486170863,
132.434425087988)) ;
#152388 = CARTESIAN_POINT('Ctrl Pts',(-16.7610712369098,14.4822486369166,
132.712559593312)) ;
#152389 = CARTESIAN_POINT('Ctrl Pts',(-16.8386672352436,14.3791733041028,
132.97219580738)) ;
#152390 = CARTESIAN_POINT('Ctrl Pts',(-16.9049174530084,14.2063740303146,
133.199006100538)) ;
#152391 = CARTESIAN_POINT('Ctrl Pts',(-16.9532362150924,13.9777765864427,
133.373293310572)) ;
#152392 = CARTESIAN_POINT('Ctrl Pts',(-16.9798528341138,13.7109259499415,
133.484028399788)) ;
#152393 = CARTESIAN_POINT('Ctrl Pts',(-16.9822174695309,13.4211174151953,
133.524197897855)) ;
#152394 = CARTESIAN_POINT('Ctrl Pts',(-16.9593603734184,13.1336909339448,
133.490426214311)) ;
#152395 = CARTESIAN_POINT('Ctrl Pts',(-16.9122699848515,12.8658812639418,
133.385975367206)) ;
#152396 = CARTESIAN_POINT('Ctrl Pts',(-16.8429275372481,12.6367690190525,
133.216731683706)) ;
#152397 = CARTESIAN_POINT('Ctrl Pts',(-16.7566414738858,12.4658337897599,
132.997733929609)) ;
#152398 = CARTESIAN_POINT('Ctrl Pts',(-16.6584445847538,12.3631245211514,
132.743942914283)) ;
#152399 = CARTESIAN_POINT('Ctrl Pts',(-16.5545911413088,12.3360466241608,
132.473621289443)) ;
#152400 = CARTESIAN_POINT('Ctrl Pts',(-16.4514231221753,12.3868688002356,
132.205414356226)) ;
#152401 = CARTESIAN_POINT('Ctrl Pts',(-16.3561369237034,12.5119418325269,
131.960173693308)) ;
#152402 = CARTESIAN_POINT('Ctrl Pts',(-16.2746048987367,12.7021783709845,
131.755117298832)) ;
#152403 = CARTESIAN_POINT('Ctrl Pts',(-16.2118058427217,12.9449353770794,
131.604890369302)) ;
#152404 = CARTESIAN_POINT('Ctrl Pts',(-16.1719673653937,13.2214383784226,
131.521650682401)) ;
#152405 = CARTESIAN_POINT('Ctrl Pts',(-16.1568634879724,13.5108147708277,
131.510491075186)) ;
#152406 = CARTESIAN_POINT('Ctrl Pts',(-16.1669300007681,13.7968084175674,
131.573203022695)) ;
#152407 = CARTESIAN_POINT('Ctrl Pts',(-16.2006569741179,14.0536576083437,
131.704754764011)) ;
#152408 = CARTESIAN_POINT('Ctrl Pts',(-16.254784608073,14.2659120564335,131.895928413579)) ;
#152409 = CARTESIAN_POINT('Ctrl Pts',(-16.3251935914364,14.4185012516542,
132.134813692496)) ;
#152410 = CARTESIAN_POINT('Ctrl Pts',(-16.4055493007845,14.4992712221482,
132.402638758212)) ;
#152411 = CARTESIAN_POINT('Ctrl Pts',(-16.4897480826034,14.5031360116066,
132.681750239267)) ;
#152412 = CARTESIAN_POINT('Ctrl Pts',(-16.5707620204115,14.4296202074177,
132.951505237183)) ;
#152413 = CARTESIAN_POINT('Ctrl Pts',(-16.6421991335516,14.2844131247839,
133.193261917155)) ;
#152414 = CARTESIAN_POINT('Ctrl Pts',(-16.6984700341114,14.0764755685082,
133.390876378768)) ;
#152415 = CARTESIAN_POINT('Ctrl Pts',(-16.7342912161991,13.8227947339683,
133.528581938243)) ;
#152416 = CARTESIAN_POINT('Ctrl Pts',(-16.7467556388197,13.5398702989391,
133.59814585037)) ;
#152417 = CARTESIAN_POINT('Ctrl Pts',(-16.7340724183047,13.2487717783427,
133.594219576124)) ;
#152418 = CARTESIAN_POINT('Ctrl Pts',(-16.6965212883533,12.9703362151756,
133.517627433161)) ;
#152419 = CARTESIAN_POINT('Ctrl Pts',(-16.6359937287517,12.7241092781338,
133.373940651091)) ;
#152420 = CARTESIAN_POINT('Ctrl Pts',(-16.5560795871543,12.5279171433205,
133.173632261453)) ;
#152421 = CARTESIAN_POINT('Ctrl Pts',(-16.4618411443677,12.3959938665945,
132.931466168076)) ;
#152422 = CARTESIAN_POINT('Ctrl Pts',(-16.3593827732272,12.3376260980812,
132.665255360874)) ;
#152423 = CARTESIAN_POINT('Ctrl Pts',(-16.2550385035652,12.3570497794023,
132.393594158916)) ;
#152424 = CARTESIAN_POINT('Ctrl Pts',(-16.1560569930776,12.4525559733436,
132.137489642659)) ;
#152425 = CARTESIAN_POINT('Ctrl Pts',(-16.0682112092327,12.6176036105847,
131.9139932347)) ;
#152426 = CARTESIAN_POINT('Ctrl Pts',(-15.9972052369213,12.8410947019102,
131.739774174027)) ;
#152427 = CARTESIAN_POINT('Ctrl Pts',(-15.9477710009751,13.1055203518464,
131.628457545108)) ;
#152428 = CARTESIAN_POINT('Ctrl Pts',(-15.9223966595682,13.3928980327512,
131.587457525944)) ;
#152429 = CARTESIAN_POINT('Ctrl Pts',(-15.9222756880834,13.6824543649216,
131.620230232659)) ;
#152430 = CARTESIAN_POINT('Ctrl Pts',(-15.9466295677973,13.9532692757644,
131.724475741057)) ;
#152431 = CARTESIAN_POINT('Ctrl Pts',(-15.9930649492766,14.1862511235797,
131.893256545959)) ;
#152432 = CARTESIAN_POINT('Ctrl Pts',(-16.0572774469947,14.3643962082537,
132.113884233036)) ;
#152433 = CARTESIAN_POINT('Ctrl Pts',(-16.1348869305229,14.4759024807437,
132.373959659061)) ;
#152434 = CARTESIAN_POINT('Ctrl Pts',(-16.2178601983213,14.5109062464403,
132.649271579231)) ;
#152435 = CARTESIAN_POINT('Ctrl Pts',(-16.3010573982548,14.4687351628052,
132.925452283273)) ;
#152436 = CARTESIAN_POINT('Ctrl Pts',(-16.3772524895357,14.351243796897,133.18118301111)) ;
#152437 = CARTESIAN_POINT('Ctrl Pts',(-16.4401554780105,14.1681343550178,
133.397975738382)) ;
#152438 = CARTESIAN_POINT('Ctrl Pts',(-16.4850310227968,13.9291093552066,
133.562448350169)) ;
#152439 = CARTESIAN_POINT('Ctrl Pts',(-16.5070926720565,13.6572015399983,
133.659816803159)) ;
#152440 = CARTESIAN_POINT('Ctrl Pts',(-16.5046943032788,13.3659146668707,
133.686064790888)) ;
#152441 = CARTESIAN_POINT('Ctrl Pts',(-16.4771547092974,13.0809591455927,
133.638599282157)) ;
#152442 = CARTESIAN_POINT('Ctrl Pts',(-16.4256137570119,12.8188859308948,
133.521201214271)) ;
#152443 = CARTESIAN_POINT('Ctrl Pts',(-16.3527339561376,12.5999510440463,
133.341543109138)) ;
#152444 = CARTESIAN_POINT('Ctrl Pts',(-16.2641281336111,12.4414984825018,
133.115647334815)) ;
#152445 = CARTESIAN_POINT('Ctrl Pts',(-16.1641430091743,12.3520343108791,
132.85671610708)) ;
#152446 = CARTESIAN_POINT('Ctrl Pts',(-16.0594698293865,12.3398054622105,
132.584157469235)) ;
#152447 = CARTESIAN_POINT('Ctrl Pts',(-15.9577980199829,12.4047865271677,
132.320144279598)) ;
#152448 = CARTESIAN_POINT('Ctrl Pts',(-15.8643756324851,12.5431933869583,
132.080444267518)) ;
#152449 = CARTESIAN_POINT('Ctrl Pts',(-15.7860699178347,12.7444965603529,
131.884816381687)) ;
#152450 = CARTESIAN_POINT('Ctrl Pts',(-15.7274833077799,12.9945025224571,
131.746812479205)) ;
#152451 = CARTESIAN_POINT('Ctrl Pts',(-15.6921182047523,13.2745329094811,
131.676561655677)) ;
#152452 = CARTESIAN_POINT('Ctrl Pts',(-15.6817523163213,13.5670626370277,
131.679561862218)) ;
#152453 = CARTESIAN_POINT('Ctrl Pts',(-15.6963153264075,13.8462370772247,
131.755016293096)) ;
#152454 = CARTESIAN_POINT('Ctrl Pts',(-15.7342967830937,14.0979241250953,
131.899230741437)) ;
#152455 = CARTESIAN_POINT('Ctrl Pts',(-15.7919436686276,14.2997383418867,
132.100703473067)) ;
#152456 = CARTESIAN_POINT('Ctrl Pts',(-15.8645031781154,14.4393312193764,
132.345773094754)) ;
#152457 = CARTESIAN_POINT('Ctrl Pts',(-15.9465184391645,14.5060643569228,
132.618629039297)) ;
#152458 = CARTESIAN_POINT('Ctrl Pts',(-16.0301677623958,14.4951758782706,
132.895935895831)) ;
#152459 = CARTESIAN_POINT('Ctrl Pts',(-16.1102104627669,14.4072623281432,
133.163000755797)) ;
#152460 = CARTESIAN_POINT('Ctrl Pts',(-16.1790779676799,14.2495039694875,
133.397213921694)) ;
#152461 = CARTESIAN_POINT('Ctrl Pts',(-16.2319003919638,14.0308221258824,
133.584830620202)) ;
#152462 = CARTESIAN_POINT('Ctrl Pts',(-16.2633270017823,13.7719100664948,
133.709489495124)) ;
#152463 = CARTESIAN_POINT('Ctrl Pts',(-16.2711876727272,13.4847456450531,
133.765738112161)) ;
#152464 = CARTESIAN_POINT('Ctrl Pts',(-16.253847194686,13.1955425031336,133.748069200693)) ;
#152465 = CARTESIAN_POINT('Ctrl Pts',(-16.2115198754741,12.9200552968874,
133.65773228028)) ;
#152466 = CARTESIAN_POINT('Ctrl Pts',(-16.147222084084,12.6831184385928,133.502892140705)) ;
#152467 = CARTESIAN_POINT('Ctrl Pts',(-16.064282599147,12.4980281206389,133.293729089209)) ;
#152468 = CARTESIAN_POINT('Ctrl Pts',(-15.9679392810076,12.3791543430107,
133.045434009803)) ;
#152469 = CARTESIAN_POINT('Ctrl Pts',(-15.8643595558364,12.3353503717386,
132.776040083288)) ;
#152470 = CARTESIAN_POINT('Ctrl Pts',(-15.7608810145636,12.3691099621928,
132.506761731086)) ;
#152471 = CARTESIAN_POINT('Ctrl Pts',(-15.6627255542582,12.4795856785055,
132.253375320536)) ;
#152472 = CARTESIAN_POINT('Ctrl Pts',(-15.5784730291827,12.6553361009926,
132.040088792181)) ;
#152473 = CARTESIAN_POINT('Ctrl Pts',(-15.5110293575352,12.8882259217544,
131.876334600156)) ;
#152474 = CARTESIAN_POINT('Ctrl Pts',(-15.4660114239873,13.1581921393272,
131.777882402057)) ;
#152475 = CARTESIAN_POINT('Ctrl Pts',(-15.4453153424862,13.4482190387101,
131.750625899504)) ;
#152476 = CARTESIAN_POINT('Ctrl Pts',(-15.4499239120655,13.7352663202425,
131.797145410483)) ;
#152477 = CARTESIAN_POINT('Ctrl Pts',(-15.4786708796544,14.0004787425337,
131.914245491789)) ;
#152478 = CARTESIAN_POINT('Ctrl Pts',(-15.528718936817,14.2242401467777,132.093531049238)) ;
#152479 = CARTESIAN_POINT('Ctrl Pts',(-15.5963327554751,14.391486003047,132.324353743837)) ;
#152480 = CARTESIAN_POINT('Ctrl Pts',(-15.6747831211035,14.4880341837757,
132.586510244365)) ;
#152481 = CARTESIAN_POINT('Ctrl Pts',(-15.7588156763009,14.5089767222778,
132.865167334381)) ;
#152482 = CARTESIAN_POINT('Ctrl Pts',(-15.8410228376495,14.4520807364783,
133.138385805997)) ;
#152483 = CARTESIAN_POINT('Ctrl Pts',(-15.9152233944989,14.3213934969356,
133.388297276998)) ;
#152484 = CARTESIAN_POINT('Ctrl Pts',(-15.9751021978438,14.126427628205,133.596336490836)) ;
#152485 = CARTESIAN_POINT('Ctrl Pts',(-16.0157883783172,13.8807880817665,
133.748352793927)) ;
#152486 = CARTESIAN_POINT('Ctrl Pts',(-16.0334719367804,13.6022566506269,
133.833171646611)) ;
#152487 = CARTESIAN_POINT('Ctrl Pts',(-16.0263427101219,13.3123739575692,
133.845337187169)) ;
#152488 = CARTESIAN_POINT('Ctrl Pts',(-15.9941097511416,13.0290004002489,
133.784332603085)) ;
#152489 = CARTESIAN_POINT('Ctrl Pts',(-15.9383247563886,12.7741270713226,
133.65449670321)) ;
#152490 = CARTESIAN_POINT('Ctrl Pts',(-15.8622768484471,12.5657352250487,
133.465472847607)) ;
#152491 = CARTESIAN_POINT('Ctrl Pts',(-15.7707760397584,12.4188762117679,
133.231275457079)) ;
#152492 = CARTESIAN_POINT('Ctrl Pts',(-15.6694610724198,12.3438128452305,
132.968446766761)) ;
#152493 = CARTESIAN_POINT('Ctrl Pts',(-15.5650490222749,12.3461025205116,
132.696542230689)) ;
#152494 = CARTESIAN_POINT('Ctrl Pts',(-15.4641117267899,12.4255735874937,
132.43482095437)) ;
#152495 = CARTESIAN_POINT('Ctrl Pts',(-15.3733010936375,12.5765456735502,
132.202668192957)) ;
#152496 = CARTESIAN_POINT('Ctrl Pts',(-15.2984189865204,12.7879286592572,
132.017014437685)) ;
#152497 = CARTESIAN_POINT('Ctrl Pts',(-15.243943520018,13.0448054046113,131.89098628761)) ;
#152498 = CARTESIAN_POINT('Ctrl Pts',(-15.2130872375626,13.329756321322,131.834065836623)) ;
#152499 = CARTESIAN_POINT('Ctrl Pts',(-15.207498078425,13.6201107178654,131.850804210703)) ;
#152500 = CARTESIAN_POINT('Ctrl Pts',(-15.226664565684,13.8967554382586,131.93990903969)) ;
#152501 = CARTESIAN_POINT('Ctrl Pts',(-15.2685096670752,14.1394983367384,
132.095250212473)) ;
#152502 = CARTESIAN_POINT('Ctrl Pts',(-15.3296325471033,14.3315001569242,
132.307040763849)) ;
#152503 = CARTESIAN_POINT('Ctrl Pts',(-15.4041948784221,14.4575222943013,
132.557868425866)) ;
#152504 = CARTESIAN_POINT('Ctrl Pts',(-15.4871845489021,14.5099977938908,
132.833577267545)) ;
#152505 = CARTESIAN_POINT('Ctrl Pts',(-15.5706474715052,14.4843800867397,
133.110384973781)) ;
#152506 = CARTESIAN_POINT('Ctrl Pts',(-15.6489358172198,14.3828781461486,
133.372231534079)) ;
#152507 = CARTESIAN_POINT('Ctrl Pts',(-15.7152215321923,14.212816168216,133.598953578525)) ;
#152508 = CARTESIAN_POINT('Ctrl Pts',(-15.7643324415315,13.9854781681749,
133.775621838138)) ;
#152509 = CARTESIAN_POINT('Ctrl Pts',(-15.7916807767753,13.7179644909653,
133.888670251454)) ;
#152510 = CARTESIAN_POINT('Ctrl Pts',(-15.7946921387686,13.4301920376034,
133.930530607513)) ;
#152511 = CARTESIAN_POINT('Ctrl Pts',(-15.7726967990617,13.1421055633853,
133.899307008492)) ;
#152512 = CARTESIAN_POINT('Ctrl Pts',(-15.725756949418,12.87150128464,133.795559990037)) ;
#152513 = CARTESIAN_POINT('Ctrl Pts',(-15.6577073073503,12.6436097991943,
133.629723531333)) ;
#152514 = CARTESIAN_POINT('Ctrl Pts',(-15.5716152896333,12.4698498437503,
133.411423269474)) ;
#152515 = CARTESIAN_POINT('Ctrl Pts',(-15.4736825799438,12.3651221856613,
133.158394352247)) ;
#152516 = CARTESIAN_POINT('Ctrl Pts',(-15.3697907387214,12.335692224637,132.887997751447)) ;
#152517 = CARTESIAN_POINT('Ctrl Pts',(-15.2664401785828,12.3844432071478,
132.619277578795)) ;
#152518 = CARTESIAN_POINT('Ctrl Pts',(-15.1710399074463,12.5072147901112,
132.373635971455)) ;
#152519 = CARTESIAN_POINT('Ctrl Pts',(-15.0889535850671,12.6957550150873,
132.166979770339)) ;
#152520 = CARTESIAN_POINT('Ctrl Pts',(-15.0255721551039,12.9372999479051,
132.01505517321)) ;
#152521 = CARTESIAN_POINT('Ctrl Pts',(-14.9850575690906,13.2121499543988,
131.929735608954)) ;
#152522 = CARTESIAN_POINT('Ctrl Pts',(-14.9691714974783,13.5032465104466,
131.91650779929)) ;
#152523 = CARTESIAN_POINT('Ctrl Pts',(-14.9783938577685,13.7871080328991,
131.976440567623)) ;
#152524 = CARTESIAN_POINT('Ctrl Pts',(-15.0115648784408,14.0469104745439,
132.106594492085)) ;
#152525 = CARTESIAN_POINT('Ctrl Pts',(-15.0651801887707,14.2605649124229,
132.296255586953)) ;
#152526 = CARTESIAN_POINT('Ctrl Pts',(-15.1354050179275,14.4153649488043,
132.534693807358)) ;
#152527 = CARTESIAN_POINT('Ctrl Pts',(-15.2152370606947,14.4978582783663,
132.800850624746)) ;
#152528 = CARTESIAN_POINT('Ctrl Pts',(-15.2994258322498,14.5041773990225,
133.079939121836)) ;
#152529 = CARTESIAN_POINT('Ctrl Pts',(-15.3806609287712,14.4329779197685,
133.350346880059)) ;
#152530 = CARTESIAN_POINT('Ctrl Pts',(-15.4527495072584,14.2890422314917,
133.594146581102)) ;
#152531 = CARTESIAN_POINT('Ctrl Pts',(-15.5093788401438,14.082779433517,133.79275764401)) ;
#152532 = CARTESIAN_POINT('Ctrl Pts',(-15.545753191267,13.8309337098099,133.931989144067)) ;
#152533 = CARTESIAN_POINT('Ctrl Pts',(-15.5589571408963,13.5483120187831,
134.003745938923)) ;
#152534 = CARTESIAN_POINT('Ctrl Pts',(-15.5470459162325,13.2574777531019,
134.002035659956)) ;
#152535 = CARTESIAN_POINT('Ctrl Pts',(-15.510131605999,12.9779697529959,133.92735890912)) ;
#152536 = CARTESIAN_POINT('Ctrl Pts',(-15.4504417667573,12.7311580251373,
133.786020643798)) ;
#152537 = CARTESIAN_POINT('Ctrl Pts',(-15.3706607271275,12.5323980592304,
133.586256423076)) ;
#152538 = CARTESIAN_POINT('Ctrl Pts',(-15.2770803375685,12.3989897288854,
133.345890363007)) ;
#152539 = CARTESIAN_POINT('Ctrl Pts',(-15.1745710010167,12.3382487603058,
133.079602207309)) ;
#152540 = CARTESIAN_POINT('Ctrl Pts',(-15.0705359722807,12.3552058083452,
132.808726876001)) ;
#152541 = CARTESIAN_POINT('Ctrl Pts',(-14.9706606470321,12.4490680703867,
132.550225448555)) ;
#152542 = CARTESIAN_POINT('Ctrl Pts',(-14.8824522342596,12.612854304799,132.325691498574)) ;
#152543 = CARTESIAN_POINT('Ctrl Pts',(-14.8113527265263,12.8333918295054,
132.150980279395)) ;
#152544 = CARTESIAN_POINT('Ctrl Pts',(-14.7610563805274,13.0975419155814,
132.037242671929)) ;
#152545 = CARTESIAN_POINT('Ctrl Pts',(-14.7349932181902,13.3843701567211,
131.99420597981)) ;
#152546 = CARTESIAN_POINT('Ctrl Pts',(-14.7341460984049,13.6749248626015,
132.024944556395)) ;
#152547 = CARTESIAN_POINT('Ctrl Pts',(-14.7579228982456,13.9463602578246,
132.127499501483)) ;
#152548 = CARTESIAN_POINT('Ctrl Pts',(-14.8035289837161,14.1798324379302,
132.293714438332)) ;
#152549 = CARTESIAN_POINT('Ctrl Pts',(-14.8677079251816,14.3606302769089,
132.514446261517)) ;
#152550 = CARTESIAN_POINT('Ctrl Pts',(-14.9443462637881,14.4733618864566,
132.771384751192)) ;
#152551 = CARTESIAN_POINT('Ctrl Pts',(-15.0280034573494,14.5110756600993,
133.049012799316)) ;
#152552 = CARTESIAN_POINT('Ctrl Pts',(-15.1108313580727,14.4709889009811,
133.323927299789)) ;
#152553 = CARTESIAN_POINT('Ctrl Pts',(-15.1874906865422,14.3556941984043,
133.581070483478)) ;
#152554 = CARTESIAN_POINT('Ctrl Pts',(-15.2510153385486,14.1731666486328,
133.79982111375)) ;
#152555 = CARTESIAN_POINT('Ctrl Pts',(-15.2960503606692,13.9378584167298,
133.964426013949)) ;
#152556 = CARTESIAN_POINT('Ctrl Pts',(-15.3190310826371,13.6656355311939,
134.064636189014)) ;
#152557 = CARTESIAN_POINT('Ctrl Pts',(-15.3173445451022,13.3744563081115,
134.092966610367)) ;
#152558 = CARTESIAN_POINT('Ctrl Pts',(-15.2904580609234,13.0885611803192,
134.047472889722)) ;
#152559 = CARTESIAN_POINT('Ctrl Pts',(-15.2396747814133,12.8263306498725,
133.932194970172)) ;
#152560 = CARTESIAN_POINT('Ctrl Pts',(-15.1677163389787,12.6063807769631,
133.755109558956)) ;
#152561 = CARTESIAN_POINT('Ctrl Pts',(-15.0788943634793,12.4447492933123,
133.528822932428)) ;
#152562 = CARTESIAN_POINT('Ctrl Pts',(-14.9791253222199,12.3535025882306,
133.270511156007)) ;
#152563 = CARTESIAN_POINT('Ctrl Pts',(-14.8746674650902,12.3391045054194,
132.998527191728)) ;
#152564 = CARTESIAN_POINT('Ctrl Pts',(-14.7728141849366,12.4018104241151,
132.733985657383)) ;
#152565 = CARTESIAN_POINT('Ctrl Pts',(-14.6787517401919,12.5389586489687,
132.49253663729)) ;
#152566 = CARTESIAN_POINT('Ctrl Pts',(-14.6003862698118,12.7377764458565,
132.296567507347)) ;
#152567 = CARTESIAN_POINT('Ctrl Pts',(-14.5411439660413,12.9863019722805,
132.156626084833)) ;
#152568 = CARTESIAN_POINT('Ctrl Pts',(-14.5050286674343,13.2660338630659,
132.084222246459)) ;
#152569 = CARTESIAN_POINT('Ctrl Pts',(-14.4938897468974,13.5582232268191,
132.08492344046)) ;
#152570 = CARTESIAN_POINT('Ctrl Pts',(-14.507818431321,13.8387404070693,132.158622706454)) ;
#152571 = CARTESIAN_POINT('Ctrl Pts',(-14.5449327754259,14.0904925183414,
132.300141702221)) ;
#152572 = CARTESIAN_POINT('Ctrl Pts',(-14.6025167026814,14.2955136011611,
132.501693163721)) ;
#152573 = CARTESIAN_POINT('Ctrl Pts',(-14.6743979140284,14.4360006812449,
132.744601960421)) ;
#152574 = CARTESIAN_POINT('Ctrl Pts',(-14.7560190059001,14.5051702931602,
133.016232266989)) ;
#152575 = CARTESIAN_POINT('Ctrl Pts',(-14.8399788108669,14.4966323764384,
133.29455720462)) ;
#152576 = CARTESIAN_POINT('Ctrl Pts',(-14.92026343514,14.4108291399258,133.562335509995)) ;
#152577 = CARTESIAN_POINT('Ctrl Pts',(-14.9895377292265,14.2547209501546,
133.797763255438)) ;
#152578 = CARTESIAN_POINT('Ctrl Pts',(-15.0426869064103,14.0388606089928,
133.986156454842)) ;
#152579 = CARTESIAN_POINT('Ctrl Pts',(-15.0750262925721,13.779405578044,134.113692915164)) ;
#152580 = CARTESIAN_POINT('Ctrl Pts',(-15.0835065338818,13.4926641580088,
134.171741504609)) ;
#152581 = CARTESIAN_POINT('Ctrl Pts',(-15.0668941196817,13.2038302112353,
134.156144137311)) ;
#152582 = CARTESIAN_POINT('Ctrl Pts',(-15.0254043328273,12.9280759931688,
134.068184900734)) ;
#152583 = CARTESIAN_POINT('Ctrl Pts',(-14.9614251335503,12.6887447492448,
133.914424357805)) ;
#152584 = CARTESIAN_POINT('Ctrl Pts',(-14.8789170489459,12.5022966343227,
133.706505074034)) ;
#152585 = CARTESIAN_POINT('Ctrl Pts',(-14.7832955283864,12.381763978882,133.460180040676)) ;
#152586 = CARTESIAN_POINT('Ctrl Pts',(-14.6794737714671,12.3354318114705,
133.190193795545)) ;
#152587 = CARTESIAN_POINT('Ctrl Pts',(-14.5760954726489,12.3672035513488,
132.921157086038)) ;
#152588 = CARTESIAN_POINT('Ctrl Pts',(-14.4781651153176,12.474426481286,132.668233520948)) ;
#152589 = CARTESIAN_POINT('Ctrl Pts',(-14.3924892268079,12.6503068829769,
132.451164645272)) ;
#152590 = CARTESIAN_POINT('Ctrl Pts',(-14.3248849840194,12.8812481424524,
132.28680518042)) ;
#152591 = CARTESIAN_POINT('Ctrl Pts',(-14.2792429233544,13.1494231082653,
132.186430077652)) ;
#152592 = CARTESIAN_POINT('Ctrl Pts',(-14.2577333010081,13.4405328283774,
132.156949660664)) ;
#152593 = CARTESIAN_POINT('Ctrl Pts',(-14.2616812486159,13.7272524095848,
132.201463654968)) ;
#152594 = CARTESIAN_POINT('Ctrl Pts',(-14.2897398061011,13.9933197786215,
132.316545259697)) ;
#152595 = CARTESIAN_POINT('Ctrl Pts',(-14.3391869583318,14.2183989061991,
132.494053529779)) ;
#152596 = CARTESIAN_POINT('Ctrl Pts',(-14.4064273444875,14.3876287517767,
132.723811096672)) ;
#152597 = CARTESIAN_POINT('Ctrl Pts',(-14.4845242454382,14.4861870970875,
132.984890006035)) ;
#152598 = CARTESIAN_POINT('Ctrl Pts',(-14.5685621236943,14.5095212297327,
133.263587921165)) ;
#152599 = CARTESIAN_POINT('Ctrl Pts',(-14.6509971062007,14.4547287275128,
133.537507814222)) ;
#152600 = CARTESIAN_POINT('Ctrl Pts',(-14.7254748058222,14.3261105544631,
133.788208742009)) ;
#152601 = CARTESIAN_POINT('Ctrl Pts',(-14.7858563786915,14.1327425032557,
133.997729271496)) ;
#152602 = CARTESIAN_POINT('Ctrl Pts',(-14.8271232484926,13.8885306001009,
134.151412460096)) ;
#152603 = CARTESIAN_POINT('Ctrl Pts',(-14.8454990345243,13.6107524410049,
134.23824836838)) ;
#152604 = CARTESIAN_POINT('Ctrl Pts',(-14.8391902936134,13.3210542583331,
134.252793238962)) ;
#152605 = CARTESIAN_POINT('Ctrl Pts',(-14.8073003870615,13.0351251235983,
134.193044709195)) ;
#152606 = CARTESIAN_POINT('Ctrl Pts',(-14.7526013452373,12.7816150209491,
134.066072694138)) ;
#152607 = CARTESIAN_POINT('Ctrl Pts',(-14.6768446022253,12.5706518061014,
133.878035031889)) ;
#152608 = CARTESIAN_POINT('Ctrl Pts',(-14.5857344899984,12.422091900903,133.644955346922)) ;
#152609 = CARTESIAN_POINT('Ctrl Pts',(-14.4844870236026,12.3448083833829,
133.382365111388)) ;
#152610 = CARTESIAN_POINT('Ctrl Pts',(-14.3801271179856,12.3450375607664,
133.110594842367)) ;
#152611 = CARTESIAN_POINT('Ctrl Pts',(-14.2791586916205,12.4222140372622,
132.848729115977)) ;
#152612 = CARTESIAN_POINT('Ctrl Pts',(-14.1879207671711,12.5713072693593,
132.615345977553)) ;
#152613 = CARTESIAN_POINT('Ctrl Pts',(-14.1124789413141,12.7812068465324,
132.428068113172)) ;
#152614 = CARTESIAN_POINT('Ctrl Pts',(-14.0572435650617,13.0378486801572,
132.299917089332)) ;
#152615 = CARTESIAN_POINT('Ctrl Pts',(-14.0258214639467,13.3220972424203,
132.241311719484)) ;
#152616 = CARTESIAN_POINT('Ctrl Pts',(-14.0195168117333,13.6116477161832,
132.255856984885)) ;
#152617 = CARTESIAN_POINT('Ctrl Pts',(-14.0380429091883,13.8896343949454,
132.343170883447)) ;
#152618 = CARTESIAN_POINT('Ctrl Pts',(-14.0792096341859,14.1329048293709,
132.496445041414)) ;
#152619 = CARTESIAN_POINT('Ctrl Pts',(-14.139739650008,14.3266157424045,132.706473107546)) ;
#152620 = CARTESIAN_POINT('Ctrl Pts',(-14.2142389199618,14.4550271923226,
132.957226742653)) ;
#152621 = CARTESIAN_POINT('Ctrl Pts',(-14.2968257149156,14.5094869156272,
133.231648652557)) ;
#152622 = CARTESIAN_POINT('Ctrl Pts',(-14.3803943332945,14.4863255111229,
133.508781433968)) ;
#152623 = CARTESIAN_POINT('Ctrl Pts',(-14.4590295914748,14.3868080890416,
133.771682898577)) ;
#152624 = CARTESIAN_POINT('Ctrl Pts',(-14.5257824357843,14.2186053771164,
133.999775534479)) ;
#152625 = CARTESIAN_POINT('Ctrl Pts',(-14.5755477699378,13.9916146831158,
134.17848468615)) ;
#152626 = CARTESIAN_POINT('Ctrl Pts',(-14.6033802697407,13.727139474133,134.292681268961)) ;
#152627 = CARTESIAN_POINT('Ctrl Pts',(-14.6071598535866,13.437362164295,134.337061191346)) ;
#152628 = CARTESIAN_POINT('Ctrl Pts',(-14.5858835306319,13.1504054531947,
134.307774902983)) ;
#152629 = CARTESIAN_POINT('Ctrl Pts',(-14.5396141567361,12.8786465021209,
134.206021789804)) ;
#152630 = CARTESIAN_POINT('Ctrl Pts',(-14.4723055377556,12.6500332814425,
134.042260729231)) ;
#152631 = CARTESIAN_POINT('Ctrl Pts',(-14.386841995621,12.4743183897028,133.825754806519)) ;
#152632 = CARTESIAN_POINT('Ctrl Pts',(-14.2885171909372,12.3668547922141,
133.571800387653)) ;
#152633 = CARTESIAN_POINT('Ctrl Pts',(-14.1851936733311,12.335562941567,133.302903084124)) ;
#152634 = CARTESIAN_POINT('Ctrl Pts',(-14.0817812802112,12.3817108072099,
133.033981832815)) ;
#152635 = CARTESIAN_POINT('Ctrl Pts',(-13.9856777323266,12.502839824897,132.78641286331)) ;
#152636 = CARTESIAN_POINT('Ctrl Pts',(-13.9030779122353,12.690351441453,132.578318888232)) ;
#152637 = CARTESIAN_POINT('Ctrl Pts',(-13.8395678233593,12.9285059391321,
132.425739358382)) ;
#152638 = CARTESIAN_POINT('Ctrl Pts',(-13.7979805061536,13.2046731907038,
132.337546584743)) ;
#152639 = CARTESIAN_POINT('Ctrl Pts',(-13.7814999331058,13.4951333113011,
132.322515878226)) ;
#152640 = CARTESIAN_POINT('Ctrl Pts',(-13.7900411291653,13.779501210584,132.380474347949)) ;
#152641 = CARTESIAN_POINT('Ctrl Pts',(-13.8224120698119,14.0394108332529,
132.508163412887)) ;
#152642 = CARTESIAN_POINT('Ctrl Pts',(-13.8756204987681,14.2552141196343,
132.696731438701)) ;
#152643 = CARTESIAN_POINT('Ctrl Pts',(-13.9451061652378,14.4112842226695,
132.932851180889)) ;
#152644 = CARTESIAN_POINT('Ctrl Pts',(-14.0249337755901,14.49663037618,133.199097915004)) ;
#152645 = CARTESIAN_POINT('Ctrl Pts',(-14.1095239733355,14.5049768783044,
133.479521095915)) ;
#152646 = CARTESIAN_POINT('Ctrl Pts',(-14.190528704622,14.4360835729073,133.749098498737)) ;
#152647 = CARTESIAN_POINT('Ctrl Pts',(-14.262882528703,14.2946513922982,133.993611762097)) ;
#152648 = CARTESIAN_POINT('Ctrl Pts',(-14.320142163076,14.0899140100411,134.194101738961)) ;
#152649 = CARTESIAN_POINT('Ctrl Pts',(-14.3572698390389,13.8386917046902,
134.335604381356)) ;
#152650 = CARTESIAN_POINT('Ctrl Pts',(-14.3711303129086,13.5555692125345,
134.40939671493)) ;
#152651 = CARTESIAN_POINT('Ctrl Pts',(-14.3599713476779,13.2663901180779,
134.409692119641)) ;
#152652 = CARTESIAN_POINT('Ctrl Pts',(-14.3238194723227,12.9858847333076,
134.337276500168)) ;
#152653 = CARTESIAN_POINT('Ctrl Pts',(-14.2645948958419,12.7375102459871,
134.197360749458)) ;
#152654 = CARTESIAN_POINT('Ctrl Pts',(-14.1856165305326,12.5376376287816,
133.99982702238)) ;
#152655 = CARTESIAN_POINT('Ctrl Pts',(-14.0918860241884,12.4015826977934,
133.759196205742)) ;
#152656 = CARTESIAN_POINT('Ctrl Pts',(-13.9900202965247,12.3390360902595,
133.494624163606)) ;
#152657 = CARTESIAN_POINT('Ctrl Pts',(-13.885715431319,12.353575403094,133.223035536617)) ;
#152658 = CARTESIAN_POINT('Ctrl Pts',(-13.7857334521546,12.445274073871,132.964183894283)) ;
#152659 = CARTESIAN_POINT('Ctrl Pts',(-13.6971224342536,12.6067971683827,
132.738446959323)) ;
#152660 = CARTESIAN_POINT('Ctrl Pts',(-13.6250522220287,12.8274892534517,
132.561122252927)) ;
#152661 = CARTESIAN_POINT('Ctrl Pts',(-13.5744828714336,13.0891408927057,
132.446378055787)) ;
#152662 = CARTESIAN_POINT('Ctrl Pts',(-13.547610803124,13.375740122579,132.401005590542)) ;
#152663 = CARTESIAN_POINT('Ctrl Pts',(-13.5460300274622,13.6659116032671,
132.429533614848)) ;
#152664 = CARTESIAN_POINT('Ctrl Pts',(-13.5689788396593,13.9383430672958,
132.529666742918)) ;
#152665 = CARTESIAN_POINT('Ctrl Pts',(-13.6144336268274,14.1747318786697,
132.695698796106)) ;
#152666 = CARTESIAN_POINT('Ctrl Pts',(-13.6775346028895,14.3556000224366,
132.912954043635)) ;
#152667 = CARTESIAN_POINT('Ctrl Pts',(-13.7545609195232,14.4715471852787,
133.171333891809)) ;
#152668 = CARTESIAN_POINT('Ctrl Pts',(-13.8375768659038,14.5109306884899,
133.446859569505)) ;
#152669 = CARTESIAN_POINT('Ctrl Pts',(-13.9206587334674,14.4734197510009,
133.722575921601)) ;
#152670 = CARTESIAN_POINT('Ctrl Pts',(-13.9978549774587,14.3595613312843,
133.981405064546)) ;
#152671 = CARTESIAN_POINT('Ctrl Pts',(-14.0615326101247,14.179466171533,134.200463448237)) ;
#152672 = CARTESIAN_POINT('Ctrl Pts',(-14.1072808462681,13.9455181185487,
134.367173049305)) ;
#152673 = CARTESIAN_POINT('Ctrl Pts',(-14.1309695714097,13.6723045745694,
134.469654422256)) ;
#152674 = CARTESIAN_POINT('Ctrl Pts',(-14.1299543421008,13.3834915874396,
134.49969517271)) ;
#152675 = CARTESIAN_POINT('Ctrl Pts',(-14.103826459953,13.0966134068724,134.456484806691)) ;
#152676 = CARTESIAN_POINT('Ctrl Pts',(-14.0536044519402,12.8330521051259,
134.342891801889)) ;
#152677 = CARTESIAN_POINT('Ctrl Pts',(-13.9819755458689,12.6112324338377,
134.166849542491)) ;
#152678 = CARTESIAN_POINT('Ctrl Pts',(-13.8936140788126,12.4482429025448,
133.941863276773)) ;
#152679 = CARTESIAN_POINT('Ctrl Pts',(-13.7945442209898,12.3553252392396,
133.68544189025)) ;
#152680 = CARTESIAN_POINT('Ctrl Pts',(-13.6902421881023,12.3382107107946,
133.413874998198)) ;
#152681 = CARTESIAN_POINT('Ctrl Pts',(-13.5876395250276,12.3992481458877,
133.147344273434)) ;
#152682 = CARTESIAN_POINT('Ctrl Pts',(-13.4940363967205,12.5331204758664,
132.906945186053)) ;
#152683 = CARTESIAN_POINT('Ctrl Pts',(-13.4146406339235,12.7309387918669,
132.708143521826)) ;
#152684 = CARTESIAN_POINT('Ctrl Pts',(-13.3546400489765,12.9791524410526,
132.566084041094)) ;
#152685 = CARTESIAN_POINT('Ctrl Pts',(-13.3178749195276,13.2585790598106,
132.491812795079)) ;
#152686 = CARTESIAN_POINT('Ctrl Pts',(-13.3060921658157,13.5499397896395,
132.490544550928)) ;
#152687 = CARTESIAN_POINT('Ctrl Pts',(-13.319267039209,13.8311712407388,132.562048975874)) ;
#152688 = CARTESIAN_POINT('Ctrl Pts',(-13.3560394645477,14.0848085651835,
132.702709571436)) ;
#152689 = CARTESIAN_POINT('Ctrl Pts',(-13.4124077844404,14.2892041446737,
132.900320701676)) ;
#152690 = CARTESIAN_POINT('Ctrl Pts',(-13.4844837717321,14.4332159069687,
133.144089592404)) ;
#152691 = CARTESIAN_POINT('Ctrl Pts',(-13.5657740695195,14.5042073782218,
133.414672215616)) ;
#152692 = CARTESIAN_POINT('Ctrl Pts',(-13.6499188668072,14.4978850554144,
133.693611525571)) ;
#152693 = CARTESIAN_POINT('Ctrl Pts',(-13.7301300690243,14.4145534025925,
133.96105201458)) ;
#152694 = CARTESIAN_POINT('Ctrl Pts',(-13.7999841881705,14.2600830965558,
134.198257775645)) ;
#152695 = CARTESIAN_POINT('Ctrl Pts',(-13.8535974701144,14.0459659620245,
134.387963859614)) ;
#152696 = CARTESIAN_POINT('Ctrl Pts',(-13.8866069561238,13.7875807752627,
134.517459877776)) ;
#152697 = CARTESIAN_POINT('Ctrl Pts',(-13.8958448391708,13.5015008973902,
134.577698082975)) ;
#152698 = CARTESIAN_POINT('Ctrl Pts',(-13.8799187621032,13.2119712102584,
134.564171528529)) ;
#152699 = CARTESIAN_POINT('Ctrl Pts',(-13.8392809382772,12.9363053782512,
134.478593815727)) ;
#152700 = CARTESIAN_POINT('Ctrl Pts',(-13.7758444278724,12.6952736602129,
134.326473645072)) ;
#152701 = CARTESIAN_POINT('Ctrl Pts',(-13.6940162958856,12.507125678723,134.120477732686)) ;
#152702 = CARTESIAN_POINT('Ctrl Pts',(-13.5977907900013,12.3837628513247,
133.872694312529)) ;
#152703 = CARTESIAN_POINT('Ctrl Pts',(-13.4952077550757,12.3357954087756,
133.605958381013)) ;
#152704 = CARTESIAN_POINT('Ctrl Pts',(-13.3909244959306,12.3652711251859,
133.33454614811)) ;
#152705 = CARTESIAN_POINT('Ctrl Pts',(-13.2930291637441,12.4705156806676,
133.081632751708)) ;
#152706 = CARTESIAN_POINT('Ctrl Pts',(-13.2071658759881,12.6439184973371,
132.863918116231)) ;
#152707 = CARTESIAN_POINT('Ctrl Pts',(-13.1389101581012,12.8730354055636,
132.697626362)) ;
#152708 = CARTESIAN_POINT('Ctrl Pts',(-13.0923226075365,13.1424159445997,
132.594737929481)) ;
#152709 = CARTESIAN_POINT('Ctrl Pts',(-13.0702865542668,13.4306391754528,
132.563415021775)) ;
#152710 = CARTESIAN_POINT('Ctrl Pts',(-13.0733966131089,13.7191539441457,
132.605650335791)) ;
#152711 = CARTESIAN_POINT('Ctrl Pts',(-13.1008205861734,13.9861293896989,
132.718874470187)) ;
#152712 = CARTESIAN_POINT('Ctrl Pts',(-13.1498037441585,14.2128684001206,
132.89508138218)) ;
#152713 = CARTESIAN_POINT('Ctrl Pts',(-13.2163126321001,14.3833347965248,
133.122557153896)) ;
#152714 = CARTESIAN_POINT('Ctrl Pts',(-13.2945517934649,14.4845639099252,
133.384224457738)) ;
#152715 = CARTESIAN_POINT('Ctrl Pts',(-13.3782996834148,14.5099092471542,
133.66197841254)) ;
#152716 = CARTESIAN_POINT('Ctrl Pts',(-13.4610067103196,14.4573341215463,
133.936748595732)) ;
#152717 = CARTESIAN_POINT('Ctrl Pts',(-13.535792979438,14.3305258270945,134.188357582262)) ;
#152718 = CARTESIAN_POINT('Ctrl Pts',(-13.5964938791261,14.1393930806654,
134.398720829303)) ;
#152719 = CARTESIAN_POINT('Ctrl Pts',(-13.6384531516596,13.8963012865058,
134.554456038958)) ;
#152720 = CARTESIAN_POINT('Ctrl Pts',(-13.6575588644819,13.618527952916,134.64350061979)) ;
#152721 = CARTESIAN_POINT('Ctrl Pts',(-13.6518640795297,13.3290638567204,
134.659826711564)) ;
#152722 = CARTESIAN_POINT('Ctrl Pts',(-13.6210222993908,13.0445549081066,
134.602903919085)) ;
#152723 = CARTESIAN_POINT('Ctrl Pts',(-13.5665781809899,12.7876683953407,
134.476958833009)) ;
#152724 = CARTESIAN_POINT('Ctrl Pts',(-13.4911864112069,12.5753843248543,
134.290002560966)) ;
#152725 = CARTESIAN_POINT('Ctrl Pts',(-13.4007901006825,12.4255194566962,
134.05888370733)) ;
#152726 = CARTESIAN_POINT('Ctrl Pts',(-13.2997237377735,12.3459765628223,
133.796830310285)) ;
#152727 = CARTESIAN_POINT('Ctrl Pts',(-13.1954991747945,12.3439073333341,
133.52541389548)) ;
#152728 = CARTESIAN_POINT('Ctrl Pts',(-13.0941541677024,12.4188279963137,
133.262499854551)) ;
#152729 = CARTESIAN_POINT('Ctrl Pts',(-13.002205997662,12.5669347456838,133.027188569075)) ;
#152730 = CARTESIAN_POINT('Ctrl Pts',(-12.9267422753913,12.7740276750078,
132.839635132885)) ;
#152731 = CARTESIAN_POINT('Ctrl Pts',(-12.8706659445136,13.0302839963835,
132.709131418789)) ;
#152732 = CARTESIAN_POINT('Ctrl Pts',(-12.8386183811773,13.3133908418281,
132.648618515674)) ;
#152733 = CARTESIAN_POINT('Ctrl Pts',(-12.8315791622469,13.603463644202,132.661074904967)) ;
#152734 = CARTESIAN_POINT('Ctrl Pts',(-12.8492844367411,13.8813033828735,
132.745878981524)) ;
#152735 = CARTESIAN_POINT('Ctrl Pts',(-12.8901906349179,14.1277803353935,
132.898667421918)) ;
#152736 = CARTESIAN_POINT('Ctrl Pts',(-12.9502027043241,14.3222499491186,
133.107092668811)) ;
#152737 = CARTESIAN_POINT('Ctrl Pts',(-13.0241102247799,14.4521801137134,
133.356004116762)) ;
#152738 = CARTESIAN_POINT('Ctrl Pts',(-13.1064456796044,14.5090397013049,
133.629648846685)) ;
#152739 = CARTESIAN_POINT('Ctrl Pts',(-13.1904091031337,14.4879536383768,
133.908074847443)) ;
#152740 = CARTESIAN_POINT('Ctrl Pts',(-13.2691730073198,14.3907169193799,
134.171290632638)) ;
#152741 = CARTESIAN_POINT('Ctrl Pts',(-13.3365717682159,14.2230874926912,
134.401446847104)) ;
#152742 = CARTESIAN_POINT('Ctrl Pts',(-13.3862837725614,14.0008521290395,
134.579526433076)) ;
#152743 = CARTESIAN_POINT('Ctrl Pts',(-13.4151850077251,13.7343152663338,
134.697246128251)) ;
#152744 = CARTESIAN_POINT('Ctrl Pts',(-13.4196674461843,13.4474451530714,
134.74336669151)) ;
#152745 = CARTESIAN_POINT('Ctrl Pts',(-13.3989374427175,13.1575373599845,
134.716000021385)) ;
#152746 = CARTESIAN_POINT('Ctrl Pts',(-13.3538701206744,12.8878586186382,
134.617383543723)) ;
#152747 = CARTESIAN_POINT('Ctrl Pts',(-13.2866697814604,12.6555337160297,
134.454240239388)) ;
#152748 = CARTESIAN_POINT('Ctrl Pts',(-13.2016717965965,12.4784852863875,
134.239051541609)) ;
#152749 = CARTESIAN_POINT('Ctrl Pts',(-13.103660140851,12.3688435126028,133.986006271584)) ;
#152750 = CARTESIAN_POINT('Ctrl Pts',(-13.0001912147535,12.335379050582,133.716752546929)) ;
#152751 = CARTESIAN_POINT('Ctrl Pts',(-12.8968764365744,12.3794309050292,
133.448054757706)) ;
#152752 = CARTESIAN_POINT('Ctrl Pts',(-12.8007211226384,12.4979553005814,
133.200237570607)) ;
#152753 = CARTESIAN_POINT('Ctrl Pts',(-12.7173411751848,12.6843641512771,
132.989987119788)) ;
#152754 = CARTESIAN_POINT('Ctrl Pts',(-12.6533675978781,12.9208195190715,
132.835987884663)) ;
#152755 = CARTESIAN_POINT('Ctrl Pts',(-12.6110523141971,13.1965599156971,
132.745711948575)) ;
#152756 = CARTESIAN_POINT('Ctrl Pts',(-12.5938677361115,13.4854150034454,
132.728459041513)) ;
#152757 = CARTESIAN_POINT('Ctrl Pts',(-12.6016166796287,13.7715245103546,
132.784247690811)) ;
#152758 = CARTESIAN_POINT('Ctrl Pts',(-12.6334808333027,14.0329603333754,
132.910531351478)) ;
#152759 = CARTESIAN_POINT('Ctrl Pts',(-12.6860159227242,14.2495174070446,
133.097035811552)) ;
#152760 = CARTESIAN_POINT('Ctrl Pts',(-12.7550120282424,14.4077221355952,
133.331704202413)) ;
#152761 = CARTESIAN_POINT('Ctrl Pts',(-12.8352852858367,14.4954974794661,
133.599515576589)) ;
#152762 = CARTESIAN_POINT('Ctrl Pts',(-12.9190639071468,14.5058124227374,
133.877251814252)) ;
#152763 = CARTESIAN_POINT('Ctrl Pts',(-13.0006861903333,14.4390540160987,
134.148810770118)) ;
#152764 = CARTESIAN_POINT('Ctrl Pts',(-13.0734798970183,14.2988995016989,
134.394674718231)) ;
#152765 = CARTESIAN_POINT('Ctrl Pts',(-13.1310605574008,14.0959846822767,
134.59603545551)) ;
#152766 = CARTESIAN_POINT('Ctrl Pts',(-13.1686602075177,13.8467238077785,
134.738805253809)) ;
#152767 = CARTESIAN_POINT('Ctrl Pts',(-13.1832960063071,13.5651499595772,
134.814759605636)) ;
#152768 = CARTESIAN_POINT('Ctrl Pts',(-13.1728859358929,13.2745210705863,
134.817404454761)) ;
#152769 = CARTESIAN_POINT('Ctrl Pts',(-13.1372979957402,12.9930481847516,
134.746685223495)) ;
#152770 = CARTESIAN_POINT('Ctrl Pts',(-13.0788464460579,12.7442685275202,
134.608933005347)) ;
#152771 = CARTESIAN_POINT('Ctrl Pts',(-13.0004860021476,12.5428869624623,
134.413170014133)) ;
#152772 = CARTESIAN_POINT('Ctrl Pts',(-12.9071846487547,12.4047083280592,
134.173773807101)) ;
#152773 = CARTESIAN_POINT('Ctrl Pts',(-12.8051561028839,12.3396945526809,
133.90883173255)) ;
#152774 = CARTESIAN_POINT('Ctrl Pts',(-12.7008909970313,12.3521469576885,
133.637337257152)) ;
#152775 = CARTESIAN_POINT('Ctrl Pts',(-12.6009173642389,12.441314353945,133.378426035197)) ;
#152776 = CARTESIAN_POINT('Ctrl Pts',(-12.5117677396135,12.6011043288198,
133.151163527727)) ;
#152777 = CARTESIAN_POINT('Ctrl Pts',(-12.4393294114449,12.8194224397463,
132.97265105268)) ;
#152778 = CARTESIAN_POINT('Ctrl Pts',(-12.387790426931,13.0811434342732,132.85522288076)) ;
#152779 = CARTESIAN_POINT('Ctrl Pts',(-12.360228261411,13.3679217852881,132.807894792067)) ;
#152780 = CARTESIAN_POINT('Ctrl Pts',(-12.3579523050129,13.6574454003315,
132.834298017918)) ;
#152781 = CARTESIAN_POINT('Ctrl Pts',(-12.3801380175334,13.9304218890574,
132.932167779584)) ;
#152782 = CARTESIAN_POINT('Ctrl Pts',(-12.4250230602689,14.1686008595605,
133.096583317216)) ;
#152783 = CARTESIAN_POINT('Ctrl Pts',(-12.4878388913045,14.3514046814191,
133.313074404504)) ;
#152784 = CARTESIAN_POINT('Ctrl Pts',(-12.5640867721586,14.4688537010489,
133.568976881112)) ;
#152785 = CARTESIAN_POINT('Ctrl Pts',(-12.6473280614042,14.5110084065472,
133.845298914204)) ;
#152786 = CARTESIAN_POINT('Ctrl Pts',(-12.7306234368668,14.4754271659884,
134.121689851781)) ;
#152787 = CARTESIAN_POINT('Ctrl Pts',(-12.8078424891508,14.3641624802179,
134.38046802569)) ;
#152788 = CARTESIAN_POINT('Ctrl Pts',(-12.8722362238059,14.1852632695012,
134.601742519835)) ;
#152789 = CARTESIAN_POINT('Ctrl Pts',(-12.9184596429682,13.9526451401233,
134.769816657982)) ;
#152790 = CARTESIAN_POINT('Ctrl Pts',(-12.9427606566985,13.6818447118076,
134.873904342633)) ;
#152791 = CARTESIAN_POINT('Ctrl Pts',(-12.9426329031674,13.3926206452482,
134.906615051885)) ;
#152792 = CARTESIAN_POINT('Ctrl Pts',(-12.9170454040847,13.1038754923078,
134.865156068369)) ;
#152793 = CARTESIAN_POINT('Ctrl Pts',(-12.8675913433402,12.8403836297391,
134.753690916011)) ;
#152794 = CARTESIAN_POINT('Ctrl Pts',(-12.7967823441445,12.6175434576375,
134.579955954179)) ;
#152795 = CARTESIAN_POINT('Ctrl Pts',(-12.70868276548,12.4520178789147,134.355810149669)) ;
#152796 = CARTESIAN_POINT('Ctrl Pts',(-12.6093449823904,12.3567780608222,
134.098765452035)) ;
#152797 = CARTESIAN_POINT('Ctrl Pts',(-12.5056341234011,12.3376561109864,
133.828749759816)) ;
#152798 = CARTESIAN_POINT('Ctrl Pts',(-12.402751079868,12.3963494804203,133.561441007829)) ;
#152799 = CARTESIAN_POINT('Ctrl Pts',(-12.3088084112223,12.5282529228556,
133.320050046839)) ;
#152800 = CARTESIAN_POINT('Ctrl Pts',(-12.2289334019483,12.7243873042916,
133.119846376778)) ;
#152801 = CARTESIAN_POINT('Ctrl Pts',(-12.1683661165357,12.9708923918956,
132.976071926915)) ;
#152802 = CARTESIAN_POINT('Ctrl Pts',(-12.1308341182304,13.2502126197918,
132.899629391339)) ;
#152803 = CARTESIAN_POINT('Ctrl Pts',(-12.1182778756421,13.5400583828972,
132.895929792219)) ;
#152804 = CARTESIAN_POINT('Ctrl Pts',(-12.1307869570981,13.8239338286533,
132.965735493257)) ;
#152805 = CARTESIAN_POINT('Ctrl Pts',(-12.1668484142908,14.0777676729547,
133.104202368024)) ;
#152806 = CARTESIAN_POINT('Ctrl Pts',(-12.222772912384,14.2841378500946,133.300577303525)) ;
#152807 = CARTESIAN_POINT('Ctrl Pts',(-12.2942910489215,14.429815657766,133.542627629611)) ;
#152808 = CARTESIAN_POINT('Ctrl Pts',(-12.3756729115768,14.5033259168077,
133.813595342621)) ;
#152809 = CARTESIAN_POINT('Ctrl Pts',(-12.4597832810724,14.499135115111,134.092410952893)) ;
#152810 = CARTESIAN_POINT('Ctrl Pts',(-12.5402566051309,14.4177798325381,
134.360648411857)) ;
#152811 = CARTESIAN_POINT('Ctrl Pts',(-12.6102648440973,14.2657377102023,
134.59819459311)) ;
#152812 = CARTESIAN_POINT('Ctrl Pts',(-12.6646057115603,14.0527574173429,
134.790109616224)) ;
#152813 = CARTESIAN_POINT('Ctrl Pts',(-12.6982822917971,13.7942044324148,
134.921686113269)) ;
#152814 = CARTESIAN_POINT('Ctrl Pts',(-12.7081236290535,13.509972220369,134.983521067054)) ;
#152815 = CARTESIAN_POINT('Ctrl Pts',(-12.6929226435767,13.219834764377,134.972169824304)) ;
#152816 = CARTESIAN_POINT('Ctrl Pts',(-12.6529041959642,12.9433154987134,
134.888419817773)) ;
#152817 = CARTESIAN_POINT('Ctrl Pts',(-12.5899125810331,12.7008042356819,
134.737648548155)) ;
#152818 = CARTESIAN_POINT('Ctrl Pts',(-12.5088132067507,12.5118988342583,
134.533656568728)) ;
#152819 = CARTESIAN_POINT('Ctrl Pts',(-12.4134247671775,12.3867144480253,
134.288156510762)) ;
#152820 = CARTESIAN_POINT('Ctrl Pts',(-12.3103723850424,12.3359851161897,
134.020244487105)) ;
#152821 = CARTESIAN_POINT('Ctrl Pts',(-12.2060535029749,12.3634203970633,
133.748717660543)) ;
#152822 = CARTESIAN_POINT('Ctrl Pts',(-12.1079177935451,12.4663876358086,
133.495088507556)) ;
#152823 = CARTESIAN_POINT('Ctrl Pts',(-12.0212873996097,12.6389701182042,
133.275282296474)) ;
#152824 = CARTESIAN_POINT('Ctrl Pts',(-11.9528459850857,12.8657474577828,
133.108290126159)) ;
#152825 = CARTESIAN_POINT('Ctrl Pts',(-11.9054705654115,13.1346343436699,
133.003152675926)) ;
#152826 = CARTESIAN_POINT('Ctrl Pts',(-11.8903642795437,13.3266512177486,
132.98106317886)) ;
#152827 = CARTESIAN_POINT('Ctrl Pts',(-11.8869647971046,13.4226801736581,
132.982153164817)) ;
#152828 = CARTESIAN_POINT('',(-33.3489959095147,13.1551399285885,127.871927411069)) ;
#152829 = CARTESIAN_POINT('',(-22.6320187065114,12.9778651918053,131.474336592418)) ;
#152830 = CARTESIAN_POINT('Ctrl Pts',(-33.3489959095147,13.1551399285885,
127.871927411069)) ;
#152831 = CARTESIAN_POINT('Ctrl Pts',(-33.3482570091173,13.1489709609094,
127.870499856875)) ;
#152832 = CARTESIAN_POINT('Ctrl Pts',(-33.3362031847492,13.0505878441039,
127.846970056077)) ;
#152833 = CARTESIAN_POINT('Ctrl Pts',(-33.303456104594,12.8648900473044,127.774282508598)) ;
#152834 = CARTESIAN_POINT('Ctrl Pts',(-33.2347176391245,12.6378996894465,
127.606502631126)) ;
#152835 = CARTESIAN_POINT('Ctrl Pts',(-33.1484631699894,12.4661938442505,
127.38763758675)) ;
#152836 = CARTESIAN_POINT('Ctrl Pts',(-33.0496339239794,12.3629468779938,
127.132205946451)) ;
#152837 = CARTESIAN_POINT('Ctrl Pts',(-32.9461836982222,12.3360866578135,
126.862930995212)) ;
#152838 = CARTESIAN_POINT('Ctrl Pts',(-32.8428524780797,12.3868467815327,
126.594300512203)) ;
#152839 = CARTESIAN_POINT('Ctrl Pts',(-32.7476240151848,12.5118616193735,
126.34920621096)) ;
#152840 = CARTESIAN_POINT('Ctrl Pts',(-32.6660393235339,12.7022376314793,
126.14402042184)) ;
#152841 = CARTESIAN_POINT('Ctrl Pts',(-32.6034202579729,12.9442211340136,
125.994217779495)) ;
#152842 = CARTESIAN_POINT('Ctrl Pts',(-32.5634889320909,13.2203922331636,
125.91068247448)) ;
#152843 = CARTESIAN_POINT('Ctrl Pts',(-32.5482836171183,13.5109001041669,
125.899354456419)) ;
#152844 = CARTESIAN_POINT('Ctrl Pts',(-32.5583885908025,13.7967277450532,
125.962163306551)) ;
#152845 = CARTESIAN_POINT('Ctrl Pts',(-32.5919970185865,14.0531634695327,
126.093303648423)) ;
#152846 = CARTESIAN_POINT('Ctrl Pts',(-32.6462352627175,14.2659161102292,
126.2848763833)) ;
#152847 = CARTESIAN_POINT('Ctrl Pts',(-32.7164440425069,14.4182155312585,
126.52308858485)) ;
#152848 = CARTESIAN_POINT('Ctrl Pts',(-32.7970929244734,14.4993926065239,
126.791896512519)) ;
#152849 = CARTESIAN_POINT('Ctrl Pts',(-32.8812312900771,14.5030674016304,
127.070805593369)) ;
#152850 = CARTESIAN_POINT('Ctrl Pts',(-32.9621947752627,14.4296658181567,
127.340390412531)) ;
#152851 = CARTESIAN_POINT('Ctrl Pts',(-33.0336799536047,14.2842405620309,
127.582320067705)) ;
#152852 = CARTESIAN_POINT('Ctrl Pts',(-33.0898518257578,14.0768885755418,
127.779563482544)) ;
#152853 = CARTESIAN_POINT('Ctrl Pts',(-33.1258131095785,13.821937566696,127.917839903426)) ;
#152854 = CARTESIAN_POINT('Ctrl Pts',(-33.1381603359796,13.5404397832619,
127.986888146398)) ;
#152855 = CARTESIAN_POINT('Ctrl Pts',(-33.1255862370588,13.2491903771815,
127.98329800545)) ;
#152856 = CARTESIAN_POINT('Ctrl Pts',(-33.0878760919221,12.9699188880577,
127.906345203758)) ;
#152857 = CARTESIAN_POINT('Ctrl Pts',(-33.0275630545352,12.7245502986717,
127.763166970814)) ;
#152858 = CARTESIAN_POINT('Ctrl Pts',(-32.9475449968705,12.5279694687298,
127.562611942766)) ;
#152859 = CARTESIAN_POINT('Ctrl Pts',(-32.853484832887,12.3961377043517,127.320906369453)) ;
#152860 = CARTESIAN_POINT('Ctrl Pts',(-32.7506275244767,12.3376103677892,
127.053662058531)) ;
#152861 = CARTESIAN_POINT('Ctrl Pts',(-32.6467508382538,12.3569098529355,
126.783214181605)) ;
#152862 = CARTESIAN_POINT('Ctrl Pts',(-32.5472606088073,12.452769019898,126.525790390631)) ;
#152863 = CARTESIAN_POINT('Ctrl Pts',(-32.4595735399336,12.6179593573441,
126.30272348908)) ;
#152864 = CARTESIAN_POINT('Ctrl Pts',(-32.388745121808,12.8405880377693,126.12891456918)) ;
#152865 = CARTESIAN_POINT('Ctrl Pts',(-32.3390681420419,13.1065246421439,
126.017073858121)) ;
#152866 = CARTESIAN_POINT('Ctrl Pts',(-32.313898204756,13.3925179674891,125.976505647384)) ;
#152867 = CARTESIAN_POINT('Ctrl Pts',(-32.3136699242009,13.6819916651313,
126.008953177836)) ;
#152868 = CARTESIAN_POINT('Ctrl Pts',(-32.3381285657715,13.9537242418059,
126.113619428421)) ;
#152869 = CARTESIAN_POINT('Ctrl Pts',(-32.384536696511,14.1863734291659,126.28227784121)) ;
#152870 = CARTESIAN_POINT('Ctrl Pts',(-32.4487957222161,14.3643807985693,
126.503053049914)) ;
#152871 = CARTESIAN_POINT('Ctrl Pts',(-32.5258074280907,14.4754559850244,
126.761140801679)) ;
#152872 = CARTESIAN_POINT('Ctrl Pts',(-32.6094667487868,14.5110246739577,
127.038737149779)) ;
#152873 = CARTESIAN_POINT('Ctrl Pts',(-32.6924145513944,14.4687063588107,
127.314091355005)) ;
#152874 = CARTESIAN_POINT('Ctrl Pts',(-32.7687110106265,14.3514018815055,
127.570143149353)) ;
#152875 = CARTESIAN_POINT('Ctrl Pts',(-32.8317732094795,14.1671964752596,
127.787539429963)) ;
#152876 = CARTESIAN_POINT('Ctrl Pts',(-32.8762267217076,13.9308608041133,
127.950416591701)) ;
#152877 = CARTESIAN_POINT('Ctrl Pts',(-32.8985780094168,13.6570089999716,
128.048890973466)) ;
#152878 = CARTESIAN_POINT('Ctrl Pts',(-32.896157678737,13.3664659574419,128.074980037028)) ;
#152879 = CARTESIAN_POINT('Ctrl Pts',(-32.8685548522265,13.0805681472547,
128.027442701697)) ;
#152880 = CARTESIAN_POINT('Ctrl Pts',(-32.8170821736547,12.8190539470386,
127.91017574478)) ;
#152881 = CARTESIAN_POINT('Ctrl Pts',(-32.7441829163896,12.5999338423892,
127.73048258649)) ;
#152882 = CARTESIAN_POINT('Ctrl Pts',(-32.6555170250936,12.4413957528131,
127.504429482033)) ;
#152883 = CARTESIAN_POINT('Ctrl Pts',(-32.5554705400289,12.3520378265489,
127.245337069314)) ;
#152884 = CARTESIAN_POINT('Ctrl Pts',(-32.4511053019089,12.339734386482,126.973578302647)) ;
#152885 = CARTESIAN_POINT('Ctrl Pts',(-32.3490815539954,12.4049383167358,
126.708653969777)) ;
#152886 = CARTESIAN_POINT('Ctrl Pts',(-32.2559652828001,12.5429634979505,
126.469740198936)) ;
#152887 = CARTESIAN_POINT('Ctrl Pts',(-32.1775406776191,12.7443553986761,
126.273802702315)) ;
#152888 = CARTESIAN_POINT('Ctrl Pts',(-32.1189511785612,12.9943521537239,
126.135786155147)) ;
#152889 = CARTESIAN_POINT('Ctrl Pts',(-32.0836266547703,13.2741647768729,
126.065632995122)) ;
#152890 = CARTESIAN_POINT('Ctrl Pts',(-32.0731422430725,13.565720269456,126.068169777388)) ;
#152891 = CARTESIAN_POINT('Ctrl Pts',(-32.0878672761987,13.8474315556546,
126.144404645481)) ;
#152892 = CARTESIAN_POINT('Ctrl Pts',(-32.1256175280986,14.0971649669908,
126.287692127083)) ;
#152893 = CARTESIAN_POINT('Ctrl Pts',(-32.1834742057281,14.3002122843455,
126.489943063825)) ;
#152894 = CARTESIAN_POINT('Ctrl Pts',(-32.2561937622249,14.4394509674979,
126.73551422792)) ;
#152895 = CARTESIAN_POINT('Ctrl Pts',(-32.3374471159419,14.5058688200503,
127.005843081603)) ;
#152896 = CARTESIAN_POINT('Ctrl Pts',(-32.4217002826958,14.4952594831202,
127.285155611484)) ;
#152897 = CARTESIAN_POINT('Ctrl Pts',(-32.5017471426193,14.4071576912799,
127.552229665334)) ;
#152898 = CARTESIAN_POINT('Ctrl Pts',(-32.5706761898774,14.2488070341169,
127.786694114575)) ;
#152899 = CARTESIAN_POINT('Ctrl Pts',(-32.6230717724866,14.032332595662,127.972746797191)) ;
#152900 = CARTESIAN_POINT('Ctrl Pts',(-32.6548239115267,13.7715185673777,
128.098623777025)) ;
#152901 = CARTESIAN_POINT('Ctrl Pts',(-32.6626680714647,13.4849968555095,
128.154735100321)) ;
#152902 = CARTESIAN_POINT('Ctrl Pts',(-32.6450616243189,13.1936954317484,
128.136543946875)) ;
#152903 = CARTESIAN_POINT('Ctrl Pts',(-32.6032602463952,12.9217410981826,
128.047311789015)) ;
#152904 = CARTESIAN_POINT('Ctrl Pts',(-32.5386314820962,12.6826993167214,
127.891757560495)) ;
#152905 = CARTESIAN_POINT('Ctrl Pts',(-32.4554412889622,12.4976839220085,
127.681914464153)) ;
#152906 = CARTESIAN_POINT('Ctrl Pts',(-32.3596753952525,12.3794711428103,
127.435114332308)) ;
#152907 = CARTESIAN_POINT('Ctrl Pts',(-32.2558253838943,12.3351744196322,
127.165019558565)) ;
#152908 = CARTESIAN_POINT('Ctrl Pts',(-32.1520107530796,12.3695012763354,
126.894875973638)) ;
#152909 = CARTESIAN_POINT('Ctrl Pts',(-32.0548036090535,12.4786183736045,
126.643923371603)) ;
#152910 = CARTESIAN_POINT('Ctrl Pts',(-31.9697179472944,12.6556201701116,
126.428500311369)) ;
#152911 = CARTESIAN_POINT('Ctrl Pts',(-31.9024466959007,12.8885376957079,
126.26521267139)) ;
#152912 = CARTESIAN_POINT('Ctrl Pts',(-31.8574815700017,13.1578672277872,
126.166847085394)) ;
#152913 = CARTESIAN_POINT('Ctrl Pts',(-31.8367167778053,13.4488181058444,
126.139492583638)) ;
#152914 = CARTESIAN_POINT('Ctrl Pts',(-31.8414313820349,13.7357351250712,
126.186316118843)) ;
#152915 = CARTESIAN_POINT('Ctrl Pts',(-31.8700151821842,14.0000244154435,
126.30281009704)) ;
#152916 = CARTESIAN_POINT('Ctrl Pts',(-31.9203616130848,14.2248063693443,
126.483142763909)) ;
#152917 = CARTESIAN_POINT('Ctrl Pts',(-31.9873859775564,14.3907221531774,
126.711954484493)) ;
#152918 = CARTESIAN_POINT('Ctrl Pts',(-32.0662309963865,14.4880878052934,
126.975454295977)) ;
#152919 = CARTESIAN_POINT('Ctrl Pts',(-32.1500140049146,14.5090844515927,
127.253273584441)) ;
#152920 = CARTESIAN_POINT('Ctrl Pts',(-32.2328114906108,14.4517331277302,
127.528461364111)) ;
#152921 = CARTESIAN_POINT('Ctrl Pts',(-32.306599429151,14.3213873494252,127.777000865602)) ;
#152922 = CARTESIAN_POINT('Ctrl Pts',(-32.3665410586647,14.1266126254878,
127.985228303146)) ;
#152923 = CARTESIAN_POINT('Ctrl Pts',(-32.4072983071001,13.8801113803002,
128.137553257528)) ;
#152924 = CARTESIAN_POINT('Ctrl Pts',(-32.4248919159062,13.6025840232108,
128.221986639911)) ;
#152925 = CARTESIAN_POINT('Ctrl Pts',(-32.4177985341224,13.3122088978665,
128.234314532032)) ;
#152926 = CARTESIAN_POINT('Ctrl Pts',(-32.3854612722872,13.0284665595888,
128.173051822567)) ;
#152927 = CARTESIAN_POINT('Ctrl Pts',(-32.3297158719588,12.7739765033465,
128.043289524966)) ;
#152928 = CARTESIAN_POINT('Ctrl Pts',(-32.2536312710535,12.5655228915478,
127.854171141032)) ;
#152929 = CARTESIAN_POINT('Ctrl Pts',(-32.1621333883639,12.4188418488155,
127.619973715704)) ;
#152930 = CARTESIAN_POINT('Ctrl Pts',(-32.0610335191924,12.3438198182334,
127.357704488195)) ;
#152931 = CARTESIAN_POINT('Ctrl Pts',(-31.9562422849269,12.3461749880073,
127.084814084959)) ;
#152932 = CARTESIAN_POINT('Ctrl Pts',(-31.8555595514267,12.4256199459212,
126.823755799531)) ;
#152933 = CARTESIAN_POINT('Ctrl Pts',(-31.7646812381954,12.5766359900473,
126.591428395529)) ;
#152934 = CARTESIAN_POINT('Ctrl Pts',(-31.6897549709183,12.7882864475543,
126.405673808487)) ;
#152935 = CARTESIAN_POINT('Ctrl Pts',(-31.6353440859288,13.0452019382586,
126.279829886042)) ;
#152936 = CARTESIAN_POINT('Ctrl Pts',(-31.6045551307125,13.3293877258915,
126.223017390213)) ;
#152937 = CARTESIAN_POINT('Ctrl Pts',(-31.598929994185,13.6204035856812,126.239726726341)) ;
#152938 = CARTESIAN_POINT('Ctrl Pts',(-31.6181519561243,13.8971496153171,
126.329008321255)) ;
#152939 = CARTESIAN_POINT('Ctrl Pts',(-31.660032440097,14.1397539052331,126.4844492787)) ;
#152940 = CARTESIAN_POINT('Ctrl Pts',(-31.7210074180807,14.3313464702874,
126.695729086547)) ;
#152941 = CARTESIAN_POINT('Ctrl Pts',(-31.7956413070931,14.4574458616527,
126.94680082343)) ;
#152942 = CARTESIAN_POINT('Ctrl Pts',(-31.8782525153513,14.5099723944026,
127.221254124399)) ;
#152943 = CARTESIAN_POINT('Ctrl Pts',(-31.9622607746967,14.4843439695083,
127.499872427198)) ;
#152944 = CARTESIAN_POINT('Ctrl Pts',(-32.0404152099778,14.3827749410654,
127.761275810437)) ;
#152945 = CARTESIAN_POINT('Ctrl Pts',(-32.1067647607671,14.2124739950545,
127.988225629159)) ;
#152946 = CARTESIAN_POINT('Ctrl Pts',(-32.1557319181306,13.9855789386979,
128.164396849995)) ;
#152947 = CARTESIAN_POINT('Ctrl Pts',(-32.1830886305706,13.7185805864342,
128.27741749427)) ;
#152948 = CARTESIAN_POINT('Ctrl Pts',(-32.1861674536437,13.4303185636673,
128.319530923703)) ;
#152949 = CARTESIAN_POINT('Ctrl Pts',(-32.164067606359,13.1417758325219,128.288060327875)) ;
#152950 = CARTESIAN_POINT('Ctrl Pts',(-32.1174319130124,12.8725286043858,
128.185023246156)) ;
#152951 = CARTESIAN_POINT('Ctrl Pts',(-32.0491401802662,12.6435096258014,
128.018626363072)) ;
#152952 = CARTESIAN_POINT('Ctrl Pts',(-31.9632199754991,12.4701546223289,
127.800755651149)) ;
#152953 = CARTESIAN_POINT('Ctrl Pts',(-31.8651776863348,12.3650501876111,
127.547453264018)) ;
#152954 = CARTESIAN_POINT('Ctrl Pts',(-31.7609862185599,12.3357586674927,
127.276274914652)) ;
#152955 = CARTESIAN_POINT('Ctrl Pts',(-31.6580563102104,12.3843195509594,
127.008647533804)) ;
#152956 = CARTESIAN_POINT('Ctrl Pts',(-31.5623522569141,12.5073666683789,
126.762219617398)) ;
#152957 = CARTESIAN_POINT('Ctrl Pts',(-31.4804283317136,12.6958200369819,
126.55599240923)) ;
#152958 = CARTESIAN_POINT('Ctrl Pts',(-31.4171911262104,12.9363649293222,
126.404372140452)) ;
#152959 = CARTESIAN_POINT('Ctrl Pts',(-31.3765204454803,13.212046231595,126.318705695641)) ;
#152960 = CARTESIAN_POINT('Ctrl Pts',(-31.3605890149829,13.5022481067603,
126.305235943963)) ;
#152961 = CARTESIAN_POINT('Ctrl Pts',(-31.3699466511949,13.7884016128943,
126.365844507772)) ;
#152962 = CARTESIAN_POINT('Ctrl Pts',(-31.402839929772,14.045945075732,126.494887877481)) ;
#152963 = CARTESIAN_POINT('Ctrl Pts',(-31.456801839307,14.2610680704969,126.685797164984)) ;
#152964 = CARTESIAN_POINT('Ctrl Pts',(-31.5263791105061,14.4145624165552,
126.922033359285)) ;
#152965 = CARTESIAN_POINT('Ctrl Pts',(-31.6068029650713,14.4980852125695,
127.190187763467)) ;
#152966 = CARTESIAN_POINT('Ctrl Pts',(-31.6909497784616,14.5041312739862,
127.469125424148)) ;
#152967 = CARTESIAN_POINT('Ctrl Pts',(-31.7722616933248,14.4326962339747,
127.739802187408)) ;
#152968 = CARTESIAN_POINT('Ctrl Pts',(-31.8440399327869,14.289424830309,127.982545178335)) ;
#152969 = CARTESIAN_POINT('Ctrl Pts',(-31.9008586342929,14.0826507854277,
128.181809264848)) ;
#152970 = CARTESIAN_POINT('Ctrl Pts',(-31.9371644477761,13.8312291814697,
128.320780138694)) ;
#152971 = CARTESIAN_POINT('Ctrl Pts',(-31.9504192122518,13.5479805821752,
128.392761416066)) ;
#152972 = CARTESIAN_POINT('Ctrl Pts',(-31.9384428607775,13.2572981016289,
128.390846357411)) ;
#152973 = CARTESIAN_POINT('Ctrl Pts',(-31.9016603090654,12.9781391944844,
128.316499055668)) ;
#152974 = CARTESIAN_POINT('Ctrl Pts',(-31.8414344653115,12.7298471383749,
128.173831316095)) ;
#152975 = CARTESIAN_POINT('Ctrl Pts',(-31.7624693619783,12.5331718510569,
127.976098656417)) ;
#152976 = CARTESIAN_POINT('Ctrl Pts',(-31.6682896816273,12.3987050488903,
127.734214112554)) ;
#152977 = CARTESIAN_POINT('Ctrl Pts',(-31.5661584069127,12.3381977133859,
127.468894861423)) ;
#152978 = CARTESIAN_POINT('Ctrl Pts',(-31.4613121151811,12.3556285786372,
127.195919765139)) ;
#152979 = CARTESIAN_POINT('Ctrl Pts',(-31.3626542471411,12.448498640132,126.940567661376)) ;
#152980 = CARTESIAN_POINT('Ctrl Pts',(-31.2739963638957,12.6124651727369,
126.714860191145)) ;
#152981 = CARTESIAN_POINT('Ctrl Pts',(-31.2028733579617,12.8330193864531,
126.540078371683)) ;
#152982 = CARTESIAN_POINT('Ctrl Pts',(-31.1524099899045,13.0981216515098,
126.425973898796)) ;
#152983 = CARTESIAN_POINT('Ctrl Pts',(-31.1264884036244,13.3840423616995,
126.383240800023)) ;
#152984 = CARTESIAN_POINT('Ctrl Pts',(-31.1255526905879,13.6738043197191,
126.413632148392)) ;
#152985 = CARTESIAN_POINT('Ctrl Pts',(-31.1492407119047,13.9458856450603,
126.515980892251)) ;
#152986 = CARTESIAN_POINT('Ctrl Pts',(-31.1951906788803,14.1805609741337,
126.683399895541)) ;
#152987 = CARTESIAN_POINT('Ctrl Pts',(-31.2589322113538,14.3602096703021,
126.902625201214)) ;
#152988 = CARTESIAN_POINT('Ctrl Pts',(-31.336152907064,14.4737146563849,127.161521971997)) ;
#152989 = CARTESIAN_POINT('Ctrl Pts',(-31.4191607366893,14.510981736058,127.436983917868)) ;
#152990 = CARTESIAN_POINT('Ctrl Pts',(-31.5023202222332,14.4710234538019,
127.713002150618)) ;
#152991 = CARTESIAN_POINT('Ctrl Pts',(-31.5788150531214,14.3558611755068,
127.9695934644)) ;
#152992 = CARTESIAN_POINT('Ctrl Pts',(-31.6423459010436,14.1736059642118,
128.188348020273)) ;
#152993 = CARTESIAN_POINT('Ctrl Pts',(-31.6874883180192,13.9381264816024,
128.353301532308)) ;
#152994 = CARTESIAN_POINT('Ctrl Pts',(-31.7104598612239,13.665192099168,128.453567738071)) ;
#152995 = CARTESIAN_POINT('Ctrl Pts',(-31.7088598170554,13.3755914984187,
128.481967244671)) ;
#152996 = CARTESIAN_POINT('Ctrl Pts',(-31.6817723867748,13.0874857506397,
128.436147123456)) ;
#152997 = CARTESIAN_POINT('Ctrl Pts',(-31.6311222896079,12.8264337657975,
128.32111606456)) ;
#152998 = CARTESIAN_POINT('Ctrl Pts',(-31.5590254861687,12.6060974389448,
128.143694924089)) ;
#152999 = CARTESIAN_POINT('Ctrl Pts',(-31.4705496041744,12.4450313389733,
127.91828768914)) ;
#153000 = CARTESIAN_POINT('Ctrl Pts',(-31.3704536339561,12.3534666197661,
127.659136554107)) ;
#153001 = CARTESIAN_POINT('Ctrl Pts',(-31.2664260741019,12.3390029903486,
127.388267266672)) ;
#153002 = CARTESIAN_POINT('Ctrl Pts',(-31.1640074542676,12.4020392430349,
127.122262231831)) ;
#153003 = CARTESIAN_POINT('Ctrl Pts',(-31.0704546098695,12.5385711173323,
126.882123477286)) ;
#153004 = CARTESIAN_POINT('Ctrl Pts',(-30.9919375233747,12.737337324062,126.685748126109)) ;
#153005 = CARTESIAN_POINT('Ctrl Pts',(-30.9326059877163,12.9861206892308,
126.545580982005)) ;
#153006 = CARTESIAN_POINT('Ctrl Pts',(-30.8964828802307,13.2660910782566,
126.473182758033)) ;
#153007 = CARTESIAN_POINT('Ctrl Pts',(-30.8853353619794,13.5573227840952,
126.473749977841)) ;
#153008 = CARTESIAN_POINT('Ctrl Pts',(-30.8992181639316,13.8386952169897,
126.547405844888)) ;
#153009 = CARTESIAN_POINT('Ctrl Pts',(-30.9364490028324,14.0906007554108,
126.689305896974)) ;
#153010 = CARTESIAN_POINT('Ctrl Pts',(-30.993577379338,14.2945039762926,126.889303441531)) ;
#153011 = CARTESIAN_POINT('Ctrl Pts',(-31.0658785833472,14.4361574187858,
127.133657392973)) ;
#153012 = CARTESIAN_POINT('Ctrl Pts',(-31.1473678175875,14.5051117570611,
127.404837868273)) ;
#153013 = CARTESIAN_POINT('Ctrl Pts',(-31.2314101845586,14.496582620466,127.68344430737)) ;
#153014 = CARTESIAN_POINT('Ctrl Pts',(-31.3113999047549,14.4113394819302,
127.950224339128)) ;
#153015 = CARTESIAN_POINT('Ctrl Pts',(-31.3810275644355,14.2546479447355,
128.186843915728)) ;
#153016 = CARTESIAN_POINT('Ctrl Pts',(-31.434079388976,14.039143877786,128.374888028828)) ;
#153017 = CARTESIAN_POINT('Ctrl Pts',(-31.4664410188237,13.7793416572316,
128.502539340318)) ;
#153018 = CARTESIAN_POINT('Ctrl Pts',(-31.4749982660917,13.4941095874199,
128.560637934817)) ;
#153019 = CARTESIAN_POINT('Ctrl Pts',(-31.4582310109701,13.2026874966814,
128.544890911873)) ;
#153020 = CARTESIAN_POINT('Ctrl Pts',(-31.4169753439866,12.928833346161,128.457383735722)) ;
#153021 = CARTESIAN_POINT('Ctrl Pts',(-31.3527956487623,12.6885083712283,
128.303172142516)) ;
#153022 = CARTESIAN_POINT('Ctrl Pts',(-31.2705703901443,12.5026390795781,
128.0959611027)) ;
#153023 = CARTESIAN_POINT('Ctrl Pts',(-31.1745744230575,12.3816810236162,
127.848677279268)) ;
#153024 = CARTESIAN_POINT('Ctrl Pts',(-31.0714307037018,12.3354826595071,
127.580451601079)) ;
#153025 = CARTESIAN_POINT('Ctrl Pts',(-30.9672895160686,12.3671988660942,
127.309429336125)) ;
#153026 = CARTESIAN_POINT('Ctrl Pts',(-30.8693900237751,12.4748749581507,
127.056599017908)) ;
#153027 = CARTESIAN_POINT('Ctrl Pts',(-30.7841568236753,12.6498955190515,
126.840662152846)) ;
#153028 = CARTESIAN_POINT('Ctrl Pts',(-30.7165115975955,12.8801431332148,
126.67612667683)) ;
#153029 = CARTESIAN_POINT('Ctrl Pts',(-30.6705876552176,13.1504415297617,
126.575185235204)) ;
#153030 = CARTESIAN_POINT('Ctrl Pts',(-30.6492401911973,13.438739202615,126.545850310757)) ;
#153031 = CARTESIAN_POINT('Ctrl Pts',(-30.6531248486497,13.7280473502378,
126.590480521703)) ;
#153032 = CARTESIAN_POINT('Ctrl Pts',(-30.6811874381857,13.9932362064335,
126.705468605857)) ;
#153033 = CARTESIAN_POINT('Ctrl Pts',(-30.7307233901376,14.2186783745982,
126.88330032276)) ;
#153034 = CARTESIAN_POINT('Ctrl Pts',(-30.7976668939673,14.3872014330787,
127.112042032862)) ;
#153035 = CARTESIAN_POINT('Ctrl Pts',(-30.8759215226086,14.486216521528,127.373662762679)) ;
#153036 = CARTESIAN_POINT('Ctrl Pts',(-30.9599483085192,14.5095010567365,
127.652320679818)) ;
#153037 = CARTESIAN_POINT('Ctrl Pts',(-31.0423602583126,14.4548476689191,
127.926162766265)) ;
#153038 = CARTESIAN_POINT('Ctrl Pts',(-31.1170261636548,14.3259646517619,
128.177490633467)) ;
#153039 = CARTESIAN_POINT('Ctrl Pts',(-31.1774376241067,14.1320240566172,
128.38715540167)) ;
#153040 = CARTESIAN_POINT('Ctrl Pts',(-31.2184772814882,13.8890687487633,
128.540002184362)) ;
#153041 = CARTESIAN_POINT('Ctrl Pts',(-31.2369718788586,13.6109288487181,
128.62723857725)) ;
#153042 = CARTESIAN_POINT('Ctrl Pts',(-31.2305830637653,13.3205780973656,
128.64162358396)) ;
#153043 = CARTESIAN_POINT('Ctrl Pts',(-31.1988306507602,13.0356410236252,
128.582156307125)) ;
#153044 = CARTESIAN_POINT('Ctrl Pts',(-31.1439236012217,12.7811568557338,
128.454705635715)) ;
#153045 = CARTESIAN_POINT('Ctrl Pts',(-31.0684038299569,12.5709851276515,
128.267243241426)) ;
#153046 = CARTESIAN_POINT('Ctrl Pts',(-30.9772756205,12.4221766619671,128.03413250274)) ;
#153047 = CARTESIAN_POINT('Ctrl Pts',(-30.8759319496152,12.3447406812541,
127.771290965256)) ;
#153048 = CARTESIAN_POINT('Ctrl Pts',(-30.7712963261735,12.3451621602759,
127.498804673837)) ;
#153049 = CARTESIAN_POINT('Ctrl Pts',(-30.6706886680026,12.4221617733591,
127.237875690043)) ;
#153050 = CARTESIAN_POINT('Ctrl Pts',(-30.5793389036692,12.5713293574021,
127.00420358355)) ;
#153051 = CARTESIAN_POINT('Ctrl Pts',(-30.5039469378259,12.7811357471148,
126.817049360709)) ;
#153052 = CARTESIAN_POINT('Ctrl Pts',(-30.4488110435835,13.037385413305,126.689142569762)) ;
#153053 = CARTESIAN_POINT('Ctrl Pts',(-30.4173468141487,13.3202247802994,
126.630258735514)) ;
#153054 = CARTESIAN_POINT('Ctrl Pts',(-30.4109588954888,13.6126649497902,
126.644895127432)) ;
#153055 = CARTESIAN_POINT('Ctrl Pts',(-30.4294392941911,13.889109539137,126.731888107809)) ;
#153056 = CARTESIAN_POINT('Ctrl Pts',(-30.47077570761,14.1334576219234,126.885811226843)) ;
#153057 = CARTESIAN_POINT('Ctrl Pts',(-30.53102912446,14.3262010857029,127.094865661672)) ;
#153058 = CARTESIAN_POINT('Ctrl Pts',(-30.6058078949067,14.4552702241494,
127.346574791049)) ;
#153059 = CARTESIAN_POINT('Ctrl Pts',(-30.6883760016807,14.5094659873619,
127.620923977953)) ;
#153060 = CARTESIAN_POINT('Ctrl Pts',(-30.7718896570381,14.48627928254,127.897878479629)) ;
#153061 = CARTESIAN_POINT('Ctrl Pts',(-30.8505404170833,14.3867194330965,
128.16082928885)) ;
#153062 = CARTESIAN_POINT('Ctrl Pts',(-30.9172652518935,14.2183273389604,
128.388850744567)) ;
#153063 = CARTESIAN_POINT('Ctrl Pts',(-30.966927867041,13.9922441011096,128.567141543632)) ;
#153064 = CARTESIAN_POINT('Ctrl Pts',(-30.9948429554227,13.7260908863955,
128.681785518138)) ;
#153065 = CARTESIAN_POINT('Ctrl Pts',(-30.9986761317404,13.4392990683917,
128.725970798859)) ;
#153066 = CARTESIAN_POINT('Ctrl Pts',(-30.9771754995003,13.1491383926391,
128.696410048975)) ;
#153067 = CARTESIAN_POINT('Ctrl Pts',(-30.9313862314932,12.880138144259,128.595705294773)) ;
#153068 = CARTESIAN_POINT('Ctrl Pts',(-30.8633741700187,12.6488312040692,
128.430267551873)) ;
#153069 = CARTESIAN_POINT('Ctrl Pts',(-30.7783096718615,12.4746173052797,
128.214724190605)) ;
#153070 = CARTESIAN_POINT('Ctrl Pts',(-30.6802839201009,12.3669410581914,
127.961566303494)) ;
#153071 = CARTESIAN_POINT('Ctrl Pts',(-30.5761954681339,12.3355244467329,
127.690674965918)) ;
#153072 = CARTESIAN_POINT('Ctrl Pts',(-30.4731987242308,12.3818824637266,
127.42284013735)) ;
#153073 = CARTESIAN_POINT('Ctrl Pts',(-30.3773601675738,12.502442440452,127.175947943775)) ;
#153074 = CARTESIAN_POINT('Ctrl Pts',(-30.2945593439143,12.6900860359651,
126.967322197996)) ;
#153075 = CARTESIAN_POINT('Ctrl Pts',(-30.2309201264915,12.9290693621117,
126.814464075625)) ;
#153076 = CARTESIAN_POINT('Ctrl Pts',(-30.1896011311781,13.2033802627449,
126.726833819823)) ;
#153077 = CARTESIAN_POINT('Ctrl Pts',(-30.1729187517655,13.493885424346,126.711224329232)) ;
#153078 = CARTESIAN_POINT('Ctrl Pts',(-30.1814818466642,13.7798208359641,
126.769425110779)) ;
#153079 = CARTESIAN_POINT('Ctrl Pts',(-30.2139166442141,14.0398147256928,
126.897315524147)) ;
#153080 = CARTESIAN_POINT('Ctrl Pts',(-30.2672327260932,14.2555980954836,
127.086230738633)) ;
#153081 = CARTESIAN_POINT('Ctrl Pts',(-30.3364241626342,14.4112165057251,
127.321355815591)) ;
#153082 = CARTESIAN_POINT('Ctrl Pts',(-30.4169483545396,14.4969135755094,
127.589920286704)) ;
#153083 = CARTESIAN_POINT('Ctrl Pts',(-30.5006568417281,14.5049696810031,
127.867411820872)) ;
#153084 = CARTESIAN_POINT('Ctrl Pts',(-30.5821059141925,14.4360249735447,
128.13846691764)) ;
#153085 = CARTESIAN_POINT('Ctrl Pts',(-30.6543269887437,14.2945754362065,
128.382542123477)) ;
#153086 = CARTESIAN_POINT('Ctrl Pts',(-30.7116365732865,14.0897548858671,
128.583199406406)) ;
#153087 = CARTESIAN_POINT('Ctrl Pts',(-30.7486474004249,13.8387001375239,
128.724327683098)) ;
#153088 = CARTESIAN_POINT('Ctrl Pts',(-30.7626160375506,13.5574044598577,
128.79823198023)) ;
#153089 = CARTESIAN_POINT('Ctrl Pts',(-30.751280169492,13.2644130009093,128.798450590054)) ;
#153090 = CARTESIAN_POINT('Ctrl Pts',(-30.7152762753897,12.9862195730077,
128.726198614227)) ;
#153091 = CARTESIAN_POINT('Ctrl Pts',(-30.6559255495121,12.7371111819008,
128.586013158079)) ;
#153092 = CARTESIAN_POINT('Ctrl Pts',(-30.5772199975952,12.5380203242925,
128.389149798631)) ;
#153093 = CARTESIAN_POINT('Ctrl Pts',(-30.4833480932253,12.4015272632005,
128.148171071429)) ;
#153094 = CARTESIAN_POINT('Ctrl Pts',(-30.3812924082162,12.3389470103484,
127.883098879055)) ;
#153095 = CARTESIAN_POINT('Ctrl Pts',(-30.2769531606877,12.3537864997403,
127.611426962061)) ;
#153096 = CARTESIAN_POINT('Ctrl Pts',(-30.1774142848297,12.4449099176858,
127.353712328041)) ;
#153097 = CARTESIAN_POINT('Ctrl Pts',(-30.0884196313121,12.6072327563546,
127.127011108624)) ;
#153098 = CARTESIAN_POINT('Ctrl Pts',(-30.0168944583603,12.8259751420657,
126.950999128042)) ;
#153099 = CARTESIAN_POINT('Ctrl Pts',(-29.9658131020968,13.0894865209779,
126.835020394129)) ;
#153100 = CARTESIAN_POINT('Ctrl Pts',(-29.9390402950618,13.3763086244584,
126.789949510195)) ;
#153101 = CARTESIAN_POINT('Ctrl Pts',(-29.9374976893148,13.666102426872,126.818551688385)) ;
#153102 = CARTESIAN_POINT('Ctrl Pts',(-29.9603659689101,13.9378774393092,
126.918366530385)) ;
#153103 = CARTESIAN_POINT('Ctrl Pts',(-30.0058557147277,14.174793298913,127.084558461599)) ;
#153104 = CARTESIAN_POINT('Ctrl Pts',(-30.0690738202602,14.355667987911,127.302193672896)) ;
#153105 = CARTESIAN_POINT('Ctrl Pts',(-30.1455851444044,14.4711053294092,
127.558860146817)) ;
#153106 = CARTESIAN_POINT('Ctrl Pts',(-30.2290907276294,14.511170979715,127.836014853784)) ;
#153107 = CARTESIAN_POINT('Ctrl Pts',(-30.3124346958538,14.4729025341711,
128.112614820692)) ;
#153108 = CARTESIAN_POINT('Ctrl Pts',(-30.3888326028229,14.3605014183323,
128.368750566373)) ;
#153109 = CARTESIAN_POINT('Ctrl Pts',(-30.4531791538599,14.1789799497678,
128.590078616567)) ;
#153110 = CARTESIAN_POINT('Ctrl Pts',(-30.4986908853725,13.9453130755044,
128.756011357139)) ;
#153111 = CARTESIAN_POINT('Ctrl Pts',(-30.5223367702664,13.673613297581,128.858202384461)) ;
#153112 = CARTESIAN_POINT('Ctrl Pts',(-30.5214927257582,13.3843416477693,
128.888796839614)) ;
#153113 = CARTESIAN_POINT('Ctrl Pts',(-30.4951356796959,13.0956424787648,
128.845131685907)) ;
#153114 = CARTESIAN_POINT('Ctrl Pts',(-30.4451353943437,12.8335787485534,
128.73200501772)) ;
#153115 = CARTESIAN_POINT('Ctrl Pts',(-30.3735874311193,12.6116522531053,
128.556195762552)) ;
#153116 = CARTESIAN_POINT('Ctrl Pts',(-30.2853579635812,12.4486058050818,
128.33155990322)) ;
#153117 = CARTESIAN_POINT('Ctrl Pts',(-30.1858663129506,12.3551665981467,
128.074050595748)) ;
#153118 = CARTESIAN_POINT('Ctrl Pts',(-30.0815496988783,12.3383111368361,
127.802444396815)) ;
#153119 = CARTESIAN_POINT('Ctrl Pts',(-29.9791399961725,12.3991318667188,
127.536410522558)) ;
#153120 = CARTESIAN_POINT('Ctrl Pts',(-29.885250975789,12.5336133546432,127.2952913997)) ;
#153121 = CARTESIAN_POINT('Ctrl Pts',(-29.8062098846917,12.7304747525644,
127.097365942919)) ;
#153122 = CARTESIAN_POINT('Ctrl Pts',(-29.7459166115697,12.9801493565206,
126.954643707808)) ;
#153123 = CARTESIAN_POINT('Ctrl Pts',(-29.7094981424688,13.2569930870622,
126.881074054437)) ;
#153124 = CARTESIAN_POINT('Ctrl Pts',(-29.697485321225,13.5493201067258,126.879249155707)) ;
#153125 = CARTESIAN_POINT('Ctrl Pts',(-29.7107148915496,13.8310609228274,
126.950973130347)) ;
#153126 = CARTESIAN_POINT('Ctrl Pts',(-29.7473686079901,14.0843638099265,
127.091228525209)) ;
#153127 = CARTESIAN_POINT('Ctrl Pts',(-29.8039983073089,14.2896244491401,
127.289751241016)) ;
#153128 = CARTESIAN_POINT('Ctrl Pts',(-29.8758248177242,14.4330063116879,
127.5326649792)) ;
#153129 = CARTESIAN_POINT('Ctrl Pts',(-29.9571776043441,14.5042107415309,
127.803464708327)) ;
#153130 = CARTESIAN_POINT('Ctrl Pts',(-30.0412713276901,14.4979449999679,
128.082232149485)) ;
#153131 = CARTESIAN_POINT('Ctrl Pts',(-30.121694639328,14.4144601779744,128.350375838408)) ;
#153132 = CARTESIAN_POINT('Ctrl Pts',(-30.1915790917938,14.2595209902124,
128.587713560571)) ;
#153133 = CARTESIAN_POINT('Ctrl Pts',(-30.2450076010872,14.046214919979,128.776755103724)) ;
#153134 = CARTESIAN_POINT('Ctrl Pts',(-30.2780878046331,13.7868053449528,
128.906585374679)) ;
#153135 = CARTESIAN_POINT('Ctrl Pts',(-30.2872906950602,13.5027357390144,
128.966484763682)) ;
#153136 = CARTESIAN_POINT('Ctrl Pts',(-30.2713500951273,13.2114164567146,
128.953122045362)) ;
#153137 = CARTESIAN_POINT('Ctrl Pts',(-30.230627814723,12.9359342983456,128.86728322249)) ;
#153138 = CARTESIAN_POINT('Ctrl Pts',(-30.1672447422047,12.6951562018299,
128.715288751686)) ;
#153139 = CARTESIAN_POINT('Ctrl Pts',(-30.0854978465419,12.5073061272103,
128.509491429827)) ;
#153140 = CARTESIAN_POINT('Ctrl Pts',(-29.9896882822811,12.3841592686752,
128.262793679839)) ;
#153141 = CARTESIAN_POINT('Ctrl Pts',(-29.8866361087517,12.3356200239572,
127.994841190901)) ;
#153142 = CARTESIAN_POINT('Ctrl Pts',(-29.7820423738734,12.3655842279676,
127.722626897302)) ;
#153143 = CARTESIAN_POINT('Ctrl Pts',(-29.6846378874882,12.4702048591763,
127.470973299483)) ;
#153144 = CARTESIAN_POINT('Ctrl Pts',(-29.5982444318826,12.6448837976238,
127.251934053335)) ;
#153145 = CARTESIAN_POINT('Ctrl Pts',(-29.530484788473,12.872508423284,127.086857758343)) ;
#153146 = CARTESIAN_POINT('Ctrl Pts',(-29.4836133061575,13.1434988331289,
126.983345728084)) ;
#153147 = CARTESIAN_POINT('Ctrl Pts',(-29.4617927517553,13.4301737780494,
126.952467269919)) ;
#153148 = CARTESIAN_POINT('Ctrl Pts',(-29.4647728375027,13.7187795914099,
126.994328449619)) ;
#153149 = CARTESIAN_POINT('Ctrl Pts',(-29.4924039666026,13.9870154433738,
127.108324446431)) ;
#153150 = CARTESIAN_POINT('Ctrl Pts',(-29.5411722729436,14.2124398345738,
127.283727368873)) ;
#153151 = CARTESIAN_POINT('Ctrl Pts',(-29.6075895922723,14.3830654461858,
127.510923381855)) ;
#153152 = CARTESIAN_POINT('Ctrl Pts',(-29.6859780654117,14.4846609541733,
127.773091506423)) ;
#153153 = CARTESIAN_POINT('Ctrl Pts',(-29.7699711987632,14.5097913616969,
128.051659371141)) ;
#153154 = CARTESIAN_POINT('Ctrl Pts',(-29.8521599614632,14.4576093080194,
128.324704513275)) ;
#153155 = CARTESIAN_POINT('Ctrl Pts',(-29.9273378651692,14.3304831317374,
128.57761366537)) ;
#153156 = CARTESIAN_POINT('Ctrl Pts',(-29.9881011678196,14.1386183822934,
128.788232639006)) ;
#153157 = CARTESIAN_POINT('Ctrl Pts',(-30.0298088081978,13.8965846856625,
128.943079017119)) ;
#153158 = CARTESIAN_POINT('Ctrl Pts',(-30.048987740085,13.6198365630073,129.032230754272)) ;
#153159 = CARTESIAN_POINT('Ctrl Pts',(-30.0433213484704,13.3288844737818,
129.048809941996)) ;
#153160 = CARTESIAN_POINT('Ctrl Pts',(-30.0124680035273,13.0447399832046,
128.991813037362)) ;
#153161 = CARTESIAN_POINT('Ctrl Pts',(-29.958162147996,12.7881836368688,128.866220633411)) ;
#153162 = CARTESIAN_POINT('Ctrl Pts',(-29.8827371039613,12.5755910115287,
128.67919720058)) ;
#153163 = CARTESIAN_POINT('Ctrl Pts',(-29.7923817501949,12.4257574465567,
128.448186718166)) ;
#153164 = CARTESIAN_POINT('Ctrl Pts',(-29.6914548654442,12.3460112405744,
128.186501449005)) ;
#153165 = CARTESIAN_POINT('Ctrl Pts',(-29.5867020660159,12.3439532504127,
127.913710488866)) ;
#153166 = CARTESIAN_POINT('Ctrl Pts',(-29.485666657119,12.4188218900739,127.651602416161)) ;
#153167 = CARTESIAN_POINT('Ctrl Pts',(-29.3936759004092,12.5668341062151,
127.416175460721)) ;
#153168 = CARTESIAN_POINT('Ctrl Pts',(-29.3182301931701,12.7739565310488,
127.2286723812)) ;
#153169 = CARTESIAN_POINT('Ctrl Pts',(-29.2623086088496,13.0292275295923,
127.098504241357)) ;
#153170 = CARTESIAN_POINT('Ctrl Pts',(-29.2301243830033,13.3121167714202,
127.037580467898)) ;
#153171 = CARTESIAN_POINT('Ctrl Pts',(-29.2229734795966,13.6036711588795,
127.049873651472)) ;
#153172 = CARTESIAN_POINT('Ctrl Pts',(-29.2408639834952,13.8822010088686,
127.135317168003)) ;
#153173 = CARTESIAN_POINT('Ctrl Pts',(-29.2814175857852,14.126534024312,127.286789452504)) ;
#153174 = CARTESIAN_POINT('Ctrl Pts',(-29.341269933413,14.3215277156221,127.494747226261)) ;
#153175 = CARTESIAN_POINT('Ctrl Pts',(-29.4156496701704,14.4523872469144,
127.745252022521)) ;
#153176 = CARTESIAN_POINT('Ctrl Pts',(-29.4979993749135,14.509081269933,128.018936330148)) ;
#153177 = CARTESIAN_POINT('Ctrl Pts',(-29.5821194390776,14.4877530584647,
128.297884507417)) ;
#153178 = CARTESIAN_POINT('Ctrl Pts',(-29.6605015766084,14.3906972492053,
128.559841528178)) ;
#153179 = CARTESIAN_POINT('Ctrl Pts',(-29.7277325620602,14.2242127265294,
128.789368837068)) ;
#153180 = CARTESIAN_POINT('Ctrl Pts',(-29.7778622908604,14.0000453961231,
128.968956847515)) ;
#153181 = CARTESIAN_POINT('Ctrl Pts',(-29.8065930602879,13.7349941187306,
129.085980593616)) ;
#153182 = CARTESIAN_POINT('Ctrl Pts',(-29.8110647581583,13.4462938086935,
129.132290262238)) ;
#153183 = CARTESIAN_POINT('Ctrl Pts',(-29.7905149481192,13.1586524064852,
129.105179558969)) ;
#153184 = CARTESIAN_POINT('Ctrl Pts',(-29.7450251194424,12.8863235925418,
129.005657518442)) ;
#153185 = CARTESIAN_POINT('Ctrl Pts',(-29.6779688870286,12.6553854575325,
128.842782884932)) ;
#153186 = CARTESIAN_POINT('Ctrl Pts',(-29.5932822353585,12.4787538591612,
128.628403260321)) ;
#153187 = CARTESIAN_POINT('Ctrl Pts',(-29.4951432611704,12.3688114822916,
128.375032108495)) ;
#153188 = CARTESIAN_POINT('Ctrl Pts',(-29.3915755638739,12.3354319136936,
128.105522888968)) ;
#153189 = CARTESIAN_POINT('Ctrl Pts',(-29.2883737439491,12.3792576310417,
127.83711019449)) ;
#153190 = CARTESIAN_POINT('Ctrl Pts',(-29.1917010872287,12.4988398999205,
127.587984309591)) ;
#153191 = CARTESIAN_POINT('Ctrl Pts',(-29.1090972687786,12.6835118512005,
127.379683329034)) ;
#153192 = CARTESIAN_POINT('Ctrl Pts',(-29.0446608613966,12.9214923912795,
127.224563683631)) ;
#153193 = CARTESIAN_POINT('Ctrl Pts',(-29.0026163941945,13.1954916424955,
127.134859426664)) ;
#153194 = CARTESIAN_POINT('Ctrl Pts',(-28.985230945197,13.4865485670219,127.117276574287)) ;
#153195 = CARTESIAN_POINT('Ctrl Pts',(-28.9931808891691,13.772471589557,127.173641275195)) ;
#153196 = CARTESIAN_POINT('Ctrl Pts',(-29.0248180797672,14.0322259092952,
127.299049560001)) ;
#153197 = CARTESIAN_POINT('Ctrl Pts',(-29.0774225647813,14.2496185339524,
127.485847881482)) ;
#153198 = CARTESIAN_POINT('Ctrl Pts',(-29.1466584272716,14.4079186586772,
127.721302692546)) ;
#153199 = CARTESIAN_POINT('Ctrl Pts',(-29.2262609733389,14.495128940057,127.986882942297)) ;
#153200 = CARTESIAN_POINT('Ctrl Pts',(-29.310377688868,14.5060206783235,128.265744239721)) ;
#153201 = CARTESIAN_POINT('Ctrl Pts',(-29.3922415681972,14.4388851972431,
128.538108177024)) ;
#153202 = CARTESIAN_POINT('Ctrl Pts',(-29.4648367940965,14.2990479598781,
128.783307296558)) ;
#153203 = CARTESIAN_POINT('Ctrl Pts',(-29.5224591681686,14.096277092635,128.984789687897)) ;
#153204 = CARTESIAN_POINT('Ctrl Pts',(-29.5601633246064,13.8463552274942,
129.12795060112)) ;
#153205 = CARTESIAN_POINT('Ctrl Pts',(-29.5747316968106,13.5643762793268,
129.203747316631)) ;
#153206 = CARTESIAN_POINT('Ctrl Pts',(-29.5643172687888,13.2747380866486,
129.206268472805)) ;
#153207 = CARTESIAN_POINT('Ctrl Pts',(-29.5288291438255,12.9934296976024,
129.135814296567)) ;
#153208 = CARTESIAN_POINT('Ctrl Pts',(-29.470171863856,12.7438068041656,128.99757323151)) ;
#153209 = CARTESIAN_POINT('Ctrl Pts',(-29.391803285665,12.5426943442427,128.801768222048)) ;
#153210 = CARTESIAN_POINT('Ctrl Pts',(-29.2986131391391,12.4046936236787,
128.56265775762)) ;
#153211 = CARTESIAN_POINT('Ctrl Pts',(-29.1964773761958,12.3396331759052,
128.297435830634)) ;
#153212 = CARTESIAN_POINT('Ctrl Pts',(-29.092230590555,12.3522550875064,128.025991131613)) ;
#153213 = CARTESIAN_POINT('Ctrl Pts',(-28.9924608185787,12.441158614988,127.767604009206)) ;
#153214 = CARTESIAN_POINT('Ctrl Pts',(-28.9030933450802,12.6013769713038,
127.539790029494)) ;
#153215 = CARTESIAN_POINT('Ctrl Pts',(-28.8308886096015,12.819071640269,127.361858709555)) ;
#153216 = CARTESIAN_POINT('Ctrl Pts',(-28.779280341327,13.0807346140254,127.244233442709)) ;
#153217 = CARTESIAN_POINT('Ctrl Pts',(-28.7517055757331,13.3675408612144,
127.196874862189)) ;
#153218 = CARTESIAN_POINT('Ctrl Pts',(-28.7493257047856,13.6570979280699,
127.222968219409)) ;
#153219 = CARTESIAN_POINT('Ctrl Pts',(-28.7718142821641,13.9319893911641,
127.321979864566)) ;
#153220 = CARTESIAN_POINT('Ctrl Pts',(-28.8162456944187,14.1676085258846,
127.484711805867)) ;
#153221 = CARTESIAN_POINT('Ctrl Pts',(-28.8794392120634,14.3519029604138,
127.702543293248)) ;
#153222 = CARTESIAN_POINT('Ctrl Pts',(-28.955521536148,14.4687263868581,127.957864396171)) ;
#153223 = CARTESIAN_POINT('Ctrl Pts',(-29.0386446837284,14.5110206744739,
128.233803590714)) ;
#153224 = CARTESIAN_POINT('Ctrl Pts',(-29.1220480184099,14.4754839101951,
128.510547823415)) ;
#153225 = CARTESIAN_POINT('Ctrl Pts',(-29.1992609632459,14.3641243881349,
128.769313204063)) ;
#153226 = CARTESIAN_POINT('Ctrl Pts',(-29.2634796257756,14.1859981150162,
128.989963010774)) ;
#153227 = CARTESIAN_POINT('Ctrl Pts',(-29.309906743687,13.9527739629267,129.158738849017)) ;
#153228 = CARTESIAN_POINT('Ctrl Pts',(-29.3342115703911,13.6818171869407,
129.262851136394)) ;
#153229 = CARTESIAN_POINT('Ctrl Pts',(-29.3340473631818,13.3923456599437,
129.295485666288)) ;
#153230 = CARTESIAN_POINT('Ctrl Pts',(-29.3085669103323,13.1044625348289,
129.254236375475)) ;
#153231 = CARTESIAN_POINT('Ctrl Pts',(-29.258986211392,12.8400820200563,129.142508243958)) ;
#153232 = CARTESIAN_POINT('Ctrl Pts',(-29.1881542029012,12.6174283224968,
128.968693652698)) ;
#153233 = CARTESIAN_POINT('Ctrl Pts',(-29.1002100971169,12.4521814963559,
128.744946986999)) ;
#153234 = CARTESIAN_POINT('Ctrl Pts',(-29.0009103649547,12.3567835155047,
128.48800496993)) ;
#153235 = CARTESIAN_POINT('Ctrl Pts',(-28.896925987083,12.3377092271658,128.21727920025)) ;
#153236 = CARTESIAN_POINT('Ctrl Pts',(-28.7942667965697,12.3962076032604,
127.950545837014)) ;
#153237 = CARTESIAN_POINT('Ctrl Pts',(-28.6998220504126,12.5290432373042,
127.70787965737)) ;
#153238 = CARTESIAN_POINT('Ctrl Pts',(-28.6204061898145,12.7244085230837,
127.508847094626)) ;
#153239 = CARTESIAN_POINT('Ctrl Pts',(-28.559819094265,12.9709500550387,127.365030411237)) ;
#153240 = CARTESIAN_POINT('Ctrl Pts',(-28.5223002592329,13.2494402817627,
127.288528530129)) ;
#153241 = CARTESIAN_POINT('Ctrl Pts',(-28.5097189788881,13.5418967084717,
127.285058220228)) ;
#153242 = CARTESIAN_POINT('Ctrl Pts',(-28.5222097719137,13.8230883914708,
127.354499660829)) ;
#153243 = CARTESIAN_POINT('Ctrl Pts',(-28.5582144837367,14.0775910910953,
127.492866930045)) ;
#153244 = CARTESIAN_POINT('Ctrl Pts',(-28.6142444612186,14.2842118886259,
127.689596183375)) ;
#153245 = CARTESIAN_POINT('Ctrl Pts',(-28.6857946550641,14.4299775435325,
127.931754504999)) ;
#153246 = CARTESIAN_POINT('Ctrl Pts',(-28.7673480084958,14.503331032243,128.203286809695)) ;
#153247 = CARTESIAN_POINT('Ctrl Pts',(-28.8509261449003,14.4992417837061,
128.480336479146)) ;
#153248 = CARTESIAN_POINT('Ctrl Pts',(-28.9318023648984,14.4177939822546,
128.749907191947)) ;
#153249 = CARTESIAN_POINT('Ctrl Pts',(-29.001910688641,14.2650806147523,128.987818507409)) ;
#153250 = CARTESIAN_POINT('Ctrl Pts',(-29.0559489688668,14.0529681509037,
129.178698338362)) ;
#153251 = CARTESIAN_POINT('Ctrl Pts',(-29.0896354038435,13.7955270319932,
129.310187588582)) ;
#153252 = CARTESIAN_POINT('Ctrl Pts',(-29.099611948193,13.5095709535078,129.372622374006)) ;
#153253 = CARTESIAN_POINT('Ctrl Pts',(-29.0842585907111,13.2189036520177,
129.360885383851)) ;
#153254 = CARTESIAN_POINT('Ctrl Pts',(-29.0443620584725,12.9437120966298,
129.277345257376)) ;
#153255 = CARTESIAN_POINT('Ctrl Pts',(-28.9817282559493,12.7018113312773,
129.127496651977)) ;
#153256 = CARTESIAN_POINT('Ctrl Pts',(-28.900103185758,12.5115374792667,128.922195104015)) ;
#153257 = CARTESIAN_POINT('Ctrl Pts',(-28.8047562754635,12.3865362509785,
128.676787399727)) ;
#153258 = CARTESIAN_POINT('Ctrl Pts',(-28.7012853562746,12.3360647683775,
128.40778833087)) ;
#153259 = CARTESIAN_POINT('Ctrl Pts',(-28.5980648305844,12.3630945002041,
128.139111767235)) ;
#153260 = CARTESIAN_POINT('Ctrl Pts',(-28.4992221941751,12.4665769548229,
127.883658010127)) ;
#153261 = CARTESIAN_POINT('Ctrl Pts',(-28.4131594840602,12.637873730405,127.665272376222)) ;
#153262 = CARTESIAN_POINT('Ctrl Pts',(-28.3441687124707,12.8661806742055,
127.496923307267)) ;
#153263 = CARTESIAN_POINT('Ctrl Pts',(-28.2971179753842,13.1333277515124,
127.392512752519)) ;
#153264 = CARTESIAN_POINT('Ctrl Pts',(-28.2742141661044,13.4221934836715,
127.358771264461)) ;
#153265 = CARTESIAN_POINT('Ctrl Pts',(-28.2765820238562,13.7107571318464,
127.398801174816)) ;
#153266 = CARTESIAN_POINT('Ctrl Pts',(-28.3034962448371,13.9798563780996,
127.510697252844)) ;
#153267 = CARTESIAN_POINT('Ctrl Pts',(-28.3518348917567,14.2070905580459,
127.684913382421)) ;
#153268 = CARTESIAN_POINT('Ctrl Pts',(-28.417736051092,14.3790287482914,127.910539859451)) ;
#153269 = CARTESIAN_POINT('Ctrl Pts',(-28.4956163030634,14.4826462514907,
128.171126340958)) ;
#153270 = CARTESIAN_POINT('Ctrl Pts',(-28.5798455524846,14.5101765749395,
128.450506444325)) ;
#153271 = CARTESIAN_POINT('Ctrl Pts',(-28.66200834704,14.4602521093363,128.723409993032)) ;
#153272 = CARTESIAN_POINT('Ctrl Pts',(-28.7375813833395,14.3349863303821,
128.977516850491)) ;
#153273 = CARTESIAN_POINT('Ctrl Pts',(-28.7985628235098,14.1459036519263,
129.188607444567)) ;
#153274 = CARTESIAN_POINT('Ctrl Pts',(-28.8411540818564,13.9042674567381,
129.346179660859)) ;
#153275 = CARTESIAN_POINT('Ctrl Pts',(-28.8610016097192,13.6274934121279,
129.437359596521)) ;
#153276 = CARTESIAN_POINT('Ctrl Pts',(-28.8560349310886,13.3375401227482,
129.455886266098)) ;
#153277 = CARTESIAN_POINT('Ctrl Pts',(-28.8260275084833,13.0529656397982,
129.401339308127)) ;
#153278 = CARTESIAN_POINT('Ctrl Pts',(-28.7718240751871,12.793542004979,129.276308893705)) ;
#153279 = CARTESIAN_POINT('Ctrl Pts',(-28.69758931411,12.5815361452067,129.09244647551)) ;
#153280 = CARTESIAN_POINT('Ctrl Pts',(-28.607191982818,12.4287258471182,128.861490887195)) ;
#153281 = CARTESIAN_POINT('Ctrl Pts',(-28.5062114306704,12.3470719994747,
128.599714513405)) ;
#153282 = CARTESIAN_POINT('Ctrl Pts',(-28.4016831964791,12.3430683223392,
128.327512526391)) ;
#153283 = CARTESIAN_POINT('Ctrl Pts',(-28.3008205475048,12.4155936091128,
128.065797526111)) ;
#153284 = CARTESIAN_POINT('Ctrl Pts',(-28.2086887982306,12.5608875783812,
127.829855784513)) ;
#153285 = CARTESIAN_POINT('Ctrl Pts',(-28.1322966051425,12.7672957855937,
127.639749496506)) ;
#153286 = CARTESIAN_POINT('Ctrl Pts',(-28.0757288054588,13.0219896288371,
127.507742576733)) ;
#153287 = CARTESIAN_POINT('Ctrl Pts',(-28.0429540969002,13.3035436342973,
127.44499916588)) ;
#153288 = CARTESIAN_POINT('Ctrl Pts',(-28.0350385580784,13.5948422510341,
127.455024273178)) ;
#153289 = CARTESIAN_POINT('Ctrl Pts',(-28.0521494910461,13.8739529691167,
127.538171398898)) ;
#153290 = CARTESIAN_POINT('Ctrl Pts',(-28.0921989061459,14.1203174233417,
127.688276422386)) ;
#153291 = CARTESIAN_POINT('Ctrl Pts',(-28.151557364416,14.3167168643634,127.894769419474)) ;
#153292 = CARTESIAN_POINT('Ctrl Pts',(-28.2253962663715,14.4494066861711,
128.14361033343)) ;
#153293 = CARTESIAN_POINT('Ctrl Pts',(-28.3077059790347,14.5084702688582,
128.41722565312)) ;
#153294 = CARTESIAN_POINT('Ctrl Pts',(-28.3916026412673,14.489700746972,128.695408809309)) ;
#153295 = CARTESIAN_POINT('Ctrl Pts',(-28.4706094716546,14.3946106074975,
128.959339303664)) ;
#153296 = CARTESIAN_POINT('Ctrl Pts',(-28.5383385063881,14.2294635345246,
129.190381875795)) ;
#153297 = CARTESIAN_POINT('Ctrl Pts',(-28.5888615094772,14.0073333887475,
129.371024757805)) ;
#153298 = CARTESIAN_POINT('Ctrl Pts',(-28.6182752167583,13.7435828448799,
129.490009369002)) ;
#153299 = CARTESIAN_POINT('Ctrl Pts',(-28.6235344183767,13.454824745877,129.538667492509)) ;
#153300 = CARTESIAN_POINT('Ctrl Pts',(-28.6035941708859,13.1663898496403,
129.513405963783)) ;
#153301 = CARTESIAN_POINT('Ctrl Pts',(-28.5591016772346,12.8948251888563,
129.416595319443)) ;
#153302 = CARTESIAN_POINT('Ctrl Pts',(-28.4924613979654,12.6613614393991,
129.255069109059)) ;
#153303 = CARTESIAN_POINT('Ctrl Pts',(-28.4079858158223,12.4827884864443,
129.041374692839)) ;
#153304 = CARTESIAN_POINT('Ctrl Pts',(-28.3106810095428,12.3713198999723,
128.790256537741)) ;
#153305 = CARTESIAN_POINT('Ctrl Pts',(-28.2071142233906,12.3351536539427,
128.520782151597)) ;
#153306 = CARTESIAN_POINT('Ctrl Pts',(-28.1033170651269,12.3771106003778,
128.250789621036)) ;
#153307 = CARTESIAN_POINT('Ctrl Pts',(-28.0070122936131,12.493746042562,128.002507073001)) ;
#153308 = CARTESIAN_POINT('Ctrl Pts',(-27.9236042223444,12.6767291405437,
127.791947198724)) ;
#153309 = CARTESIAN_POINT('Ctrl Pts',(-27.8582788554542,12.9147362953278,
127.634399931538)) ;
#153310 = CARTESIAN_POINT('Ctrl Pts',(-27.8157639814054,13.1870897175325,
127.543206911709)) ;
#153311 = CARTESIAN_POINT('Ctrl Pts',(-27.7976113632335,13.4771402294594,
127.523294837643)) ;
#153312 = CARTESIAN_POINT('Ctrl Pts',(-27.8047562191335,13.7642376991577,
127.577383148529)) ;
#153313 = CARTESIAN_POINT('Ctrl Pts',(-27.8359687279842,14.0261140050281,
127.701710177171)) ;
#153314 = CARTESIAN_POINT('Ctrl Pts',(-27.8877875139809,14.2437566095146,
127.886037495367)) ;
#153315 = CARTESIAN_POINT('Ctrl Pts',(-27.9566643830394,14.4043004510961,
128.12048462873)) ;
#153316 = CARTESIAN_POINT('Ctrl Pts',(-28.0360570915207,14.4936451763547,
128.385451901082)) ;
#153317 = CARTESIAN_POINT('Ctrl Pts',(-28.120129115805,14.5067755223083,128.664180642723)) ;
#153318 = CARTESIAN_POINT('Ctrl Pts',(-28.2020346856407,14.4421251633059,
128.936606880987)) ;
#153319 = CARTESIAN_POINT('Ctrl Pts',(-28.2751125216823,14.3039891726026,
129.183284767789)) ;
#153320 = CARTESIAN_POINT('Ctrl Pts',(-28.3330260630189,14.1040922169467,
129.385445944809)) ;
#153321 = CARTESIAN_POINT('Ctrl Pts',(-28.3716774412633,13.8535852347893,
129.531620171577)) ;
#153322 = CARTESIAN_POINT('Ctrl Pts',(-28.3868553207156,13.5730952435811,
129.609080622274)) ;
#153323 = CARTESIAN_POINT('Ctrl Pts',(-28.3771751540194,13.2829861782011,
129.613807074417)) ;
#153324 = CARTESIAN_POINT('Ctrl Pts',(-28.3425095932928,13.0017737284941,
129.545666888846)) ;
#153325 = CARTESIAN_POINT('Ctrl Pts',(-28.284301937165,12.7500890797144,129.408856898039)) ;
#153326 = CARTESIAN_POINT('Ctrl Pts',(-28.2064572920802,12.5475577998432,
129.214559307957)) ;
#153327 = CARTESIAN_POINT('Ctrl Pts',(-28.1135171544018,12.4075652478031,
128.976210428243)) ;
#153328 = CARTESIAN_POINT('Ctrl Pts',(-28.0118850220544,12.3405227377109,
128.712349934362)) ;
#153329 = CARTESIAN_POINT('Ctrl Pts',(-27.9073393263242,12.3506975715296,
128.440115510787)) ;
#153330 = CARTESIAN_POINT('Ctrl Pts',(-27.8069898708441,12.438177489278,128.180166701549)) ;
#153331 = CARTESIAN_POINT('Ctrl Pts',(-27.7177045614419,12.5958827964123,
127.952426644854)) ;
#153332 = CARTESIAN_POINT('Ctrl Pts',(-27.6448174995369,12.8123887822574,
127.772559198421)) ;
#153333 = CARTESIAN_POINT('Ctrl Pts',(-27.5925658802496,13.0732934241726,
127.653072879261)) ;
#153334 = CARTESIAN_POINT('Ctrl Pts',(-27.5643119574423,13.3601444544887,
127.603779546763)) ;
#153335 = CARTESIAN_POINT('Ctrl Pts',(-27.5613082454556,13.6487324697402,
127.627925538602)) ;
#153336 = CARTESIAN_POINT('Ctrl Pts',(-27.5828722691528,13.9231969052117,
127.724074394844)) ;
#153337 = CARTESIAN_POINT('Ctrl Pts',(-27.6269024064909,14.1616648845749,
127.885829090303)) ;
#153338 = CARTESIAN_POINT('Ctrl Pts',(-27.6896598747405,14.3474885130478,
128.102376258084)) ;
#153339 = CARTESIAN_POINT('Ctrl Pts',(-27.7653992680876,14.4664584587802,
128.356681964705)) ;
#153340 = CARTESIAN_POINT('Ctrl Pts',(-27.8487981620875,14.5109046603937,
128.633576137683)) ;
#153341 = CARTESIAN_POINT('Ctrl Pts',(-27.9318850392023,14.477538406395,128.909237750788)) ;
#153342 = CARTESIAN_POINT('Ctrl Pts',(-28.0095052256554,14.3681997132881,
129.169245881706)) ;
#153343 = CARTESIAN_POINT('Ctrl Pts',(-28.0741401659524,14.19161807787,129.391120281656)) ;
#153344 = CARTESIAN_POINT('Ctrl Pts',(-28.1210449004513,13.9603524956053,
129.561209556167)) ;
#153345 = CARTESIAN_POINT('Ctrl Pts',(-28.1460961632202,13.6895220911817,
129.667588782595)) ;
#153346 = CARTESIAN_POINT('Ctrl Pts',(-28.1465838645101,13.4007319641459,
129.702076763037)) ;
#153347 = CARTESIAN_POINT('Ctrl Pts',(-28.1219792750298,13.1132078283894,
129.663296512428)) ;
#153348 = CARTESIAN_POINT('Ctrl Pts',(-28.072797303837,12.8466068578935,129.552900494661)) ;
#153349 = CARTESIAN_POINT('Ctrl Pts',(-28.0028760663637,12.6236984730367,
129.381571768306)) ;
#153350 = CARTESIAN_POINT('Ctrl Pts',(-27.9152289217031,12.4561011970055,
129.15875880179)) ;
#153351 = CARTESIAN_POINT('Ctrl Pts',(-27.8163074914158,12.3585968124196,
128.902876316079)) ;
#153352 = CARTESIAN_POINT('Ctrl Pts',(-27.7120492591559,12.3371246735504,
128.631455165304)) ;
#153353 = CARTESIAN_POINT('Ctrl Pts',(-27.6093731664381,12.3935413485491,
128.364635405542)) ;
#153354 = CARTESIAN_POINT('Ctrl Pts',(-27.5149001295544,12.5236723848828,
128.121769416389)) ;
#153355 = CARTESIAN_POINT('Ctrl Pts',(-27.4346201824783,12.7179304240541,
127.920341279588)) ;
#153356 = CARTESIAN_POINT('Ctrl Pts',(-27.3732833708595,12.9643000603806,
127.774449881944)) ;
#153357 = CARTESIAN_POINT('Ctrl Pts',(-27.3353218805088,13.2410161239663,
127.696515666237)) ;
#153358 = CARTESIAN_POINT('Ctrl Pts',(-27.3219345106549,13.5320326358814,
127.690536193544)) ;
#153359 = CARTESIAN_POINT('Ctrl Pts',(-27.3336868555628,13.8151976332958,
127.757981771659)) ;
#153360 = CARTESIAN_POINT('Ctrl Pts',(-27.3691045396702,14.070965110173,127.894657472177)) ;
#153361 = CARTESIAN_POINT('Ctrl Pts',(-27.4247538548607,14.2795161854134,
128.090342542637)) ;
#153362 = CARTESIAN_POINT('Ctrl Pts',(-27.495823154164,14.4266233568165,128.331023842141)) ;
#153363 = CARTESIAN_POINT('Ctrl Pts',(-27.5766922115291,14.5021444966585,
128.600366276399)) ;
#153364 = CARTESIAN_POINT('Ctrl Pts',(-27.6609223179021,14.5004799279669,
128.8795751742)) ;
#153365 = CARTESIAN_POINT('Ctrl Pts',(-27.7417671934519,14.4210758361391,
129.14896837329)) ;
#153366 = CARTESIAN_POINT('Ctrl Pts',(-27.8120265768946,14.2711637356508,
129.38719326095)) ;
#153367 = CARTESIAN_POINT('Ctrl Pts',(-27.866891762874,14.0600320259714,129.580611011308)) ;
#153368 = CARTESIAN_POINT('Ctrl Pts',(-27.9012411174026,13.8025046463563,
129.714162963611)) ;
#153369 = CARTESIAN_POINT('Ctrl Pts',(-27.9118652501947,13.5194350300881,
129.778210865001)) ;
#153370 = CARTESIAN_POINT('Ctrl Pts',(-27.8973675127668,13.227929848522,129.769057927685)) ;
#153371 = CARTESIAN_POINT('Ctrl Pts',(-27.8581217638387,12.9514279979351,
129.687479679852)) ;
#153372 = CARTESIAN_POINT('Ctrl Pts',(-27.7958487933346,12.7076270254922,
129.538792895781)) ;
#153373 = CARTESIAN_POINT('Ctrl Pts',(-27.7150442368328,12.5164543914562,
129.335744778992)) ;
#153374 = CARTESIAN_POINT('Ctrl Pts',(-27.6197799723084,12.3891143889345,
129.090666143106)) ;
#153375 = CARTESIAN_POINT('Ctrl Pts',(-27.5169840616899,12.3364756158918,
128.823462340777)) ;
#153376 = CARTESIAN_POINT('Ctrl Pts',(-27.4129425204162,12.3612642231578,
128.552629149903)) ;
#153377 = CARTESIAN_POINT('Ctrl Pts',(-27.3139116309648,12.4629838840005,
128.296612691349)) ;
#153378 = CARTESIAN_POINT('Ctrl Pts',(-27.2276350555539,12.6321971699934,
128.077535896234)) ;
#153379 = CARTESIAN_POINT('Ctrl Pts',(-27.1581753164316,12.8584558798932,
127.907740199772)) ;
#153380 = CARTESIAN_POINT('Ctrl Pts',(-27.1102193532803,13.1261648647243,
127.800864060768)) ;
#153381 = CARTESIAN_POINT('Ctrl Pts',(-27.0867427780488,13.4141234552309,
127.765371910168)) ;
#153382 = CARTESIAN_POINT('Ctrl Pts',(-27.088405263082,13.7023852342343,127.803282253112)) ;
#153383 = CARTESIAN_POINT('Ctrl Pts',(-27.1144094066955,13.9714212012371,
127.912378068659)) ;
#153384 = CARTESIAN_POINT('Ctrl Pts',(-27.1625636190418,14.202020081249,128.086338189894)) ;
#153385 = CARTESIAN_POINT('Ctrl Pts',(-27.2279041571622,14.3750071736422,
128.310222999053)) ;
#153386 = CARTESIAN_POINT('Ctrl Pts',(-27.3055089641359,14.4806351346196,
128.570006270221)) ;
#153387 = CARTESIAN_POINT('Ctrl Pts',(-27.3892702869014,14.5105855297535,
128.847858683373)) ;
#153388 = CARTESIAN_POINT('Ctrl Pts',(-27.4721256647169,14.4625550657111,
129.123019817885)) ;
#153389 = CARTESIAN_POINT('Ctrl Pts',(-27.5475424958297,14.3400369417443,
129.376461860258)) ;
#153390 = CARTESIAN_POINT('Ctrl Pts',(-27.6092868870231,14.1521957535254,
129.589908595948)) ;
#153391 = CARTESIAN_POINT('Ctrl Pts',(-27.6524549950664,13.9116489154345,
129.749173070005)) ;
#153392 = CARTESIAN_POINT('Ctrl Pts',(-27.6729767158619,13.6358544266559,
129.842295420114)) ;
#153393 = CARTESIAN_POINT('Ctrl Pts',(-27.6687686357343,13.3459427675745,
129.863045715734)) ;
#153394 = CARTESIAN_POINT('Ctrl Pts',(-27.6393546558192,13.0604649745041,
129.810291983176)) ;
#153395 = CARTESIAN_POINT('Ctrl Pts',(-27.5861749748563,12.8015143832803,
129.688047174148)) ;
#153396 = CARTESIAN_POINT('Ctrl Pts',(-27.5122453552566,12.586871423154,129.505215644939)) ;
#153397 = CARTESIAN_POINT('Ctrl Pts',(-27.4222257102063,12.4323032180318,
129.275353955494)) ;
#153398 = CARTESIAN_POINT('Ctrl Pts',(-27.321814640165,12.348604012381,129.015131363742)) ;
#153399 = CARTESIAN_POINT('Ctrl Pts',(-27.2172646277251,12.3418345254331,
128.742874357153)) ;
#153400 = CARTESIAN_POINT('Ctrl Pts',(-27.1155991989799,12.4127257697425,
128.479021774659)) ;
#153401 = CARTESIAN_POINT('Ctrl Pts',(-27.0235546029965,12.5554430365515,
128.24317434018)) ;
#153402 = CARTESIAN_POINT('Ctrl Pts',(-26.946364611968,12.7608029240068,128.050846584327)) ;
#153403 = CARTESIAN_POINT('Ctrl Pts',(-26.8892425932522,13.0143079229722,
127.917197312737)) ;
#153404 = CARTESIAN_POINT('Ctrl Pts',(-26.8557397574038,13.2953661026702,
127.852335782128)) ;
#153405 = CARTESIAN_POINT('Ctrl Pts',(-26.8471237684322,13.587499191953,127.86040257377)) ;
#153406 = CARTESIAN_POINT('Ctrl Pts',(-26.8636409106043,13.8669338626205,
127.941791701437)) ;
#153407 = CARTESIAN_POINT('Ctrl Pts',(-26.9028894020443,14.1134263503453,
128.089413302891)) ;
#153408 = CARTESIAN_POINT('Ctrl Pts',(-26.9618864660315,14.3121780897716,
128.294946112899)) ;
#153409 = CARTESIAN_POINT('Ctrl Pts',(-27.0356609756341,14.4470050265316,
128.543696981495)) ;
#153410 = CARTESIAN_POINT('Ctrl Pts',(-27.1176846698481,14.5078086325279,
128.816414339099)) ;
#153411 = CARTESIAN_POINT('Ctrl Pts',(-27.2013501944063,14.4913412737729,
129.093814747738)) ;
#153412 = CARTESIAN_POINT('Ctrl Pts',(-27.2805727554514,14.3985299043882,
129.358365317732)) ;
#153413 = CARTESIAN_POINT('Ctrl Pts',(-27.3487809879748,14.2353764928408,
129.590815975098)) ;
#153414 = CARTESIAN_POINT('Ctrl Pts',(-27.4000923756535,14.0132824388172,
129.773951949604)) ;
#153415 = CARTESIAN_POINT('Ctrl Pts',(-27.4299031588905,13.751770584179,129.893917739675)) ;
#153416 = CARTESIAN_POINT('Ctrl Pts',(-27.4360065328396,13.4639004603942,
129.944990740374)) ;
#153417 = CARTESIAN_POINT('Ctrl Pts',(-27.4166194504997,13.1736259559936,
129.921533138526)) ;
#153418 = CARTESIAN_POINT('Ctrl Pts',(-27.3730557967721,12.9029494351804,
129.827230137503)) ;
#153419 = CARTESIAN_POINT('Ctrl Pts',(-27.3068239081708,12.6670694829694,
129.667025348139)) ;
#153420 = CARTESIAN_POINT('Ctrl Pts',(-27.2225807375648,12.4867414535482,
129.454064281963)) ;
#153421 = CARTESIAN_POINT('Ctrl Pts',(-27.1260163205075,12.3736046950475,
129.204955161642)) ;
#153422 = CARTESIAN_POINT('Ctrl Pts',(-27.0219531940928,12.3351061359291,
128.934221171249)) ;
#153423 = CARTESIAN_POINT('Ctrl Pts',(-26.9187654991147,12.3747297412366,
128.665782677207)) ;
#153424 = CARTESIAN_POINT('Ctrl Pts',(-26.8219192185406,12.4890530273647,
128.415981781108)) ;
#153425 = CARTESIAN_POINT('Ctrl Pts',(-26.7375618368722,12.6718473822343,
128.20287552548)) ;
#153426 = CARTESIAN_POINT('Ctrl Pts',(-26.6721408995713,12.9071471042355,
128.044830293244)) ;
#153427 = CARTESIAN_POINT('Ctrl Pts',(-26.6288268693924,13.1791583633753,
127.951366546025)) ;
#153428 = CARTESIAN_POINT('Ctrl Pts',(-26.6100146219695,13.4685703303894,
127.929472625113)) ;
#153429 = CARTESIAN_POINT('Ctrl Pts',(-26.6163965606096,13.7556865610863,
127.981289936006)) ;
#153430 = CARTESIAN_POINT('Ctrl Pts',(-26.6468365176563,14.0184520779736,
128.103328446011)) ;
#153431 = CARTESIAN_POINT('Ctrl Pts',(-26.6983664732469,14.2386835545227,
128.286981099105)) ;
#153432 = CARTESIAN_POINT('Ctrl Pts',(-26.7668561678463,14.4009245247973,
128.520283146029)) ;
#153433 = CARTESIAN_POINT('Ctrl Pts',(-26.8462801396179,14.4923209079493,
128.785440445302)) ;
#153434 = CARTESIAN_POINT('Ctrl Pts',(-26.9299042318789,14.5074993821674,
129.062691208225)) ;
#153435 = CARTESIAN_POINT('Ctrl Pts',(-27.0123042045344,14.4446391320812,
129.336708219525)) ;
#153436 = CARTESIAN_POINT('Ctrl Pts',(-27.0853285109314,14.309013886893,129.583057807955)) ;
#153437 = CARTESIAN_POINT('Ctrl Pts',(-27.1438828659143,14.1104149351794,
129.787163074108)) ;
#153438 = CARTESIAN_POINT('Ctrl Pts',(-27.1830524640317,13.8614588559076,
129.934789891105)) ;
#153439 = CARTESIAN_POINT('Ctrl Pts',(-27.1989887778394,13.5819687002437,
130.014428956727)) ;
#153440 = CARTESIAN_POINT('Ctrl Pts',(-27.1899960665713,13.2906279013141,
130.021303572167)) ;
#153441 = CARTESIAN_POINT('Ctrl Pts',(-27.1559614540415,13.009243305788,129.95497149067)) ;
#153442 = CARTESIAN_POINT('Ctrl Pts',(-27.0987240639522,12.7575168112921,
129.820836098485)) ;
#153443 = CARTESIAN_POINT('Ctrl Pts',(-27.0211347642334,12.5525240138587,
129.627409702748)) ;
#153444 = CARTESIAN_POINT('Ctrl Pts',(-26.9288019853003,12.4108770336832,
129.390743830787)) ;
#153445 = CARTESIAN_POINT('Ctrl Pts',(-26.8269925769389,12.3412909140522,
129.126483822534)) ;
#153446 = CARTESIAN_POINT('Ctrl Pts',(-26.7225678003105,12.3493861735078,
128.854556329981)) ;
#153447 = CARTESIAN_POINT('Ctrl Pts',(-26.6222736426069,12.4342727909203,
128.594675298208)) ;
#153448 = CARTESIAN_POINT('Ctrl Pts',(-26.5324245140866,12.5900489009072,
128.365332500197)) ;
#153449 = CARTESIAN_POINT('Ctrl Pts',(-26.4587946173494,12.8056265995217,
128.183382042886)) ;
#153450 = CARTESIAN_POINT('Ctrl Pts',(-26.4059966216722,13.0653848746049,
128.062274396553)) ;
#153451 = CARTESIAN_POINT('Ctrl Pts',(-26.3770384247468,13.3504851063388,
128.01077693268)) ;
#153452 = CARTESIAN_POINT('Ctrl Pts',(-26.3732580768289,13.6412798147236,
128.032889399786)) ;
#153453 = CARTESIAN_POINT('Ctrl Pts',(-26.3941468859038,13.915548156852,128.126957619226)) ;
#153454 = CARTESIAN_POINT('Ctrl Pts',(-26.4375236270793,14.1552942040558,
128.286796725341)) ;
#153455 = CARTESIAN_POINT('Ctrl Pts',(-26.499786802166,14.3429101935435,128.501891901076)) ;
#153456 = CARTESIAN_POINT('Ctrl Pts',(-26.5753221744753,14.4639893047867,
128.755644371512)) ;
#153457 = CARTESIAN_POINT('Ctrl Pts',(-26.658258796401,14.5107279953385,129.031049167775)) ;
#153458 = CARTESIAN_POINT('Ctrl Pts',(-26.7418770326506,14.4794893752074,
129.308446128137)) ;
#153459 = CARTESIAN_POINT('Ctrl Pts',(-26.819410154467,14.3727211578977,129.56804219168)) ;
#153460 = CARTESIAN_POINT('Ctrl Pts',(-26.884660652684,14.1977799584113,129.791786901947)) ;
#153461 = CARTESIAN_POINT('Ctrl Pts',(-26.9321606344241,13.9680803032242,
129.963592933574)) ;
#153462 = CARTESIAN_POINT('Ctrl Pts',(-26.9579703404882,13.6967826933105,
130.072347583536)) ;
#153463 = CARTESIAN_POINT('Ctrl Pts',(-26.9591310030642,13.4094043760888,
130.108663362794)) ;
#153464 = CARTESIAN_POINT('Ctrl Pts',(-26.935231210856,13.1212039321583,130.071985580596)) ;
#153465 = CARTESIAN_POINT('Ctrl Pts',(-26.8869426549206,12.8546896237207,
129.964066829109)) ;
#153466 = CARTESIAN_POINT('Ctrl Pts',(-26.8174482093006,12.6293810356165,
129.794091823838)) ;
#153467 = CARTESIAN_POINT('Ctrl Pts',(-26.7297563031988,12.4594635396626,
129.571300039305)) ;
#153468 = CARTESIAN_POINT('Ctrl Pts',(-26.6315768169788,12.3604529302704,
129.317412505758)) ;
#153469 = CARTESIAN_POINT('Ctrl Pts',(-26.527041677516,12.3366695079855,129.045292118923)) ;
#153470 = CARTESIAN_POINT('Ctrl Pts',(-26.4246632418904,12.3907630606801,
128.779202667163)) ;
#153471 = CARTESIAN_POINT('Ctrl Pts',(-26.3296624090555,12.5187717527639,
128.534846855937)) ;
#153472 = CARTESIAN_POINT('Ctrl Pts',(-26.2486292653153,12.7125553045139,
128.331370691531)) ;
#153473 = CARTESIAN_POINT('Ctrl Pts',(-26.187290463919,12.9551208485313,128.185129058602)) ;
#153474 = CARTESIAN_POINT('Ctrl Pts',(-26.1482420973643,13.2325620060974,
128.104210130242)) ;
#153475 = CARTESIAN_POINT('Ctrl Pts',(-26.1341913899476,13.5243419796884,
128.096383572714)) ;
#153476 = CARTESIAN_POINT('Ctrl Pts',(-26.1452118388481,13.8069926528057,
128.161574113629)) ;
#153477 = CARTESIAN_POINT('Ctrl Pts',(-26.1799390075941,14.0639000199269,
128.296232665471)) ;
#153478 = CARTESIAN_POINT('Ctrl Pts',(-26.2350489546991,14.2741558930926,
128.490347023028)) ;
#153479 = CARTESIAN_POINT('Ctrl Pts',(-26.3059077450582,14.4234615625839,
128.730487186166)) ;
#153480 = CARTESIAN_POINT('Ctrl Pts',(-26.386494169588,14.5011170686614,128.998961276038)) ;
#153481 = CARTESIAN_POINT('Ctrl Pts',(-26.4710372754606,14.5013614779113,
129.279215621043)) ;
#153482 = CARTESIAN_POINT('Ctrl Pts',(-26.5513450363698,14.4249956630962,
129.546727763435)) ;
#153483 = CARTESIAN_POINT('Ctrl Pts',(-26.6226216620681,14.2760171565871,
129.788206158856)) ;
#153484 = CARTESIAN_POINT('Ctrl Pts',(-26.6777858163634,14.0665442400002,
129.982426179449)) ;
#153485 = CARTESIAN_POINT('Ctrl Pts',(-26.7127743428566,13.8110528410318,
130.117741076645)) ;
#153486 = CARTESIAN_POINT('Ctrl Pts',(-26.7241069347589,13.5262786463887,
130.184114351317)) ;
#153487 = CARTESIAN_POINT('Ctrl Pts',(-26.7103978253846,13.2368369901033,
130.177011615775)) ;
#153488 = CARTESIAN_POINT('Ctrl Pts',(-26.6716560461567,12.9583255903659,
130.097075764209)) ;
#153489 = CARTESIAN_POINT('Ctrl Pts',(-26.6103674672222,12.7145800096232,
129.95106877123)) ;
#153490 = CARTESIAN_POINT('Ctrl Pts',(-26.5292783226885,12.5201730384604,
129.747494551372)) ;
#153491 = CARTESIAN_POINT('Ctrl Pts',(-26.4353195353877,12.392297716127,129.505869698294)) ;
#153492 = CARTESIAN_POINT('Ctrl Pts',(-26.3321003131888,12.3368042043637,
129.23762472755)) ;
#153493 = CARTESIAN_POINT('Ctrl Pts',(-26.2283359448761,12.3594079574846,
128.967488898529)) ;
#153494 = CARTESIAN_POINT('Ctrl Pts',(-26.1289374320057,12.4588426243277,
128.710432008687)) ;
#153495 = CARTESIAN_POINT('Ctrl Pts',(-26.0421433826271,12.6263832935465,
128.489874381818)) ;
#153496 = CARTESIAN_POINT('Ctrl Pts',(-25.9721170036289,12.8513078071139,
128.318433909601)) ;
#153497 = CARTESIAN_POINT('Ctrl Pts',(-25.9235411833855,13.1175341941134,
128.209680256936)) ;
#153498 = CARTESIAN_POINT('Ctrl Pts',(-25.8992723616796,13.4059954970849,
128.171974342421)) ;
#153499 = CARTESIAN_POINT('Ctrl Pts',(-25.9001789667653,13.6942419645787,
128.207632461566)) ;
#153500 = CARTESIAN_POINT('Ctrl Pts',(-25.9258216003677,13.9656571359195,
128.31589284879)) ;
#153501 = CARTESIAN_POINT('Ctrl Pts',(-25.9727492712161,14.1945698215837,
128.485818180082)) ;
#153502 = CARTESIAN_POINT('Ctrl Pts',(-26.0380351219601,14.3711224528334,
128.709801837872)) ;
#153503 = CARTESIAN_POINT('Ctrl Pts',(-26.115372034482,14.4785950091488,128.968780330961)) ;
#153504 = CARTESIAN_POINT('Ctrl Pts',(-26.1991386228248,14.5108133112394,
129.246686766249)) ;
#153505 = CARTESIAN_POINT('Ctrl Pts',(-26.281961118953,14.4650394200622,129.521689731091)) ;
#153506 = CARTESIAN_POINT('Ctrl Pts',(-26.3576691539897,14.3446919400874,
129.775975443665)) ;
#153507 = CARTESIAN_POINT('Ctrl Pts',(-26.4199450377268,14.1586507898245,
129.990981699106)) ;
#153508 = CARTESIAN_POINT('Ctrl Pts',(-26.4638325348643,13.9182142591253,
130.152493567261)) ;
#153509 = CARTESIAN_POINT('Ctrl Pts',(-26.4849121372087,13.6446894301756,
130.247054976681)) ;
#153510 = CARTESIAN_POINT('Ctrl Pts',(-26.4814409395297,13.3538163555555,
130.270090586414)) ;
#153511 = CARTESIAN_POINT('Ctrl Pts',(-26.4527946492839,13.0687529323482,
130.219476965581)) ;
#153512 = CARTESIAN_POINT('Ctrl Pts',(-26.4002320096581,12.8084025711039,
130.099079794229)) ;
#153513 = CARTESIAN_POINT('Ctrl Pts',(-26.3268756685072,12.5923662507696,
129.91790410308)) ;
#153514 = CARTESIAN_POINT('Ctrl Pts',(-26.2371123368209,12.4355966936421,
129.688843066008)) ;
#153515 = CARTESIAN_POINT('Ctrl Pts',(-26.1367181878628,12.3498834173245,
129.42872587461)) ;
#153516 = CARTESIAN_POINT('Ctrl Pts',(-26.032722719753,12.3409542808635,129.157919642926)) ;
#153517 = CARTESIAN_POINT('Ctrl Pts',(-25.9308084387583,12.4093757248112,
128.893357587352)) ;
#153518 = CARTESIAN_POINT('Ctrl Pts',(-25.838155620905,12.5505196315372,128.655821078007)) ;
#153519 = CARTESIAN_POINT('Ctrl Pts',(-25.7605740007468,12.7541803006072,
128.462316845571)) ;
#153520 = CARTESIAN_POINT('Ctrl Pts',(-25.7029450253967,13.0055267425044,
128.327067990315)) ;
#153521 = CARTESIAN_POINT('Ctrl Pts',(-25.6685657347824,13.2870724884799,
128.259776019344)) ;
#153522 = CARTESIAN_POINT('Ctrl Pts',(-25.6592502061655,13.5781354317469,
128.265673438089)) ;
#153523 = CARTESIAN_POINT('Ctrl Pts',(-25.6749179654199,13.8583662507443,
128.344586199981)) ;
#153524 = CARTESIAN_POINT('Ctrl Pts',(-25.7137374162889,14.1072755060793,
128.491117013587)) ;
#153525 = CARTESIAN_POINT('Ctrl Pts',(-25.7721169966564,14.3069765889331,
128.694755702354)) ;
#153526 = CARTESIAN_POINT('Ctrl Pts',(-25.845207577047,14.443614067786,128.941381531894)) ;
#153527 = CARTESIAN_POINT('Ctrl Pts',(-25.9273346325596,14.5071928082345,
129.214515131727)) ;
#153528 = CARTESIAN_POINT('Ctrl Pts',(-26.011234962119,14.4928945220509,129.492675842775)) ;
#153529 = CARTESIAN_POINT('Ctrl Pts',(-26.0906570279007,14.4021254936154,
129.757803067043)) ;
#153530 = CARTESIAN_POINT('Ctrl Pts',(-26.159082383682,14.2413770477371,129.990792154917)) ;
#153531 = CARTESIAN_POINT('Ctrl Pts',(-26.2110152100895,14.0210258594474,
130.175736142196)) ;
#153532 = CARTESIAN_POINT('Ctrl Pts',(-26.241635177827,13.7594508415378,130.298196601018)) ;
#153533 = CARTESIAN_POINT('Ctrl Pts',(-26.2483473113095,13.4716753030503,
130.351078692086)) ;
#153534 = CARTESIAN_POINT('Ctrl Pts',(-26.2298541426232,13.18278007244,130.330045835803)) ;
#153535 = CARTESIAN_POINT('Ctrl Pts',(-26.1867418068547,12.9097866347109,
130.237249070666)) ;
#153536 = CARTESIAN_POINT('Ctrl Pts',(-26.1214552754847,12.6739761120234,
130.079613973061)) ;
#153537 = CARTESIAN_POINT('Ctrl Pts',(-26.037598712626,12.4911376353209,129.867849268882)) ;
#153538 = CARTESIAN_POINT('Ctrl Pts',(-25.9407649580424,12.3755758788311,
129.618129131331)) ;
#153539 = CARTESIAN_POINT('Ctrl Pts',(-25.8374214950217,12.3352662329562,
129.34929906656)) ;
#153540 = CARTESIAN_POINT('Ctrl Pts',(-25.7340098362028,12.3722006143293,
129.0802369826)) ;
#153541 = CARTESIAN_POINT('Ctrl Pts',(-25.6361773432197,12.4858118722087,
128.827819165484)) ;
#153542 = CARTESIAN_POINT('Ctrl Pts',(-25.5523274084712,12.6649628027199,
128.615825895545)) ;
#153543 = CARTESIAN_POINT('Ctrl Pts',(-25.4859513870995,12.8995424291904,
128.455121245363)) ;
#153544 = CARTESIAN_POINT('Ctrl Pts',(-25.4419863750333,13.1707489990253,
128.359746169264)) ;
#153545 = CARTESIAN_POINT('Ctrl Pts',(-25.4224009992562,13.4602465419289,
128.335630931104)) ;
#153546 = CARTESIAN_POINT('Ctrl Pts',(-25.4281061795563,13.7479094104328,
128.385491263721)) ;
#153547 = CARTESIAN_POINT('Ctrl Pts',(-25.4578216450762,14.0110933638022,
128.505345635233)) ;
#153548 = CARTESIAN_POINT('Ctrl Pts',(-25.5087967768197,14.2330195298938,
128.687396943834)) ;
#153549 = CARTESIAN_POINT('Ctrl Pts',(-25.5768933622651,14.397056415232,128.919554215411)) ;
#153550 = CARTESIAN_POINT('Ctrl Pts',(-25.6558147544988,14.4906410938832,
129.183138561615)) ;
#153551 = CARTESIAN_POINT('Ctrl Pts',(-25.7399301950195,14.5080280130628,
129.462041474598)) ;
#153552 = CARTESIAN_POINT('Ctrl Pts',(-25.8217364878674,14.4480725424633,
129.734011003358)) ;
#153553 = CARTESIAN_POINT('Ctrl Pts',(-25.8956483813608,14.3139470607326,
129.983179734343)) ;
#153554 = CARTESIAN_POINT('Ctrl Pts',(-25.9546615112484,14.1169437524237,
130.188609280051)) ;
#153555 = CARTESIAN_POINT('Ctrl Pts',(-25.994519421204,13.8684682048696,130.338337741358)) ;
#153556 = CARTESIAN_POINT('Ctrl Pts',(-26.0110568377318,13.5907243651,130.419594305655)) ;
#153557 = CARTESIAN_POINT('Ctrl Pts',(-26.0028570943019,13.2994062522709,
130.428791647391)) ;
#153558 = CARTESIAN_POINT('Ctrl Pts',(-25.9695704025357,13.0173302811176,
130.364651136717)) ;
#153559 = CARTESIAN_POINT('Ctrl Pts',(-25.9127012517306,12.7634586998748,
130.23173138777)) ;
#153560 = CARTESIAN_POINT('Ctrl Pts',(-25.8356694959319,12.5574053612187,
130.039883250671)) ;
#153561 = CARTESIAN_POINT('Ctrl Pts',(-25.7439581375389,12.4141338116398,
129.804942699892)) ;
#153562 = CARTESIAN_POINT('Ctrl Pts',(-25.6422361078924,12.342233208706,129.540970477651)) ;
#153563 = CARTESIAN_POINT('Ctrl Pts',(-25.5379082160016,12.3479816385131,
129.269286803224)) ;
#153564 = CARTESIAN_POINT('Ctrl Pts',(-25.4372492426153,12.4308508598937,
129.00839512309)) ;
#153565 = CARTESIAN_POINT('Ctrl Pts',(-25.3472402005208,12.5841342714032,
128.778486490676)) ;
#153566 = CARTESIAN_POINT('Ctrl Pts',(-25.272730898508,12.7991564308112,128.594122402279)) ;
#153567 = CARTESIAN_POINT('Ctrl Pts',(-25.2194888387276,13.0569999610756,
128.471595214616)) ;
#153568 = CARTESIAN_POINT('Ctrl Pts',(-25.1897401476562,13.3421921034464,
128.417860044275)) ;
#153569 = CARTESIAN_POINT('Ctrl Pts',(-25.1851966857885,13.6321454574867,
128.437625751363)) ;
#153570 = CARTESIAN_POINT('Ctrl Pts',(-25.2054882351433,13.9089725412032,
128.530163374861)) ;
#153571 = CARTESIAN_POINT('Ctrl Pts',(-25.2484501051326,14.1498188340954,
128.688812325716)) ;
#153572 = CARTESIAN_POINT('Ctrl Pts',(-25.3098239459612,14.3379335225619,
128.901090604678)) ;
#153573 = CARTESIAN_POINT('Ctrl Pts',(-25.3852409841119,14.4615825769609,
129.154594863581)) ;
#153574 = CARTESIAN_POINT('Ctrl Pts',(-25.4680078103566,14.5104718339952,
129.429479188798)) ;
#153575 = CARTESIAN_POINT('Ctrl Pts',(-25.5519233175472,14.4813917081873,
129.707831723369)) ;
#153576 = CARTESIAN_POINT('Ctrl Pts',(-25.6296594879759,14.3764101476522,
129.968016081421)) ;
#153577 = CARTESIAN_POINT('Ctrl Pts',(-25.6951131634194,14.2041613001764,
130.192211432841)) ;
#153578 = CARTESIAN_POINT('Ctrl Pts',(-25.7434116042681,13.9743839791119,
130.36655070585)) ;
#153579 = CARTESIAN_POINT('Ctrl Pts',(-25.7697062526325,13.7063210401926,
130.476427371815)) ;
#153580 = CARTESIAN_POINT('Ctrl Pts',(-25.7716643333024,13.416701167449,130.515370896243)) ;
#153581 = CARTESIAN_POINT('Ctrl Pts',(-25.7484303453548,13.1291677758352,
130.480525076402)) ;
#153582 = CARTESIAN_POINT('Ctrl Pts',(-25.7008468729498,12.86171027905,130.374668312212)) ;
#153583 = CARTESIAN_POINT('Ctrl Pts',(-25.6318421414092,12.6350478480017,
130.206135995294)) ;
#153584 = CARTESIAN_POINT('Ctrl Pts',(-25.5450073178082,12.4638699665219,
129.985698129429)) ;
#153585 = CARTESIAN_POINT('Ctrl Pts',(-25.4465855133018,12.3621126869917,
129.731275230113)) ;
#153586 = CARTESIAN_POINT('Ctrl Pts',(-25.3422723144961,12.336288293437,129.459748523319)) ;
#153587 = CARTESIAN_POINT('Ctrl Pts',(-25.2395464146887,12.3882079133966,
129.192710014154)) ;
#153588 = CARTESIAN_POINT('Ctrl Pts',(-25.1441554739243,12.5148240028862,
128.947268201873)) ;
#153589 = CARTESIAN_POINT('Ctrl Pts',(-25.0632912716036,12.7050812653244,
128.743995286524)) ;
#153590 = CARTESIAN_POINT('Ctrl Pts',(-25.0008040035337,12.9482677220772,
128.594669933562)) ;
#153591 = CARTESIAN_POINT('Ctrl Pts',(-24.9612989083473,13.2238578222556,
128.512263188183)) ;
#153592 = CARTESIAN_POINT('Ctrl Pts',(-24.9464400414306,13.5162932448957,
128.502169911524)) ;
#153593 = CARTESIAN_POINT('Ctrl Pts',(-24.9567559801261,13.799165239793,128.565264390033)) ;
#153594 = CARTESIAN_POINT('Ctrl Pts',(-24.9910303138475,14.0580267764743,
128.698731518742)) ;
#153595 = CARTESIAN_POINT('Ctrl Pts',(-25.0453888541943,14.2686028129511,
128.890481281382)) ;
#153596 = CARTESIAN_POINT('Ctrl Pts',(-25.1157749327763,14.4199618502008,
129.129219228183)) ;
#153597 = CARTESIAN_POINT('Ctrl Pts',(-25.1962537469819,14.4998958219189,
129.397417258709)) ;
#153598 = CARTESIAN_POINT('Ctrl Pts',(-25.2806998076144,14.5025664794371,
129.677347381576)) ;
#153599 = CARTESIAN_POINT('Ctrl Pts',(-25.3614130293349,14.4280652825415,
129.946141834169)) ;
#153600 = CARTESIAN_POINT('Ctrl Pts',(-25.4327613411336,14.2819177513075,
130.187667258866)) ;
#153601 = CARTESIAN_POINT('Ctrl Pts',(-25.4888836010397,14.0723877227319,
130.384948804485)) ;
#153602 = CARTESIAN_POINT('Ctrl Pts',(-25.524217369076,13.8191595273478,130.52109290564)) ;
#153603 = CARTESIAN_POINT('Ctrl Pts',(-25.5363621720147,13.5356702848312,
130.589764696207)) ;
#153604 = CARTESIAN_POINT('Ctrl Pts',(-25.5233799731752,13.2451626614465,
130.584896539849)) ;
#153605 = CARTESIAN_POINT('Ctrl Pts',(-25.4853193673611,12.9658959397094,
130.506957297054)) ;
#153606 = CARTESIAN_POINT('Ctrl Pts',(-25.4245567948317,12.720867949973,130.362513148524)) ;
#153607 = CARTESIAN_POINT('Ctrl Pts',(-25.3444357384131,12.5256178596935,
130.161588938401)) ;
#153608 = CARTESIAN_POINT('Ctrl Pts',(-25.2502354927177,12.3947249390078,
129.91946984754)) ;
#153609 = CARTESIAN_POINT('Ctrl Pts',(-25.1471557384846,12.3373274128747,
129.651622343389)) ;
#153610 = CARTESIAN_POINT('Ctrl Pts',(-25.04352722843,12.3577351376061,129.3818280718)) ;
#153611 = CARTESIAN_POINT('Ctrl Pts',(-24.9440625937448,12.4546492514378,
129.124509048456)) ;
#153612 = CARTESIAN_POINT('Ctrl Pts',(-24.8564471604785,12.6210676591383,
128.901700870073)) ;
#153613 = CARTESIAN_POINT('Ctrl Pts',(-24.7859855036776,12.8446766854148,
128.728972290107)) ;
#153614 = CARTESIAN_POINT('Ctrl Pts',(-24.7369148940067,13.108808163257,128.618635013836)) ;
#153615 = CARTESIAN_POINT('Ctrl Pts',(-24.7117898455147,13.3979062620311,
128.578541432007)) ;
#153616 = CARTESIAN_POINT('Ctrl Pts',(-24.7120774707783,13.6859097607706,
128.612344349061)) ;
#153617 = CARTESIAN_POINT('Ctrl Pts',(-24.7366917620368,13.9567565280856,
128.717390290963)) ;
#153618 = CARTESIAN_POINT('Ctrl Pts',(-24.7836759760245,14.1899349125241,
128.887914867791)) ;
#153619 = CARTESIAN_POINT('Ctrl Pts',(-24.8478937377255,14.3662692626876,
129.10842421568)) ;
#153620 = CARTESIAN_POINT('Ctrl Pts',(-24.9254379812952,14.4768289979695,
129.368240618362)) ;
#153621 = CARTESIAN_POINT('Ctrl Pts',(-25.0089189154175,14.5109207090365,
129.645218161262)) ;
#153622 = CARTESIAN_POINT('Ctrl Pts',(-25.0919501200887,14.4673589954117,
129.920875758852)) ;
#153623 = CARTESIAN_POINT('Ctrl Pts',(-25.1679324131496,14.3490298117359,
130.175949093355)) ;
#153624 = CARTESIAN_POINT('Ctrl Pts',(-25.2306776791176,14.1643442573792,
130.392364551844)) ;
#153625 = CARTESIAN_POINT('Ctrl Pts',(-25.2749172208417,13.9269540764464,
130.554674425406)) ;
#153626 = CARTESIAN_POINT('Ctrl Pts',(-25.296881801977,13.6529087066834,130.651991768824)) ;
#153627 = CARTESIAN_POINT('Ctrl Pts',(-25.294121582554,13.3625040426011,130.677064089887)) ;
#153628 = CARTESIAN_POINT('Ctrl Pts',(-25.2661584777254,13.0764917625792,
130.628507586136)) ;
#153629 = CARTESIAN_POINT('Ctrl Pts',(-25.2142358128611,12.8152457852602,
130.509968872735)) ;
#153630 = CARTESIAN_POINT('Ctrl Pts',(-25.1414105163864,12.5977360848388,
130.330346617025)) ;
#153631 = CARTESIAN_POINT('Ctrl Pts',(-25.0521369052221,12.4392301767845,
130.102679861577)) ;
#153632 = CARTESIAN_POINT('Ctrl Pts',(-24.9519825847367,12.3513755992719,
129.843259987167)) ;
#153633 = CARTESIAN_POINT('Ctrl Pts',(-24.8480528333298,12.3399316332142,
129.572627714051)) ;
#153634 = CARTESIAN_POINT('Ctrl Pts',(-24.7452323261505,12.4070554351268,
129.305672373312)) ;
#153635 = CARTESIAN_POINT('Ctrl Pts',(-24.653114699296,12.5451369869361,129.069390792946)) ;
#153636 = CARTESIAN_POINT('Ctrl Pts',(-24.574658401759,12.7477726868892,128.873467031278)) ;
#153637 = CARTESIAN_POINT('Ctrl Pts',(-24.516485448288,12.9979367372735,128.736605448719)) ;
#153638 = CARTESIAN_POINT('Ctrl Pts',(-24.4813744014041,13.2792370978739,
128.667217092649)) ;
#153639 = CARTESIAN_POINT('Ctrl Pts',(-24.4713970354524,13.5701580555343,
128.671163049425)) ;
#153640 = CARTESIAN_POINT('Ctrl Pts',(-24.4863380916386,13.8505377724051,
128.747899411962)) ;
#153641 = CARTESIAN_POINT('Ctrl Pts',(-24.5245439679385,14.1007512372239,
128.892655666103)) ;
#153642 = CARTESIAN_POINT('Ctrl Pts',(-24.5824402788279,14.3021715583994,
129.094893574169)) ;
#153643 = CARTESIAN_POINT('Ctrl Pts',(-24.6554257346924,14.4410638226486,
129.341309329826)) ;
#153644 = CARTESIAN_POINT('Ctrl Pts',(-24.7373356695316,14.506420576945,129.613776649341)) ;
#153645 = CARTESIAN_POINT('Ctrl Pts',(-24.8210078848283,14.4944296739133,
129.89116801343)) ;
#153646 = CARTESIAN_POINT('Ctrl Pts',(-24.9008406879447,14.4055611915821,
130.157574926146)) ;
#153647 = CARTESIAN_POINT('Ctrl Pts',(-24.9694636925505,14.2469875620131,
130.391056099313)) ;
#153648 = CARTESIAN_POINT('Ctrl Pts',(-25.0219599711088,14.0284942715184,
130.577615505577)) ;
#153649 = CARTESIAN_POINT('Ctrl Pts',(-25.053320022464,13.7670074742828,130.70234813533)) ;
#153650 = CARTESIAN_POINT('Ctrl Pts',(-25.0607089051815,13.4805781215048,
130.757097162265)) ;
#153651 = CARTESIAN_POINT('Ctrl Pts',(-25.0430061476845,13.1913388058783,
130.73838961606)) ;
#153652 = CARTESIAN_POINT('Ctrl Pts',(-25.0005234997867,12.9172330933754,
130.647473812606)) ;
#153653 = CARTESIAN_POINT('Ctrl Pts',(-24.9358367964898,12.6799728703758,
130.491596969194)) ;
#153654 = CARTESIAN_POINT('Ctrl Pts',(-24.8520526958292,12.4949910418975,
130.280173035867)) ;
#153655 = CARTESIAN_POINT('Ctrl Pts',(-24.756283433586,12.3781840447206,130.033296564361)) ;
#153656 = CARTESIAN_POINT('Ctrl Pts',(-24.6522083130104,12.3352411023339,
129.762603753164)) ;
#153657 = CARTESIAN_POINT('Ctrl Pts',(-24.5492013359519,12.3701183957634,
129.494563600041)) ;
#153658 = CARTESIAN_POINT('Ctrl Pts',(-24.4510228781676,12.4815908370187,
129.241159666924)) ;
#153659 = CARTESIAN_POINT('Ctrl Pts',(-24.3668186999168,12.6586744463426,
129.02808228214)) ;
#153660 = CARTESIAN_POINT('Ctrl Pts',(-24.2996856218142,12.8927064505131,
128.86527445598)) ;
#153661 = CARTESIAN_POINT('Ctrl Pts',(-24.2552426505653,13.1615895986342,
128.768318934161)) ;
#153662 = CARTESIAN_POINT('Ctrl Pts',(-24.2347791741716,13.4527337961883,
128.741859841865)) ;
#153663 = CARTESIAN_POINT('Ctrl Pts',(-24.2398184692911,13.7397606263225,
128.789657130047)) ;
#153664 = CARTESIAN_POINT('Ctrl Pts',(-24.2689320023009,14.0044956878458,
128.907831044878)) ;
#153665 = CARTESIAN_POINT('Ctrl Pts',(-24.3192589693072,14.2270717047825,
129.087893938316)) ;
#153666 = CARTESIAN_POINT('Ctrl Pts',(-24.386637598686,14.3928428531141,129.31784383242)) ;
#153667 = CARTESIAN_POINT('Ctrl Pts',(-24.4659391407555,14.4891679896536,
129.582798342604)) ;
#153668 = CARTESIAN_POINT('Ctrl Pts',(-24.5493645856168,14.5086708936273,
129.859423076708)) ;
#153669 = CARTESIAN_POINT('Ctrl Pts',(-24.6318807172738,14.4507091204102,
130.133696348165)) ;
#153670 = CARTESIAN_POINT('Ctrl Pts',(-24.7058567597393,14.318823465338,130.382937634357)) ;
#153671 = CARTESIAN_POINT('Ctrl Pts',(-24.7654056750014,14.1234067424229,
130.589957999186)) ;
#153672 = CARTESIAN_POINT('Ctrl Pts',(-24.8057595992627,13.8772496577341,
130.740994985991)) ;
#153673 = CARTESIAN_POINT('Ctrl Pts',(-24.8231799857801,13.5994498547175,
130.82492878504)) ;
#153674 = CARTESIAN_POINT('Ctrl Pts',(-24.8155893045152,13.3067289539218,
130.836068714423)) ;
#153675 = CARTESIAN_POINT('Ctrl Pts',(-24.7830973206933,13.025513208076,130.774091996489)) ;
#153676 = CARTESIAN_POINT('Ctrl Pts',(-24.7270577046474,12.7708776887036,
130.643534343482)) ;
#153677 = CARTESIAN_POINT('Ctrl Pts',(-24.6505077984341,12.5628412979246,
130.453131427416)) ;
#153678 = CARTESIAN_POINT('Ctrl Pts',(-24.5589760348122,12.4171764122364,
130.218786009453)) ;
#153679 = CARTESIAN_POINT('Ctrl Pts',(-24.4570551071365,12.3431378359771,
129.954350410602)) ;
#153680 = CARTESIAN_POINT('Ctrl Pts',(-24.3533214115063,12.3467434972734,
129.684210676246)) ;
#153681 = CARTESIAN_POINT('Ctrl Pts',(-24.2523283182393,12.4272274658185,
129.422376802438)) ;
#153682 = CARTESIAN_POINT('Ctrl Pts',(-24.1617932807192,12.5790158149027,
129.190994958755)) ;
#153683 = CARTESIAN_POINT('Ctrl Pts',(-24.0869579392724,12.7916687829571,
129.005564094205)) ;
#153684 = CARTESIAN_POINT('Ctrl Pts',(-24.0328055760906,13.0498138992039,
128.8805514449)) ;
#153685 = CARTESIAN_POINT('Ctrl Pts',(-24.002521804032,13.3331756720239,128.825089124936)) ;
#153686 = CARTESIAN_POINT('Ctrl Pts',(-23.9971725769105,13.6238935345468,
128.842575947387)) ;
#153687 = CARTESIAN_POINT('Ctrl Pts',(-24.0167753636582,13.9010885274901,
128.933062863381)) ;
#153688 = CARTESIAN_POINT('Ctrl Pts',(-24.0590128945408,14.1432054793993,
129.089568959686)) ;
#153689 = CARTESIAN_POINT('Ctrl Pts',(-24.1203695555296,14.3341070280144,
129.302019247719)) ;
#153690 = CARTESIAN_POINT('Ctrl Pts',(-24.1950418049019,14.4587991787124,
129.553138711427)) ;
#153691 = CARTESIAN_POINT('Ctrl Pts',(-24.2777268658875,14.5101605081857,
129.827811432152)) ;
#153692 = CARTESIAN_POINT('Ctrl Pts',(-24.3615395865942,14.4834097576633,
130.105796352381)) ;
#153693 = CARTESIAN_POINT('Ctrl Pts',(-24.4396001237497,14.380986704451,130.366925214371)) ;
#153694 = CARTESIAN_POINT('Ctrl Pts',(-24.5059188478657,14.2089571607828,
130.593906733665)) ;
#153695 = CARTESIAN_POINT('Ctrl Pts',(-24.5543423873352,13.9828180453883,
130.768283768123)) ;
#153696 = CARTESIAN_POINT('Ctrl Pts',(-24.5815804292821,13.7132629209954,
130.881224790375)) ;
#153697 = CARTESIAN_POINT('Ctrl Pts',(-24.5841620980753,13.42583764063,130.921759059005)) ;
#153698 = CARTESIAN_POINT('Ctrl Pts',(-24.5616991302751,13.1374631065902,
130.889232264708)) ;
#153699 = CARTESIAN_POINT('Ctrl Pts',(-24.5148271925072,12.8691197006536,
130.785439835784)) ;
#153700 = CARTESIAN_POINT('Ctrl Pts',(-24.4460595852779,12.6403113443668,
130.617737495797)) ;
#153701 = CARTESIAN_POINT('Ctrl Pts',(-24.3602783070861,12.468420702256,130.400139902644)) ;
#153702 = CARTESIAN_POINT('Ctrl Pts',(-24.2614984282295,12.3638000217504,
130.144889114756)) ;
#153703 = CARTESIAN_POINT('Ctrl Pts',(-24.1577920148866,12.3359859144704,
129.874955907544)) ;
#153704 = CARTESIAN_POINT('Ctrl Pts',(-24.054756872384,12.3855342690204,129.607074345636)) ;
#153705 = CARTESIAN_POINT('Ctrl Pts',(-23.9592387590454,12.5097023136888,
129.361184743235)) ;
#153706 = CARTESIAN_POINT('Ctrl Pts',(-23.8775758716564,12.6987169895182,
129.155691106511)) ;
#153707 = CARTESIAN_POINT('Ctrl Pts',(-23.8143557456443,12.9413958856346,
129.004310292951)) ;
#153708 = CARTESIAN_POINT('Ctrl Pts',(-23.7742609530853,13.2164083911014,
128.920187229679)) ;
#153709 = CARTESIAN_POINT('Ctrl Pts',(-23.7587189631835,13.5077476116907,
128.907983756604)) ;
#153710 = CARTESIAN_POINT('Ctrl Pts',(-23.7683966260473,13.7917084995172,
128.969294505237)) ;
#153711 = CARTESIAN_POINT('Ctrl Pts',(-23.8017090745378,14.0497089633418,
129.099691778832)) ;
#153712 = CARTESIAN_POINT('Ctrl Pts',(-23.855687851068,14.2632250030891,129.290500820459)) ;
#153713 = CARTESIAN_POINT('Ctrl Pts',(-23.9259445764529,14.4168537708596,
129.528960264585)) ;
#153714 = CARTESIAN_POINT('Ctrl Pts',(-24.0063154571533,14.4987598986465,
129.796873298139)) ;
#153715 = CARTESIAN_POINT('Ctrl Pts',(-24.0905209887515,14.5035045718472,
130.07601230486)) ;
#153716 = CARTESIAN_POINT('Ctrl Pts',(-24.1714640122117,14.4313229997249,
130.345485263966)) ;
#153717 = CARTESIAN_POINT('Ctrl Pts',(-24.243380136318,14.286096674379,130.588809864043)) ;
#153718 = CARTESIAN_POINT('Ctrl Pts',(-24.2994203289572,14.0806888556304,
130.785462444038)) ;
#153719 = CARTESIAN_POINT('Ctrl Pts',(-24.3358061636431,13.8265805447723,
130.924971011733)) ;
#153720 = CARTESIAN_POINT('Ctrl Pts',(-24.3485662665821,13.5441879409374,
130.995358908411)) ;
#153721 = CARTESIAN_POINT('Ctrl Pts',(-24.3362787692544,13.2530370689606,
130.992594119063)) ;
#153722 = CARTESIAN_POINT('Ctrl Pts',(-24.2990565233592,12.9741114175935,
130.916980614884)) ;
#153723 = CARTESIAN_POINT('Ctrl Pts',(-24.2387980421576,12.7272119216586,
130.774093243821)) ;
#153724 = CARTESIAN_POINT('Ctrl Pts',(-24.1592542721153,12.5305677659782,
130.57481255156)) ;
#153725 = CARTESIAN_POINT('Ctrl Pts',(-24.0653992661587,12.3976028767503,
130.333704016612)) ;
#153726 = CARTESIAN_POINT('Ctrl Pts',(-23.9625403093089,12.3378877564715,
130.06647786499)) ;
#153727 = CARTESIAN_POINT('Ctrl Pts',(-23.8586656317476,12.3561146457162,
129.796030313594)) ;
#153728 = CARTESIAN_POINT('Ctrl Pts',(-23.7592617382335,12.4504996091204,
129.538781451731)) ;
#153729 = CARTESIAN_POINT('Ctrl Pts',(-23.6710781493093,12.6151918179393,
129.314368558311)) ;
#153730 = CARTESIAN_POINT('Ctrl Pts',(-23.6000847768971,12.8367627956422,
129.140023816127)) ;
#153731 = CARTESIAN_POINT('Ctrl Pts',(-23.5500037307086,13.102471284239,129.027040548326)) ;
#153732 = CARTESIAN_POINT('Ctrl Pts',(-23.5244629176484,13.388098474674,128.985365037134)) ;
#153733 = CARTESIAN_POINT('Ctrl Pts',(-23.5239179211507,13.6786302634614,
129.017000214703)) ;
#153734 = CARTESIAN_POINT('Ctrl Pts',(-23.5479482075075,13.9495118019851,
129.120261172471)) ;
#153735 = CARTESIAN_POINT('Ctrl Pts',(-23.5940539896427,14.1831630717315,
129.28807205042)) ;
#153736 = CARTESIAN_POINT('Ctrl Pts',(-23.658087369295,14.3622887251467,129.508197418047)) ;
#153737 = CARTESIAN_POINT('Ctrl Pts',(-23.7354964858561,14.4748192529362,
129.767663246934)) ;
#153738 = CARTESIAN_POINT('Ctrl Pts',(-23.8186008712506,14.5109473630978,
130.043427649505)) ;
#153739 = CARTESIAN_POINT('Ctrl Pts',(-23.9016485189198,14.46989386631,130.319093678178)) ;
#153740 = CARTESIAN_POINT('Ctrl Pts',(-23.9780326629865,14.3536144736526,
130.57538079303)) ;
#153741 = CARTESIAN_POINT('Ctrl Pts',(-24.041317392537,14.17062113719,130.793395793898)) ;
#153742 = CARTESIAN_POINT('Ctrl Pts',(-24.0862233608817,13.933736573907,130.957750623604)) ;
#153743 = CARTESIAN_POINT('Ctrl Pts',(-24.1087782693582,13.6617104442443,
131.056639640472)) ;
#153744 = CARTESIAN_POINT('Ctrl Pts',(-24.1067652069901,13.3701432171844,
131.084050982405)) ;
#153745 = CARTESIAN_POINT('Ctrl Pts',(-24.0794150200347,13.0839501475181,
131.037263800254)) ;
#153746 = CARTESIAN_POINT('Ctrl Pts',(-24.0283415442683,12.8226369063403,
130.921088721576)) ;
#153747 = CARTESIAN_POINT('Ctrl Pts',(-23.9561135287856,12.6036153158418,
130.74320474868)) ;
#153748 = CARTESIAN_POINT('Ctrl Pts',(-23.8674374985634,12.4432239429731,
130.517228131168)) ;
#153749 = CARTESIAN_POINT('Ctrl Pts',(-23.7669177824065,12.3525997513282,
130.256937329486)) ;
#153750 = CARTESIAN_POINT('Ctrl Pts',(-23.6631589097691,12.3393903655815,
129.986759745082)) ;
#153751 = CARTESIAN_POINT('Ctrl Pts',(-23.5608451726887,12.403468098602,129.721057322036)) ;
#153752 = CARTESIAN_POINT('Ctrl Pts',(-23.4675538333872,12.5405072085783,
129.481626938511)) ;
#153753 = CARTESIAN_POINT('Ctrl Pts',(-23.388662980097,12.7420005519616,129.284449551793)) ;
#153754 = CARTESIAN_POINT('Ctrl Pts',(-23.3301053404809,12.9900801149227,
129.146339662681)) ;
#153755 = CARTESIAN_POINT('Ctrl Pts',(-23.2942598700259,13.2708158721555,
129.07481369419)) ;
#153756 = CARTESIAN_POINT('Ctrl Pts',(-23.2835507653219,13.5613604134334,
129.07658052044)) ;
#153757 = CARTESIAN_POINT('Ctrl Pts',(-23.2977457009926,13.8428560081929,
129.151189048699)) ;
#153758 = CARTESIAN_POINT('Ctrl Pts',(-23.3355877732922,14.0951246502648,
129.295029201952)) ;
#153759 = CARTESIAN_POINT('Ctrl Pts',(-23.392640021767,14.2968154125605,129.494589775277)) ;
#153760 = CARTESIAN_POINT('Ctrl Pts',(-23.4654695271126,14.4382062812648,
129.740653917803)) ;
#153761 = CARTESIAN_POINT('Ctrl Pts',(-23.5470349400498,14.5055713938207,
130.012034404642)) ;
#153762 = CARTESIAN_POINT('Ctrl Pts',(-23.6308595315768,14.4957941932041,
130.289927886282)) ;
#153763 = CARTESIAN_POINT('Ctrl Pts',(-23.7106798599952,14.4095662340998,
130.556186374908)) ;
#153764 = CARTESIAN_POINT('Ctrl Pts',(-23.7802571461447,14.2515335127425,
130.792730605287)) ;
#153765 = CARTESIAN_POINT('Ctrl Pts',(-23.8330271584667,14.0347236874785,
130.979999898394)) ;
#153766 = CARTESIAN_POINT('Ctrl Pts',(-23.8649144470802,13.7751700114088,
131.106159195577)) ;
#153767 = CARTESIAN_POINT('Ctrl Pts',(-23.8730939748177,13.489555102194,131.163174955555)) ;
#153768 = CARTESIAN_POINT('Ctrl Pts',(-23.8560200827014,13.1989624545804,
131.146444379055)) ;
#153769 = CARTESIAN_POINT('Ctrl Pts',(-23.8142948031392,12.9245155762064,
131.057679563774)) ;
#153770 = CARTESIAN_POINT('Ctrl Pts',(-23.7497390288408,12.6850932088169,
130.90236186876)) ;
#153771 = CARTESIAN_POINT('Ctrl Pts',(-23.6676401734867,12.5007200500438,
130.695387264516)) ;
#153772 = CARTESIAN_POINT('Ctrl Pts',(-23.5710799792398,12.3802348015134,
130.446601105623)) ;
#153773 = CARTESIAN_POINT('Ctrl Pts',(-23.4680387193144,12.3354177830535,
130.178616720221)) ;
#153774 = CARTESIAN_POINT('Ctrl Pts',(-23.3639870057212,12.3682931650198,
129.907845197495)) ;
#153775 = CARTESIAN_POINT('Ctrl Pts',(-23.2665557781875,12.4764500222757,
129.656260795804)) ;
#153776 = CARTESIAN_POINT('Ctrl Pts',(-23.1812074615382,12.6527561756398,
129.440099421206)) ;
#153777 = CARTESIAN_POINT('Ctrl Pts',(-23.1137789148354,12.8841372675975,
129.276247072773)) ;
#153778 = CARTESIAN_POINT('Ctrl Pts',(-23.0682028417558,13.1550291136418,
129.176337392218)) ;
#153779 = CARTESIAN_POINT('Ctrl Pts',(-23.0472767378411,13.4437302360126,
129.148261982065)) ;
#153780 = CARTESIAN_POINT('Ctrl Pts',(-23.0515496084932,13.7319393007276,
129.193922359653)) ;
#153781 = CARTESIAN_POINT('Ctrl Pts',(-23.079878251099,13.9965481623833,129.309665379139)) ;
#153782 = CARTESIAN_POINT('Ctrl Pts',(-23.129741526764,14.2215298170475,129.488488454029)) ;
#153783 = CARTESIAN_POINT('Ctrl Pts',(-23.1968818888558,14.3891483272759,
129.717799600751)) ;
#153784 = CARTESIAN_POINT('Ctrl Pts',(-23.2754021964238,14.4871687024338,
129.980255089599)) ;
#153785 = CARTESIAN_POINT('Ctrl Pts',(-23.3593328759968,14.5093408079897,
130.258577404978)) ;
#153786 = CARTESIAN_POINT('Ctrl Pts',(-23.4420335332337,14.4530254583256,
130.533420307647)) ;
#153787 = CARTESIAN_POINT('Ctrl Pts',(-23.5159486858221,14.3240305585518,
130.782295669503)) ;
#153788 = CARTESIAN_POINT('Ctrl Pts',(-23.5763068870408,14.1290979717854,
130.991878121919)) ;
#153789 = CARTESIAN_POINT('Ctrl Pts',(-23.617068843589,13.8855604155571,131.143910620301)) ;
#153790 = CARTESIAN_POINT('Ctrl Pts',(-23.6352727286933,13.6058416707122,
131.230442968303)) ;
#153791 = CARTESIAN_POINT('Ctrl Pts',(-23.6283964341607,13.3160021377259,
131.243341112372)) ;
#153792 = CARTESIAN_POINT('Ctrl Pts',(-23.5965464340223,13.0326886676077,
131.183420690455)) ;
#153793 = CARTESIAN_POINT('Ctrl Pts',(-23.5408985622457,12.7766372190837,
131.054072194123)) ;
#153794 = CARTESIAN_POINT('Ctrl Pts',(-23.4649595861684,12.5676698161814,
130.865387166735)) ;
#153795 = CARTESIAN_POINT('Ctrl Pts',(-23.3740967453034,12.4206517790888,
130.632884178497)) ;
#153796 = CARTESIAN_POINT('Ctrl Pts',(-23.2727082372118,12.3443150505119,
130.369901024895)) ;
#153797 = CARTESIAN_POINT('Ctrl Pts',(-23.1684546893583,12.3454567433165,
130.098404386445)) ;
#153798 = CARTESIAN_POINT('Ctrl Pts',(-23.0671327036379,12.4241540146565,
129.835658717647)) ;
#153799 = CARTESIAN_POINT('Ctrl Pts',(-22.9764947583752,12.5736454649868,
129.60388157098)) ;
#153800 = CARTESIAN_POINT('Ctrl Pts',(-22.9011806814661,12.7844244258342,
129.417017819213)) ;
#153801 = CARTESIAN_POINT('Ctrl Pts',(-22.8463459628872,13.041264478038,129.289992771218)) ;
#153802 = CARTESIAN_POINT('Ctrl Pts',(-22.815230919969,13.3250313838274,129.232207692813)) ;
#153803 = CARTESIAN_POINT('Ctrl Pts',(-22.8092125202162,13.6156492492809,
129.247717690027)) ;
#153804 = CARTESIAN_POINT('Ctrl Pts',(-22.8280212526032,13.8929002803611,
129.335801002832)) ;
#153805 = CARTESIAN_POINT('Ctrl Pts',(-22.8696833153775,14.1366366428793,
129.490673844657)) ;
#153806 = CARTESIAN_POINT('Ctrl Pts',(-22.9303059421642,14.3287833833703,
129.70086742119)) ;
#153807 = CARTESIAN_POINT('Ctrl Pts',(-23.0049559964505,14.4563288342089,
129.952070625789)) ;
#153808 = CARTESIAN_POINT('Ctrl Pts',(-23.0876811988293,14.5097636463918,
130.226920951019)) ;
#153809 = CARTESIAN_POINT('Ctrl Pts',(-23.171313625943,14.4852491819093,130.504285160366)) ;
#153810 = CARTESIAN_POINT('Ctrl Pts',(-23.2495616828516,14.385213180382,130.765927789329)) ;
#153811 = CARTESIAN_POINT('Ctrl Pts',(-23.3164467304666,14.2148994362801,
130.994611083723)) ;
#153812 = CARTESIAN_POINT('Ctrl Pts',(-23.3654737459425,13.9895605141043,
131.170821580244)) ;
#153813 = CARTESIAN_POINT('Ctrl Pts',(-23.3932709418014,13.7226496289756,
131.285186238845)) ;
#153814 = CARTESIAN_POINT('Ctrl Pts',(-23.3966715321499,13.4342098859693,
131.328274909581)) ;
#153815 = CARTESIAN_POINT('Ctrl Pts',(-23.3749521692447,13.1458182759752,
131.297881508113)) ;
#153816 = CARTESIAN_POINT('Ctrl Pts',(-23.3285769346008,12.8759127132536,
131.195640591877)) ;
#153817 = CARTESIAN_POINT('Ctrl Pts',(-23.2608087751802,12.6468868556867,
131.030665242811)) ;
#153818 = CARTESIAN_POINT('Ctrl Pts',(-23.1749384545703,12.4721832296684,
130.81301511834)) ;
#153819 = CARTESIAN_POINT('Ctrl Pts',(-23.0772501521557,12.3661739274481,
130.560671910315)) ;
#153820 = CARTESIAN_POINT('Ctrl Pts',(-22.972758046801,12.3355863385396,130.288726503058)) ;
#153821 = CARTESIAN_POINT('Ctrl Pts',(-22.8698300820149,12.3831198658751,
130.021082533712)) ;
#153822 = CARTESIAN_POINT('Ctrl Pts',(-22.7739061268904,12.5053833023315,
129.774046335208)) ;
#153823 = CARTESIAN_POINT('Ctrl Pts',(-22.6919791045737,12.6923270702948,
129.567704270438)) ;
#153824 = CARTESIAN_POINT('Ctrl Pts',(-22.6281112723494,12.9335865705139,
129.414426275698)) ;
#153825 = CARTESIAN_POINT('Ctrl Pts',(-22.5872544610613,13.2085814539572,
129.328158922446)) ;
#153826 = CARTESIAN_POINT('Ctrl Pts',(-22.5710404902249,13.4990557588074,
129.313907984072)) ;
#153827 = CARTESIAN_POINT('Ctrl Pts',(-22.5799753665134,13.7836907462661,
129.373072556554)) ;
#153828 = CARTESIAN_POINT('Ctrl Pts',(-22.612638583778,14.0427281414566,129.501571243045)) ;
#153829 = CARTESIAN_POINT('Ctrl Pts',(-22.6660762367978,14.2577309750281,
129.69079806233)) ;
#153830 = CARTESIAN_POINT('Ctrl Pts',(-22.7357975374954,14.4131664617501,
129.927633756715)) ;
#153831 = CARTESIAN_POINT('Ctrl Pts',(-22.8161137666784,14.4973755702956,
130.195456113862)) ;
#153832 = CARTESIAN_POINT('Ctrl Pts',(-22.8998820017925,14.5046724130054,
130.47314586159)) ;
#153833 = CARTESIAN_POINT('Ctrl Pts',(-22.9816064513032,14.4343111747756,
130.745147804022)) ;
#153834 = CARTESIAN_POINT('Ctrl Pts',(-23.0536227051492,14.2913904033354,
130.98864811284)) ;
#153835 = CARTESIAN_POINT('Ctrl Pts',(-23.1102843211941,14.0872940403586,
131.187176359758)) ;
#153836 = CARTESIAN_POINT('Ctrl Pts',(-23.1472375329922,13.8349907742835,
131.328253449348)) ;
#153837 = CARTESIAN_POINT('Ctrl Pts',(-23.1607772342592,13.5522018199285,
131.401036362566)) ;
#153838 = CARTESIAN_POINT('Ctrl Pts',(-23.1491871925298,13.2611771320633,
131.400285897439)) ;
#153839 = CARTESIAN_POINT('Ctrl Pts',(-23.1125952006362,12.9814107201437,
131.326544774095)) ;
#153840 = CARTESIAN_POINT('Ctrl Pts',(-23.0531566614903,12.7341369610279,
131.185942865115)) ;
#153841 = CARTESIAN_POINT('Ctrl Pts',(-22.9739547949964,12.535166216503,130.98774443351)) ;
#153842 = CARTESIAN_POINT('Ctrl Pts',(-22.8800044204222,12.4000170891871,
130.746489022896)) ;
#153843 = CARTESIAN_POINT('Ctrl Pts',(-22.7777942394703,12.3385941106561,
130.480992016477)) ;
#153844 = CARTESIAN_POINT('Ctrl Pts',(-22.6737045237347,12.3545286685026,
130.209973410253)) ;
#153845 = CARTESIAN_POINT('Ctrl Pts',(-22.574018025731,12.4469846430608,129.951917332464)) ;
#153846 = CARTESIAN_POINT('Ctrl Pts',(-22.4853397321754,12.6102579412087,
129.726108518223)) ;
#153847 = CARTESIAN_POINT('Ctrl Pts',(-22.4141387274598,12.8296977311719,
129.551032278381)) ;
#153848 = CARTESIAN_POINT('Ctrl Pts',(-22.3635165048781,13.0929763552362,
129.436306120848)) ;
#153849 = CARTESIAN_POINT('Ctrl Pts',(-22.3370222640428,13.3798715107165,
129.392040554444)) ;
#153850 = CARTESIAN_POINT('Ctrl Pts',(-22.3358180956749,13.6705227535771,
129.421738962196)) ;
#153851 = CARTESIAN_POINT('Ctrl Pts',(-22.359121262081,13.9421700423004,129.522864634634)) ;
#153852 = CARTESIAN_POINT('Ctrl Pts',(-22.4048936915904,14.1780191011813,
129.689842088352)) ;
#153853 = CARTESIAN_POINT('Ctrl Pts',(-22.4683015911897,14.3579768124892,
129.908015928199)) ;
#153854 = CARTESIAN_POINT('Ctrl Pts',(-22.5452274463354,14.4725057553617,
130.165996866725)) ;
#153855 = CARTESIAN_POINT('Ctrl Pts',(-22.6283868280108,14.5110248787396,
130.441981808158)) ;
#153856 = CARTESIAN_POINT('Ctrl Pts',(-22.7115926468901,14.4721191969269,
130.718131866034)) ;
#153857 = CARTESIAN_POINT('Ctrl Pts',(-22.7882774144574,14.3577454336847,
130.975310558445)) ;
#153858 = CARTESIAN_POINT('Ctrl Pts',(-22.8518198048839,14.1770688666527,
131.193977525084)) ;
#153859 = CARTESIAN_POINT('Ctrl Pts',(-22.8974027115045,13.9416997327419,
131.360307596844)) ;
#153860 = CARTESIAN_POINT('Ctrl Pts',(-22.9206820190988,13.6694104353782,
131.461436266431)) ;
#153861 = CARTESIAN_POINT('Ctrl Pts',(-22.9194213574652,13.3798585935035,
131.490838835533)) ;
#153862 = CARTESIAN_POINT('Ctrl Pts',(-22.8929170330155,13.0927640382574,
131.446571141722)) ;
#153863 = CARTESIAN_POINT('Ctrl Pts',(-22.8423030043868,12.8294542733058,
131.331865445954)) ;
#153864 = CARTESIAN_POINT('Ctrl Pts',(-22.7706185679307,12.6090080043084,
131.155563913664)) ;
#153865 = CARTESIAN_POINT('Ctrl Pts',(-22.6821571255679,12.4466659582347,
130.930272433196)) ;
#153866 = CARTESIAN_POINT('Ctrl Pts',(-22.5824728331909,12.3544265354386,
130.672221564255)) ;
#153867 = CARTESIAN_POINT('Ctrl Pts',(-22.478522759517,12.338485550426,130.401560070963)) ;
#153868 = CARTESIAN_POINT('Ctrl Pts',(-22.3754966015088,12.4009576070215,
130.133958949611)) ;
#153869 = CARTESIAN_POINT('Ctrl Pts',(-22.2823680889779,12.5356622675021,
129.894847033385)) ;
#153870 = CARTESIAN_POINT('Ctrl Pts',(-22.2032360996956,12.7342792931547,
129.696815676907)) ;
#153871 = CARTESIAN_POINT('Ctrl Pts',(-22.1436939987442,12.9822470405306,
129.555989965758)) ;
#153872 = CARTESIAN_POINT('Ctrl Pts',(-22.1071406671597,13.2626104241267,
129.482419788097)) ;
#153873 = CARTESIAN_POINT('Ctrl Pts',(-22.0957144593787,13.5537330357078,
129.482159506806)) ;
#153874 = CARTESIAN_POINT('Ctrl Pts',(-22.1092685563454,13.8350780443648,
129.554823798795)) ;
#153875 = CARTESIAN_POINT('Ctrl Pts',(-22.1461475103679,14.0872562376869,
129.695659561939)) ;
#153876 = CARTESIAN_POINT('Ctrl Pts',(-22.2030821358645,14.2922552735091,
129.895131181954)) ;
#153877 = CARTESIAN_POINT('Ctrl Pts',(-22.2754289643042,14.4349645919609,
130.139699349458)) ;
#153878 = CARTESIAN_POINT('Ctrl Pts',(-22.3564708008619,14.5045540577175,
130.40942261917)) ;
#153879 = CARTESIAN_POINT('Ctrl Pts',(-22.4406441329642,14.4973581396257,
130.688457173911)) ;
#153880 = CARTESIAN_POINT('Ctrl Pts',(-22.5209414268602,14.4126016842873,
130.956235143864)) ;
#153881 = CARTESIAN_POINT('Ctrl Pts',(-22.5903401138937,14.2578370889756,
131.191978979017)) ;
#153882 = CARTESIAN_POINT('Ctrl Pts',(-22.643899231601,14.0423606370671,131.381638018117)) ;
#153883 = CARTESIAN_POINT('Ctrl Pts',(-22.676541227732,13.7833430848993,131.510062783894)) ;
#153884 = CARTESIAN_POINT('Ctrl Pts',(-22.6854014712124,13.4972454461382,
131.569174829683)) ;
#153885 = CARTESIAN_POINT('Ctrl Pts',(-22.6699589229826,13.2225256872019,
131.55537794912)) ;
#153886 = CARTESIAN_POINT('Ctrl Pts',(-22.6458119565126,13.0520853568101,
131.505271480944)) ;
#153887 = CARTESIAN_POINT('Ctrl Pts',(-22.6320187065114,12.9778651918053,
131.474336592418)) ;
#153888 = CARTESIAN_POINT('',(-33.2541723945531,13.1734341962953,127.827509047315)) ;
#153889 = CARTESIAN_POINT('Origin',(-33.2777287689504,13.1551399285885,127.896323413507)) ;
#153890 = CARTESIAN_POINT('',(-33.3012851433477,13.1368456608817,127.965137779698)) ;
#153891 = CARTESIAN_POINT('Origin',(-33.2777287689504,13.1551399285885,127.896323413507)) ;
#153892 = CARTESIAN_POINT('Origin',(-33.2777287689504,13.1551399285885,127.896323413507)) ;
#153893 = CARTESIAN_POINT('Ctrl Pts',(-22.3151378258161,14.5729486667267,
130.548644386657)) ;
#153894 = CARTESIAN_POINT('Ctrl Pts',(-22.329099593949,14.5730368300439,130.589430393716)) ;
#153895 = CARTESIAN_POINT('Ctrl Pts',(-22.3430755637926,14.5706665958407,
130.630257665154)) ;
#153896 = CARTESIAN_POINT('Ctrl Pts',(-22.3569679467077,14.5658273790944,
130.670840970083)) ;
#153897 = CARTESIAN_POINT('Ctrl Pts',(-22.3627375743675,14.5638176102188,
130.687695570196)) ;
#153898 = CARTESIAN_POINT('Ctrl Pts',(-22.3684933027053,14.5613818550179,
130.704509566733)) ;
#153899 = CARTESIAN_POINT('Ctrl Pts',(-22.3742281245136,14.5585193175848,
130.721262489797)) ;
#153900 = CARTESIAN_POINT('Ctrl Pts',(-22.4010526679328,14.5451298414636,
130.799624037403)) ;
#153901 = CARTESIAN_POINT('Ctrl Pts',(-22.4274099090546,14.5224036480322,
130.876620256302)) ;
#153902 = CARTESIAN_POINT('Ctrl Pts',(-22.4525800025406,14.4911112211554,
130.950148872058)) ;
#153903 = CARTESIAN_POINT('Ctrl Pts',(-22.4583236353459,14.4839705162681,
130.96692756896)) ;
#153904 = CARTESIAN_POINT('Ctrl Pts',(-22.4640054819444,14.4763839522856,
130.983525767063)) ;
#153905 = CARTESIAN_POINT('Ctrl Pts',(-22.4696170489507,14.4683610330769,
130.999918630428)) ;
#153906 = CARTESIAN_POINT('Ctrl Pts',(-22.4947273752802,14.4324605227176,
131.073272498985)) ;
#153907 = CARTESIAN_POINT('Ctrl Pts',(-22.5184294421355,14.3878194900791,
131.14251292154)) ;
#153908 = CARTESIAN_POINT('Ctrl Pts',(-22.54019892772,14.3354941538346,131.206106994967)) ;
#153909 = CARTESIAN_POINT('Ctrl Pts',(-22.5446195882161,14.324868613512,131.219020842062)) ;
#153910 = CARTESIAN_POINT('Ctrl Pts',(-22.5489605756069,14.3139263466219,
131.231701943349)) ;
#153911 = CARTESIAN_POINT('Ctrl Pts',(-22.5532175237182,14.3026764237554,
131.244137608586)) ;
#153912 = CARTESIAN_POINT('Ctrl Pts',(-22.5727750268273,14.2509914147576,
131.301270219829)) ;
#153913 = CARTESIAN_POINT('Ctrl Pts',(-22.5905566144932,14.1928134151902,
131.353216627627)) ;
#153914 = CARTESIAN_POINT('Ctrl Pts',(-22.6061216929628,14.1296950731466,
131.398685264081)) ;
#153915 = CARTESIAN_POINT('Ctrl Pts',(-22.6106418870564,14.1113651201394,
131.411889634515)) ;
#153916 = CARTESIAN_POINT('Ctrl Pts',(-22.6149751810526,14.0926186905486,
131.424547971201)) ;
#153917 = CARTESIAN_POINT('Ctrl Pts',(-22.6191108667609,14.0734942173741,
131.43662939706)) ;
#153918 = CARTESIAN_POINT('Ctrl Pts',(-22.6323692360561,14.0121841116725,
131.475360581426)) ;
#153919 = CARTESIAN_POINT('Ctrl Pts',(-22.6435936004016,13.9469968841546,
131.508155446611)) ;
#153920 = CARTESIAN_POINT('Ctrl Pts',(-22.652601471037,13.8791719111477,131.534467013303)) ;
#153921 = CARTESIAN_POINT('Ctrl Pts',(-22.6560966798024,13.8528546548554,
131.544676353806)) ;
#153922 = CARTESIAN_POINT('Ctrl Pts',(-22.659258086565,13.8261405468826,131.553909986958)) ;
#153923 = CARTESIAN_POINT('Ctrl Pts',(-22.66207462569,13.799103138409,131.562137838641)) ;
#153924 = CARTESIAN_POINT('Ctrl Pts',(-22.6646263132483,13.774608176419,131.569591989228)) ;
#153925 = CARTESIAN_POINT('Ctrl Pts',(-22.666928934256,13.7495103406014,131.576318680967)) ;
#153926 = CARTESIAN_POINT('Ctrl Pts',(-22.6689450781796,13.7240463055939,
131.582208381066)) ;
#153927 = CARTESIAN_POINT('Ctrl Pts',(-22.6709623724016,13.6985677422402,
131.588101441496)) ;
#153928 = CARTESIAN_POINT('Ctrl Pts',(-22.6726927838211,13.6727232379278,
131.593156345059)) ;
#153929 = CARTESIAN_POINT('Ctrl Pts',(-22.6741146695638,13.646767549545,131.597309957245)) ;
#153930 = CARTESIAN_POINT('Ctrl Pts',(-22.6755372042712,13.6208000146915,
131.601465465186)) ;
#153931 = CARTESIAN_POINT('Ctrl Pts',(-22.6766508920783,13.5947219208586,
131.604718769158)) ;
#153932 = CARTESIAN_POINT('Ctrl Pts',(-22.6774507939397,13.5687954659975,
131.607055523305)) ;
#153933 = CARTESIAN_POINT('Ctrl Pts',(-22.6781594759397,13.5458256333621,
131.609125796775)) ;
#153934 = CARTESIAN_POINT('Ctrl Pts',(-22.6786221002216,13.5229752443451,
131.610477364612)) ;
#153935 = CARTESIAN_POINT('Ctrl Pts',(-22.6788463775648,13.5004244329661,
131.611132537728)) ;
#153936 = CARTESIAN_POINT('Ctrl Pts',(-22.6790376668692,13.4811905283751,
131.611691344105)) ;
#153937 = CARTESIAN_POINT('Ctrl Pts',(-22.679062679477,13.4613698797398,131.611765143739)) ;
#153938 = CARTESIAN_POINT('Ctrl Pts',(-22.6788952846805,13.4412408608155,
131.611276429829)) ;
#153939 = CARTESIAN_POINT('Ctrl Pts',(-22.6787281656732,13.4211450051914,
131.610788521094)) ;
#153940 = CARTESIAN_POINT('Ctrl Pts',(-22.6783691766662,13.4007422200768,
131.609739715094)) ;
#153941 = CARTESIAN_POINT('Ctrl Pts',(-22.6778091707993,13.3803126577526,
131.608103354377)) ;
#153942 = CARTESIAN_POINT('Ctrl Pts',(-22.677257716648,13.3601950703848,131.606491982133)) ;
#153943 = CARTESIAN_POINT('Ctrl Pts',(-22.6765113567921,13.3400519549882,
131.604310971553)) ;
#153944 = CARTESIAN_POINT('Ctrl Pts',(-22.6755782124765,13.3201474123105,
131.601584558884)) ;
#153945 = CARTESIAN_POINT('Ctrl Pts',(-22.6746233619552,13.2997798629072,
131.598794726149)) ;
#153946 = CARTESIAN_POINT('Ctrl Pts',(-22.6734729150999,13.2796626021655,
131.5954338265)) ;
#153947 = CARTESIAN_POINT('Ctrl Pts',(-22.6721535433962,13.2600678710267,
131.591579895431)) ;
#153948 = CARTESIAN_POINT('Ctrl Pts',(-22.6708341716925,13.2404731398879,
131.587725964362)) ;
#153949 = CARTESIAN_POINT('Ctrl Pts',(-22.6693459978666,13.2214012994026,
131.583379429525)) ;
#153950 = CARTESIAN_POINT('Ctrl Pts',(-22.6677325901906,13.2031075416911,
131.578666241292)) ;
#153951 = CARTESIAN_POINT('Ctrl Pts',(-22.6665744709625,13.1899761100796,
131.57528307038)) ;
#153952 = CARTESIAN_POINT('Ctrl Pts',(-22.6652834410313,13.1764783865927,
131.571511826004)) ;
#153953 = CARTESIAN_POINT('Ctrl Pts',(-22.6638758082619,13.1629676618293,
131.567399713087)) ;
#153954 = CARTESIAN_POINT('Ctrl Pts',(-22.6624577740388,13.1493571019527,
131.563257214438)) ;
#153955 = CARTESIAN_POINT('Ctrl Pts',(-22.6609213606832,13.1357338594017,
131.558768747133)) ;
#153956 = CARTESIAN_POINT('Ctrl Pts',(-22.659299870578,13.1224444824643,131.554031896726)) ;
#153957 = CARTESIAN_POINT('Ctrl Pts',(-22.6576783804728,13.109155105527,131.54929504632)) ;
#153958 = CARTESIAN_POINT('Ctrl Pts',(-22.655971922004,13.096199960817,131.544310235839)) ;
#153959 = CARTESIAN_POINT('Ctrl Pts',(-22.6542298620055,13.0839043074199,
131.539221220329)) ;
#153960 = CARTESIAN_POINT('Ctrl Pts',(-22.6529520299329,13.0748852264018,
131.535488336708)) ;
#153961 = CARTESIAN_POINT('Ctrl Pts',(-22.6515626734834,13.0655735645419,
131.531429739391)) ;
#153962 = CARTESIAN_POINT('Ctrl Pts',(-22.6501095358714,13.0564196733478,
131.52718467415)) ;
#153963 = CARTESIAN_POINT('Ctrl Pts',(-22.6486476168762,13.0472104647311,
131.522913955767)) ;
#153964 = CARTESIAN_POINT('Ctrl Pts',(-22.6471211407257,13.0381613456492,
131.518454725706)) ;
#153965 = CARTESIAN_POINT('Ctrl Pts',(-22.6455941107226,13.0297062023841,
131.513993911399)) ;
#153966 = CARTESIAN_POINT('Ctrl Pts',(-22.6454270609541,13.0287812502074,
131.51350591968)) ;
#153967 = CARTESIAN_POINT('Ctrl Pts',(-22.6452600191918,13.0278633792219,
131.513017949926)) ;
#153968 = CARTESIAN_POINT('Ctrl Pts',(-22.645093079739,13.0269531373025,131.51253027587)) ;
#153969 = CARTESIAN_POINT('Ctrl Pts',(-22.6439417998698,13.0206757524139,
131.509167084525)) ;
#153970 = CARTESIAN_POINT('Ctrl Pts',(-22.6426928969163,13.0142106156177,
131.505518699242)) ;
#153971 = CARTESIAN_POINT('Ctrl Pts',(-22.6414278770865,13.008138163139,131.501823231953)) ;
#153972 = CARTESIAN_POINT('Ctrl Pts',(-22.6408214929086,13.0052273478162,
131.500051818699)) ;
#153973 = CARTESIAN_POINT('Ctrl Pts',(-22.6402116170566,13.0024063418278,
131.498270239291)) ;
#153974 = CARTESIAN_POINT('Ctrl Pts',(-22.6396083673344,12.9997366350286,
131.496507988166)) ;
#153975 = CARTESIAN_POINT('Ctrl Pts',(-22.6385793197154,12.9951825418823,
131.493501869377)) ;
#153976 = CARTESIAN_POINT('Ctrl Pts',(-22.6374677582898,12.9906247701674,
131.490254706053)) ;
#153977 = CARTESIAN_POINT('Ctrl Pts',(-22.6364008830054,12.9868577736952,
131.487138082702)) ;
#153978 = CARTESIAN_POINT('Ctrl Pts',(-22.635773853454,12.984643814723,131.485306364441)) ;
#153979 = CARTESIAN_POINT('Ctrl Pts',(-22.6351266524276,12.9825760105869,
131.483415720087)) ;
#153980 = CARTESIAN_POINT('Ctrl Pts',(-22.6345107978493,12.9809630503241,
131.481616646861)) ;
#153981 = CARTESIAN_POINT('Ctrl Pts',(-22.6335563000255,12.9784631629888,
131.478828307635)) ;
#153982 = CARTESIAN_POINT('Ctrl Pts',(-22.6326519325366,12.9769886520828,
131.47618641221)) ;
#153983 = CARTESIAN_POINT('Ctrl Pts',(-22.6320187065114,12.9778651918053,
131.474336592418)) ;
#153984 = CARTESIAN_POINT('Ctrl Pts',(-22.3151378869398,14.4232238463042,
130.548644361976)) ;
#153985 = CARTESIAN_POINT('Ctrl Pts',(-22.2811439325193,14.4234782772113,
130.449339078899)) ;
#153986 = CARTESIAN_POINT('Ctrl Pts',(-22.2474191728421,14.4076338778521,
130.350820184447)) ;
#153987 = CARTESIAN_POINT('Ctrl Pts',(-22.1822291641438,14.3443721936545,
130.160383020607)) ;
#153988 = CARTESIAN_POINT('Ctrl Pts',(-22.1511321866922,14.2967160993894,
130.069540569355)) ;
#153989 = CARTESIAN_POINT('Ctrl Pts',(-22.0867514375386,14.1569964530343,
129.881467465523)) ;
#153990 = CARTESIAN_POINT('Ctrl Pts',(-22.0558391935788,14.0563340831254,
129.79116466935)) ;
#153991 = CARTESIAN_POINT('Ctrl Pts',(-22.0081129613856,13.8232128942773,
129.651743790581)) ;
#153992 = CARTESIAN_POINT('Ctrl Pts',(-21.9920420955645,13.6947112909488,
129.604796564568)) ;
#153993 = CARTESIAN_POINT('Ctrl Pts',(-21.9745761371278,13.4112788385579,
129.553773905501)) ;
#153994 = CARTESIAN_POINT('Ctrl Pts',(-21.9770346938545,13.2936995343157,
129.560955995889)) ;
#153995 = CARTESIAN_POINT('Ctrl Pts',(-21.9761622047819,13.2297469423984,
129.558407225797)) ;
#153996 = CARTESIAN_POINT('Ctrl Pts',(-21.9759501313551,13.2215607234671,
129.55778770353)) ;
#153997 = CARTESIAN_POINT('Ctrl Pts',(-21.9753726991377,13.2141115604543,
129.556100872128)) ;
#153998 = CARTESIAN_POINT('Ctrl Pts',(-21.9751899121014,13.2123135011625,
129.555566903112)) ;
#153999 = CARTESIAN_POINT('Ctrl Pts',(-21.9748392577633,13.2102931177125,
129.55454254955)) ;
#154000 = CARTESIAN_POINT('Ctrl Pts',(-21.9747072455502,13.2096748296432,
129.554156907149)) ;
#154001 = CARTESIAN_POINT('Ctrl Pts',(-21.9744488989635,13.2088894196123,
129.553402208811)) ;
#154002 = CARTESIAN_POINT('Ctrl Pts',(-21.9743389556033,13.2086342290074,
129.553081035335)) ;
#154003 = CARTESIAN_POINT('Ctrl Pts',(-21.9741045372372,13.2082979781231,
129.552396237623)) ;
#154004 = CARTESIAN_POINT('Ctrl Pts',(-21.9739885035561,13.2082090859891,
129.552057272717)) ;
#154005 = CARTESIAN_POINT('Ctrl Pts',(-21.973721487045,13.2081743377998,129.551277247249)) ;
#154006 = CARTESIAN_POINT('Ctrl Pts',(-21.9735786216205,13.2082608228111,
129.550859899763)) ;
#154007 = CARTESIAN_POINT('Ctrl Pts',(-21.9732155601285,13.2086648958773,
129.54979930164)) ;
#154008 = CARTESIAN_POINT('Ctrl Pts',(-21.9730009907799,13.2091027938618,
129.549172488204)) ;
#154009 = CARTESIAN_POINT('Ctrl Pts',(-21.972108851907,13.2113394407767,129.546566315876)) ;
#154010 = CARTESIAN_POINT('Ctrl Pts',(-21.9714067112402,13.2145328967391,
129.544515178214)) ;
#154011 = CARTESIAN_POINT('Ctrl Pts',(-21.9683523963269,13.2306316253467,
129.535592720905)) ;
#154012 = CARTESIAN_POINT('Ctrl Pts',(-21.9651612110957,13.2574016528,129.526270429292)) ;
#154013 = CARTESIAN_POINT('Ctrl Pts',(-21.9565989464617,13.3672753503857,
129.501257801966)) ;
#154014 = CARTESIAN_POINT('Ctrl Pts',(-21.9516425801557,13.489837765544,129.486778952301)) ;
#154015 = CARTESIAN_POINT('Ctrl Pts',(-21.9656761119371,13.7782522629322,
129.527774590198)) ;
#154016 = CARTESIAN_POINT('Ctrl Pts',(-21.9813770244683,13.911436662301,129.57364108585)) ;
#154017 = CARTESIAN_POINT('Ctrl Pts',(-22.0290989771478,14.1573235247066,
129.713049463034)) ;
#154018 = CARTESIAN_POINT('Ctrl Pts',(-22.0613649266162,14.2666151380173,
129.807306789113)) ;
#154019 = CARTESIAN_POINT('Ctrl Pts',(-22.1305065476335,14.4241005029476,
130.009287652021)) ;
#154020 = CARTESIAN_POINT('Ctrl Pts',(-22.1651065040721,14.4793817119498,
130.110363226373)) ;
#154021 = CARTESIAN_POINT('Ctrl Pts',(-22.2385031763588,14.5537967295509,
130.324774213343)) ;
#154022 = CARTESIAN_POINT('Ctrl Pts',(-22.2766625743414,14.5727057162824,
130.436247852826)) ;
#154023 = CARTESIAN_POINT('Ctrl Pts',(-22.315137886939,14.5729486706397,130.548644361973)) ;
#154024 = CARTESIAN_POINT('Ctrl Pts',(-22.6320187065115,12.9778651918055,
131.474336592418)) ;
#154025 = CARTESIAN_POINT('Ctrl Pts',(-22.6319017381682,12.9780271046061,
131.473994897119)) ;
#154026 = CARTESIAN_POINT('Ctrl Pts',(-22.6318028115373,12.9782537499186,
131.473705906407)) ;
#154027 = CARTESIAN_POINT('Ctrl Pts',(-22.631613822165,12.9788663176294,131.473153818736)) ;
#154028 = CARTESIAN_POINT('Ctrl Pts',(-22.6315335379757,12.9792529318746,
131.4729192875)) ;
#154029 = CARTESIAN_POINT('Ctrl Pts',(-22.6313068850366,12.9806654239861,
131.472257174643)) ;
#154030 = CARTESIAN_POINT('Ctrl Pts',(-22.6312165058438,12.9819390751954,
131.471993153247)) ;
#154031 = CARTESIAN_POINT('Ctrl Pts',(-22.6310413042841,12.9863682734726,
131.471481343404)) ;
#154032 = CARTESIAN_POINT('Ctrl Pts',(-22.6311111509824,12.990696770219,131.471685383983)) ;
#154033 = CARTESIAN_POINT('Ctrl Pts',(-22.6317823753756,13.0076193276447,
131.473646207003)) ;
#154034 = CARTESIAN_POINT('Ctrl Pts',(-22.632964539542,13.0243616968384,131.477099619508)) ;
#154035 = CARTESIAN_POINT('Ctrl Pts',(-22.6380372471069,13.0936611830537,
131.491918332697)) ;
#154036 = CARTESIAN_POINT('Ctrl Pts',(-22.6433073952143,13.1624395523347,
131.507313821644)) ;
#154037 = CARTESIAN_POINT('Ctrl Pts',(-22.6510369822631,13.3897587207643,
131.529893978705)) ;
#154038 = CARTESIAN_POINT('Ctrl Pts',(-22.6470299561775,13.5079529376015,
131.518188401448)) ;
#154039 = CARTESIAN_POINT('Ctrl Pts',(-22.6312468100604,13.7299217778491,
131.472081679835)) ;
#154040 = CARTESIAN_POINT('Ctrl Pts',(-22.6154442941006,13.847789885417,131.425918373818)) ;
#154041 = CARTESIAN_POINT('Ctrl Pts',(-22.568941208862,14.0688613754809,131.290070629056)) ;
#154042 = CARTESIAN_POINT('Ctrl Pts',(-22.5376677274684,14.1680229125909,
131.198712563319)) ;
#154043 = CARTESIAN_POINT('Ctrl Pts',(-22.4733491505273,14.3035692712769,
131.010821080874)) ;
#154044 = CARTESIAN_POINT('Ctrl Pts',(-22.4429615479491,14.3485547863788,
130.922050900127)) ;
#154045 = CARTESIAN_POINT('Ctrl Pts',(-22.3797662254967,14.4080651754862,
130.737440739519)) ;
#154046 = CARTESIAN_POINT('Ctrl Pts',(-22.3476163144776,14.4229807584986,
130.643522392363)) ;
#154047 = CARTESIAN_POINT('Ctrl Pts',(-22.3151378869399,14.4232238463042,
130.548644361976)) ;
#154048 = CARTESIAN_POINT('Ctrl Pts',(-33.3489959095147,13.1551399285885,
127.871927411069)) ;
#154049 = CARTESIAN_POINT('Ctrl Pts',(-33.3254395351173,13.1734341962953,
127.803113044878)) ;
#154050 = CARTESIAN_POINT('Ctrl Pts',(-33.254172394553,13.1734341962953,127.827509047315)) ;
#154051 = CARTESIAN_POINT('Ctrl Pts',(-33.1829052539887,13.1734341962953,
127.851905049753)) ;
#154052 = CARTESIAN_POINT('Ctrl Pts',(-33.2064616283861,13.1551399285885,
127.920719415945)) ;
#154053 = CARTESIAN_POINT('Ctrl Pts',(-33.2300180027834,13.1368456608817,
127.989533782136)) ;
#154054 = CARTESIAN_POINT('Ctrl Pts',(-33.3012851433477,13.1368456608817,
127.965137779698)) ;
#154055 = CARTESIAN_POINT('Ctrl Pts',(-33.372552283912,13.1368456608817,127.94074177726)) ;
#154056 = CARTESIAN_POINT('Ctrl Pts',(-33.3489959095147,13.1551399285885,
127.871927411069)) ;
#154057 = CARTESIAN_POINT('Ctrl Pts',(-33.3504264730207,13.191264605624,127.881753249117)) ;
#154058 = CARTESIAN_POINT('Ctrl Pts',(-33.3264562033862,13.1991216594078,
127.810292753008)) ;
#154059 = CARTESIAN_POINT('Ctrl Pts',(-33.2553374556519,13.2028260557706,
127.835126718908)) ;
#154060 = CARTESIAN_POINT('Ctrl Pts',(-33.1842187079176,13.2065304521335,
127.859960684809)) ;
#154061 = CARTESIAN_POINT('Ctrl Pts',(-33.2081889775521,13.1986733983497,
127.931421180918)) ;
#154062 = CARTESIAN_POINT('Ctrl Pts',(-33.2321592471865,13.1908163445659,
128.002881677027)) ;
#154063 = CARTESIAN_POINT('Ctrl Pts',(-33.3032779949208,13.1871119482031,
127.978047711127)) ;
#154064 = CARTESIAN_POINT('Ctrl Pts',(-33.3743967426551,13.1834075518402,
127.953213745226)) ;
#154065 = CARTESIAN_POINT('Ctrl Pts',(-33.3504264730207,13.191264605624,127.881753249117)) ;
#154066 = CARTESIAN_POINT('Ctrl Pts',(-33.3535207816705,13.268036520819,127.884470294454)) ;
#154067 = CARTESIAN_POINT('Ctrl Pts',(-33.3286589899815,13.2538025217343,
127.812609970312)) ;
#154068 = CARTESIAN_POINT('Ctrl Pts',(-33.2578501843241,13.2651134066728,
127.836584356188)) ;
#154069 = CARTESIAN_POINT('Ctrl Pts',(-33.1870413786667,13.2764242916113,
127.860558742064)) ;
#154070 = CARTESIAN_POINT('Ctrl Pts',(-33.2119031703558,13.290658290696,127.932419066205)) ;
#154071 = CARTESIAN_POINT('Ctrl Pts',(-33.2367649620448,13.3048922897807,
128.004279390347)) ;
#154072 = CARTESIAN_POINT('Ctrl Pts',(-33.3075737677022,13.2935814048422,
127.980305004471)) ;
#154073 = CARTESIAN_POINT('Ctrl Pts',(-33.3783825733595,13.2822705199037,
127.956330618595)) ;
#154074 = CARTESIAN_POINT('Ctrl Pts',(-33.3535207816705,13.268036520819,127.884470294454)) ;
#154075 = CARTESIAN_POINT('Ctrl Pts',(-33.3579140346178,13.3732912215196,
127.837501420712)) ;
#154076 = CARTESIAN_POINT('Ctrl Pts',(-33.3317967099876,13.3290215614615,
127.779671185695)) ;
#154077 = CARTESIAN_POINT('Ctrl Pts',(-33.2613977067381,13.3500184403787,
127.797470635037)) ;
#154078 = CARTESIAN_POINT('Ctrl Pts',(-33.1909987034886,13.371015319296,127.815270084379)) ;
#154079 = CARTESIAN_POINT('Ctrl Pts',(-33.2171160281188,13.4152849793541,
127.873100319396)) ;
#154080 = CARTESIAN_POINT('Ctrl Pts',(-33.243233352749,13.4595546394122,127.930930554413)) ;
#154081 = CARTESIAN_POINT('Ctrl Pts',(-33.3136323559985,13.4385577604949,
127.913131105071)) ;
#154082 = CARTESIAN_POINT('Ctrl Pts',(-33.3840313592479,13.4175608815777,
127.895331655729)) ;
#154083 = CARTESIAN_POINT('Ctrl Pts',(-33.3579140346178,13.3732912215196,
127.837501420712)) ;
#154084 = CARTESIAN_POINT('Ctrl Pts',(-33.3611609335145,13.4471111688333,
127.748905537657)) ;
#154085 = CARTESIAN_POINT('Ctrl Pts',(-33.3341265408441,13.3820520008154,
127.716920013205)) ;
#154086 = CARTESIAN_POINT('Ctrl Pts',(-33.2639983405158,13.409026910249,127.724903336633)) ;
#154087 = CARTESIAN_POINT('Ctrl Pts',(-33.1938701401876,13.4360018196825,
127.732886660062)) ;
#154088 = CARTESIAN_POINT('Ctrl Pts',(-33.220904532858,13.5010609877004,127.764872184514)) ;
#154089 = CARTESIAN_POINT('Ctrl Pts',(-33.2479389255284,13.5661201557183,
127.796857708966)) ;
#154090 = CARTESIAN_POINT('Ctrl Pts',(-33.3180671258566,13.5391452462847,
127.788874385537)) ;
#154091 = CARTESIAN_POINT('Ctrl Pts',(-33.3881953261848,13.5121703368512,
127.780891062108)) ;
#154092 = CARTESIAN_POINT('Ctrl Pts',(-33.3611609335145,13.4471111688333,
127.748905537657)) ;
#154093 = CARTESIAN_POINT('Ctrl Pts',(-33.3621234180406,13.4654248347116,
127.67420492204)) ;
#154094 = CARTESIAN_POINT('Ctrl Pts',(-33.3348269327376,13.3954694274565,
127.663792350738)) ;
#154095 = CARTESIAN_POINT('Ctrl Pts',(-33.2647501798453,13.4231551632892,
127.664144174588)) ;
#154096 = CARTESIAN_POINT('Ctrl Pts',(-33.1946734269531,13.4508408991218,
127.664495998438)) ;
#154097 = CARTESIAN_POINT('Ctrl Pts',(-33.2219699122561,13.5207963063769,
127.67490856974)) ;
#154098 = CARTESIAN_POINT('Ctrl Pts',(-33.2492663975591,13.5907517136319,
127.685321141042)) ;
#154099 = CARTESIAN_POINT('Ctrl Pts',(-33.3193431504514,13.5630659777992,
127.684969317192)) ;
#154100 = CARTESIAN_POINT('Ctrl Pts',(-33.3894199033436,13.5353802419666,
127.684617493342)) ;
#154101 = CARTESIAN_POINT('Ctrl Pts',(-33.3621234180406,13.4654248347116,
127.67420492204)) ;
#154102 = CARTESIAN_POINT('Ctrl Pts',(-33.3622513221686,13.4658285122696,
127.63672629787)) ;
#154103 = CARTESIAN_POINT('Ctrl Pts',(-33.3349255565294,13.3959427988304,
127.637093604187)) ;
#154104 = CARTESIAN_POINT('Ctrl Pts',(-33.2648392434469,13.4231193515827,
127.633745568972)) ;
#154105 = CARTESIAN_POINT('Ctrl Pts',(-33.1947529303645,13.4502959043349,
127.630397533756)) ;
#154106 = CARTESIAN_POINT('Ctrl Pts',(-33.2220786960038,13.5201816177741,
127.63003022744)) ;
#154107 = CARTESIAN_POINT('Ctrl Pts',(-33.2494044616431,13.5900673312133,
127.629662921123)) ;
#154108 = CARTESIAN_POINT('Ctrl Pts',(-33.3194907747255,13.562890778461,127.633010956338)) ;
#154109 = CARTESIAN_POINT('Ctrl Pts',(-33.3895770878079,13.5357142257088,
127.636358991554)) ;
#154110 = CARTESIAN_POINT('Ctrl Pts',(-33.3622513221686,13.4658285122696,
127.63672629787)) ;
#154111 = CARTESIAN_POINT('',(-33.3622513221686,13.4658285122696,127.63672629787)) ;
#154112 = CARTESIAN_POINT('Ctrl Pts',(-33.3489959095147,13.1551399285885,
127.871927411069)) ;
#154113 = CARTESIAN_POINT('Ctrl Pts',(-33.3504264730207,13.191264605624,127.881753249117)) ;
#154114 = CARTESIAN_POINT('Ctrl Pts',(-33.3535207816705,13.268036520819,127.884470294454)) ;
#154115 = CARTESIAN_POINT('Ctrl Pts',(-33.3579140346178,13.3732912215196,
127.837501420712)) ;
#154116 = CARTESIAN_POINT('Ctrl Pts',(-33.3611609335145,13.4471111688333,
127.748905537657)) ;
#154117 = CARTESIAN_POINT('Ctrl Pts',(-33.3621234180406,13.4654248347116,
127.67420492204)) ;
#154118 = CARTESIAN_POINT('Ctrl Pts',(-33.3622513221686,13.4658285122696,
127.63672629787)) ;
#154119 = CARTESIAN_POINT('Origin',(-33.2921650090862,13.4930050650219,127.633378262655)) ;
#154120 = CARTESIAN_POINT('Ctrl Pts',(-33.3622513221686,13.4658285122696,
127.63672629787)) ;
#154121 = CARTESIAN_POINT('Ctrl Pts',(-33.3349255565294,13.3959427988304,
127.637093604187)) ;
#154122 = CARTESIAN_POINT('Ctrl Pts',(-33.2648392434469,13.4231193515827,
127.633745568972)) ;
#154123 = CARTESIAN_POINT('Ctrl Pts',(-33.1947529303645,13.4502959043349,
127.630397533756)) ;
#154124 = CARTESIAN_POINT('Ctrl Pts',(-33.2220786960038,13.5201816177741,
127.63003022744)) ;
#154125 = CARTESIAN_POINT('Ctrl Pts',(-33.2494044616431,13.5900673312133,
127.629662921123)) ;
#154126 = CARTESIAN_POINT('Ctrl Pts',(-33.3194907747255,13.562890778461,127.633010956338)) ;
#154127 = CARTESIAN_POINT('Ctrl Pts',(-33.3895770878079,13.5357142257088,
127.636358991554)) ;
#154128 = CARTESIAN_POINT('Ctrl Pts',(-33.3622513221686,13.4658285122696,
127.63672629787)) ;
#154129 = CARTESIAN_POINT('Ctrl Pts',(-33.3634081045458,13.4658294080177,
127.254746417056)) ;
#154130 = CARTESIAN_POINT('Ctrl Pts',(-33.3360823389065,13.3959436945786,
127.255113723373)) ;
#154131 = CARTESIAN_POINT('Ctrl Pts',(-33.2659960258241,13.4231202473308,
127.251765688157)) ;
#154132 = CARTESIAN_POINT('Ctrl Pts',(-33.1959097127417,13.4502968000831,
127.248417652942)) ;
#154133 = CARTESIAN_POINT('Ctrl Pts',(-33.2232354783809,13.5201825135223,
127.248050346625)) ;
#154134 = CARTESIAN_POINT('Ctrl Pts',(-33.2505612440202,13.5900682269615,
127.247683040309)) ;
#154135 = CARTESIAN_POINT('Ctrl Pts',(-33.3206475571026,13.5628916742092,
127.251031075524)) ;
#154136 = CARTESIAN_POINT('Ctrl Pts',(-33.3907338701851,13.5357151214569,
127.25437911074)) ;
#154137 = CARTESIAN_POINT('Ctrl Pts',(-33.3634081045458,13.4658294080177,
127.254746417056)) ;
#154138 = CARTESIAN_POINT('Ctrl Pts',(-33.364564886923,13.4658303037659,126.872766536242)) ;
#154139 = CARTESIAN_POINT('Ctrl Pts',(-33.3372391212837,13.3959445903267,
126.873133842559)) ;
#154140 = CARTESIAN_POINT('Ctrl Pts',(-33.2671528082013,13.423121143079,126.869785807343)) ;
#154141 = CARTESIAN_POINT('Ctrl Pts',(-33.1970664951188,13.4502976958313,
126.866437772128)) ;
#154142 = CARTESIAN_POINT('Ctrl Pts',(-33.2243922607581,13.5201834092705,
126.866070465811)) ;
#154143 = CARTESIAN_POINT('Ctrl Pts',(-33.2517180263974,13.5900691227097,
126.865703159495)) ;
#154144 = CARTESIAN_POINT('Ctrl Pts',(-33.3218043394798,13.5628925699574,
126.86905119471)) ;
#154145 = CARTESIAN_POINT('Ctrl Pts',(-33.3918906525622,13.5357160172051,
126.872399229925)) ;
#154146 = CARTESIAN_POINT('Ctrl Pts',(-33.364564886923,13.4658303037659,126.872766536242)) ;
#154147 = CARTESIAN_POINT('Ctrl Pts',(-33.3657216693001,13.4658311995141,
126.490786655428)) ;
#154148 = CARTESIAN_POINT('Ctrl Pts',(-33.3383959036609,13.3959454860749,
126.491153961744)) ;
#154149 = CARTESIAN_POINT('Ctrl Pts',(-33.2683095905784,13.4231220388272,
126.487805926529)) ;
#154150 = CARTESIAN_POINT('Ctrl Pts',(-33.198223277496,13.4502985915795,126.484457891314)) ;
#154151 = CARTESIAN_POINT('Ctrl Pts',(-33.2255490431353,13.5201843050187,
126.484090584997)) ;
#154152 = CARTESIAN_POINT('Ctrl Pts',(-33.2528748087745,13.5900700184578,
126.48372327868)) ;
#154153 = CARTESIAN_POINT('Ctrl Pts',(-33.322961121857,13.5628934657056,126.487071313896)) ;
#154154 = CARTESIAN_POINT('Ctrl Pts',(-33.3930474349394,13.5357169129533,
126.490419349111)) ;
#154155 = CARTESIAN_POINT('Ctrl Pts',(-33.3657216693001,13.4658311995141,
126.490786655428)) ;
#154156 = CARTESIAN_POINT('',(-33.3657216693001,13.4658311995141,126.490786655428)) ;
#154157 = CARTESIAN_POINT('',(-33.3622513221686,13.4658285122696,127.63672629787)) ;
#154158 = CARTESIAN_POINT('',(-33.2955665703368,13.4180239009611,126.488994292619)) ;
#154159 = CARTESIAN_POINT('Origin',(-33.2956353562177,13.4930077522664,126.487438620212)) ;
#154160 = CARTESIAN_POINT('',(-33.2957040070394,13.5679916035759,126.485882942442)) ;
#154161 = CARTESIAN_POINT('Origin',(-33.2956353562177,13.4930077522664,126.487438620212)) ;
#154162 = CARTESIAN_POINT('Origin',(-33.2956353562177,13.4930077522664,126.487438620212)) ;
#154163 = CARTESIAN_POINT('Ctrl Pts',(-33.3657216693001,13.4658311995141,
126.490786655428)) ;
#154164 = CARTESIAN_POINT('Ctrl Pts',(-33.3383959036609,13.3959454860749,
126.491153961744)) ;
#154165 = CARTESIAN_POINT('Ctrl Pts',(-33.2683095905784,13.4231220388272,
126.487805926529)) ;
#154166 = CARTESIAN_POINT('Ctrl Pts',(-33.198223277496,13.4502985915795,126.484457891314)) ;
#154167 = CARTESIAN_POINT('Ctrl Pts',(-33.2255490431353,13.5201843050187,
126.484090584997)) ;
#154168 = CARTESIAN_POINT('Ctrl Pts',(-33.2528748087745,13.5900700184578,
126.48372327868)) ;
#154169 = CARTESIAN_POINT('Ctrl Pts',(-33.322961121857,13.5628934657056,126.487071313896)) ;
#154170 = CARTESIAN_POINT('Ctrl Pts',(-33.3930474349394,13.5357169129533,
126.490419349111)) ;
#154171 = CARTESIAN_POINT('Ctrl Pts',(-33.3657216693001,13.4658311995141,
126.490786655428)) ;
#154172 = CARTESIAN_POINT('Ctrl Pts',(-33.3710709437106,13.4658311995141,
126.425157509608)) ;
#154173 = CARTESIAN_POINT('Ctrl Pts',(-33.343714479123,13.3959454860749,126.422780862853)) ;
#154174 = CARTESIAN_POINT('Ctrl Pts',(-33.2739832165657,13.4231220388272,
126.412393722814)) ;
#154175 = CARTESIAN_POINT('Ctrl Pts',(-33.2042519540084,13.4502985915795,
126.402006582774)) ;
#154176 = CARTESIAN_POINT('Ctrl Pts',(-33.2316084185959,13.5201843050187,
126.404383229528)) ;
#154177 = CARTESIAN_POINT('Ctrl Pts',(-33.2589648831834,13.5900700184579,
126.406759876282)) ;
#154178 = CARTESIAN_POINT('Ctrl Pts',(-33.3286961457408,13.5628934657056,
126.417147016322)) ;
#154179 = CARTESIAN_POINT('Ctrl Pts',(-33.3984274082981,13.5357169129533,
126.427534156362)) ;
#154180 = CARTESIAN_POINT('Ctrl Pts',(-33.3710709437106,13.4658311995141,
126.425157509608)) ;
#154181 = CARTESIAN_POINT('Ctrl Pts',(-33.4026727151281,13.4658311995141,
126.292213744632)) ;
#154182 = CARTESIAN_POINT('Ctrl Pts',(-33.3761162339872,13.3959454860749,
126.284199283461)) ;
#154183 = CARTESIAN_POINT('Ctrl Pts',(-33.3093262459584,13.4231220388272,
126.259484856214)) ;
#154184 = CARTESIAN_POINT('Ctrl Pts',(-33.2425362579296,13.4502985915795,
126.234770428968)) ;
#154185 = CARTESIAN_POINT('Ctrl Pts',(-33.2690927390706,13.5201843050187,
126.242784890139)) ;
#154186 = CARTESIAN_POINT('Ctrl Pts',(-33.2956492202115,13.5900700184578,
126.250799351311)) ;
#154187 = CARTESIAN_POINT('Ctrl Pts',(-33.3624392082402,13.5628934657056,
126.275513778557)) ;
#154188 = CARTESIAN_POINT('Ctrl Pts',(-33.429229196269,13.5357169129533,126.300228205804)) ;
#154189 = CARTESIAN_POINT('Ctrl Pts',(-33.4026727151281,13.4658311995141,
126.292213744632)) ;
#154190 = CARTESIAN_POINT('Ctrl Pts',(-33.5097508222684,13.4658311995141,
126.114873926673)) ;
#154191 = CARTESIAN_POINT('Ctrl Pts',(-33.4869569930479,13.3959454860749,
126.099090565098)) ;
#154192 = CARTESIAN_POINT('Ctrl Pts',(-33.4310376162827,13.4231220388272,
126.055050770833)) ;
#154193 = CARTESIAN_POINT('Ctrl Pts',(-33.3751182395174,13.4502985915795,
126.011010976568)) ;
#154194 = CARTESIAN_POINT('Ctrl Pts',(-33.3979120687378,13.5201843050187,
126.026794338144)) ;
#154195 = CARTESIAN_POINT('Ctrl Pts',(-33.4207058979582,13.5900700184579,
126.042577699719)) ;
#154196 = CARTESIAN_POINT('Ctrl Pts',(-33.4766252747235,13.5628934657056,
126.086617493984)) ;
#154197 = CARTESIAN_POINT('Ctrl Pts',(-33.5325446514888,13.5357169129533,
126.130657288248)) ;
#154198 = CARTESIAN_POINT('Ctrl Pts',(-33.5097508222684,13.4658311995141,
126.114873926673)) ;
#154199 = CARTESIAN_POINT('Ctrl Pts',(-33.6669726245832,13.4658311995141,
125.979587612656)) ;
#154200 = CARTESIAN_POINT('Ctrl Pts',(-33.6501853294574,13.3959454860749,
125.957588672145)) ;
#154201 = CARTESIAN_POINT('Ctrl Pts',(-33.6106414771463,13.4231220388272,
125.898557790685)) ;
#154202 = CARTESIAN_POINT('Ctrl Pts',(-33.5710976248353,13.4502985915795,
125.839526909225)) ;
#154203 = CARTESIAN_POINT('Ctrl Pts',(-33.5878849199611,13.5201843050187,
125.861525849736)) ;
#154204 = CARTESIAN_POINT('Ctrl Pts',(-33.6046722150869,13.5900700184578,
125.883524790247)) ;
#154205 = CARTESIAN_POINT('Ctrl Pts',(-33.6442160673979,13.5628934657056,
125.942555671708)) ;
#154206 = CARTESIAN_POINT('Ctrl Pts',(-33.683759919709,13.5357169129533,126.001586553168)) ;
#154207 = CARTESIAN_POINT('Ctrl Pts',(-33.6669726245832,13.4658311995141,
125.979587612656)) ;
#154208 = CARTESIAN_POINT('Ctrl Pts',(-33.8546539670386,13.4658311995141,
125.899837483417)) ;
#154209 = CARTESIAN_POINT('Ctrl Pts',(-33.8453517619418,13.3959454860749,
125.873811092798)) ;
#154210 = CARTESIAN_POINT('Ctrl Pts',(-33.825626690385,13.4231220388272,125.805630627847)) ;
#154211 = CARTESIAN_POINT('Ctrl Pts',(-33.8059016188281,13.4502985915795,
125.737450162897)) ;
#154212 = CARTESIAN_POINT('Ctrl Pts',(-33.8152038239249,13.5201843050187,
125.763476553515)) ;
#154213 = CARTESIAN_POINT('Ctrl Pts',(-33.8245060290216,13.5900700184579,
125.789502944134)) ;
#154214 = CARTESIAN_POINT('Ctrl Pts',(-33.8442311005785,13.5628934657056,
125.857683409085)) ;
#154215 = CARTESIAN_POINT('Ctrl Pts',(-33.8639561721354,13.5357169129533,
125.925863874035)) ;
#154216 = CARTESIAN_POINT('Ctrl Pts',(-33.8546539670386,13.4658311995141,
125.899837483417)) ;
#154217 = CARTESIAN_POINT('Ctrl Pts',(-34.0574909713096,13.4658311995141,
125.879315368324)) ;
#154218 = CARTESIAN_POINT('Ctrl Pts',(-34.056531236216,13.3959454860749,125.851661404809)) ;
#154219 = CARTESIAN_POINT('Ctrl Pts',(-34.0584428323337,13.4231220388272,
125.780618176254)) ;
#154220 = CARTESIAN_POINT('Ctrl Pts',(-34.0603544284514,13.4502985915795,
125.709574947699)) ;
#154221 = CARTESIAN_POINT('Ctrl Pts',(-34.061314163545,13.5201843050187,125.737228911215)) ;
#154222 = CARTESIAN_POINT('Ctrl Pts',(-34.0622738986387,13.5900700184579,
125.76488287473)) ;
#154223 = CARTESIAN_POINT('Ctrl Pts',(-34.0603623025209,13.5628934657056,
125.835926103285)) ;
#154224 = CARTESIAN_POINT('Ctrl Pts',(-34.0584507064032,13.5357169129533,
125.90696933184)) ;
#154225 = CARTESIAN_POINT('Ctrl Pts',(-34.0574909713096,13.4658311995141,
125.879315368324)) ;
#154226 = CARTESIAN_POINT('Ctrl Pts',(-34.2603174788621,13.4658311995141,
125.922153820006)) ;
#154227 = CARTESIAN_POINT('Ctrl Pts',(-34.2679438333246,13.3959454860749,
125.895501671555)) ;
#154228 = CARTESIAN_POINT('Ctrl Pts',(-34.2917008109883,13.4231220388272,
125.828374514453)) ;
#154229 = CARTESIAN_POINT('Ctrl Pts',(-34.3154577886521,13.4502985915795,
125.76124735735)) ;
#154230 = CARTESIAN_POINT('Ctrl Pts',(-34.3078314341896,13.5201843050187,
125.787899505801)) ;
#154231 = CARTESIAN_POINT('Ctrl Pts',(-34.3002050797271,13.5900700184579,
125.814551654251)) ;
#154232 = CARTESIAN_POINT('Ctrl Pts',(-34.2764481020633,13.5628934657056,
125.881678811354)) ;
#154233 = CARTESIAN_POINT('Ctrl Pts',(-34.2526911243996,13.5357169129533,
125.948805968456)) ;
#154234 = CARTESIAN_POINT('Ctrl Pts',(-34.2603174788621,13.4658311995141,
125.922153820006)) ;
#154235 = CARTESIAN_POINT('Ctrl Pts',(-34.4394051996481,13.4658311995141,
126.026010217586)) ;
#154236 = CARTESIAN_POINT('Ctrl Pts',(-34.4548670732842,13.3959454860749,
126.002982829036)) ;
#154237 = CARTESIAN_POINT('Ctrl Pts',(-34.4981313355085,13.4231220388272,
125.946377991427)) ;
#154238 = CARTESIAN_POINT('Ctrl Pts',(-34.5413955977328,13.4502985915795,
125.889773153818)) ;
#154239 = CARTESIAN_POINT('Ctrl Pts',(-34.5259337240967,13.5201843050187,
125.912800542368)) ;
#154240 = CARTESIAN_POINT('Ctrl Pts',(-34.5104718504605,13.5900700184578,
125.935827930917)) ;
#154241 = CARTESIAN_POINT('Ctrl Pts',(-34.4672075882362,13.5628934657056,
125.992432768526)) ;
#154242 = CARTESIAN_POINT('Ctrl Pts',(-34.423943326012,13.5357169129533,126.049037606135)) ;
#154243 = CARTESIAN_POINT('Ctrl Pts',(-34.4394051996481,13.4658311995141,
126.026010217586)) ;
#154244 = CARTESIAN_POINT('Ctrl Pts',(-34.5756161826405,13.4658311995141,
126.176769282622)) ;
#154245 = CARTESIAN_POINT('Ctrl Pts',(-34.5973140532962,13.3959454860749,
126.159477051786)) ;
#154246 = CARTESIAN_POINT('Ctrl Pts',(-34.6556528941974,13.4231220388272,
126.118553567228)) ;
#154247 = CARTESIAN_POINT('Ctrl Pts',(-34.7139917350986,13.4502985915795,
126.07763008267)) ;
#154248 = CARTESIAN_POINT('Ctrl Pts',(-34.6922938644429,13.5201843050187,
126.094922313507)) ;
#154249 = CARTESIAN_POINT('Ctrl Pts',(-34.6705959937872,13.5900700184578,
126.112214544343)) ;
#154250 = CARTESIAN_POINT('Ctrl Pts',(-34.612257152886,13.5628934657056,126.153138028901)) ;
#154251 = CARTESIAN_POINT('Ctrl Pts',(-34.5539183119848,13.5357169129533,
126.194061513458)) ;
#154252 = CARTESIAN_POINT('Ctrl Pts',(-34.5756161826405,13.4658311995141,
126.176769282622)) ;
#154253 = CARTESIAN_POINT('Ctrl Pts',(-34.6605098387667,13.4658311995141,
126.361211761343)) ;
#154254 = CARTESIAN_POINT('Ctrl Pts',(-34.6864428238696,13.3959454860749,
126.351248800186)) ;
#154255 = CARTESIAN_POINT('Ctrl Pts',(-34.7544765704431,13.4231220388272,
126.329779166733)) ;
#154256 = CARTESIAN_POINT('Ctrl Pts',(-34.8225103170166,13.4502985915795,
126.308309533281)) ;
#154257 = CARTESIAN_POINT('Ctrl Pts',(-34.7965773319137,13.5201843050187,
126.318272494438)) ;
#154258 = CARTESIAN_POINT('Ctrl Pts',(-34.7706443468108,13.5900700184578,
126.328235455595)) ;
#154259 = CARTESIAN_POINT('Ctrl Pts',(-34.7026106002373,13.5628934657056,
126.349705089048)) ;
#154260 = CARTESIAN_POINT('Ctrl Pts',(-34.6345768536637,13.5357169129533,
126.3711747225)) ;
#154261 = CARTESIAN_POINT('Ctrl Pts',(-34.6605098387667,13.4658311995141,
126.361211761343)) ;
#154262 = CARTESIAN_POINT('Ctrl Pts',(-34.6852735030978,13.4658311995141,
126.56639932233)) ;
#154263 = CARTESIAN_POINT('Ctrl Pts',(-34.7130249936416,13.3959454860749,
126.564856538092)) ;
#154264 = CARTESIAN_POINT('Ctrl Pts',(-34.7843881220333,13.4231220388272,
126.56525799732)) ;
#154265 = CARTESIAN_POINT('Ctrl Pts',(-34.8557512504251,13.4502985915795,
126.565659456548)) ;
#154266 = CARTESIAN_POINT('Ctrl Pts',(-34.8279997598812,13.5201843050187,
126.567202240786)) ;
#154267 = CARTESIAN_POINT('Ctrl Pts',(-34.8002482693373,13.5900700184579,
126.568745025024)) ;
#154268 = CARTESIAN_POINT('Ctrl Pts',(-34.7288851409456,13.5628934657056,
126.568343565796)) ;
#154269 = CARTESIAN_POINT('Ctrl Pts',(-34.6575220125539,13.5357169129533,
126.567942106568)) ;
#154270 = CARTESIAN_POINT('Ctrl Pts',(-34.6852735030978,13.4658311995141,
126.56639932233)) ;
#154271 = CARTESIAN_POINT('Ctrl Pts',(-34.6444773076006,13.4658311995141,
126.769201249595)) ;
#154272 = CARTESIAN_POINT('Ctrl Pts',(-34.6713161577667,13.3959454860749,
126.776230438729)) ;
#154273 = CARTESIAN_POINT('Ctrl Pts',(-34.7389855153722,13.4231220388272,
126.79846338974)) ;
#154274 = CARTESIAN_POINT('Ctrl Pts',(-34.8066548729777,13.4502985915795,
126.820696340751)) ;
#154275 = CARTESIAN_POINT('Ctrl Pts',(-34.7798160228116,13.5201843050187,
126.813667151617)) ;
#154276 = CARTESIAN_POINT('Ctrl Pts',(-34.7529771726455,13.5900700184579,
126.806637962483)) ;
#154277 = CARTESIAN_POINT('Ctrl Pts',(-34.68530781504,13.5628934657056,126.784405011472)) ;
#154278 = CARTESIAN_POINT('Ctrl Pts',(-34.6176384574345,13.5357169129533,
126.762172060461)) ;
#154279 = CARTESIAN_POINT('Ctrl Pts',(-34.6444773076006,13.4658311995141,
126.769201249595)) ;
#154280 = CARTESIAN_POINT('Ctrl Pts',(-34.5453436411495,13.4658311995141,
126.946957684585)) ;
#154281 = CARTESIAN_POINT('Ctrl Pts',(-34.5687512865745,13.3959454860749,
126.961742671916)) ;
#154282 = CARTESIAN_POINT('Ctrl Pts',(-34.6264015098537,13.4231220388272,
127.003319432827)) ;
#154283 = CARTESIAN_POINT('Ctrl Pts',(-34.6840517331329,13.4502985915795,
127.044896193737)) ;
#154284 = CARTESIAN_POINT('Ctrl Pts',(-34.6606440877079,13.5201843050187,
127.030111206405)) ;
#154285 = CARTESIAN_POINT('Ctrl Pts',(-34.6372364422829,13.5900700184578,
127.015326219074)) ;
#154286 = CARTESIAN_POINT('Ctrl Pts',(-34.5795862190037,13.5628934657056,
126.973749458163)) ;
#154287 = CARTESIAN_POINT('Ctrl Pts',(-34.5219359957245,13.5357169129533,
126.932172697253)) ;
#154288 = CARTESIAN_POINT('Ctrl Pts',(-34.5453436411495,13.4658311995141,
126.946957684585)) ;
#154289 = CARTESIAN_POINT('Ctrl Pts',(-34.397695173349,13.4658311995141,127.087382113455)) ;
#154290 = CARTESIAN_POINT('Ctrl Pts',(-34.4155135478261,13.3959454860749,
127.108559279803)) ;
#154291 = CARTESIAN_POINT('Ctrl Pts',(-34.4578296604691,13.4231220388272,
127.16564535534)) ;
#154292 = CARTESIAN_POINT('Ctrl Pts',(-34.500145773112,13.4502985915795,127.222731430876)) ;
#154293 = CARTESIAN_POINT('Ctrl Pts',(-34.4823273986348,13.5201843050187,
127.201554264528)) ;
#154294 = CARTESIAN_POINT('Ctrl Pts',(-34.4645090241577,13.5900700184578,
127.18037709818)) ;
#154295 = CARTESIAN_POINT('Ctrl Pts',(-34.4221929115148,13.5628934657056,
127.123291022643)) ;
#154296 = CARTESIAN_POINT('Ctrl Pts',(-34.3798767988718,13.5357169129533,
127.066204947107)) ;
#154297 = CARTESIAN_POINT('Ctrl Pts',(-34.397695173349,13.4658311995141,127.087382113455)) ;
#154298 = CARTESIAN_POINT('Ctrl Pts',(-34.2109661436266,13.4658311995141,
127.177936318607)) ;
#154299 = CARTESIAN_POINT('Ctrl Pts',(-34.2213805824851,13.3959454860749,
127.203585641458)) ;
#154300 = CARTESIAN_POINT('Ctrl Pts',(-34.244015597737,13.4231220388272,127.270974071339)) ;
#154301 = CARTESIAN_POINT('Ctrl Pts',(-34.266650612989,13.4502985915795,127.338362501219)) ;
#154302 = CARTESIAN_POINT('Ctrl Pts',(-34.2562361741305,13.5201843050187,
127.312713178368)) ;
#154303 = CARTESIAN_POINT('Ctrl Pts',(-34.245821735272,13.5900700184579,127.287063855517)) ;
#154304 = CARTESIAN_POINT('Ctrl Pts',(-34.2231867200201,13.5628934657056,
127.219675425636)) ;
#154305 = CARTESIAN_POINT('Ctrl Pts',(-34.2005517047682,13.5357169129533,
127.152286995756)) ;
#154306 = CARTESIAN_POINT('Ctrl Pts',(-34.2109661436266,13.4658311995141,
127.177936318607)) ;
#154307 = CARTESIAN_POINT('Ctrl Pts',(-34.0053608811418,13.4658311995141,
127.205905827809)) ;
#154308 = CARTESIAN_POINT('Ctrl Pts',(-34.0073466019005,13.3959454860749,
127.233502366642)) ;
#154309 = CARTESIAN_POINT('Ctrl Pts',(-34.0080733954292,13.4231220388272,
127.304559444664)) ;
#154310 = CARTESIAN_POINT('Ctrl Pts',(-34.0088001889578,13.4502985915795,
127.375616522685)) ;
#154311 = CARTESIAN_POINT('Ctrl Pts',(-34.006814468199,13.5201843050187,127.348019983852)) ;
#154312 = CARTESIAN_POINT('Ctrl Pts',(-34.0048287474402,13.5900700184578,
127.320423445019)) ;
#154313 = CARTESIAN_POINT('Ctrl Pts',(-34.0041019539116,13.5628934657056,
127.249366366998)) ;
#154314 = CARTESIAN_POINT('Ctrl Pts',(-34.003375160383,13.5357169129533,127.178309288976)) ;
#154315 = CARTESIAN_POINT('Ctrl Pts',(-34.0053608811418,13.4658311995141,
127.205905827809)) ;
#154316 = CARTESIAN_POINT('Ctrl Pts',(-33.8704755222901,13.4658311995141,
127.182274454702)) ;
#154317 = CARTESIAN_POINT('Ctrl Pts',(-33.8667699608776,13.3959454860749,
127.209406331759)) ;
#154318 = CARTESIAN_POINT('Ctrl Pts',(-33.8529850451152,13.4231220388272,
127.278378794431)) ;
#154319 = CARTESIAN_POINT('Ctrl Pts',(-33.8392001293528,13.4502985915795,
127.347351257104)) ;
#154320 = CARTESIAN_POINT('Ctrl Pts',(-33.8429056907652,13.5201843050187,
127.320219380047)) ;
#154321 = CARTESIAN_POINT('Ctrl Pts',(-33.8466112521777,13.5900700184578,
127.29308750299)) ;
#154322 = CARTESIAN_POINT('Ctrl Pts',(-33.8603961679402,13.5628934657056,
127.224115040317)) ;
#154323 = CARTESIAN_POINT('Ctrl Pts',(-33.8741810837025,13.5357169129533,
127.155142577645)) ;
#154324 = CARTESIAN_POINT('Ctrl Pts',(-33.8704755222901,13.4658311995141,
127.182274454702)) ;
#154325 = CARTESIAN_POINT('Ctrl Pts',(-33.8079438763917,13.4658311995141,
127.161214257016)) ;
#154326 = CARTESIAN_POINT('Ctrl Pts',(-33.8015609648991,13.3959454860749,
127.187711385949)) ;
#154327 = CARTESIAN_POINT('Ctrl Pts',(-33.7810150851566,13.4231220388272,
127.254636339226)) ;
#154328 = CARTESIAN_POINT('Ctrl Pts',(-33.760469205414,13.4502985915795,127.321561292503)) ;
#154329 = CARTESIAN_POINT('Ctrl Pts',(-33.7668521169066,13.5201843050187,
127.295064163571)) ;
#154330 = CARTESIAN_POINT('Ctrl Pts',(-33.7732350283992,13.5900700184578,
127.268567034639)) ;
#154331 = CARTESIAN_POINT('Ctrl Pts',(-33.7937809081418,13.5628934657056,
127.201642081362)) ;
#154332 = CARTESIAN_POINT('Ctrl Pts',(-33.8143267878844,13.5357169129533,
127.134717128084)) ;
#154333 = CARTESIAN_POINT('Ctrl Pts',(-33.8079438763917,13.4658311995141,
127.161214257016)) ;
#154334 = CARTESIAN_POINT('Ctrl Pts',(-33.3657216693001,13.4658311995141,
126.490786655428)) ;
#154335 = CARTESIAN_POINT('Ctrl Pts',(-33.3710709437106,13.4658311995141,
126.425157509608)) ;
#154336 = CARTESIAN_POINT('Ctrl Pts',(-33.4026727151281,13.4658311995141,
126.292213744632)) ;
#154337 = CARTESIAN_POINT('Ctrl Pts',(-33.5097508222684,13.4658311995141,
126.114873926673)) ;
#154338 = CARTESIAN_POINT('Ctrl Pts',(-33.6669726245832,13.4658311995141,
125.979587612656)) ;
#154339 = CARTESIAN_POINT('Ctrl Pts',(-33.8546539670386,13.4658311995141,
125.899837483417)) ;
#154340 = CARTESIAN_POINT('Ctrl Pts',(-34.0574909713096,13.4658311995141,
125.879315368324)) ;
#154341 = CARTESIAN_POINT('Ctrl Pts',(-34.2603174788621,13.4658311995141,
125.922153820006)) ;
#154342 = CARTESIAN_POINT('Ctrl Pts',(-34.4394051996481,13.4658311995141,
126.026010217586)) ;
#154343 = CARTESIAN_POINT('Ctrl Pts',(-34.5756161826405,13.4658311995141,
126.176769282622)) ;
#154344 = CARTESIAN_POINT('Ctrl Pts',(-34.6605098387667,13.4658311995141,
126.361211761343)) ;
#154345 = CARTESIAN_POINT('Ctrl Pts',(-34.6852735030978,13.4658311995141,
126.56639932233)) ;
#154346 = CARTESIAN_POINT('Ctrl Pts',(-34.6444773076006,13.4658311995141,
126.769201249595)) ;
#154347 = CARTESIAN_POINT('Ctrl Pts',(-34.5453436411495,13.4658311995141,
126.946957684585)) ;
#154348 = CARTESIAN_POINT('Ctrl Pts',(-34.397695173349,13.4658311995141,127.087382113455)) ;
#154349 = CARTESIAN_POINT('Ctrl Pts',(-34.2109661436266,13.4658311995141,
127.177936318607)) ;
#154350 = CARTESIAN_POINT('Ctrl Pts',(-34.0053608811418,13.4658311995141,
127.205905827809)) ;
#154351 = CARTESIAN_POINT('Ctrl Pts',(-33.8704755222901,13.4658311995141,
127.182274454702)) ;
#154352 = CARTESIAN_POINT('Ctrl Pts',(-33.8079438763917,13.4658311995141,
127.161214257016)) ;
#154353 = CARTESIAN_POINT('Origin',(-21.2276309348583,13.4231221026609,127.371750482897)) ;
#154354 = CARTESIAN_POINT('Origin',(-23.4026448390223,13.4231221026609,133.725538241056)) ;
#154355 = CARTESIAN_POINT('Origin',(-29.5339383493105,-0.00455472950331615,
111.201234636506)) ;
#154356 = CARTESIAN_POINT('',(-30.095421224107,-0.00455472950331526,112.911420878209)) ;
#154357 = CARTESIAN_POINT('Origin',(-29.8146797867088,-0.00455472950331526,
112.056327757358)) ;
#154358 = CARTESIAN_POINT('',(-29.8146797867088,-0.00455472950331526,112.056327757358)) ;
#154359 = CARTESIAN_POINT('',(-30.0954212241071,-0.00455472950331526,112.911420878209)) ;
#154360 = CARTESIAN_POINT('Ctrl Pts',(-29.8146797867088,-14.2808450589491,
112.056327757358)) ;
#154361 = CARTESIAN_POINT('Ctrl Pts',(-29.9825532383426,-14.2808450589491,
112.567643204753)) ;
#154362 = CARTESIAN_POINT('Ctrl Pts',(-30.1266147171513,-14.0045547295033,
113.006431224971)) ;
#154363 = CARTESIAN_POINT('Ctrl Pts',(-29.8146797867088,-14.2808450589491,
112.056327757358)) ;
#154364 = CARTESIAN_POINT('Ctrl Pts',(-29.4529681773643,-14.2808450589491,
112.741514877461)) ;
#154365 = CARTESIAN_POINT('Ctrl Pts',(-29.1425634716928,-14.0045547295033,
113.329511781213)) ;
#154366 = CARTESIAN_POINT('Ctrl Pts',(-29.8146797867088,-14.2808450589491,
112.056327757358)) ;
#154367 = CARTESIAN_POINT('Ctrl Pts',(-29.2850947257306,-14.2808450589491,
112.230199430066)) ;
#154368 = CARTESIAN_POINT('Ctrl Pts',(-28.8306285412503,-14.0045547295033,
112.3794083136)) ;
#154369 = CARTESIAN_POINT('Ctrl Pts',(-29.8146797867088,-14.2808450589491,
112.056327757358)) ;
#154370 = CARTESIAN_POINT('Ctrl Pts',(-29.1172212740968,-14.2808450589491,
111.718883982671)) ;
#154371 = CARTESIAN_POINT('Ctrl Pts',(-28.5186936108078,-14.0045547295033,
111.429304845987)) ;
#154372 = CARTESIAN_POINT('Ctrl Pts',(-29.8146797867088,-14.2808450589491,
112.056327757358)) ;
#154373 = CARTESIAN_POINT('Ctrl Pts',(-29.646806335075,-14.2808450589491,
111.545012309963)) ;
#154374 = CARTESIAN_POINT('Ctrl Pts',(-29.5027448562663,-14.0045547295033,
111.106224289745)) ;
#154375 = CARTESIAN_POINT('Ctrl Pts',(-29.8146797867088,-14.2808450589491,
112.056327757358)) ;
#154376 = CARTESIAN_POINT('Ctrl Pts',(-30.1763913960532,-14.2808450589491,
111.371140637255)) ;
#154377 = CARTESIAN_POINT('Ctrl Pts',(-30.4867961017248,-14.0045547295033,
110.783143733503)) ;
#154378 = CARTESIAN_POINT('Ctrl Pts',(-29.8146797867088,-14.2808450589491,
112.056327757358)) ;
#154379 = CARTESIAN_POINT('Ctrl Pts',(-30.344264847687,-14.2808450589491,
111.88245608465)) ;
#154380 = CARTESIAN_POINT('Ctrl Pts',(-30.7987310321673,-14.0045547295033,
111.733247201116)) ;
#154381 = CARTESIAN_POINT('Ctrl Pts',(-29.8146797867088,-14.2808450589491,
112.056327757358)) ;
#154382 = CARTESIAN_POINT('Ctrl Pts',(-30.5121382993208,-14.2808450589491,
112.393771532045)) ;
#154383 = CARTESIAN_POINT('Ctrl Pts',(-31.1106659626098,-14.0045547295033,
112.683350668729)) ;
#154384 = CARTESIAN_POINT('Ctrl Pts',(-29.8146797867088,-14.2808450589491,
112.056327757358)) ;
#154385 = CARTESIAN_POINT('Ctrl Pts',(-29.9825532383426,-14.2808450589491,
112.567643204753)) ;
#154386 = CARTESIAN_POINT('Ctrl Pts',(-30.1266147171513,-14.0045547295033,
113.006431224971)) ;
#154387 = CARTESIAN_POINT('',(-29.8146797867088,-14.2808450589491,112.056327757358)) ;
#154388 = CARTESIAN_POINT('',(-30.1266147171513,-14.0045547295033,113.006431224971)) ;
#154389 = CARTESIAN_POINT('Origin',(-29.8146797867086,-12.3330093379082,112.056327757358)) ;
#154390 = CARTESIAN_POINT('Origin',(-29.8146797867088,-14.0045547295033,112.056327757358)) ;
#154391 = CARTESIAN_POINT('Ctrl Pts',(-30.1266147171513,-14.0045547295033,
113.006431224971)) ;
#154392 = CARTESIAN_POINT('Ctrl Pts',(-30.1266147171513,-13.5496951436933,
113.006431224971)) ;
#154393 = CARTESIAN_POINT('Ctrl Pts',(-29.1425634716928,-14.0045547295033,
113.329511781213)) ;
#154394 = CARTESIAN_POINT('Ctrl Pts',(-29.1425634716928,-13.5496951436933,
113.329511781213)) ;
#154395 = CARTESIAN_POINT('Ctrl Pts',(-28.8306285412503,-14.0045547295033,
112.3794083136)) ;
#154396 = CARTESIAN_POINT('Ctrl Pts',(-28.8306285412503,-13.5496951436933,
112.3794083136)) ;
#154397 = CARTESIAN_POINT('Ctrl Pts',(-28.5186936108078,-14.0045547295033,
111.429304845987)) ;
#154398 = CARTESIAN_POINT('Ctrl Pts',(-28.5186936108078,-13.5496951436933,
111.429304845987)) ;
#154399 = CARTESIAN_POINT('Ctrl Pts',(-29.5027448562663,-14.0045547295033,
111.106224289745)) ;
#154400 = CARTESIAN_POINT('Ctrl Pts',(-29.5027448562663,-13.5496951436933,
111.106224289745)) ;
#154401 = CARTESIAN_POINT('Ctrl Pts',(-30.4867961017248,-14.0045547295033,
110.783143733503)) ;
#154402 = CARTESIAN_POINT('Ctrl Pts',(-30.4867961017248,-13.5496951436933,
110.783143733503)) ;
#154403 = CARTESIAN_POINT('Ctrl Pts',(-30.7987310321673,-14.0045547295033,
111.733247201116)) ;
#154404 = CARTESIAN_POINT('Ctrl Pts',(-30.7987310321673,-13.5496951436933,
111.733247201116)) ;
#154405 = CARTESIAN_POINT('Ctrl Pts',(-31.1106659626098,-14.0045547295033,
112.683350668729)) ;
#154406 = CARTESIAN_POINT('Ctrl Pts',(-31.1106659626098,-13.5496951436933,
112.683350668729)) ;
#154407 = CARTESIAN_POINT('Ctrl Pts',(-30.1266147171513,-14.0045547295033,
113.006431224971)) ;
#154408 = CARTESIAN_POINT('Ctrl Pts',(-30.1266147171513,-13.5496951436933,
113.006431224971)) ;
#154409 = CARTESIAN_POINT('',(-30.1266147171513,-13.6255050746616,113.006431224971)) ;
#154410 = CARTESIAN_POINT('',(-30.1266147171513,-14.0045547295033,113.006431224971)) ;
#154411 = CARTESIAN_POINT('Origin',(-29.8146797867088,-13.6255050746616,112.056327757358)) ;
#154412 = CARTESIAN_POINT('Ctrl Pts',(-30.1266147171513,-13.6255050746616,
113.006431224971)) ;
#154413 = CARTESIAN_POINT('Ctrl Pts',(-30.0958894083694,-13.6255050746616,
112.912846891931)) ;
#154414 = CARTESIAN_POINT('Ctrl Pts',(-30.0651640995875,-13.6255050746616,
112.819262558892)) ;
#154415 = CARTESIAN_POINT('Ctrl Pts',(-30.0183738600211,-13.6255050746616,
112.67674703875)) ;
#154416 = CARTESIAN_POINT('Ctrl Pts',(-30.0183738600211,-13.4755050746616,
112.67674703875)) ;
#154417 = CARTESIAN_POINT('Ctrl Pts',(-30.0183738600211,-13.3255050746616,
112.67674703875)) ;
#154418 = CARTESIAN_POINT('Ctrl Pts',(-30.0651640995875,-13.3255050746616,
112.819262558892)) ;
#154419 = CARTESIAN_POINT('Ctrl Pts',(-30.0958894083694,-13.3255050746616,
112.912846891931)) ;
#154420 = CARTESIAN_POINT('Ctrl Pts',(-30.1266147171513,-13.3255050746616,
113.006431224971)) ;
#154421 = CARTESIAN_POINT('Ctrl Pts',(-29.1425634716928,-13.6255050746616,
113.329511781213)) ;
#154422 = CARTESIAN_POINT('Ctrl Pts',(-29.2087663213927,-13.6255050746616,
113.204104305322)) ;
#154423 = CARTESIAN_POINT('Ctrl Pts',(-29.2749691710926,-13.6255050746616,
113.07869682943)) ;
#154424 = CARTESIAN_POINT('Ctrl Pts',(-29.375786618345,-13.6255050746616,
112.887719225852)) ;
#154425 = CARTESIAN_POINT('Ctrl Pts',(-29.375786618345,-13.4755050746616,
112.887719225852)) ;
#154426 = CARTESIAN_POINT('Ctrl Pts',(-29.375786618345,-13.3255050746616,
112.887719225852)) ;
#154427 = CARTESIAN_POINT('Ctrl Pts',(-29.2749691710926,-13.3255050746616,
113.07869682943)) ;
#154428 = CARTESIAN_POINT('Ctrl Pts',(-29.2087663213927,-13.3255050746616,
113.204104305322)) ;
#154429 = CARTESIAN_POINT('Ctrl Pts',(-29.1425634716928,-13.3255050746616,
113.329511781213)) ;
#154430 = CARTESIAN_POINT('Ctrl Pts',(-28.8306285412503,-13.6255050746616,
112.3794083136)) ;
#154431 = CARTESIAN_POINT('Ctrl Pts',(-28.9275566997321,-13.6255050746616,
112.347585170748)) ;
#154432 = CARTESIAN_POINT('Ctrl Pts',(-29.0244848582139,-13.6255050746616,
112.315762027896)) ;
#154433 = CARTESIAN_POINT('Ctrl Pts',(-29.1720925450327,-13.6255050746616,
112.26729994446)) ;
#154434 = CARTESIAN_POINT('Ctrl Pts',(-29.1720925450326,-13.4755050746616,
112.26729994446)) ;
#154435 = CARTESIAN_POINT('Ctrl Pts',(-29.1720925450327,-13.3255050746616,
112.26729994446)) ;
#154436 = CARTESIAN_POINT('Ctrl Pts',(-29.0244848582139,-13.3255050746616,
112.315762027896)) ;
#154437 = CARTESIAN_POINT('Ctrl Pts',(-28.9275566997321,-13.3255050746616,
112.347585170748)) ;
#154438 = CARTESIAN_POINT('Ctrl Pts',(-28.8306285412503,-13.3255050746616,
112.3794083136)) ;
#154439 = CARTESIAN_POINT('Ctrl Pts',(-28.5186936108078,-13.6255050746616,
111.429304845987)) ;
#154440 = CARTESIAN_POINT('Ctrl Pts',(-28.6463470780715,-13.6255050746616,
111.491066036175)) ;
#154441 = CARTESIAN_POINT('Ctrl Pts',(-28.7740005453352,-13.6255050746616,
111.552827226362)) ;
#154442 = CARTESIAN_POINT('Ctrl Pts',(-28.9683984717204,-13.6255050746616,
111.646880663068)) ;
#154443 = CARTESIAN_POINT('Ctrl Pts',(-28.9683984717203,-13.4755050746616,
111.646880663068)) ;
#154444 = CARTESIAN_POINT('Ctrl Pts',(-28.9683984717204,-13.3255050746616,
111.646880663068)) ;
#154445 = CARTESIAN_POINT('Ctrl Pts',(-28.7740005453352,-13.3255050746616,
111.552827226362)) ;
#154446 = CARTESIAN_POINT('Ctrl Pts',(-28.6463470780715,-13.3255050746616,
111.491066036175)) ;
#154447 = CARTESIAN_POINT('Ctrl Pts',(-28.5186936108078,-13.3255050746616,
111.429304845987)) ;
#154448 = CARTESIAN_POINT('Ctrl Pts',(-29.5027448562663,-13.6255050746616,
111.106224289745)) ;
#154449 = CARTESIAN_POINT('Ctrl Pts',(-29.5334701650482,-13.6255050746616,
111.199808622785)) ;
#154450 = CARTESIAN_POINT('Ctrl Pts',(-29.5641954738301,-13.6255050746616,
111.293392955824)) ;
#154451 = CARTESIAN_POINT('Ctrl Pts',(-29.6109857133965,-13.6255050746616,
111.435908475966)) ;
#154452 = CARTESIAN_POINT('Ctrl Pts',(-29.6109857133965,-13.4755050746616,
111.435908475966)) ;
#154453 = CARTESIAN_POINT('Ctrl Pts',(-29.6109857133965,-13.3255050746616,
111.435908475966)) ;
#154454 = CARTESIAN_POINT('Ctrl Pts',(-29.5641954738301,-13.3255050746616,
111.293392955824)) ;
#154455 = CARTESIAN_POINT('Ctrl Pts',(-29.5334701650482,-13.3255050746616,
111.199808622785)) ;
#154456 = CARTESIAN_POINT('Ctrl Pts',(-29.5027448562663,-13.3255050746616,
111.106224289745)) ;
#154457 = CARTESIAN_POINT('Ctrl Pts',(-30.4867961017248,-13.6255050746616,
110.783143733503)) ;
#154458 = CARTESIAN_POINT('Ctrl Pts',(-30.4205932520249,-13.6255050746616,
110.908551209394)) ;
#154459 = CARTESIAN_POINT('Ctrl Pts',(-30.354390402325,-13.6255050746616,
111.033958685286)) ;
#154460 = CARTESIAN_POINT('Ctrl Pts',(-30.2535729550726,-13.6255050746616,
111.224936288864)) ;
#154461 = CARTESIAN_POINT('Ctrl Pts',(-30.2535729550726,-13.4755050746616,
111.224936288864)) ;
#154462 = CARTESIAN_POINT('Ctrl Pts',(-30.2535729550726,-13.3255050746616,
111.224936288864)) ;
#154463 = CARTESIAN_POINT('Ctrl Pts',(-30.354390402325,-13.3255050746616,
111.033958685286)) ;
#154464 = CARTESIAN_POINT('Ctrl Pts',(-30.4205932520249,-13.3255050746616,
110.908551209394)) ;
#154465 = CARTESIAN_POINT('Ctrl Pts',(-30.4867961017248,-13.3255050746616,
110.783143733503)) ;
#154466 = CARTESIAN_POINT('Ctrl Pts',(-30.7987310321673,-13.6255050746616,
111.733247201116)) ;
#154467 = CARTESIAN_POINT('Ctrl Pts',(-30.7018028736855,-13.6255050746616,
111.765070343968)) ;
#154468 = CARTESIAN_POINT('Ctrl Pts',(-30.6048747152037,-13.6255050746616,
111.79689348682)) ;
#154469 = CARTESIAN_POINT('Ctrl Pts',(-30.4572670283849,-13.6255050746616,
111.845355570256)) ;
#154470 = CARTESIAN_POINT('Ctrl Pts',(-30.4572670283849,-13.4755050746616,
111.845355570256)) ;
#154471 = CARTESIAN_POINT('Ctrl Pts',(-30.4572670283849,-13.3255050746616,
111.845355570256)) ;
#154472 = CARTESIAN_POINT('Ctrl Pts',(-30.6048747152037,-13.3255050746616,
111.79689348682)) ;
#154473 = CARTESIAN_POINT('Ctrl Pts',(-30.7018028736855,-13.3255050746616,
111.765070343968)) ;
#154474 = CARTESIAN_POINT('Ctrl Pts',(-30.7987310321673,-13.3255050746616,
111.733247201116)) ;
#154475 = CARTESIAN_POINT('Ctrl Pts',(-31.1106659626098,-13.6255050746616,
112.683350668729)) ;
#154476 = CARTESIAN_POINT('Ctrl Pts',(-30.9830124953461,-13.6255050746616,
112.621589478541)) ;
#154477 = CARTESIAN_POINT('Ctrl Pts',(-30.8553590280824,-13.6255050746616,
112.559828288353)) ;
#154478 = CARTESIAN_POINT('Ctrl Pts',(-30.6609611016972,-13.6255050746616,
112.465774851648)) ;
#154479 = CARTESIAN_POINT('Ctrl Pts',(-30.6609611016972,-13.4755050746616,
112.465774851648)) ;
#154480 = CARTESIAN_POINT('Ctrl Pts',(-30.6609611016972,-13.3255050746616,
112.465774851648)) ;
#154481 = CARTESIAN_POINT('Ctrl Pts',(-30.8553590280824,-13.3255050746616,
112.559828288353)) ;
#154482 = CARTESIAN_POINT('Ctrl Pts',(-30.9830124953461,-13.3255050746616,
112.621589478541)) ;
#154483 = CARTESIAN_POINT('Ctrl Pts',(-31.1106659626098,-13.3255050746616,
112.683350668729)) ;
#154484 = CARTESIAN_POINT('Ctrl Pts',(-30.1266147171513,-13.6255050746616,
113.006431224971)) ;
#154485 = CARTESIAN_POINT('Ctrl Pts',(-30.0958894083694,-13.6255050746616,
112.912846891931)) ;
#154486 = CARTESIAN_POINT('Ctrl Pts',(-30.0651640995875,-13.6255050746616,
112.819262558892)) ;
#154487 = CARTESIAN_POINT('Ctrl Pts',(-30.0183738600211,-13.6255050746616,
112.67674703875)) ;
#154488 = CARTESIAN_POINT('Ctrl Pts',(-30.0183738600211,-13.4755050746616,
112.67674703875)) ;
#154489 = CARTESIAN_POINT('Ctrl Pts',(-30.0183738600211,-13.3255050746616,
112.67674703875)) ;
#154490 = CARTESIAN_POINT('Ctrl Pts',(-30.0651640995875,-13.3255050746616,
112.819262558892)) ;
#154491 = CARTESIAN_POINT('Ctrl Pts',(-30.0958894083694,-13.3255050746616,
112.912846891931)) ;
#154492 = CARTESIAN_POINT('Ctrl Pts',(-30.1266147171513,-13.3255050746616,
113.006431224971)) ;
#154493 = CARTESIAN_POINT('',(-30.1266147171513,-13.3255050746616,113.006431224971)) ;
#154494 = CARTESIAN_POINT('Ctrl Pts',(-30.1266147171513,-13.6255050746616,
113.006431224971)) ;
#154495 = CARTESIAN_POINT('Ctrl Pts',(-30.0958894083694,-13.6255050746616,
112.912846891931)) ;
#154496 = CARTESIAN_POINT('Ctrl Pts',(-30.0651640995875,-13.6255050746616,
112.819262558892)) ;
#154497 = CARTESIAN_POINT('Ctrl Pts',(-30.0183738600211,-13.6255050746616,
112.67674703875)) ;
#154498 = CARTESIAN_POINT('Ctrl Pts',(-30.0183738600211,-13.4755050746616,
112.67674703875)) ;
#154499 = CARTESIAN_POINT('Ctrl Pts',(-30.0183738600211,-13.3255050746616,
112.67674703875)) ;
#154500 = CARTESIAN_POINT('Ctrl Pts',(-30.0651640995875,-13.3255050746616,
112.819262558892)) ;
#154501 = CARTESIAN_POINT('Ctrl Pts',(-30.0958894083694,-13.3255050746616,
112.912846891931)) ;
#154502 = CARTESIAN_POINT('Ctrl Pts',(-30.1266147171513,-13.3255050746616,
113.006431224971)) ;
#154503 = CARTESIAN_POINT('Origin',(-29.8146797867088,-13.3255050746616,112.056327757358)) ;
#154504 = CARTESIAN_POINT('Ctrl Pts',(-30.1266147171513,-13.3255050746616,
113.006431224971)) ;
#154505 = CARTESIAN_POINT('Ctrl Pts',(-30.1266147171513,2.53963533952835,
113.006431224971)) ;
#154506 = CARTESIAN_POINT('Ctrl Pts',(-29.1425634716928,-13.3255050746616,
113.329511781213)) ;
#154507 = CARTESIAN_POINT('Ctrl Pts',(-29.1425634716928,2.53963533952835,
113.329511781213)) ;
#154508 = CARTESIAN_POINT('Ctrl Pts',(-28.8306285412503,-13.3255050746616,
112.3794083136)) ;
#154509 = CARTESIAN_POINT('Ctrl Pts',(-28.8306285412503,2.53963533952835,
112.3794083136)) ;
#154510 = CARTESIAN_POINT('Ctrl Pts',(-28.5186936108078,-13.3255050746616,
111.429304845987)) ;
#154511 = CARTESIAN_POINT('Ctrl Pts',(-28.5186936108078,2.53963533952835,
111.429304845987)) ;
#154512 = CARTESIAN_POINT('Ctrl Pts',(-29.5027448562663,-13.3255050746616,
111.106224289745)) ;
#154513 = CARTESIAN_POINT('Ctrl Pts',(-29.5027448562663,2.53963533952835,
111.106224289745)) ;
#154514 = CARTESIAN_POINT('Ctrl Pts',(-30.4867961017248,-13.3255050746616,
110.783143733503)) ;
#154515 = CARTESIAN_POINT('Ctrl Pts',(-30.4867961017248,2.53963533952835,
110.783143733503)) ;
#154516 = CARTESIAN_POINT('Ctrl Pts',(-30.7987310321673,-13.3255050746616,
111.733247201116)) ;
#154517 = CARTESIAN_POINT('Ctrl Pts',(-30.7987310321673,2.53963533952835,
111.733247201116)) ;
#154518 = CARTESIAN_POINT('Ctrl Pts',(-31.1106659626098,-13.3255050746616,
112.683350668729)) ;
#154519 = CARTESIAN_POINT('Ctrl Pts',(-31.1106659626098,2.53963533952835,
112.683350668729)) ;
#154520 = CARTESIAN_POINT('Ctrl Pts',(-30.1266147171513,-13.3255050746616,
113.006431224971)) ;
#154521 = CARTESIAN_POINT('Ctrl Pts',(-30.1266147171513,2.53963533952835,
113.006431224971)) ;
#154522 = CARTESIAN_POINT('',(-30.1266147171513,-0.104554729503315,113.006431224971)) ;
#154523 = CARTESIAN_POINT('',(-30.1266147171513,-13.3255050746616,113.006431224971)) ;
#154524 = CARTESIAN_POINT('Origin',(-29.8146797867088,-0.104554729503315,
112.056327757358)) ;
#154525 = CARTESIAN_POINT('Ctrl Pts',(-30.1266147171513,-0.104554729503315,
113.006431224971)) ;
#154526 = CARTESIAN_POINT('Ctrl Pts',(-30.095421224107,-0.00455472950331526,
112.911420878209)) ;
#154527 = CARTESIAN_POINT('Ctrl Pts',(-29.1425634716928,-0.104554729503315,
113.329511781213)) ;
#154528 = CARTESIAN_POINT('Ctrl Pts',(-29.2097751031944,-0.00455472950331526,
113.202193378827)) ;
#154529 = CARTESIAN_POINT('Ctrl Pts',(-28.8306285412503,-0.104554729503315,
112.3794083136)) ;
#154530 = CARTESIAN_POINT('Ctrl Pts',(-28.9290336657961,-0.00455472950331526,
112.347100257976)) ;
#154531 = CARTESIAN_POINT('Ctrl Pts',(-28.5186936108078,-0.104554729503315,
111.429304845987)) ;
#154532 = CARTESIAN_POINT('Ctrl Pts',(-28.6482922283979,-0.00455472950331526,
111.492007137124)) ;
#154533 = CARTESIAN_POINT('Ctrl Pts',(-29.5027448562663,-0.104554729503315,
111.106224289745)) ;
#154534 = CARTESIAN_POINT('Ctrl Pts',(-29.5339383493105,-0.00455472950331526,
111.201234636506)) ;
#154535 = CARTESIAN_POINT('Ctrl Pts',(-30.4867961017248,-0.104554729503315,
110.783143733503)) ;
#154536 = CARTESIAN_POINT('Ctrl Pts',(-30.4195844702232,-0.00455472950331526,
110.910462135889)) ;
#154537 = CARTESIAN_POINT('Ctrl Pts',(-30.7987310321673,-0.104554729503315,
111.733247201116)) ;
#154538 = CARTESIAN_POINT('Ctrl Pts',(-30.7003259076214,-0.00455472950331526,
111.76555525674)) ;
#154539 = CARTESIAN_POINT('Ctrl Pts',(-31.1106659626098,-0.104554729503315,
112.683350668729)) ;
#154540 = CARTESIAN_POINT('Ctrl Pts',(-30.9810673450197,-0.00455472950331526,
112.620648377591)) ;
#154541 = CARTESIAN_POINT('Ctrl Pts',(-30.1266147171513,-0.104554729503315,
113.006431224971)) ;
#154542 = CARTESIAN_POINT('Ctrl Pts',(-30.095421224107,-0.00455472950331526,
112.911420878209)) ;
#154543 = CARTESIAN_POINT('',(-30.1266147171513,-0.104554729503315,113.006431224971)) ;
#154544 = CARTESIAN_POINT('Origin',(-5.81917539329314,-0.00455472950331526,
120.408087607083)) ;
#154545 = CARTESIAN_POINT('',(-5.95954611199226,-0.00455472950331526,120.835634167509)) ;
#154546 = CARTESIAN_POINT('',(-5.67880467459401,-0.00455472950331526,119.980541046657)) ;
#154547 = CARTESIAN_POINT('',(-5.95954611199226,-0.00455472950331526,120.835634167509)) ;
#154548 = CARTESIAN_POINT('Origin',(-5.67880467459401,-0.00455472950331526,
119.980541046657)) ;
#154549 = CARTESIAN_POINT('Ctrl Pts',(-5.67880467459401,-14.2808450589491,
119.980541046657)) ;
#154550 = CARTESIAN_POINT('Ctrl Pts',(-5.67880467459401,-14.2808450589491,
119.980541046657)) ;
#154551 = CARTESIAN_POINT('Ctrl Pts',(-5.67880467459401,-14.2808450589491,
119.980541046657)) ;
#154552 = CARTESIAN_POINT('Ctrl Pts',(-5.67880467459401,-14.2808450589491,
119.980541046657)) ;
#154553 = CARTESIAN_POINT('Ctrl Pts',(-5.67880467459401,-14.2808450589491,
119.980541046657)) ;
#154554 = CARTESIAN_POINT('Ctrl Pts',(-5.67880467459401,-14.2808450589491,
119.980541046657)) ;
#154555 = CARTESIAN_POINT('Ctrl Pts',(-5.67880467459401,-14.2808450589491,
119.980541046657)) ;
#154556 = CARTESIAN_POINT('Ctrl Pts',(-5.67880467459401,-14.2808450589491,
119.980541046657)) ;
#154557 = CARTESIAN_POINT('Ctrl Pts',(-5.67880467459401,-14.2808450589491,
119.980541046657)) ;
#154558 = CARTESIAN_POINT('Ctrl Pts',(-5.84667812622779,-14.2808450589491,
120.491856494052)) ;
#154559 = CARTESIAN_POINT('Ctrl Pts',(-6.37626318720601,-14.2808450589491,
120.317984821344)) ;
#154560 = CARTESIAN_POINT('Ctrl Pts',(-6.20838973557223,-14.2808450589491,
119.806669373949)) ;
#154561 = CARTESIAN_POINT('Ctrl Pts',(-6.04051628393846,-14.2808450589491,
119.295353926554)) ;
#154562 = CARTESIAN_POINT('Ctrl Pts',(-5.51093122296023,-14.2808450589491,
119.469225599262)) ;
#154563 = CARTESIAN_POINT('Ctrl Pts',(-4.981346161982,-14.2808450589491,119.64309727197)) ;
#154564 = CARTESIAN_POINT('Ctrl Pts',(-5.14921961361578,-14.2808450589491,
120.154412719365)) ;
#154565 = CARTESIAN_POINT('Ctrl Pts',(-5.31709306524956,-14.2808450589491,
120.66572816676)) ;
#154566 = CARTESIAN_POINT('Ctrl Pts',(-5.84667812622779,-14.2808450589491,
120.491856494052)) ;
#154567 = CARTESIAN_POINT('Ctrl Pts',(-5.99073960503651,-14.0045547295033,
120.93064451427)) ;
#154568 = CARTESIAN_POINT('Ctrl Pts',(-6.97479085049501,-14.0045547295033,
120.607563958028)) ;
#154569 = CARTESIAN_POINT('Ctrl Pts',(-6.6628559200525,-14.0045547295033,
119.657460490415)) ;
#154570 = CARTESIAN_POINT('Ctrl Pts',(-6.35092098961,-14.0045547295033,118.707357022802)) ;
#154571 = CARTESIAN_POINT('Ctrl Pts',(-5.36686974415151,-14.0045547295033,
119.030437579044)) ;
#154572 = CARTESIAN_POINT('Ctrl Pts',(-4.38281849869301,-14.0045547295033,
119.353518135287)) ;
#154573 = CARTESIAN_POINT('Ctrl Pts',(-4.69475342913551,-14.0045547295033,
120.303621602899)) ;
#154574 = CARTESIAN_POINT('Ctrl Pts',(-5.00668835957801,-14.0045547295033,
121.253725070512)) ;
#154575 = CARTESIAN_POINT('Ctrl Pts',(-5.99073960503651,-14.0045547295033,
120.93064451427)) ;
#154576 = CARTESIAN_POINT('',(-5.99073960503651,-14.0045547295033,120.93064451427)) ;
#154577 = CARTESIAN_POINT('Origin',(-5.67880467459401,-14.0045547295033,119.980541046657)) ;
#154578 = CARTESIAN_POINT('',(-5.67880467459401,-14.2808450589491,119.980541046657)) ;
#154579 = CARTESIAN_POINT('Origin',(-5.67880467459393,-12.333009337908,119.980541046657)) ;
#154580 = CARTESIAN_POINT('Ctrl Pts',(-5.99073960503651,-14.0045547295033,
120.93064451427)) ;
#154581 = CARTESIAN_POINT('Ctrl Pts',(-5.99073960503651,-13.5496951436933,
120.93064451427)) ;
#154582 = CARTESIAN_POINT('Ctrl Pts',(-6.97479085049501,-14.0045547295033,
120.607563958028)) ;
#154583 = CARTESIAN_POINT('Ctrl Pts',(-6.97479085049501,-13.5496951436933,
120.607563958028)) ;
#154584 = CARTESIAN_POINT('Ctrl Pts',(-6.6628559200525,-14.0045547295033,
119.657460490415)) ;
#154585 = CARTESIAN_POINT('Ctrl Pts',(-6.6628559200525,-13.5496951436933,
119.657460490415)) ;
#154586 = CARTESIAN_POINT('Ctrl Pts',(-6.35092098961,-14.0045547295033,118.707357022802)) ;
#154587 = CARTESIAN_POINT('Ctrl Pts',(-6.35092098961,-13.5496951436933,118.707357022802)) ;
#154588 = CARTESIAN_POINT('Ctrl Pts',(-5.3668697441515,-14.0045547295033,
119.030437579044)) ;
#154589 = CARTESIAN_POINT('Ctrl Pts',(-5.3668697441515,-13.5496951436933,
119.030437579044)) ;
#154590 = CARTESIAN_POINT('Ctrl Pts',(-4.38281849869301,-14.0045547295033,
119.353518135287)) ;
#154591 = CARTESIAN_POINT('Ctrl Pts',(-4.38281849869301,-13.5496951436933,
119.353518135287)) ;
#154592 = CARTESIAN_POINT('Ctrl Pts',(-4.69475342913551,-14.0045547295033,
120.303621602899)) ;
#154593 = CARTESIAN_POINT('Ctrl Pts',(-4.69475342913551,-13.5496951436933,
120.303621602899)) ;
#154594 = CARTESIAN_POINT('Ctrl Pts',(-5.00668835957802,-14.0045547295033,
121.253725070512)) ;
#154595 = CARTESIAN_POINT('Ctrl Pts',(-5.00668835957802,-13.5496951436933,
121.253725070512)) ;
#154596 = CARTESIAN_POINT('Ctrl Pts',(-5.99073960503651,-14.0045547295033,
120.93064451427)) ;
#154597 = CARTESIAN_POINT('Ctrl Pts',(-5.99073960503651,-13.5496951436933,
120.93064451427)) ;
#154598 = CARTESIAN_POINT('',(-5.99073960503651,-13.6255050746616,120.93064451427)) ;
#154599 = CARTESIAN_POINT('Origin',(-5.67880467459401,-13.6255050746616,119.980541046657)) ;
#154600 = CARTESIAN_POINT('',(-5.99073960503651,-14.0045547295033,120.93064451427)) ;
#154601 = CARTESIAN_POINT('Ctrl Pts',(-5.99073960503651,-13.6255050746616,
120.93064451427)) ;
#154602 = CARTESIAN_POINT('Ctrl Pts',(-6.97479085049501,-13.6255050746616,
120.607563958028)) ;
#154603 = CARTESIAN_POINT('Ctrl Pts',(-6.6628559200525,-13.6255050746616,
119.657460490415)) ;
#154604 = CARTESIAN_POINT('Ctrl Pts',(-6.35092098961,-13.6255050746616,118.707357022802)) ;
#154605 = CARTESIAN_POINT('Ctrl Pts',(-5.3668697441515,-13.6255050746616,
119.030437579044)) ;
#154606 = CARTESIAN_POINT('Ctrl Pts',(-4.38281849869301,-13.6255050746616,
119.353518135287)) ;
#154607 = CARTESIAN_POINT('Ctrl Pts',(-4.69475342913551,-13.6255050746616,
120.303621602899)) ;
#154608 = CARTESIAN_POINT('Ctrl Pts',(-5.00668835957802,-13.6255050746616,
121.253725070512)) ;
#154609 = CARTESIAN_POINT('Ctrl Pts',(-5.99073960503651,-13.6255050746616,
120.93064451427)) ;
#154610 = CARTESIAN_POINT('Ctrl Pts',(-5.9600142962546,-13.6255050746616,
120.837060181231)) ;
#154611 = CARTESIAN_POINT('Ctrl Pts',(-6.84713738323131,-13.6255050746616,
120.54580276784)) ;
#154612 = CARTESIAN_POINT('Ctrl Pts',(-6.56592776157072,-13.6255050746616,
119.689283633267)) ;
#154613 = CARTESIAN_POINT('Ctrl Pts',(-6.28471813991013,-13.6255050746616,
118.832764498694)) ;
#154614 = CARTESIAN_POINT('Ctrl Pts',(-5.39759505293342,-13.6255050746616,
119.124021912084)) ;
#154615 = CARTESIAN_POINT('Ctrl Pts',(-4.51047196595671,-13.6255050746616,
119.415279325474)) ;
#154616 = CARTESIAN_POINT('Ctrl Pts',(-4.7916815876173,-13.6255050746616,
120.271798460047)) ;
#154617 = CARTESIAN_POINT('Ctrl Pts',(-5.07289120927789,-13.6255050746616,
121.128317594621)) ;
#154618 = CARTESIAN_POINT('Ctrl Pts',(-5.9600142962546,-13.6255050746616,
120.837060181231)) ;
#154619 = CARTESIAN_POINT('Ctrl Pts',(-5.92928898747268,-13.6255050746616,
120.743475848191)) ;
#154620 = CARTESIAN_POINT('Ctrl Pts',(-6.71948391596759,-13.6255050746616,
120.484041577653)) ;
#154621 = CARTESIAN_POINT('Ctrl Pts',(-6.46899960308891,-13.6255050746616,
119.721106776119)) ;
#154622 = CARTESIAN_POINT('Ctrl Pts',(-6.21851529021024,-13.6255050746616,
118.958171974585)) ;
#154623 = CARTESIAN_POINT('Ctrl Pts',(-5.42832036171533,-13.6255050746616,
119.217606245123)) ;
#154624 = CARTESIAN_POINT('Ctrl Pts',(-4.63812543322043,-13.6255050746616,
119.477040515662)) ;
#154625 = CARTESIAN_POINT('Ctrl Pts',(-4.8886097460991,-13.6255050746616,
120.239975317196)) ;
#154626 = CARTESIAN_POINT('Ctrl Pts',(-5.13909405897778,-13.6255050746616,
121.002910118729)) ;
#154627 = CARTESIAN_POINT('Ctrl Pts',(-5.92928898747268,-13.6255050746616,
120.743475848191)) ;
#154628 = CARTESIAN_POINT('Ctrl Pts',(-5.88249874790631,-13.6255050746616,
120.600960328049)) ;
#154629 = CARTESIAN_POINT('Ctrl Pts',(-6.52508598958243,-13.6255050746616,
120.389988140947)) ;
#154630 = CARTESIAN_POINT('Ctrl Pts',(-6.32139191627013,-13.6255050746616,
119.769568859555)) ;
#154631 = CARTESIAN_POINT('Ctrl Pts',(-6.11769784295783,-13.6255050746616,
119.149149578163)) ;
#154632 = CARTESIAN_POINT('Ctrl Pts',(-5.47511060128171,-13.6255050746616,
119.360121765265)) ;
#154633 = CARTESIAN_POINT('Ctrl Pts',(-4.83252335960559,-13.6255050746616,
119.571093952367)) ;
#154634 = CARTESIAN_POINT('Ctrl Pts',(-5.03621743291789,-13.6255050746616,
120.191513233759)) ;
#154635 = CARTESIAN_POINT('Ctrl Pts',(-5.23991150623019,-13.6255050746616,
120.811932515151)) ;
#154636 = CARTESIAN_POINT('Ctrl Pts',(-5.88249874790631,-13.6255050746616,
120.600960328049)) ;
#154637 = CARTESIAN_POINT('Ctrl Pts',(-5.88249874790631,-13.4755050746616,
120.600960328049)) ;
#154638 = CARTESIAN_POINT('Ctrl Pts',(-6.52508598958244,-13.4755050746616,
120.389988140947)) ;
#154639 = CARTESIAN_POINT('Ctrl Pts',(-6.32139191627014,-13.4755050746616,
119.769568859555)) ;
#154640 = CARTESIAN_POINT('Ctrl Pts',(-6.11769784295784,-13.4755050746616,
119.149149578163)) ;
#154641 = CARTESIAN_POINT('Ctrl Pts',(-5.47511060128171,-13.4755050746616,
119.360121765265)) ;
#154642 = CARTESIAN_POINT('Ctrl Pts',(-4.83252335960557,-13.4755050746616,
119.571093952367)) ;
#154643 = CARTESIAN_POINT('Ctrl Pts',(-5.03621743291787,-13.4755050746616,
120.191513233759)) ;
#154644 = CARTESIAN_POINT('Ctrl Pts',(-5.23991150623018,-13.4755050746616,
120.811932515151)) ;
#154645 = CARTESIAN_POINT('Ctrl Pts',(-5.88249874790631,-13.4755050746616,
120.600960328049)) ;
#154646 = CARTESIAN_POINT('Ctrl Pts',(-5.88249874790631,-13.3255050746616,
120.600960328049)) ;
#154647 = CARTESIAN_POINT('Ctrl Pts',(-6.52508598958243,-13.3255050746616,
120.389988140947)) ;
#154648 = CARTESIAN_POINT('Ctrl Pts',(-6.32139191627013,-13.3255050746616,
119.769568859555)) ;
#154649 = CARTESIAN_POINT('Ctrl Pts',(-6.11769784295783,-13.3255050746616,
119.149149578163)) ;
#154650 = CARTESIAN_POINT('Ctrl Pts',(-5.47511060128171,-13.3255050746616,
119.360121765265)) ;
#154651 = CARTESIAN_POINT('Ctrl Pts',(-4.83252335960559,-13.3255050746616,
119.571093952367)) ;
#154652 = CARTESIAN_POINT('Ctrl Pts',(-5.03621743291789,-13.3255050746616,
120.191513233759)) ;
#154653 = CARTESIAN_POINT('Ctrl Pts',(-5.23991150623019,-13.3255050746616,
120.811932515151)) ;
#154654 = CARTESIAN_POINT('Ctrl Pts',(-5.88249874790631,-13.3255050746616,
120.600960328049)) ;
#154655 = CARTESIAN_POINT('Ctrl Pts',(-5.92928898747268,-13.3255050746616,
120.743475848191)) ;
#154656 = CARTESIAN_POINT('Ctrl Pts',(-6.71948391596759,-13.3255050746616,
120.484041577653)) ;
#154657 = CARTESIAN_POINT('Ctrl Pts',(-6.46899960308891,-13.3255050746616,
119.721106776119)) ;
#154658 = CARTESIAN_POINT('Ctrl Pts',(-6.21851529021024,-13.3255050746616,
118.958171974585)) ;
#154659 = CARTESIAN_POINT('Ctrl Pts',(-5.42832036171533,-13.3255050746616,
119.217606245123)) ;
#154660 = CARTESIAN_POINT('Ctrl Pts',(-4.63812543322043,-13.3255050746616,
119.477040515662)) ;
#154661 = CARTESIAN_POINT('Ctrl Pts',(-4.8886097460991,-13.3255050746616,
120.239975317196)) ;
#154662 = CARTESIAN_POINT('Ctrl Pts',(-5.13909405897778,-13.3255050746616,
121.002910118729)) ;
#154663 = CARTESIAN_POINT('Ctrl Pts',(-5.92928898747268,-13.3255050746616,
120.743475848191)) ;
#154664 = CARTESIAN_POINT('Ctrl Pts',(-5.9600142962546,-13.3255050746616,
120.837060181231)) ;
#154665 = CARTESIAN_POINT('Ctrl Pts',(-6.84713738323131,-13.3255050746616,
120.54580276784)) ;
#154666 = CARTESIAN_POINT('Ctrl Pts',(-6.56592776157072,-13.3255050746616,
119.689283633267)) ;
#154667 = CARTESIAN_POINT('Ctrl Pts',(-6.28471813991013,-13.3255050746616,
118.832764498694)) ;
#154668 = CARTESIAN_POINT('Ctrl Pts',(-5.39759505293342,-13.3255050746616,
119.124021912084)) ;
#154669 = CARTESIAN_POINT('Ctrl Pts',(-4.51047196595671,-13.3255050746616,
119.415279325474)) ;
#154670 = CARTESIAN_POINT('Ctrl Pts',(-4.7916815876173,-13.3255050746616,
120.271798460047)) ;
#154671 = CARTESIAN_POINT('Ctrl Pts',(-5.07289120927789,-13.3255050746616,
121.128317594621)) ;
#154672 = CARTESIAN_POINT('Ctrl Pts',(-5.9600142962546,-13.3255050746616,
120.837060181231)) ;
#154673 = CARTESIAN_POINT('Ctrl Pts',(-5.99073960503651,-13.3255050746616,
120.93064451427)) ;
#154674 = CARTESIAN_POINT('Ctrl Pts',(-6.97479085049501,-13.3255050746616,
120.607563958028)) ;
#154675 = CARTESIAN_POINT('Ctrl Pts',(-6.6628559200525,-13.3255050746616,
119.657460490415)) ;
#154676 = CARTESIAN_POINT('Ctrl Pts',(-6.35092098961,-13.3255050746616,118.707357022802)) ;
#154677 = CARTESIAN_POINT('Ctrl Pts',(-5.3668697441515,-13.3255050746616,
119.030437579044)) ;
#154678 = CARTESIAN_POINT('Ctrl Pts',(-4.38281849869301,-13.3255050746616,
119.353518135287)) ;
#154679 = CARTESIAN_POINT('Ctrl Pts',(-4.69475342913551,-13.3255050746616,
120.303621602899)) ;
#154680 = CARTESIAN_POINT('Ctrl Pts',(-5.00668835957802,-13.3255050746616,
121.253725070512)) ;
#154681 = CARTESIAN_POINT('Ctrl Pts',(-5.99073960503651,-13.3255050746616,
120.93064451427)) ;
#154682 = CARTESIAN_POINT('',(-5.99073960503651,-13.3255050746616,120.93064451427)) ;
#154683 = CARTESIAN_POINT('Origin',(-5.67880467459401,-13.3255050746616,119.980541046657)) ;
#154684 = CARTESIAN_POINT('Ctrl Pts',(-5.99073960503651,-13.6255050746616,
120.93064451427)) ;
#154685 = CARTESIAN_POINT('Ctrl Pts',(-5.9600142962546,-13.6255050746616,
120.837060181231)) ;
#154686 = CARTESIAN_POINT('Ctrl Pts',(-5.92928898747268,-13.6255050746616,
120.743475848191)) ;
#154687 = CARTESIAN_POINT('Ctrl Pts',(-5.88249874790631,-13.6255050746616,
120.600960328049)) ;
#154688 = CARTESIAN_POINT('Ctrl Pts',(-5.88249874790631,-13.4755050746616,
120.600960328049)) ;
#154689 = CARTESIAN_POINT('Ctrl Pts',(-5.88249874790631,-13.3255050746616,
120.600960328049)) ;
#154690 = CARTESIAN_POINT('Ctrl Pts',(-5.92928898747268,-13.3255050746616,
120.743475848191)) ;
#154691 = CARTESIAN_POINT('Ctrl Pts',(-5.9600142962546,-13.3255050746616,
120.837060181231)) ;
#154692 = CARTESIAN_POINT('Ctrl Pts',(-5.99073960503651,-13.3255050746616,
120.93064451427)) ;
#154693 = CARTESIAN_POINT('Ctrl Pts',(-5.99073960503651,-13.3255050746616,
120.93064451427)) ;
#154694 = CARTESIAN_POINT('Ctrl Pts',(-5.99073960503651,2.53963533952835,
120.93064451427)) ;
#154695 = CARTESIAN_POINT('Ctrl Pts',(-6.97479085049501,-13.3255050746616,
120.607563958028)) ;
#154696 = CARTESIAN_POINT('Ctrl Pts',(-6.97479085049501,2.53963533952835,
120.607563958028)) ;
#154697 = CARTESIAN_POINT('Ctrl Pts',(-6.6628559200525,-13.3255050746616,
119.657460490415)) ;
#154698 = CARTESIAN_POINT('Ctrl Pts',(-6.6628559200525,2.53963533952835,119.657460490415)) ;
#154699 = CARTESIAN_POINT('Ctrl Pts',(-6.35092098961,-13.3255050746616,118.707357022802)) ;
#154700 = CARTESIAN_POINT('Ctrl Pts',(-6.35092098961,2.53963533952835,118.707357022802)) ;
#154701 = CARTESIAN_POINT('Ctrl Pts',(-5.3668697441515,-13.3255050746616,
119.030437579044)) ;
#154702 = CARTESIAN_POINT('Ctrl Pts',(-5.3668697441515,2.53963533952835,119.030437579044)) ;
#154703 = CARTESIAN_POINT('Ctrl Pts',(-4.38281849869301,-13.3255050746616,
119.353518135287)) ;
#154704 = CARTESIAN_POINT('Ctrl Pts',(-4.38281849869301,2.53963533952835,
119.353518135287)) ;
#154705 = CARTESIAN_POINT('Ctrl Pts',(-4.69475342913551,-13.3255050746616,
120.303621602899)) ;
#154706 = CARTESIAN_POINT('Ctrl Pts',(-4.69475342913551,2.53963533952835,
120.303621602899)) ;
#154707 = CARTESIAN_POINT('Ctrl Pts',(-5.00668835957802,-13.3255050746616,
121.253725070512)) ;
#154708 = CARTESIAN_POINT('Ctrl Pts',(-5.00668835957802,2.53963533952835,
121.253725070512)) ;
#154709 = CARTESIAN_POINT('Ctrl Pts',(-5.99073960503651,-13.3255050746616,
120.93064451427)) ;
#154710 = CARTESIAN_POINT('Ctrl Pts',(-5.99073960503651,2.53963533952835,
120.93064451427)) ;
#154711 = CARTESIAN_POINT('',(-5.99073960503651,-0.104554729503315,120.93064451427)) ;
#154712 = CARTESIAN_POINT('Origin',(-5.67880467459401,-0.104554729503315,
119.980541046657)) ;
#154713 = CARTESIAN_POINT('',(-5.99073960503651,-13.3255050746616,120.93064451427)) ;
#154714 = CARTESIAN_POINT('Ctrl Pts',(-5.99073960503651,-0.104554729503315,
120.93064451427)) ;
#154715 = CARTESIAN_POINT('Ctrl Pts',(-6.97479085049501,-0.104554729503315,
120.607563958028)) ;
#154716 = CARTESIAN_POINT('Ctrl Pts',(-6.6628559200525,-0.104554729503315,
119.657460490415)) ;
#154717 = CARTESIAN_POINT('Ctrl Pts',(-6.35092098961,-0.104554729503315,118.707357022802)) ;
#154718 = CARTESIAN_POINT('Ctrl Pts',(-5.3668697441515,-0.104554729503315,
119.030437579044)) ;
#154719 = CARTESIAN_POINT('Ctrl Pts',(-4.38281849869301,-0.104554729503315,
119.353518135287)) ;
#154720 = CARTESIAN_POINT('Ctrl Pts',(-4.69475342913551,-0.104554729503315,
120.303621602899)) ;
#154721 = CARTESIAN_POINT('Ctrl Pts',(-5.00668835957802,-0.104554729503315,
121.253725070512)) ;
#154722 = CARTESIAN_POINT('Ctrl Pts',(-5.99073960503651,-0.104554729503315,
120.93064451427)) ;
#154723 = CARTESIAN_POINT('Ctrl Pts',(-5.95954611199226,-0.00455472950331526,
120.835634167509)) ;
#154724 = CARTESIAN_POINT('Ctrl Pts',(-6.8451922329049,-0.00455472950331526,
120.544861666891)) ;
#154725 = CARTESIAN_POINT('Ctrl Pts',(-6.56445079550665,-0.00455472950331526,
119.689768546039)) ;
#154726 = CARTESIAN_POINT('Ctrl Pts',(-6.28370935810839,-0.00455472950331526,
118.834675425188)) ;
#154727 = CARTESIAN_POINT('Ctrl Pts',(-5.39806323719575,-0.00455472950331526,
119.125447925806)) ;
#154728 = CARTESIAN_POINT('Ctrl Pts',(-4.51241711628311,-0.00455472950331526,
119.416220426424)) ;
#154729 = CARTESIAN_POINT('Ctrl Pts',(-4.79315855368137,-0.00455472950331526,
120.271313547275)) ;
#154730 = CARTESIAN_POINT('Ctrl Pts',(-5.07389999107962,-0.00455472950331526,
121.126406668127)) ;
#154731 = CARTESIAN_POINT('Ctrl Pts',(-5.95954611199226,-0.00455472950331526,
120.835634167509)) ;
#154732 = CARTESIAN_POINT('',(-5.99073960503651,-0.104554729503315,120.93064451427)) ;
#154733 = CARTESIAN_POINT('Origin',(-5.91338286987807,-13.4878920043255,119.207537192558)) ;
#154734 = CARTESIAN_POINT('',(-5.85699395434883,-13.4607154515732,119.377580402306)) ;
#154735 = CARTESIAN_POINT('Origin',(-5.8796005086299,-13.4878920043255,119.310518769832)) ;
#154736 = CARTESIAN_POINT('Ctrl Pts',(-6.34456572554058,-13.1500241806476,
118.666226584225)) ;
#154737 = CARTESIAN_POINT('Ctrl Pts',(-6.36725418306881,-13.1683184483544,
118.735331965087)) ;
#154738 = CARTESIAN_POINT('Ctrl Pts',(-6.44105802647819,-13.1683184483544,
118.711100923369)) ;
#154739 = CARTESIAN_POINT('Ctrl Pts',(-6.51486186988758,-13.1683184483544,
118.686869881651)) ;
#154740 = CARTESIAN_POINT('Ctrl Pts',(-6.49217341235936,-13.1500241806476,
118.617764500789)) ;
#154741 = CARTESIAN_POINT('Ctrl Pts',(-6.46948495483114,-13.1317299129408,
118.548659119927)) ;
#154742 = CARTESIAN_POINT('Ctrl Pts',(-6.39568111142176,-13.1317299129408,
118.572890161645)) ;
#154743 = CARTESIAN_POINT('Ctrl Pts',(-6.32187726801236,-13.1317299129408,
118.597121203363)) ;
#154744 = CARTESIAN_POINT('Ctrl Pts',(-6.34456572554058,-13.1500241806476,
118.666226584225)) ;
#154745 = CARTESIAN_POINT('Ctrl Pts',(-6.34529362630125,-13.1438552129684,
118.667661018198)) ;
#154746 = CARTESIAN_POINT('Ctrl Pts',(-6.36794803444601,-13.1625827638083,
118.736662689976)) ;
#154747 = CARTESIAN_POINT('Ctrl Pts',(-6.44175187709088,-13.1625827713816,
118.712431645929)) ;
#154748 = CARTESIAN_POINT('Ctrl Pts',(-6.51555571973573,-13.1625827789549,
118.688200601882)) ;
#154749 = CARTESIAN_POINT('Ctrl Pts',(-6.49290131159096,-13.143855228115,
118.619198930104)) ;
#154750 = CARTESIAN_POINT('Ctrl Pts',(-6.4702469034462,-13.1251276772751,
118.550197258326)) ;
#154751 = CARTESIAN_POINT('Ctrl Pts',(-6.39644306080134,-13.1251276697018,
118.574428302373)) ;
#154752 = CARTESIAN_POINT('Ctrl Pts',(-6.32263921815648,-13.1251276621286,
118.59865934642)) ;
#154753 = CARTESIAN_POINT('Ctrl Pts',(-6.34529362630125,-13.1438552129684,
118.667661018198)) ;
#154754 = CARTESIAN_POINT('Ctrl Pts',(-6.35716264371204,-13.045472096163,
118.691303794064)) ;
#154755 = CARTESIAN_POINT('Ctrl Pts',(-6.37925822797836,-13.0710887780094,
118.758603382009)) ;
#154756 = CARTESIAN_POINT('Ctrl Pts',(-6.45306208999897,-13.0710886158947,
118.734372396978)) ;
#154757 = CARTESIAN_POINT('Ctrl Pts',(-6.52686595201958,-13.07108845378,118.710141411947)) ;
#154758 = CARTESIAN_POINT('Ctrl Pts',(-6.50477036775327,-13.0454717719336,
118.642841824001)) ;
#154759 = CARTESIAN_POINT('Ctrl Pts',(-6.48267478348697,-13.0198550900872,
118.575542236056)) ;
#154760 = CARTESIAN_POINT('Ctrl Pts',(-6.40887092146635,-13.0198552522019,
118.599773221087)) ;
#154761 = CARTESIAN_POINT('Ctrl Pts',(-6.33506705944574,-13.0198554143166,
118.624004206118)) ;
#154762 = CARTESIAN_POINT('Ctrl Pts',(-6.35716264371204,-13.045472096163,
118.691303794064)) ;
#154763 = CARTESIAN_POINT('Ctrl Pts',(-6.38921314251039,-12.8597742993635,
118.764325222303)) ;
#154764 = CARTESIAN_POINT('Ctrl Pts',(-6.40960406991293,-12.8983625293638,
118.826432695618)) ;
#154765 = CARTESIAN_POINT('Ctrl Pts',(-6.48340790505723,-12.8983626007157,
118.802201628725)) ;
#154766 = CARTESIAN_POINT('Ctrl Pts',(-6.55721174020152,-12.8983626720675,
118.777970561833)) ;
#154767 = CARTESIAN_POINT('Ctrl Pts',(-6.53682081279897,-12.8597744420672,
118.715863088518)) ;
#154768 = CARTESIAN_POINT('Ctrl Pts',(-6.51642988539642,-12.821186212067,
118.653755615204)) ;
#154769 = CARTESIAN_POINT('Ctrl Pts',(-6.44262605025212,-12.8211861407151,
118.677986682097)) ;
#154770 = CARTESIAN_POINT('Ctrl Pts',(-6.36882221510784,-12.8211860693632,
118.702217748989)) ;
#154771 = CARTESIAN_POINT('Ctrl Pts',(-6.38921314251039,-12.8597742993635,
118.764325222303)) ;
#154772 = CARTESIAN_POINT('Ctrl Pts',(-6.45615197626408,-12.6327839415056,
118.932852707777)) ;
#154773 = CARTESIAN_POINT('Ctrl Pts',(-6.47262988951442,-12.6872840912264,
118.983041773343)) ;
#154774 = CARTESIAN_POINT('Ctrl Pts',(-6.54643373625563,-12.6872840678826,
118.958810741773)) ;
#154775 = CARTESIAN_POINT('Ctrl Pts',(-6.62023758299684,-12.6872840445389,
118.934579710203)) ;
#154776 = CARTESIAN_POINT('Ctrl Pts',(-6.6037596697465,-12.6327838948181,
118.884390644637)) ;
#154777 = CARTESIAN_POINT('Ctrl Pts',(-6.58728175649615,-12.5782837450973,
118.834201579071)) ;
#154778 = CARTESIAN_POINT('Ctrl Pts',(-6.51347790975495,-12.578283768441,
118.858432610641)) ;
#154779 = CARTESIAN_POINT('Ctrl Pts',(-6.43967406301373,-12.5782837917848,
118.882663642211)) ;
#154780 = CARTESIAN_POINT('Ctrl Pts',(-6.45615197626408,-12.6327839415056,
118.932852707777)) ;
#154781 = CARTESIAN_POINT('Ctrl Pts',(-6.53996330725217,-12.4610780963096,
119.152681494851)) ;
#154782 = CARTESIAN_POINT('Ctrl Pts',(-6.55134680489055,-12.5276451730564,
119.187353792041)) ;
#154783 = CARTESIAN_POINT('Ctrl Pts',(-6.62515065062138,-12.52764517241,119.163122757393)) ;
#154784 = CARTESIAN_POINT('Ctrl Pts',(-6.6989544963522,-12.5276451717636,
119.138891722746)) ;
#154785 = CARTESIAN_POINT('Ctrl Pts',(-6.68757099871382,-12.4610780950169,
119.104219425556)) ;
#154786 = CARTESIAN_POINT('Ctrl Pts',(-6.67618750107543,-12.3945110182701,
119.069547128366)) ;
#154787 = CARTESIAN_POINT('Ctrl Pts',(-6.60238365534461,-12.3945110189165,
119.093778163013)) ;
#154788 = CARTESIAN_POINT('Ctrl Pts',(-6.52857980961378,-12.3945110195628,
119.11800919766)) ;
#154789 = CARTESIAN_POINT('Ctrl Pts',(-6.53996330725217,-12.4610780963096,
119.152681494851)) ;
#154790 = CARTESIAN_POINT('Ctrl Pts',(-6.63588982776904,-12.3578311300529,
119.409231710552)) ;
#154791 = CARTESIAN_POINT('Ctrl Pts',(-6.64132916621594,-12.431704833434,
119.425799058233)) ;
#154792 = CARTESIAN_POINT('Ctrl Pts',(-6.71513301565431,-12.4317048270663,
119.401568034878)) ;
#154793 = CARTESIAN_POINT('Ctrl Pts',(-6.78893686509269,-12.4317048206985,
119.377337011523)) ;
#154794 = CARTESIAN_POINT('Ctrl Pts',(-6.78349752664579,-12.3578311173174,
119.360769663843)) ;
#154795 = CARTESIAN_POINT('Ctrl Pts',(-6.7780581881989,-12.2839574139363,
119.344202316162)) ;
#154796 = CARTESIAN_POINT('Ctrl Pts',(-6.70425433876052,-12.283957420304,
119.368433339517)) ;
#154797 = CARTESIAN_POINT('Ctrl Pts',(-6.63045048932215,-12.2839574266718,
119.392664362872)) ;
#154798 = CARTESIAN_POINT('Ctrl Pts',(-6.63588982776904,-12.3578311300529,
119.409231710552)) ;
#154799 = CARTESIAN_POINT('Ctrl Pts',(-6.736259431342,-12.3309709098726,119.679683383479)) ;
#154800 = CARTESIAN_POINT('Ctrl Pts',(-6.73542828981625,-12.4068262743209,
119.677151860981)) ;
#154801 = CARTESIAN_POINT('Ctrl Pts',(-6.80923214114053,-12.4068262750749,
119.65292084337)) ;
#154802 = CARTESIAN_POINT('Ctrl Pts',(-6.88303599246479,-12.4068262758288,
119.62868982576)) ;
#154803 = CARTESIAN_POINT('Ctrl Pts',(-6.88386713399053,-12.3309709113806,
119.631221348258)) ;
#154804 = CARTESIAN_POINT('Ctrl Pts',(-6.88469827551626,-12.2551155469323,
119.633752870756)) ;
#154805 = CARTESIAN_POINT('Ctrl Pts',(-6.81089442419199,-12.2551155461783,
119.657983888367)) ;
#154806 = CARTESIAN_POINT('Ctrl Pts',(-6.73709057286772,-12.2551155454244,
119.682214905978)) ;
#154807 = CARTESIAN_POINT('Ctrl Pts',(-6.736259431342,-12.3309709098726,119.679683383479)) ;
#154808 = CARTESIAN_POINT('Ctrl Pts',(-6.83652100223137,-12.3817310335918,
119.949488204916)) ;
#154809 = CARTESIAN_POINT('Ctrl Pts',(-6.82942443523005,-12.4541523823842,
119.927873207533)) ;
#154810 = CARTESIAN_POINT('Ctrl Pts',(-6.90322828907729,-12.4541523921254,
119.903642197606)) ;
#154811 = CARTESIAN_POINT('Ctrl Pts',(-6.97703214292451,-12.4541524018665,
119.87941118768)) ;
#154812 = CARTESIAN_POINT('Ctrl Pts',(-6.98412870992583,-12.3817310530741,
119.901026185064)) ;
#154813 = CARTESIAN_POINT('Ctrl Pts',(-6.99122527692713,-12.3093097042818,
119.922641182447)) ;
#154814 = CARTESIAN_POINT('Ctrl Pts',(-6.9174214230799,-12.3093096945406,
119.946872192373)) ;
#154815 = CARTESIAN_POINT('Ctrl Pts',(-6.84361756923268,-12.3093096847995,
119.971103202299)) ;
#154816 = CARTESIAN_POINT('Ctrl Pts',(-6.83652100223137,-12.3817310335918,
119.949488204916)) ;
#154817 = CARTESIAN_POINT('Ctrl Pts',(-6.92897537929249,-12.5067458714326,
120.195657155914)) ;
#154818 = CARTESIAN_POINT('Ctrl Pts',(-6.91614658582664,-12.5705432422448,
120.15658272177)) ;
#154819 = CARTESIAN_POINT('Ctrl Pts',(-6.98995044064887,-12.57054326527,120.132351714814)) ;
#154820 = CARTESIAN_POINT('Ctrl Pts',(-7.06375429547111,-12.5705432882951,
120.108120707857)) ;
#154821 = CARTESIAN_POINT('Ctrl Pts',(-7.07658308893695,-12.5067459174828,
120.147195142002)) ;
#154822 = CARTESIAN_POINT('Ctrl Pts',(-7.08941188240279,-12.4429485466705,
120.186269576146)) ;
#154823 = CARTESIAN_POINT('Ctrl Pts',(-7.01560802758057,-12.4429485236454,
120.210500583102)) ;
#154824 = CARTESIAN_POINT('Ctrl Pts',(-6.94180417275833,-12.4429485006203,
120.234731590059)) ;
#154825 = CARTESIAN_POINT('Ctrl Pts',(-6.92897537929249,-12.5067458714326,
120.195657155914)) ;
#154826 = CARTESIAN_POINT('Ctrl Pts',(-7.00828982195215,-12.6971218835384,
120.401748881771)) ;
#154827 = CARTESIAN_POINT('Ctrl Pts',(-6.99063912619378,-12.7477196021645,
120.347987711428)) ;
#154828 = CARTESIAN_POINT('Ctrl Pts',(-7.06444298055982,-12.7477196406968,
120.323756703082)) ;
#154829 = CARTESIAN_POINT('Ctrl Pts',(-7.13824683492587,-12.7477196792291,
120.299525694736)) ;
#154830 = CARTESIAN_POINT('Ctrl Pts',(-7.15589753068423,-12.697121960603,
120.353286865079)) ;
#154831 = CARTESIAN_POINT('Ctrl Pts',(-7.17354822644261,-12.646524241977,
120.407048035422)) ;
#154832 = CARTESIAN_POINT('Ctrl Pts',(-7.09974437207656,-12.6465242034447,
120.431279043767)) ;
#154833 = CARTESIAN_POINT('Ctrl Pts',(-7.02594051771052,-12.6465241649123,
120.455510052113)) ;
#154834 = CARTESIAN_POINT('Ctrl Pts',(-7.00828982195215,-12.6971218835384,
120.401748881771)) ;
#154835 = CARTESIAN_POINT('Ctrl Pts',(-7.06933695913004,-12.9391053860727,
120.552223222998)) ;
#154836 = CARTESIAN_POINT('Ctrl Pts',(-7.04813238576582,-12.9728813246928,
120.48763751505)) ;
#154837 = CARTESIAN_POINT('Ctrl Pts',(-7.1219362377198,-12.9728813789312,
120.463406499357)) ;
#154838 = CARTESIAN_POINT('Ctrl Pts',(-7.19574008967378,-12.9728814331696,
120.439175483665)) ;
#154839 = CARTESIAN_POINT('Ctrl Pts',(-7.21694466303801,-12.9391054945495,
120.503761191613)) ;
#154840 = CARTESIAN_POINT('Ctrl Pts',(-7.23814923640224,-12.9053295559293,
120.568346899561)) ;
#154841 = CARTESIAN_POINT('Ctrl Pts',(-7.16434538444827,-12.9053295016909,
120.592577915254)) ;
#154842 = CARTESIAN_POINT('Ctrl Pts',(-7.09054153249427,-12.9053294474525,
120.616808930946)) ;
#154843 = CARTESIAN_POINT('Ctrl Pts',(-7.06933695913004,-12.9391053860727,
120.552223222998)) ;
#154844 = CARTESIAN_POINT('Ctrl Pts',(-7.10853205803656,-13.2152764852227,
120.63614997259)) ;
#154845 = CARTESIAN_POINT('Ctrl Pts',(-7.08529393427628,-13.2298195844166,
120.565370398405)) ;
#154846 = CARTESIAN_POINT('Ctrl Pts',(-7.1590977818874,-13.2298196519975,
120.541139369485)) ;
#154847 = CARTESIAN_POINT('Ctrl Pts',(-7.2329016294985,-13.2298197195784,
120.516908340565)) ;
#154848 = CARTESIAN_POINT('Ctrl Pts',(-7.25613975325877,-13.2152766203844,
120.587687914749)) ;
#154849 = CARTESIAN_POINT('Ctrl Pts',(-7.27937787701905,-13.2007335211905,
120.658467488933)) ;
#154850 = CARTESIAN_POINT('Ctrl Pts',(-7.20557402940794,-13.2007334536096,
120.682698517854)) ;
#154851 = CARTESIAN_POINT('Ctrl Pts',(-7.13177018179683,-13.2007333860287,
120.706929546774)) ;
#154852 = CARTESIAN_POINT('Ctrl Pts',(-7.10853205803656,-13.2152764852227,
120.63614997259)) ;
#154853 = CARTESIAN_POINT('Ctrl Pts',(-7.12391162690117,-13.505784356226,
120.64756404441)) ;
#154854 = CARTESIAN_POINT('Ctrl Pts',(-7.10029921937121,-13.5000660445819,
120.5756444624)) ;
#154855 = CARTESIAN_POINT('Ctrl Pts',(-7.17410306107907,-13.5000661208921,
120.5514134155)) ;
#154856 = CARTESIAN_POINT('Ctrl Pts',(-7.24790690278691,-13.5000661972022,
120.527182368599)) ;
#154857 = CARTESIAN_POINT('Ctrl Pts',(-7.27151931031687,-13.5057845088464,
120.599101950609)) ;
#154858 = CARTESIAN_POINT('Ctrl Pts',(-7.29513171784683,-13.5115028204905,
120.671021532619)) ;
#154859 = CARTESIAN_POINT('Ctrl Pts',(-7.22132787613898,-13.5115027441803,
120.69525257952)) ;
#154860 = CARTESIAN_POINT('Ctrl Pts',(-7.14752403443112,-13.5115026678702,
120.719483626421)) ;
#154861 = CARTESIAN_POINT('Ctrl Pts',(-7.12391162690117,-13.505784356226,
120.64756404441)) ;
#154862 = CARTESIAN_POINT('Ctrl Pts',(-7.11491785946518,-13.7916119971123,
120.584527953854)) ;
#154863 = CARTESIAN_POINT('Ctrl Pts',(-7.09263642037673,-13.7659297998844,
120.516662287132)) ;
#154864 = CARTESIAN_POINT('Ctrl Pts',(-7.16644025484466,-13.7659298799449,
120.492431218179)) ;
#154865 = CARTESIAN_POINT('Ctrl Pts',(-7.2402440893126,-13.7659299600053,
120.468200149227)) ;
#154866 = CARTESIAN_POINT('Ctrl Pts',(-7.26252552840107,-13.7916121572332,
120.53606581595)) ;
#154867 = CARTESIAN_POINT('Ctrl Pts',(-7.28480696748951,-13.817294354461,
120.603931482673)) ;
#154868 = CARTESIAN_POINT('Ctrl Pts',(-7.21100313302158,-13.8172942744006,
120.628162551625)) ;
#154869 = CARTESIAN_POINT('Ctrl Pts',(-7.13719929855364,-13.8172941943401,
120.652393620577)) ;
#154870 = CARTESIAN_POINT('Ctrl Pts',(-7.11491785946518,-13.7916119971123,
120.584527953854)) ;
#154871 = CARTESIAN_POINT('Ctrl Pts',(-7.08327931847018,-14.0480477215918,
120.452871020505)) ;
#154872 = CARTESIAN_POINT('Ctrl Pts',(-7.06390476968655,-14.00442476396,120.393859272724)) ;
#154873 = CARTESIAN_POINT('Ctrl Pts',(-7.13770859691392,-14.0044248376781,
120.369628181718)) ;
#154874 = CARTESIAN_POINT('Ctrl Pts',(-7.21151242414129,-14.0044249113963,
120.345397090713)) ;
#154875 = CARTESIAN_POINT('Ctrl Pts',(-7.23088697292491,-14.0480478690281,
120.404408838494)) ;
#154876 = CARTESIAN_POINT('Ctrl Pts',(-7.25026152170854,-14.0916708266599,
120.463420586275)) ;
#154877 = CARTESIAN_POINT('Ctrl Pts',(-7.17645769448117,-14.0916707529417,
120.48765167728)) ;
#154878 = CARTESIAN_POINT('Ctrl Pts',(-7.10265386725381,-14.0916706792236,
120.511882768286)) ;
#154879 = CARTESIAN_POINT('Ctrl Pts',(-7.08327931847018,-14.0480477215918,
120.452871020505)) ;
#154880 = CARTESIAN_POINT('Ctrl Pts',(-7.03177476396055,-14.2608003622883,
120.260526319525)) ;
#154881 = CARTESIAN_POINT('Ctrl Pts',(-7.01670175571782,-14.2022602348381,
120.214616370291)) ;
#154882 = CARTESIAN_POINT('Ctrl Pts',(-7.09050557606073,-14.2022602957698,
120.190385258316)) ;
#154883 = CARTESIAN_POINT('Ctrl Pts',(-7.16430939640363,-14.2022603567015,
120.166154146341)) ;
#154884 = CARTESIAN_POINT('Ctrl Pts',(-7.17938240464634,-14.2608004841518,
120.212064095575)) ;
#154885 = CARTESIAN_POINT('Ctrl Pts',(-7.19445541288906,-14.319340611602,
120.25797404481)) ;
#154886 = CARTESIAN_POINT('Ctrl Pts',(-7.12065159254616,-14.3193405506703,
120.282205156785)) ;
#154887 = CARTESIAN_POINT('Ctrl Pts',(-7.04684777220326,-14.3193404897386,
120.306436268759)) ;
#154888 = CARTESIAN_POINT('Ctrl Pts',(-7.03177476396055,-14.2608003622883,
120.260526319525)) ;
#154889 = CARTESIAN_POINT('Ctrl Pts',(-6.96488777055259,-14.4130997833176,
120.021344897526)) ;
#154890 = CARTESIAN_POINT('Ctrl Pts',(-6.9551961334502,-14.3438411557226,
119.991825736593)) ;
#154891 = CARTESIAN_POINT('Ctrl Pts',(-7.02899994823942,-14.3438411966561,
119.967594607703)) ;
#154892 = CARTESIAN_POINT('Ctrl Pts',(-7.10280376302866,-14.3438412375897,
119.943363478813)) ;
#154893 = CARTESIAN_POINT('Ctrl Pts',(-7.11249540013105,-14.4130998651847,
119.972882639745)) ;
#154894 = CARTESIAN_POINT('Ctrl Pts',(-7.12218703723345,-14.4823584927798,
120.002401800678)) ;
#154895 = CARTESIAN_POINT('Ctrl Pts',(-7.04838322244423,-14.4823584518462,
120.026632929568)) ;
#154896 = CARTESIAN_POINT('Ctrl Pts',(-6.974579407655,-14.4823584109127,120.050864058458)) ;
#154897 = CARTESIAN_POINT('Ctrl Pts',(-6.96488777055259,-14.4130997833176,
120.021344897526)) ;
#154898 = CARTESIAN_POINT('Ctrl Pts',(-6.88794749547868,-14.494276858583,
119.751438472986)) ;
#154899 = CARTESIAN_POINT('Ctrl Pts',(-6.88434901109577,-14.419248986888,
119.740478072188)) ;
#154900 = CARTESIAN_POINT('Ctrl Pts',(-6.95815282228635,-14.4192490024428,
119.716246932336)) ;
#154901 = CARTESIAN_POINT('Ctrl Pts',(-7.03195663347692,-14.4192490179976,
119.692015792485)) ;
#154902 = CARTESIAN_POINT('Ctrl Pts',(-7.03555511785984,-14.4942768896926,
119.702976193283)) ;
#154903 = CARTESIAN_POINT('Ctrl Pts',(-7.03915360224275,-14.5693047613875,
119.713936594082)) ;
#154904 = CARTESIAN_POINT('Ctrl Pts',(-6.96534979105218,-14.5693047458327,
119.738167733933)) ;
#154905 = CARTESIAN_POINT('Ctrl Pts',(-6.8915459798616,-14.569304730278,119.762398873784)) ;
#154906 = CARTESIAN_POINT('Ctrl Pts',(-6.88794749547868,-14.494276858583,
119.751438472986)) ;
#154907 = CARTESIAN_POINT('Ctrl Pts',(-6.80764424999997,-14.4979516536895,
119.471388070987)) ;
#154908 = CARTESIAN_POINT('Ctrl Pts',(-6.81038065083614,-14.4225568687656,
119.479722708482)) ;
#154909 = CARTESIAN_POINT('Ctrl Pts',(-6.88418446115919,-14.4225568559479,
119.455491565989)) ;
#154910 = CARTESIAN_POINT('Ctrl Pts',(-6.95798827148224,-14.4225568431301,
119.431260423495)) ;
#154911 = CARTESIAN_POINT('Ctrl Pts',(-6.9552518706461,-14.497951628054,119.422925786)) ;
#154912 = CARTESIAN_POINT('Ctrl Pts',(-6.95251546980995,-14.5733464129779,
119.414591148505)) ;
#154913 = CARTESIAN_POINT('Ctrl Pts',(-6.87871165948689,-14.5733464257956,
119.438822290999)) ;
#154914 = CARTESIAN_POINT('Ctrl Pts',(-6.80490784916383,-14.5733464386134,
119.463053433492)) ;
#154915 = CARTESIAN_POINT('Ctrl Pts',(-6.80764424999997,-14.4979516536895,
119.471388070987)) ;
#154916 = CARTESIAN_POINT('Ctrl Pts',(-6.73039780792071,-14.4245500702158,
119.200701305624)) ;
#154917 = CARTESIAN_POINT('Ctrl Pts',(-6.73926391619148,-14.3541688694618,
119.227706042965)) ;
#154918 = CARTESIAN_POINT('Ctrl Pts',(-6.81306772839461,-14.3541688284501,
119.203474906198)) ;
#154919 = CARTESIAN_POINT('Ctrl Pts',(-6.88687154059774,-14.3541687874384,
119.179243769431)) ;
#154920 = CARTESIAN_POINT('Ctrl Pts',(-6.87800543232696,-14.4245499881925,
119.15223903209)) ;
#154921 = CARTESIAN_POINT('Ctrl Pts',(-6.86913932405619,-14.4949311889465,
119.125234294749)) ;
#154922 = CARTESIAN_POINT('Ctrl Pts',(-6.79533551185306,-14.4949312299582,
119.149465431516)) ;
#154923 = CARTESIAN_POINT('Ctrl Pts',(-6.72153169964993,-14.4949312709699,
119.173696568283)) ;
#154924 = CARTESIAN_POINT('Ctrl Pts',(-6.73039780792071,-14.4245500702158,
119.200701305624)) ;
#154925 = CARTESIAN_POINT('Ctrl Pts',(-6.66228119436863,-14.27912481409,118.957786696)) ;
#154926 = CARTESIAN_POINT('Ctrl Pts',(-6.67664941802772,-14.2187925848184,
119.001549989056)) ;
#154927 = CARTESIAN_POINT('Ctrl Pts',(-6.75045323468118,-14.2187925185092,
118.977318865844)) ;
#154928 = CARTESIAN_POINT('Ctrl Pts',(-6.82425705133464,-14.2187924522,118.953087742632)) ;
#154929 = CARTESIAN_POINT('Ctrl Pts',(-6.80988882767555,-14.2791246814716,
118.909324449576)) ;
#154930 = CARTESIAN_POINT('Ctrl Pts',(-6.79552060401646,-14.3394569107431,
118.865561156519)) ;
#154931 = CARTESIAN_POINT('Ctrl Pts',(-6.72171678736299,-14.3394569770523,
118.889792279731)) ;
#154932 = CARTESIAN_POINT('Ctrl Pts',(-6.64791297070954,-14.3394570433615,
118.914023402943)) ;
#154933 = CARTESIAN_POINT('Ctrl Pts',(-6.66228119436863,-14.27912481409,118.957786696)) ;
#154934 = CARTESIAN_POINT('Ctrl Pts',(-6.60891474419106,-14.0717728276009,
118.75974735927)) ;
#154935 = CARTESIAN_POINT('Ctrl Pts',(-6.62776457270004,-14.0258274816855,
118.817160897579)) ;
#154936 = CARTESIAN_POINT('Ctrl Pts',(-6.70156839599648,-14.0258273955752,
118.7929297946)) ;
#154937 = CARTESIAN_POINT('Ctrl Pts',(-6.7753722192929,-14.025827309465,118.768698691621)) ;
#154938 = CARTESIAN_POINT('Ctrl Pts',(-6.7565223907839,-14.0717726553804,
118.711285153312)) ;
#154939 = CARTESIAN_POINT('Ctrl Pts',(-6.73767256227492,-14.1177180012958,
118.653871615004)) ;
#154940 = CARTESIAN_POINT('Ctrl Pts',(-6.66386873897849,-14.1177180874061,
118.678102717983)) ;
#154941 = CARTESIAN_POINT('Ctrl Pts',(-6.59006491568207,-14.1177181735163,
118.702333820961)) ;
#154942 = CARTESIAN_POINT('Ctrl Pts',(-6.60891474419106,-14.0717728276009,
118.75974735927)) ;
#154943 = CARTESIAN_POINT('Ctrl Pts',(-6.57501586876472,-13.8168218187551,
118.62092447149)) ;
#154944 = CARTESIAN_POINT('Ctrl Pts',(-6.59699661459439,-13.7886075890761,
118.687874278739)) ;
#154945 = CARTESIAN_POINT('Ctrl Pts',(-6.67080044605695,-13.7886074911404,
118.663643200633)) ;
#154946 = CARTESIAN_POINT('Ctrl Pts',(-6.7446042775195,-13.7886073932047,
118.639412122527)) ;
#154947 = CARTESIAN_POINT('Ctrl Pts',(-6.72262353168983,-13.8168216228837,
118.572462315278)) ;
#154948 = CARTESIAN_POINT('Ctrl Pts',(-6.70064278586015,-13.8450358525627,
118.505512508029)) ;
#154949 = CARTESIAN_POINT('Ctrl Pts',(-6.6268389543976,-13.8450359504984,
118.529743586135)) ;
#154950 = CARTESIAN_POINT('Ctrl Pts',(-6.55303512293504,-13.8450360484341,
118.553974664241)) ;
#154951 = CARTESIAN_POINT('Ctrl Pts',(-6.57501586876472,-13.8168218187551,
118.62092447149)) ;
#154952 = CARTESIAN_POINT('Ctrl Pts',(-6.56385556381707,-13.535324035321,
118.551622243501)) ;
#154953 = CARTESIAN_POINT('Ctrl Pts',(-6.58737882351097,-13.5267213387171,
118.623270299046)) ;
#154954 = CARTESIAN_POINT('Ctrl Pts',(-6.6611826635699,-13.5267212367711,
118.599039247123)) ;
#154955 = CARTESIAN_POINT('Ctrl Pts',(-6.73498650362882,-13.526721134825,
118.5748081952)) ;
#154956 = CARTESIAN_POINT('Ctrl Pts',(-6.71146324393492,-13.5353238314288,
118.503160139655)) ;
#154957 = CARTESIAN_POINT('Ctrl Pts',(-6.68793998424103,-13.5439265280327,
118.43151208411)) ;
#154958 = CARTESIAN_POINT('Ctrl Pts',(-6.61413614418211,-13.5439266299788,
118.455743136033)) ;
#154959 = CARTESIAN_POINT('Ctrl Pts',(-6.54033230412318,-13.5439267319248,
118.479974187956)) ;
#154960 = CARTESIAN_POINT('Ctrl Pts',(-6.56385556381707,-13.535324035321,
118.551622243501)) ;
#154961 = CARTESIAN_POINT('Ctrl Pts',(-6.57670200274292,-13.2440746292406,
118.55526577413)) ;
#154962 = CARTESIAN_POINT('Ctrl Pts',(-6.60009785377443,-13.2557932048074,
118.626525763366)) ;
#154963 = CARTESIAN_POINT('Ctrl Pts',(-6.67390170224611,-13.2557931077727,
118.602294737067)) ;
#154964 = CARTESIAN_POINT('Ctrl Pts',(-6.74770555071778,-13.2557930107381,
118.578063710768)) ;
#154965 = CARTESIAN_POINT('Ctrl Pts',(-6.72430969968627,-13.2440744351713,
118.506803721532)) ;
#154966 = CARTESIAN_POINT('Ctrl Pts',(-6.70091384865477,-13.2323558596045,
118.435543732295)) ;
#154967 = CARTESIAN_POINT('Ctrl Pts',(-6.62711000018308,-13.2323559566392,
118.459774758594)) ;
#154968 = CARTESIAN_POINT('Ctrl Pts',(-6.55330615171141,-13.2323560536738,
118.484005784893)) ;
#154969 = CARTESIAN_POINT('Ctrl Pts',(-6.57670200274292,-13.2440746292406,
118.55526577413)) ;
#154970 = CARTESIAN_POINT('Ctrl Pts',(-6.61375984173444,-12.9648031401168,
118.632582291307)) ;
#154971 = CARTESIAN_POINT('Ctrl Pts',(-6.63533936183605,-12.9960374765742,
118.698310029483)) ;
#154972 = CARTESIAN_POINT('Ctrl Pts',(-6.7091432174225,-12.9960373926029,
118.674079024855)) ;
#154973 = CARTESIAN_POINT('Ctrl Pts',(-6.78294707300893,-12.9960373086315,
118.649848020226)) ;
#154974 = CARTESIAN_POINT('Ctrl Pts',(-6.76136755290732,-12.964802972174,
118.58412028205)) ;
#154975 = CARTESIAN_POINT('Ctrl Pts',(-6.73978803280568,-12.9335686357166,
118.518392543873)) ;
#154976 = CARTESIAN_POINT('Ctrl Pts',(-6.66598417721924,-12.933568719688,
118.542623548502)) ;
#154977 = CARTESIAN_POINT('Ctrl Pts',(-6.5921803216328,-12.9335688036593,
118.56685455313)) ;
#154978 = CARTESIAN_POINT('Ctrl Pts',(-6.61375984173444,-12.9648031401168,
118.632582291307)) ;
#154979 = CARTESIAN_POINT('Ctrl Pts',(-6.67258342631208,-12.7194345507308,
118.776404079392)) ;
#154980 = CARTESIAN_POINT('Ctrl Pts',(-6.69081973876519,-12.7678470581872,
118.831948946394)) ;
#154981 = CARTESIAN_POINT('Ctrl Pts',(-6.76462359980993,-12.7678469916176,
118.80771795839)) ;
#154982 = CARTESIAN_POINT('Ctrl Pts',(-6.83842746085466,-12.767846925048,
118.783486970387)) ;
#154983 = CARTESIAN_POINT('Ctrl Pts',(-6.82019114840154,-12.7194344175916,
118.727942103385)) ;
#154984 = CARTESIAN_POINT('Ctrl Pts',(-6.80195483594844,-12.6710219101352,
118.672397236382)) ;
#154985 = CARTESIAN_POINT('Ctrl Pts',(-6.72815097490371,-12.6710219767048,
118.696628224386)) ;
#154986 = CARTESIAN_POINT('Ctrl Pts',(-6.65434711385897,-12.6710220432744,
118.720859212389)) ;
#154987 = CARTESIAN_POINT('Ctrl Pts',(-6.67258342631208,-12.7194345507308,
118.776404079392)) ;
#154988 = CARTESIAN_POINT('Ctrl Pts',(-6.75039015970557,-12.5228537207888,
118.97784552327)) ;
#154989 = CARTESIAN_POINT('Ctrl Pts',(-6.76395720799441,-12.5850644655665,
119.019168564866)) ;
#154990 = CARTESIAN_POINT('Ctrl Pts',(-6.83776107202866,-12.5850644207041,
118.994937585968)) ;
#154991 = CARTESIAN_POINT('Ctrl Pts',(-6.91156493606291,-12.5850643758416,
118.97070660707)) ;
#154992 = CARTESIAN_POINT('Ctrl Pts',(-6.89799788777407,-12.522853631064,
118.929383565474)) ;
#154993 = CARTESIAN_POINT('Ctrl Pts',(-6.88443083948523,-12.4606428862864,
118.888060523877)) ;
#154994 = CARTESIAN_POINT('Ctrl Pts',(-6.81062697545099,-12.4606429311488,
118.912291502775)) ;
#154995 = CARTESIAN_POINT('Ctrl Pts',(-6.73682311141673,-12.4606429760112,
118.936522481673)) ;
#154996 = CARTESIAN_POINT('Ctrl Pts',(-6.75039015970557,-12.5228537207888,
118.97784552327)) ;
#154997 = CARTESIAN_POINT('Ctrl Pts',(-6.84171874623714,-12.3910219564108,
119.220611387595)) ;
#154998 = CARTESIAN_POINT('Ctrl Pts',(-6.84966241347004,-12.4625310700348,
119.244806517688)) ;
#154999 = CARTESIAN_POINT('Ctrl Pts',(-6.92346627839763,-12.4625310467126,
119.220575541511)) ;
#155000 = CARTESIAN_POINT('Ctrl Pts',(-6.99727014332522,-12.4625310233905,
119.196344565334)) ;
#155001 = CARTESIAN_POINT('Ctrl Pts',(-6.98932647609232,-12.3910219097665,
119.172149435241)) ;
#155002 = CARTESIAN_POINT('Ctrl Pts',(-6.98138280885941,-12.3195127961425,
119.147954305148)) ;
#155003 = CARTESIAN_POINT('Ctrl Pts',(-6.90757894393183,-12.3195128194647,
119.172185281325)) ;
#155004 = CARTESIAN_POINT('Ctrl Pts',(-6.83377507900424,-12.3195128427868,
119.196416257502)) ;
#155005 = CARTESIAN_POINT('Ctrl Pts',(-6.84171874623714,-12.3910219564108,
119.220611387595)) ;
#155006 = CARTESIAN_POINT('Ctrl Pts',(-6.94152390518599,-12.3324946198483,
119.489024176868)) ;
#155007 = CARTESIAN_POINT('Ctrl Pts',(-6.94324743147265,-12.408198760168,
119.494273761078)) ;
#155008 = CARTESIAN_POINT('Ctrl Pts',(-7.01705129472505,-12.4081987566325,
119.470042779798)) ;
#155009 = CARTESIAN_POINT('Ctrl Pts',(-7.09085515797744,-12.4081987530971,
119.445811798519)) ;
#155010 = CARTESIAN_POINT('Ctrl Pts',(-7.08913163169077,-12.3324946127775,
119.440562214309)) ;
#155011 = CARTESIAN_POINT('Ctrl Pts',(-7.08740810540409,-12.2567904724578,
119.435312630098)) ;
#155012 = CARTESIAN_POINT('Ctrl Pts',(-7.01360424215171,-12.2567904759932,
119.459543611378)) ;
#155013 = CARTESIAN_POINT('Ctrl Pts',(-6.93980037889931,-12.2567904795287,
119.483774592657)) ;
#155014 = CARTESIAN_POINT('Ctrl Pts',(-6.94152390518599,-12.3324946198483,
119.489024176868)) ;
#155015 = CARTESIAN_POINT('Ctrl Pts',(-7.04230587420137,-12.3517941049946,
119.760653819778)) ;
#155016 = CARTESIAN_POINT('Ctrl Pts',(-7.03772653183689,-12.426265134033,
119.746705882901)) ;
#155017 = CARTESIAN_POINT('Ctrl Pts',(-7.11153039244817,-12.426265145997,
119.722474893577)) ;
#155018 = CARTESIAN_POINT('Ctrl Pts',(-7.18533425305945,-12.4262651579609,
119.698243904253)) ;
#155019 = CARTESIAN_POINT('Ctrl Pts',(-7.18991359542393,-12.3517941289225,
119.71219184113)) ;
#155020 = CARTESIAN_POINT('Ctrl Pts',(-7.19449293778842,-12.2773230998841,
119.726139778008)) ;
#155021 = CARTESIAN_POINT('Ctrl Pts',(-7.12068907717713,-12.2773230879201,
119.750370767332)) ;
#155022 = CARTESIAN_POINT('Ctrl Pts',(-7.04688521656585,-12.2773230759562,
119.774601756655)) ;
#155023 = CARTESIAN_POINT('Ctrl Pts',(-7.04230587420137,-12.3517941049946,
119.760653819778)) ;
#155024 = CARTESIAN_POINT('Ctrl Pts',(-7.13886766534031,-12.4476532719571,
120.019204540318)) ;
#155025 = CARTESIAN_POINT('Ctrl Pts',(-7.12827513854447,-12.5155445566341,
119.986941413701)) ;
#155026 = CARTESIAN_POINT('Ctrl Pts',(-7.2020789948579,-12.5155445785794,
119.962710411286)) ;
#155027 = CARTESIAN_POINT('Ctrl Pts',(-7.27588285117132,-12.5155446005247,
119.938479408872)) ;
#155028 = CARTESIAN_POINT('Ctrl Pts',(-7.28647537796717,-12.4476533158478,
119.970742535489)) ;
#155029 = CARTESIAN_POINT('Ctrl Pts',(-7.297067904763,-12.3797620311708,120.003005662107)) ;
#155030 = CARTESIAN_POINT('Ctrl Pts',(-7.22326404844958,-12.3797620092255,
120.027236664521)) ;
#155031 = CARTESIAN_POINT('Ctrl Pts',(-7.14946019213615,-12.3797619872802,
120.051467666936)) ;
#155032 = CARTESIAN_POINT('Ctrl Pts',(-7.13886766534031,-12.4476532719571,
120.019204540318)) ;
#155033 = CARTESIAN_POINT('Ctrl Pts',(-7.22405843886179,-12.6128436094032,
120.24325293471)) ;
#155034 = CARTESIAN_POINT('Ctrl Pts',(-7.20823477368357,-12.6693038141033,
120.195056604459)) ;
#155035 = CARTESIAN_POINT('Ctrl Pts',(-7.28203862582447,-12.669303840492,
120.170825589336)) ;
#155036 = CARTESIAN_POINT('Ctrl Pts',(-7.35584247796537,-12.6693038668807,
120.146594574213)) ;
#155037 = CARTESIAN_POINT('Ctrl Pts',(-7.3716661431436,-12.6128436621805,
120.194790904463)) ;
#155038 = CARTESIAN_POINT('Ctrl Pts',(-7.38748980832182,-12.5563834574804,
120.242987234714)) ;
#155039 = CARTESIAN_POINT('Ctrl Pts',(-7.31368595618093,-12.5563834310917,
120.267218249837)) ;
#155040 = CARTESIAN_POINT('Ctrl Pts',(-7.23988210404002,-12.556383404703,
120.29144926496)) ;
#155041 = CARTESIAN_POINT('Ctrl Pts',(-7.22405843886179,-12.6128436094032,
120.24325293471)) ;
#155042 = CARTESIAN_POINT('Ctrl Pts',(-7.29301191518833,-12.8354722898284,
120.417835047233)) ;
#155043 = CARTESIAN_POINT('Ctrl Pts',(-7.27308310321733,-12.8764735343339,
120.357135102054)) ;
#155044 = CARTESIAN_POINT('Ctrl Pts',(-7.34688695143518,-12.8764735602594,
120.332904074982)) ;
#155045 = CARTESIAN_POINT('Ctrl Pts',(-7.42069079965303,-12.8764735861849,
120.308673047909)) ;
#155046 = CARTESIAN_POINT('Ctrl Pts',(-7.44061961162404,-12.8354723416794,
120.369372993088)) ;
#155047 = CARTESIAN_POINT('Ctrl Pts',(-7.46054842359504,-12.794471097174,
120.430072938267)) ;
#155048 = CARTESIAN_POINT('Ctrl Pts',(-7.38674457537718,-12.7944710712485,
120.454303965339)) ;
#155049 = CARTESIAN_POINT('Ctrl Pts',(-7.31294072715933,-12.794471045323,
120.478534992412)) ;
#155050 = CARTESIAN_POINT('Ctrl Pts',(-7.29301191518833,-12.8354722898284,
120.417835047233)) ;
#155051 = CARTESIAN_POINT('Ctrl Pts',(-7.34159724157024,-13.101408894203,
120.530187095211)) ;
#155052 = CARTESIAN_POINT('Ctrl Pts',(-7.31898299520702,-13.1239035578376,
120.461307749982)) ;
#155053 = CARTESIAN_POINT('Ctrl Pts',(-7.39278684027698,-13.1239035777503,
120.437076713321)) ;
#155054 = CARTESIAN_POINT('Ctrl Pts',(-7.46659068534692,-13.1239035976629,
120.412845676661)) ;
#155055 = CARTESIAN_POINT('Ctrl Pts',(-7.48920493171014,-13.1014089340283,
120.48172502189)) ;
#155056 = CARTESIAN_POINT('Ctrl Pts',(-7.51181917807333,-13.0789142703937,
120.550604367119)) ;
#155057 = CARTESIAN_POINT('Ctrl Pts',(-7.43801533300339,-13.078914250481,
120.574835403779)) ;
#155058 = CARTESIAN_POINT('Ctrl Pts',(-7.36421148793344,-13.0789142305684,
120.59906644044)) ;
#155059 = CARTESIAN_POINT('Ctrl Pts',(-7.34159724157024,-13.101408894203,
120.530187095211)) ;
#155060 = CARTESIAN_POINT('Ctrl Pts',(-7.36657138807077,-13.3874022195482,
120.570964865022)) ;
#155061 = CARTESIAN_POINT('Ctrl Pts',(-7.34290959708444,-13.3899614744304,
120.498894867778)) ;
#155062 = CARTESIAN_POINT('Ctrl Pts',(-7.41671344046239,-13.389961489155,
120.474663825964)) ;
#155063 = CARTESIAN_POINT('Ctrl Pts',(-7.49051728384033,-13.3899615038795,
120.45043278415)) ;
#155064 = CARTESIAN_POINT('Ctrl Pts',(-7.51417907482665,-13.3874022489973,
120.522502781394)) ;
#155065 = CARTESIAN_POINT('Ctrl Pts',(-7.53784086581298,-13.384842994115,
120.594572778638)) ;
#155066 = CARTESIAN_POINT('Ctrl Pts',(-7.46403702243505,-13.3848429793905,
120.618803820452)) ;
#155067 = CARTESIAN_POINT('Ctrl Pts',(-7.3902331790571,-13.3848429646659,
120.643034862266)) ;
#155068 = CARTESIAN_POINT('Ctrl Pts',(-7.36657138807077,-13.3874022195482,
120.570964865022)) ;
#155069 = CARTESIAN_POINT('Ctrl Pts',(-7.36752626591963,-13.6768759171903,
120.538418289664)) ;
#155070 = CARTESIAN_POINT('Ctrl Pts',(-7.34449582013555,-13.6592264507691,
120.468271267912)) ;
#155071 = CARTESIAN_POINT('Ctrl Pts',(-7.41829966275664,-13.6592264585441,
120.444040223793)) ;
#155072 = CARTESIAN_POINT('Ctrl Pts',(-7.49210350537773,-13.6592264663191,
120.419809179674)) ;
#155073 = CARTESIAN_POINT('Ctrl Pts',(-7.51513395116179,-13.6768759327404,
120.489956201426)) ;
#155074 = CARTESIAN_POINT('Ctrl Pts',(-7.53816439694586,-13.6945253991617,
120.560103223178)) ;
#155075 = CARTESIAN_POINT('Ctrl Pts',(-7.46436055432477,-13.6945253913867,
120.584334267297)) ;
#155076 = CARTESIAN_POINT('Ctrl Pts',(-7.39055671170369,-13.6945253836116,
120.608565311417)) ;
#155077 = CARTESIAN_POINT('Ctrl Pts',(-7.36752626591963,-13.6768759171903,
120.538418289664)) ;
#155078 = CARTESIAN_POINT('Ctrl Pts',(-7.34470605061851,-13.948608493865,
120.433347699827)) ;
#155079 = CARTESIAN_POINT('Ctrl Pts',(-7.32397035086195,-13.9119580024122,
120.370190104105)) ;
#155080 = CARTESIAN_POINT('Ctrl Pts',(-7.39777419381241,-13.9119580041773,
120.345959060989)) ;
#155081 = CARTESIAN_POINT('Ctrl Pts',(-7.47157803676287,-13.9119580059424,
120.321728017873)) ;
#155082 = CARTESIAN_POINT('Ctrl Pts',(-7.49231373651943,-13.9486084973951,
120.384885613595)) ;
#155083 = CARTESIAN_POINT('Ctrl Pts',(-7.51304943627599,-13.9852589888479,
120.448043209317)) ;
#155084 = CARTESIAN_POINT('Ctrl Pts',(-7.43924559332553,-13.9852589870828,
120.472274252433)) ;
#155085 = CARTESIAN_POINT('Ctrl Pts',(-7.36544175037507,-13.9852589853178,
120.496505295549)) ;
#155086 = CARTESIAN_POINT('Ctrl Pts',(-7.34470605061851,-13.948608493865,
120.433347699827)) ;
#155087 = CARTESIAN_POINT('Ctrl Pts',(-7.30074221590675,-14.181257681225,
120.264014178484)) ;
#155088 = CARTESIAN_POINT('Ctrl Pts',(-7.28377855552149,-14.12830707033,120.212345606003)) ;
#155089 = CARTESIAN_POINT('Ctrl Pts',(-7.35758239915043,-14.1283070692883,
120.188114564954)) ;
#155090 = CARTESIAN_POINT('Ctrl Pts',(-7.43138624277937,-14.1283070682466,
120.163883523905)) ;
#155091 = CARTESIAN_POINT('Ctrl Pts',(-7.44834990316463,-14.1812576791416,
120.215552096385)) ;
#155092 = CARTESIAN_POINT('Ctrl Pts',(-7.46531356354989,-14.2342082900366,
120.267220668866)) ;
#155093 = CARTESIAN_POINT('Ctrl Pts',(-7.39150971992095,-14.2342082910783,
120.291451709916)) ;
#155094 = CARTESIAN_POINT('Ctrl Pts',(-7.31770587629201,-14.23420829212,120.315682750965)) ;
#155095 = CARTESIAN_POINT('Ctrl Pts',(-7.30074221590675,-14.181257681225,
120.264014178484)) ;
#155096 = CARTESIAN_POINT('Ctrl Pts',(-7.23958451504645,-14.3592650506284,
120.042343425265)) ;
#155097 = CARTESIAN_POINT('Ctrl Pts',(-7.22759862181639,-14.2938058183535,
120.005836328342)) ;
#155098 = CARTESIAN_POINT('Ctrl Pts',(-7.30140246605262,-14.2938058167003,
119.981605289143)) ;
#155099 = CARTESIAN_POINT('Ctrl Pts',(-7.37520631028883,-14.293805815047,
119.957374249943)) ;
#155100 = CARTESIAN_POINT('Ctrl Pts',(-7.38719220351889,-14.359265047322,
119.993881346865)) ;
#155101 = CARTESIAN_POINT('Ctrl Pts',(-7.39917809674894,-14.4247242795969,
120.030388443787)) ;
#155102 = CARTESIAN_POINT('Ctrl Pts',(-7.32537425251272,-14.4247242812501,
120.054619482987)) ;
#155103 = CARTESIAN_POINT('Ctrl Pts',(-7.2515704082765,-14.4247242829034,
120.078850522187)) ;
#155104 = CARTESIAN_POINT('Ctrl Pts',(-7.23958451504645,-14.3592650506284,
120.042343425265)) ;
#155105 = CARTESIAN_POINT('Ctrl Pts',(-7.16614529781219,-14.4703402370834,
119.783202402502)) ;
#155106 = CARTESIAN_POINT('Ctrl Pts',(-7.16000368885189,-14.3970277006435,
119.764496052493)) ;
#155107 = CARTESIAN_POINT('Ctrl Pts',(-7.23380753322604,-14.3970276999611,
119.740265013713)) ;
#155108 = CARTESIAN_POINT('Ctrl Pts',(-7.30761137760024,-14.3970276992787,
119.716033974934)) ;
#155109 = CARTESIAN_POINT('Ctrl Pts',(-7.31375298656054,-14.4703402357187,
119.734740324943)) ;
#155110 = CARTESIAN_POINT('Ctrl Pts',(-7.31989459552087,-14.5436527721586,
119.753446674952)) ;
#155111 = CARTESIAN_POINT('Ctrl Pts',(-7.24609075114669,-14.543652772841,
119.777677713732)) ;
#155112 = CARTESIAN_POINT('Ctrl Pts',(-7.17228690677252,-14.5436527735234,
119.801908752511)) ;
#155113 = CARTESIAN_POINT('Ctrl Pts',(-7.16614529781219,-14.4703402370834,
119.783202402502)) ;
#155114 = CARTESIAN_POINT('Ctrl Pts',(-7.08630537122041,-14.5059089260168,
119.504470384707)) ;
#155115 = CARTESIAN_POINT('Ctrl Pts',(-7.08646558971183,-14.4300045540626,
119.504958384369)) ;
#155116 = CARTESIAN_POINT('Ctrl Pts',(-7.16026943329858,-14.4300045543585,
119.480727343191)) ;
#155117 = CARTESIAN_POINT('Ctrl Pts',(-7.23407327688532,-14.4300045546544,
119.456496302013)) ;
#155118 = CARTESIAN_POINT('Ctrl Pts',(-7.2339130583939,-14.5059089266086,
119.456008302351)) ;
#155119 = CARTESIAN_POINT('Ctrl Pts',(-7.23375283990247,-14.5818132985628,
119.455520302688)) ;
#155120 = CARTESIAN_POINT('Ctrl Pts',(-7.15994899631572,-14.5818132982669,
119.479751343866)) ;
#155121 = CARTESIAN_POINT('Ctrl Pts',(-7.08614515272898,-14.581813297971,
119.503982385044)) ;
#155122 = CARTESIAN_POINT('Ctrl Pts',(-7.08630537122041,-14.5059089260168,
119.504470384707)) ;
#155123 = CARTESIAN_POINT('Ctrl Pts',(-7.00714711584661,-14.4635906108697,
119.22798980315)) ;
#155124 = CARTESIAN_POINT('Ctrl Pts',(-7.01356694457032,-14.3905302812958,
119.247543565668)) ;
#155125 = CARTESIAN_POINT('Ctrl Pts',(-7.08737078700817,-14.3905302808225,
119.22331252099)) ;
#155126 = CARTESIAN_POINT('Ctrl Pts',(-7.16117462944603,-14.3905302803492,
119.199081476313)) ;
#155127 = CARTESIAN_POINT('Ctrl Pts',(-7.15475480072232,-14.4635906099231,
119.179527713796)) ;
#155128 = CARTESIAN_POINT('Ctrl Pts',(-7.14833497199862,-14.536650939497,
119.159973951278)) ;
#155129 = CARTESIAN_POINT('Ctrl Pts',(-7.07453112956076,-14.5366509399703,
119.184204995956)) ;
#155130 = CARTESIAN_POINT('Ctrl Pts',(-7.0007272871229,-14.5366509404436,
119.208436040633)) ;
#155131 = CARTESIAN_POINT('Ctrl Pts',(-7.00714711584661,-14.4635906108697,
119.22798980315)) ;
#155132 = CARTESIAN_POINT('Ctrl Pts',(-6.9343979792678,-14.3462861335646,
118.970893409468)) ;
#155133 = CARTESIAN_POINT('Ctrl Pts',(-6.94664184382201,-14.2813098903358,
119.008186245531)) ;
#155134 = CARTESIAN_POINT('Ctrl Pts',(-7.02044568477505,-14.2813098862363,
118.983955196331)) ;
#155135 = CARTESIAN_POINT('Ctrl Pts',(-7.0942495257281,-14.2813098821367,
118.959724147132)) ;
#155136 = CARTESIAN_POINT('Ctrl Pts',(-7.0820056611739,-14.3462861253655,
118.922431311069)) ;
#155137 = CARTESIAN_POINT('Ctrl Pts',(-7.06976179661971,-14.4112623685942,
118.885138475006)) ;
#155138 = CARTESIAN_POINT('Ctrl Pts',(-6.99595795566666,-14.4112623726938,
118.909369524205)) ;
#155139 = CARTESIAN_POINT('Ctrl Pts',(-6.9221541147136,-14.4112623767934,
118.933600573405)) ;
#155140 = CARTESIAN_POINT('Ctrl Pts',(-6.9343979792678,-14.3462861335646,
118.970893409468)) ;
#155141 = CARTESIAN_POINT('Ctrl Pts',(-6.87439561306881,-14.1620807273187,
118.752616009014)) ;
#155142 = CARTESIAN_POINT('Ctrl Pts',(-6.8915819369104,-14.1098718676652,
118.804962778742)) ;
#155143 = CARTESIAN_POINT('Ctrl Pts',(-6.96538577675959,-14.1098718563613,
118.780731726181)) ;
#155144 = CARTESIAN_POINT('Ctrl Pts',(-7.03918961660877,-14.1098718450575,
118.756500673619)) ;
#155145 = CARTESIAN_POINT('Ctrl Pts',(-7.02200329276718,-14.162080704711,
118.70415390389)) ;
#155146 = CARTESIAN_POINT('Ctrl Pts',(-7.00481696892557,-14.2142895643646,
118.651807134161)) ;
#155147 = CARTESIAN_POINT('Ctrl Pts',(-6.9310131290764,-14.2142895756684,
118.676038186723)) ;
#155148 = CARTESIAN_POINT('Ctrl Pts',(-6.8572092892272,-14.2142895869723,
118.700269239285)) ;
#155149 = CARTESIAN_POINT('Ctrl Pts',(-6.87439561306881,-14.1620807273187,
118.752616009014)) ;
#155150 = CARTESIAN_POINT('Ctrl Pts',(-6.83231279792918,-13.9257450561724,
118.589088105333)) ;
#155151 = CARTESIAN_POINT('Ctrl Pts',(-6.85319376491815,-13.8899621379748,
118.652688162088)) ;
#155152 = CARTESIAN_POINT('Ctrl Pts',(-6.92699760485068,-13.8899621182589,
118.62845710978)) ;
#155153 = CARTESIAN_POINT('Ctrl Pts',(-7.0008014447832,-13.889962098543,118.604226057471)) ;
#155154 = CARTESIAN_POINT('Ctrl Pts',(-6.97992047779423,-13.9257450167406,
118.540626000717)) ;
#155155 = CARTESIAN_POINT('Ctrl Pts',(-6.95903951080526,-13.9615279349381,
118.477025943963)) ;
#155156 = CARTESIAN_POINT('Ctrl Pts',(-6.88523567087274,-13.961527954654,
118.501256996271)) ;
#155157 = CARTESIAN_POINT('Ctrl Pts',(-6.81143183094022,-13.9615279743699,
118.525488048579)) ;
#155158 = CARTESIAN_POINT('Ctrl Pts',(-6.83231279792918,-13.9257450561724,
118.589088105333)) ;
#155159 = CARTESIAN_POINT('Ctrl Pts',(-6.81152149947454,-13.6518932520307,
118.490235528419)) ;
#155160 = CARTESIAN_POINT('Ctrl Pts',(-6.83461955364127,-13.6351791904555,
118.560588475159)) ;
#155161 = CARTESIAN_POINT('Ctrl Pts',(-6.90842339470331,-13.6351791600229,
118.536357426292)) ;
#155162 = CARTESIAN_POINT('Ctrl Pts',(-6.98222723576535,-13.6351791295903,
118.512126377424)) ;
#155163 = CARTESIAN_POINT('Ctrl Pts',(-6.95912918159862,-13.6518931911655,
118.441773430683)) ;
#155164 = CARTESIAN_POINT('Ctrl Pts',(-6.93603112743188,-13.6686072527407,
118.371420483943)) ;
#155165 = CARTESIAN_POINT('Ctrl Pts',(-6.86222728636984,-13.6686072831733,
118.395651532811)) ;
#155166 = CARTESIAN_POINT('Ctrl Pts',(-6.78842344530779,-13.6686073136059,
118.419882581678)) ;
#155167 = CARTESIAN_POINT('Ctrl Pts',(-6.81152149947454,-13.6518932520307,
118.490235528419)) ;
#155168 = CARTESIAN_POINT('Ctrl Pts',(-6.81458866379034,-13.361350209501,
118.464074361768)) ;
#155169 = CARTESIAN_POINT('Ctrl Pts',(-6.83824065261878,-13.3648978107094,
118.536114504284)) ;
#155170 = CARTESIAN_POINT('Ctrl Pts',(-6.91204449644649,-13.3648977704052,
118.51188346384)) ;
#155171 = CARTESIAN_POINT('Ctrl Pts',(-6.9858483402742,-13.364897730101,118.487652423396)) ;
#155172 = CARTESIAN_POINT('Ctrl Pts',(-6.96219635144575,-13.3613501288926,
118.41561228088)) ;
#155173 = CARTESIAN_POINT('Ctrl Pts',(-6.9385443626173,-13.3578025276842,
118.343572138364)) ;
#155174 = CARTESIAN_POINT('Ctrl Pts',(-6.86474051878959,-13.3578025679884,
118.367803178808)) ;
#155175 = CARTESIAN_POINT('Ctrl Pts',(-6.79093667496188,-13.3578026082926,
118.392034219252)) ;
#155176 = CARTESIAN_POINT('Ctrl Pts',(-6.81458866379034,-13.361350209501,
118.464074361768)) ;
#155177 = CARTESIAN_POINT('Ctrl Pts',(-6.84190912425954,-13.0754523993138,
118.511850887542)) ;
#155178 = CARTESIAN_POINT('Ctrl Pts',(-6.86442104202547,-13.0989663539562,
118.580418557715)) ;
#155179 = CARTESIAN_POINT('Ctrl Pts',(-6.93822489001608,-13.0989663074807,
118.556187529951)) ;
#155180 = CARTESIAN_POINT('Ctrl Pts',(-7.01202873800668,-13.0989662610053,
118.531956502186)) ;
#155181 = CARTESIAN_POINT('Ctrl Pts',(-6.98951682024076,-13.0754523063629,
118.463388832014)) ;
#155182 = CARTESIAN_POINT('Ctrl Pts',(-6.96700490247481,-13.0519383517206,
118.394821161841)) ;
#155183 = CARTESIAN_POINT('Ctrl Pts',(-6.89320105448421,-13.051938398196,
118.419052189605)) ;
#155184 = CARTESIAN_POINT('Ctrl Pts',(-6.8193972064936,-13.0519384446715,
118.44328321737)) ;
#155185 = CARTESIAN_POINT('Ctrl Pts',(-6.84190912425954,-13.0754523993138,
118.511850887542)) ;
#155186 = CARTESIAN_POINT('Ctrl Pts',(-6.89221998106671,-12.8139381990977,
118.629651920743)) ;
#155187 = CARTESIAN_POINT('Ctrl Pts',(-6.91198505624896,-12.8557446579336,
118.68985315177)) ;
#155188 = CARTESIAN_POINT('Ctrl Pts',(-6.98578890934624,-12.8557446099044,
118.66562213956)) ;
#155189 = CARTESIAN_POINT('Ctrl Pts',(-7.05959276244351,-12.8557445618753,
118.641391127349)) ;
#155190 = CARTESIAN_POINT('Ctrl Pts',(-7.03982768726127,-12.8139381030394,
118.581189896322)) ;
#155191 = CARTESIAN_POINT('Ctrl Pts',(-7.02006261207903,-12.7721316442036,
118.520988665295)) ;
#155192 = CARTESIAN_POINT('Ctrl Pts',(-6.94625875898175,-12.7721316922327,
118.545219677506)) ;
#155193 = CARTESIAN_POINT('Ctrl Pts',(-6.87245490588448,-12.7721317402619,
118.569450689716)) ;
#155194 = CARTESIAN_POINT('Ctrl Pts',(-6.89221998106671,-12.8139381990977,
118.629651920743)) ;
#155195 = CARTESIAN_POINT('Ctrl Pts',(-6.96317166541847,-12.5948180944483,
118.810143346469)) ;
#155196 = CARTESIAN_POINT('Ctrl Pts',(-6.97874870279201,-12.6519838381849,
118.857588490258)) ;
#155197 = CARTESIAN_POINT('Ctrl Pts',(-7.05255256187162,-12.6519837938663,
118.833357496269)) ;
#155198 = CARTESIAN_POINT('Ctrl Pts',(-7.12635642095122,-12.6519837495477,
118.80912650228)) ;
#155199 = CARTESIAN_POINT('Ctrl Pts',(-7.11077938357767,-12.5948180058111,
118.761681358491)) ;
#155200 = CARTESIAN_POINT('Ctrl Pts',(-7.09520234620412,-12.5376522620745,
118.714236214702)) ;
#155201 = CARTESIAN_POINT('Ctrl Pts',(-7.02139848712452,-12.537652306393,
118.738467208691)) ;
#155202 = CARTESIAN_POINT('Ctrl Pts',(-6.94759462804491,-12.5376523507116,
118.76269820268)) ;
#155203 = CARTESIAN_POINT('Ctrl Pts',(-6.96317166541847,-12.5948180944483,
118.810143346469)) ;
#155204 = CARTESIAN_POINT('Ctrl Pts',(-7.04930238281719,-12.4362800048722,
119.037190426179)) ;
#155205 = CARTESIAN_POINT('Ctrl Pts',(-7.05961869911306,-12.5045968794166,
119.068612262503)) ;
#155206 = CARTESIAN_POINT('Ctrl Pts',(-7.13342256311478,-12.5045968472639,
119.044381283506)) ;
#155207 = CARTESIAN_POINT('Ctrl Pts',(-7.20722642711649,-12.5045968151111,
119.020150304509)) ;
#155208 = CARTESIAN_POINT('Ctrl Pts',(-7.19691011082063,-12.4362799405667,
118.988728468185)) ;
#155209 = CARTESIAN_POINT('Ctrl Pts',(-7.18659379452477,-12.3679630660223,
118.95730663186)) ;
#155210 = CARTESIAN_POINT('Ctrl Pts',(-7.11278993052304,-12.367963098175,
118.981537610857)) ;
#155211 = CARTESIAN_POINT('Ctrl Pts',(-7.03898606652133,-12.3679631303278,
119.005768589854)) ;
#155212 = CARTESIAN_POINT('Ctrl Pts',(-7.04930238281719,-12.4362800048722,
119.037190426179)) ;
#155213 = CARTESIAN_POINT('Ctrl Pts',(-7.14639896583729,-12.346922078608,
119.29741677471)) ;
#155214 = CARTESIAN_POINT('Ctrl Pts',(-7.15068612719803,-12.4215768384595,
119.310474778056)) ;
#155215 = CARTESIAN_POINT('Ctrl Pts',(-7.22448999554273,-12.4215768235296,
119.286243812287)) ;
#155216 = CARTESIAN_POINT('Ctrl Pts',(-7.29829386388744,-12.4215768085998,
119.262012846518)) ;
#155217 = CARTESIAN_POINT('Ctrl Pts',(-7.2940067025267,-12.3469220487482,
119.248954843172)) ;
#155218 = CARTESIAN_POINT('Ctrl Pts',(-7.28971954116596,-12.2722672888967,
119.235896839826)) ;
#155219 = CARTESIAN_POINT('Ctrl Pts',(-7.21591567282126,-12.2722673038266,
119.260127805595)) ;
#155220 = CARTESIAN_POINT('Ctrl Pts',(-7.14211180447654,-12.2722673187564,
119.284358771364)) ;
#155221 = CARTESIAN_POINT('Ctrl Pts',(-7.14639896583729,-12.346922078608,
119.29741677471)) ;
#155222 = CARTESIAN_POINT('Ctrl Pts',(-7.24765406779605,-12.3346186385411,
119.570362985162)) ;
#155223 = CARTESIAN_POINT('Ctrl Pts',(-7.24561188999,-12.4102408597983,119.56414284277)) ;
#155224 = CARTESIAN_POINT('Ctrl Pts',(-7.3194157607563,-12.4102408673589,
119.539911884376)) ;
#155225 = CARTESIAN_POINT('Ctrl Pts',(-7.3932196315226,-12.4102408749196,
119.515680925983)) ;
#155226 = CARTESIAN_POINT('Ctrl Pts',(-7.39526180932864,-12.3346186536624,
119.521901068375)) ;
#155227 = CARTESIAN_POINT('Ctrl Pts',(-7.3973039871347,-12.2589964324052,
119.528121210767)) ;
#155228 = CARTESIAN_POINT('Ctrl Pts',(-7.3235001163684,-12.2589964248446,
119.55235216916)) ;
#155229 = CARTESIAN_POINT('Ctrl Pts',(-7.24969624560211,-12.2589964172839,
119.576583127554)) ;
#155230 = CARTESIAN_POINT('Ctrl Pts',(-7.24765406779605,-12.3346186385411,
119.570362985162)) ;
#155231 = CARTESIAN_POINT('Ctrl Pts',(-7.34665382402801,-12.3998225687949,
119.836445852581)) ;
#155232 = CARTESIAN_POINT('Ctrl Pts',(-7.33843046780754,-12.4710025852177,
119.811398838181)) ;
#155233 = CARTESIAN_POINT('Ctrl Pts',(-7.41223433866837,-12.4710026178869,
119.787167880076)) ;
#155234 = CARTESIAN_POINT('Ctrl Pts',(-7.48603820952917,-12.4710026505561,
119.762936921971)) ;
#155235 = CARTESIAN_POINT('Ctrl Pts',(-7.49426156574964,-12.3998226341332,
119.78798393637)) ;
#155236 = CARTESIAN_POINT('Ctrl Pts',(-7.5024849219701,-12.3286426177104,
119.81303095077)) ;
#155237 = CARTESIAN_POINT('Ctrl Pts',(-7.42868105110929,-12.3286425850412,
119.837261908875)) ;
#155238 = CARTESIAN_POINT('Ctrl Pts',(-7.35487718024847,-12.328642552372,
119.861492866981)) ;
#155239 = CARTESIAN_POINT('Ctrl Pts',(-7.34665382402801,-12.3998225687949,
119.836445852581)) ;
#155240 = CARTESIAN_POINT('Ctrl Pts',(-7.4370740592955,-12.5378477500096,
120.076408147661)) ;
#155241 = CARTESIAN_POINT('Ctrl Pts',(-7.42325927266372,-12.599495230749,
120.034330538498)) ;
#155242 = CARTESIAN_POINT('Ctrl Pts',(-7.497063141071,-12.5994952885301,120.01009957292)) ;
#155243 = CARTESIAN_POINT('Ctrl Pts',(-7.57086700947827,-12.5994953463112,
119.985868607341)) ;
#155244 = CARTESIAN_POINT('Ctrl Pts',(-7.58468179611005,-12.5378478655717,
120.027946216505)) ;
#155245 = CARTESIAN_POINT('Ctrl Pts',(-7.59849658274182,-12.4762003848323,
120.070023825668)) ;
#155246 = CARTESIAN_POINT('Ctrl Pts',(-7.52469271433454,-12.4762003270512,
120.094254791246)) ;
#155247 = CARTESIAN_POINT('Ctrl Pts',(-7.45088884592727,-12.4762002692701,
120.118485756825)) ;
#155248 = CARTESIAN_POINT('Ctrl Pts',(-7.4370740592955,-12.5378477500096,
120.076408147661)) ;
#155249 = CARTESIAN_POINT('Ctrl Pts',(-7.5133452204639,-12.7392396507352,
120.273212489585)) ;
#155250 = CARTESIAN_POINT('Ctrl Pts',(-7.49491989486196,-12.7869171442881,
120.217091922708)) ;
#155251 = CARTESIAN_POINT('Ctrl Pts',(-7.56872375838898,-12.7869172246325,
120.192860942265)) ;
#155252 = CARTESIAN_POINT('Ctrl Pts',(-7.64252762191598,-12.786917304977,
120.168629961822)) ;
#155253 = CARTESIAN_POINT('Ctrl Pts',(-7.66095294751793,-12.7392398114241,
120.2247505287)) ;
#155254 = CARTESIAN_POINT('Ctrl Pts',(-7.67937827311986,-12.6915623178712,
120.280871095577)) ;
#155255 = CARTESIAN_POINT('Ctrl Pts',(-7.60557440959285,-12.6915622375267,
120.30510207602)) ;
#155256 = CARTESIAN_POINT('Ctrl Pts',(-7.53177054606584,-12.6915621571823,
120.329333056462)) ;
#155257 = CARTESIAN_POINT('Ctrl Pts',(-7.5133452204639,-12.7392396507352,
120.273212489585)) ;
#155258 = CARTESIAN_POINT('Ctrl Pts',(-7.57051158312834,-12.989236405783,
120.411850909373)) ;
#155259 = CARTESIAN_POINT('Ctrl Pts',(-7.54880219935677,-13.019530175167,
120.345727631249)) ;
#155260 = CARTESIAN_POINT('Ctrl Pts',(-7.62260605583471,-13.019530272485,
120.321496629336)) ;
#155261 = CARTESIAN_POINT('Ctrl Pts',(-7.69640991231264,-13.0195303698031,
120.297265627423)) ;
#155262 = CARTESIAN_POINT('Ctrl Pts',(-7.71811929608421,-12.9892366004191,
120.363388905547)) ;
#155263 = CARTESIAN_POINT('Ctrl Pts',(-7.7398286798558,-12.9589428310352,
120.429512183671)) ;
#155264 = CARTESIAN_POINT('Ctrl Pts',(-7.66602482337786,-12.9589427337171,
120.453743185585)) ;
#155265 = CARTESIAN_POINT('Ctrl Pts',(-7.59222096689992,-12.9589426363991,
120.477974187498)) ;
#155266 = CARTESIAN_POINT('Ctrl Pts',(-7.57051158312834,-12.989236405783,
120.411850909373)) ;
#155267 = CARTESIAN_POINT('Ctrl Pts',(-7.60526793750275,-13.269049028932,
120.482338834054)) ;
#155268 = CARTESIAN_POINT('Ctrl Pts',(-7.58183203791737,-13.279851801729,
120.410956867366)) ;
#155269 = CARTESIAN_POINT('Ctrl Pts',(-7.65563588594552,-13.2798519083315,
120.386725839716)) ;
#155270 = CARTESIAN_POINT('Ctrl Pts',(-7.7294397339737,-13.279852014934,120.362494812066)) ;
#155271 = CARTESIAN_POINT('Ctrl Pts',(-7.75287563355908,-13.269049242137,
120.433876778754)) ;
#155272 = CARTESIAN_POINT('Ctrl Pts',(-7.77631153314448,-13.2582464693401,
120.505258745443)) ;
#155273 = CARTESIAN_POINT('Ctrl Pts',(-7.7025076851163,-13.2582463627375,
120.529489773093)) ;
#155274 = CARTESIAN_POINT('Ctrl Pts',(-7.62870383708814,-13.258246256135,
120.553720800743)) ;
#155275 = CARTESIAN_POINT('Ctrl Pts',(-7.60526793750275,-13.269049028932,
120.482338834054)) ;
#155276 = CARTESIAN_POINT('Ctrl Pts',(-7.61610217928452,-13.560604521515,
120.479829556645)) ;
#155277 = CARTESIAN_POINT('Ctrl Pts',(-7.59260992748901,-13.5510680943663,
120.408275950233)) ;
#155278 = CARTESIAN_POINT('Ctrl Pts',(-7.66641376645151,-13.5510682019353,
120.384044894971)) ;
#155279 = CARTESIAN_POINT('Ctrl Pts',(-7.74021760541402,-13.5510683095042,
120.359813839708)) ;
#155280 = CARTESIAN_POINT('Ctrl Pts',(-7.76370985720953,-13.5606047366529,
120.43136744612)) ;
#155281 = CARTESIAN_POINT('Ctrl Pts',(-7.78720210900504,-13.5701411638016,
120.502921052531)) ;
#155282 = CARTESIAN_POINT('Ctrl Pts',(-7.71339827004254,-13.5701410562327,
120.527152107794)) ;
#155283 = CARTESIAN_POINT('Ctrl Pts',(-7.63959443108004,-13.5701409486637,
120.551383163056)) ;
#155284 = CARTESIAN_POINT('Ctrl Pts',(-7.61610217928452,-13.560604521515,
120.479829556645)) ;
#155285 = CARTESIAN_POINT('Ctrl Pts',(-7.60265701261583,-13.8423158077137,
120.4033105886)) ;
#155286 = CARTESIAN_POINT('Ctrl Pts',(-7.58080443900952,-13.8130971975032,
120.33675117738)) ;
#155287 = CARTESIAN_POINT('Ctrl Pts',(-7.65460826925647,-13.8130972967894,
120.312520095571)) ;
#155288 = CARTESIAN_POINT('Ctrl Pts',(-7.72841209950342,-13.8130973960757,
120.288289013763)) ;
#155289 = CARTESIAN_POINT('Ctrl Pts',(-7.75026467310974,-13.8423160062862,
120.354848424983)) ;
#155290 = CARTESIAN_POINT('Ctrl Pts',(-7.77211724671606,-13.8715346164967,
120.421407836203)) ;
#155291 = CARTESIAN_POINT('Ctrl Pts',(-7.6983134164691,-13.8715345172104,
120.445638918011)) ;
#155292 = CARTESIAN_POINT('Ctrl Pts',(-7.62450958622215,-13.8715344179242,
120.46986999982)) ;
#155293 = CARTESIAN_POINT('Ctrl Pts',(-7.60265701261583,-13.8423158077137,
120.4033105886)) ;
#155294 = CARTESIAN_POINT('Ctrl Pts',(-7.56703031046435,-14.0920492190499,
120.259455200578)) ;
#155295 = CARTESIAN_POINT('Ctrl Pts',(-7.5483639780729,-14.0453516515009,
120.202600565973)) ;
#155296 = CARTESIAN_POINT('Ctrl Pts',(-7.62216780084486,-14.0453517349523,
120.178369461397)) ;
#155297 = CARTESIAN_POINT('Ctrl Pts',(-7.69597162361682,-14.0453518184037,
120.154138356821)) ;
#155298 = CARTESIAN_POINT('Ctrl Pts',(-7.71463795600827,-14.0920493859528,
120.210992991425)) ;
#155299 = CARTESIAN_POINT('Ctrl Pts',(-7.73330428839972,-14.1387469535018,
120.26784762603)) ;
#155300 = CARTESIAN_POINT('Ctrl Pts',(-7.65950046562776,-14.1387468700504,
120.292078730606)) ;
#155301 = CARTESIAN_POINT('Ctrl Pts',(-7.5856966428558,-14.138746786599,120.316309835182)) ;
#155302 = CARTESIAN_POINT('Ctrl Pts',(-7.56703031046435,-14.0920492190499,
120.259455200578)) ;
#155303 = CARTESIAN_POINT('Ctrl Pts',(-7.51204303377268,-14.2950965364046,
120.056387264096)) ;
#155304 = CARTESIAN_POINT('Ctrl Pts',(-7.49792407955998,-14.2341530477557,
120.013383209649)) ;
#155305 = CARTESIAN_POINT('Ctrl Pts',(-7.57172789688386,-14.2341531086755,
119.989152088479)) ;
#155306 = CARTESIAN_POINT('Ctrl Pts',(-7.64553171420774,-14.2341531695953,
119.964920967308)) ;
#155307 = CARTESIAN_POINT('Ctrl Pts',(-7.65965066842044,-14.2950966582441,
120.007925021756)) ;
#155308 = CARTESIAN_POINT('Ctrl Pts',(-7.67376962263314,-14.3560401468929,
120.050929076204)) ;
#155309 = CARTESIAN_POINT('Ctrl Pts',(-7.59996580530926,-14.3560400859732,
120.075160197374)) ;
#155310 = CARTESIAN_POINT('Ctrl Pts',(-7.52616198798538,-14.3560400250534,
120.099391318544)) ;
#155311 = CARTESIAN_POINT('Ctrl Pts',(-7.51204303377268,-14.2950965364046,
120.056387264096)) ;
#155312 = CARTESIAN_POINT('Ctrl Pts',(-7.44273831121475,-14.434335219557,
119.809815786678)) ;
#155313 = CARTESIAN_POINT('Ctrl Pts',(-7.43417104149911,-14.3635791231233,
119.783721267369)) ;
#155314 = CARTESIAN_POINT('Ctrl Pts',(-7.50797485590469,-14.3635791582218,
119.75949013731)) ;
#155315 = CARTESIAN_POINT('Ctrl Pts',(-7.58177867031028,-14.3635791933204,
119.735259007251)) ;
#155316 = CARTESIAN_POINT('Ctrl Pts',(-7.59034594002593,-14.4343352897541,
119.76135352656)) ;
#155317 = CARTESIAN_POINT('Ctrl Pts',(-7.59891320974157,-14.5050913861879,
119.787448045869)) ;
#155318 = CARTESIAN_POINT('Ctrl Pts',(-7.52510939533598,-14.5050913510893,
119.811679175928)) ;
#155319 = CARTESIAN_POINT('Ctrl Pts',(-7.45130558093039,-14.5050913159907,
119.835910305987)) ;
#155320 = CARTESIAN_POINT('Ctrl Pts',(-7.44273831121475,-14.434335219557,
119.809815786678)) ;
#155321 = CARTESIAN_POINT('Ctrl Pts',(-7.36521040000063,-14.5007530721094,
119.538381721836)) ;
#155322 = CARTESIAN_POINT('Ctrl Pts',(-7.36277354008315,-14.4252541131167,
119.530959441559)) ;
#155323 = CARTESIAN_POINT('Ctrl Pts',(-7.4365773538254,-14.4252541219683,
119.50672830948)) ;
#155324 = CARTESIAN_POINT('Ctrl Pts',(-7.51038116756764,-14.4252541308198,
119.482497177401)) ;
#155325 = CARTESIAN_POINT('Ctrl Pts',(-7.51281802748512,-14.5007530898126,
119.489919457677)) ;
#155326 = CARTESIAN_POINT('Ctrl Pts',(-7.51525488740261,-14.5762520488053,
119.497341737954)) ;
#155327 = CARTESIAN_POINT('Ctrl Pts',(-7.44145107366037,-14.5762520399537,
119.521572870033)) ;
#155328 = CARTESIAN_POINT('Ctrl Pts',(-7.36764725991812,-14.5762520311022,
119.545804002113)) ;
#155329 = CARTESIAN_POINT('Ctrl Pts',(-7.36521040000063,-14.5007530721094,
119.538381721836)) ;
#155330 = CARTESIAN_POINT('Ctrl Pts',(-7.28479809434297,-14.4901437351793,
119.257926243117)) ;
#155331 = CARTESIAN_POINT('Ctrl Pts',(-7.28870699471344,-14.415271701562,
119.269832124676)) ;
#155332 = CARTESIAN_POINT('Ctrl Pts',(-7.36251081065682,-14.4152716856427,
119.245600999301)) ;
#155333 = CARTESIAN_POINT('Ctrl Pts',(-7.43631462660021,-14.4152716697234,
119.221369873926)) ;
#155334 = CARTESIAN_POINT('Ctrl Pts',(-7.43240572622976,-14.4901437033406,
119.209463992367)) ;
#155335 = CARTESIAN_POINT('Ctrl Pts',(-7.42849682585929,-14.5650157369579,
119.197558110808)) ;
#155336 = CARTESIAN_POINT('Ctrl Pts',(-7.3546930099159,-14.5650157528772,
119.221789236183)) ;
#155337 = CARTESIAN_POINT('Ctrl Pts',(-7.28088919397251,-14.5650157687965,
119.246020361558)) ;
#155338 = CARTESIAN_POINT('Ctrl Pts',(-7.28479809434297,-14.4901437351793,
119.257926243117)) ;
#155339 = CARTESIAN_POINT('Ctrl Pts',(-7.20843821052364,-14.402041943339,
118.989761053497)) ;
#155340 = CARTESIAN_POINT('Ctrl Pts',(-7.21842069556288,-14.3332076954044,
119.020166093841)) ;
#155341 = CARTESIAN_POINT('Ctrl Pts',(-7.29222451596317,-14.3332076598222,
118.995934982041)) ;
#155342 = CARTESIAN_POINT('Ctrl Pts',(-7.36602833636344,-14.33320762424,118.971703870241)) ;
#155343 = CARTESIAN_POINT('Ctrl Pts',(-7.3560458513242,-14.4020418721746,
118.941298829897)) ;
#155344 = CARTESIAN_POINT('Ctrl Pts',(-7.34606336628494,-14.4708761201093,
118.910893789552)) ;
#155345 = CARTESIAN_POINT('Ctrl Pts',(-7.27225954588466,-14.4708761556915,
118.935124901352)) ;
#155346 = CARTESIAN_POINT('Ctrl Pts',(-7.19845572548438,-14.4708761912736,
118.959356013152)) ;
#155347 = CARTESIAN_POINT('Ctrl Pts',(-7.20843821052364,-14.402041943339,
118.989761053497)) ;
#155348 = CARTESIAN_POINT('Ctrl Pts',(-7.1427835920666,-14.243691286176,118.754343222241)) ;
#155349 = CARTESIAN_POINT('Ctrl Pts',(-7.15809856623828,-14.18580899599,118.800990163949)) ;
#155350 = CARTESIAN_POINT('Ctrl Pts',(-7.23190239210298,-14.1858089469242,
118.776759068792)) ;
#155351 = CARTESIAN_POINT('Ctrl Pts',(-7.30570621796767,-14.1858088978584,
118.752527973636)) ;
#155352 = CARTESIAN_POINT('Ctrl Pts',(-7.290391243796,-14.2436911880444,118.705881031928)) ;
#155353 = CARTESIAN_POINT('Ctrl Pts',(-7.27507626962433,-14.3015734782304,
118.659234090221)) ;
#155354 = CARTESIAN_POINT('Ctrl Pts',(-7.20127244375963,-14.3015735272962,
118.683465185377)) ;
#155355 = CARTESIAN_POINT('Ctrl Pts',(-7.12746861789493,-14.301573576362,
118.707696280533)) ;
#155356 = CARTESIAN_POINT('Ctrl Pts',(-7.1427835920666,-14.243691286176,118.754343222241)) ;
#155357 = CARTESIAN_POINT('Ctrl Pts',(-7.09305076334606,-14.0272168477211,
118.567541759605)) ;
#155358 = CARTESIAN_POINT('Ctrl Pts',(-7.11259210256672,-13.9843615039812,
118.627061527202)) ;
#155359 = CARTESIAN_POINT('Ctrl Pts',(-7.18639593427092,-13.9843614472663,
118.602830449832)) ;
#155360 = CARTESIAN_POINT('Ctrl Pts',(-7.26019976597513,-13.9843613905514,
118.578599372462)) ;
#155361 = CARTESIAN_POINT('Ctrl Pts',(-7.24065842675446,-14.0272167342913,
118.519079604865)) ;
#155362 = CARTESIAN_POINT('Ctrl Pts',(-7.22111708753381,-14.0700720780313,
118.459559837268)) ;
#155363 = CARTESIAN_POINT('Ctrl Pts',(-7.1473132558296,-14.0700721347462,
118.483790914638)) ;
#155364 = CARTESIAN_POINT('Ctrl Pts',(-7.0735094241254,-14.0700721914611,
118.508021992008)) ;
#155365 = CARTESIAN_POINT('Ctrl Pts',(-7.09305076334606,-14.0272168477211,
118.567541759605)) ;
#155366 = CARTESIAN_POINT('Ctrl Pts',(-7.06320365437595,-13.7664028194368,
118.441170630651)) ;
#155367 = CARTESIAN_POINT('Ctrl Pts',(-7.08559233431929,-13.7416926429616,
118.509362938513)) ;
#155368 = CARTESIAN_POINT('Ctrl Pts',(-7.15939617199936,-13.7416925860971,
118.485131879344)) ;
#155369 = CARTESIAN_POINT('Ctrl Pts',(-7.23320000967943,-13.7416925292327,
118.460900820176)) ;
#155370 = CARTESIAN_POINT('Ctrl Pts',(-7.21081132973608,-13.7664027057079,
118.392708512314)) ;
#155371 = CARTESIAN_POINT('Ctrl Pts',(-7.18842264979274,-13.791112882183,
118.324516204452)) ;
#155372 = CARTESIAN_POINT('Ctrl Pts',(-7.11461881211266,-13.7911129390475,
118.348747263621)) ;
#155373 = CARTESIAN_POINT('Ctrl Pts',(-7.0408149744326,-13.7911129959119,
118.37297832279)) ;
#155374 = CARTESIAN_POINT('Ctrl Pts',(-7.06320365437595,-13.7664028194368,
118.441170630651)) ;
#155375 = CARTESIAN_POINT('Ctrl Pts',(-7.05638533636368,-13.4798811075686,
118.384860283325)) ;
#155376 = CARTESIAN_POINT('Ctrl Pts',(-7.08001960465576,-13.4751386073872,
118.456846452141)) ;
#155377 = CARTESIAN_POINT('Ctrl Pts',(-7.15382344746782,-13.4751385570953,
118.432615408603)) ;
#155378 = CARTESIAN_POINT('Ctrl Pts',(-7.22762729027988,-13.4751385068035,
118.408384365066)) ;
#155379 = CARTESIAN_POINT('Ctrl Pts',(-7.2039930219878,-13.4798810069848,
118.33639819625)) ;
#155380 = CARTESIAN_POINT('Ctrl Pts',(-7.18035875369573,-13.4846235071661,
118.264412027435)) ;
#155381 = CARTESIAN_POINT('Ctrl Pts',(-7.10655491088367,-13.484623557458,
118.288643070972)) ;
#155382 = CARTESIAN_POINT('Ctrl Pts',(-7.03275106807161,-13.4846236077499,
118.31287411451)) ;
#155383 = CARTESIAN_POINT('Ctrl Pts',(-7.05638533636368,-13.4798811075686,
118.384860283325)) ;
#155384 = CARTESIAN_POINT('Ctrl Pts',(-7.07408092560861,-13.1885796838075,
118.403166688914)) ;
#155385 = CARTESIAN_POINT('Ctrl Pts',(-7.09725213348969,-13.2041693777773,
118.473742450239)) ;
#155386 = CARTESIAN_POINT('Ctrl Pts',(-7.17105597976469,-13.2041693384602,
118.449511417249)) ;
#155387 = CARTESIAN_POINT('Ctrl Pts',(-7.24485982603969,-13.2041692991432,
118.425280384259)) ;
#155388 = CARTESIAN_POINT('Ctrl Pts',(-7.2216886181586,-13.1885796051734,
118.354704622934)) ;
#155389 = CARTESIAN_POINT('Ctrl Pts',(-7.19851741027751,-13.1729899112036,
118.284128861609)) ;
#155390 = CARTESIAN_POINT('Ctrl Pts',(-7.12471356400251,-13.1729899505207,
118.308359894599)) ;
#155391 = CARTESIAN_POINT('Ctrl Pts',(-7.05090971772751,-13.1729899898377,
118.332590927589)) ;
#155392 = CARTESIAN_POINT('Ctrl Pts',(-7.07408092560861,-13.1885796838075,
118.403166688914)) ;
#155393 = CARTESIAN_POINT('Ctrl Pts',(-7.11507198338345,-12.9166253502417,
118.492814113544)) ;
#155394 = CARTESIAN_POINT('Ctrl Pts',(-7.13614450236063,-12.9512269476541,
118.556997606973)) ;
#155395 = CARTESIAN_POINT('Ctrl Pts',(-7.209948350884,-12.951226917539,118.532766580832)) ;
#155396 = CARTESIAN_POINT('Ctrl Pts',(-7.28375219940736,-12.951226887424,
118.50853555469)) ;
#155397 = CARTESIAN_POINT('Ctrl Pts',(-7.26267968043019,-12.9166252900117,
118.444352061261)) ;
#155398 = CARTESIAN_POINT('Ctrl Pts',(-7.241607161453,-12.8820236925993,118.380168567832)) ;
#155399 = CARTESIAN_POINT('Ctrl Pts',(-7.16780331292964,-12.8820237227144,
118.404399593974)) ;
#155400 = CARTESIAN_POINT('Ctrl Pts',(-7.09399946440627,-12.8820237528294,
118.428630620115)) ;
#155401 = CARTESIAN_POINT('Ctrl Pts',(-7.11507198338345,-12.9166253502417,
118.492814113544)) ;
#155402 = CARTESIAN_POINT('Ctrl Pts',(-7.1780574208389,-12.6775835687805,
118.649064501798)) ;
#155403 = CARTESIAN_POINT('Ctrl Pts',(-7.19550067995718,-12.7289285556427,
118.70219385509)) ;
#155404 = CARTESIAN_POINT('Ctrl Pts',(-7.26930452881846,-12.728928538127,
118.677962829978)) ;
#155405 = CARTESIAN_POINT('Ctrl Pts',(-7.34310837767973,-12.7289285206112,
118.653731804865)) ;
#155406 = CARTESIAN_POINT('Ctrl Pts',(-7.32566511856146,-12.6775835337489,
118.600602451572)) ;
#155407 = CARTESIAN_POINT('Ctrl Pts',(-7.30822185944318,-12.6262385468866,
118.54747309828)) ;
#155408 = CARTESIAN_POINT('Ctrl Pts',(-7.2344180105819,-12.6262385644024,
118.571704123392)) ;
#155409 = CARTESIAN_POINT('Ctrl Pts',(-7.16061416172062,-12.6262385819182,
118.595935148505)) ;
#155410 = CARTESIAN_POINT('Ctrl Pts',(-7.1780574208389,-12.6775835687805,
118.649064501798)) ;
#155411 = CARTESIAN_POINT('Ctrl Pts',(-7.25891893918462,-12.4925681740676,
118.859833268336)) ;
#155412 = CARTESIAN_POINT('Ctrl Pts',(-7.27147756279767,-12.5569096995895,
118.898084809856)) ;
#155413 = CARTESIAN_POINT('Ctrl Pts',(-7.34528141070538,-12.5569096913385,
118.873853781839)) ;
#155414 = CARTESIAN_POINT('Ctrl Pts',(-7.4190852586131,-12.5569096830874,
118.849622753822)) ;
#155415 = CARTESIAN_POINT('Ctrl Pts',(-7.40652663500005,-12.4925681575655,
118.811371212302)) ;
#155416 = CARTESIAN_POINT('Ctrl Pts',(-7.393968011387,-12.4282266320435,118.773119670782)) ;
#155417 = CARTESIAN_POINT('Ctrl Pts',(-7.32016416347927,-12.4282266402946,
118.797350698799)) ;
#155418 = CARTESIAN_POINT('Ctrl Pts',(-7.24636031557156,-12.4282266485456,
118.821581726816)) ;
#155419 = CARTESIAN_POINT('Ctrl Pts',(-7.25891893918462,-12.4925681740676,
118.859833268336)) ;
#155420 = CARTESIAN_POINT('Ctrl Pts',(-7.35188793041178,-12.3743553948694,
119.107715107246)) ;
#155421 = CARTESIAN_POINT('Ctrl Pts',(-7.35870415945858,-12.4470477080891,
119.128476241342)) ;
#155422 = CARTESIAN_POINT('Ctrl Pts',(-7.43250800622119,-12.447047705519,
119.104245209837)) ;
#155423 = CARTESIAN_POINT('Ctrl Pts',(-7.50631185298381,-12.4470477029489,
119.080014178332)) ;
#155424 = CARTESIAN_POINT('Ctrl Pts',(-7.49949562393702,-12.3743553897291,
119.059253044237)) ;
#155425 = CARTESIAN_POINT('Ctrl Pts',(-7.49267939489023,-12.3016630765093,
119.038491910141)) ;
#155426 = CARTESIAN_POINT('Ctrl Pts',(-7.41887554812762,-12.3016630790795,
119.062722941646)) ;
#155427 = CARTESIAN_POINT('Ctrl Pts',(-7.345071701365,-12.3016630816496,119.086953973151)) ;
#155428 = CARTESIAN_POINT('Ctrl Pts',(-7.35188793041178,-12.3743553948694,
119.107715107246)) ;
#155429 = CARTESIAN_POINT('Ctrl Pts',(-7.45265031525607,-12.3300586716913,
119.37899047094)) ;
#155430 = CARTESIAN_POINT('Ctrl Pts',(-7.45317826435854,-12.4059540802535,
119.3805985188)) ;
#155431 = CARTESIAN_POINT('Ctrl Pts',(-7.52698210902912,-12.4059540807321,
119.356367480923)) ;
#155432 = CARTESIAN_POINT('Ctrl Pts',(-7.60078595369971,-12.4059540812107,
119.332136443046)) ;
#155433 = CARTESIAN_POINT('Ctrl Pts',(-7.60025800459724,-12.3300586726485,
119.330528395187)) ;
#155434 = CARTESIAN_POINT('Ctrl Pts',(-7.59973005549478,-12.2541632640863,
119.328920347327)) ;
#155435 = CARTESIAN_POINT('Ctrl Pts',(-7.52592621082419,-12.2541632636077,
119.353151385204)) ;
#155436 = CARTESIAN_POINT('Ctrl Pts',(-7.4521223661536,-12.254163263129,119.37738242308)) ;
#155437 = CARTESIAN_POINT('Ctrl Pts',(-7.45265031525607,-12.3300586716913,
119.37899047094)) ;
#155438 = CARTESIAN_POINT('Ctrl Pts',(-7.55337524562207,-12.3643855283945,
119.650314676817)) ;
#155439 = CARTESIAN_POINT('Ctrl Pts',(-7.54760458625465,-12.4379977305632,
119.632738179473)) ;
#155440 = CARTESIAN_POINT('Ctrl Pts',(-7.62140842959395,-12.4379977307755,
119.608507137542)) ;
#155441 = CARTESIAN_POINT('Ctrl Pts',(-7.69521227293323,-12.4379977309879,
119.58427609561)) ;
#155442 = CARTESIAN_POINT('Ctrl Pts',(-7.70098293230066,-12.3643855288192,
119.601852592954)) ;
#155443 = CARTESIAN_POINT('Ctrl Pts',(-7.70675359166808,-12.2907733266505,
119.619429090297)) ;
#155444 = CARTESIAN_POINT('Ctrl Pts',(-7.63294974832878,-12.2907733264382,
119.643660132229)) ;
#155445 = CARTESIAN_POINT('Ctrl Pts',(-7.55914590498948,-12.2907733262258,
119.66789117416)) ;
#155446 = CARTESIAN_POINT('Ctrl Pts',(-7.55337524562207,-12.3643855283945,
119.650314676817)) ;
#155447 = CARTESIAN_POINT('Ctrl Pts',(-7.64773366833853,-12.4735026256636,
119.902366613272)) ;
#155448 = CARTESIAN_POINT('Ctrl Pts',(-7.63609718343747,-12.5396050352221,
119.866923757755)) ;
#155449 = CARTESIAN_POINT('Ctrl Pts',(-7.70990102613766,-12.5396050341181,
119.842692713877)) ;
#155450 = CARTESIAN_POINT('Ctrl Pts',(-7.78370486883785,-12.5396050330141,
119.818461669998)) ;
#155451 = CARTESIAN_POINT('Ctrl Pts',(-7.79534135373891,-12.4735026234556,
119.853904525516)) ;
#155452 = CARTESIAN_POINT('Ctrl Pts',(-7.80697783863996,-12.4074002138971,
119.889347381033)) ;
#155453 = CARTESIAN_POINT('Ctrl Pts',(-7.73317399593978,-12.4074002150011,
119.913578424911)) ;
#155454 = CARTESIAN_POINT('Ctrl Pts',(-7.65937015323959,-12.4074002161051,
119.93780946879)) ;
#155455 = CARTESIAN_POINT('Ctrl Pts',(-7.64773366833853,-12.4735026256636,
119.902366613272)) ;
#155456 = CARTESIAN_POINT('Ctrl Pts',(-7.73041986817396,-12.6505044221707,
120.118738891923)) ;
#155457 = CARTESIAN_POINT('Ctrl Pts',(-7.71372634252646,-12.7043450691342,
120.067893106223)) ;
#155458 = CARTESIAN_POINT('Ctrl Pts',(-7.7875301851787,-12.7043450666146,
120.043662062199)) ;
#155459 = CARTESIAN_POINT('Ctrl Pts',(-7.86133402783094,-12.7043450640951,
120.019431018175)) ;
#155460 = CARTESIAN_POINT('Ctrl Pts',(-7.87802755347846,-12.6505044171317,
120.070276803874)) ;
#155461 = CARTESIAN_POINT('Ctrl Pts',(-7.89472107912596,-12.5966637701682,
120.121122589574)) ;
#155462 = CARTESIAN_POINT('Ctrl Pts',(-7.82091723647372,-12.5966637726878,
120.145353633598)) ;
#155463 = CARTESIAN_POINT('Ctrl Pts',(-7.74711339382147,-12.5966637752073,
120.169584677622)) ;
#155464 = CARTESIAN_POINT('Ctrl Pts',(-7.73041986817396,-12.6505044221707,
120.118738891923)) ;
#155465 = CARTESIAN_POINT('Ctrl Pts',(-7.79595012127722,-12.883421947767,
120.282755379935)) ;
#155466 = CARTESIAN_POINT('Ctrl Pts',(-7.77539224983967,-12.9210776018657,
120.220139420507)) ;
#155467 = CARTESIAN_POINT('Ctrl Pts',(-7.84919609306675,-12.9210776004055,
120.195908378234)) ;
#155468 = CARTESIAN_POINT('Ctrl Pts',(-7.92299993629382,-12.9210775989452,
120.17167733596)) ;
#155469 = CARTESIAN_POINT('Ctrl Pts',(-7.94355780773136,-12.8834219448465,
120.234293295388)) ;
#155470 = CARTESIAN_POINT('Ctrl Pts',(-7.96411567916889,-12.8457662907479,
120.296909254817)) ;
#155471 = CARTESIAN_POINT('Ctrl Pts',(-7.89031183594182,-12.8457662922081,
120.32114029709)) ;
#155472 = CARTESIAN_POINT('Ctrl Pts',(-7.81650799271475,-12.8457662936684,
120.345371339364)) ;
#155473 = CARTESIAN_POINT('Ctrl Pts',(-7.79595012127722,-12.883421947767,
120.282755379935)) ;
#155474 = CARTESIAN_POINT('Ctrl Pts',(-7.83999077408972,-13.1527514798463,
120.381574983125)) ;
#155475 = CARTESIAN_POINT('Ctrl Pts',(-7.81705865500437,-13.1716560829413,
120.3117274485)) ;
#155476 = CARTESIAN_POINT('Ctrl Pts',(-7.8908624986358,-13.1716560841151,
120.287496407458)) ;
#155477 = CARTESIAN_POINT('Ctrl Pts',(-7.96466634226723,-13.1716560852888,
120.263265366416)) ;
#155478 = CARTESIAN_POINT('Ctrl Pts',(-7.98759846135258,-13.1527514821937,
120.333112901041)) ;
#155479 = CARTESIAN_POINT('Ctrl Pts',(-8.01053058043792,-13.1338468790986,
120.402960435666)) ;
#155480 = CARTESIAN_POINT('Ctrl Pts',(-7.93672673680649,-13.1338468779249,
120.427191476708)) ;
#155481 = CARTESIAN_POINT('Ctrl Pts',(-7.86292289317506,-13.1338468767512,
120.451422517749)) ;
#155482 = CARTESIAN_POINT('Ctrl Pts',(-7.83999077408972,-13.1527514798463,
120.381574983125)) ;
#155483 = CARTESIAN_POINT('Ctrl Pts',(-7.86072974007722,-13.4437023579035,
120.40908356129)) ;
#155484 = CARTESIAN_POINT('Ctrl Pts',(-7.83705375696572,-13.4423185568972,
120.336970336981)) ;
#155485 = CARTESIAN_POINT('Ctrl Pts',(-7.91085760050323,-13.442318564338,
120.312739295653)) ;
#155486 = CARTESIAN_POINT('Ctrl Pts',(-7.98466144404073,-13.4423185717788,
120.288508254326)) ;
#155487 = CARTESIAN_POINT('Ctrl Pts',(-8.00833742715221,-13.443702372785,
120.360621478634)) ;
#155488 = CARTESIAN_POINT('Ctrl Pts',(-8.0320134102637,-13.4450861737913,
120.432734702942)) ;
#155489 = CARTESIAN_POINT('Ctrl Pts',(-7.95820956672621,-13.4450861663505,
120.45696574427)) ;
#155490 = CARTESIAN_POINT('Ctrl Pts',(-7.88440572318869,-13.4450861589097,
120.481196785598)) ;
#155491 = CARTESIAN_POINT('Ctrl Pts',(-7.86072974007722,-13.4437023579035,
120.40908356129)) ;
#155492 = CARTESIAN_POINT('Ctrl Pts',(-7.85692244140455,-13.7306193771303,
120.362100112163)) ;
#155493 = CARTESIAN_POINT('Ctrl Pts',(-7.83421023585808,-13.7091999974399,
120.292922398928)) ;
#155494 = CARTESIAN_POINT('Ctrl Pts',(-7.90801407820719,-13.7092000104109,
120.268691353981)) ;
#155495 = CARTESIAN_POINT('Ctrl Pts',(-7.9818179205563,-13.7092000233819,
120.244460309033)) ;
#155496 = CARTESIAN_POINT('Ctrl Pts',(-8.00453012610277,-13.7306194030722,
120.313638022267)) ;
#155497 = CARTESIAN_POINT('Ctrl Pts',(-8.02724233164922,-13.7520387827626,
120.382815735502)) ;
#155498 = CARTESIAN_POINT('Ctrl Pts',(-7.95343848930012,-13.7520387697916,
120.40704678045)) ;
#155499 = CARTESIAN_POINT('Ctrl Pts',(-7.87963464695101,-13.7520387568206,
120.431277825397)) ;
#155500 = CARTESIAN_POINT('Ctrl Pts',(-7.85692244140455,-13.7306193771303,
120.362100112163)) ;
#155501 = CARTESIAN_POINT('Ctrl Pts',(-7.83012410737516,-13.9949086675026,
120.245151518457)) ;
#155502 = CARTESIAN_POINT('Ctrl Pts',(-7.80998117065526,-13.9550051326843,
120.183799383634)) ;
#155503 = CARTESIAN_POINT('Ctrl Pts',(-7.8837850110375,-13.9550051495312,
120.159568332696)) ;
#155504 = CARTESIAN_POINT('Ctrl Pts',(-7.95758885141974,-13.9550051663781,
120.135337281758)) ;
#155505 = CARTESIAN_POINT('Ctrl Pts',(-7.97773178813963,-13.9949087011963,
120.19668941658)) ;
#155506 = CARTESIAN_POINT('Ctrl Pts',(-7.99787472485951,-14.0348122360146,
120.258041551403)) ;
#155507 = CARTESIAN_POINT('Ctrl Pts',(-7.92407088447728,-14.0348122191677,
120.282272602341)) ;
#155508 = CARTESIAN_POINT('Ctrl Pts',(-7.85026704409504,-14.0348122023208,
120.306503653279)) ;
#155509 = CARTESIAN_POINT('Ctrl Pts',(-7.83012410737516,-13.9949086675026,
120.245151518457)) ;
#155510 = CARTESIAN_POINT('Ctrl Pts',(-7.78237083717385,-14.2196906214034,
120.06409456817)) ;
#155511 = CARTESIAN_POINT('Ctrl Pts',(-7.76626970535942,-14.1640342666894,
120.015053119126)) ;
#155512 = CARTESIAN_POINT('Ctrl Pts',(-7.84007354233546,-14.1640342866179,
119.990822057813)) ;
#155513 = CARTESIAN_POINT('Ctrl Pts',(-7.91387737931149,-14.1640343065465,
119.9665909965)) ;
#155514 = CARTESIAN_POINT('Ctrl Pts',(-7.9299785111259,-14.2196906612605,
120.015632445544)) ;
#155515 = CARTESIAN_POINT('Ctrl Pts',(-7.94607964294033,-14.2753470159745,
120.064673894588)) ;
#155516 = CARTESIAN_POINT('Ctrl Pts',(-7.8722758059643,-14.275346996046,120.088904955901)) ;
#155517 = CARTESIAN_POINT('Ctrl Pts',(-7.79847196898827,-14.2753469761174,
120.113136017214)) ;
#155518 = CARTESIAN_POINT('Ctrl Pts',(-7.78237083717385,-14.2196906214034,
120.06409456817)) ;
#155519 = CARTESIAN_POINT('Ctrl Pts',(-7.71854875724072,-14.3856064052365,
119.834353268658)) ;
#155520 = CARTESIAN_POINT('Ctrl Pts',(-7.70761197878153,-14.3182855334349,
119.801041606811)) ;
#155521 = CARTESIAN_POINT('Ctrl Pts',(-7.78141581228379,-14.3182855505584,
119.776810534917)) ;
#155522 = CARTESIAN_POINT('Ctrl Pts',(-7.85521964578606,-14.318285567682,
119.752579463024)) ;
#155523 = CARTESIAN_POINT('Ctrl Pts',(-7.86615642424525,-14.3856064394836,
119.785891124871)) ;
#155524 = CARTESIAN_POINT('Ctrl Pts',(-7.87709320270443,-14.4529273112853,
119.819202786718)) ;
#155525 = CARTESIAN_POINT('Ctrl Pts',(-7.80328936920217,-14.4529272941617,
119.843433858612)) ;
#155526 = CARTESIAN_POINT('Ctrl Pts',(-7.7294855356999,-14.4529272770382,
119.867664930505)) ;
#155527 = CARTESIAN_POINT('Ctrl Pts',(-7.71854875724072,-14.3856064052365,
119.834353268658)) ;
#155528 = CARTESIAN_POINT('Ctrl Pts',(-7.64334502750247,-14.4829720573525,
119.569777363778)) ;
#155529 = CARTESIAN_POINT('Ctrl Pts',(-7.63837808621904,-14.4087556909408,
119.554648862916)) ;
#155530 = CARTESIAN_POINT('Ctrl Pts',(-7.71218191587185,-14.4087557009118,
119.530417779298)) ;
#155531 = CARTESIAN_POINT('Ctrl Pts',(-7.78598574552467,-14.4087557108828,
119.506186695679)) ;
#155532 = CARTESIAN_POINT('Ctrl Pts',(-7.7909526868081,-14.4829720772946,
119.521315196541)) ;
#155533 = CARTESIAN_POINT('Ctrl Pts',(-7.79591962809152,-14.5571884437063,
119.536443697403)) ;
#155534 = CARTESIAN_POINT('Ctrl Pts',(-7.7221157984387,-14.5571884337353,
119.560674781022)) ;
#155535 = CARTESIAN_POINT('Ctrl Pts',(-7.64831196878589,-14.5571884237643,
119.58490586464)) ;
#155536 = CARTESIAN_POINT('Ctrl Pts',(-7.64334502750247,-14.4829720573525,
119.569777363778)) ;
#155537 = CARTESIAN_POINT('Ctrl Pts',(-7.56338289868114,-14.5039687036518,
119.290821303275)) ;
#155538 = CARTESIAN_POINT('Ctrl Pts',(-7.56472425461539,-14.4281793222941,
119.294906858056)) ;
#155539 = CARTESIAN_POINT('Ctrl Pts',(-7.63852808138411,-14.4281793198172,
119.270675765653)) ;
#155540 = CARTESIAN_POINT('Ctrl Pts',(-7.71233190815282,-14.4281793173403,
119.24644467325)) ;
#155541 = CARTESIAN_POINT('Ctrl Pts',(-7.71099055221857,-14.503968698698,
119.242359118469)) ;
#155542 = CARTESIAN_POINT('Ctrl Pts',(-7.7096491962843,-14.5797580800556,
119.238273563689)) ;
#155543 = CARTESIAN_POINT('Ctrl Pts',(-7.63584536951559,-14.5797580825325,
119.262504656092)) ;
#155544 = CARTESIAN_POINT('Ctrl Pts',(-7.56204154274688,-14.5797580850095,
119.286735748495)) ;
#155545 = CARTESIAN_POINT('Ctrl Pts',(-7.56338289868114,-14.5039687036518,
119.290821303275)) ;
#155546 = CARTESIAN_POINT('Ctrl Pts',(-7.48437547453331,-14.4466173797893,
119.014508165448)) ;
#155547 = CARTESIAN_POINT('Ctrl Pts',(-7.49197302414555,-14.3747219587681,
119.037649076942)) ;
#155548 = CARTESIAN_POINT('Ctrl Pts',(-7.56577684864369,-14.3747219386736,
119.013417977623)) ;
#155549 = CARTESIAN_POINT('Ctrl Pts',(-7.63958067314183,-14.3747219185791,
118.989186878304)) ;
#155550 = CARTESIAN_POINT('Ctrl Pts',(-7.63198312352959,-14.4466173396002,
118.966045966811)) ;
#155551 = CARTESIAN_POINT('Ctrl Pts',(-7.62438557391735,-14.5185127606213,
118.942905055318)) ;
#155552 = CARTESIAN_POINT('Ctrl Pts',(-7.55058174941921,-14.5185127807159,
118.967136154636)) ;
#155553 = CARTESIAN_POINT('Ctrl Pts',(-7.47677792492107,-14.5185128008104,
118.991367253955)) ;
#155554 = CARTESIAN_POINT('Ctrl Pts',(-7.48437547453331,-14.4466173797893,
119.014508165448)) ;
#155555 = CARTESIAN_POINT('Ctrl Pts',(-7.41403834460529,-14.3162716014842,
118.764955621569)) ;
#155556 = CARTESIAN_POINT('Ctrl Pts',(-7.42728841454722,-14.2533730380978,
118.805313198086)) ;
#155557 = CARTESIAN_POINT('Ctrl Pts',(-7.50109223966777,-14.2533729987048,
118.781082100663)) ;
#155558 = CARTESIAN_POINT('Ctrl Pts',(-7.57489606478832,-14.2533729593119,
118.75685100324)) ;
#155559 = CARTESIAN_POINT('Ctrl Pts',(-7.56164599484638,-14.3162715226984,
118.716493426723)) ;
#155560 = CARTESIAN_POINT('Ctrl Pts',(-7.54839592490445,-14.3791700860849,
118.676135850206)) ;
#155561 = CARTESIAN_POINT('Ctrl Pts',(-7.4745920997839,-14.3791701254778,
118.700366947629)) ;
#155562 = CARTESIAN_POINT('Ctrl Pts',(-7.40078827466335,-14.3791701648707,
118.724598045051)) ;
#155563 = CARTESIAN_POINT('Ctrl Pts',(-7.41403834460529,-14.3162716014842,
118.764955621569)) ;
#155564 = CARTESIAN_POINT('Ctrl Pts',(-7.35704039989976,-14.1214968775469,
118.555885778132)) ;
#155565 = CARTESIAN_POINT('Ctrl Pts',(-7.37502288865875,-14.0721057771866,
118.610657538943)) ;
#155566 = CARTESIAN_POINT('Ctrl Pts',(-7.44882671608949,-14.0721057178665,
118.586426448556)) ;
#155567 = CARTESIAN_POINT('Ctrl Pts',(-7.52263054352023,-14.0721056585463,
118.56219535817)) ;
#155568 = CARTESIAN_POINT('Ctrl Pts',(-7.50464805476125,-14.1214967589066,
118.507423597359)) ;
#155569 = CARTESIAN_POINT('Ctrl Pts',(-7.48666556600226,-14.170887859267,
118.452651836549)) ;
#155570 = CARTESIAN_POINT('Ctrl Pts',(-7.41286173857152,-14.1708879185871,
118.476882926935)) ;
#155571 = CARTESIAN_POINT('Ctrl Pts',(-7.33905791114077,-14.1708879779072,
118.501114017322)) ;
#155572 = CARTESIAN_POINT('Ctrl Pts',(-7.35704039989976,-14.1214968775469,
118.555885778132)) ;
#155573 = CARTESIAN_POINT('Ctrl Pts',(-7.31852311276589,-13.8749956323593,
118.402954989973)) ;
#155574 = CARTESIAN_POINT('Ctrl Pts',(-7.33995787032347,-13.8427423803111,
118.46824180468)) ;
#155575 = CARTESIAN_POINT('Ctrl Pts',(-7.4137617022352,-13.8427423020325,
118.444010727942)) ;
#155576 = CARTESIAN_POINT('Ctrl Pts',(-7.48756553414692,-13.8427422237539,
118.419779651204)) ;
#155577 = CARTESIAN_POINT('Ctrl Pts',(-7.46613077658935,-13.8749954758022,
118.354492836497)) ;
#155578 = CARTESIAN_POINT('Ctrl Pts',(-7.44469601903177,-13.9072487278505,
118.28920602179)) ;
#155579 = CARTESIAN_POINT('Ctrl Pts',(-7.37089218712003,-13.907248806129,
118.313437098528)) ;
#155580 = CARTESIAN_POINT('Ctrl Pts',(-7.2970883552083,-13.9072488844076,
118.337668175266)) ;
#155581 = CARTESIAN_POINT('Ctrl Pts',(-7.31852311276589,-13.8749956323593,
118.402954989973)) ;
#155582 = CARTESIAN_POINT('Ctrl Pts',(-7.30231103568058,-13.5974682752699,
118.318202627209)) ;
#155583 = CARTESIAN_POINT('Ctrl Pts',(-7.32564071440279,-13.5845442893725,
118.389261066145)) ;
#155584 = CARTESIAN_POINT('Ctrl Pts',(-7.39944455296119,-13.584544198723,
118.365030009652)) ;
#155585 = CARTESIAN_POINT('Ctrl Pts',(-7.4732483915196,-13.5845441080735,
118.340798953159)) ;
#155586 = CARTESIAN_POINT('Ctrl Pts',(-7.4499187127974,-13.597468093971,118.269740514223)) ;
#155587 = CARTESIAN_POINT('Ctrl Pts',(-7.42658903407519,-13.6103920798684,
118.198682075287)) ;
#155588 = CARTESIAN_POINT('Ctrl Pts',(-7.35278519551678,-13.6103921705179,
118.22291313178)) ;
#155589 = CARTESIAN_POINT('Ctrl Pts',(-7.27898135695837,-13.6103922611673,
118.247144188274)) ;
#155590 = CARTESIAN_POINT('Ctrl Pts',(-7.30231103568058,-13.5974682752699,
118.318202627209)) ;
#155591 = CARTESIAN_POINT('Ctrl Pts',(-7.30987663537963,-13.3070931499256,
118.305860700972)) ;
#155592 = CARTESIAN_POINT('Ctrl Pts',(-7.33344423912749,-13.3144232873773,
118.377643821243)) ;
#155593 = CARTESIAN_POINT('Ctrl Pts',(-7.40724808549206,-13.3144231909102,
118.353412788526)) ;
#155594 = CARTESIAN_POINT('Ctrl Pts',(-7.48105193185662,-13.314423094443,
118.329181755809)) ;
#155595 = CARTESIAN_POINT('Ctrl Pts',(-7.45748432810876,-13.3070929569913,
118.257398635538)) ;
#155596 = CARTESIAN_POINT('Ctrl Pts',(-7.43391672436091,-13.2997628195396,
118.185615515268)) ;
#155597 = CARTESIAN_POINT('Ctrl Pts',(-7.36011287799634,-13.2997629160068,
118.209846547985)) ;
#155598 = CARTESIAN_POINT('Ctrl Pts',(-7.28630903163177,-13.2997630124739,
118.234077580702)) ;
#155599 = CARTESIAN_POINT('Ctrl Pts',(-7.30987663537963,-13.3070931499256,
118.305860700972)) ;
#155600 = CARTESIAN_POINT('Ctrl Pts',(-7.34175942853511,-13.0233508116479,
118.36742076646)) ;
#155601 = CARTESIAN_POINT('Ctrl Pts',(-7.36387123793272,-13.0505014151777,
118.434769772124)) ;
#155602 = CARTESIAN_POINT('Ctrl Pts',(-7.43767509276429,-13.0505013202395,
118.410538765196)) ;
#155603 = CARTESIAN_POINT('Ctrl Pts',(-7.51147894759584,-13.0505012253013,
118.386307758269)) ;
#155604 = CARTESIAN_POINT('Ctrl Pts',(-7.48936713819821,-13.0233506217714,
118.318958752604)) ;
#155605 = CARTESIAN_POINT('Ctrl Pts',(-7.4672553288006,-12.9962000182415,
118.25160974694)) ;
#155606 = CARTESIAN_POINT('Ctrl Pts',(-7.39345147396905,-12.9962001131797,
118.275840753868)) ;
#155607 = CARTESIAN_POINT('Ctrl Pts',(-7.31964761913749,-12.996200208118,
118.300071760795)) ;
#155608 = CARTESIAN_POINT('Ctrl Pts',(-7.34175942853511,-13.0233508116479,
118.36742076646)) ;
#155609 = CARTESIAN_POINT('Ctrl Pts',(-7.39618528009665,-12.7688607554056,
118.497769967232)) ;
#155610 = CARTESIAN_POINT('Ctrl Pts',(-7.41526264461118,-12.8138186885295,
118.55587654345)) ;
#155611 = CARTESIAN_POINT('Ctrl Pts',(-7.48906650749834,-12.8138186042271,
118.531645561058)) ;
#155612 = CARTESIAN_POINT('Ctrl Pts',(-7.56287037038549,-12.8138185199248,
118.507414578666)) ;
#155613 = CARTESIAN_POINT('Ctrl Pts',(-7.54379300587095,-12.7688605868009,
118.449308002449)) ;
#155614 = CARTESIAN_POINT('Ctrl Pts',(-7.52471564135643,-12.723902653677,
118.391201426231)) ;
#155615 = CARTESIAN_POINT('Ctrl Pts',(-7.45091177846927,-12.7239027379794,
118.415432408623)) ;
#155616 = CARTESIAN_POINT('Ctrl Pts',(-7.37710791558212,-12.7239028222818,
118.439663391015)) ;
#155617 = CARTESIAN_POINT('Ctrl Pts',(-7.39618528009665,-12.7688607554056,
118.497769967232)) ;
#155618 = CARTESIAN_POINT('Ctrl Pts',(-7.47020228300154,-12.5604071436069,
118.687726339368)) ;
#155619 = CARTESIAN_POINT('Ctrl Pts',(-7.4848744582239,-12.6199846631104,
118.732415419821)) ;
#155620 = CARTESIAN_POINT('Ctrl Pts',(-7.5586783279789,-12.6199845970407,
118.708184458347)) ;
#155621 = CARTESIAN_POINT('Ctrl Pts',(-7.63248219773388,-12.6199845309711,
118.683953496874)) ;
#155622 = CARTESIAN_POINT('Ctrl Pts',(-7.61781002251153,-12.5604070114677,
118.639264416421)) ;
#155623 = CARTESIAN_POINT('Ctrl Pts',(-7.60313784728917,-12.5008294919642,
118.594575335968)) ;
#155624 = CARTESIAN_POINT('Ctrl Pts',(-7.52933397753417,-12.5008295580339,
118.618806297441)) ;
#155625 = CARTESIAN_POINT('Ctrl Pts',(-7.45553010777918,-12.5008296241035,
118.643037258915)) ;
#155626 = CARTESIAN_POINT('Ctrl Pts',(-7.47020228300154,-12.5604071436069,
118.687726339368)) ;
#155627 = CARTESIAN_POINT('Ctrl Pts',(-7.55906350518853,-12.4137261008746,
118.922952330464)) ;
#155628 = CARTESIAN_POINT('Ctrl Pts',(-7.56828647533281,-12.4836322376362,
118.951044011495)) ;
#155629 = CARTESIAN_POINT('Ctrl Pts',(-7.64209034991756,-12.4836321960017,
118.926813064733)) ;
#155630 = CARTESIAN_POINT('Ctrl Pts',(-7.71589422450231,-12.4836321543672,
118.90258211797)) ;
#155631 = CARTESIAN_POINT('Ctrl Pts',(-7.70667125435802,-12.4137260176056,
118.874490436939)) ;
#155632 = CARTESIAN_POINT('Ctrl Pts',(-7.69744828421375,-12.343819880844,
118.846398755907)) ;
#155633 = CARTESIAN_POINT('Ctrl Pts',(-7.623644409629,-12.3438199224785,118.87062970267)) ;
#155634 = CARTESIAN_POINT('Ctrl Pts',(-7.54984053504425,-12.343819964113,
118.894860649433)) ;
#155635 = CARTESIAN_POINT('Ctrl Pts',(-7.55906350518853,-12.4137261008746,
118.922952330464)) ;
#155636 = CARTESIAN_POINT('Ctrl Pts',(-7.65717245038672,-12.3387040702925,
119.186368813652)) ;
#155637 = CARTESIAN_POINT('Ctrl Pts',(-7.66029208335573,-12.4139513070211,
119.195870714419)) ;
#155638 = CARTESIAN_POINT('Ctrl Pts',(-7.7340959603037,-12.4139512934304,
119.171639774854)) ;
#155639 = CARTESIAN_POINT('Ctrl Pts',(-7.80789983725165,-12.4139512798397,
119.147408835289)) ;
#155640 = CARTESIAN_POINT('Ctrl Pts',(-7.80478020428264,-12.3387040431111,
119.137906934522)) ;
#155641 = CARTESIAN_POINT('Ctrl Pts',(-7.80166057131362,-12.2634568063825,
119.128405033755)) ;
#155642 = CARTESIAN_POINT('Ctrl Pts',(-7.72785669436566,-12.2634568199732,
119.15263597332)) ;
#155643 = CARTESIAN_POINT('Ctrl Pts',(-7.65405281741769,-12.2634568335639,
119.176866912885)) ;
#155644 = CARTESIAN_POINT('Ctrl Pts',(-7.65717245038672,-12.3387040702925,
119.186368813652)) ;
#155645 = CARTESIAN_POINT('Ctrl Pts',(-7.75884035692309,-12.3410592400664,
119.460451576393)) ;
#155646 = CARTESIAN_POINT('Ctrl Pts',(-7.75560281377236,-12.4162542159503,
119.450590544401)) ;
#155647 = CARTESIAN_POINT('Ctrl Pts',(-7.8294066902323,-12.4162542313705,
119.426359603349)) ;
#155648 = CARTESIAN_POINT('Ctrl Pts',(-7.90321056669223,-12.4162542467908,
119.402128662298)) ;
#155649 = CARTESIAN_POINT('Ctrl Pts',(-7.90644810984295,-12.3410592709069,
119.41198969429)) ;
#155650 = CARTESIAN_POINT('Ctrl Pts',(-7.90968565299367,-12.265864295023,
119.421850726283)) ;
#155651 = CARTESIAN_POINT('Ctrl Pts',(-7.83588177653374,-12.2658642796027,
119.446081667334)) ;
#155652 = CARTESIAN_POINT('Ctrl Pts',(-7.76207790007381,-12.2658642641825,
119.470312608385)) ;
#155653 = CARTESIAN_POINT('Ctrl Pts',(-7.75884035692309,-12.3410592400664,
119.460451576393)) ;
#155654 = CARTESIAN_POINT('Ctrl Pts',(-7.85654736634483,-12.4205041979803,
119.722651987663)) ;
#155655 = CARTESIAN_POINT('Ctrl Pts',(-7.84721586315474,-12.4902644552577,
119.694229736606)) ;
#155656 = CARTESIAN_POINT('Ctrl Pts',(-7.92101973652683,-12.4902644973908,
119.66999878615)) ;
#155657 = CARTESIAN_POINT('Ctrl Pts',(-7.99482360989893,-12.4902645395239,
119.645767835693)) ;
#155658 = CARTESIAN_POINT('Ctrl Pts',(-8.00415511308902,-12.4205042822464,
119.674190086751)) ;
#155659 = CARTESIAN_POINT('Ctrl Pts',(-8.0134866162791,-12.350744024969,119.702612337808)) ;
#155660 = CARTESIAN_POINT('Ctrl Pts',(-7.939682742907,-12.3507439828359,119.726843288264)) ;
#155661 = CARTESIAN_POINT('Ctrl Pts',(-7.86587886953491,-12.3507439407028,
119.751074238721)) ;
#155662 = CARTESIAN_POINT('Ctrl Pts',(-7.85654736634483,-12.4205041979803,
119.722651987663)) ;
#155663 = CARTESIAN_POINT('Ctrl Pts',(-7.94481318053513,-12.5715202421064,
119.956000118428)) ;
#155664 = CARTESIAN_POINT('Ctrl Pts',(-7.93003972839049,-12.6308413998765,
119.911002568843)) ;
#155665 = CARTESIAN_POINT('Ctrl Pts',(-8.00384359633958,-12.6308414639116,
119.886771601869)) ;
#155666 = CARTESIAN_POINT('Ctrl Pts',(-8.07764746428867,-12.6308415279467,
119.862540634895)) ;
#155667 = CARTESIAN_POINT('Ctrl Pts',(-8.09242091643331,-12.5715203701767,
119.90753818448)) ;
#155668 = CARTESIAN_POINT('Ctrl Pts',(-8.10719436857796,-12.5121992124066,
119.952535734065)) ;
#155669 = CARTESIAN_POINT('Ctrl Pts',(-8.03339050062888,-12.5121991483715,
119.976766701039)) ;
#155670 = CARTESIAN_POINT('Ctrl Pts',(-7.95958663267978,-12.5121990843364,
120.000997668012)) ;
#155671 = CARTESIAN_POINT('Ctrl Pts',(-7.94481318053513,-12.5715202421064,
119.956000118428)) ;
#155672 = CARTESIAN_POINT('Ctrl Pts',(-8.01771408381364,-12.7831706996134,
120.142578445181)) ;
#155673 = CARTESIAN_POINT('Ctrl Pts',(-7.99856257426153,-12.827803906149,
120.084246039043)) ;
#155674 = CARTESIAN_POINT('Ctrl Pts',(-8.07236643520165,-12.8278039851649,
120.060015050721)) ;
#155675 = CARTESIAN_POINT('Ctrl Pts',(-8.14617029614177,-12.8278040641808,
120.035784062399)) ;
#155676 = CARTESIAN_POINT('Ctrl Pts',(-8.16532180569389,-12.7831708576452,
120.094116468536)) ;
#155677 = CARTESIAN_POINT('Ctrl Pts',(-8.18447331524599,-12.7385376511096,
120.152448874673)) ;
#155678 = CARTESIAN_POINT('Ctrl Pts',(-8.11066945430587,-12.7385375720937,
120.176679862995)) ;
#155679 = CARTESIAN_POINT('Ctrl Pts',(-8.03686559336574,-12.7385374930778,
120.200910851318)) ;
#155680 = CARTESIAN_POINT('Ctrl Pts',(-8.01771408381364,-12.7831706996134,
120.142578445181)) ;
#155681 = CARTESIAN_POINT('Ctrl Pts',(-8.07085503105618,-13.0400861903177,
120.268992723008)) ;
#155682 = CARTESIAN_POINT('Ctrl Pts',(-8.04869796956498,-13.0668491450616,
120.201505890507)) ;
#155683 = CARTESIAN_POINT('Ctrl Pts',(-8.12250182275097,-13.0668492312408,
120.177274878567)) ;
#155684 = CARTESIAN_POINT('Ctrl Pts',(-8.19630567593696,-13.06684931742,120.153043866627)) ;
#155685 = CARTESIAN_POINT('Ctrl Pts',(-8.21846273742817,-13.0400863626762,
120.220530699128)) ;
#155686 = CARTESIAN_POINT('Ctrl Pts',(-8.24061979891935,-13.0133234079323,
120.288017531629)) ;
#155687 = CARTESIAN_POINT('Ctrl Pts',(-8.16681594573337,-13.0133233217531,
120.312248543569)) ;
#155688 = CARTESIAN_POINT('Ctrl Pts',(-8.09301209254737,-13.0133232355738,
120.336479555509)) ;
#155689 = CARTESIAN_POINT('Ctrl Pts',(-8.07085503105618,-13.0400861903177,
120.268992723008)) ;
#155690 = CARTESIAN_POINT('Ctrl Pts',(-8.1012449479731,-13.3242719779506,
120.326083671067)) ;
#155691 = CARTESIAN_POINT('Ctrl Pts',(-8.0776667011033,-13.3312338876365,
120.254268137088)) ;
#155692 = CARTESIAN_POINT('Ctrl Pts',(-8.15147054661026,-13.3312339727679,
120.230037101759)) ;
#155693 = CARTESIAN_POINT('Ctrl Pts',(-8.22527439211721,-13.3312340578993,
120.20580606643)) ;
#155694 = CARTESIAN_POINT('Ctrl Pts',(-8.24885263898701,-13.3242721482135,
120.277621600409)) ;
#155695 = CARTESIAN_POINT('Ctrl Pts',(-8.2724308858568,-13.3173102385276,
120.349437134388)) ;
#155696 = CARTESIAN_POINT('Ctrl Pts',(-8.19862704034984,-13.3173101533962,
120.373668169717)) ;
#155697 = CARTESIAN_POINT('Ctrl Pts',(-8.12482319484289,-13.3173100682647,
120.397899205046)) ;
#155698 = CARTESIAN_POINT('Ctrl Pts',(-8.1012449479731,-13.3242719779506,
120.326083671067)) ;
#155699 = CARTESIAN_POINT('Ctrl Pts',(-8.10739844779683,-13.6152878377403,
120.309341878199)) ;
#155700 = CARTESIAN_POINT('Ctrl Pts',(-8.08408919078993,-13.601941852712,
120.238345643802)) ;
#155701 = CARTESIAN_POINT('Ctrl Pts',(-8.15789302956165,-13.6019419294696,
120.214114587959)) ;
#155702 = CARTESIAN_POINT('Ctrl Pts',(-8.23169686833337,-13.6019420062272,
120.189883532115)) ;
#155703 = CARTESIAN_POINT('Ctrl Pts',(-8.25500612534027,-13.6152879912555,
120.260879766512)) ;
#155704 = CARTESIAN_POINT('Ctrl Pts',(-8.27831538234716,-13.6286339762838,
120.33187600091)) ;
#155705 = CARTESIAN_POINT('Ctrl Pts',(-8.20451154357544,-13.6286338995262,
120.356107056753)) ;
#155706 = CARTESIAN_POINT('Ctrl Pts',(-8.13070770480371,-13.6286338227686,
120.380338112597)) ;
#155707 = CARTESIAN_POINT('Ctrl Pts',(-8.10739844779683,-13.6152878377403,
120.309341878199)) ;
#155708 = CARTESIAN_POINT('Ctrl Pts',(-8.08962004095609,-13.8920338673762,
120.219720905231)) ;
#155709 = CARTESIAN_POINT('Ctrl Pts',(-8.06825077036232,-13.8593453805719,
120.154633556283)) ;
#155710 = CARTESIAN_POINT('Ctrl Pts',(-8.14205460400106,-13.8593454436439,
120.130402484805)) ;
#155711 = CARTESIAN_POINT('Ctrl Pts',(-8.21585843763983,-13.859345506716,
120.106171413327)) ;
#155712 = CARTESIAN_POINT('Ctrl Pts',(-8.23722770823361,-13.8920339935203,
120.171258762276)) ;
#155713 = CARTESIAN_POINT('Ctrl Pts',(-8.2585969788274,-13.9247224803246,
120.236346111225)) ;
#155714 = CARTESIAN_POINT('Ctrl Pts',(-8.18479314518863,-13.9247224172525,
120.260577182702)) ;
#155715 = CARTESIAN_POINT('Ctrl Pts',(-8.11098931154989,-13.9247223541804,
120.28480825418)) ;
#155716 = CARTESIAN_POINT('Ctrl Pts',(-8.08962004095609,-13.8920338673762,
120.219720905231)) ;
#155717 = CARTESIAN_POINT('Ctrl Pts',(-8.05001723486067,-14.1346381572922,
120.063660745971)) ;
#155718 = CARTESIAN_POINT('Ctrl Pts',(-8.03211395972011,-14.0849615058488,
120.009130259783)) ;
#155719 = CARTESIAN_POINT('Ctrl Pts',(-8.10591779010873,-14.0849615523416,
119.984899178406)) ;
#155720 = CARTESIAN_POINT('Ctrl Pts',(-8.17972162049735,-14.0849615988343,
119.960668097028)) ;
#155721 = CARTESIAN_POINT('Ctrl Pts',(-8.19762489563791,-14.1346382502777,
120.015198583216)) ;
#155722 = CARTESIAN_POINT('Ctrl Pts',(-8.21552817077847,-14.1843149017211,
120.069729069404)) ;
#155723 = CARTESIAN_POINT('Ctrl Pts',(-8.14172434038985,-14.1843148552283,
120.093960150781)) ;
#155724 = CARTESIAN_POINT('Ctrl Pts',(-8.06792051000123,-14.1843148087356,
120.118191232158)) ;
#155725 = CARTESIAN_POINT('Ctrl Pts',(-8.05001723486067,-14.1346381572922,
120.063660745971)) ;
#155726 = CARTESIAN_POINT('Ctrl Pts',(-7.992024762362,-14.3262307223465,119.85152566265)) ;
#155727 = CARTESIAN_POINT('Ctrl Pts',(-7.97887798500129,-14.263101480961,
119.81148270107)) ;
#155728 = CARTESIAN_POINT('Ctrl Pts',(-8.05268181432158,-14.2631015098285,
119.787251616438)) ;
#155729 = CARTESIAN_POINT('Ctrl Pts',(-8.12648564364185,-14.263101538696,
119.763020531807)) ;
#155730 = CARTESIAN_POINT('Ctrl Pts',(-8.13963242100255,-14.3262307800815,
119.803063493387)) ;
#155731 = CARTESIAN_POINT('Ctrl Pts',(-8.15277919836325,-14.3893600214671,
119.843106454968)) ;
#155732 = CARTESIAN_POINT('Ctrl Pts',(-8.07897536904298,-14.3893599925996,
119.867337539599)) ;
#155733 = CARTESIAN_POINT('Ctrl Pts',(-8.00517153972269,-14.3893599637321,
119.89156862423)) ;
#155734 = CARTESIAN_POINT('Ctrl Pts',(-7.992024762362,-14.3262307223465,119.85152566265)) ;
#155735 = CARTESIAN_POINT('Ctrl Pts',(-7.92087420413947,-14.4523301137118,
119.599430244914)) ;
#155736 = CARTESIAN_POINT('Ctrl Pts',(-7.913407539792,-14.380300846747,119.576687990937)) ;
#155737 = CARTESIAN_POINT('Ctrl Pts',(-7.98721136957771,-14.3803008602231,
119.552456907723)) ;
#155738 = CARTESIAN_POINT('Ctrl Pts',(-8.06101519936343,-14.3803008736991,
119.52822582451)) ;
#155739 = CARTESIAN_POINT('Ctrl Pts',(-8.0684818637109,-14.4523301406639,
119.550968078487)) ;
#155740 = CARTESIAN_POINT('Ctrl Pts',(-8.07594852805837,-14.5243594076287,
119.573710332464)) ;
#155741 = CARTESIAN_POINT('Ctrl Pts',(-8.00214469827266,-14.5243593941527,
119.597941415678)) ;
#155742 = CARTESIAN_POINT('Ctrl Pts',(-7.92834086848694,-14.5243593806767,
119.622172498891)) ;
#155743 = CARTESIAN_POINT('Ctrl Pts',(-7.92087420413947,-14.4523301137118,
119.599430244914)) ;
#155744 = CARTESIAN_POINT('Ctrl Pts',(-7.84204196997817,-14.5048566464616,
119.323854472488)) ;
#155745 = CARTESIAN_POINT('Ctrl Pts',(-7.84080211163026,-14.4290505733795,
119.320078064726)) ;
#155746 = CARTESIAN_POINT('Ctrl Pts',(-7.91460594349901,-14.4290505742608,
119.295846987857)) ;
#155747 = CARTESIAN_POINT('Ctrl Pts',(-7.98840977536776,-14.429050575142,
119.271615910988)) ;
#155748 = CARTESIAN_POINT('Ctrl Pts',(-7.98964963371567,-14.5048566482241,
119.27539231875)) ;
#155749 = CARTESIAN_POINT('Ctrl Pts',(-7.99088949206357,-14.5806627213062,
119.279168726512)) ;
#155750 = CARTESIAN_POINT('Ctrl Pts',(-7.91708566019482,-14.580662720425,
119.303399803381)) ;
#155751 = CARTESIAN_POINT('Ctrl Pts',(-7.84328182832607,-14.5806627195438,
119.32763088025)) ;
#155752 = CARTESIAN_POINT('Ctrl Pts',(-7.84204196997817,-14.5048566464616,
119.323854472488)) ;
#155753 = CARTESIAN_POINT('Ctrl Pts',(-7.76186601911956,-14.4792282215674,
119.044096181178)) ;
#155754 = CARTESIAN_POINT('Ctrl Pts',(-7.76695821637415,-14.405096385773,
119.059606192928)) ;
#155755 = CARTESIAN_POINT('Ctrl Pts',(-7.84076205141397,-14.4050963789129,
119.035375125717)) ;
#155756 = CARTESIAN_POINT('Ctrl Pts',(-7.91456588645379,-14.4050963720528,
119.011144058507)) ;
#155757 = CARTESIAN_POINT('Ctrl Pts',(-7.9094736891992,-14.4792282078472,
118.995634046757)) ;
#155758 = CARTESIAN_POINT('Ctrl Pts',(-7.90438149194462,-14.5533600436416,
118.980124035008)) ;
#155759 = CARTESIAN_POINT('Ctrl Pts',(-7.8305776569048,-14.5533600505017,
119.004355102218)) ;
#155760 = CARTESIAN_POINT('Ctrl Pts',(-7.75677382186498,-14.5533600573618,
119.028586169429)) ;
#155761 = CARTESIAN_POINT('Ctrl Pts',(-7.76186601911956,-14.4792282215674,
119.044096181178)) ;
#155762 = CARTESIAN_POINT('Ctrl Pts',(-7.68732567425835,-14.3776591931245,
118.781625479166)) ;
#155763 = CARTESIAN_POINT('Ctrl Pts',(-7.69836352724098,-14.3105071713144,
118.815244998788)) ;
#155764 = CARTESIAN_POINT('Ctrl Pts',(-7.77216736523883,-14.3105071612984,
118.791013940587)) ;
#155765 = CARTESIAN_POINT('Ctrl Pts',(-7.84597120323668,-14.3105071512824,
118.766782882386)) ;
#155766 = CARTESIAN_POINT('Ctrl Pts',(-7.83493335025406,-14.3776591730925,
118.733163362765)) ;
#155767 = CARTESIAN_POINT('Ctrl Pts',(-7.82389549727142,-14.4448111949025,
118.699543843143)) ;
#155768 = CARTESIAN_POINT('Ctrl Pts',(-7.75009165927358,-14.4448112049185,
118.723774901344)) ;
#155769 = CARTESIAN_POINT('Ctrl Pts',(-7.67628782127572,-14.4448112149345,
118.748005959545)) ;
#155770 = CARTESIAN_POINT('Ctrl Pts',(-7.68732567425835,-14.3776591931245,
118.781625479166)) ;
#155771 = CARTESIAN_POINT('Ctrl Pts',(-7.62415597339361,-14.2073582471136,
118.553754081591)) ;
#155772 = CARTESIAN_POINT('Ctrl Pts',(-7.64035528068796,-14.1519959883529,
118.603094558107)) ;
#155773 = CARTESIAN_POINT('Ctrl Pts',(-7.71415912134421,-14.1519959791231,
118.578863508004)) ;
#155774 = CARTESIAN_POINT('Ctrl Pts',(-7.78796296200047,-14.1519959698933,
118.5546324579)) ;
#155775 = CARTESIAN_POINT('Ctrl Pts',(-7.77176365470613,-14.207358228654,
118.505291981383)) ;
#155776 = CARTESIAN_POINT('Ctrl Pts',(-7.75556434741179,-14.2627204874147,
118.455951504867)) ;
#155777 = CARTESIAN_POINT('Ctrl Pts',(-7.68176050675553,-14.2627204966445,
118.48018255497)) ;
#155778 = CARTESIAN_POINT('Ctrl Pts',(-7.60795666609927,-14.2627205058743,
118.504413605074)) ;
#155779 = CARTESIAN_POINT('Ctrl Pts',(-7.62415597339361,-14.2073582471136,
118.553754081591)) ;
#155780 = CARTESIAN_POINT('Ctrl Pts',(-7.57772822356053,-13.980463190757,
118.376876023582)) ;
#155781 = CARTESIAN_POINT('Ctrl Pts',(-7.59792777189917,-13.9408606598198,
118.438400588762)) ;
#155782 = CARTESIAN_POINT('Ctrl Pts',(-7.67173161439476,-13.9408606539983,
118.41416954426)) ;
#155783 = CARTESIAN_POINT('Ctrl Pts',(-7.74553545689033,-13.9408606481768,
118.389938499759)) ;
#155784 = CARTESIAN_POINT('Ctrl Pts',(-7.72533590855169,-13.9804631791139,
118.328413934579)) ;
#155785 = CARTESIAN_POINT('Ctrl Pts',(-7.70513636021303,-14.0200657100511,
118.266889369399)) ;
#155786 = CARTESIAN_POINT('Ctrl Pts',(-7.63133251771746,-14.0200657158726,
118.2911204139)) ;
#155787 = CARTESIAN_POINT('Ctrl Pts',(-7.55752867522188,-14.0200657216941,
118.315351458402)) ;
#155788 = CARTESIAN_POINT('Ctrl Pts',(-7.57772822356053,-13.980463190757,
118.376876023582)) ;
#155789 = CARTESIAN_POINT('Ctrl Pts',(-7.55211423680401,-13.7134648384933,
118.263415580786)) ;
#155790 = CARTESIAN_POINT('Ctrl Pts',(-7.57486615867029,-13.6924464842837,
118.332714263813)) ;
#155791 = CARTESIAN_POINT('Ctrl Pts',(-7.64867000205498,-13.6924464826294,
118.308483222019)) ;
#155792 = CARTESIAN_POINT('Ctrl Pts',(-7.72247384543967,-13.6924464809751,
118.284252180226)) ;
#155793 = CARTESIAN_POINT('Ctrl Pts',(-7.69972192357337,-13.7134648351847,
118.214953497199)) ;
#155794 = CARTESIAN_POINT('Ctrl Pts',(-7.67697000170707,-13.7344831893942,
118.145654814172)) ;
#155795 = CARTESIAN_POINT('Ctrl Pts',(-7.60316615832239,-13.7344831910485,
118.169885855965)) ;
#155796 = CARTESIAN_POINT('Ctrl Pts',(-7.5293623149377,-13.7344831927028,
118.194116897759)) ;
#155797 = CARTESIAN_POINT('Ctrl Pts',(-7.55211423680401,-13.7134648384933,
118.263415580786)) ;
#155798 = CARTESIAN_POINT('Ctrl Pts',(-7.54988396928805,-13.4252028157263,
118.221162235282)) ;
#155799 = CARTESIAN_POINT('Ctrl Pts',(-7.57355949818283,-13.4242817506044,
118.293274076228)) ;
#155800 = CARTESIAN_POINT('Ctrl Pts',(-7.64736334166818,-13.4242817523867,
118.269043034742)) ;
#155801 = CARTESIAN_POINT('Ctrl Pts',(-7.72116718515352,-13.4242817541689,
118.244811993255)) ;
#155802 = CARTESIAN_POINT('Ctrl Pts',(-7.69749165625874,-13.4252028192908,
118.172700152308)) ;
#155803 = CARTESIAN_POINT('Ctrl Pts',(-7.67381612736396,-13.4261238844127,
118.100588311361)) ;
#155804 = CARTESIAN_POINT('Ctrl Pts',(-7.60001228387861,-13.4261238826305,
118.124819352848)) ;
#155805 = CARTESIAN_POINT('Ctrl Pts',(-7.52620844039326,-13.4261238808483,
118.149050394335)) ;
#155806 = CARTESIAN_POINT('Ctrl Pts',(-7.54988396928805,-13.4252028157263,
118.221162235282)) ;
#155807 = CARTESIAN_POINT('Ctrl Pts',(-7.57190400588021,-13.136660084581,
118.252804065339)) ;
#155808 = CARTESIAN_POINT('Ctrl Pts',(-7.59481029167102,-13.1558861878268,
118.322572915877)) ;
#155809 = CARTESIAN_POINT('Ctrl Pts',(-7.66861413481843,-13.1558861911127,
118.298341873361)) ;
#155810 = CARTESIAN_POINT('Ctrl Pts',(-7.74241797796585,-13.1558861943986,
118.274110830845)) ;
#155811 = CARTESIAN_POINT('Ctrl Pts',(-7.71951169217504,-13.1366600911528,
118.204341980307)) ;
#155812 = CARTESIAN_POINT('Ctrl Pts',(-7.69660540638423,-13.117433987907,
118.134573129769)) ;
#155813 = CARTESIAN_POINT('Ctrl Pts',(-7.62280156323682,-13.1174339846211,
118.158804172285)) ;
#155814 = CARTESIAN_POINT('Ctrl Pts',(-7.54899772008939,-13.1174339813352,
118.183035214801)) ;
#155815 = CARTESIAN_POINT('Ctrl Pts',(-7.57190400588021,-13.136660084581,
118.252804065339)) ;
#155816 = CARTESIAN_POINT('Ctrl Pts',(-7.61755830701388,-12.8674128564449,
118.356315160482)) ;
#155817 = CARTESIAN_POINT('Ctrl Pts',(-7.63804609281463,-12.9054690960976,
118.418717650288)) ;
#155818 = CARTESIAN_POINT('Ctrl Pts',(-7.71184993576395,-12.9054690982831,
118.394486607169)) ;
#155819 = CARTESIAN_POINT('Ctrl Pts',(-7.78565377871326,-12.9054691004687,
118.370255564049)) ;
#155820 = CARTESIAN_POINT('Ctrl Pts',(-7.7651659929125,-12.867412860816,118.307853074243)) ;
#155821 = CARTESIAN_POINT('Ctrl Pts',(-7.74467820711173,-12.8293566211633,
118.245450584436)) ;
#155822 = CARTESIAN_POINT('Ctrl Pts',(-7.67087436416242,-12.8293566189777,
118.269681627556)) ;
#155823 = CARTESIAN_POINT('Ctrl Pts',(-7.59707052121311,-12.8293566167922,
118.293912670675)) ;
#155824 = CARTESIAN_POINT('Ctrl Pts',(-7.61755830701388,-12.8674128564449,
118.356315160482)) ;
#155825 = CARTESIAN_POINT('Ctrl Pts',(-7.68406859821228,-12.6383938778605,
118.523453892796)) ;
#155826 = CARTESIAN_POINT('Ctrl Pts',(-7.70067567677603,-12.6924977231703,
118.574036374563)) ;
#155827 = CARTESIAN_POINT('Ctrl Pts',(-7.77447952014917,-12.6924977228183,
118.549805332734)) ;
#155828 = CARTESIAN_POINT('Ctrl Pts',(-7.84828336352231,-12.6924977224664,
118.525574290905)) ;
#155829 = CARTESIAN_POINT('Ctrl Pts',(-7.83167628495855,-12.6383938771567,
118.474991809139)) ;
#155830 = CARTESIAN_POINT('Ctrl Pts',(-7.8150692063948,-12.5842900318469,
118.424409327373)) ;
#155831 = CARTESIAN_POINT('Ctrl Pts',(-7.74126536302167,-12.5842900321988,
118.448640369202)) ;
#155832 = CARTESIAN_POINT('Ctrl Pts',(-7.66746151964852,-12.5842900325507,
118.47287141103)) ;
#155833 = CARTESIAN_POINT('Ctrl Pts',(-7.68406859821228,-12.6383938778605,
118.523453892796)) ;
#155834 = CARTESIAN_POINT('Ctrl Pts',(-7.76755837693475,-12.465038874388,
118.74228416299)) ;
#155835 = CARTESIAN_POINT('Ctrl Pts',(-7.77909394316923,-12.531326536537,
118.777419636573)) ;
#155836 = CARTESIAN_POINT('Ctrl Pts',(-7.85289778777235,-12.5313265339241,
118.753188598491)) ;
#155837 = CARTESIAN_POINT('Ctrl Pts',(-7.92670163237547,-12.5313265313111,
118.728957560409)) ;
#155838 = CARTESIAN_POINT('Ctrl Pts',(-7.91516606614098,-12.4650388691621,
118.693822086826)) ;
#155839 = CARTESIAN_POINT('Ctrl Pts',(-7.90363049990651,-12.3987512070131,
118.658686613243)) ;
#155840 = CARTESIAN_POINT('Ctrl Pts',(-7.82982665530339,-12.3987512096261,
118.682917651325)) ;
#155841 = CARTESIAN_POINT('Ctrl Pts',(-7.75602281070027,-12.398751212239,
118.707148689407)) ;
#155842 = CARTESIAN_POINT('Ctrl Pts',(-7.76755837693475,-12.465038874388,
118.74228416299)) ;
#155843 = CARTESIAN_POINT('Ctrl Pts',(-7.86272316977547,-12.3599344396702,
118.99669592537)) ;
#155844 = CARTESIAN_POINT('Ctrl Pts',(-7.86836420348592,-12.4336574817887,
119.013877604073)) ;
#155845 = CARTESIAN_POINT('Ctrl Pts',(-7.94216804997685,-12.4336574787988,
118.989646571741)) ;
#155846 = CARTESIAN_POINT('Ctrl Pts',(-8.01597189646776,-12.4336574758088,
118.965415539409)) ;
#155847 = CARTESIAN_POINT('Ctrl Pts',(-8.01033086275732,-12.3599344336902,
118.948233860705)) ;
#155848 = CARTESIAN_POINT('Ctrl Pts',(-8.00468982904687,-12.2862113915716,
118.931052182002)) ;
#155849 = CARTESIAN_POINT('Ctrl Pts',(-7.93088598255596,-12.2862113945616,
118.955283214334)) ;
#155850 = CARTESIAN_POINT('Ctrl Pts',(-7.85708213606502,-12.2862113975516,
118.979514246666)) ;
#155851 = CARTESIAN_POINT('Ctrl Pts',(-7.86272316977547,-12.3599344396702,
118.99669592537)) ;
#155852 = CARTESIAN_POINT('Ctrl Pts',(-7.96381251944024,-12.3306429195518,
119.269059347859)) ;
#155853 = CARTESIAN_POINT('Ctrl Pts',(-7.9631387544268,-12.4065184959483,
119.267007168685)) ;
#155854 = CARTESIAN_POINT('Ctrl Pts',(-8.0369426034021,-12.4065184959014,
119.24277614392)) ;
#155855 = CARTESIAN_POINT('Ctrl Pts',(-8.11074645237739,-12.4065184958546,
119.218545119154)) ;
#155856 = CARTESIAN_POINT('Ctrl Pts',(-8.11142021739083,-12.330642919458,
119.220597298329)) ;
#155857 = CARTESIAN_POINT('Ctrl Pts',(-8.11209398240426,-12.2547673430615,
119.222649477503)) ;
#155858 = CARTESIAN_POINT('Ctrl Pts',(-8.03829013342897,-12.2547673431084,
119.246880502269)) ;
#155859 = CARTESIAN_POINT('Ctrl Pts',(-7.96448628445367,-12.2547673431553,
119.271111527034)) ;
#155860 = CARTESIAN_POINT('Ctrl Pts',(-7.96381251944024,-12.3306429195518,
119.269059347859)) ;
#155861 = CARTESIAN_POINT('Ctrl Pts',(-8.06368380821921,-12.3792038030185,
119.537856629935)) ;
#155862 = CARTESIAN_POINT('Ctrl Pts',(-8.05676830195218,-12.4517984874487,
119.516793114142)) ;
#155863 = CARTESIAN_POINT('Ctrl Pts',(-8.13057215287077,-12.4517984942269,
119.492562095296)) ;
#155864 = CARTESIAN_POINT('Ctrl Pts',(-8.20437600378937,-12.4517985010052,
119.468331076449)) ;
#155865 = CARTESIAN_POINT('Ctrl Pts',(-8.2112915100564,-12.379203816575,119.489394592243)) ;
#155866 = CARTESIAN_POINT('Ctrl Pts',(-8.21820701632344,-12.3066091321447,
119.510458108036)) ;
#155867 = CARTESIAN_POINT('Ctrl Pts',(-8.14440316540483,-12.3066091253665,
119.534689126882)) ;
#155868 = CARTESIAN_POINT('Ctrl Pts',(-8.07059931448624,-12.3066091185883,
119.558920145729)) ;
#155869 = CARTESIAN_POINT('Ctrl Pts',(-8.06368380821921,-12.3792038030185,
119.537856629935)) ;
#155870 = CARTESIAN_POINT('Ctrl Pts',(-8.15659748944132,-12.502250920438,
119.785364900155)) ;
#155871 = CARTESIAN_POINT('Ctrl Pts',(-8.14391906293416,-12.5663594268052,
119.746748459319)) ;
#155872 = CARTESIAN_POINT('Ctrl Pts',(-8.21772291527402,-12.5663594442773,
119.722517444801)) ;
#155873 = CARTESIAN_POINT('Ctrl Pts',(-8.29152676761388,-12.5663594617495,
119.698286430284)) ;
#155874 = CARTESIAN_POINT('Ctrl Pts',(-8.30420519412103,-12.5022509553824,
119.73690287112)) ;
#155875 = CARTESIAN_POINT('Ctrl Pts',(-8.31688362062818,-12.4381424490152,
119.775519311956)) ;
#155876 = CARTESIAN_POINT('Ctrl Pts',(-8.24307976828833,-12.4381424315431,
119.799750326474)) ;
#155877 = CARTESIAN_POINT('Ctrl Pts',(-8.16927591594847,-12.4381424140709,
119.823981340991)) ;
#155878 = CARTESIAN_POINT('Ctrl Pts',(-8.15659748944132,-12.502250920438,
119.785364900155)) ;
#155879 = CARTESIAN_POINT('Ctrl Pts',(-8.23623754753109,-12.690704289041,
119.992502391065)) ;
#155880 = CARTESIAN_POINT('Ctrl Pts',(-8.21871354461729,-12.7417475393675,
119.939127106486)) ;
#155881 = CARTESIAN_POINT('Ctrl Pts',(-8.29251739692174,-12.7417475700136,
119.914896091861)) ;
#155882 = CARTESIAN_POINT('Ctrl Pts',(-8.36632124922617,-12.7417476006596,
119.890665077235)) ;
#155883 = CARTESIAN_POINT('Ctrl Pts',(-8.38384525213997,-12.6907043503331,
119.944040361814)) ;
#155884 = CARTESIAN_POINT('Ctrl Pts',(-8.40136925505376,-12.6396611000066,
119.997415646394)) ;
#155885 = CARTESIAN_POINT('Ctrl Pts',(-8.32756540274933,-12.6396610693606,
120.021646661019)) ;
#155886 = CARTESIAN_POINT('Ctrl Pts',(-8.25376155044489,-12.6396610387145,
120.045877675644)) ;
#155887 = CARTESIAN_POINT('Ctrl Pts',(-8.23623754753109,-12.690704289041,
119.992502391065)) ;
#155888 = CARTESIAN_POINT('Ctrl Pts',(-8.29787978612712,-12.9312491813812,
120.144802031741)) ;
#155889 = CARTESIAN_POINT('Ctrl Pts',(-8.27676025616477,-12.9655714979513,
120.080475352075)) ;
#155890 = CARTESIAN_POINT('Ctrl Pts',(-8.35056410683368,-12.9655715427417,
120.056244332468)) ;
#155891 = CARTESIAN_POINT('Ctrl Pts',(-8.42436795750258,-12.9655715875322,
120.032013312861)) ;
#155892 = CARTESIAN_POINT('Ctrl Pts',(-8.44548748746493,-12.9312492709622,
120.096339992527)) ;
#155893 = CARTESIAN_POINT('Ctrl Pts',(-8.46660701742727,-12.8969269543922,
120.160666672194)) ;
#155894 = CARTESIAN_POINT('Ctrl Pts',(-8.39280316675835,-12.8969269096017,
120.184897691801)) ;
#155895 = CARTESIAN_POINT('Ctrl Pts',(-8.31899931608945,-12.8969268648112,
120.209128711407)) ;
#155896 = CARTESIAN_POINT('Ctrl Pts',(-8.29787978612712,-12.9312491813812,
120.144802031741)) ;
#155897 = CARTESIAN_POINT('Ctrl Pts',(-8.33778763616187,-13.2069304836541,
120.230868966777)) ;
#155898 = CARTESIAN_POINT('Ctrl Pts',(-8.31458553285275,-13.2220547357584,
120.160199104889)) ;
#155899 = CARTESIAN_POINT('Ctrl Pts',(-8.38838938005927,-13.2220547937704,
120.135968074736)) ;
#155900 = CARTESIAN_POINT('Ctrl Pts',(-8.46219322726581,-13.2220548517825,
120.111737044583)) ;
#155901 = CARTESIAN_POINT('Ctrl Pts',(-8.48539533057494,-13.2069305996783,
120.182406906472)) ;
#155902 = CARTESIAN_POINT('Ctrl Pts',(-8.50859743388407,-13.191806347574,
120.25307676836)) ;
#155903 = CARTESIAN_POINT('Ctrl Pts',(-8.43479358667754,-13.191806289562,
120.277307798513)) ;
#155904 = CARTESIAN_POINT('Ctrl Pts',(-8.36098973947101,-13.1918062315499,
120.301538828665)) ;
#155905 = CARTESIAN_POINT('Ctrl Pts',(-8.33778763616187,-13.2069304836541,
120.230868966777)) ;
#155906 = CARTESIAN_POINT('Ctrl Pts',(-8.35386611104003,-13.4971323588194,
120.244433805866)) ;
#155907 = CARTESIAN_POINT('Ctrl Pts',(-8.33024059213342,-13.4920171795336,
120.172474288537)) ;
#155908 = CARTESIAN_POINT('Ctrl Pts',(-8.40404443425814,-13.4920172465716,
120.148243242906)) ;
#155909 = CARTESIAN_POINT('Ctrl Pts',(-8.47784827638287,-13.4920173136096,
120.124012197275)) ;
#155910 = CARTESIAN_POINT('Ctrl Pts',(-8.50147379528949,-13.4971324928954,
120.195971714604)) ;
#155911 = CARTESIAN_POINT('Ctrl Pts',(-8.52509931419611,-13.5022476721812,
120.267931231933)) ;
#155912 = CARTESIAN_POINT('Ctrl Pts',(-8.45129547207138,-13.5022476051432,
120.292162277563)) ;
#155913 = CARTESIAN_POINT('Ctrl Pts',(-8.37749162994666,-13.5022475381053,
120.316393323194)) ;
#155914 = CARTESIAN_POINT('Ctrl Pts',(-8.35386611104003,-13.4971323588194,
120.244433805866)) ;
#155915 = CARTESIAN_POINT('Ctrl Pts',(-8.34559176606117,-13.7832858649534,
120.183607286869)) ;
#155916 = CARTESIAN_POINT('Ctrl Pts',(-8.32324669305239,-13.7581847544607,
120.115547801325)) ;
#155917 = CARTESIAN_POINT('Ctrl Pts',(-8.39705052864382,-13.7581848266256,
120.091316735795)) ;
#155918 = CARTESIAN_POINT('Ctrl Pts',(-8.47085436423525,-13.7581848987905,
120.067085670265)) ;
#155919 = CARTESIAN_POINT('Ctrl Pts',(-8.49319943724403,-13.7832860092831,
120.135145155809)) ;
#155920 = CARTESIAN_POINT('Ctrl Pts',(-8.51554451025281,-13.8083871197758,
120.203204641352)) ;
#155921 = CARTESIAN_POINT('Ctrl Pts',(-8.44174067466138,-13.808387047611,
120.227435706883)) ;
#155922 = CARTESIAN_POINT('Ctrl Pts',(-8.36793683906994,-13.8083869754461,
120.251666772413)) ;
#155923 = CARTESIAN_POINT('Ctrl Pts',(-8.34559176606117,-13.7832858649534,
120.183607286869)) ;
#155924 = CARTESIAN_POINT('Ctrl Pts',(-8.31464185127322,-14.0408293277911,
120.054056184709)) ;
#155925 = CARTESIAN_POINT('Ctrl Pts',(-8.29515542606811,-13.9977110227071,
119.994703679246)) ;
#155926 = CARTESIAN_POINT('Ctrl Pts',(-8.36895925493502,-13.997711090453,
119.970472593234)) ;
#155927 = CARTESIAN_POINT('Ctrl Pts',(-8.44276308380194,-13.9977111581989,
119.946241507222)) ;
#155928 = CARTESIAN_POINT('Ctrl Pts',(-8.46224950900705,-14.0408294632829,
120.005594012685)) ;
#155929 = CARTESIAN_POINT('Ctrl Pts',(-8.48173593421216,-14.0839477683669,
120.064946518147)) ;
#155930 = CARTESIAN_POINT('Ctrl Pts',(-8.40793210534524,-14.083947700621,
120.089177604159)) ;
#155931 = CARTESIAN_POINT('Ctrl Pts',(-8.33412827647834,-14.0839476328751,
120.113408690171)) ;
#155932 = CARTESIAN_POINT('Ctrl Pts',(-8.31464185127322,-14.0408293277911,
120.054056184709)) ;
#155933 = CARTESIAN_POINT('Ctrl Pts',(-8.26340664177902,-14.255952322556,
119.862377902584)) ;
#155934 = CARTESIAN_POINT('Ctrl Pts',(-8.24820592875809,-14.1977519640159,
119.816078985087)) ;
#155935 = CARTESIAN_POINT('Ctrl Pts',(-8.32200975066257,-14.1977520218044,
119.791847877869)) ;
#155936 = CARTESIAN_POINT('Ctrl Pts',(-8.39581357256705,-14.1977520795929,
119.76761677065)) ;
#155937 = CARTESIAN_POINT('Ctrl Pts',(-8.41101428558798,-14.2559524381331,
119.813915688147)) ;
#155938 = CARTESIAN_POINT('Ctrl Pts',(-8.4262149986089,-14.3141527966732,
119.860214605644)) ;
#155939 = CARTESIAN_POINT('Ctrl Pts',(-8.35241117670443,-14.3141527388846,
119.884445712862)) ;
#155940 = CARTESIAN_POINT('Ctrl Pts',(-8.27860735479995,-14.3141526810961,
119.908676820081)) ;
#155941 = CARTESIAN_POINT('Ctrl Pts',(-8.26340664177902,-14.255952322556,
119.862377902584)) ;
#155942 = CARTESIAN_POINT('Ctrl Pts',(-8.1971249772834,-14.4094466686143,
119.625180693076)) ;
#155943 = CARTESIAN_POINT('Ctrl Pts',(-8.18726048315509,-14.3404453655438,
119.595135037421)) ;
#155944 = CARTESIAN_POINT('Ctrl Pts',(-8.26106429969089,-14.3404454048825,
119.570903913851)) ;
#155945 = CARTESIAN_POINT('Ctrl Pts',(-8.33486811622669,-14.3404454442213,
119.54667279028)) ;
#155946 = CARTESIAN_POINT('Ctrl Pts',(-8.344732610355,-14.4094467472918,119.576718445934)) ;
#155947 = CARTESIAN_POINT('Ctrl Pts',(-8.35459710448329,-14.4784480503623,
119.606764101589)) ;
#155948 = CARTESIAN_POINT('Ctrl Pts',(-8.2807932879475,-14.4784480110235,
119.630995225159)) ;
#155949 = CARTESIAN_POINT('Ctrl Pts',(-8.20698947141171,-14.4784479716848,
119.65522634873)) ;
#155950 = CARTESIAN_POINT('Ctrl Pts',(-8.1971249772834,-14.4094466686143,
119.625180693076)) ;
#155951 = CARTESIAN_POINT('Ctrl Pts',(-8.12040152389499,-14.4929694646286,
119.35593056019)) ;
#155952 = CARTESIAN_POINT('Ctrl Pts',(-8.11661493104229,-14.4180358803258,
119.34439721126)) ;
#155953 = CARTESIAN_POINT('Ctrl Pts',(-8.19041874362283,-14.4180358961808,
119.320166075642)) ;
#155954 = CARTESIAN_POINT('Ctrl Pts',(-8.26422255620336,-14.4180359120358,
119.295934940024)) ;
#155955 = CARTESIAN_POINT('Ctrl Pts',(-8.26800914905606,-14.4929694963386,
119.307468288954)) ;
#155956 = CARTESIAN_POINT('Ctrl Pts',(-8.27179574190875,-14.5679030806414,
119.319001637885)) ;
#155957 = CARTESIAN_POINT('Ctrl Pts',(-8.19799192932821,-14.5679030647864,
119.343232773502)) ;
#155958 = CARTESIAN_POINT('Ctrl Pts',(-8.12418811674768,-14.5679030489314,
119.36746390912)) ;
#155959 = CARTESIAN_POINT('Ctrl Pts',(-8.12040152389499,-14.4929694646286,
119.35593056019)) ;
#155960 = CARTESIAN_POINT('Ctrl Pts',(-8.04009022848257,-14.4990155260453,
119.075851461994)) ;
#155961 = CARTESIAN_POINT('Ctrl Pts',(-8.04263890692783,-14.4235500005798,
119.083614327317)) ;
#155962 = CARTESIAN_POINT('Ctrl Pts',(-8.11644271815056,-14.4235499890681,
119.059383187563)) ;
#155963 = CARTESIAN_POINT('Ctrl Pts',(-8.19024652937329,-14.4235499775565,
119.03515204781)) ;
#155964 = CARTESIAN_POINT('Ctrl Pts',(-8.18769785092804,-14.499015503022,
119.027389182487)) ;
#155965 = CARTESIAN_POINT('Ctrl Pts',(-8.18514917248278,-14.5744810284875,
119.019626317164)) ;
#155966 = CARTESIAN_POINT('Ctrl Pts',(-8.11134536126006,-14.5744810399991,
119.043857456918)) ;
#155967 = CARTESIAN_POINT('Ctrl Pts',(-8.03754155003731,-14.5744810515108,
119.068088596671)) ;
#155968 = CARTESIAN_POINT('Ctrl Pts',(-8.04009022848257,-14.4990155260453,
119.075851461994)) ;
#155969 = CARTESIAN_POINT('Ctrl Pts',(-7.9625098388441,-14.4275804860338,
118.804068220134)) ;
#155970 = CARTESIAN_POINT('Ctrl Pts',(-7.97121287685695,-14.3569912762542,
118.830576271749)) ;
#155971 = CARTESIAN_POINT('Ctrl Pts',(-8.04501668942195,-14.3569912367052,
118.806345136084)) ;
#155972 = CARTESIAN_POINT('Ctrl Pts',(-8.11882050198696,-14.3569911971563,
118.782114000419)) ;
#155973 = CARTESIAN_POINT('Ctrl Pts',(-8.11011746397412,-14.4275804069359,
118.755605948804)) ;
#155974 = CARTESIAN_POINT('Ctrl Pts',(-8.10141442596128,-14.4981696167155,
118.729097897188)) ;
#155975 = CARTESIAN_POINT('Ctrl Pts',(-8.02761061339627,-14.4981696562644,
118.753329032853)) ;
#155976 = CARTESIAN_POINT('Ctrl Pts',(-7.95380680083127,-14.4981696958134,
118.777560168518)) ;
#155977 = CARTESIAN_POINT('Ctrl Pts',(-7.9625098388441,-14.4275804860338,
118.804068220134)) ;
#155978 = CARTESIAN_POINT('Ctrl Pts',(-7.8941100124004,-14.284309082368,118.560336785865)) ;
#155979 = CARTESIAN_POINT('Ctrl Pts',(-7.90833367643576,-14.223618657059,
118.603659773624)) ;
#155980 = CARTESIAN_POINT('Ctrl Pts',(-7.98213749300733,-14.2236185917218,
118.579428650163)) ;
#155981 = CARTESIAN_POINT('Ctrl Pts',(-8.05594130957889,-14.2236185263845,
118.555197526701)) ;
#155982 = CARTESIAN_POINT('Ctrl Pts',(-8.04171764554352,-14.2843089516935,
118.511874538942)) ;
#155983 = CARTESIAN_POINT('Ctrl Pts',(-8.02749398150816,-14.3449993770025,
118.468551551182)) ;
#155984 = CARTESIAN_POINT('Ctrl Pts',(-7.95369016493661,-14.3449994423398,
118.492782674643)) ;
#155985 = CARTESIAN_POINT('Ctrl Pts',(-7.87988634836503,-14.3449995076771,
118.517013798105)) ;
#155986 = CARTESIAN_POINT('Ctrl Pts',(-7.8941100124004,-14.284309082368,118.560336785865)) ;
#155987 = CARTESIAN_POINT('Ctrl Pts',(-7.84012347499757,-14.0775350374868,
118.360268383229)) ;
#155988 = CARTESIAN_POINT('Ctrl Pts',(-7.85887471453744,-14.0311904705444,
118.417381635461)) ;
#155989 = CARTESIAN_POINT('Ctrl Pts',(-7.93267853746199,-14.0311903843125,
118.39315053135)) ;
#155990 = CARTESIAN_POINT('Ctrl Pts',(-8.00648236038654,-14.0311902980806,
118.368919427238)) ;
#155991 = CARTESIAN_POINT('Ctrl Pts',(-7.98773112084667,-14.0775348650229,
118.311806175006)) ;
#155992 = CARTESIAN_POINT('Ctrl Pts',(-7.96897988130681,-14.1238794319653,
118.254692922774)) ;
#155993 = CARTESIAN_POINT('Ctrl Pts',(-7.89517605838225,-14.1238795181972,
118.278924026886)) ;
#155994 = CARTESIAN_POINT('Ctrl Pts',(-7.8213722354577,-14.1238796044292,
118.303155130997)) ;
#155995 = CARTESIAN_POINT('Ctrl Pts',(-7.84012347499757,-14.0775350374868,
118.360268383229)) ;
#155996 = CARTESIAN_POINT('Ctrl Pts',(-7.80588583848825,-13.8261134335288,
118.220747745965)) ;
#155997 = CARTESIAN_POINT('Ctrl Pts',(-7.82778425353249,-13.7972540806325,
118.287446786978)) ;
#155998 = CARTESIAN_POINT('Ctrl Pts',(-7.90158808437181,-13.7972539806286,
118.263215706973)) ;
#155999 = CARTESIAN_POINT('Ctrl Pts',(-7.97539191521112,-13.7972538806247,
118.238984626969)) ;
#156000 = CARTESIAN_POINT('Ctrl Pts',(-7.95349350016687,-13.826113233521,
118.172285585957)) ;
#156001 = CARTESIAN_POINT('Ctrl Pts',(-7.93159508512261,-13.8549725864173,
118.105586544944)) ;
#156002 = CARTESIAN_POINT('Ctrl Pts',(-7.85779125428331,-13.8549726864212,
118.129817624949)) ;
#156003 = CARTESIAN_POINT('Ctrl Pts',(-7.78398742344399,-13.8549727864252,
118.154048704953)) ;
#156004 = CARTESIAN_POINT('Ctrl Pts',(-7.80588583848825,-13.8261134335288,
118.220747745965)) ;
#156005 = CARTESIAN_POINT('Ctrl Pts',(-7.79385768957157,-13.5428648342343,
118.148500404782)) ;
#156006 = CARTESIAN_POINT('Ctrl Pts',(-7.81736543683943,-13.5337376171051,
118.220101212043)) ;
#156007 = CARTESIAN_POINT('Ctrl Pts',(-7.89116927654803,-13.5337375120109,
118.195870159053)) ;
#156008 = CARTESIAN_POINT('Ctrl Pts',(-7.96497311625663,-13.5337374069167,
118.171639106063)) ;
#156009 = CARTESIAN_POINT('Ctrl Pts',(-7.94146536898876,-13.5428646240459,
118.100038298802)) ;
#156010 = CARTESIAN_POINT('Ctrl Pts',(-7.9179576217209,-13.551991841175,118.028437491541)) ;
#156011 = CARTESIAN_POINT('Ctrl Pts',(-7.84415378201231,-13.5519919462692,
118.052668544531)) ;
#156012 = CARTESIAN_POINT('Ctrl Pts',(-7.7703499423037,-13.5519920513634,
118.076899597521)) ;
#156013 = CARTESIAN_POINT('Ctrl Pts',(-7.79385768957157,-13.5428648342343,
118.148500404782)) ;
#156014 = CARTESIAN_POINT('Ctrl Pts',(-7.80612682657335,-13.252182353688,
118.150461687266)) ;
#156015 = CARTESIAN_POINT('Ctrl Pts',(-7.82954570480992,-13.263336213575,
118.22179181374)) ;
#156016 = CARTESIAN_POINT('Ctrl Pts',(-7.90334955320528,-13.2633361119795,
118.197560787209)) ;
#156017 = CARTESIAN_POINT('Ctrl Pts',(-7.97715340160061,-13.2633360103841,
118.173329760677)) ;
#156018 = CARTESIAN_POINT('Ctrl Pts',(-7.95373452336405,-13.2521821504971,
118.101999634203)) ;
#156019 = CARTESIAN_POINT('Ctrl Pts',(-7.93031564512747,-13.2410282906101,
118.030669507729)) ;
#156020 = CARTESIAN_POINT('Ctrl Pts',(-7.85651179673213,-13.2410283922056,
118.05490053426)) ;
#156021 = CARTESIAN_POINT('Ctrl Pts',(-7.78270794833677,-13.241028493801,
118.079131560792)) ;
#156022 = CARTESIAN_POINT('Ctrl Pts',(-7.80612682657335,-13.252182353688,
118.150461687266)) ;
#156023 = CARTESIAN_POINT('Ctrl Pts',(-7.84228893480843,-12.9730234465435,
118.225161565708)) ;
#156024 = CARTESIAN_POINT('Ctrl Pts',(-7.86395152537764,-13.0036840588297,
118.29114232325)) ;
#156025 = CARTESIAN_POINT('Ctrl Pts',(-7.9377553815644,-13.0036839686776,
118.26691132045)) ;
#156026 = CARTESIAN_POINT('Ctrl Pts',(-8.01155923775114,-13.0036838785254,
118.242680317649)) ;
#156027 = CARTESIAN_POINT('Ctrl Pts',(-7.98989664718192,-12.9730232662392,
118.176699560108)) ;
#156028 = CARTESIAN_POINT('Ctrl Pts',(-7.9682340566127,-12.9423626539529,
118.110718802566)) ;
#156029 = CARTESIAN_POINT('Ctrl Pts',(-7.89443020042595,-12.942362744105,
118.134949805366)) ;
#156030 = CARTESIAN_POINT('Ctrl Pts',(-7.8206263442392,-12.9423628342572,
118.159180808167)) ;
#156031 = CARTESIAN_POINT('Ctrl Pts',(-7.84228893480843,-12.9730234465435,
118.225161565708)) ;
#156032 = CARTESIAN_POINT('Ctrl Pts',(-7.90103421558884,-12.724731390434,
118.368470996422)) ;
#156033 = CARTESIAN_POINT('Ctrl Pts',(-7.91936506739964,-12.77277340565,118.424303815163)) ;
#156034 = CARTESIAN_POINT('Ctrl Pts',(-7.99316892941168,-12.7727733343003,
118.400072830106)) ;
#156035 = CARTESIAN_POINT('Ctrl Pts',(-8.06697279142372,-12.7727732629506,
118.375841845048)) ;
#156036 = CARTESIAN_POINT('Ctrl Pts',(-8.04864193961291,-12.7247312477346,
118.320009026308)) ;
#156037 = CARTESIAN_POINT('Ctrl Pts',(-8.0303110878021,-12.6766892325185,
118.264176207567)) ;
#156038 = CARTESIAN_POINT('Ctrl Pts',(-7.95650722579007,-12.6766893038683,
118.288407192625)) ;
#156039 = CARTESIAN_POINT('Ctrl Pts',(-7.88270336377803,-12.676689375218,
118.312638177682)) ;
#156040 = CARTESIAN_POINT('Ctrl Pts',(-7.90103421558884,-12.724731390434,
118.368470996422)) ;
#156041 = CARTESIAN_POINT('Ctrl Pts',(-7.97782116130876,-12.5280561031159,
118.567077843843)) ;
#156042 = CARTESIAN_POINT('Ctrl Pts',(-7.99154820293211,-12.5899016984486,
118.608888199484)) ;
#156043 = CARTESIAN_POINT('Ctrl Pts',(-8.06535206896777,-12.5899016481567,
118.584657226682)) ;
#156044 = CARTESIAN_POINT('Ctrl Pts',(-8.13915593500343,-12.5899015978648,
118.56042625388)) ;
#156045 = CARTESIAN_POINT('Ctrl Pts',(-8.12542889338008,-12.5280560025322,
118.518615898239)) ;
#156046 = CARTESIAN_POINT('Ctrl Pts',(-8.11170185175672,-12.4662104071995,
118.476805542598)) ;
#156047 = CARTESIAN_POINT('Ctrl Pts',(-8.03789798572106,-12.4662104574914,
118.5010365154)) ;
#156048 = CARTESIAN_POINT('Ctrl Pts',(-7.96409411968541,-12.4662105077833,
118.525267488202)) ;
#156049 = CARTESIAN_POINT('Ctrl Pts',(-7.97782116130876,-12.5280561031159,
118.567077843843)) ;
#156050 = CARTESIAN_POINT('Ctrl Pts',(-8.0692686377754,-12.3935893009494,
118.810023631757)) ;
#156051 = CARTESIAN_POINT('Ctrl Pts',(-8.07736813977987,-12.4649167907205,
118.834693409571)) ;
#156052 = CARTESIAN_POINT('Ctrl Pts',(-8.15117200694027,-12.464916764178,
118.810462440194)) ;
#156053 = CARTESIAN_POINT('Ctrl Pts',(-8.22497587410067,-12.4649167376354,
118.786231470818)) ;
#156054 = CARTESIAN_POINT('Ctrl Pts',(-8.21687637209619,-12.3935892478642,
118.761561693005)) ;
#156055 = CARTESIAN_POINT('Ctrl Pts',(-8.20877687009171,-12.322261758093,
118.736891915191)) ;
#156056 = CARTESIAN_POINT('Ctrl Pts',(-8.13497300293131,-12.3222617846356,
118.761122884567)) ;
#156057 = CARTESIAN_POINT('Ctrl Pts',(-8.06116913577091,-12.3222618111782,
118.785353853944)) ;
#156058 = CARTESIAN_POINT('Ctrl Pts',(-8.0692686377754,-12.3935893009494,
118.810023631757)) ;
#156059 = CARTESIAN_POINT('Ctrl Pts',(-8.16837016553241,-12.333081965445,
119.076502994386)) ;
#156060 = CARTESIAN_POINT('Ctrl Pts',(-8.17029452669112,-12.4087416290775,
119.08236428941)) ;
#156061 = CARTESIAN_POINT('Ctrl Pts',(-8.24409839311102,-12.4087416242859,
119.058133317778)) ;
#156062 = CARTESIAN_POINT('Ctrl Pts',(-8.31790225953092,-12.4087416194943,
119.033902346147)) ;
#156063 = CARTESIAN_POINT('Ctrl Pts',(-8.31597789837221,-12.3330819558618,
119.028041051122)) ;
#156064 = CARTESIAN_POINT('Ctrl Pts',(-8.31405353721349,-12.2574222922293,
119.022179756098)) ;
#156065 = CARTESIAN_POINT('Ctrl Pts',(-8.24024967079359,-12.2574222970209,
119.04641072773)) ;
#156066 = CARTESIAN_POINT('Ctrl Pts',(-8.16644580437368,-12.2574223018125,
119.070641699362)) ;
#156067 = CARTESIAN_POINT('Ctrl Pts',(-8.16837016553241,-12.333081965445,
119.076502994386)) ;
#156068 = CARTESIAN_POINT('Ctrl Pts',(-8.27009279108481,-12.3505128306963,
119.350670896121)) ;
#156069 = CARTESIAN_POINT('Ctrl Pts',(-8.26565575692453,-12.4250706656238,
119.33715640722)) ;
#156070 = CARTESIAN_POINT('Ctrl Pts',(-8.33945961991325,-12.4250706786686,
119.312925425138)) ;
#156071 = CARTESIAN_POINT('Ctrl Pts',(-8.41326348290199,-12.4250706917134,
119.288694443055)) ;
#156072 = CARTESIAN_POINT('Ctrl Pts',(-8.41770051706228,-12.3505128567859,
119.302208931956)) ;
#156073 = CARTESIAN_POINT('Ctrl Pts',(-8.42213755122257,-12.2759550218584,
119.315723420857)) ;
#156074 = CARTESIAN_POINT('Ctrl Pts',(-8.34833368823383,-12.2759550088136,
119.33995440294)) ;
#156075 = CARTESIAN_POINT('Ctrl Pts',(-8.2745298252451,-12.2759549957688,
119.364185385022)) ;
#156076 = CARTESIAN_POINT('Ctrl Pts',(-8.27009279108481,-12.3505128306963,
119.350670896121)) ;
#156077 = CARTESIAN_POINT('Ctrl Pts',(-8.3658449010965,-12.4433828921911,
119.60714075347)) ;
#156078 = CARTESIAN_POINT('Ctrl Pts',(-8.35544359845222,-12.5115686405398,
119.575460064988)) ;
#156079 = CARTESIAN_POINT('Ctrl Pts',(-8.42924745806618,-12.5115686671103,
119.551229072627)) ;
#156080 = CARTESIAN_POINT('Ctrl Pts',(-8.50305131768015,-12.5115686936807,
119.526998080265)) ;
#156081 = CARTESIAN_POINT('Ctrl Pts',(-8.51345262032444,-12.443382945332,
119.558678768747)) ;
#156082 = CARTESIAN_POINT('Ctrl Pts',(-8.52385392296872,-12.3751971969833,
119.590359457229)) ;
#156083 = CARTESIAN_POINT('Ctrl Pts',(-8.45005006335476,-12.3751971704129,
119.614590449591)) ;
#156084 = CARTESIAN_POINT('Ctrl Pts',(-8.37624620374079,-12.3751971438424,
119.638821441952)) ;
#156085 = CARTESIAN_POINT('Ctrl Pts',(-8.3658449010965,-12.4433828921911,
119.60714075347)) ;
#156086 = CARTESIAN_POINT('Ctrl Pts',(-8.45197505795687,-12.607349424796,
119.833841108759)) ;
#156087 = CARTESIAN_POINT('Ctrl Pts',(-8.43628164446657,-12.6641907157574,
119.786041504319)) ;
#156088 = CARTESIAN_POINT('Ctrl Pts',(-8.51008549888229,-12.6641907484467,
119.761810496124)) ;
#156089 = CARTESIAN_POINT('Ctrl Pts',(-8.58388935329801,-12.664190781136,
119.73757948793)) ;
#156090 = CARTESIAN_POINT('Ctrl Pts',(-8.59958276678831,-12.6073494901747,
119.78537909237)) ;
#156091 = CARTESIAN_POINT('Ctrl Pts',(-8.6152761802786,-12.5505081992133,
119.83317869681)) ;
#156092 = CARTESIAN_POINT('Ctrl Pts',(-8.54147232586288,-12.5505081665239,
119.857409705004)) ;
#156093 = CARTESIAN_POINT('Ctrl Pts',(-8.46766847144716,-12.5505081338346,
119.881640713199)) ;
#156094 = CARTESIAN_POINT('Ctrl Pts',(-8.45197505795687,-12.607349424796,
119.833841108759)) ;
#156095 = CARTESIAN_POINT('Ctrl Pts',(-8.52120977492203,-12.8279036385121,
120.00940010572)) ;
#156096 = CARTESIAN_POINT('Ctrl Pts',(-8.50138939635353,-12.8694313461383,
119.949030431395)) ;
#156097 = CARTESIAN_POINT('Ctrl Pts',(-8.57519324644018,-12.8694313807778,
119.924799410014)) ;
#156098 = CARTESIAN_POINT('Ctrl Pts',(-8.64899709652682,-12.8694314154173,
119.900568388634)) ;
#156099 = CARTESIAN_POINT('Ctrl Pts',(-8.66881747509531,-12.8279037077911,
119.96093806296)) ;
#156100 = CARTESIAN_POINT('Ctrl Pts',(-8.68863785366382,-12.7863760001649,
120.021307737286)) ;
#156101 = CARTESIAN_POINT('Ctrl Pts',(-8.61483400357718,-12.7863759655254,
120.045538758666)) ;
#156102 = CARTESIAN_POINT('Ctrl Pts',(-8.54103015349054,-12.7863759308859,
120.069769780046)) ;
#156103 = CARTESIAN_POINT('Ctrl Pts',(-8.52120977492203,-12.8279036385121,
120.00940010572)) ;
#156104 = CARTESIAN_POINT('Ctrl Pts',(-8.57055325895007,-13.0930059035689,
120.124025527535)) ;
#156105 = CARTESIAN_POINT('Ctrl Pts',(-8.54799540220528,-13.1160865947577,
120.055317936172)) ;
#156106 = CARTESIAN_POINT('Ctrl Pts',(-8.62179924818873,-13.1160866238806,
120.031086902294)) ;
#156107 = CARTESIAN_POINT('Ctrl Pts',(-8.69560309417219,-13.1160866530036,
120.006855868416)) ;
#156108 = CARTESIAN_POINT('Ctrl Pts',(-8.71816095091697,-13.0930059618148,
120.075563459779)) ;
#156109 = CARTESIAN_POINT('Ctrl Pts',(-8.74071880766174,-13.069925270626,
120.144271051143)) ;
#156110 = CARTESIAN_POINT('Ctrl Pts',(-8.6669149616783,-13.069925241503,120.168502085021)) ;
#156111 = CARTESIAN_POINT('Ctrl Pts',(-8.59311111569484,-13.0699252123801,
120.192733118899)) ;
#156112 = CARTESIAN_POINT('Ctrl Pts',(-8.57055325895007,-13.0930059035689,
120.124025527535)) ;
#156113 = CARTESIAN_POINT('Ctrl Pts',(-8.59625204583721,-13.3789266137586,
120.166977376249)) ;
#156114 = CARTESIAN_POINT('Ctrl Pts',(-8.57259671566402,-13.3820781397035,
120.094927057768)) ;
#156115 = CARTESIAN_POINT('Ctrl Pts',(-8.64640055914781,-13.3820781631016,
120.070696016276)) ;
#156116 = CARTESIAN_POINT('Ctrl Pts',(-8.72020440263158,-13.3820781864996,
120.046464974784)) ;
#156117 = CARTESIAN_POINT('Ctrl Pts',(-8.74385973280477,-13.3789266605547,
120.118515293266)) ;
#156118 = CARTESIAN_POINT('Ctrl Pts',(-8.76751506297795,-13.3757751346097,
120.190565611747)) ;
#156119 = CARTESIAN_POINT('Ctrl Pts',(-8.69371121949417,-13.3757751112117,
120.214796653239)) ;
#156120 = CARTESIAN_POINT('Ctrl Pts',(-8.61990737601039,-13.3757750878137,
120.239027694731)) ;
#156121 = CARTESIAN_POINT('Ctrl Pts',(-8.59625204583721,-13.3789266137586,
120.166977376249)) ;
#156122 = CARTESIAN_POINT('Ctrl Pts',(-8.59788852250651,-13.6686885717782,
120.136495690536)) ;
#156123 = CARTESIAN_POINT('Ctrl Pts',(-8.57481707676371,-13.6516124113894,
120.066223789672)) ;
#156124 = CARTESIAN_POINT('Ctrl Pts',(-8.64862091882858,-13.6516124266104,
120.041992743859)) ;
#156125 = CARTESIAN_POINT('Ctrl Pts',(-8.72242476089344,-13.6516124418314,
120.017761698045)) ;
#156126 = CARTESIAN_POINT('Ctrl Pts',(-8.74549620663624,-13.6686886022201,
120.088033598909)) ;
#156127 = CARTESIAN_POINT('Ctrl Pts',(-8.76856765237905,-13.6857647626089,
120.158305499772)) ;
#156128 = CARTESIAN_POINT('Ctrl Pts',(-8.69476381031418,-13.6857647473879,
120.182536545585)) ;
#156129 = CARTESIAN_POINT('Ctrl Pts',(-8.62095996824932,-13.6857647321669,
120.206767591399)) ;
#156130 = CARTESIAN_POINT('Ctrl Pts',(-8.59788852250651,-13.6686885717782,
120.136495690536)) ;
#156131 = CARTESIAN_POINT('Ctrl Pts',(-8.57580906244584,-13.9407698971193,
120.033752331659)) ;
#156132 = CARTESIAN_POINT('Ctrl Pts',(-8.55497897586174,-13.9046696710089,
119.970307249017)) ;
#156133 = CARTESIAN_POINT('Ctrl Pts',(-8.62878281778872,-13.904669678464,
119.946076202783)) ;
#156134 = CARTESIAN_POINT('Ctrl Pts',(-8.70258665971571,-13.9046696859191,
119.92184515655)) ;
#156135 = CARTESIAN_POINT('Ctrl Pts',(-8.72341674629981,-13.9407699120296,
119.985290239192)) ;
#156136 = CARTESIAN_POINT('Ctrl Pts',(-8.74424683288391,-13.97687013814,120.048735321835)) ;
#156137 = CARTESIAN_POINT('Ctrl Pts',(-8.67044299095692,-13.9768701306849,
120.072966368068)) ;
#156138 = CARTESIAN_POINT('Ctrl Pts',(-8.59663914902995,-13.9768701232298,
120.097197414301)) ;
#156139 = CARTESIAN_POINT('Ctrl Pts',(-8.57580906244584,-13.9407698971193,
120.033752331659)) ;
#156140 = CARTESIAN_POINT('Ctrl Pts',(-8.53228870836988,-14.1754452261927,
119.865663575393)) ;
#156141 = CARTESIAN_POINT('Ctrl Pts',(-8.51520149123549,-14.122903887043,
119.813618669073)) ;
#156142 = CARTESIAN_POINT('Ctrl Pts',(-8.58900533389292,-14.1229038889288,
119.789387625064)) ;
#156143 = CARTESIAN_POINT('Ctrl Pts',(-8.66280917655036,-14.1229038908147,
119.765156581056)) ;
#156144 = CARTESIAN_POINT('Ctrl Pts',(-8.67989639368476,-14.1754452299645,
119.817201487376)) ;
#156145 = CARTESIAN_POINT('Ctrl Pts',(-8.69698361081914,-14.2279865691142,
119.869246393697)) ;
#156146 = CARTESIAN_POINT('Ctrl Pts',(-8.6231797681617,-14.2279865672284,
119.893477437705)) ;
#156147 = CARTESIAN_POINT('Ctrl Pts',(-8.54937592550426,-14.2279865653425,
119.917708481714)) ;
#156148 = CARTESIAN_POINT('Ctrl Pts',(-8.53228870836988,-14.1754452261927,
119.865663575393)) ;
#156149 = CARTESIAN_POINT('Ctrl Pts',(-8.47162858688881,-14.3550939223612,
119.645549235714)) ;
#156150 = CARTESIAN_POINT('Ctrl Pts',(-8.45948313829748,-14.2899298530335,
119.608556158953)) ;
#156151 = CARTESIAN_POINT('Ctrl Pts',(-8.5332869818319,-14.2899298524596,
119.584325117616)) ;
#156152 = CARTESIAN_POINT('Ctrl Pts',(-8.60709082536632,-14.2899298518858,
119.560094076279)) ;
#156153 = CARTESIAN_POINT('Ctrl Pts',(-8.61923627395765,-14.3550939212134,
119.597087153039)) ;
#156154 = CARTESIAN_POINT('Ctrl Pts',(-8.63138172254897,-14.4202579905411,
119.634080229799)) ;
#156155 = CARTESIAN_POINT('Ctrl Pts',(-8.55757787901455,-14.420257991115,
119.658311271137)) ;
#156156 = CARTESIAN_POINT('Ctrl Pts',(-8.48377403548013,-14.4202579916889,
119.682542312474)) ;
#156157 = CARTESIAN_POINT('Ctrl Pts',(-8.47162858688881,-14.3550939223612,
119.645549235714)) ;
#156158 = CARTESIAN_POINT('Ctrl Pts',(-8.39799248590873,-14.468598908444,
119.385596001449)) ;
#156159 = CARTESIAN_POINT('Ctrl Pts',(-8.3917090967398,-14.3954110161889,
119.366457811798)) ;
#156160 = CARTESIAN_POINT('Ctrl Pts',(-8.46551294113031,-14.3954110152214,
119.342226773068)) ;
#156161 = CARTESIAN_POINT('Ctrl Pts',(-8.53931678552082,-14.395411014254,
119.317995734338)) ;
#156162 = CARTESIAN_POINT('Ctrl Pts',(-8.54560017468974,-14.4685989065091,
119.337133923989)) ;
#156163 = CARTESIAN_POINT('Ctrl Pts',(-8.55188356385866,-14.5417867987642,
119.35627211364)) ;
#156164 = CARTESIAN_POINT('Ctrl Pts',(-8.47807971946816,-14.5417867997317,
119.38050315237)) ;
#156165 = CARTESIAN_POINT('Ctrl Pts',(-8.40427587507765,-14.5417868006991,
119.4047341911)) ;
#156166 = CARTESIAN_POINT('Ctrl Pts',(-8.39799248590873,-14.468598908444,
119.385596001449)) ;
#156167 = CARTESIAN_POINT('Ctrl Pts',(-8.31877491440371,-14.5058659881171,
119.109007145666)) ;
#156168 = CARTESIAN_POINT('Ctrl Pts',(-8.31874453084561,-14.4299679241318,
119.108914602191)) ;
#156169 = CARTESIAN_POINT('Ctrl Pts',(-8.39254837521704,-14.4299679242476,
119.084683563403)) ;
#156170 = CARTESIAN_POINT('Ctrl Pts',(-8.46635221958846,-14.4299679243634,
119.060452524615)) ;
#156171 = CARTESIAN_POINT('Ctrl Pts',(-8.46638260314656,-14.5058659883488,
119.06054506809)) ;
#156172 = CARTESIAN_POINT('Ctrl Pts',(-8.46641298670466,-14.5817640523341,
119.060637611565)) ;
#156173 = CARTESIAN_POINT('Ctrl Pts',(-8.39260914233323,-14.5817640522183,
119.084868650353)) ;
#156174 = CARTESIAN_POINT('Ctrl Pts',(-8.31880529796181,-14.5817640521025,
119.109099689141)) ;
#156175 = CARTESIAN_POINT('Ctrl Pts',(-8.31877491440371,-14.5058659881171,
119.109007145666)) ;
#156176 = CARTESIAN_POINT('Ctrl Pts',(-8.23941378855136,-14.465907705861,
118.831859781048)) ;
#156177 = CARTESIAN_POINT('Ctrl Pts',(-8.24565808732545,-14.3926881487027,
118.850878907574)) ;
#156178 = CARTESIAN_POINT('Ctrl Pts',(-8.31946193110952,-14.3926881492861,
118.826647866997)) ;
#156179 = CARTESIAN_POINT('Ctrl Pts',(-8.3932657748936,-14.3926881498695,
118.80241682642)) ;
#156180 = CARTESIAN_POINT('Ctrl Pts',(-8.38702147611951,-14.4659077070278,
118.783397699894)) ;
#156181 = CARTESIAN_POINT('Ctrl Pts',(-8.38077717734542,-14.5391272641861,
118.764378573367)) ;
#156182 = CARTESIAN_POINT('Ctrl Pts',(-8.30697333356135,-14.5391272636027,
118.788609613944)) ;
#156183 = CARTESIAN_POINT('Ctrl Pts',(-8.23316948977728,-14.5391272630193,
118.812840654521)) ;
#156184 = CARTESIAN_POINT('Ctrl Pts',(-8.23941378855136,-14.465907705861,
118.831859781048)) ;
#156185 = CARTESIAN_POINT('Ctrl Pts',(-8.16647270185438,-14.3507454275659,
118.574221540228)) ;
#156186 = CARTESIAN_POINT('Ctrl Pts',(-8.17855345341657,-14.2854599330561,
118.611017560312)) ;
#156187 = CARTESIAN_POINT('Ctrl Pts',(-8.25235729609328,-14.2854599321569,
118.586786516362)) ;
#156188 = CARTESIAN_POINT('Ctrl Pts',(-8.32616113876998,-14.2854599312576,
118.562555472413)) ;
#156189 = CARTESIAN_POINT('Ctrl Pts',(-8.31408038720779,-14.3507454257675,
118.525759452328)) ;
#156190 = CARTESIAN_POINT('Ctrl Pts',(-8.30199963564559,-14.4160309202774,
118.488963432244)) ;
#156191 = CARTESIAN_POINT('Ctrl Pts',(-8.22819579296889,-14.4160309211766,
118.513194476194)) ;
#156192 = CARTESIAN_POINT('Ctrl Pts',(-8.15439195029218,-14.4160309220758,
118.537425520144)) ;
#156193 = CARTESIAN_POINT('Ctrl Pts',(-8.16647270185438,-14.3507454275659,
118.574221540228)) ;
#156194 = CARTESIAN_POINT('Ctrl Pts',(-8.10601871451368,-14.1684902162708,
118.354580107972)) ;
#156195 = CARTESIAN_POINT('Ctrl Pts',(-8.12307315420655,-14.1158354027091,
118.406525179709)) ;
#156196 = CARTESIAN_POINT('Ctrl Pts',(-8.19687699576229,-14.1158353972228,
118.382294132345)) ;
#156197 = CARTESIAN_POINT('Ctrl Pts',(-8.27068083731801,-14.1158353917364,
118.358063084981)) ;
#156198 = CARTESIAN_POINT('Ctrl Pts',(-8.25362639762513,-14.1684902052981,
118.306118013244)) ;
#156199 = CARTESIAN_POINT('Ctrl Pts',(-8.23657195793224,-14.2211450188598,
118.254172941506)) ;
#156200 = CARTESIAN_POINT('Ctrl Pts',(-8.16276811637651,-14.2211450243462,
118.278403988871)) ;
#156201 = CARTESIAN_POINT('Ctrl Pts',(-8.08896427482079,-14.2211450298325,
118.302635036235)) ;
#156202 = CARTESIAN_POINT('Ctrl Pts',(-8.10601871451368,-14.1684902162708,
118.354580107972)) ;
#156203 = CARTESIAN_POINT('Ctrl Pts',(-8.06327379464778,-13.9330107336615,
118.188967146787)) ;
#156204 = CARTESIAN_POINT('Ctrl Pts',(-8.08407054318253,-13.8967214466837,
118.252310687557)) ;
#156205 = CARTESIAN_POINT('Ctrl Pts',(-8.15787438431086,-13.8967214344113,
118.228079638891)) ;
#156206 = CARTESIAN_POINT('Ctrl Pts',(-8.23167822543917,-13.8967214221389,
118.203848590225)) ;
#156207 = CARTESIAN_POINT('Ctrl Pts',(-8.21088147690444,-13.9330107091168,
118.140505049456)) ;
#156208 = CARTESIAN_POINT('Ctrl Pts',(-8.19008472836968,-13.9692999960946,
118.077161508686)) ;
#156209 = CARTESIAN_POINT('Ctrl Pts',(-8.11628088724137,-13.969300008367,
118.101392557352)) ;
#156210 = CARTESIAN_POINT('Ctrl Pts',(-8.04247704611305,-13.9693000206394,
118.125623606018)) ;
#156211 = CARTESIAN_POINT('Ctrl Pts',(-8.06327379464778,-13.9330107336615,
118.188967146787)) ;
#156212 = CARTESIAN_POINT('Ctrl Pts',(-8.04188464728271,-13.6600763512271,
118.088315145107)) ;
#156213 = CARTESIAN_POINT('Ctrl Pts',(-8.06493974041926,-13.6427914121404,
118.158537239301)) ;
#156214 = CARTESIAN_POINT('Ctrl Pts',(-8.13874358210421,-13.6427913908253,
118.134306192331)) ;
#156215 = CARTESIAN_POINT('Ctrl Pts',(-8.21254742378915,-13.6427913695102,
118.11007514536)) ;
#156216 = CARTESIAN_POINT('Ctrl Pts',(-8.18949233065261,-13.6600763085969,
118.039853051166)) ;
#156217 = CARTESIAN_POINT('Ctrl Pts',(-8.16643723751604,-13.6773612476836,
117.969630956972)) ;
#156218 = CARTESIAN_POINT('Ctrl Pts',(-8.09263339583109,-13.6773612689987,
117.993862003942)) ;
#156219 = CARTESIAN_POINT('Ctrl Pts',(-8.01882955414613,-13.6773612903137,
118.018093050913)) ;
#156220 = CARTESIAN_POINT('Ctrl Pts',(-8.04188464728271,-13.6600763512271,
118.088315145107)) ;
#156221 = CARTESIAN_POINT('Ctrl Pts',(-8.04415984284868,-13.3704757504778,
118.059833665652)) ;
#156222 = CARTESIAN_POINT('Ctrl Pts',(-8.06782216910361,-13.3733860820227,
118.131905294094)) ;
#156223 = CARTESIAN_POINT('Ctrl Pts',(-8.1416260126549,-13.3733860523621,
118.107674252808)) ;
#156224 = CARTESIAN_POINT('Ctrl Pts',(-8.21542985620619,-13.3733860227015,
118.083443211523)) ;
#156225 = CARTESIAN_POINT('Ctrl Pts',(-8.19176752995126,-13.3704756911566,
118.01137158308)) ;
#156226 = CARTESIAN_POINT('Ctrl Pts',(-8.16810520369634,-13.3675653596117,
117.939299954637)) ;
#156227 = CARTESIAN_POINT('Ctrl Pts',(-8.09430136014505,-13.3675653892723,
117.963530995923)) ;
#156228 = CARTESIAN_POINT('Ctrl Pts',(-8.02049751659377,-13.3675654189329,
117.987762037209)) ;
#156229 = CARTESIAN_POINT('Ctrl Pts',(-8.04415984284868,-13.3704757504778,
118.059833665652)) ;
#156230 = CARTESIAN_POINT('Ctrl Pts',(-8.07098859328993,-13.0823700026988,
118.105885959188)) ;
#156231 = CARTESIAN_POINT('Ctrl Pts',(-8.09355009795567,-13.1054004112685,
118.17460466289)) ;
#156232 = CARTESIAN_POINT('Ctrl Pts',(-8.16735394500072,-13.1054003729185,
118.150373632246)) ;
#156233 = CARTESIAN_POINT('Ctrl Pts',(-8.24115779204577,-13.1054003345686,
118.126142601601)) ;
#156234 = CARTESIAN_POINT('Ctrl Pts',(-8.21859628738003,-13.0823699259989,
118.057423897899)) ;
#156235 = CARTESIAN_POINT('Ctrl Pts',(-8.19603478271429,-13.0593395174292,
117.988705194198)) ;
#156236 = CARTESIAN_POINT('Ctrl Pts',(-8.12223093566923,-13.0593395557792,
118.012936224842)) ;
#156237 = CARTESIAN_POINT('Ctrl Pts',(-8.04842708862418,-13.0593395941291,
118.037167255487)) ;
#156238 = CARTESIAN_POINT('Ctrl Pts',(-8.07098859328993,-13.0823700026988,
118.105885959188)) ;
#156239 = CARTESIAN_POINT('Ctrl Pts',(-8.120503467602,-12.8213180178566,118.221441446184)) ;
#156240 = CARTESIAN_POINT('Ctrl Pts',(-8.14036987651576,-12.8626079589609,
118.281951323206)) ;
#156241 = CARTESIAN_POINT('Ctrl Pts',(-8.21417372776093,-12.862607919451,
118.257720305355)) ;
#156242 = CARTESIAN_POINT('Ctrl Pts',(-8.2879775790061,-12.8626078799411,
118.233489287503)) ;
#156243 = CARTESIAN_POINT('Ctrl Pts',(-8.26811117009233,-12.8213179388368,
118.172979410481)) ;
#156244 = CARTESIAN_POINT('Ctrl Pts',(-8.24824476117856,-12.7800279977325,
118.112469533458)) ;
#156245 = CARTESIAN_POINT('Ctrl Pts',(-8.1744409099334,-12.7800280372424,
118.13670055131)) ;
#156246 = CARTESIAN_POINT('Ctrl Pts',(-8.10063705868823,-12.7800280767523,
118.160931569162)) ;
#156247 = CARTESIAN_POINT('Ctrl Pts',(-8.120503467602,-12.8213180178566,118.221441446184)) ;
#156248 = CARTESIAN_POINT('Ctrl Pts',(-8.19068066224925,-12.6009816910039,
118.399651162582)) ;
#156249 = CARTESIAN_POINT('Ctrl Pts',(-8.20641152323964,-12.6577150521394,
118.44756482808)) ;
#156250 = CARTESIAN_POINT('Ctrl Pts',(-8.28021537965013,-12.6577150144821,
118.423333825961)) ;
#156251 = CARTESIAN_POINT('Ctrl Pts',(-8.35401923606062,-12.6577149768248,
118.399102823842)) ;
#156252 = CARTESIAN_POINT('Ctrl Pts',(-8.33828837507023,-12.6009816156892,
118.351189158345)) ;
#156253 = CARTESIAN_POINT('Ctrl Pts',(-8.32255751407984,-12.5442482545536,
118.303275492847)) ;
#156254 = CARTESIAN_POINT('Ctrl Pts',(-8.24875365766935,-12.5442482922109,
118.327506494966)) ;
#156255 = CARTESIAN_POINT('Ctrl Pts',(-8.17494980125887,-12.5442483298683,
118.351737497085)) ;
#156256 = CARTESIAN_POINT('Ctrl Pts',(-8.19068066224925,-12.6009816910039,
118.399651162582)) ;
#156257 = CARTESIAN_POINT('Ctrl Pts',(-8.27663038654765,-12.4399155910324,
118.626049746092)) ;
#156258 = CARTESIAN_POINT('Ctrl Pts',(-8.28711539330814,-12.5079761461326,
118.657985386172)) ;
#156259 = CARTESIAN_POINT('Ctrl Pts',(-8.36091925456453,-12.5079761174331,
118.633754398813)) ;
#156260 = CARTESIAN_POINT('Ctrl Pts',(-8.43472311582091,-12.5079760887335,
118.609523411454)) ;
#156261 = CARTESIAN_POINT('Ctrl Pts',(-8.42423810906042,-12.4399155336333,
118.577587771374)) ;
#156262 = CARTESIAN_POINT('Ctrl Pts',(-8.41375310229993,-12.3718549785331,
118.545652131295)) ;
#156263 = CARTESIAN_POINT('Ctrl Pts',(-8.33994924104354,-12.3718550072327,
118.569883118654)) ;
#156264 = CARTESIAN_POINT('Ctrl Pts',(-8.26614537978715,-12.3718550359322,
118.594114106013)) ;
#156265 = CARTESIAN_POINT('Ctrl Pts',(-8.27663038654765,-12.4399155910324,
118.626049746092)) ;
#156266 = CARTESIAN_POINT('Ctrl Pts',(-8.37377653671491,-12.3483508718252,
118.886335164228)) ;
#156267 = CARTESIAN_POINT('Ctrl Pts',(-8.3782310343859,-12.4229031690547,
118.899902846821)) ;
#156268 = CARTESIAN_POINT('Ctrl Pts',(-8.45203490024531,-12.4229031549688,
118.875671873482)) ;
#156269 = CARTESIAN_POINT('Ctrl Pts',(-8.52583876610469,-12.4229031408829,
118.851440900143)) ;
#156270 = CARTESIAN_POINT('Ctrl Pts',(-8.5213842684337,-12.3483508436534,
118.83787321755)) ;
#156271 = CARTESIAN_POINT('Ctrl Pts',(-8.51692977076269,-12.2737985464239,
118.824305534957)) ;
#156272 = CARTESIAN_POINT('Ctrl Pts',(-8.4431259049033,-12.2737985605098,
118.848536508296)) ;
#156273 = CARTESIAN_POINT('Ctrl Pts',(-8.3693220390439,-12.2737985745957,
118.872767481635)) ;
#156274 = CARTESIAN_POINT('Ctrl Pts',(-8.37377653671491,-12.3483508718252,
118.886335164228)) ;
#156275 = CARTESIAN_POINT('Ctrl Pts',(-8.47470424960895,-12.3338872424077,
119.158388022071)) ;
#156276 = CARTESIAN_POINT('Ctrl Pts',(-8.47285027545596,-12.4095571114995,
119.152741117483)) ;
#156277 = CARTESIAN_POINT('Ctrl Pts',(-8.54665414372756,-12.4095571176329,
119.128510151491)) ;
#156278 = CARTESIAN_POINT('Ctrl Pts',(-8.62045801199916,-12.4095571237664,
119.1042791855)) ;
#156279 = CARTESIAN_POINT('Ctrl Pts',(-8.62231198615215,-12.3338872546745,
119.109926090087)) ;
#156280 = CARTESIAN_POINT('Ctrl Pts',(-8.62416596030512,-12.2582173855827,
119.115572994675)) ;
#156281 = CARTESIAN_POINT('Ctrl Pts',(-8.55036209203353,-12.2582173794493,
119.139803960667)) ;
#156282 = CARTESIAN_POINT('Ctrl Pts',(-8.47655822376192,-12.2582173733159,
119.164034926658)) ;
#156283 = CARTESIAN_POINT('Ctrl Pts',(-8.47470424960895,-12.3338872424077,
119.158388022071)) ;
#156284 = CARTESIAN_POINT('Ctrl Pts',(-8.5740859453798,-12.396923495094,119.425556245681)) ;
#156285 = CARTESIAN_POINT('Ctrl Pts',(-8.5660260133282,-12.4683025104667,
119.401006994805)) ;
#156286 = CARTESIAN_POINT('Ctrl Pts',(-8.63982988237598,-12.4683025400751,
119.376776031178)) ;
#156287 = CARTESIAN_POINT('Ctrl Pts',(-8.71363375142374,-12.4683025696834,
119.35254506755)) ;
#156288 = CARTESIAN_POINT('Ctrl Pts',(-8.72169368347534,-12.3969235543106,
119.377094318426)) ;
#156289 = CARTESIAN_POINT('Ctrl Pts',(-8.72975361552693,-12.3255445389379,
119.401643569301)) ;
#156290 = CARTESIAN_POINT('Ctrl Pts',(-8.65594974647916,-12.3255445093296,
119.425874532929)) ;
#156291 = CARTESIAN_POINT('Ctrl Pts',(-8.58214587743139,-12.3255444797213,
119.450105496557)) ;
#156292 = CARTESIAN_POINT('Ctrl Pts',(-8.5740859453798,-12.396923495094,119.425556245681)) ;
#156293 = CARTESIAN_POINT('Ctrl Pts',(-8.6649277864638,-12.5334553693914,
119.666748762957)) ;
#156294 = CARTESIAN_POINT('Ctrl Pts',(-8.65124833264428,-12.595406254364,
119.625083355602)) ;
#156295 = CARTESIAN_POINT('Ctrl Pts',(-8.72505219984459,-12.5954063084814,
119.600852386347)) ;
#156296 = CARTESIAN_POINT('Ctrl Pts',(-8.79885606704489,-12.5954063625988,
119.576621417092)) ;
#156297 = CARTESIAN_POINT('Ctrl Pts',(-8.81253552086441,-12.5334554776262,
119.618286824447)) ;
#156298 = CARTESIAN_POINT('Ctrl Pts',(-8.82621497468392,-12.4715045926535,
119.659952231802)) ;
#156299 = CARTESIAN_POINT('Ctrl Pts',(-8.75241110748362,-12.4715045385361,
119.684183201057)) ;
#156300 = CARTESIAN_POINT('Ctrl Pts',(-8.67860724028331,-12.4715044844187,
119.708414170312)) ;
#156301 = CARTESIAN_POINT('Ctrl Pts',(-8.6649277864638,-12.5334553693914,
119.666748762957)) ;
#156302 = CARTESIAN_POINT('Ctrl Pts',(-8.74128429943828,-12.7322215761211,
119.863992617795)) ;
#156303 = CARTESIAN_POINT('Ctrl Pts',(-8.72298495132889,-12.7803853400704,
119.808255757934)) ;
#156304 = CARTESIAN_POINT('Ctrl Pts',(-8.7967888140635,-12.7803854158274,
119.784024775078)) ;
#156305 = CARTESIAN_POINT('Ctrl Pts',(-8.8705926767981,-12.7803854915845,
119.759793792221)) ;
#156306 = CARTESIAN_POINT('Ctrl Pts',(-8.88889202490748,-12.7322217276352,
119.815530652082)) ;
#156307 = CARTESIAN_POINT('Ctrl Pts',(-8.90719137301686,-12.6840579636859,
119.871267511943)) ;
#156308 = CARTESIAN_POINT('Ctrl Pts',(-8.83338751028226,-12.6840578879289,
119.895498494799)) ;
#156309 = CARTESIAN_POINT('Ctrl Pts',(-8.75958364754765,-12.6840578121718,
119.919729477656)) ;
#156310 = CARTESIAN_POINT('Ctrl Pts',(-8.74128429943828,-12.7322215761211,
119.863992617795)) ;
#156311 = CARTESIAN_POINT('Ctrl Pts',(-8.79916573819104,-12.9810049412899,
120.004790749052)) ;
#156312 = CARTESIAN_POINT('Ctrl Pts',(-8.77753307281271,-13.0118702151138,
119.938901142704)) ;
#156313 = CARTESIAN_POINT('Ctrl Pts',(-8.85133692912627,-13.0118703086727,
119.91467014029)) ;
#156314 = CARTESIAN_POINT('Ctrl Pts',(-8.92514078543982,-13.0118704022315,
119.890439137876)) ;
#156315 = CARTESIAN_POINT('Ctrl Pts',(-8.94677345081817,-12.9810051284076,
119.956328744224)) ;
#156316 = CARTESIAN_POINT('Ctrl Pts',(-8.96840611619649,-12.9501398545836,
120.022218350571)) ;
#156317 = CARTESIAN_POINT('Ctrl Pts',(-8.89460225988293,-12.9501397610248,
120.046449352985)) ;
#156318 = CARTESIAN_POINT('Ctrl Pts',(-8.82079840356937,-12.9501396674659,
120.070680355399)) ;
#156319 = CARTESIAN_POINT('Ctrl Pts',(-8.79916573819104,-12.9810049412899,
120.004790749052)) ;
#156320 = CARTESIAN_POINT('Ctrl Pts',(-8.83469320205863,-13.2609753303157,
120.077533333241)) ;
#156321 = CARTESIAN_POINT('Ctrl Pts',(-8.81128227802888,-13.2723394892272,
120.006227438023)) ;
#156322 = CARTESIAN_POINT('Ctrl Pts',(-8.88508612624132,-13.2723395935458,
119.981996410934)) ;
#156323 = CARTESIAN_POINT('Ctrl Pts',(-8.95888997445376,-13.2723396978644,
119.957765383845)) ;
#156324 = CARTESIAN_POINT('Ctrl Pts',(-8.9823008984835,-13.260975538953,120.029071279063)) ;
#156325 = CARTESIAN_POINT('Ctrl Pts',(-9.00571182251326,-13.2496113800415,
120.100377174282)) ;
#156326 = CARTESIAN_POINT('Ctrl Pts',(-8.93190797430082,-13.2496112757229,
120.12460820137)) ;
#156327 = CARTESIAN_POINT('Ctrl Pts',(-8.85810412608837,-13.2496111714043,
120.148839228459)) ;
#156328 = CARTESIAN_POINT('Ctrl Pts',(-8.83469320205863,-13.2609753303157,
120.077533333241)) ;
#156329 = CARTESIAN_POINT('Ctrl Pts',(-8.84616539838749,-13.5522070361543,
120.07700191012)) ;
#156330 = CARTESIAN_POINT('Ctrl Pts',(-8.82265305360655,-13.5432552863656,
120.005387103697)) ;
#156331 = CARTESIAN_POINT('Ctrl Pts',(-8.89645689290648,-13.5432553930549,
119.981156049463)) ;
#156332 = CARTESIAN_POINT('Ctrl Pts',(-8.97026073220642,-13.5432554997441,
119.956924995228)) ;
#156333 = CARTESIAN_POINT('Ctrl Pts',(-8.99377307698736,-13.5522072495328,
120.02853980165)) ;
#156334 = CARTESIAN_POINT('Ctrl Pts',(-9.0172854217683,-13.5611589993214,
120.100154608073)) ;
#156335 = CARTESIAN_POINT('Ctrl Pts',(-8.94348158246836,-13.5611588926322,
120.124385662307)) ;
#156336 = CARTESIAN_POINT('Ctrl Pts',(-8.86967774316843,-13.5611587859429,
120.148616716542)) ;
#156337 = CARTESIAN_POINT('Ctrl Pts',(-8.84616539838749,-13.5522070361543,
120.07700191012)) ;
#156338 = CARTESIAN_POINT('Ctrl Pts',(-8.83352879857719,-13.8335794690488,
120.003072712917)) ;
#156339 = CARTESIAN_POINT('Ctrl Pts',(-8.81159729377728,-13.8049701426201,
119.936272890026)) ;
#156340 = CARTESIAN_POINT('Ctrl Pts',(-8.88540112426656,-13.8049702427903,
119.912041808956)) ;
#156341 = CARTESIAN_POINT('Ctrl Pts',(-8.95920495475583,-13.8049703429605,
119.887810727885)) ;
#156342 = CARTESIAN_POINT('Ctrl Pts',(-8.98113645955575,-13.8335796693892,
119.954610550776)) ;
#156343 = CARTESIAN_POINT('Ctrl Pts',(-9.00306796435566,-13.862188995818,
120.021410373666)) ;
#156344 = CARTESIAN_POINT('Ctrl Pts',(-8.92926413386639,-13.8621888956478,
120.045641454737)) ;
#156345 = CARTESIAN_POINT('Ctrl Pts',(-8.8554603033771,-13.8621887954776,
120.069872535807)) ;
#156346 = CARTESIAN_POINT('Ctrl Pts',(-8.83352879857719,-13.8335794690488,
120.003072712917)) ;
#156347 = CARTESIAN_POINT('Ctrl Pts',(-8.79840525558534,-14.0854850074698,
119.86061077159)) ;
#156348 = CARTESIAN_POINT('Ctrl Pts',(-8.77962758865732,-14.0392461681425,
119.803417029983)) ;
#156349 = CARTESIAN_POINT('Ctrl Pts',(-8.85343141133836,-14.0392462534928,
119.77918592513)) ;
#156350 = CARTESIAN_POINT('Ctrl Pts',(-8.92723523401938,-14.039246338843,
119.754954820277)) ;
#156351 = CARTESIAN_POINT('Ctrl Pts',(-8.94601290094739,-14.0854851781703,
119.812148561884)) ;
#156352 = CARTESIAN_POINT('Ctrl Pts',(-8.96479056787539,-14.1317240174977,
119.869342303491)) ;
#156353 = CARTESIAN_POINT('Ctrl Pts',(-8.89098674519436,-14.1317239321474,
119.893573408344)) ;
#156354 = CARTESIAN_POINT('Ctrl Pts',(-8.81718292251333,-14.1317238467972,
119.917804513197)) ;
#156355 = CARTESIAN_POINT('Ctrl Pts',(-8.79840525558534,-14.0854850074698,
119.86061077159)) ;
#156356 = CARTESIAN_POINT('Ctrl Pts',(-8.74411665331808,-14.2893882283517,
119.659805611785)) ;
#156357 = CARTESIAN_POINT('Ctrl Pts',(-8.72983485738257,-14.2288448467623,
119.616305567789)) ;
#156358 = CARTESIAN_POINT('Ctrl Pts',(-8.80363867406561,-14.2288449105474,
119.592074444667)) ;
#156359 = CARTESIAN_POINT('Ctrl Pts',(-8.87744249074863,-14.2288449743324,
119.567843321545)) ;
#156360 = CARTESIAN_POINT('Ctrl Pts',(-8.89172428668414,-14.2893883559219,
119.611343365541)) ;
#156361 = CARTESIAN_POINT('Ctrl Pts',(-8.90600608261964,-14.3499317375113,
119.654843409537)) ;
#156362 = CARTESIAN_POINT('Ctrl Pts',(-8.83220226593662,-14.3499316737262,
119.679074532659)) ;
#156363 = CARTESIAN_POINT('Ctrl Pts',(-8.75839844925359,-14.3499316099411,
119.703305655781)) ;
#156364 = CARTESIAN_POINT('Ctrl Pts',(-8.74411665331808,-14.2893882283517,
119.659805611785)) ;
#156365 = CARTESIAN_POINT('Ctrl Pts',(-8.67521497823715,-14.4310416708449,
119.414456500244)) ;
#156366 = CARTESIAN_POINT('Ctrl Pts',(-8.66645661513697,-14.3605181681089,
119.387779941412)) ;
#156367 = CARTESIAN_POINT('Ctrl Pts',(-8.74026042822641,-14.3605182058442,
119.363548807345)) ;
#156368 = CARTESIAN_POINT('Ctrl Pts',(-8.81406424131583,-14.3605182435796,
119.339317673277)) ;
#156369 = CARTESIAN_POINT('Ctrl Pts',(-8.82282260441602,-14.4310417463156,
119.365994232109)) ;
#156370 = CARTESIAN_POINT('Ctrl Pts',(-8.83158096751619,-14.5015652490516,
119.39267079094)) ;
#156371 = CARTESIAN_POINT('Ctrl Pts',(-8.75777715442677,-14.5015652113162,
119.416901925008)) ;
#156372 = CARTESIAN_POINT('Ctrl Pts',(-8.68397334133732,-14.5015651735809,
119.441133059075)) ;
#156373 = CARTESIAN_POINT('Ctrl Pts',(-8.67521497823715,-14.4310416708449,
119.414456500244)) ;
#156374 = CARTESIAN_POINT('Ctrl Pts',(-8.59746348536126,-14.4999960091202,
119.142167399687)) ;
#156375 = CARTESIAN_POINT('Ctrl Pts',(-8.5948543547224,-14.4245527843061,
119.134220410688)) ;
#156376 = CARTESIAN_POINT('Ctrl Pts',(-8.66865816690361,-14.4245527944394,
119.109989273854)) ;
#156377 = CARTESIAN_POINT('Ctrl Pts',(-8.74246197908482,-14.4245528045727,
119.08575813702)) ;
#156378 = CARTESIAN_POINT('Ctrl Pts',(-8.74507110972368,-14.4999960293868,
119.093705126019)) ;
#156379 = CARTESIAN_POINT('Ctrl Pts',(-8.74768024036255,-14.5754392542009,
119.101652115019)) ;
#156380 = CARTESIAN_POINT('Ctrl Pts',(-8.67387642818134,-14.5754392440676,
119.125883251853)) ;
#156381 = CARTESIAN_POINT('Ctrl Pts',(-8.60007261600012,-14.5754392339344,
119.150114388687)) ;
#156382 = CARTESIAN_POINT('Ctrl Pts',(-8.59746348536126,-14.4999960091202,
119.142167399687)) ;
#156383 = CARTESIAN_POINT('Ctrl Pts',(-8.51725220866625,-14.4914668725251,
118.862420893709)) ;
#156384 = CARTESIAN_POINT('Ctrl Pts',(-8.52097256831155,-14.4165060453907,
118.873752510769)) ;
#156385 = CARTESIAN_POINT('Ctrl Pts',(-8.59477638215005,-14.4165060293028,
118.849521378983)) ;
#156386 = CARTESIAN_POINT('Ctrl Pts',(-8.66858019598853,-14.416506013215,
118.825290247197)) ;
#156387 = CARTESIAN_POINT('Ctrl Pts',(-8.66485983634323,-14.4914668403494,
118.813958630137)) ;
#156388 = CARTESIAN_POINT('Ctrl Pts',(-8.6611394766979,-14.5664276674838,
118.802627013077)) ;
#156389 = CARTESIAN_POINT('Ctrl Pts',(-8.58733566285942,-14.5664276835716,
118.826858144863)) ;
#156390 = CARTESIAN_POINT('Ctrl Pts',(-8.51353184902093,-14.5664276996595,
118.851089276649)) ;
#156391 = CARTESIAN_POINT('Ctrl Pts',(-8.51725220866625,-14.4914668725251,
118.862420893709)) ;
#156392 = CARTESIAN_POINT('Ctrl Pts',(-8.44094453814601,-14.4062237339893,
118.594550823069)) ;
#156393 = CARTESIAN_POINT('Ctrl Pts',(-8.45073164518584,-14.3371017134928,
118.624360773722)) ;
#156394 = CARTESIAN_POINT('Ctrl Pts',(-8.52453546296583,-14.337101674971,
118.600129653941)) ;
#156395 = CARTESIAN_POINT('Ctrl Pts',(-8.59833928074581,-14.3371016364492,
118.57589853416)) ;
#156396 = CARTESIAN_POINT('Ctrl Pts',(-8.58855217370597,-14.4062236569457,
118.546088583507)) ;
#156397 = CARTESIAN_POINT('Ctrl Pts',(-8.57876506666614,-14.4753456774423,
118.516278632854)) ;
#156398 = CARTESIAN_POINT('Ctrl Pts',(-8.50496124888616,-14.4753457159641,
118.540509752635)) ;
#156399 = CARTESIAN_POINT('Ctrl Pts',(-8.43115743110617,-14.4753457544858,
118.564740872416)) ;
#156400 = CARTESIAN_POINT('Ctrl Pts',(-8.44094453814601,-14.4062237339893,
118.594550823069)) ;
#156401 = CARTESIAN_POINT('Ctrl Pts',(-8.37461958404781,-14.2495321967945,
118.356968882225)) ;
#156402 = CARTESIAN_POINT('Ctrl Pts',(-8.38978814218742,-14.1912456004984,
118.403169864494)) ;
#156403 = CARTESIAN_POINT('Ctrl Pts',(-8.46359196581185,-14.1912455461204,
118.378938762515)) ;
#156404 = CARTESIAN_POINT('Ctrl Pts',(-8.53739578943627,-14.1912454917425,
118.354707660535)) ;
#156405 = CARTESIAN_POINT('Ctrl Pts',(-8.52222723129668,-14.2495320880387,
118.308506678265)) ;
#156406 = CARTESIAN_POINT('Ctrl Pts',(-8.50705867315707,-14.3078186843349,
118.262305695995)) ;
#156407 = CARTESIAN_POINT('Ctrl Pts',(-8.43325484953264,-14.3078187387128,
118.286536797975)) ;
#156408 = CARTESIAN_POINT('Ctrl Pts',(-8.3594510259082,-14.3078187930907,
118.310767899955)) ;
#156409 = CARTESIAN_POINT('Ctrl Pts',(-8.37461958404781,-14.2495321967945,
118.356968882225)) ;
#156410 = CARTESIAN_POINT('Ctrl Pts',(-8.32425634296907,-14.0340281298451,
118.168167653125)) ;
#156411 = CARTESIAN_POINT('Ctrl Pts',(-8.34369668060544,-13.990699945468,
118.227379786363)) ;
#156412 = CARTESIAN_POINT('Ctrl Pts',(-8.41750051062051,-13.9906998817967,
118.203148703848)) ;
#156413 = CARTESIAN_POINT('Ctrl Pts',(-8.49130434063558,-13.9906998181254,
118.178917621333)) ;
#156414 = CARTESIAN_POINT('Ctrl Pts',(-8.47186400299921,-14.0340280025025,
118.119705488095)) ;
#156415 = CARTESIAN_POINT('Ctrl Pts',(-8.45242366536283,-14.0773561868796,
118.060493354857)) ;
#156416 = CARTESIAN_POINT('Ctrl Pts',(-8.37861983534776,-14.0773562505509,
118.084724437372)) ;
#156417 = CARTESIAN_POINT('Ctrl Pts',(-8.30481600533269,-14.0773563142222,
118.108955519887)) ;
#156418 = CARTESIAN_POINT('Ctrl Pts',(-8.32425634296907,-14.0340281298451,
118.168167653125)) ;
#156419 = CARTESIAN_POINT('Ctrl Pts',(-8.29382206288613,-13.7742259092907,
118.040014681808)) ;
#156420 = CARTESIAN_POINT('Ctrl Pts',(-8.31615037608938,-13.7489714833696,
118.108023122501)) ;
#156421 = CARTESIAN_POINT('Ctrl Pts',(-8.38995421264838,-13.7489714178304,
118.083792059918)) ;
#156422 = CARTESIAN_POINT('Ctrl Pts',(-8.46375804920739,-13.7489713522911,
118.059560997334)) ;
#156423 = CARTESIAN_POINT('Ctrl Pts',(-8.44142973600415,-13.7742257782122,
117.991552556642)) ;
#156424 = CARTESIAN_POINT('Ctrl Pts',(-8.4191014228009,-13.7994802041333,
117.923544115949)) ;
#156425 = CARTESIAN_POINT('Ctrl Pts',(-8.34529758624189,-13.7994802696726,
117.947775178532)) ;
#156426 = CARTESIAN_POINT('Ctrl Pts',(-8.27149374968289,-13.7994803352118,
117.972006241116)) ;
#156427 = CARTESIAN_POINT('Ctrl Pts',(-8.29382206288613,-13.7742259092907,
118.040014681808)) ;
#156428 = CARTESIAN_POINT('Ctrl Pts',(-8.28631480334285,-13.488993839479,
117.981708548653)) ;
#156429 = CARTESIAN_POINT('Ctrl Pts',(-8.30993444408831,-13.4836161224244,
118.053650164529)) ;
#156430 = CARTESIAN_POINT('Ctrl Pts',(-8.38373828651983,-13.4836160614426,
118.029419119833)) ;
#156431 = CARTESIAN_POINT('Ctrl Pts',(-8.45754212895135,-13.4836160004609,
118.005188075136)) ;
#156432 = CARTESIAN_POINT('Ctrl Pts',(-8.43392248820588,-13.4889937175154,
117.93324645926)) ;
#156433 = CARTESIAN_POINT('Ctrl Pts',(-8.41030284746041,-13.49437143457,117.861304843384)) ;
#156434 = CARTESIAN_POINT('Ctrl Pts',(-8.33649900502889,-13.4943714955518,
117.885535888081)) ;
#156435 = CARTESIAN_POINT('Ctrl Pts',(-8.26269516259738,-13.4943715565336,
117.909766932777)) ;
#156436 = CARTESIAN_POINT('Ctrl Pts',(-8.28631480334285,-13.488993839479,
117.981708548653)) ;
#156437 = CARTESIAN_POINT('Ctrl Pts',(-8.30320195637338,-13.1975717487405,
117.997560479062)) ;
#156438 = CARTESIAN_POINT('Ctrl Pts',(-8.32641478554093,-13.2125333094721,
118.068263012322)) ;
#156439 = CARTESIAN_POINT('Ctrl Pts',(-8.40021863242881,-13.2125332593627,
118.044031981199)) ;
#156440 = CARTESIAN_POINT('Ctrl Pts',(-8.4740224793167,-13.2125332092533,
118.019800950075)) ;
#156441 = CARTESIAN_POINT('Ctrl Pts',(-8.45080965014914,-13.1975716485217,
117.949098416815)) ;
#156442 = CARTESIAN_POINT('Ctrl Pts',(-8.42759682098158,-13.1826100877902,
117.878395883556)) ;
#156443 = CARTESIAN_POINT('Ctrl Pts',(-8.35379297409371,-13.1826101378995,
117.902626914679)) ;
#156444 = CARTESIAN_POINT('Ctrl Pts',(-8.27998912720583,-13.1826101880089,
117.926857945802)) ;
#156445 = CARTESIAN_POINT('Ctrl Pts',(-8.30320195637338,-13.1975717487405,
117.997560479062)) ;
#156446 = CARTESIAN_POINT('Ctrl Pts',(-8.3436703131233,-12.9237175982201,
118.085475777875)) ;
#156447 = CARTESIAN_POINT('Ctrl Pts',(-8.36482407973362,-12.9578227208983,
118.149906738669)) ;
#156448 = CARTESIAN_POINT('Ctrl Pts',(-8.43862792956874,-12.9578226823066,
118.125675716522)) ;
#156449 = CARTESIAN_POINT('Ctrl Pts',(-8.51243177940384,-12.9578226437149,
118.101444694376)) ;
#156450 = CARTESIAN_POINT('Ctrl Pts',(-8.49127801279351,-12.9237175210368,
118.037013733583)) ;
#156451 = CARTESIAN_POINT('Ctrl Pts',(-8.47012424618317,-12.8896123983586,
117.972582772789)) ;
#156452 = CARTESIAN_POINT('Ctrl Pts',(-8.39632039634807,-12.8896124369503,
117.996813794936)) ;
#156453 = CARTESIAN_POINT('Ctrl Pts',(-8.32251654651295,-12.889612475542,
118.021044817082)) ;
#156454 = CARTESIAN_POINT('Ctrl Pts',(-8.3436703131233,-12.9237175982201,
118.085475777875)) ;
#156455 = CARTESIAN_POINT('Ctrl Pts',(-8.4062239104521,-12.6833926232874,
118.240377888327)) ;
#156456 = CARTESIAN_POINT('Ctrl Pts',(-8.4237794536085,-12.7343299181759,
118.293849240853)) ;
#156457 = CARTESIAN_POINT('Ctrl Pts',(-8.49758330427195,-12.7343298939571,
118.26961822123)) ;
#156458 = CARTESIAN_POINT('Ctrl Pts',(-8.57138715493539,-12.7343298697383,
118.245387201606)) ;
#156459 = CARTESIAN_POINT('Ctrl Pts',(-8.553831611779,-12.6833925748499,118.19191584908)) ;
#156460 = CARTESIAN_POINT('Ctrl Pts',(-8.5362760686226,-12.6324552799614,
118.138444496554)) ;
#156461 = CARTESIAN_POINT('Ctrl Pts',(-8.46247221795915,-12.6324553041802,
118.162675516177)) ;
#156462 = CARTESIAN_POINT('Ctrl Pts',(-8.38866836729569,-12.632455328399,
118.186906535801)) ;
#156463 = CARTESIAN_POINT('Ctrl Pts',(-8.4062239104521,-12.6833926232874,
118.240377888327)) ;
#156464 = CARTESIAN_POINT('Ctrl Pts',(-8.48615190099208,-12.4975233316372,
118.448503252107)) ;
#156465 = CARTESIAN_POINT('Ctrl Pts',(-8.4988840715495,-12.5615155230103,
118.48728338981)) ;
#156466 = CARTESIAN_POINT('Ctrl Pts',(-8.57268792207089,-12.5615155094136,
118.463052369754)) ;
#156467 = CARTESIAN_POINT('Ctrl Pts',(-8.64649177259229,-12.561515495817,
118.438821349698)) ;
#156468 = CARTESIAN_POINT('Ctrl Pts',(-8.63375960203489,-12.4975233044439,
118.400041211994)) ;
#156469 = CARTESIAN_POINT('Ctrl Pts',(-8.62102743147748,-12.4335311130708,
118.361261074291)) ;
#156470 = CARTESIAN_POINT('Ctrl Pts',(-8.54722358095607,-12.4335311266674,
118.385492094347)) ;
#156471 = CARTESIAN_POINT('Ctrl Pts',(-8.47341973043468,-12.433531140264,
118.409723114404)) ;
#156472 = CARTESIAN_POINT('Ctrl Pts',(-8.48615190099208,-12.4975233316372,
118.448503252107)) ;
#156473 = CARTESIAN_POINT('Ctrl Pts',(-8.57934667074232,-12.3765652756753,
118.696871045336)) ;
#156474 = CARTESIAN_POINT('Ctrl Pts',(-8.58632526391847,-12.4491001941253,
118.718126714516)) ;
#156475 = CARTESIAN_POINT('Ctrl Pts',(-8.66012911291596,-12.44910018943,118.693895689818)) ;
#156476 = CARTESIAN_POINT('Ctrl Pts',(-8.73393296191344,-12.4491001847347,
118.66966466512)) ;
#156477 = CARTESIAN_POINT('Ctrl Pts',(-8.72695436873729,-12.3765652662847,
118.64840899594)) ;
#156478 = CARTESIAN_POINT('Ctrl Pts',(-8.71997577556115,-12.3040303478347,
118.62715332676)) ;
#156479 = CARTESIAN_POINT('Ctrl Pts',(-8.64617192656366,-12.30403035253,118.651384351458)) ;
#156480 = CARTESIAN_POINT('Ctrl Pts',(-8.57236807756618,-12.3040303572253,
118.675615376155)) ;
#156481 = CARTESIAN_POINT('Ctrl Pts',(-8.57934667074232,-12.3765652756753,
118.696871045336)) ;
#156482 = CARTESIAN_POINT('Ctrl Pts',(-8.67942447659642,-12.3303669115662,
118.966269185261)) ;
#156483 = CARTESIAN_POINT('Ctrl Pts',(-8.68015871203297,-12.4062370893219,
118.968505548159)) ;
#156484 = CARTESIAN_POINT('Ctrl Pts',(-8.75396255910231,-12.4062370896233,
118.944274517589)) ;
#156485 = CARTESIAN_POINT('Ctrl Pts',(-8.82776640617164,-12.4062370899248,
118.920043487018)) ;
#156486 = CARTESIAN_POINT('Ctrl Pts',(-8.82703217073509,-12.3303669121692,
118.91780712412)) ;
#156487 = CARTESIAN_POINT('Ctrl Pts',(-8.82629793529853,-12.2544967344135,
118.915570761222)) ;
#156488 = CARTESIAN_POINT('Ctrl Pts',(-8.7524940882292,-12.2544967341121,
118.939801791793)) ;
#156489 = CARTESIAN_POINT('Ctrl Pts',(-8.67869024115987,-12.2544967338106,
118.964032822363)) ;
#156490 = CARTESIAN_POINT('Ctrl Pts',(-8.67942447659642,-12.3303669115662,
118.966269185261)) ;
#156491 = CARTESIAN_POINT('Ctrl Pts',(-8.78046560292115,-12.3620831181533,
119.23847587387)) ;
#156492 = CARTESIAN_POINT('Ctrl Pts',(-8.77488124433053,-12.4358532268962,
119.221466818734)) ;
#156493 = CARTESIAN_POINT('Ctrl Pts',(-8.84868508924219,-12.4358532286459,
119.197235781592)) ;
#156494 = CARTESIAN_POINT('Ctrl Pts',(-8.92248893415383,-12.4358532303956,
119.173004744449)) ;
#156495 = CARTESIAN_POINT('Ctrl Pts',(-8.92807329274446,-12.3620831216526,
119.190013799585)) ;
#156496 = CARTESIAN_POINT('Ctrl Pts',(-8.93365765133506,-12.2883130129096,
119.20702285472)) ;
#156497 = CARTESIAN_POINT('Ctrl Pts',(-8.85985380642342,-12.28831301116,119.231253891863)) ;
#156498 = CARTESIAN_POINT('Ctrl Pts',(-8.78604996151176,-12.2883130094103,
119.255484929005)) ;
#156499 = CARTESIAN_POINT('Ctrl Pts',(-8.78046560292115,-12.3620831181533,
119.23847587387)) ;
#156500 = CARTESIAN_POINT('Ctrl Pts',(-8.87549407917763,-12.4697592102098,
119.49241363428)) ;
#156501 = CARTESIAN_POINT('Ctrl Pts',(-8.86400045518284,-12.536121336536,
119.457405910088)) ;
#156502 = CARTESIAN_POINT('Ctrl Pts',(-8.93780429864287,-12.5361213369903,
119.433174868524)) ;
#156503 = CARTESIAN_POINT('Ctrl Pts',(-9.0116081421029,-12.5361213374447,
119.40894382696)) ;
#156504 = CARTESIAN_POINT('Ctrl Pts',(-9.02310176609769,-12.4697592111185,
119.443951551152)) ;
#156505 = CARTESIAN_POINT('Ctrl Pts',(-9.03459539009248,-12.4033970847922,
119.478959275343)) ;
#156506 = CARTESIAN_POINT('Ctrl Pts',(-8.96079154663245,-12.4033970843379,
119.503190316907)) ;
#156507 = CARTESIAN_POINT('Ctrl Pts',(-8.88698770317242,-12.4033970838835,
119.527421358471)) ;
#156508 = CARTESIAN_POINT('Ctrl Pts',(-8.87549407917763,-12.4697592102098,
119.49241363428)) ;
#156509 = CARTESIAN_POINT('Ctrl Pts',(-8.95832054343873,-12.6447797711106,
119.709301795168)) ;
#156510 = CARTESIAN_POINT('Ctrl Pts',(-8.94175857502336,-12.6990195583039,
119.658856711595)) ;
#156511 = CARTESIAN_POINT('Ctrl Pts',(-9.0155624178882,-12.69901955683,119.634625668218)) ;
#156512 = CARTESIAN_POINT('Ctrl Pts',(-9.08936626075305,-12.6990195553562,
119.610394624842)) ;
#156513 = CARTESIAN_POINT('Ctrl Pts',(-9.10592822916841,-12.6447797681629,
119.660839708415)) ;
#156514 = CARTESIAN_POINT('Ctrl Pts',(-9.1224901975838,-12.5905399809696,
119.711284791988)) ;
#156515 = CARTESIAN_POINT('Ctrl Pts',(-9.04868635471895,-12.5905399824434,
119.735515835365)) ;
#156516 = CARTESIAN_POINT('Ctrl Pts',(-8.97488251185411,-12.5905399839173,
119.759746878742)) ;
#156517 = CARTESIAN_POINT('Ctrl Pts',(-8.95832054343873,-12.6447797711106,
119.709301795168)) ;
#156518 = CARTESIAN_POINT('Ctrl Pts',(-9.02420754409074,-12.8750273852739,
119.874571217192)) ;
#156519 = CARTESIAN_POINT('Ctrl Pts',(-9.00375303558084,-12.9132697898462,
119.812270084526)) ;
#156520 = CARTESIAN_POINT('Ctrl Pts',(-9.0775568784528,-12.9132697868245,
119.788039041171)) ;
#156521 = CARTESIAN_POINT('Ctrl Pts',(-9.15136072132475,-12.9132697838028,
119.763807997816)) ;
#156522 = CARTESIAN_POINT('Ctrl Pts',(-9.17181522983464,-12.8750273792305,
119.826109130482)) ;
#156523 = CARTESIAN_POINT('Ctrl Pts',(-9.19226973834453,-12.8367849746583,
119.888410263147)) ;
#156524 = CARTESIAN_POINT('Ctrl Pts',(-9.11846589547259,-12.8367849776799,
119.912641306503)) ;
#156525 = CARTESIAN_POINT('Ctrl Pts',(-9.04466205260062,-12.8367849807016,
119.936872349858)) ;
#156526 = CARTESIAN_POINT('Ctrl Pts',(-9.02420754409074,-12.8750273852739,
119.874571217192)) ;
#156527 = CARTESIAN_POINT('Ctrl Pts',(-9.06917668282671,-13.1453257818208,
119.975977828757)) ;
#156528 = CARTESIAN_POINT('Ctrl Pts',(-9.04628767891136,-13.1647498113274,
119.906261615918)) ;
#156529 = CARTESIAN_POINT('Ctrl Pts',(-9.12009152221,-13.1647498092517,119.882030573863)) ;
#156530 = CARTESIAN_POINT('Ctrl Pts',(-9.19389536550866,-13.164749807176,
119.857799531807)) ;
#156531 = CARTESIAN_POINT('Ctrl Pts',(-9.21678436942402,-13.1453257776693,
119.927515744647)) ;
#156532 = CARTESIAN_POINT('Ctrl Pts',(-9.23967337333938,-13.1259017481627,
119.997231957486)) ;
#156533 = CARTESIAN_POINT('Ctrl Pts',(-9.16586953004072,-13.1259017502384,
120.021462999541)) ;
#156534 = CARTESIAN_POINT('Ctrl Pts',(-9.09206568674207,-13.1259017523141,
120.045694041597)) ;
#156535 = CARTESIAN_POINT('Ctrl Pts',(-9.06917668282671,-13.1453257818208,
119.975977828757)) ;
#156536 = CARTESIAN_POINT('Ctrl Pts',(-9.09047067571145,-13.4336234546741,
120.005474883971)) ;
#156537 = CARTESIAN_POINT('Ctrl Pts',(-9.06679306728316,-13.4329452228824,
119.933356709079)) ;
#156538 = CARTESIAN_POINT('Ctrl Pts',(-9.14059691081299,-13.4329452235498,
119.909125667728)) ;
#156539 = CARTESIAN_POINT('Ctrl Pts',(-9.21440075434283,-13.4329452242172,
119.884894626377)) ;
#156540 = CARTESIAN_POINT('Ctrl Pts',(-9.23807836277112,-13.433623456009,
119.957012801268)) ;
#156541 = CARTESIAN_POINT('Ctrl Pts',(-9.2617559711994,-13.4343016878008,
120.02913097616)) ;
#156542 = CARTESIAN_POINT('Ctrl Pts',(-9.18795212766956,-13.4343016871333,
120.053362017511)) ;
#156543 = CARTESIAN_POINT('Ctrl Pts',(-9.11414828413973,-13.4343016864659,
120.077593058863)) ;
#156544 = CARTESIAN_POINT('Ctrl Pts',(-9.09047067571145,-13.4336234546741,
120.005474883971)) ;
#156545 = CARTESIAN_POINT('Ctrl Pts',(-9.08746787607695,-13.7229316022969,
119.960694301127)) ;
#156546 = CARTESIAN_POINT('Ctrl Pts',(-9.06470262091767,-13.7020508739217,
119.891355007195)) ;
#156547 = CARTESIAN_POINT('Ctrl Pts',(-9.13850646392357,-13.7020508801849,
119.867123964248)) ;
#156548 = CARTESIAN_POINT('Ctrl Pts',(-9.21231030692947,-13.7020508864481,
119.842892921301)) ;
#156549 = CARTESIAN_POINT('Ctrl Pts',(-9.23507556208875,-13.7229316148234,
119.912232215233)) ;
#156550 = CARTESIAN_POINT('Ctrl Pts',(-9.25784081724804,-13.7438123431986,
119.981571509164)) ;
#156551 = CARTESIAN_POINT('Ctrl Pts',(-9.18403697424214,-13.7438123369354,
120.005802552111)) ;
#156552 = CARTESIAN_POINT('Ctrl Pts',(-9.11023313123624,-13.7438123306722,
120.030033595058)) ;
#156553 = CARTESIAN_POINT('Ctrl Pts',(-9.08746787607695,-13.7229316022969,
119.960694301127)) ;
#156554 = CARTESIAN_POINT('Ctrl Pts',(-9.06117191970581,-13.9881204584926,
119.845257989114)) ;
#156555 = CARTESIAN_POINT('Ctrl Pts',(-9.0409411018076,-13.948693047744,119.783638182254)) ;
#156556 = CARTESIAN_POINT('Ctrl Pts',(-9.11474494342789,-13.9486930580491,
119.759407135087)) ;
#156557 = CARTESIAN_POINT('Ctrl Pts',(-9.18854878504819,-13.9486930683542,
119.735176087919)) ;
#156558 = CARTESIAN_POINT('Ctrl Pts',(-9.2087796029464,-13.9881204791028,
119.796795894779)) ;
#156559 = CARTESIAN_POINT('Ctrl Pts',(-9.2290104208446,-14.0275478898515,
119.858415701639)) ;
#156560 = CARTESIAN_POINT('Ctrl Pts',(-9.1552065792243,-14.0275478795464,
119.882646748806)) ;
#156561 = CARTESIAN_POINT('Ctrl Pts',(-9.081402737604,-14.0275478692412,119.906877795974)) ;
#156562 = CARTESIAN_POINT('Ctrl Pts',(-9.06117191970581,-13.9881204584926,
119.845257989114)) ;
#156563 = CARTESIAN_POINT('Ctrl Pts',(-9.01419630762022,-14.2135626266573,
119.66671241156)) ;
#156564 = CARTESIAN_POINT('Ctrl Pts',(-8.99794998984458,-14.1583369427659,
119.617228749313)) ;
#156565 = CARTESIAN_POINT('Ctrl Pts',(-9.07175382911603,-14.1583369561378,
119.592997694991)) ;
#156566 = CARTESIAN_POINT('Ctrl Pts',(-9.14555766838748,-14.1583369695098,
119.568766640669)) ;
#156567 = CARTESIAN_POINT('Ctrl Pts',(-9.16180398616311,-14.2135626534012,
119.618250302917)) ;
#156568 = CARTESIAN_POINT('Ctrl Pts',(-9.17805030393876,-14.2687883372926,
119.667733965164)) ;
#156569 = CARTESIAN_POINT('Ctrl Pts',(-9.10424646466731,-14.2687883239207,
119.691965019485)) ;
#156570 = CARTESIAN_POINT('Ctrl Pts',(-9.03044262539586,-14.2687883105487,
119.716196073807)) ;
#156571 = CARTESIAN_POINT('Ctrl Pts',(-9.01419630762022,-14.2135626266573,
119.66671241156)) ;
#156572 = CARTESIAN_POINT('Ctrl Pts',(-8.95045579816424,-14.3820856851378,
119.437041610208)) ;
#156573 = CARTESIAN_POINT('Ctrl Pts',(-8.93937158994986,-14.3150132250762,
119.403280900945)) ;
#156574 = CARTESIAN_POINT('Ctrl Pts',(-9.01317542591036,-14.3150132383268,
119.379049836539)) ;
#156575 = CARTESIAN_POINT('Ctrl Pts',(-9.08697926187084,-14.3150132515775,
119.354818772132)) ;
#156576 = CARTESIAN_POINT('Ctrl Pts',(-9.09806347008522,-14.3820857116392,
119.388579481395)) ;
#156577 = CARTESIAN_POINT('Ctrl Pts',(-9.10914767829959,-14.4491581717009,
119.422340190658)) ;
#156578 = CARTESIAN_POINT('Ctrl Pts',(-9.0353438423391,-14.4491581584502,
119.446571255064)) ;
#156579 = CARTESIAN_POINT('Ctrl Pts',(-8.96154000637861,-14.4491581451995,
119.47080231947)) ;
#156580 = CARTESIAN_POINT('Ctrl Pts',(-8.95045579816424,-14.3820856851378,
119.437041610208)) ;
#156581 = CARTESIAN_POINT('Ctrl Pts',(-8.87581727914137,-14.4811007735871,
119.174352555604)) ;
#156582 = CARTESIAN_POINT('Ctrl Pts',(-8.8706599200612,-14.4070183383993,
119.158644072651)) ;
#156583 = CARTESIAN_POINT('Ctrl Pts',(-8.94446375296266,-14.4070183464706,
119.134412998928)) ;
#156584 = CARTESIAN_POINT('Ctrl Pts',(-9.0182675858641,-14.4070183545419,
119.110181925204)) ;
#156585 = CARTESIAN_POINT('Ctrl Pts',(-9.02342494494427,-14.4811007897297,
119.125890408156)) ;
#156586 = CARTESIAN_POINT('Ctrl Pts',(-9.02858230402444,-14.5551832249176,
119.141598891109)) ;
#156587 = CARTESIAN_POINT('Ctrl Pts',(-8.95477847112299,-14.5551832168463,
119.165829964832)) ;
#156588 = CARTESIAN_POINT('Ctrl Pts',(-8.88097463822153,-14.555183208775,
119.190061038556)) ;
#156589 = CARTESIAN_POINT('Ctrl Pts',(-8.87581727914137,-14.4811007735871,
119.174352555604)) ;
#156590 = CARTESIAN_POINT('Ctrl Pts',(-8.79562316232527,-14.5043853087956,
118.894554465702)) ;
#156591 = CARTESIAN_POINT('Ctrl Pts',(-8.79679290375713,-14.4285698473868,
118.898117310217)) ;
#156592 = CARTESIAN_POINT('Ctrl Pts',(-8.87059673344941,-14.4285698457663,
118.873886226719)) ;
#156593 = CARTESIAN_POINT('Ctrl Pts',(-8.9444005631417,-14.4285698441458,
118.849655143221)) ;
#156594 = CARTESIAN_POINT('Ctrl Pts',(-8.94323082170984,-14.5043853055546,
118.846092298706)) ;
#156595 = CARTESIAN_POINT('Ctrl Pts',(-8.94206108027798,-14.5802007669634,
118.842529454191)) ;
#156596 = CARTESIAN_POINT('Ctrl Pts',(-8.86825725058571,-14.5802007685839,
118.866760537689)) ;
#156597 = CARTESIAN_POINT('Ctrl Pts',(-8.79445342089341,-14.5802007702044,
118.890991621187)) ;
#156598 = CARTESIAN_POINT('Ctrl Pts',(-8.79562316232527,-14.5043853087956,
118.894554465702)) ;
#156599 = CARTESIAN_POINT('Ctrl Pts',(-8.71698219857194,-14.4497319209782,
118.619592459032)) ;
#156600 = CARTESIAN_POINT('Ctrl Pts',(-8.72437748963348,-14.3776228604659,
118.642117323393)) ;
#156601 = CARTESIAN_POINT('Ctrl Pts',(-8.79818131745724,-14.3776228445383,
118.617886234204)) ;
#156602 = CARTESIAN_POINT('Ctrl Pts',(-8.87198514528099,-14.3776228286107,
118.593655145014)) ;
#156603 = CARTESIAN_POINT('Ctrl Pts',(-8.86458985421945,-14.449731889123,
118.571130280654)) ;
#156604 = CARTESIAN_POINT('Ctrl Pts',(-8.85719456315791,-14.5218409496353,
118.548605416293)) ;
#156605 = CARTESIAN_POINT('Ctrl Pts',(-8.78339073533415,-14.5218409655629,
118.572836505482)) ;
#156606 = CARTESIAN_POINT('Ctrl Pts',(-8.7095869075104,-14.5218409814906,
118.597067594671)) ;
#156607 = CARTESIAN_POINT('Ctrl Pts',(-8.71698219857194,-14.4497319209782,
118.619592459032)) ;
#156608 = CARTESIAN_POINT('Ctrl Pts',(-8.64580441276013,-14.3208489038209,
118.36724001526)) ;
#156609 = CARTESIAN_POINT('Ctrl Pts',(-8.65891567247647,-14.25763373208,118.407174798059)) ;
#156610 = CARTESIAN_POINT('Ctrl Pts',(-8.73271949971065,-14.2576336982123,
118.382943707073)) ;
#156611 = CARTESIAN_POINT('Ctrl Pts',(-8.80652332694482,-14.2576336643446,
118.358712616088)) ;
#156612 = CARTESIAN_POINT('Ctrl Pts',(-8.79341206722847,-14.3208488360855,
118.318777833289)) ;
#156613 = CARTESIAN_POINT('Ctrl Pts',(-8.78030080751211,-14.3840640078265,
118.278843050491)) ;
#156614 = CARTESIAN_POINT('Ctrl Pts',(-8.70649698027795,-14.3840640416942,
118.303074141476)) ;
#156615 = CARTESIAN_POINT('Ctrl Pts',(-8.63269315304377,-14.3840640755619,
118.327305232461)) ;
#156616 = CARTESIAN_POINT('Ctrl Pts',(-8.64580441276013,-14.3208489038209,
118.36724001526)) ;
#156617 = CARTESIAN_POINT('Ctrl Pts',(-8.5883553866719,-14.1269083086763,
118.156726837458)) ;
#156618 = CARTESIAN_POINT('Ctrl Pts',(-8.60623187044661,-14.0771420046429,
118.211175724042)) ;
#156619 = CARTESIAN_POINT('Ctrl Pts',(-8.68003569934284,-14.0771419513953,
118.18694463812)) ;
#156620 = CARTESIAN_POINT('Ctrl Pts',(-8.75383952823908,-14.0771418981477,
118.162713552197)) ;
#156621 = CARTESIAN_POINT('Ctrl Pts',(-8.73596304446436,-14.1269082021811,
118.108264665612)) ;
#156622 = CARTESIAN_POINT('Ctrl Pts',(-8.71808656068964,-14.1766745062146,
118.053815779028)) ;
#156623 = CARTESIAN_POINT('Ctrl Pts',(-8.64428273179342,-14.1766745594622,
118.07804686495)) ;
#156624 = CARTESIAN_POINT('Ctrl Pts',(-8.57047890289718,-14.1766746127098,
118.102277950873)) ;
#156625 = CARTESIAN_POINT('Ctrl Pts',(-8.5883553866719,-14.1269083086763,
118.156726837458)) ;
#156626 = CARTESIAN_POINT('Ctrl Pts',(-8.54955936673305,-13.8839530008224,
118.003271664693)) ;
#156627 = CARTESIAN_POINT('Ctrl Pts',(-8.5709004469701,-13.8510774674815,
118.068273153212)) ;
#156628 = CARTESIAN_POINT('Ctrl Pts',(-8.64470427993426,-13.8510773982051,
118.044042079679)) ;
#156629 = CARTESIAN_POINT('Ctrl Pts',(-8.71850811289841,-13.8510773289287,
118.019811006147)) ;
#156630 = CARTESIAN_POINT('Ctrl Pts',(-8.69716703266136,-13.8839528622696,
117.954809517628)) ;
#156631 = CARTESIAN_POINT('Ctrl Pts',(-8.6758259524243,-13.9168283956105,
117.88980802911)) ;
#156632 = CARTESIAN_POINT('Ctrl Pts',(-8.60202211946015,-13.9168284648869,
117.914039102643)) ;
#156633 = CARTESIAN_POINT('Ctrl Pts',(-8.52821828649599,-13.9168285341632,
117.938270176175)) ;
#156634 = CARTESIAN_POINT('Ctrl Pts',(-8.54955936673305,-13.8839530008224,
118.003271664693)) ;
#156635 = CARTESIAN_POINT('Ctrl Pts',(-8.53248329253628,-13.6058131007772,
117.915704634662)) ;
#156636 = CARTESIAN_POINT('Ctrl Pts',(-8.55578333401837,-13.592308546656,
117.986672803208)) ;
#156637 = CARTESIAN_POINT('Ctrl Pts',(-8.62958717268441,-13.5923084632408,
117.962441747043)) ;
#156638 = CARTESIAN_POINT('Ctrl Pts',(-8.70339101135044,-13.5923083798256,
117.938210690877)) ;
#156639 = CARTESIAN_POINT('Ctrl Pts',(-8.68009096986836,-13.6058129339469,
117.867242522331)) ;
#156640 = CARTESIAN_POINT('Ctrl Pts',(-8.65679092838625,-13.6193174880682,
117.796274353786)) ;
#156641 = CARTESIAN_POINT('Ctrl Pts',(-8.58298708972022,-13.6193175714834,
117.820505409951)) ;
#156642 = CARTESIAN_POINT('Ctrl Pts',(-8.50918325105419,-13.6193176548985,
117.844736466117)) ;
#156643 = CARTESIAN_POINT('Ctrl Pts',(-8.53248329253628,-13.6058131007772,
117.915704634662)) ;
#156644 = CARTESIAN_POINT('Ctrl Pts',(-8.53937026013509,-13.3154623494247,
117.901296893058)) ;
#156645 = CARTESIAN_POINT('Ctrl Pts',(-8.56295544834905,-13.3222095128514,
117.973133572653)) ;
#156646 = CARTESIAN_POINT('Ctrl Pts',(-8.63675929426366,-13.3222094225439,
117.948902538566)) ;
#156647 = CARTESIAN_POINT('Ctrl Pts',(-8.71056314017827,-13.3222093322365,
117.924671504478)) ;
#156648 = CARTESIAN_POINT('Ctrl Pts',(-8.68697795196431,-13.3154621688099,
117.852834824883)) ;
#156649 = CARTESIAN_POINT('Ctrl Pts',(-8.66339276375033,-13.3087150053832,
117.780998145287)) ;
#156650 = CARTESIAN_POINT('Ctrl Pts',(-8.58958891783573,-13.3087150956907,
117.805229179375)) ;
#156651 = CARTESIAN_POINT('Ctrl Pts',(-8.51578507192111,-13.3087151859981,
117.829460213462)) ;
#156652 = CARTESIAN_POINT('Ctrl Pts',(-8.53937026013509,-13.3154623494247,
117.901296893058)) ;
#156653 = CARTESIAN_POINT('Ctrl Pts',(-8.57069168239456,-13.0305252756843,
117.961054033285)) ;
#156654 = CARTESIAN_POINT('Ctrl Pts',(-8.59286220817367,-13.057175468413,
118.028581879486)) ;
#156655 = CARTESIAN_POINT('Ctrl Pts',(-8.66666606225781,-13.0571753774731,
118.004350870281)) ;
#156656 = CARTESIAN_POINT('Ctrl Pts',(-8.74046991634194,-13.0571752865332,
117.980119861077)) ;
#156657 = CARTESIAN_POINT('Ctrl Pts',(-8.71829939056283,-13.0305250938045,
117.912592014877)) ;
#156658 = CARTESIAN_POINT('Ctrl Pts',(-8.69612886478371,-13.0038749010759,
117.845064168676)) ;
#156659 = CARTESIAN_POINT('Ctrl Pts',(-8.62232501069957,-13.0038749920158,
117.869295177881)) ;
#156660 = CARTESIAN_POINT('Ctrl Pts',(-8.54852115661543,-13.0038750829557,
117.893526187085)) ;
#156661 = CARTESIAN_POINT('Ctrl Pts',(-8.57069168239456,-13.0305252756843,
117.961054033285)) ;
#156662 = CARTESIAN_POINT('Ctrl Pts',(-8.62430702145784,-12.7760411077928,
118.089081673625)) ;
#156663 = CARTESIAN_POINT('Ctrl Pts',(-8.64349646537957,-12.8204973460342,
118.147529625551)) ;
#156664 = CARTESIAN_POINT('Ctrl Pts',(-8.71730032725692,-12.8204972646132,
118.123298640083)) ;
#156665 = CARTESIAN_POINT('Ctrl Pts',(-8.79110418913424,-12.8204971831922,
118.099067654616)) ;
#156666 = CARTESIAN_POINT('Ctrl Pts',(-8.77191474521251,-12.7760409449508,
118.04061970269)) ;
#156667 = CARTESIAN_POINT('Ctrl Pts',(-8.75272530129079,-12.7315847067095,
117.982171750764)) ;
#156668 = CARTESIAN_POINT('Ctrl Pts',(-8.67892143941345,-12.7315847881305,
118.006402736232)) ;
#156669 = CARTESIAN_POINT('Ctrl Pts',(-8.60511757753611,-12.7315848695515,
118.030633721699)) ;
#156670 = CARTESIAN_POINT('Ctrl Pts',(-8.62430702145784,-12.7760411077928,
118.089081673625)) ;
#156671 = CARTESIAN_POINT('Ctrl Pts',(-8.69778013803695,-12.5658693797106,
118.277375059853)) ;
#156672 = CARTESIAN_POINT('Ctrl Pts',(-8.71260256265765,-12.6250641545161,
118.322521775676)) ;
#156673 = CARTESIAN_POINT('Ctrl Pts',(-8.78640643152489,-12.6250640894152,
118.298290811498)) ;
#156674 = CARTESIAN_POINT('Ctrl Pts',(-8.86021030039212,-12.6250640243143,
118.274059847321)) ;
#156675 = CARTESIAN_POINT('Ctrl Pts',(-8.84538787577142,-12.5658692495088,
118.228913131498)) ;
#156676 = CARTESIAN_POINT('Ctrl Pts',(-8.83056545115072,-12.5066744747032,
118.183766415675)) ;
#156677 = CARTESIAN_POINT('Ctrl Pts',(-8.75676158228349,-12.5066745398042,
118.207997379852)) ;
#156678 = CARTESIAN_POINT('Ctrl Pts',(-8.68295771341625,-12.506674604905,
118.232228344029)) ;
#156679 = CARTESIAN_POINT('Ctrl Pts',(-8.69778013803695,-12.5658693797106,
118.277375059853)) ;
#156680 = CARTESIAN_POINT('Ctrl Pts',(-8.78628545767639,-12.4170609140262,
118.511509776539)) ;
#156681 = CARTESIAN_POINT('Ctrl Pts',(-8.79568383392516,-12.4867319202062,
118.540135716234)) ;
#156682 = CARTESIAN_POINT('Ctrl Pts',(-8.86948770797218,-12.4867318782286,
118.515904767834)) ;
#156683 = CARTESIAN_POINT('Ctrl Pts',(-8.94329158201918,-12.4867318362511,
118.491673819433)) ;
#156684 = CARTESIAN_POINT('Ctrl Pts',(-8.9338932057704,-12.4170608300712,
118.463047879737)) ;
#156685 = CARTESIAN_POINT('Ctrl Pts',(-8.92449482952162,-12.3473898238912,
118.434421940042)) ;
#156686 = CARTESIAN_POINT('Ctrl Pts',(-8.85069095547461,-12.3473898658687,
118.458652888443)) ;
#156687 = CARTESIAN_POINT('Ctrl Pts',(-8.7768870814276,-12.3473899078463,
118.482883836843)) ;
#156688 = CARTESIAN_POINT('Ctrl Pts',(-8.78628545767639,-12.4170609140262,
118.511509776539)) ;
#156689 = CARTESIAN_POINT('Ctrl Pts',(-8.88463232709871,-12.3396249333132,
118.775501151269)) ;
#156690 = CARTESIAN_POINT('Ctrl Pts',(-8.8879141833157,-12.4148052434578,
118.785497157874)) ;
#156691 = CARTESIAN_POINT('Ctrl Pts',(-8.9617180602112,-12.4148052290128,
118.761266218149)) ;
#156692 = CARTESIAN_POINT('Ctrl Pts',(-9.0355219371067,-12.4148052145678,
118.737035278425)) ;
#156693 = CARTESIAN_POINT('Ctrl Pts',(-9.03224008088971,-12.3396249044232,
118.72703927182)) ;
#156694 = CARTESIAN_POINT('Ctrl Pts',(-9.02895822467271,-12.2644445942785,
118.717043265215)) ;
#156695 = CARTESIAN_POINT('Ctrl Pts',(-8.95515434777721,-12.2644446087235,
118.74127420494)) ;
#156696 = CARTESIAN_POINT('Ctrl Pts',(-8.88135047088172,-12.2644446231686,
118.765505144665)) ;
#156697 = CARTESIAN_POINT('Ctrl Pts',(-8.88463232709871,-12.3396249333132,
118.775501151269)) ;
#156698 = CARTESIAN_POINT('Ctrl Pts',(-8.9861492359783,-12.340046412335,119.04917803503)) ;
#156699 = CARTESIAN_POINT('Ctrl Pts',(-8.98308354184458,-12.4153088432885,
119.03984042744)) ;
#156700 = CARTESIAN_POINT('Ctrl Pts',(-9.05688741871824,-12.4153088579802,
119.015609487649)) ;
#156701 = CARTESIAN_POINT('Ctrl Pts',(-9.13069129559191,-12.4153088726718,
118.991378547857)) ;
#156702 = CARTESIAN_POINT('Ctrl Pts',(-9.13375698972563,-12.3400464417183,
119.000716155448)) ;
#156703 = CARTESIAN_POINT('Ctrl Pts',(-9.13682268385935,-12.2647840107648,
119.010053763039)) ;
#156704 = CARTESIAN_POINT('Ctrl Pts',(-9.06301880698568,-12.2647839960732,
119.03428470283)) ;
#156705 = CARTESIAN_POINT('Ctrl Pts',(-8.98921493011202,-12.2647839813815,
119.058515642621)) ;
#156706 = CARTESIAN_POINT('Ctrl Pts',(-8.9861492359783,-12.340046412335,119.04917803503)) ;
#156707 = CARTESIAN_POINT('Ctrl Pts',(-9.08378193823022,-12.4170460254182,
119.311248494083)) ;
#156708 = CARTESIAN_POINT('Ctrl Pts',(-9.07462576737877,-12.4870438442232,
119.283360277089)) ;
#156709 = CARTESIAN_POINT('Ctrl Pts',(-9.14842964160796,-12.487043886487,
119.259129329243)) ;
#156710 = CARTESIAN_POINT('Ctrl Pts',(-9.22223351583714,-12.4870439287509,
119.234898381398)) ;
#156711 = CARTESIAN_POINT('Ctrl Pts',(-9.23138968668858,-12.4170461099459,
119.262786598391)) ;
#156712 = CARTESIAN_POINT('Ctrl Pts',(-9.24054585754002,-12.3470482911409,
119.290674815385)) ;
#156713 = CARTESIAN_POINT('Ctrl Pts',(-9.16674198331085,-12.3470482488771,
119.314905763231)) ;
#156714 = CARTESIAN_POINT('Ctrl Pts',(-9.09293810908166,-12.3470482066133,
119.339136711077)) ;
#156715 = CARTESIAN_POINT('Ctrl Pts',(-9.08378193823022,-12.4170460254182,
119.311248494083)) ;
#156716 = CARTESIAN_POINT('Ctrl Pts',(-9.17250255530307,-12.5662136094611,
119.545947051563)) ;
#156717 = CARTESIAN_POINT('Ctrl Pts',(-9.1578737421701,-12.625901534808,119.501390049144)) ;
#156718 = CARTESIAN_POINT('Ctrl Pts',(-9.23167761123566,-12.6259016005162,
119.477159085571)) ;
#156719 = CARTESIAN_POINT('Ctrl Pts',(-9.3054814803012,-12.6259016662244,
119.452928121997)) ;
#156720 = CARTESIAN_POINT('Ctrl Pts',(-9.32011029343416,-12.5662137408776,
119.497485124416)) ;
#156721 = CARTESIAN_POINT('Ctrl Pts',(-9.33473910656713,-12.5065258155307,
119.542042126834)) ;
#156722 = CARTESIAN_POINT('Ctrl Pts',(-9.26093523750158,-12.5065257498225,
119.566273090408)) ;
#156723 = CARTESIAN_POINT('Ctrl Pts',(-9.18713136843604,-12.5065256841143,
119.590504053981)) ;
#156724 = CARTESIAN_POINT('Ctrl Pts',(-9.17250255530307,-12.5662136094611,
119.545947051563)) ;
#156725 = CARTESIAN_POINT('Ctrl Pts',(-9.24585112857785,-12.7760199991739,
119.733930887948)) ;
#156726 = CARTESIAN_POINT('Ctrl Pts',(-9.22681247363185,-12.8211489416697,
119.675942218833)) ;
#156727 = CARTESIAN_POINT('Ctrl Pts',(-9.30061633575258,-12.8211490243987,
119.651711234107)) ;
#156728 = CARTESIAN_POINT('Ctrl Pts',(-9.37442019787332,-12.8211491071278,
119.627480249381)) ;
#156729 = CARTESIAN_POINT('Ctrl Pts',(-9.39345885281933,-12.776020164632,
119.685468918496)) ;
#156730 = CARTESIAN_POINT('Ctrl Pts',(-9.41249750776533,-12.7308912221363,
119.743457587611)) ;
#156731 = CARTESIAN_POINT('Ctrl Pts',(-9.33869364564458,-12.7308911394072,
119.767688572337)) ;
#156732 = CARTESIAN_POINT('Ctrl Pts',(-9.26488978352385,-12.7308910566782,
119.791919557063)) ;
#156733 = CARTESIAN_POINT('Ctrl Pts',(-9.24585112857785,-12.7760199991739,
119.733930887948)) ;
#156734 = CARTESIAN_POINT('Ctrl Pts',(-9.29969159508292,-13.0322696653641,
119.862416821601)) ;
#156735 = CARTESIAN_POINT('Ctrl Pts',(-9.27760000870786,-13.0595756323769,
119.795129415856)) ;
#156736 = CARTESIAN_POINT('Ctrl Pts',(-9.35140386280755,-13.059575723918,
119.770898406699)) ;
#156737 = CARTESIAN_POINT('Ctrl Pts',(-9.42520771690725,-13.0595758154591,
119.746667397542)) ;
#156738 = CARTESIAN_POINT('Ctrl Pts',(-9.44729930328231,-13.0322698484462,
119.813954803287)) ;
#156739 = CARTESIAN_POINT('Ctrl Pts',(-9.46939088965738,-13.0049638814334,
119.881242209032)) ;
#156740 = CARTESIAN_POINT('Ctrl Pts',(-9.39558703555768,-13.0049637898923,
119.905473218189)) ;
#156741 = CARTESIAN_POINT('Ctrl Pts',(-9.32178318145799,-13.0049636983512,
119.929704227346)) ;
#156742 = CARTESIAN_POINT('Ctrl Pts',(-9.29969159508292,-13.0322696653641,
119.862416821601)) ;
#156743 = CARTESIAN_POINT('Ctrl Pts',(-9.33072971583805,-13.3151090323585,
119.921587753964)) ;
#156744 = CARTESIAN_POINT('Ctrl Pts',(-9.30716980380042,-13.3227086607463,
119.849828065076)) ;
#156745 = CARTESIAN_POINT('Ctrl Pts',(-9.38097364977465,-13.3227087535366,
119.82559703117)) ;
#156746 = CARTESIAN_POINT('Ctrl Pts',(-9.4547774957489,-13.3227088463268,
119.801365997264)) ;
#156747 = CARTESIAN_POINT('Ctrl Pts',(-9.47833740778652,-13.315109217939,
119.873125686152)) ;
#156748 = CARTESIAN_POINT('Ctrl Pts',(-9.50189731982416,-13.3075095895512,
119.944885375041)) ;
#156749 = CARTESIAN_POINT('Ctrl Pts',(-9.42809347384992,-13.307509496761,
119.969116408947)) ;
#156750 = CARTESIAN_POINT('Ctrl Pts',(-9.35428962787569,-13.3075094039707,
119.993347442852)) ;
#156751 = CARTESIAN_POINT('Ctrl Pts',(-9.33072971583805,-13.3151090323585,
119.921587753964)) ;
#156752 = CARTESIAN_POINT('Ctrl Pts',(-9.33762134165996,-13.6075492018493,
119.906927850832)) ;
#156753 = CARTESIAN_POINT('Ctrl Pts',(-9.31428227870287,-13.5947427678056,
119.835840832465)) ;
#156754 = CARTESIAN_POINT('Ctrl Pts',(-9.38808611725758,-13.5947428521219,
119.81160977596)) ;
#156755 = CARTESIAN_POINT('Ctrl Pts',(-9.4618899558123,-13.594742936438,119.787378719456)) ;
#156756 = CARTESIAN_POINT('Ctrl Pts',(-9.48522901876938,-13.6075493704817,
119.858465737822)) ;
#156757 = CARTESIAN_POINT('Ctrl Pts',(-9.50856808172646,-13.6203558045254,
119.929552756189)) ;
#156758 = CARTESIAN_POINT('Ctrl Pts',(-9.43476424317175,-13.6203557202092,
119.953783812694)) ;
#156759 = CARTESIAN_POINT('Ctrl Pts',(-9.36096040461704,-13.620355635893,
119.978014869198)) ;
#156760 = CARTESIAN_POINT('Ctrl Pts',(-9.33762134165996,-13.6075492018493,
119.906927850832)) ;
#156761 = CARTESIAN_POINT('Ctrl Pts',(-9.32055446084888,-13.8839937911961,
119.819605029903)) ;
#156762 = CARTESIAN_POINT('Ctrl Pts',(-9.29910313304257,-13.8518669319433,
119.754267748105)) ;
#156763 = CARTESIAN_POINT('Ctrl Pts',(-9.37290696562471,-13.8518670036745,
119.730036673409)) ;
#156764 = CARTESIAN_POINT('Ctrl Pts',(-9.44671079820685,-13.8518670754058,
119.705805598712)) ;
#156765 = CARTESIAN_POINT('Ctrl Pts',(-9.46816212601316,-13.8839939346586,
119.771142880511)) ;
#156766 = CARTESIAN_POINT('Ctrl Pts',(-9.48961345381948,-13.9161207939113,
119.83648016231)) ;
#156767 = CARTESIAN_POINT('Ctrl Pts',(-9.41580962123734,-13.9161207221801,
119.860711237006)) ;
#156768 = CARTESIAN_POINT('Ctrl Pts',(-9.3420057886552,-13.9161206504489,
119.884942311702)) ;
#156769 = CARTESIAN_POINT('Ctrl Pts',(-9.32055446084888,-13.8839937911961,
119.819605029903)) ;
#156770 = CARTESIAN_POINT('Ctrl Pts',(-9.28147726722591,-14.1283418739825,
119.665069210431)) ;
#156771 = CARTESIAN_POINT('Ctrl Pts',(-9.2634566491389,-14.0791061363548,
119.610181316741)) ;
#156772 = CARTESIAN_POINT('Ctrl Pts',(-9.33726047777319,-14.079106190233,
119.58595023002)) ;
#156773 = CARTESIAN_POINT('Ctrl Pts',(-9.41106430640748,-14.0791062441112,
119.561719143299)) ;
#156774 = CARTESIAN_POINT('Ctrl Pts',(-9.42908492449449,-14.1283419817388,
119.61660703699)) ;
#156775 = CARTESIAN_POINT('Ctrl Pts',(-9.44710554258149,-14.1775777193664,
119.671494930681)) ;
#156776 = CARTESIAN_POINT('Ctrl Pts',(-9.37330171394721,-14.1775776654883,
119.695726017402)) ;
#156777 = CARTESIAN_POINT('Ctrl Pts',(-9.29949788531291,-14.1775776116101,
119.719957104122)) ;
#156778 = CARTESIAN_POINT('Ctrl Pts',(-9.28147726722591,-14.1283418739825,
119.665069210431)) ;
#156779 = CARTESIAN_POINT('Ctrl Pts',(-9.22417716238159,-14.321085337762,
119.455168775729)) ;
#156780 = CARTESIAN_POINT('Ctrl Pts',(-9.21086198390688,-14.2583178356259,
119.414612891736)) ;
#156781 = CARTESIAN_POINT('Ctrl Pts',(-9.28466581049705,-14.2583178709165,
119.390381798789)) ;
#156782 = CARTESIAN_POINT('Ctrl Pts',(-9.35846963708723,-14.2583179062071,
119.366150705843)) ;
#156783 = CARTESIAN_POINT('Ctrl Pts',(-9.37178481556196,-14.3210854083432,
119.406706589835)) ;
#156784 = CARTESIAN_POINT('Ctrl Pts',(-9.38509999403666,-14.3838529104793,
119.447262473828)) ;
#156785 = CARTESIAN_POINT('Ctrl Pts',(-9.31129616744649,-14.3838528751887,
119.471493566774)) ;
#156786 = CARTESIAN_POINT('Ctrl Pts',(-9.23749234085631,-14.3838528398981,
119.495724659721)) ;
#156787 = CARTESIAN_POINT('Ctrl Pts',(-9.22417716238159,-14.321085337762,
119.455168775729)) ;
#156788 = CARTESIAN_POINT('Ctrl Pts',(-9.1528918141783,-14.4501544762085,
119.202433516862)) ;
#156789 = CARTESIAN_POINT('Ctrl Pts',(-9.1452704554292,-14.3782797175252,
119.179220088868)) ;
#156790 = CARTESIAN_POINT('Ctrl Pts',(-9.21907428260848,-14.378279733915,
119.154988997716)) ;
#156791 = CARTESIAN_POINT('Ctrl Pts',(-9.29287810978775,-14.3782797503047,
119.130757906563)) ;
#156792 = CARTESIAN_POINT('Ctrl Pts',(-9.30049946853686,-14.450154508988,
119.153971334557)) ;
#156793 = CARTESIAN_POINT('Ctrl Pts',(-9.30812082728596,-14.5220292676713,
119.177184762551)) ;
#156794 = CARTESIAN_POINT('Ctrl Pts',(-9.23431700010668,-14.5220292512815,
119.201415853704)) ;
#156795 = CARTESIAN_POINT('Ctrl Pts',(-9.1605131729274,-14.5220292348918,
119.225646944856)) ;
#156796 = CARTESIAN_POINT('Ctrl Pts',(-9.1528918141783,-14.4501544762085,
119.202433516862)) ;
#156797 = CARTESIAN_POINT('Ctrl Pts',(-9.07410157725992,-14.504350239421,
118.926962323926)) ;
#156798 = CARTESIAN_POINT('Ctrl Pts',(-9.07270431240989,-14.4285822954382,
118.922706481521)) ;
#156799 = CARTESIAN_POINT('Ctrl Pts',(-9.14650814161148,-14.4285822971821,
118.898475396528)) ;
#156800 = CARTESIAN_POINT('Ctrl Pts',(-9.22031197081306,-14.4285822989259,
118.874244311535)) ;
#156801 = CARTESIAN_POINT('Ctrl Pts',(-9.2217092356631,-14.5043502429086,
118.87850015394)) ;
#156802 = CARTESIAN_POINT('Ctrl Pts',(-9.22310650051312,-14.5801181868914,
118.882755996344)) ;
#156803 = CARTESIAN_POINT('Ctrl Pts',(-9.14930267131155,-14.5801181851475,
118.906987081337)) ;
#156804 = CARTESIAN_POINT('Ctrl Pts',(-9.07549884210995,-14.5801181834037,
118.93121816633)) ;
#156805 = CARTESIAN_POINT('Ctrl Pts',(-9.07410157725992,-14.504350239421,
118.926962323926)) ;
#156806 = CARTESIAN_POINT('Ctrl Pts',(-8.99439714763998,-14.4811635345991,
118.648874617531)) ;
#156807 = CARTESIAN_POINT('Ctrl Pts',(-8.99929378974257,-14.4069000332384,
118.663789000046)) ;
#156808 = CARTESIAN_POINT('Ctrl Pts',(-9.0730976215289,-14.4069000243761,
118.639557922925)) ;
#156809 = CARTESIAN_POINT('Ctrl Pts',(-9.14690145331523,-14.4069000155138,
118.615326845805)) ;
#156810 = CARTESIAN_POINT('Ctrl Pts',(-9.14200481121263,-14.4811635168746,
118.600412463291)) ;
#156811 = CARTESIAN_POINT('Ctrl Pts',(-9.13710816911003,-14.5554270182353,
118.585498080776)) ;
#156812 = CARTESIAN_POINT('Ctrl Pts',(-9.0633043373237,-14.5554270270976,
118.609729157896)) ;
#156813 = CARTESIAN_POINT('Ctrl Pts',(-8.98950050553737,-14.5554270359599,
118.633960235017)) ;
#156814 = CARTESIAN_POINT('Ctrl Pts',(-8.99439714763998,-14.4811635345991,
118.648874617531)) ;
#156815 = CARTESIAN_POINT('Ctrl Pts',(-8.91938092952298,-14.3816036851556,
118.384850057937)) ;
#156816 = CARTESIAN_POINT('Ctrl Pts',(-8.93025827732114,-14.3141789361096,
118.417980704839)) ;
#156817 = CARTESIAN_POINT('Ctrl Pts',(-9.00406211280163,-14.3141789218921,
118.393749638971)) ;
#156818 = CARTESIAN_POINT('Ctrl Pts',(-9.0778659482821,-14.3141789076745,
118.369518573102)) ;
#156819 = CARTESIAN_POINT('Ctrl Pts',(-9.06698860048393,-14.3816036567204,
118.3363879262)) ;
#156820 = CARTESIAN_POINT('Ctrl Pts',(-9.05611125268575,-14.4490284057664,
118.303257279298)) ;
#156821 = CARTESIAN_POINT('Ctrl Pts',(-8.98230741720528,-14.449028419984,
118.327488345167)) ;
#156822 = CARTESIAN_POINT('Ctrl Pts',(-8.9085035817248,-14.4490284342016,
118.351719411035)) ;
#156823 = CARTESIAN_POINT('Ctrl Pts',(-8.91938092952298,-14.3816036851556,
118.384850057937)) ;
#156824 = CARTESIAN_POINT('Ctrl Pts',(-8.8558492241993,-14.2132115910195,
118.155902462999)) ;
#156825 = CARTESIAN_POINT('Ctrl Pts',(-8.8719124615394,-14.1574425718006,
118.204828492554)) ;
#156826 = CARTESIAN_POINT('Ctrl Pts',(-8.94571630025698,-14.1574425567691,
118.180597436545)) ;
#156827 = CARTESIAN_POINT('Ctrl Pts',(-9.01952013897455,-14.1574425417376,
118.156366380536)) ;
#156828 = CARTESIAN_POINT('Ctrl Pts',(-9.00345690163445,-14.2132115609565,
118.107440350981)) ;
#156829 = CARTESIAN_POINT('Ctrl Pts',(-8.98739366429436,-14.2689805801753,
118.058514321426)) ;
#156830 = CARTESIAN_POINT('Ctrl Pts',(-8.91358982557679,-14.2689805952068,
118.082745377435)) ;
#156831 = CARTESIAN_POINT('Ctrl Pts',(-8.8397859868592,-14.2689806102383,
118.106976433443)) ;
#156832 = CARTESIAN_POINT('Ctrl Pts',(-8.8558492241993,-14.2132115910195,
118.155902462999)) ;
#156833 = CARTESIAN_POINT('Ctrl Pts',(-8.80875359263179,-13.9871283531687,
117.97689596451)) ;
#156834 = CARTESIAN_POINT('Ctrl Pts',(-8.8288655504278,-13.9470611393289,
118.038153743158)) ;
#156835 = CARTESIAN_POINT('Ctrl Pts',(-8.9026693918761,-13.9470611278095,
118.013922695466)) ;
#156836 = CARTESIAN_POINT('Ctrl Pts',(-8.97647323332439,-13.9470611162902,
117.989691647775)) ;
#156837 = CARTESIAN_POINT('Ctrl Pts',(-8.95636127552838,-13.98712833013,117.928433869127)) ;
#156838 = CARTESIAN_POINT('Ctrl Pts',(-8.93624931773237,-14.0271955439699,
117.86717609048)) ;
#156839 = CARTESIAN_POINT('Ctrl Pts',(-8.86244547628407,-14.0271955554892,
117.891407138171)) ;
#156840 = CARTESIAN_POINT('Ctrl Pts',(-8.78864163483579,-14.0271955670085,
117.915638185862)) ;
#156841 = CARTESIAN_POINT('Ctrl Pts',(-8.80875359263179,-13.9871283531687,
117.97689596451)) ;
#156842 = CARTESIAN_POINT('Ctrl Pts',(-8.78260162901795,-13.7209751384546,
117.86180531742)) ;
#156843 = CARTESIAN_POINT('Ctrl Pts',(-8.80530328477739,-13.6994320003675,
117.930950898101)) ;
#156844 = CARTESIAN_POINT('Ctrl Pts',(-8.87910712770323,-13.6994319934453,
117.90671985491)) ;
#156845 = CARTESIAN_POINT('Ctrl Pts',(-8.95291097062908,-13.699431986523,
117.882488811719)) ;
#156846 = CARTESIAN_POINT('Ctrl Pts',(-8.93020931486964,-13.72097512461,117.813343231038)) ;
#156847 = CARTESIAN_POINT('Ctrl Pts',(-8.9075076591102,-13.7425182626971,
117.744197650356)) ;
#156848 = CARTESIAN_POINT('Ctrl Pts',(-8.83370381618435,-13.7425182696194,
117.768428693547)) ;
#156849 = CARTESIAN_POINT('Ctrl Pts',(-8.75989997325851,-13.7425182765416,
117.792659736738)) ;
#156850 = CARTESIAN_POINT('Ctrl Pts',(-8.78260162901795,-13.7209751384546,
117.86180531742)) ;
#156851 = CARTESIAN_POINT('Ctrl Pts',(-8.7796418761099,-13.4341833204507,
117.817471206849)) ;
#156852 = CARTESIAN_POINT('Ctrl Pts',(-8.80331509092212,-13.4326332891495,
117.889575999558)) ;
#156853 = CARTESIAN_POINT('Ctrl Pts',(-8.87711893444489,-13.4326332865185,
117.865344958186)) ;
#156854 = CARTESIAN_POINT('Ctrl Pts',(-8.95092277796765,-13.4326332838874,
117.841113916813)) ;
#156855 = CARTESIAN_POINT('Ctrl Pts',(-8.92724956315542,-13.4341833151887,
117.769009124103)) ;
#156856 = CARTESIAN_POINT('Ctrl Pts',(-8.90357634834319,-13.4357333464899,
117.696904331393)) ;
#156857 = CARTESIAN_POINT('Ctrl Pts',(-8.82977250482043,-13.435733349121,
117.721135372766)) ;
#156858 = CARTESIAN_POINT('Ctrl Pts',(-8.75596866129766,-13.435733351752,
117.745366414139)) ;
#156859 = CARTESIAN_POINT('Ctrl Pts',(-8.7796418761099,-13.4341833204507,
117.817471206849)) ;
#156860 = CARTESIAN_POINT('Ctrl Pts',(-8.80108831291345,-13.1440226446982,
117.847195297999)) ;
#156861 = CARTESIAN_POINT('Ctrl Pts',(-8.82403622680466,-13.1627318776024,
117.917090941048)) ;
#156862 = CARTESIAN_POINT('Ctrl Pts',(-8.89784007017418,-13.1627318792492,
117.892859899208)) ;
#156863 = CARTESIAN_POINT('Ctrl Pts',(-8.97164391354369,-13.1627318808959,
117.868628857369)) ;
#156864 = CARTESIAN_POINT('Ctrl Pts',(-8.94869599965246,-13.1440226479917,
117.79873321432)) ;
#156865 = CARTESIAN_POINT('Ctrl Pts',(-8.92574808576123,-13.1253134150875,
117.72883757127)) ;
#156866 = CARTESIAN_POINT('Ctrl Pts',(-8.85194424239172,-13.1253134134407,
117.75306861311)) ;
#156867 = CARTESIAN_POINT('Ctrl Pts',(-8.7781403990222,-13.125313411794,117.77729965495)) ;
#156868 = CARTESIAN_POINT('Ctrl Pts',(-8.80108831291345,-13.1440226446982,
117.847195297999)) ;
#156869 = CARTESIAN_POINT('Ctrl Pts',(-8.84592426043001,-12.8750223963181,
117.948364040509)) ;
#156870 = CARTESIAN_POINT('Ctrl Pts',(-8.86650795627559,-12.9125432630704,
118.011058656823)) ;
#156871 = CARTESIAN_POINT('Ctrl Pts',(-8.94031179917461,-12.9125432659671,
117.986827613551)) ;
#156872 = CARTESIAN_POINT('Ctrl Pts',(-9.01411564207361,-12.9125432688638,
117.962596570278)) ;
#156873 = CARTESIAN_POINT('Ctrl Pts',(-8.99353194622804,-12.8750224021116,
117.899901953963)) ;
#156874 = CARTESIAN_POINT('Ctrl Pts',(-8.97294825038245,-12.8375015353593,
117.837207337649)) ;
#156875 = CARTESIAN_POINT('Ctrl Pts',(-8.89914440748345,-12.8375015324626,
117.861438380922)) ;
#156876 = CARTESIAN_POINT('Ctrl Pts',(-8.82534056458443,-12.8375015295659,
117.885669424194)) ;
#156877 = CARTESIAN_POINT('Ctrl Pts',(-8.84592426043001,-12.8750223963181,
117.948364040509)) ;
#156878 = CARTESIAN_POINT('Ctrl Pts',(-8.91216833972909,-12.6437154561283,
118.114539740324)) ;
#156879 = CARTESIAN_POINT('Ctrl Pts',(-8.92889332303276,-12.6974444198838,
118.165481340849)) ;
#156880 = CARTESIAN_POINT('Ctrl Pts',(-9.00269716581704,-12.6974444216942,
118.141250297227)) ;
#156881 = CARTESIAN_POINT('Ctrl Pts',(-9.07650100860129,-12.6974444235046,
118.117019253605)) ;
#156882 = CARTESIAN_POINT('Ctrl Pts',(-9.05977602529763,-12.6437154597491,
118.06607765308)) ;
#156883 = CARTESIAN_POINT('Ctrl Pts',(-9.04305104199395,-12.5899864959936,
118.015136052555)) ;
#156884 = CARTESIAN_POINT('Ctrl Pts',(-8.96924719920968,-12.5899864941832,
118.039367096177)) ;
#156885 = CARTESIAN_POINT('Ctrl Pts',(-8.89544335642542,-12.5899864923728,
118.063598139799)) ;
#156886 = CARTESIAN_POINT('Ctrl Pts',(-8.91216833972909,-12.6437154561283,
118.114539740324)) ;
#156887 = CARTESIAN_POINT('Ctrl Pts',(-8.99483011325719,-12.4695015573388,
118.331032618802)) ;
#156888 = CARTESIAN_POINT('Ctrl Pts',(-9.00653775971677,-12.5354737259947,
118.366692220884)) ;
#156889 = CARTESIAN_POINT('Ctrl Pts',(-9.08034160291349,-12.5354737260558,
118.342461178518)) ;
#156890 = CARTESIAN_POINT('Ctrl Pts',(-9.15414544611019,-12.5354737261168,
118.318230136152)) ;
#156891 = CARTESIAN_POINT('Ctrl Pts',(-9.1424377996506,-12.4695015574609,
118.28257053407)) ;
#156892 = CARTESIAN_POINT('Ctrl Pts',(-9.130730153191,-12.403529388805,118.246910931988)) ;
#156893 = CARTESIAN_POINT('Ctrl Pts',(-9.0569263099943,-12.403529388744,118.271141974354)) ;
#156894 = CARTESIAN_POINT('Ctrl Pts',(-8.98312246679759,-12.4035293886829,
118.29537301672)) ;
#156895 = CARTESIAN_POINT('Ctrl Pts',(-8.99483011325719,-12.4695015573388,
118.331032618802)) ;
#156896 = CARTESIAN_POINT('Ctrl Pts',(-9.08998111303647,-12.3618253102505,
118.585299380963)) ;
#156897 = CARTESIAN_POINT('Ctrl Pts',(-9.09579750273664,-12.4354130130407,
118.603015165592)) ;
#156898 = CARTESIAN_POINT('Ctrl Pts',(-9.16960134725352,-12.4354130116483,
118.578784127247)) ;
#156899 = CARTESIAN_POINT('Ctrl Pts',(-9.2434051917704,-12.4354130102558,
118.554553088902)) ;
#156900 = CARTESIAN_POINT('Ctrl Pts',(-9.23758880207023,-12.3618253074657,
118.536837304273)) ;
#156901 = CARTESIAN_POINT('Ctrl Pts',(-9.23177241237007,-12.2882376046756,
118.519121519645)) ;
#156902 = CARTESIAN_POINT('Ctrl Pts',(-9.15796856785319,-12.288237606068,
118.543352557989)) ;
#156903 = CARTESIAN_POINT('Ctrl Pts',(-9.0841647233363,-12.2882376074604,
118.567583596334)) ;
#156904 = CARTESIAN_POINT('Ctrl Pts',(-9.08998111303647,-12.3618253102505,
118.585299380963)) ;
#156905 = CARTESIAN_POINT('Ctrl Pts',(-9.1909709333649,-12.3304086987919,
118.857374561843)) ;
#156906 = CARTESIAN_POINT('Ctrl Pts',(-9.19047930770828,-12.406297480682,
118.855877149609)) ;
#156907 = CARTESIAN_POINT('Ctrl Pts',(-9.26428315423005,-12.4062974803833,
118.83164611737)) ;
#156908 = CARTESIAN_POINT('Ctrl Pts',(-9.3380870007518,-12.4062974800845,
118.807415085132)) ;
#156909 = CARTESIAN_POINT('Ctrl Pts',(-9.33857862640842,-12.3304086981944,
118.808912497366)) ;
#156910 = CARTESIAN_POINT('Ctrl Pts',(-9.33907025206503,-12.2545199163043,
118.8104099096)) ;
#156911 = CARTESIAN_POINT('Ctrl Pts',(-9.26526640554327,-12.2545199166031,
118.834640941838)) ;
#156912 = CARTESIAN_POINT('Ctrl Pts',(-9.19146255902151,-12.2545199169019,
118.858871974077)) ;
#156913 = CARTESIAN_POINT('Ctrl Pts',(-9.1909709333649,-12.3304086987919,
118.857374561843)) ;
#156914 = CARTESIAN_POINT('Ctrl Pts',(-9.29090632432286,-12.3767667157857,
119.126380154863)) ;
#156915 = CARTESIAN_POINT('Ctrl Pts',(-9.28416836803978,-12.4495286298161,
119.105857427502)) ;
#156916 = CARTESIAN_POINT('Ctrl Pts',(-9.35797221631645,-12.4495286339673,
119.081626400609)) ;
#156917 = CARTESIAN_POINT('Ctrl Pts',(-9.43177606459311,-12.4495286381184,
119.057395373716)) ;
#156918 = CARTESIAN_POINT('Ctrl Pts',(-9.4385140208762,-12.376766724088,119.077918101077)) ;
#156919 = CARTESIAN_POINT('Ctrl Pts',(-9.4452519771593,-12.3040048100576,
119.098440828438)) ;
#156920 = CARTESIAN_POINT('Ctrl Pts',(-9.37144812888264,-12.3040048059064,
119.122671855331)) ;
#156921 = CARTESIAN_POINT('Ctrl Pts',(-9.29764428060597,-12.3040048017553,
119.146902882224)) ;
#156922 = CARTESIAN_POINT('Ctrl Pts',(-9.29090632432286,-12.3767667157857,
119.126380154863)) ;
#156923 = CARTESIAN_POINT('Ctrl Pts',(-9.38394796937826,-12.4973266925111,
119.374354583408)) ;
#156924 = CARTESIAN_POINT('Ctrl Pts',(-9.37143676374085,-12.5617762145597,
119.336247470161)) ;
#156925 = CARTESIAN_POINT('Ctrl Pts',(-9.44524061342147,-12.5617762263117,
119.312016447545)) ;
#156926 = CARTESIAN_POINT('Ctrl Pts',(-9.51904446310207,-12.5617762380637,
119.287785424927)) ;
#156927 = CARTESIAN_POINT('Ctrl Pts',(-9.53155566873948,-12.497326716015,
119.325892538174)) ;
#156928 = CARTESIAN_POINT('Ctrl Pts',(-9.54406687437688,-12.4328771939664,
119.36399965142)) ;
#156929 = CARTESIAN_POINT('Ctrl Pts',(-9.47026302469627,-12.4328771822144,
119.388230674037)) ;
#156930 = CARTESIAN_POINT('Ctrl Pts',(-9.39645917501566,-12.4328771704624,
119.412461696654)) ;
#156931 = CARTESIAN_POINT('Ctrl Pts',(-9.38394796937826,-12.4973266925111,
119.374354583408)) ;
#156932 = CARTESIAN_POINT('Ctrl Pts',(-9.4644362377349,-12.6849702880242,
119.583900943341)) ;
#156933 = CARTESIAN_POINT('Ctrl Pts',(-9.4470238617794,-12.7364118506539,
119.530865656292)) ;
#156934 = CARTESIAN_POINT('Ctrl Pts',(-9.52082771227271,-12.7364118743968,
119.506634636151)) ;
#156935 = CARTESIAN_POINT('Ctrl Pts',(-9.59463156276601,-12.7364118981397,
119.482403616009)) ;
#156936 = CARTESIAN_POINT('Ctrl Pts',(-9.61204393872151,-12.68497033551,119.535438903058)) ;
#156937 = CARTESIAN_POINT('Ctrl Pts',(-9.62945631467699,-12.6335287728803,
119.588474190107)) ;
#156938 = CARTESIAN_POINT('Ctrl Pts',(-9.5556524641837,-12.6335287491374,
119.612705210249)) ;
#156939 = CARTESIAN_POINT('Ctrl Pts',(-9.48184861369038,-12.6335287253945,
119.63693623039)) ;
#156940 = CARTESIAN_POINT('Ctrl Pts',(-9.4644362377349,-12.6849702880242,
119.583900943341)) ;
#156941 = CARTESIAN_POINT('Ctrl Pts',(-9.5264642676195,-12.9239536141708,
119.737443599299)) ;
#156942 = CARTESIAN_POINT('Ctrl Pts',(-9.50542818056897,-12.958783516276,
119.67337107309)) ;
#156943 = CARTESIAN_POINT('Ctrl Pts',(-9.57923202992662,-12.9587835522301,
119.649140049489)) ;
#156944 = CARTESIAN_POINT('Ctrl Pts',(-9.65303587928429,-12.9587835881843,
119.624909025889)) ;
#156945 = CARTESIAN_POINT('Ctrl Pts',(-9.67407196633483,-12.9239536860792,
119.688981552098)) ;
#156946 = CARTESIAN_POINT('Ctrl Pts',(-9.69510805338537,-12.889123783974,
119.753054078307)) ;
#156947 = CARTESIAN_POINT('Ctrl Pts',(-9.6213042040277,-12.8891237480199,
119.777285101908)) ;
#156948 = CARTESIAN_POINT('Ctrl Pts',(-9.54750035467004,-12.8891237120657,
119.801516125509)) ;
#156949 = CARTESIAN_POINT('Ctrl Pts',(-9.5264642676195,-12.9239536141708,
119.737443599299)) ;
#156950 = CARTESIAN_POINT('Ctrl Pts',(-9.56699499377198,-13.198264514804,
119.825482569648)) ;
#156951 = CARTESIAN_POINT('Ctrl Pts',(-9.54383147105243,-13.2139924714054,
119.754930217809)) ;
#156952 = CARTESIAN_POINT('Ctrl Pts',(-9.61763531776289,-13.2139925191053,
119.730699186145)) ;
#156953 = CARTESIAN_POINT('Ctrl Pts',(-9.69143916447335,-13.2139925668051,
119.706468154482)) ;
#156954 = CARTESIAN_POINT('Ctrl Pts',(-9.71460268719289,-13.1982646102037,
119.777020506321)) ;
#156955 = CARTESIAN_POINT('Ctrl Pts',(-9.73776620991244,-13.1825366536022,
119.847572858159)) ;
#156956 = CARTESIAN_POINT('Ctrl Pts',(-9.66396236320198,-13.1825366059024,
119.871803889823)) ;
#156957 = CARTESIAN_POINT('Ctrl Pts',(-9.59015851649152,-13.1825365582025,
119.896034921487)) ;
#156958 = CARTESIAN_POINT('Ctrl Pts',(-9.56699499377198,-13.198264514804,
119.825482569648)) ;
#156959 = CARTESIAN_POINT('Ctrl Pts',(-9.58379794756891,-13.4887696764051,
119.841196258796)) ;
#156960 = CARTESIAN_POINT('Ctrl Pts',(-9.56016164623923,-13.4842376804655,
119.769203899761)) ;
#156961 = CARTESIAN_POINT('Ctrl Pts',(-9.63396548872277,-13.4842377379434,
119.744972855222)) ;
#156962 = CARTESIAN_POINT('Ctrl Pts',(-9.70776933120628,-13.4842377954214,
119.720741810684)) ;
#156963 = CARTESIAN_POINT('Ctrl Pts',(-9.73140563253596,-13.488769791361,
119.792734169719)) ;
#156964 = CARTESIAN_POINT('Ctrl Pts',(-9.75504193386563,-13.4933017873006,
119.864726528754)) ;
#156965 = CARTESIAN_POINT('Ctrl Pts',(-9.68123809138211,-13.4933017298226,
119.888957573292)) ;
#156966 = CARTESIAN_POINT('Ctrl Pts',(-9.60743424889859,-13.4933016723446,
119.91318861783)) ;
#156967 = CARTESIAN_POINT('Ctrl Pts',(-9.58379794756891,-13.4887696764051,
119.841196258796)) ;
#156968 = CARTESIAN_POINT('Ctrl Pts',(-9.57628694483019,-13.7747050880232,
119.782787604556)) ;
#156969 = CARTESIAN_POINT('Ctrl Pts',(-9.55387601395397,-13.7502030722453,
119.714527526385)) ;
#156970 = CARTESIAN_POINT('Ctrl Pts',(-9.62767985077114,-13.7502031353853,
119.690296464588)) ;
#156971 = CARTESIAN_POINT('Ctrl Pts',(-9.70148368758833,-13.7502031985253,
119.666065402791)) ;
#156972 = CARTESIAN_POINT('Ctrl Pts',(-9.72389461846455,-13.7747052143032,
119.734325480963)) ;
#156973 = CARTESIAN_POINT('Ctrl Pts',(-9.74630554934077,-13.7992072300811,
119.802585559134)) ;
#156974 = CARTESIAN_POINT('Ctrl Pts',(-9.67250171252359,-13.7992071669411,
119.826816620931)) ;
#156975 = CARTESIAN_POINT('Ctrl Pts',(-9.59869787570641,-13.7992071038011,
119.851047682728)) ;
#156976 = CARTESIAN_POINT('Ctrl Pts',(-9.57628694483019,-13.7747050880232,
119.782787604556)) ;
#156977 = CARTESIAN_POINT('Ctrl Pts',(-9.54578275574017,-14.0346989777519,
119.65439454944)) ;
#156978 = CARTESIAN_POINT('Ctrl Pts',(-9.5262032717922,-13.9920093582588,
119.594758601917)) ;
#156979 = CARTESIAN_POINT('Ctrl Pts',(-9.60000710216503,-13.9920094202152,
119.570527520491)) ;
#156980 = CARTESIAN_POINT('Ctrl Pts',(-9.67381093253786,-13.9920094821717,
119.546296439066)) ;
#156981 = CARTESIAN_POINT('Ctrl Pts',(-9.69339041648583,-14.0346991016648,
119.605932386589)) ;
#156982 = CARTESIAN_POINT('Ctrl Pts',(-9.71296990043381,-14.077388721158,
119.665568334113)) ;
#156983 = CARTESIAN_POINT('Ctrl Pts',(-9.63916607006098,-14.0773886592015,
119.689799415538)) ;
#156984 = CARTESIAN_POINT('Ctrl Pts',(-9.56536223968815,-14.077388597245,
119.714030496963)) ;
#156985 = CARTESIAN_POINT('Ctrl Pts',(-9.54578275574017,-14.0346989777519,
119.65439454944)) ;
#156986 = CARTESIAN_POINT('Ctrl Pts',(-9.49516719411495,-14.2504823475427,
119.464718649369)) ;
#156987 = CARTESIAN_POINT('Ctrl Pts',(-9.47982784694189,-14.1926653559339,
119.417997474467)) ;
#156988 = CARTESIAN_POINT('Ctrl Pts',(-9.5536316707946,-14.192665409366,119.393766373183)) ;
#156989 = CARTESIAN_POINT('Ctrl Pts',(-9.62743549464732,-14.1926654627981,
119.369535271898)) ;
#156990 = CARTESIAN_POINT('Ctrl Pts',(-9.64277484182037,-14.2504824544068,
119.4162564468)) ;
#156991 = CARTESIAN_POINT('Ctrl Pts',(-9.65811418899341,-14.3082994460156,
119.462977621703)) ;
#156992 = CARTESIAN_POINT('Ctrl Pts',(-9.58431036514069,-14.3082993925835,
119.487208722987)) ;
#156993 = CARTESIAN_POINT('Ctrl Pts',(-9.51050654128798,-14.3082993391515,
119.511439824272)) ;
#156994 = CARTESIAN_POINT('Ctrl Pts',(-9.49516719411495,-14.2504823475427,
119.464718649369)) ;
#156995 = CARTESIAN_POINT('Ctrl Pts',(-9.42925750378619,-14.4061007577842,
119.228637274552)) ;
#156996 = CARTESIAN_POINT('Ctrl Pts',(-9.41922861107984,-14.3373352952271,
119.198090887228)) ;
#156997 = CARTESIAN_POINT('Ctrl Pts',(-9.49303242959301,-14.3373353326338,
119.17385976968)) ;
#156998 = CARTESIAN_POINT('Ctrl Pts',(-9.56683624810616,-14.3373353700405,
119.149628652132)) ;
#156999 = CARTESIAN_POINT('Ctrl Pts',(-9.57686514081249,-14.4061008325976,
119.180175039457)) ;
#157000 = CARTESIAN_POINT('Ctrl Pts',(-9.58689403351884,-14.4748662951547,
119.210721426781)) ;
#157001 = CARTESIAN_POINT('Ctrl Pts',(-9.51309021500568,-14.474866257748,
119.234952544329)) ;
#157002 = CARTESIAN_POINT('Ctrl Pts',(-9.43928639649253,-14.4748662203413,
119.259183661877)) ;
#157003 = CARTESIAN_POINT('Ctrl Pts',(-9.42925750378619,-14.4061007577842,
119.228637274552)) ;
#157004 = CARTESIAN_POINT('Ctrl Pts',(-9.35244000585146,-14.4917978275685,
118.958975475398)) ;
#157005 = CARTESIAN_POINT('Ctrl Pts',(-9.34849792368344,-14.4169485235802,
118.946968531011)) ;
#157006 = CARTESIAN_POINT('Ctrl Pts',(-9.42230173775408,-14.4169485394119,
118.922737399932)) ;
#157007 = CARTESIAN_POINT('Ctrl Pts',(-9.49610555182472,-14.4169485552436,
118.898506268853)) ;
#157008 = CARTESIAN_POINT('Ctrl Pts',(-9.50004763399274,-14.4917978592319,
118.91051321324)) ;
#157009 = CARTESIAN_POINT('Ctrl Pts',(-9.50398971616077,-14.5666471632202,
118.922520157628)) ;
#157010 = CARTESIAN_POINT('Ctrl Pts',(-9.43018590209014,-14.5666471473885,
118.946751288707)) ;
#157011 = CARTESIAN_POINT('Ctrl Pts',(-9.35638208801949,-14.5666471315568,
118.970982419786)) ;
#157012 = CARTESIAN_POINT('Ctrl Pts',(-9.35244000585146,-14.4917978275685,
118.958975475398)) ;
#157013 = CARTESIAN_POINT('Ctrl Pts',(-9.27254720983972,-14.4998539330622,
118.680348428381)) ;
#157014 = CARTESIAN_POINT('Ctrl Pts',(-9.27490739751976,-14.4243333592347,
118.687537181156)) ;
#157015 = CARTESIAN_POINT('Ctrl Pts',(-9.34871121015168,-14.4243333490761,
118.663306045695)) ;
#157016 = CARTESIAN_POINT('Ctrl Pts',(-9.42251502278361,-14.4243333389175,
118.639074910234)) ;
#157017 = CARTESIAN_POINT('Ctrl Pts',(-9.42015483510357,-14.4998539127449,
118.631886157459)) ;
#157018 = CARTESIAN_POINT('Ctrl Pts',(-9.41779464742353,-14.5753744865724,
118.624697404683)) ;
#157019 = CARTESIAN_POINT('Ctrl Pts',(-9.3439908347916,-14.575374496731,118.648928540144)) ;
#157020 = CARTESIAN_POINT('Ctrl Pts',(-9.27018702215968,-14.5753745068897,
118.673159675605)) ;
#157021 = CARTESIAN_POINT('Ctrl Pts',(-9.27254720983972,-14.4998539330622,
118.680348428381)) ;
#157022 = CARTESIAN_POINT('Ctrl Pts',(-9.19483422021103,-14.4309092256038,
118.408185227294)) ;
#157023 = CARTESIAN_POINT('Ctrl Pts',(-9.20335723096026,-14.3600915226302,
118.434144944847)) ;
#157024 = CARTESIAN_POINT('Ctrl Pts',(-9.27716104438173,-14.3600914852358,
118.409913811791)) ;
#157025 = CARTESIAN_POINT('Ctrl Pts',(-9.35096485780319,-14.3600914478414,
118.385682678734)) ;
#157026 = CARTESIAN_POINT('Ctrl Pts',(-9.34244184705396,-14.430909150815,
118.359722961181)) ;
#157027 = CARTESIAN_POINT('Ctrl Pts',(-9.33391883630474,-14.5017268537886,
118.333763243628)) ;
#157028 = CARTESIAN_POINT('Ctrl Pts',(-9.26011502288327,-14.501726891183,
118.357994376684)) ;
#157029 = CARTESIAN_POINT('Ctrl Pts',(-9.1863112094618,-14.5017269285774,
118.38222550974)) ;
#157030 = CARTESIAN_POINT('Ctrl Pts',(-9.19483422021103,-14.4309092256038,
118.408185227294)) ;
#157031 = CARTESIAN_POINT('Ctrl Pts',(-9.12600873086239,-14.2894596882656,
118.163115988674)) ;
#157032 = CARTESIAN_POINT('Ctrl Pts',(-9.14008263562817,-14.2284134835687,
118.205982833824)) ;
#157033 = CARTESIAN_POINT('Ctrl Pts',(-9.21388645251701,-14.2284134202247,
118.181751711328)) ;
#157034 = CARTESIAN_POINT('Ctrl Pts',(-9.28769026940583,-14.2284133568807,
118.157520588833)) ;
#157035 = CARTESIAN_POINT('Ctrl Pts',(-9.27361636464005,-14.2894595615776,
118.114653743684)) ;
#157036 = CARTESIAN_POINT('Ctrl Pts',(-9.25954245987426,-14.3505057662746,
118.071786898535)) ;
#157037 = CARTESIAN_POINT('Ctrl Pts',(-9.18573864298543,-14.3505058296186,
118.09601802103)) ;
#157038 = CARTESIAN_POINT('Ctrl Pts',(-9.1119348260966,-14.3505058929625,
118.120249143525)) ;
#157039 = CARTESIAN_POINT('Ctrl Pts',(-9.12600873086239,-14.2894596882656,
118.163115988674)) ;
#157040 = CARTESIAN_POINT('Ctrl Pts',(-9.07154849099475,-14.0846391379262,
117.961648450783)) ;
#157041 = CARTESIAN_POINT('Ctrl Pts',(-9.09018180458957,-14.0378023203219,
118.018402519606)) ;
#157042 = CARTESIAN_POINT('Ctrl Pts',(-9.16398562735108,-14.0378022350358,
117.994171414998)) ;
#157043 = CARTESIAN_POINT('Ctrl Pts',(-9.23778945011258,-14.0378021497496,
117.96994031039)) ;
#157044 = CARTESIAN_POINT('Ctrl Pts',(-9.21915613651776,-14.0846389673539,
117.913186241567)) ;
#157045 = CARTESIAN_POINT('Ctrl Pts',(-9.20052282292294,-14.1314757849582,
117.856432172745)) ;
#157046 = CARTESIAN_POINT('Ctrl Pts',(-9.12671900016143,-14.1314758702443,
117.880663277353)) ;
#157047 = CARTESIAN_POINT('Ctrl Pts',(-9.05291517739992,-14.1314759555304,
117.904894381961)) ;
#157048 = CARTESIAN_POINT('Ctrl Pts',(-9.07154849099475,-14.0846391379262,
117.961648450783)) ;
#157049 = CARTESIAN_POINT('Ctrl Pts',(-9.036633988908,-13.833584389583,117.819961399887)) ;
#157050 = CARTESIAN_POINT('Ctrl Pts',(-9.05846369099851,-13.8042063937381,
117.88645115234)) ;
#157051 = CARTESIAN_POINT('Ctrl Pts',(-9.13226752150254,-13.8042062935713,
117.862220071314)) ;
#157052 = CARTESIAN_POINT('Ctrl Pts',(-9.20607135200658,-13.8042061934045,
117.837988990289)) ;
#157053 = CARTESIAN_POINT('Ctrl Pts',(-9.18424164991607,-13.8335841892493,
117.771499237836)) ;
#157054 = CARTESIAN_POINT('Ctrl Pts',(-9.16241194782554,-13.8629621850941,
117.705009485383)) ;
#157055 = CARTESIAN_POINT('Ctrl Pts',(-9.08860811732153,-13.862962285261,
117.729240566409)) ;
#157056 = CARTESIAN_POINT('Ctrl Pts',(-9.01480428681749,-13.8629623854278,
117.753471647434)) ;
#157057 = CARTESIAN_POINT('Ctrl Pts',(-9.036633988908,-13.833584389583,117.819961399887)) ;
#157058 = CARTESIAN_POINT('Ctrl Pts',(-9.02391466502751,-13.5522887119168,
117.745782719323)) ;
#157059 = CARTESIAN_POINT('Ctrl Pts',(-9.04739797225372,-13.5425061564868,
117.817309086205)) ;
#157060 = CARTESIAN_POINT('Ctrl Pts',(-9.1212018115543,-13.542506049205,117.793078031972)) ;
#157061 = CARTESIAN_POINT('Ctrl Pts',(-9.19500565085488,-13.5425059419231,
117.768846977739)) ;
#157062 = CARTESIAN_POINT('Ctrl Pts',(-9.17152234362867,-13.5522884973531,
117.697320610857)) ;
#157063 = CARTESIAN_POINT('Ctrl Pts',(-9.14803903640246,-13.5620710527831,
117.625794243975)) ;
#157064 = CARTESIAN_POINT('Ctrl Pts',(-9.07423519710187,-13.5620711600649,
117.650025298208)) ;
#157065 = CARTESIAN_POINT('Ctrl Pts',(-9.0004313578013,-13.5620712673468,
117.67425635244)) ;
#157066 = CARTESIAN_POINT('Ctrl Pts',(-9.02391466502751,-13.5522887119168,
117.745782719323)) ;
#157067 = CARTESIAN_POINT('Ctrl Pts',(-9.03557274648368,-13.2592972529684,
117.745601612871)) ;
#157068 = CARTESIAN_POINT('Ctrl Pts',(-9.05901578034276,-13.2699555383047,
117.817005313531)) ;
#157069 = CARTESIAN_POINT('Ctrl Pts',(-9.13281962864124,-13.2699554336479,
117.792774286704)) ;
#157070 = CARTESIAN_POINT('Ctrl Pts',(-9.20662347693971,-13.2699553289911,
117.768543259878)) ;
#157071 = CARTESIAN_POINT('Ctrl Pts',(-9.18318044308064,-13.2592970436547,
117.697139559218)) ;
#157072 = CARTESIAN_POINT('Ctrl Pts',(-9.15973740922156,-13.2486387583184,
117.625735858557)) ;
#157073 = CARTESIAN_POINT('Ctrl Pts',(-9.08593356092309,-13.2486388629752,
117.649966885384)) ;
#157074 = CARTESIAN_POINT('Ctrl Pts',(-9.0121297126246,-13.248638967632,117.67419791221)) ;
#157075 = CARTESIAN_POINT('Ctrl Pts',(-9.03557274648368,-13.2592972529684,
117.745601612871)) ;
#157076 = CARTESIAN_POINT('Ctrl Pts',(-9.07098090557538,-12.9811038250668,
117.818197097558)) ;
#157077 = CARTESIAN_POINT('Ctrl Pts',(-9.09271605071885,-13.0112007681919,
117.884398844714)) ;
#157078 = CARTESIAN_POINT('Ctrl Pts',(-9.166519907195,-13.0112006734562,117.860167842795)) ;
#157079 = CARTESIAN_POINT('Ctrl Pts',(-9.24032376367114,-13.0112005787204,
117.835936840877)) ;
#157080 = CARTESIAN_POINT('Ctrl Pts',(-9.21858861852767,-12.9811036355953,
117.76973509372)) ;
#157081 = CARTESIAN_POINT('Ctrl Pts',(-9.19685347338419,-12.9510066924703,
117.703533346564)) ;
#157082 = CARTESIAN_POINT('Ctrl Pts',(-9.12304961690805,-12.951006787206,
117.727764348482)) ;
#157083 = CARTESIAN_POINT('Ctrl Pts',(-9.0492457604319,-12.9510068819417,
117.751995350401)) ;
#157084 = CARTESIAN_POINT('Ctrl Pts',(-9.07098090557538,-12.9811038250668,
117.818197097558)) ;
#157085 = CARTESIAN_POINT('Ctrl Pts',(-9.1288816653457,-12.7319954339599,
117.959013661815)) ;
#157086 = CARTESIAN_POINT('Ctrl Pts',(-9.14734233324813,-12.7795294847017,
118.015241879551)) ;
#157087 = CARTESIAN_POINT('Ctrl Pts',(-9.22114619632656,-12.7795294077386,
117.991010897742)) ;
#157088 = CARTESIAN_POINT('Ctrl Pts',(-9.29495005940499,-12.7795293307755,
117.966779915932)) ;
#157089 = CARTESIAN_POINT('Ctrl Pts',(-9.27648939150257,-12.7319952800337,
117.910551698197)) ;
#157090 = CARTESIAN_POINT('Ctrl Pts',(-9.25802872360013,-12.6844612292919,
117.854323480461)) ;
#157091 = CARTESIAN_POINT('Ctrl Pts',(-9.1842248605217,-12.684461306255,117.87855446227)) ;
#157092 = CARTESIAN_POINT('Ctrl Pts',(-9.11042099744327,-12.6844613832181,
117.902785444079)) ;
#157093 = CARTESIAN_POINT('Ctrl Pts',(-9.1288816653457,-12.7319954339599,
117.959013661815)) ;
#157094 = CARTESIAN_POINT('Ctrl Pts',(-9.20542108821079,-12.5329045763516,
118.156747660811)) ;
#157095 = CARTESIAN_POINT('Ctrl Pts',(-9.21929794557474,-12.5944099452727,
118.199014331155)) ;
#157096 = CARTESIAN_POINT('Ctrl Pts',(-9.2931018131911,-12.5944098904592,
118.174783363168)) ;
#157097 = CARTESIAN_POINT('Ctrl Pts',(-9.36690568080745,-12.5944098356456,
118.15055239518)) ;
#157098 = CARTESIAN_POINT('Ctrl Pts',(-9.3530288234435,-12.5329044667245,
118.108285724836)) ;
#157099 = CARTESIAN_POINT('Ctrl Pts',(-9.33915196607953,-12.4713990978033,
118.066019054492)) ;
#157100 = CARTESIAN_POINT('Ctrl Pts',(-9.26534809846318,-12.4713991526168,
118.090250022479)) ;
#157101 = CARTESIAN_POINT('Ctrl Pts',(-9.19154423084681,-12.4713992074304,
118.114480990467)) ;
#157102 = CARTESIAN_POINT('Ctrl Pts',(-9.20542108821079,-12.5329045763516,
118.156747660811)) ;
#157103 = CARTESIAN_POINT('Ctrl Pts',(-9.2965722776736,-12.3964115152595,
118.398783809131)) ;
#157104 = CARTESIAN_POINT('Ctrl Pts',(-9.30484266398313,-12.467539433598,
118.423974073115)) ;
#157105 = CARTESIAN_POINT('Ctrl Pts',(-9.37864653333808,-12.4675394037743,
118.399743110423)) ;
#157106 = CARTESIAN_POINT('Ctrl Pts',(-9.45245040269302,-12.4675393739507,
118.375512147731)) ;
#157107 = CARTESIAN_POINT('Ctrl Pts',(-9.44418001638348,-12.3964114556122,
118.350321883747)) ;
#157108 = CARTESIAN_POINT('Ctrl Pts',(-9.43590963007394,-12.3252835372738,
118.325131619762)) ;
#157109 = CARTESIAN_POINT('Ctrl Pts',(-9.36210576071901,-12.3252835670974,
118.349362582454)) ;
#157110 = CARTESIAN_POINT('Ctrl Pts',(-9.28830189136406,-12.3252835969211,
118.373593545146)) ;
#157111 = CARTESIAN_POINT('Ctrl Pts',(-9.2965722776736,-12.3964115152595,
118.398783809131)) ;
#157112 = CARTESIAN_POINT('Ctrl Pts',(-9.39560158322444,-12.3338312624075,
118.665015098447)) ;
#157113 = CARTESIAN_POINT('Ctrl Pts',(-9.39770272998261,-12.4094356003857,
118.671414854041)) ;
#157114 = CARTESIAN_POINT('Ctrl Pts',(-9.47150659893981,-12.409435594184,
118.647183890138)) ;
#157115 = CARTESIAN_POINT('Ctrl Pts',(-9.54531046789698,-12.4094355879822,
118.622952926234)) ;
#157116 = CARTESIAN_POINT('Ctrl Pts',(-9.54320932113881,-12.333831250004,
118.61655317064)) ;
#157117 = CARTESIAN_POINT('Ctrl Pts',(-9.54110817438061,-12.2582269120257,
118.610153415045)) ;
#157118 = CARTESIAN_POINT('Ctrl Pts',(-9.46730430542344,-12.2582269182275,
118.634384378949)) ;
#157119 = CARTESIAN_POINT('Ctrl Pts',(-9.39350043646624,-12.2582269244292,
118.658615342853)) ;
#157120 = CARTESIAN_POINT('Ctrl Pts',(-9.39560158322444,-12.3338312624075,
118.665015098447)) ;
#157121 = CARTESIAN_POINT('Ctrl Pts',(-9.4968318946719,-12.3486707517994,
118.937874104534)) ;
#157122 = CARTESIAN_POINT('Ctrl Pts',(-9.49260239676129,-12.4233532981751,
118.92499173777)) ;
#157123 = CARTESIAN_POINT('Ctrl Pts',(-9.56640626305169,-12.4233533125853,
118.900760765744)) ;
#157124 = CARTESIAN_POINT('Ctrl Pts',(-9.64021012934211,-12.4233533269956,
118.876529793718)) ;
#157125 = CARTESIAN_POINT('Ctrl Pts',(-9.64443962725272,-12.3486707806198,
118.889412160482)) ;
#157126 = CARTESIAN_POINT('Ctrl Pts',(-9.64866912516332,-12.2739882342441,
118.902294527246)) ;
#157127 = CARTESIAN_POINT('Ctrl Pts',(-9.5748652588729,-12.2739882198339,
118.926525499272)) ;
#157128 = CARTESIAN_POINT('Ctrl Pts',(-9.5010613925825,-12.2739882054237,
118.950756471299)) ;
#157129 = CARTESIAN_POINT('Ctrl Pts',(-9.4968318946719,-12.3486707517994,
118.937874104534)) ;
#157130 = CARTESIAN_POINT('Ctrl Pts',(-9.59343723857601,-12.4397941697449,
119.196716726627)) ;
#157131 = CARTESIAN_POINT('Ctrl Pts',(-9.58318893999786,-12.5082273902753,
119.165502064017)) ;
#157132 = CARTESIAN_POINT('Ctrl Pts',(-9.65699280218564,-12.5082274205257,
119.141271079495)) ;
#157133 = CARTESIAN_POINT('Ctrl Pts',(-9.73079666437343,-12.508227450776,
119.117040094973)) ;
#157134 = CARTESIAN_POINT('Ctrl Pts',(-9.74104496295157,-12.4397942302456,
119.148254757583)) ;
#157135 = CARTESIAN_POINT('Ctrl Pts',(-9.75129326152971,-12.3713610097152,
119.179469420192)) ;
#157136 = CARTESIAN_POINT('Ctrl Pts',(-9.67748939934194,-12.3713609794648,
119.203700404715)) ;
#157137 = CARTESIAN_POINT('Ctrl Pts',(-9.60368553715415,-12.3713609492144,
119.227931389237)) ;
#157138 = CARTESIAN_POINT('Ctrl Pts',(-9.59343723857601,-12.4397941697449,
119.196716726627)) ;
#157139 = CARTESIAN_POINT('Ctrl Pts',(-9.67989153670841,-12.6021170084136,
119.424415022172)) ;
#157140 = CARTESIAN_POINT('Ctrl Pts',(-9.66432856763324,-12.6593209317561,
119.377012730555)) ;
#157141 = CARTESIAN_POINT('Ctrl Pts',(-9.73813242432927,-12.6593209703252,
119.352781729306)) ;
#157142 = CARTESIAN_POINT('Ctrl Pts',(-9.81193628102528,-12.6593210088944,
119.328550728057)) ;
#157143 = CARTESIAN_POINT('Ctrl Pts',(-9.82749925010046,-12.6021170855519,
119.375953019674)) ;
#157144 = CARTESIAN_POINT('Ctrl Pts',(-9.84306221917561,-12.5449131622094,
119.423355311291)) ;
#157145 = CARTESIAN_POINT('Ctrl Pts',(-9.7692583624796,-12.5449131236403,
119.44758631254)) ;
#157146 = CARTESIAN_POINT('Ctrl Pts',(-9.69545450578357,-12.5449130850712,
119.47181731379)) ;
#157147 = CARTESIAN_POINT('Ctrl Pts',(-9.67989153670841,-12.6021170084136,
119.424415022172)) ;
#157148 = CARTESIAN_POINT('Ctrl Pts',(-9.74951237514481,-12.8208593941247,
119.601209318802)) ;
#157149 = CARTESIAN_POINT('Ctrl Pts',(-9.7297945436342,-12.862876765698,119.541151986463)) ;
#157150 = CARTESIAN_POINT('Ctrl Pts',(-9.80359839554776,-12.8628768085356,
119.516920970647)) ;
#157151 = CARTESIAN_POINT('Ctrl Pts',(-9.87740224746131,-12.8628768513732,
119.492689954831)) ;
#157152 = CARTESIAN_POINT('Ctrl Pts',(-9.89712007897192,-12.8208594798,119.552747287171)) ;
#157153 = CARTESIAN_POINT('Ctrl Pts',(-9.91683791048251,-12.7788421082267,
119.61280461951)) ;
#157154 = CARTESIAN_POINT('Ctrl Pts',(-9.84303405856896,-12.7788420653891,
119.637035635326)) ;
#157155 = CARTESIAN_POINT('Ctrl Pts',(-9.76923020665541,-12.7788420225515,
119.661266651141)) ;
#157156 = CARTESIAN_POINT('Ctrl Pts',(-9.74951237514481,-12.8208593941247,
119.601209318802)) ;
#157157 = CARTESIAN_POINT('Ctrl Pts',(-9.79944954754396,-13.084370773037,
119.717716848365)) ;
#157158 = CARTESIAN_POINT('Ctrl Pts',(-9.77695151881111,-13.1080532494665,
119.649191483677)) ;
#157159 = CARTESIAN_POINT('Ctrl Pts',(-9.85075536585704,-13.1080532886094,
119.624960453035)) ;
#157160 = CARTESIAN_POINT('Ctrl Pts',(-9.92455921290298,-13.1080533277524,
119.600729422393)) ;
#157161 = CARTESIAN_POINT('Ctrl Pts',(-9.94705724163583,-13.0843708513228,
119.669254787081)) ;
#157162 = CARTESIAN_POINT('Ctrl Pts',(-9.96955527036869,-13.0606883748933,
119.737780151769)) ;
#157163 = CARTESIAN_POINT('Ctrl Pts',(-9.89575142332274,-13.0606883357504,
119.762011182411)) ;
#157164 = CARTESIAN_POINT('Ctrl Pts',(-9.82194757627682,-13.0606882966075,
119.786242213053)) ;
#157165 = CARTESIAN_POINT('Ctrl Pts',(-9.79944954754396,-13.084370773037,
119.717716848365)) ;
#157166 = CARTESIAN_POINT('Ctrl Pts',(-9.82597149657916,-13.3711928765175,
119.763016540292)) ;
#157167 = CARTESIAN_POINT('Ctrl Pts',(-9.80232171969241,-13.3748845002412,
119.690983136391)) ;
#157168 = CARTESIAN_POINT('Ctrl Pts',(-9.87612556329562,-13.3748845322642,
119.666752095263)) ;
#157169 = CARTESIAN_POINT('Ctrl Pts',(-9.94992940689882,-13.3748845642871,
119.642521054136)) ;
#157170 = CARTESIAN_POINT('Ctrl Pts',(-9.97357918378556,-13.3711929405634,
119.714554458036)) ;
#157171 = CARTESIAN_POINT('Ctrl Pts',(-9.99722896067229,-13.3675013168397,
119.786587861936)) ;
#157172 = CARTESIAN_POINT('Ctrl Pts',(-9.92342511706909,-13.3675012848167,
119.810818903064)) ;
#157173 = CARTESIAN_POINT('Ctrl Pts',(-9.84962127346588,-13.3675012527938,
119.835049944192)) ;
#157174 = CARTESIAN_POINT('Ctrl Pts',(-9.82597149657916,-13.3711928765175,
119.763016540292)) ;
#157175 = CARTESIAN_POINT('Ctrl Pts',(-9.82819214417096,-13.6609866789311,
119.734331572361)) ;
#157176 = CARTESIAN_POINT('Ctrl Pts',(-9.80508506706182,-13.644449399206,
119.663951144264)) ;
#157177 = CARTESIAN_POINT('Ctrl Pts',(-9.87888890860554,-13.6444494224757,
119.639720096863)) ;
#157178 = CARTESIAN_POINT('Ctrl Pts',(-9.95269275014925,-13.6444494457453,
119.615489049462)) ;
#157179 = CARTESIAN_POINT('Ctrl Pts',(-9.97579982725838,-13.6609867254704,
119.68586947756)) ;
#157180 = CARTESIAN_POINT('Ctrl Pts',(-9.99890690436752,-13.6775240051955,
119.756249905657)) ;
#157181 = CARTESIAN_POINT('Ctrl Pts',(-9.9251030628238,-13.6775239819258,
119.780480953058)) ;
#157182 = CARTESIAN_POINT('Ctrl Pts',(-9.85129922128009,-13.6775239586562,
119.804712000459)) ;
#157183 = CARTESIAN_POINT('Ctrl Pts',(-9.82819214417096,-13.6609866789311,
119.734331572361)) ;
#157184 = CARTESIAN_POINT('Ctrl Pts',(-9.8068991329201,-13.9327616913683,
119.63413267067)) ;
#157185 = CARTESIAN_POINT('Ctrl Pts',(-9.785975348665,-13.8972231314794,119.570402200203)) ;
#157186 = CARTESIAN_POINT('Ctrl Pts',(-9.85977918932944,-13.8972231463685,
119.546171150125)) ;
#157187 = CARTESIAN_POINT('Ctrl Pts',(-9.9335830299939,-13.8972231612576,
119.521940100046)) ;
#157188 = CARTESIAN_POINT('Ctrl Pts',(-9.954506814249,-13.9327617211465,119.585670570512)) ;
#157189 = CARTESIAN_POINT('Ctrl Pts',(-9.9754305985041,-13.9683002810353,
119.649401040979)) ;
#157190 = CARTESIAN_POINT('Ctrl Pts',(-9.90162675783965,-13.9683002661462,
119.673632091058)) ;
#157191 = CARTESIAN_POINT('Ctrl Pts',(-9.8278229171752,-13.9683002512571,
119.697863141137)) ;
#157192 = CARTESIAN_POINT('Ctrl Pts',(-9.8068991329201,-13.9327616913683,
119.63413267067)) ;
#157193 = CARTESIAN_POINT('Ctrl Pts',(-9.76382464831486,-14.1696775509721,
119.467276311035)) ;
#157194 = CARTESIAN_POINT('Ctrl Pts',(-9.74661479432104,-14.117542024341,
119.414857872744)) ;
#157195 = CARTESIAN_POINT('Ctrl Pts',(-9.82041863565303,-14.1175420304562,
119.390626824698)) ;
#157196 = CARTESIAN_POINT('Ctrl Pts',(-9.89422247698502,-14.1175420365713,
119.366395776653)) ;
#157197 = CARTESIAN_POINT('Ctrl Pts',(-9.91143233097885,-14.1696775632024,
119.418814214944)) ;
#157198 = CARTESIAN_POINT('Ctrl Pts',(-9.92864218497269,-14.2218130898334,
119.471232653236)) ;
#157199 = CARTESIAN_POINT('Ctrl Pts',(-9.85483834364069,-14.2218130837183,
119.495463701281)) ;
#157200 = CARTESIAN_POINT('Ctrl Pts',(-9.7810345023087,-14.2218130776032,
119.519694749327)) ;
#157201 = CARTESIAN_POINT('Ctrl Pts',(-9.76382464831486,-14.1696775509721,
119.467276311035)) ;
#157202 = CARTESIAN_POINT('Ctrl Pts',(-9.7036673139555,-14.3505522399701,
119.248758719857)) ;
#157203 = CARTESIAN_POINT('Ctrl Pts',(-9.69136245748043,-14.2857090044566,
119.211280112503)) ;
#157204 = CARTESIAN_POINT('Ctrl Pts',(-9.76516629961979,-14.2857090064648,
119.187049066917)) ;
#157205 = CARTESIAN_POINT('Ctrl Pts',(-9.83897014175914,-14.285709008473,
119.16281802133)) ;
#157206 = CARTESIAN_POINT('Ctrl Pts',(-9.8512749982342,-14.3505522439865,
119.200296628684)) ;
#157207 = CARTESIAN_POINT('Ctrl Pts',(-9.86357985470927,-14.4153954795,119.237775236038)) ;
#157208 = CARTESIAN_POINT('Ctrl Pts',(-9.78977601256991,-14.4153954774918,
119.262006281625)) ;
#157209 = CARTESIAN_POINT('Ctrl Pts',(-9.71597217043056,-14.4153954754836,
119.286237327211)) ;
#157210 = CARTESIAN_POINT('Ctrl Pts',(-9.7036673139555,-14.3505522399701,
119.248758719857)) ;
#157211 = CARTESIAN_POINT('Ctrl Pts',(-9.63071094051081,-14.4659895814683,
118.991045032151)) ;
#157212 = CARTESIAN_POINT('Ctrl Pts',(-9.62421662360605,-14.39298831287,118.97126439071)) ;
#157213 = CARTESIAN_POINT('Ctrl Pts',(-9.69802046703066,-14.392988312459,
118.947033349038)) ;
#157214 = CARTESIAN_POINT('Ctrl Pts',(-9.77182431045527,-14.3929883120481,
118.922802307366)) ;
#157215 = CARTESIAN_POINT('Ctrl Pts',(-9.77831862736004,-14.4659895806463,
118.942582948807)) ;
#157216 = CARTESIAN_POINT('Ctrl Pts',(-9.78481294426479,-14.5389908492445,
118.962363590248)) ;
#157217 = CARTESIAN_POINT('Ctrl Pts',(-9.71100910084019,-14.5389908496555,
118.98659463192)) ;
#157218 = CARTESIAN_POINT('Ctrl Pts',(-9.63720525741557,-14.5389908500665,
119.010825673591)) ;
#157219 = CARTESIAN_POINT('Ctrl Pts',(-9.63071094051081,-14.4659895814683,
118.991045032151)) ;
#157220 = CARTESIAN_POINT('Ctrl Pts',(-9.55101925277455,-14.5060552317741,
118.712756531787)) ;
#157221 = CARTESIAN_POINT('Ctrl Pts',(-9.55081597857438,-14.4301469447621,
118.712137391313)) ;
#157222 = CARTESIAN_POINT('Ctrl Pts',(-9.62461982292271,-14.4301469446393,
118.687906352455)) ;
#157223 = CARTESIAN_POINT('Ctrl Pts',(-9.69842366727105,-14.4301469445164,
118.663675313597)) ;
#157224 = CARTESIAN_POINT('Ctrl Pts',(-9.69862694147122,-14.5060552315285,
118.66429445407)) ;
#157225 = CARTESIAN_POINT('Ctrl Pts',(-9.69883021567139,-14.5819635185405,
118.664913594544)) ;
#157226 = CARTESIAN_POINT('Ctrl Pts',(-9.62502637132304,-14.5819635186633,
118.689144633402)) ;
#157227 = CARTESIAN_POINT('Ctrl Pts',(-9.55122252697472,-14.5819635187861,
118.713375672261)) ;
#157228 = CARTESIAN_POINT('Ctrl Pts',(-9.55101925277455,-14.5060552317741,
118.712756531787)) ;
#157229 = CARTESIAN_POINT('Ctrl Pts',(-9.4714813916173,-14.4677867862301,
118.435025022222)) ;
#157230 = CARTESIAN_POINT('Ctrl Pts',(-9.47756606505661,-14.3944382757636,
118.453557955699)) ;
#157231 = CARTESIAN_POINT('Ctrl Pts',(-9.55136990941469,-14.3944382766233,
118.42932691687)) ;
#157232 = CARTESIAN_POINT('Ctrl Pts',(-9.62517375377276,-14.3944382774829,
118.405095878042)) ;
#157233 = CARTESIAN_POINT('Ctrl Pts',(-9.61908908033345,-14.4677867879495,
118.386562944565)) ;
#157234 = CARTESIAN_POINT('Ctrl Pts',(-9.61300440689413,-14.541135298416,
118.368030011088)) ;
#157235 = CARTESIAN_POINT('Ctrl Pts',(-9.53920056253606,-14.5411352975563,
118.392261049916)) ;
#157236 = CARTESIAN_POINT('Ctrl Pts',(-9.46539671817799,-14.5411352966967,
118.416492088745)) ;
#157237 = CARTESIAN_POINT('Ctrl Pts',(-9.4714813916173,-14.4677867862301,
118.435025022222)) ;
#157238 = CARTESIAN_POINT('Ctrl Pts',(-9.39862983053746,-14.3553856703914,
118.177844077314)) ;
#157239 = CARTESIAN_POINT('Ctrl Pts',(-9.41054063802838,-14.2897781146532,
118.214122475092)) ;
#157240 = CARTESIAN_POINT('Ctrl Pts',(-9.4843444819206,-14.2897781158864,
118.189891434844)) ;
#157241 = CARTESIAN_POINT('Ctrl Pts',(-9.55814832581283,-14.2897781171196,
118.165660394597)) ;
#157242 = CARTESIAN_POINT('Ctrl Pts',(-9.54623751832192,-14.3553856728579,
118.129381996819)) ;
#157243 = CARTESIAN_POINT('Ctrl Pts',(-9.534326710831,-14.4209932285961,118.093103599041)) ;
#157244 = CARTESIAN_POINT('Ctrl Pts',(-9.46052286693878,-14.4209932273629,
118.117334639289)) ;
#157245 = CARTESIAN_POINT('Ctrl Pts',(-9.38671902304655,-14.4209932261297,
118.141565679537)) ;
#157246 = CARTESIAN_POINT('Ctrl Pts',(-9.39862983053746,-14.3553856703914,
118.177844077314)) ;
#157247 = CARTESIAN_POINT('Ctrl Pts',(-9.33739442485482,-14.1738642018268,
117.955618487218)) ;
#157248 = CARTESIAN_POINT('Ctrl Pts',(-9.3543378978728,-14.1208352191847,
118.007225572262)) ;
#157249 = CARTESIAN_POINT('Ctrl Pts',(-9.42814174061825,-14.1208352175881,
117.982994528522)) ;
#157250 = CARTESIAN_POINT('Ctrl Pts',(-9.50194558336371,-14.1208352159916,
117.958763484782)) ;
#157251 = CARTESIAN_POINT('Ctrl Pts',(-9.48500211034573,-14.1738641986337,
117.907156399737)) ;
#157252 = CARTESIAN_POINT('Ctrl Pts',(-9.46805863732774,-14.2268931812759,
117.855549314692)) ;
#157253 = CARTESIAN_POINT('Ctrl Pts',(-9.39425479458228,-14.2268931828724,
117.879780358433)) ;
#157254 = CARTESIAN_POINT('Ctrl Pts',(-9.32045095183683,-14.226893184469,
117.904011402173)) ;
#157255 = CARTESIAN_POINT('Ctrl Pts',(-9.33739442485482,-14.1738642018268,
117.955618487218)) ;
#157256 = CARTESIAN_POINT('Ctrl Pts',(-9.29429158603599,-13.9401973275635,
117.789022041494)) ;
#157257 = CARTESIAN_POINT('Ctrl Pts',(-9.31500003079175,-13.9034069013251,
117.852096623063)) ;
#157258 = CARTESIAN_POINT('Ctrl Pts',(-9.38880387300515,-13.9034068952956,
117.827865577702)) ;
#157259 = CARTESIAN_POINT('Ctrl Pts',(-9.46260771521854,-13.903406889266,
117.803634532341)) ;
#157260 = CARTESIAN_POINT('Ctrl Pts',(-9.44189927046278,-13.9401973155044,
117.740559950772)) ;
#157261 = CARTESIAN_POINT('Ctrl Pts',(-9.42119082570701,-13.9769877417428,
117.677485369204)) ;
#157262 = CARTESIAN_POINT('Ctrl Pts',(-9.34738698349362,-13.9769877477723,
117.701716414565)) ;
#157263 = CARTESIAN_POINT('Ctrl Pts',(-9.27358314128022,-13.9769877538019,
117.725947459926)) ;
#157264 = CARTESIAN_POINT('Ctrl Pts',(-9.29429158603599,-13.9401973275635,
117.789022041494)) ;
#157265 = CARTESIAN_POINT('Ctrl Pts',(-9.27225194137694,-13.6684975496401,
117.686437026218)) ;
#157266 = CARTESIAN_POINT('Ctrl Pts',(-9.29526311301215,-13.650624726406,
117.756525342438)) ;
#157267 = CARTESIAN_POINT('Ctrl Pts',(-9.36906695530124,-13.6506247135771,
117.732294297308)) ;
#157268 = CARTESIAN_POINT('Ctrl Pts',(-9.44287079759031,-13.6506247007482,
117.708063252177)) ;
#157269 = CARTESIAN_POINT('Ctrl Pts',(-9.4198596259551,-13.6684975239824,
117.637974935957)) ;
#157270 = CARTESIAN_POINT('Ctrl Pts',(-9.39684845431988,-13.6863703472165,
117.567886619738)) ;
#157271 = CARTESIAN_POINT('Ctrl Pts',(-9.3230446120308,-13.6863703600454,
117.592117664868)) ;
#157272 = CARTESIAN_POINT('Ctrl Pts',(-9.24924076974172,-13.6863703728742,
117.616348709998)) ;
#157273 = CARTESIAN_POINT('Ctrl Pts',(-9.27225194137694,-13.6684975496401,
117.686437026218)) ;
#157274 = CARTESIAN_POINT('Ctrl Pts',(-9.27379869131216,-13.3792258998284,
117.65575130022)) ;
#157275 = CARTESIAN_POINT('Ctrl Pts',(-9.29746767065879,-13.3815248172849,
117.727843192722)) ;
#157276 = CARTESIAN_POINT('Ctrl Pts',(-9.37127151404433,-13.3815247972218,
117.703612150931)) ;
#157277 = CARTESIAN_POINT('Ctrl Pts',(-9.44507535742988,-13.3815247771587,
117.67938110914)) ;
#157278 = CARTESIAN_POINT('Ctrl Pts',(-9.42140637808324,-13.3792258597022,
117.607289216639)) ;
#157279 = CARTESIAN_POINT('Ctrl Pts',(-9.39773739873661,-13.3769269422458,
117.535197324138)) ;
#157280 = CARTESIAN_POINT('Ctrl Pts',(-9.32393355535107,-13.3769269623089,
117.559428365928)) ;
#157281 = CARTESIAN_POINT('Ctrl Pts',(-9.25012971196552,-13.3769269823719,
117.583659407719)) ;
#157282 = CARTESIAN_POINT('Ctrl Pts',(-9.27379869131216,-13.3792258998284,
117.65575130022)) ;
#157283 = CARTESIAN_POINT('Ctrl Pts',(-9.29992444127897,-13.0905267308239,
117.699639537515)) ;
#157284 = CARTESIAN_POINT('Ctrl Pts',(-9.32254221362511,-13.1129867022683,
117.768529623299)) ;
#157285 = CARTESIAN_POINT('Ctrl Pts',(-9.39634605964063,-13.1129866733618,
117.744298589519)) ;
#157286 = CARTESIAN_POINT('Ctrl Pts',(-9.47014990565614,-13.1129866444553,
117.720067555738)) ;
#157287 = CARTESIAN_POINT('Ctrl Pts',(-9.44753213330999,-13.0905266730108,
117.651177469954)) ;
#157288 = CARTESIAN_POINT('Ctrl Pts',(-9.42491436096384,-13.0680667015663,
117.58228738417)) ;
#157289 = CARTESIAN_POINT('Ctrl Pts',(-9.35111051494833,-13.0680667304729,
117.60651841795)) ;
#157290 = CARTESIAN_POINT('Ctrl Pts',(-9.27730666893281,-13.0680667593794,
117.630749451731)) ;
#157291 = CARTESIAN_POINT('Ctrl Pts',(-9.29992444127897,-13.0905267308239,
117.699639537515)) ;
#157292 = CARTESIAN_POINT('Ctrl Pts',(-9.34881358143102,-12.8284630006125,
117.813282587224)) ;
#157293 = CARTESIAN_POINT('Ctrl Pts',(-9.36878015715335,-12.8692525646979,
117.874097555988)) ;
#157294 = CARTESIAN_POINT('Ctrl Pts',(-9.44258400659655,-12.869252533481,
117.849866532648)) ;
#157295 = CARTESIAN_POINT('Ctrl Pts',(-9.51638785603974,-12.869252502264,
117.825635509308)) ;
#157296 = CARTESIAN_POINT('Ctrl Pts',(-9.49642128031742,-12.8284629381786,
117.764820540543)) ;
#157297 = CARTESIAN_POINT('Ctrl Pts',(-9.47645470459509,-12.7876733740933,
117.704005571779)) ;
#157298 = CARTESIAN_POINT('Ctrl Pts',(-9.40265085515189,-12.7876734053102,
117.728236595119)) ;
#157299 = CARTESIAN_POINT('Ctrl Pts',(-9.3288470057087,-12.7876734365271,
117.752467618459)) ;
#157300 = CARTESIAN_POINT('Ctrl Pts',(-9.34881358143102,-12.8284630006125,
117.813282587224)) ;
#157301 = CARTESIAN_POINT('Ctrl Pts',(-9.41846234787993,-12.6065365051644,
117.989873611575)) ;
#157302 = CARTESIAN_POINT('Ctrl Pts',(-9.43433055933074,-12.6628800161341,
118.03820562422)) ;
#157303 = CARTESIAN_POINT('Ctrl Pts',(-9.50813441331065,-12.6628799847594,
118.013974614698)) ;
#157304 = CARTESIAN_POINT('Ctrl Pts',(-9.58193826729053,-12.6628799533848,
117.989743605176)) ;
#157305 = CARTESIAN_POINT('Ctrl Pts',(-9.56607005583973,-12.6065364424151,
117.941411592531)) ;
#157306 = CARTESIAN_POINT('Ctrl Pts',(-9.55020184438891,-12.5501929314454,
117.893079579885)) ;
#157307 = CARTESIAN_POINT('Ctrl Pts',(-9.47639799040901,-12.5501929628201,
117.917310589407)) ;
#157308 = CARTESIAN_POINT('Ctrl Pts',(-9.40259413642911,-12.5501929941947,
117.941541598929)) ;
#157309 = CARTESIAN_POINT('Ctrl Pts',(-9.41846234787993,-12.6065365051644,
117.989873611575)) ;
#157310 = CARTESIAN_POINT('Ctrl Pts',(-9.50417588053103,-12.4434900571409,
118.215497616744)) ;
#157311 = CARTESIAN_POINT('Ctrl Pts',(-9.51481602660928,-12.5112986804866,
118.247905785975)) ;
#157312 = CARTESIAN_POINT('Ctrl Pts',(-9.58861988520866,-12.5112986555149,
118.223674790523)) ;
#157313 = CARTESIAN_POINT('Ctrl Pts',(-9.66242374380803,-12.5112986305432,
118.199443795071)) ;
#157314 = CARTESIAN_POINT('Ctrl Pts',(-9.65178359772977,-12.4434900071976,
118.16703562584)) ;
#157315 = CARTESIAN_POINT('Ctrl Pts',(-9.64114345165152,-12.3756813838519,
118.13462745661)) ;
#157316 = CARTESIAN_POINT('Ctrl Pts',(-9.56733959305215,-12.3756814088236,
118.158858452062)) ;
#157317 = CARTESIAN_POINT('Ctrl Pts',(-9.49353573445278,-12.3756814337953,
118.183089447514)) ;
#157318 = CARTESIAN_POINT('Ctrl Pts',(-9.50417588053103,-12.4434900571409,
118.215497616744)) ;
#157319 = CARTESIAN_POINT('Ctrl Pts',(-9.60073723451511,-12.3500508502058,
118.474134121631)) ;
#157320 = CARTESIAN_POINT('Ctrl Pts',(-9.60538505037241,-12.4244812912888,
118.488290620034)) ;
#157321 = CARTESIAN_POINT('Ctrl Pts',(-9.67918891312454,-12.424481278477,
118.464059637231)) ;
#157322 = CARTESIAN_POINT('Ctrl Pts',(-9.75299277587668,-12.4244812656651,
118.439828654428)) ;
#157323 = CARTESIAN_POINT('Ctrl Pts',(-9.74834496001938,-12.3500508245822,
118.425672156025)) ;
#157324 = CARTESIAN_POINT('Ctrl Pts',(-9.74369714416208,-12.2756203834992,
118.411515657622)) ;
#157325 = CARTESIAN_POINT('Ctrl Pts',(-9.66989328140994,-12.275620396311,
118.435746640425)) ;
#157326 = CARTESIAN_POINT('Ctrl Pts',(-9.5960894186578,-12.2756204091229,
118.459977623229)) ;
#157327 = CARTESIAN_POINT('Ctrl Pts',(-9.60073723451511,-12.3500508502058,
118.474134121631)) ;
#157328 = CARTESIAN_POINT('Ctrl Pts',(-9.70194573753584,-12.3331953888952,
118.746927131276)) ;
#157329 = CARTESIAN_POINT('Ctrl Pts',(-9.70026811438521,-12.4089103805945,
118.741817363225)) ;
#157330 = CARTESIAN_POINT('Ctrl Pts',(-9.77407198005636,-12.4089103853774,
118.717586389313)) ;
#157331 = CARTESIAN_POINT('Ctrl Pts',(-9.84787584572754,-12.4089103901604,
118.693355415401)) ;
#157332 = CARTESIAN_POINT('Ctrl Pts',(-9.84955346887816,-12.3331953984611,
118.698465183452)) ;
#157333 = CARTESIAN_POINT('Ctrl Pts',(-9.8512310920288,-12.2574804067618,
118.703574951503)) ;
#157334 = CARTESIAN_POINT('Ctrl Pts',(-9.77742722635763,-12.2574804019789,
118.727805925415)) ;
#157335 = CARTESIAN_POINT('Ctrl Pts',(-9.70362336068647,-12.2574803971959,
118.752036899327)) ;
#157336 = CARTESIAN_POINT('Ctrl Pts',(-9.70194573753584,-12.3331953888952,
118.746927131276)) ;
#157337 = CARTESIAN_POINT('Ctrl Pts',(-9.80131762641198,-12.3940161187778,
119.014124252987)) ;
#157338 = CARTESIAN_POINT('Ctrl Pts',(-9.79343372369382,-12.4655945537366,
118.990111158902)) ;
#157339 = CARTESIAN_POINT('Ctrl Pts',(-9.86723759044243,-12.4655945799172,
118.965880188271)) ;
#157340 = CARTESIAN_POINT('Ctrl Pts',(-9.94104145719105,-12.4655946060978,
118.941649217641)) ;
#157341 = CARTESIAN_POINT('Ctrl Pts',(-9.94892535990921,-12.3940161711391,
118.965662311726)) ;
#157342 = CARTESIAN_POINT('Ctrl Pts',(-9.95680926262737,-12.3224377361804,
118.98967540581)) ;
#157343 = CARTESIAN_POINT('Ctrl Pts',(-9.88300539587875,-12.3224377099997,
119.013906376441)) ;
#157344 = CARTESIAN_POINT('Ctrl Pts',(-9.80920152913014,-12.3224376838191,
119.038137347071)) ;
#157345 = CARTESIAN_POINT('Ctrl Pts',(-9.80131762641198,-12.3940161187778,
119.014124252987)) ;
#157346 = CARTESIAN_POINT('Ctrl Pts',(-9.89248329484562,-12.5284976067023,
119.256301286483)) ;
#157347 = CARTESIAN_POINT('Ctrl Pts',(-9.87895755535242,-12.5907910171459,
119.215104068027)) ;
#157348 = CARTESIAN_POINT('Ctrl Pts',(-9.95276142087398,-12.590791066487,
119.190873093659)) ;
#157349 = CARTESIAN_POINT('Ctrl Pts',(-10.0265652863955,-12.5907911158281,
119.166642119291)) ;
#157350 = CARTESIAN_POINT('Ctrl Pts',(-10.0400910258887,-12.5284977053845,
119.207839337747)) ;
#157351 = CARTESIAN_POINT('Ctrl Pts',(-10.0536167653819,-12.466204294941,
119.249036556204)) ;
#157352 = CARTESIAN_POINT('Ctrl Pts',(-9.97981289986036,-12.4662042455999,
119.273267530572)) ;
#157353 = CARTESIAN_POINT('Ctrl Pts',(-9.9060090343388,-12.4662041962588,
119.29749850494)) ;
#157354 = CARTESIAN_POINT('Ctrl Pts',(-9.89248329484562,-12.5284976067023,
119.256301286483)) ;
#157355 = CARTESIAN_POINT('Ctrl Pts',(-9.9693440763676,-12.7253590046235,
119.455101779986)) ;
#157356 = CARTESIAN_POINT('Ctrl Pts',(-9.95116310647556,-12.7739984449888,
119.399725480954)) ;
#157357 = CARTESIAN_POINT('Ctrl Pts',(-10.0249669682071,-12.7739985153053,
119.375494495042)) ;
#157358 = CARTESIAN_POINT('Ctrl Pts',(-10.0987708299386,-12.7739985856217,
119.35126350913)) ;
#157359 = CARTESIAN_POINT('Ctrl Pts',(-10.1169517998307,-12.7253591452565,
119.406639808163)) ;
#157360 = CARTESIAN_POINT('Ctrl Pts',(-10.1351327697227,-12.6767197048912,
119.462016107195)) ;
#157361 = CARTESIAN_POINT('Ctrl Pts',(-10.0613289079912,-12.6767196345747,
119.486247093107)) ;
#157362 = CARTESIAN_POINT('Ctrl Pts',(-9.98752504625965,-12.6767195642582,
119.510478079019)) ;
#157363 = CARTESIAN_POINT('Ctrl Pts',(-9.9693440763676,-12.7253590046235,
119.455101779986)) ;
#157364 = CARTESIAN_POINT('Ctrl Pts',(-10.0281574646971,-12.9750336085797,
119.598466100957)) ;
#157365 = CARTESIAN_POINT('Ctrl Pts',(-10.006583801685,-13.0063134744705,
119.532756206226)) ;
#157366 = CARTESIAN_POINT('Ctrl Pts',(-10.0803876577271,-13.0063135643594,
119.508525202985)) ;
#157367 = CARTESIAN_POINT('Ctrl Pts',(-10.1541915137692,-13.0063136542484,
119.484294199744)) ;
#157368 = CARTESIAN_POINT('Ctrl Pts',(-10.1757651767812,-12.9750337883576,
119.550004094475)) ;
#157369 = CARTESIAN_POINT('Ctrl Pts',(-10.1973388397932,-12.9437539224668,
119.615713989206)) ;
#157370 = CARTESIAN_POINT('Ctrl Pts',(-10.1235349837511,-12.9437538325779,
119.639944992447)) ;
#157371 = CARTESIAN_POINT('Ctrl Pts',(-10.0497311277091,-12.943753742689,
119.664175995688)) ;
#157372 = CARTESIAN_POINT('Ctrl Pts',(-10.0281574646971,-12.9750336085797,
119.598466100957)) ;
#157373 = CARTESIAN_POINT('Ctrl Pts',(-10.0639625581,-13.2518773391213,119.672384712737)) ;
#157374 = CARTESIAN_POINT('Ctrl Pts',(-10.0405848667401,-13.2638740920304,
119.601180038788)) ;
#157375 = CARTESIAN_POINT('Ctrl Pts',(-10.1143887150386,-13.2638741920649,
119.576949011961)) ;
#157376 = CARTESIAN_POINT('Ctrl Pts',(-10.1881925633371,-13.2638742920995,
119.552717985135)) ;
#157377 = CARTESIAN_POINT('Ctrl Pts',(-10.211570254697,-13.2518775391904,
119.623922659084)) ;
#157378 = CARTESIAN_POINT('Ctrl Pts',(-10.2349479460568,-13.2398807862813,
119.695127333032)) ;
#157379 = CARTESIAN_POINT('Ctrl Pts',(-10.1611440977583,-13.2398806862467,
119.719358359859)) ;
#157380 = CARTESIAN_POINT('Ctrl Pts',(-10.0873402494598,-13.2398805862122,
119.743589386686)) ;
#157381 = CARTESIAN_POINT('Ctrl Pts',(-10.0639625581,-13.2518773391213,119.672384712737)) ;
#157382 = CARTESIAN_POINT('Ctrl Pts',(-10.0762711870781,-13.5442043587849,
119.674255680769)) ;
#157383 = CARTESIAN_POINT('Ctrl Pts',(-10.052736732687,-13.5358098803519,
119.602573531998)) ;
#157384 = CARTESIAN_POINT('Ctrl Pts',(-10.1265405723682,-13.5358099849276,
119.578342478924)) ;
#157385 = CARTESIAN_POINT('Ctrl Pts',(-10.2003444120494,-13.5358100895033,
119.554111425851)) ;
#157386 = CARTESIAN_POINT('Ctrl Pts',(-10.2238788664405,-13.5442045679364,
119.625793574622)) ;
#157387 = CARTESIAN_POINT('Ctrl Pts',(-10.2474133208317,-13.5525990463694,
119.697475723393)) ;
#157388 = CARTESIAN_POINT('Ctrl Pts',(-10.1736094811505,-13.5525989417936,
119.721706776466)) ;
#157389 = CARTESIAN_POINT('Ctrl Pts',(-10.0998056414693,-13.5525988372179,
119.745937829539)) ;
#157390 = CARTESIAN_POINT('Ctrl Pts',(-10.0762711870781,-13.5442043587849,
119.674255680769)) ;
#157391 = CARTESIAN_POINT('Ctrl Pts',(-10.0642632265541,-13.8259451748865,
119.602266518667)) ;
#157392 = CARTESIAN_POINT('Ctrl Pts',(-10.0422653073509,-13.7978682383242,
119.535264408198)) ;
#157393 = CARTESIAN_POINT('Ctrl Pts',(-10.1160691382364,-13.7978683377893,
119.511033328335)) ;
#157394 = CARTESIAN_POINT('Ctrl Pts',(-10.1898729691219,-13.7978684372543,
119.486802248471)) ;
#157395 = CARTESIAN_POINT('Ctrl Pts',(-10.2118708883251,-13.8259453738167,
119.55380435894)) ;
#157396 = CARTESIAN_POINT('Ctrl Pts',(-10.2338688075283,-13.8540223103791,
119.620806469409)) ;
#157397 = CARTESIAN_POINT('Ctrl Pts',(-10.1600649766428,-13.854022210914,
119.645037549273)) ;
#157398 = CARTESIAN_POINT('Ctrl Pts',(-10.0862611457573,-13.8540221114489,
119.669268629136)) ;
#157399 = CARTESIAN_POINT('Ctrl Pts',(-10.0642632265541,-13.8259451748865,
119.602266518667)) ;
#157400 = CARTESIAN_POINT('Ctrl Pts',(-10.0296964583947,-14.0792480619856,
119.461456237366)) ;
#157401 = CARTESIAN_POINT('Ctrl Pts',(-10.0108143826101,-14.0334450409061,
119.403944483233)) ;
#157402 = CARTESIAN_POINT('Ctrl Pts',(-10.0846182054714,-14.0334451269848,
119.379713378929)) ;
#157403 = CARTESIAN_POINT('Ctrl Pts',(-10.1584220283326,-14.0334452130635,
119.355482274624)) ;
#157404 = CARTESIAN_POINT('Ctrl Pts',(-10.1773041041172,-14.079248234143,
119.412994028758)) ;
#157405 = CARTESIAN_POINT('Ctrl Pts',(-10.1961861799017,-14.1250512552225,
119.470505782891)) ;
#157406 = CARTESIAN_POINT('Ctrl Pts',(-10.1223823570405,-14.1250511691438,
119.494736887195)) ;
#157407 = CARTESIAN_POINT('Ctrl Pts',(-10.0485785341793,-14.1250510830651,
119.518967991499)) ;
#157408 = CARTESIAN_POINT('Ctrl Pts',(-10.0296964583947,-14.0792480619856,
119.461456237366)) ;
#157409 = CARTESIAN_POINT('Ctrl Pts',(-9.97588775903519,-14.2845087011992,
119.262132122512)) ;
#157410 = CARTESIAN_POINT('Ctrl Pts',(-9.96146759893467,-14.2243072924303,
119.218210643622)) ;
#157411 = CARTESIAN_POINT('Ctrl Pts',(-10.0352714154371,-14.2243073577872,
119.19397951995)) ;
#157412 = CARTESIAN_POINT('Ctrl Pts',(-10.1090752319395,-14.2243074231441,
119.169748396277)) ;
#157413 = CARTESIAN_POINT('Ctrl Pts',(-10.12349539204,-14.284508831913,119.213669875168)) ;
#157414 = CARTESIAN_POINT('Ctrl Pts',(-10.1379155521406,-14.3447102406819,
119.257591354058)) ;
#157415 = CARTESIAN_POINT('Ctrl Pts',(-10.0641117356382,-14.344710175325,
119.28182247773)) ;
#157416 = CARTESIAN_POINT('Ctrl Pts',(-9.99030791913573,-14.3447101099681,
119.306053601403)) ;
#157417 = CARTESIAN_POINT('Ctrl Pts',(-9.97588775903519,-14.2845087011992,
119.262132122512)) ;
#157418 = CARTESIAN_POINT('Ctrl Pts',(-9.90744210014645,-14.4278905637469,
119.018229253178)) ;
#157419 = CARTESIAN_POINT('Ctrl Pts',(-9.89851224393999,-14.3575893614837,
118.991030354069)) ;
#157420 = CARTESIAN_POINT('Ctrl Pts',(-9.97231605632315,-14.3575894011323,
118.96679921785)) ;
#157421 = CARTESIAN_POINT('Ctrl Pts',(-10.0461198687063,-14.3575894407809,
118.942568081632)) ;
#157422 = CARTESIAN_POINT('Ctrl Pts',(-10.0550497249128,-14.4278906430441,
118.96976698074)) ;
#157423 = CARTESIAN_POINT('Ctrl Pts',(-10.0639795811192,-14.4981918453073,
118.996965879848)) ;
#157424 = CARTESIAN_POINT('Ctrl Pts',(-9.99017576873607,-14.4981918056587,
119.021197016067)) ;
#157425 = CARTESIAN_POINT('Ctrl Pts',(-9.91637195635291,-14.4981917660102,
119.045428152286)) ;
#157426 = CARTESIAN_POINT('Ctrl Pts',(-9.90744210014645,-14.4278905637469,
119.018229253178)) ;
#157427 = CARTESIAN_POINT('Ctrl Pts',(-9.82982242385163,-14.49909499359,118.746322529544)) ;
#157428 = CARTESIAN_POINT('Ctrl Pts',(-9.8270327331662,-14.4237176570017,
118.737825583854)) ;
#157429 = CARTESIAN_POINT('Ctrl Pts',(-9.90083654412551,-14.4237176684641,
118.713594443298)) ;
#157430 = CARTESIAN_POINT('Ctrl Pts',(-9.97464035508483,-14.4237176799264,
118.689363302743)) ;
#157431 = CARTESIAN_POINT('Ctrl Pts',(-9.97743004577026,-14.4990950165147,
118.697860248433)) ;
#157432 = CARTESIAN_POINT('Ctrl Pts',(-9.9802197364557,-14.5744723531029,
118.706357194123)) ;
#157433 = CARTESIAN_POINT('Ctrl Pts',(-9.90641592549639,-14.5744723416406,
118.730588334679)) ;
#157434 = CARTESIAN_POINT('Ctrl Pts',(-9.83261211453707,-14.5744723301783,
118.754819475234)) ;
#157435 = CARTESIAN_POINT('Ctrl Pts',(-9.82982242385163,-14.49909499359,118.746322529544)) ;
#157436 = CARTESIAN_POINT('Ctrl Pts',(-9.74956192660519,-14.492829252027,
118.466414353285)) ;
#157437 = CARTESIAN_POINT('Ctrl Pts',(-9.75310509711621,-14.4177767154629,
118.477206280931)) ;
#157438 = CARTESIAN_POINT('Ctrl Pts',(-9.82690890932998,-14.4177766993577,
118.452975144196)) ;
#157439 = CARTESIAN_POINT('Ctrl Pts',(-9.90071272154373,-14.4177766832525,
118.428744007461)) ;
#157440 = CARTESIAN_POINT('Ctrl Pts',(-9.8971695510327,-14.4928292198167,
118.417952079816)) ;
#157441 = CARTESIAN_POINT('Ctrl Pts',(-9.89362638052167,-14.5678817563809,
118.40716015217)) ;
#157442 = CARTESIAN_POINT('Ctrl Pts',(-9.81982256830792,-14.567881772486,
118.431391288905)) ;
#157443 = CARTESIAN_POINT('Ctrl Pts',(-9.74601875609416,-14.5678817885912,
118.45562242564)) ;
#157444 = CARTESIAN_POINT('Ctrl Pts',(-9.74956192660519,-14.492829252027,
118.466414353285)) ;
#157445 = CARTESIAN_POINT('Ctrl Pts',(-9.67283879350772,-14.4093444300335,
118.197174970448)) ;
#157446 = CARTESIAN_POINT('Ctrl Pts',(-9.68247953277884,-14.3400077238797,
118.226539108603)) ;
#157447 = CARTESIAN_POINT('Ctrl Pts',(-9.75628334887631,-14.3400076836513,
118.202307983697)) ;
#157448 = CARTESIAN_POINT('Ctrl Pts',(-9.8300871649738,-14.340007643423,118.178076858792)) ;
#157449 = CARTESIAN_POINT('Ctrl Pts',(-9.82044642570268,-14.4093443495768,
118.148712720637)) ;
#157450 = CARTESIAN_POINT('Ctrl Pts',(-9.81080568643156,-14.4786810557306,
118.119348582483)) ;
#157451 = CARTESIAN_POINT('Ctrl Pts',(-9.73700187033407,-14.4786810959589,
118.143579707388)) ;
#157452 = CARTESIAN_POINT('Ctrl Pts',(-9.66319805423659,-14.4786811361873,
118.167810832294)) ;
#157453 = CARTESIAN_POINT('Ctrl Pts',(-9.67283879350772,-14.4093444300335,
118.197174970448)) ;
#157454 = CARTESIAN_POINT('Ctrl Pts',(-9.60626579738372,-14.2544052422715,
117.958871810111)) ;
#157455 = CARTESIAN_POINT('Ctrl Pts',(-9.62130430767447,-14.1957815883073,
118.004676687747)) ;
#157456 = CARTESIAN_POINT('Ctrl Pts',(-9.69510812953136,-14.1957815301846,
117.980445580384)) ;
#157457 = CARTESIAN_POINT('Ctrl Pts',(-9.76891195138824,-14.1957814720619,
117.95621447302)) ;
#157458 = CARTESIAN_POINT('Ctrl Pts',(-9.75387344109749,-14.2544051260261,
117.910409595385)) ;
#157459 = CARTESIAN_POINT('Ctrl Pts',(-9.73883493080673,-14.3130287799903,
117.864604717749)) ;
#157460 = CARTESIAN_POINT('Ctrl Pts',(-9.66503110894986,-14.313028838113,
117.888835825112)) ;
#157461 = CARTESIAN_POINT('Ctrl Pts',(-9.59122728709297,-14.3130288962357,
117.913066932476)) ;
#157462 = CARTESIAN_POINT('Ctrl Pts',(-9.60626579738372,-14.2544052422715,
117.958871810111)) ;
#157463 = CARTESIAN_POINT('Ctrl Pts',(-9.55553746479956,-14.0410991720381,
117.769068814144)) ;
#157464 = CARTESIAN_POINT('Ctrl Pts',(-9.57487061302664,-13.9972803376337,
117.827954465898)) ;
#157465 = CARTESIAN_POINT('Ctrl Pts',(-9.64867444137708,-13.9972802674836,
117.803723378313)) ;
#157466 = CARTESIAN_POINT('Ctrl Pts',(-9.72247826972751,-13.9972801973335,
117.779492290728)) ;
#157467 = CARTESIAN_POINT('Ctrl Pts',(-9.70314512150042,-14.0410990317379,
117.720606638974)) ;
#157468 = CARTESIAN_POINT('Ctrl Pts',(-9.68381197327334,-14.0849178661423,
117.66172098722)) ;
#157469 = CARTESIAN_POINT('Ctrl Pts',(-9.6100081449229,-14.0849179362924,
117.685952074805)) ;
#157470 = CARTESIAN_POINT('Ctrl Pts',(-9.53620431657246,-14.0849180064424,
117.71018316239)) ;
#157471 = CARTESIAN_POINT('Ctrl Pts',(-9.55553746479956,-14.0410991720381,
117.769068814144)) ;
#157472 = CARTESIAN_POINT('Ctrl Pts',(-9.52441285793816,-13.7816895970119,
117.638727760598)) ;
#157473 = CARTESIAN_POINT('Ctrl Pts',(-9.5466837632346,-13.7559161217153,
117.706561346231)) ;
#157474 = CARTESIAN_POINT('Ctrl Pts',(-9.62048759876048,-13.7559160484501,
117.682330280501)) ;
#157475 = CARTESIAN_POINT('Ctrl Pts',(-9.69429143428636,-13.7559159751849,
117.658099214771)) ;
#157476 = CARTESIAN_POINT('Ctrl Pts',(-9.67202052898993,-13.7816894504815,
117.590265629138)) ;
#157477 = CARTESIAN_POINT('Ctrl Pts',(-9.64974962369348,-13.8074629257781,
117.522432043505)) ;
#157478 = CARTESIAN_POINT('Ctrl Pts',(-9.5759457881676,-13.8074629990433,
117.546663109235)) ;
#157479 = CARTESIAN_POINT('Ctrl Pts',(-9.50214195264172,-13.8074630723084,
117.570894174964)) ;
#157480 = CARTESIAN_POINT('Ctrl Pts',(-9.52441285793816,-13.7816895970119,
117.638727760598)) ;
#157481 = CARTESIAN_POINT('Ctrl Pts',(-9.51628185017245,-13.4976199910735,
117.578613119079)) ;
#157482 = CARTESIAN_POINT('Ctrl Pts',(-9.53988551258455,-13.4916413053213,
117.650506067717)) ;
#157483 = CARTESIAN_POINT('Ctrl Pts',(-9.61368935460016,-13.4916412347082,
117.626275021754)) ;
#157484 = CARTESIAN_POINT('Ctrl Pts',(-9.68749319661578,-13.4916411640951,
117.60204397579)) ;
#157485 = CARTESIAN_POINT('Ctrl Pts',(-9.66388953420369,-13.4976198498473,
117.530151027152)) ;
#157486 = CARTESIAN_POINT('Ctrl Pts',(-9.6402858717916,-13.5035985355994,
117.458258078514)) ;
#157487 = CARTESIAN_POINT('Ctrl Pts',(-9.56648202977599,-13.5035986062125,
117.482489124477)) ;
#157488 = CARTESIAN_POINT('Ctrl Pts',(-9.49267818776037,-13.5035986768257,
117.506720170441)) ;
#157489 = CARTESIAN_POINT('Ctrl Pts',(-9.51628185017245,-13.4976199910735,
117.578613119079)) ;
#157490 = CARTESIAN_POINT('Ctrl Pts',(-9.53237212691088,-13.2063007087737,
117.592070626438)) ;
#157491 = CARTESIAN_POINT('Ctrl Pts',(-9.55562384876197,-13.2206528794354,
117.662891620739)) ;
#157492 = CARTESIAN_POINT('Ctrl Pts',(-9.62942769617348,-13.2206528189828,
117.63866059121)) ;
#157493 = CARTESIAN_POINT('Ctrl Pts',(-9.70323154358499,-13.2206527585302,
117.614429561682)) ;
#157494 = CARTESIAN_POINT('Ctrl Pts',(-9.67997982173389,-13.2063005878686,
117.543608567381)) ;
#157495 = CARTESIAN_POINT('Ctrl Pts',(-9.6567280998828,-13.1919484172069,
117.47278757308)) ;
#157496 = CARTESIAN_POINT('Ctrl Pts',(-9.5829242524713,-13.1919484776594,
117.497018602609)) ;
#157497 = CARTESIAN_POINT('Ctrl Pts',(-9.50912040505978,-13.191948538112,
117.521249632137)) ;
#157498 = CARTESIAN_POINT('Ctrl Pts',(-9.53237212691088,-13.2063007087737,
117.592070626438)) ;
#157499 = CARTESIAN_POINT('Ctrl Pts',(-9.57232919510587,-12.9308185504047,
117.678310643569)) ;
#157500 = CARTESIAN_POINT('Ctrl Pts',(-9.5935601703269,-12.9644269321628,
117.742976769516)) ;
#157501 = CARTESIAN_POINT('Ctrl Pts',(-9.66736402139537,-12.9644268849646,
117.718745751126)) ;
#157502 = CARTESIAN_POINT('Ctrl Pts',(-9.74116787246387,-12.9644268377663,
117.694514732736)) ;
#157503 = CARTESIAN_POINT('Ctrl Pts',(-9.71993689724284,-12.9308184560083,
117.62984860679)) ;
#157504 = CARTESIAN_POINT('Ctrl Pts',(-9.69870592202183,-12.8972100742503,
117.565182480843)) ;
#157505 = CARTESIAN_POINT('Ctrl Pts',(-9.62490207095333,-12.8972101214485,
117.589413499233)) ;
#157506 = CARTESIAN_POINT('Ctrl Pts',(-9.55109821988485,-12.8972101686467,
117.613644517623)) ;
#157507 = CARTESIAN_POINT('Ctrl Pts',(-9.57232919510587,-12.9308185504047,
117.678310643569)) ;
#157508 = CARTESIAN_POINT('Ctrl Pts',(-9.634113078639,-12.690040453889,117.830986128613)) ;
#157509 = CARTESIAN_POINT('Ctrl Pts',(-9.65179721230132,-12.7405114660654,
117.884849147276)) ;
#157510 = CARTESIAN_POINT('Ctrl Pts',(-9.72560106508382,-12.7405114337976,
117.860618134107)) ;
#157511 = CARTESIAN_POINT('Ctrl Pts',(-9.79940491786632,-12.7405114015298,
117.836387120937)) ;
#157512 = CARTESIAN_POINT('Ctrl Pts',(-9.78172078420399,-12.6900403893535,
117.782524102275)) ;
#157513 = CARTESIAN_POINT('Ctrl Pts',(-9.76403665054166,-12.6395693771771,
117.728661083612)) ;
#157514 = CARTESIAN_POINT('Ctrl Pts',(-9.69023279775917,-12.6395694094449,
117.752892096781)) ;
#157515 = CARTESIAN_POINT('Ctrl Pts',(-9.61642894497667,-12.6395694417127,
117.77712310995)) ;
#157516 = CARTESIAN_POINT('Ctrl Pts',(-9.634113078639,-12.690040453889,117.830986128613)) ;
#157517 = CARTESIAN_POINT('Ctrl Pts',(-9.713580692807,-12.5021903792694,118.037691814633)) ;
#157518 = CARTESIAN_POINT('Ctrl Pts',(-9.72647426064452,-12.5658538076965,
118.076963542604)) ;
#157519 = CARTESIAN_POINT('Ctrl Pts',(-9.80027811379014,-12.5658537885695,
118.052732530541)) ;
#157520 = CARTESIAN_POINT('Ctrl Pts',(-9.87408196693574,-12.5658537694425,
118.028501518478)) ;
#157521 = CARTESIAN_POINT('Ctrl Pts',(-9.86118839909822,-12.5021903410154,
117.989229790506)) ;
#157522 = CARTESIAN_POINT('Ctrl Pts',(-9.84829483126071,-12.4385269125883,
117.949958062535)) ;
#157523 = CARTESIAN_POINT('Ctrl Pts',(-9.77449097811509,-12.4385269317153,
117.974189074598)) ;
#157524 = CARTESIAN_POINT('Ctrl Pts',(-9.70068712496948,-12.4385269508424,
117.998420086661)) ;
#157525 = CARTESIAN_POINT('Ctrl Pts',(-9.713580692807,-12.5021903792694,118.037691814633)) ;
#157526 = CARTESIAN_POINT('Ctrl Pts',(-9.80659684966496,-12.3790435207342,
118.285471103814)) ;
#157527 = CARTESIAN_POINT('Ctrl Pts',(-9.81375059597936,-12.4514021719633,
118.307260261368)) ;
#157528 = CARTESIAN_POINT('Ctrl Pts',(-9.887554447672,-12.4514021645019,118.283029244879)) ;
#157529 = CARTESIAN_POINT('Ctrl Pts',(-9.96135829936465,-12.4514021570405,
118.25879822839)) ;
#157530 = CARTESIAN_POINT('Ctrl Pts',(-9.95420455305025,-12.3790435058114,
118.237009070837)) ;
#157531 = CARTESIAN_POINT('Ctrl Pts',(-9.94705080673585,-12.3066848545823,
118.215219913283)) ;
#157532 = CARTESIAN_POINT('Ctrl Pts',(-9.87324695504321,-12.3066848620437,
118.239450929772)) ;
#157533 = CARTESIAN_POINT('Ctrl Pts',(-9.79944310335057,-12.3066848695051,
118.263681946261)) ;
#157534 = CARTESIAN_POINT('Ctrl Pts',(-9.80659684966496,-12.3790435207342,
118.285471103814)) ;
#157535 = CARTESIAN_POINT('Ctrl Pts',(-9.90658661047469,-12.3305042760163,
118.554594905817)) ;
#157536 = CARTESIAN_POINT('Ctrl Pts',(-9.90750267093768,-12.4063616289538,
118.557385078565)) ;
#157537 = CARTESIAN_POINT('Ctrl Pts',(-9.98130652053492,-12.4063616290811,
118.533154055694)) ;
#157538 = CARTESIAN_POINT('Ctrl Pts',(-10.0551103701321,-12.4063616292084,
118.508923032823)) ;
#157539 = CARTESIAN_POINT('Ctrl Pts',(-10.0541943096692,-12.3305042762709,
118.506132860075)) ;
#157540 = CARTESIAN_POINT('Ctrl Pts',(-10.0532782492062,-12.2546469233334,
118.503342687327)) ;
#157541 = CARTESIAN_POINT('Ctrl Pts',(-9.97947439960893,-12.2546469232061,
118.527573710198)) ;
#157542 = CARTESIAN_POINT('Ctrl Pts',(-9.9056705500117,-12.2546469230788,
118.551804733069)) ;
#157543 = CARTESIAN_POINT('Ctrl Pts',(-9.90658661047469,-12.3305042760163,
118.554594905817)) ;
#157544 = CARTESIAN_POINT('Ctrl Pts',(-10.008066495342,-12.3604684800267,
118.827998813982)) ;
#157545 = CARTESIAN_POINT('Ctrl Pts',(-10.0026364882404,-12.434348796245,
118.811459888692)) ;
#157546 = CARTESIAN_POINT('Ctrl Pts',(-10.0764403349558,-12.4343487994094,
118.787228857044)) ;
#157547 = CARTESIAN_POINT('Ctrl Pts',(-10.1502441816713,-12.4343488025737,
118.762997825396)) ;
#157548 = CARTESIAN_POINT('Ctrl Pts',(-10.1556741887729,-12.3604684863554,
118.779536750686)) ;
#157549 = CARTESIAN_POINT('Ctrl Pts',(-10.1611041958745,-12.2865881701371,
118.796075675976)) ;
#157550 = CARTESIAN_POINT('Ctrl Pts',(-10.087300349159,-12.2865881669728,
118.820306707624)) ;
#157551 = CARTESIAN_POINT('Ctrl Pts',(-10.0134965024436,-12.2865881638084,
118.844537739272)) ;
#157552 = CARTESIAN_POINT('Ctrl Pts',(-10.008066495342,-12.3604684800267,
118.827998813982)) ;
#157553 = CARTESIAN_POINT('Ctrl Pts',(-10.1026122259296,-12.4650891112354,
119.080754567184)) ;
#157554 = CARTESIAN_POINT('Ctrl Pts',(-10.0913012354726,-12.5317749496589,
119.0463031154)) ;
#157555 = CARTESIAN_POINT('Ctrl Pts',(-10.1651050806005,-12.5317749532163,
119.022072078917)) ;
#157556 = CARTESIAN_POINT('Ctrl Pts',(-10.2389089257285,-12.5317749567737,
118.997841042433)) ;
#157557 = CARTESIAN_POINT('Ctrl Pts',(-10.2502199161856,-12.4650891183502,
119.032292494217)) ;
#157558 = CARTESIAN_POINT('Ctrl Pts',(-10.2615309066426,-12.3984032799266,
119.066743946)) ;
#157559 = CARTESIAN_POINT('Ctrl Pts',(-10.1877270615146,-12.3984032763692,
119.090974982484)) ;
#157560 = CARTESIAN_POINT('Ctrl Pts',(-10.1139232163866,-12.3984032728119,
119.115206018967)) ;
#157561 = CARTESIAN_POINT('Ctrl Pts',(-10.1026122259296,-12.4650891112354,
119.080754567184)) ;
#157562 = CARTESIAN_POINT('Ctrl Pts',(-10.1865625678926,-12.6397680496829,
119.300758559966)) ;
#157563 = CARTESIAN_POINT('Ctrl Pts',(-10.1701110588088,-12.6943569653302,
119.25064991775)) ;
#157564 = CARTESIAN_POINT('Ctrl Pts',(-10.2439149022629,-12.6943569660359,
119.226418876168)) ;
#157565 = CARTESIAN_POINT('Ctrl Pts',(-10.317718745717,-12.6943569667415,
119.202187834586)) ;
#157566 = CARTESIAN_POINT('Ctrl Pts',(-10.3341702548008,-12.6397680510942,
119.252296476803)) ;
#157567 = CARTESIAN_POINT('Ctrl Pts',(-10.3506217638846,-12.5851791354469,
119.302405119019)) ;
#157568 = CARTESIAN_POINT('Ctrl Pts',(-10.2768179204305,-12.5851791347412,
119.326636160601)) ;
#157569 = CARTESIAN_POINT('Ctrl Pts',(-10.2030140769763,-12.5851791340356,
119.350867202183)) ;
#157570 = CARTESIAN_POINT('Ctrl Pts',(-10.1865625678926,-12.6397680496829,
119.300758559966)) ;
#157571 = CARTESIAN_POINT('Ctrl Pts',(-10.2525551850904,-12.8673926753431,
119.466570849935)) ;
#157572 = CARTESIAN_POINT('Ctrl Pts',(-10.2321995339973,-12.9061686393151,
119.404570821043)) ;
#157573 = CARTESIAN_POINT('Ctrl Pts',(-10.3060033770812,-12.9061686378558,
119.380339778333)) ;
#157574 = CARTESIAN_POINT('Ctrl Pts',(-10.379807220165,-12.9061686363964,
119.356108735624)) ;
#157575 = CARTESIAN_POINT('Ctrl Pts',(-10.4001628712581,-12.8673926724244,
119.418108764515)) ;
#157576 = CARTESIAN_POINT('Ctrl Pts',(-10.4205185223511,-12.8286167084523,
119.480108793406)) ;
#157577 = CARTESIAN_POINT('Ctrl Pts',(-10.3467146792673,-12.8286167099117,
119.504339836116)) ;
#157578 = CARTESIAN_POINT('Ctrl Pts',(-10.2729108361835,-12.828616711371,
119.528570878826)) ;
#157579 = CARTESIAN_POINT('Ctrl Pts',(-10.2525551850904,-12.8673926753431,
119.466570849935)) ;
#157580 = CARTESIAN_POINT('Ctrl Pts',(-10.2984413344148,-13.138383085188,
119.5705591487)) ;
#157581 = CARTESIAN_POINT('Ctrl Pts',(-10.2755911957919,-13.1582932670834,
119.500961313244)) ;
#157582 = CARTESIAN_POINT('Ctrl Pts',(-10.3493950389077,-13.15829326372,119.476730270631)) ;
#157583 = CARTESIAN_POINT('Ctrl Pts',(-10.4231988820235,-13.1582932603565,
119.452499228019)) ;
#157584 = CARTESIAN_POINT('Ctrl Pts',(-10.4460490206464,-13.1383830784611,
119.522097063476)) ;
#157585 = CARTESIAN_POINT('Ctrl Pts',(-10.4688991592693,-13.1184728965658,
119.591694898932)) ;
#157586 = CARTESIAN_POINT('Ctrl Pts',(-10.3950953161535,-13.1184728999292,
119.615925941545)) ;
#157587 = CARTESIAN_POINT('Ctrl Pts',(-10.3212914730377,-13.1184729032926,
119.640156984157)) ;
#157588 = CARTESIAN_POINT('Ctrl Pts',(-10.2984413344148,-13.138383085188,
119.5705591487)) ;
#157589 = CARTESIAN_POINT('Ctrl Pts',(-10.3201874020919,-13.4250580301084,
119.601606079011)) ;
#157590 = CARTESIAN_POINT('Ctrl Pts',(-10.2965135474119,-13.4249798616491,
119.52949933737)) ;
#157591 = CARTESIAN_POINT('Ctrl Pts',(-10.3703173908735,-13.4249798591319,
119.50526829581)) ;
#157592 = CARTESIAN_POINT('Ctrl Pts',(-10.444121234335,-13.4249798566146,
119.481037254251)) ;
#157593 = CARTESIAN_POINT('Ctrl Pts',(-10.467795089015,-13.4250580250739,
119.553143995892)) ;
#157594 = CARTESIAN_POINT('Ctrl Pts',(-10.491468943695,-13.4251361935332,
119.625250737534)) ;
#157595 = CARTESIAN_POINT('Ctrl Pts',(-10.4176651002335,-13.4251361960505,
119.649481779093)) ;
#157596 = CARTESIAN_POINT('Ctrl Pts',(-10.3438612567719,-13.4251361985678,
119.673712820652)) ;
#157597 = CARTESIAN_POINT('Ctrl Pts',(-10.3201874020919,-13.4250580301084,
119.601606079011)) ;
#157598 = CARTESIAN_POINT('Ctrl Pts',(-10.3180530372285,-13.713663843469,
119.559606091718)) ;
#157599 = CARTESIAN_POINT('Ctrl Pts',(-10.2952280150007,-13.6934329579285,
119.490084756816)) ;
#157600 = CARTESIAN_POINT('Ctrl Pts',(-10.3690318585251,-13.6934329580841,
119.465853715448)) ;
#157601 = CARTESIAN_POINT('Ctrl Pts',(-10.4428357020495,-13.6934329582396,
119.441622674081)) ;
#157602 = CARTESIAN_POINT('Ctrl Pts',(-10.4656607242774,-13.7136638437801,
119.511144008982)) ;
#157603 = CARTESIAN_POINT('Ctrl Pts',(-10.4884857465052,-13.7338947293205,
119.580665343884)) ;
#157604 = CARTESIAN_POINT('Ctrl Pts',(-10.4146819029808,-13.733894729165,
119.604896385251)) ;
#157605 = CARTESIAN_POINT('Ctrl Pts',(-10.3408780594563,-13.7338947290095,
119.629127426619)) ;
#157606 = CARTESIAN_POINT('Ctrl Pts',(-10.3180530372285,-13.713663843469,
119.559606091718)) ;
#157607 = CARTESIAN_POINT('Ctrl Pts',(-10.2921786001434,-13.9818996954329,
119.445166371893)) ;
#157608 = CARTESIAN_POINT('Ctrl Pts',(-10.2718641660542,-13.9429089187137,
119.383291883489)) ;
#157609 = CARTESIAN_POINT('Ctrl Pts',(-10.3456680086685,-13.9429089238121,
119.359060839349)) ;
#157610 = CARTESIAN_POINT('Ctrl Pts',(-10.4194718512827,-13.9429089289105,
119.334829795209)) ;
#157611 = CARTESIAN_POINT('Ctrl Pts',(-10.4397862853719,-13.9818997056297,
119.396704283613)) ;
#157612 = CARTESIAN_POINT('Ctrl Pts',(-10.4601007194611,-14.0208904823489,
119.458578772017)) ;
#157613 = CARTESIAN_POINT('Ctrl Pts',(-10.3862968768469,-14.0208904772505,
119.482809816157)) ;
#157614 = CARTESIAN_POINT('Ctrl Pts',(-10.3124930342326,-14.0208904721521,
119.507040860297)) ;
#157615 = CARTESIAN_POINT('Ctrl Pts',(-10.2921786001434,-13.9818996954329,
119.445166371893)) ;
#157616 = CARTESIAN_POINT('Ctrl Pts',(-10.245938215231,-14.2073240866329,
119.269059645356)) ;
#157617 = CARTESIAN_POINT('Ctrl Pts',(-10.2295527871486,-14.1525370337597,
119.219152275396)) ;
#157618 = CARTESIAN_POINT('Ctrl Pts',(-10.303356628324,-14.1525370412397,
119.194921226873)) ;
#157619 = CARTESIAN_POINT('Ctrl Pts',(-10.3771604694994,-14.1525370487197,
119.170690178351)) ;
#157620 = CARTESIAN_POINT('Ctrl Pts',(-10.3935458975818,-14.2073241015929,
119.220597548311)) ;
#157621 = CARTESIAN_POINT('Ctrl Pts',(-10.4099313256642,-14.2621111544661,
119.270504918271)) ;
#157622 = CARTESIAN_POINT('Ctrl Pts',(-10.3361274844888,-14.2621111469861,
119.294735966793)) ;
#157623 = CARTESIAN_POINT('Ctrl Pts',(-10.2623236433134,-14.2621111395061,
119.318967015316)) ;
#157624 = CARTESIAN_POINT('Ctrl Pts',(-10.245938215231,-14.2073240866329,
119.269059645356)) ;
#157625 = CARTESIAN_POINT('Ctrl Pts',(-10.1827043131007,-14.3779496982449,
119.040941067964)) ;
#157626 = CARTESIAN_POINT('Ctrl Pts',(-10.1714452553299,-14.3111692669398,
119.006647794977)) ;
#157627 = CARTESIAN_POINT('Ctrl Pts',(-10.245249094003,-14.3111692758398,
118.982416738833)) ;
#157628 = CARTESIAN_POINT('Ctrl Pts',(-10.3190529326762,-14.3111692847398,
118.958185682689)) ;
#157629 = CARTESIAN_POINT('Ctrl Pts',(-10.330311990447,-14.3779497160448,
118.992478955676)) ;
#157630 = CARTESIAN_POINT('Ctrl Pts',(-10.3415710482178,-14.4447301473499,
119.026772228663)) ;
#157631 = CARTESIAN_POINT('Ctrl Pts',(-10.2677672095446,-14.4447301384499,
119.051003284807)) ;
#157632 = CARTESIAN_POINT('Ctrl Pts',(-10.1939633708715,-14.4447301295499,
119.075234340951)) ;
#157633 = CARTESIAN_POINT('Ctrl Pts',(-10.1827043131007,-14.3779496982449,
119.040941067964)) ;
#157634 = CARTESIAN_POINT('Ctrl Pts',(-10.1079403524329,-14.4795452062324,
118.777702483988)) ;
#157635 = CARTESIAN_POINT('Ctrl Pts',(-10.1026201618355,-14.405574238108,
118.761498042339)) ;
#157636 = CARTESIAN_POINT('Ctrl Pts',(-10.1764239974123,-14.4055742445888,
118.737266976764)) ;
#157637 = CARTESIAN_POINT('Ctrl Pts',(-10.250227832989,-14.4055742510696,
118.713035911189)) ;
#157638 = CARTESIAN_POINT('Ctrl Pts',(-10.2555480235865,-14.4795452191939,
118.729240352838)) ;
#157639 = CARTESIAN_POINT('Ctrl Pts',(-10.2608682141839,-14.5535161873183,
118.745444794488)) ;
#157640 = CARTESIAN_POINT('Ctrl Pts',(-10.1870643786071,-14.5535161808375,
118.769675860063)) ;
#157641 = CARTESIAN_POINT('Ctrl Pts',(-10.1132605430304,-14.5535161743567,
118.793906925638)) ;
#157642 = CARTESIAN_POINT('Ctrl Pts',(-10.1079403524329,-14.4795452062324,
118.777702483988)) ;
#157643 = CARTESIAN_POINT('Ctrl Pts',(-10.0277788315133,-14.504675613756,
118.497994836855)) ;
#157644 = CARTESIAN_POINT('Ctrl Pts',(-10.0287835153218,-14.4288427645242,
118.501054942308)) ;
#157645 = CARTESIAN_POINT('Ctrl Pts',(-10.1025873477986,-14.4288427635045,
118.476823867291)) ;
#157646 = CARTESIAN_POINT('Ctrl Pts',(-10.1763911802754,-14.4288427624848,
118.452592792274)) ;
#157647 = CARTESIAN_POINT('Ctrl Pts',(-10.1753864964669,-14.5046756117167,
118.449532686821)) ;
#157648 = CARTESIAN_POINT('Ctrl Pts',(-10.1743818126584,-14.5805084609485,
118.446472581367)) ;
#157649 = CARTESIAN_POINT('Ctrl Pts',(-10.1005779801816,-14.5805084619682,
118.470703656384)) ;
#157650 = CARTESIAN_POINT('Ctrl Pts',(-10.0267741477048,-14.5805084629879,
118.494934731401)) ;
#157651 = CARTESIAN_POINT('Ctrl Pts',(-10.0277788315133,-14.504675613756,
118.497994836855)) ;
#157652 = CARTESIAN_POINT('Ctrl Pts',(-9.94934961424335,-14.4524935600785,
118.223832977652)) ;
#157653 = CARTESIAN_POINT('Ctrl Pts',(-9.95656164691611,-14.3801950254555,
118.245799666326)) ;
#157654 = CARTESIAN_POINT('Ctrl Pts',(-10.030365477824,-14.3801950131856,
118.22156858653)) ;
#157655 = CARTESIAN_POINT('Ctrl Pts',(-10.1041693087319,-14.3801950009157,
118.197337506734)) ;
#157656 = CARTESIAN_POINT('Ctrl Pts',(-10.0969572760591,-14.4524935355387,
118.175370818061)) ;
#157657 = CARTESIAN_POINT('Ctrl Pts',(-10.0897452433863,-14.5247920701618,
118.153404129387)) ;
#157658 = CARTESIAN_POINT('Ctrl Pts',(-10.0159414124784,-14.5247920824317,
118.177635209183)) ;
#157659 = CARTESIAN_POINT('Ctrl Pts',(-9.94213758157056,-14.5247920947016,
118.201866288978)) ;
#157660 = CARTESIAN_POINT('Ctrl Pts',(-9.94934961424335,-14.4524935600785,
118.223832977652)) ;
#157661 = CARTESIAN_POINT('Ctrl Pts',(-9.8776805943081,-14.3253673837965,
117.969892660447)) ;
#157662 = CARTESIAN_POINT('Ctrl Pts',(-9.89064463115639,-14.2618396984513,
118.009379025961)) ;
#157663 = CARTESIAN_POINT('Ctrl Pts',(-9.96444846077423,-14.2618396702595,
117.985147942236)) ;
#157664 = CARTESIAN_POINT('Ctrl Pts',(-10.0382522903921,-14.2618396420677,
117.960916858511)) ;
#157665 = CARTESIAN_POINT('Ctrl Pts',(-10.0252882535438,-14.325367327413,
117.921430492997)) ;
#157666 = CARTESIAN_POINT('Ctrl Pts',(-10.0123242166955,-14.3888950127582,
117.881944127484)) ;
#157667 = CARTESIAN_POINT('Ctrl Pts',(-9.93852038707766,-14.38889504095,117.906175211209)) ;
#157668 = CARTESIAN_POINT('Ctrl Pts',(-9.86471655745981,-14.3888950691418,
117.930406294933)) ;
#157669 = CARTESIAN_POINT('Ctrl Pts',(-9.8776805943081,-14.3253673837965,
117.969892660447)) ;
#157670 = CARTESIAN_POINT('Ctrl Pts',(-9.81989105535084,-14.1335026343525,
117.758421157027)) ;
#157671 = CARTESIAN_POINT('Ctrl Pts',(-9.83764223195818,-14.0832788793335,
117.812488378008)) ;
#157672 = CARTESIAN_POINT('Ctrl Pts',(-9.91144606272761,-14.0832788338596,
117.78825729779)) ;
#157673 = CARTESIAN_POINT('Ctrl Pts',(-9.98524989349704,-14.0832787883857,
117.764026217573)) ;
#157674 = CARTESIAN_POINT('Ctrl Pts',(-9.96749871688968,-14.1335025434047,
117.709958996592)) ;
#157675 = CARTESIAN_POINT('Ctrl Pts',(-9.94974754028233,-14.1837262984236,
117.655891775611)) ;
#157676 = CARTESIAN_POINT('Ctrl Pts',(-9.87594370951292,-14.1837263438975,
117.680122855828)) ;
#157677 = CARTESIAN_POINT('Ctrl Pts',(-9.80213987874348,-14.1837263893715,
117.704353936045)) ;
#157678 = CARTESIAN_POINT('Ctrl Pts',(-9.81989105535084,-14.1335026343525,
117.758421157027)) ;
#157679 = CARTESIAN_POINT('Ctrl Pts',(-9.78045273451247,-13.8914689377216,
117.602957988204)) ;
#157680 = CARTESIAN_POINT('Ctrl Pts',(-9.80171425934229,-13.8580710694063,
117.667717163616)) ;
#157681 = CARTESIAN_POINT('Ctrl Pts',(-9.87551809334006,-13.8580710084392,
117.643486093231)) ;
#157682 = CARTESIAN_POINT('Ctrl Pts',(-9.94932192733782,-13.8580709474722,
117.619255022847)) ;
#157683 = CARTESIAN_POINT('Ctrl Pts',(-9.92806040250799,-13.8914688157875,
117.554495847435)) ;
#157684 = CARTESIAN_POINT('Ctrl Pts',(-9.90679887767815,-13.9248666841028,
117.489736672023)) ;
#157685 = CARTESIAN_POINT('Ctrl Pts',(-9.83299504368039,-13.9248667450698,
117.513967742407)) ;
#157686 = CARTESIAN_POINT('Ctrl Pts',(-9.75919120968263,-13.9248668060369,
117.538198812791)) ;
#157687 = CARTESIAN_POINT('Ctrl Pts',(-9.78045273451247,-13.8914689377216,
117.602957988204)) ;
#157688 = CARTESIAN_POINT('Ctrl Pts',(-9.76271568007487,-13.6147208150664,
117.513467417372)) ;
#157689 = CARTESIAN_POINT('Ctrl Pts',(-9.78598021616308,-13.6005963890855,
117.584327442045)) ;
#157690 = CARTESIAN_POINT('Ctrl Pts',(-9.85978405508859,-13.6005963145347,
117.56009638667)) ;
#157691 = CARTESIAN_POINT('Ctrl Pts',(-9.93358789401411,-13.600596239984,
117.535865331294)) ;
#157692 = CARTESIAN_POINT('Ctrl Pts',(-9.91032335792589,-13.6147206659649,
117.465005306621)) ;
#157693 = CARTESIAN_POINT('Ctrl Pts',(-9.88705882183766,-13.6288450919457,
117.394145281948)) ;
#157694 = CARTESIAN_POINT('Ctrl Pts',(-9.81325498291215,-13.6288451664965,
117.418376337323)) ;
#157695 = CARTESIAN_POINT('Ctrl Pts',(-9.73945114398663,-13.6288452410473,
117.442607392699)) ;
#157696 = CARTESIAN_POINT('Ctrl Pts',(-9.76271568007487,-13.6147208150664,
117.513467417372)) ;
#157697 = CARTESIAN_POINT('Ctrl Pts',(-9.76890870119331,-13.3237687258409,
117.4968563122)) ;
#157698 = CARTESIAN_POINT('Ctrl Pts',(-9.7925086415556,-13.3299371797537,
117.568737924317)) ;
#157699 = CARTESIAN_POINT('Ctrl Pts',(-9.86631248703233,-13.3299370967314,
117.544506888895)) ;
#157700 = CARTESIAN_POINT('Ctrl Pts',(-9.94011633250904,-13.329937013709,
117.520275853474)) ;
#157701 = CARTESIAN_POINT('Ctrl Pts',(-9.91651639214676,-13.3237685597962,
117.448394241357)) ;
#157702 = CARTESIAN_POINT('Ctrl Pts',(-9.89291645178446,-13.3176001058834,
117.376512629241)) ;
#157703 = CARTESIAN_POINT('Ctrl Pts',(-9.81911260630774,-13.3176001889057,
117.400743664662)) ;
#157704 = CARTESIAN_POINT('Ctrl Pts',(-9.74530876083102,-13.3176002719281,
117.424974700083)) ;
#157705 = CARTESIAN_POINT('Ctrl Pts',(-9.76890870119331,-13.3237687258409,
117.4968563122)) ;
#157706 = CARTESIAN_POINT('Ctrl Pts',(-9.79936071736111,-13.0396242352637,
117.554132453179)) ;
#157707 = CARTESIAN_POINT('Ctrl Pts',(-9.82160297578344,-13.0656396906541,
117.621878785295)) ;
#157708 = CARTESIAN_POINT('Ctrl Pts',(-9.89540682880252,-13.0656396062825,
117.597647772846)) ;
#157709 = CARTESIAN_POINT('Ctrl Pts',(-9.96921068182159,-13.0656395219109,
117.573416760398)) ;
#157710 = CARTESIAN_POINT('Ctrl Pts',(-9.94696842339928,-13.0396240665205,
117.505670428282)) ;
#157711 = CARTESIAN_POINT('Ctrl Pts',(-9.92472616497694,-13.0136086111301,
117.437924096167)) ;
#157712 = CARTESIAN_POINT('Ctrl Pts',(-9.85092231195787,-13.0136086955017,
117.462155108615)) ;
#157713 = CARTESIAN_POINT('Ctrl Pts',(-9.77711845893878,-13.0136087798733,
117.486386121064)) ;
#157714 = CARTESIAN_POINT('Ctrl Pts',(-9.79936071736111,-13.0396242352637,
117.554132453179)) ;
#157715 = CARTESIAN_POINT('Ctrl Pts',(-9.85239927743223,-12.7830678889279,
117.680294085095)) ;
#157716 = CARTESIAN_POINT('Ctrl Pts',(-9.87170308697766,-12.8270330002595,
117.73909037615)) ;
#157717 = CARTESIAN_POINT('Ctrl Pts',(-9.94550694758217,-12.8270329227443,
117.714859386806)) ;
#157718 = CARTESIAN_POINT('Ctrl Pts',(-10.0193108081867,-12.8270328452292,
117.690628397462)) ;
#157719 = CARTESIAN_POINT('Ctrl Pts',(-10.0000069986413,-12.7830677338975,
117.631832106406)) ;
#157720 = CARTESIAN_POINT('Ctrl Pts',(-9.98070318909583,-12.7391026225659,
117.573035815351)) ;
#157721 = CARTESIAN_POINT('Ctrl Pts',(-9.90689932849131,-12.739102700081,
117.597266804696)) ;
#157722 = CARTESIAN_POINT('Ctrl Pts',(-9.83309546788681,-12.7391027775962,
117.62149779404)) ;
#157723 = CARTESIAN_POINT('Ctrl Pts',(-9.85239927743223,-12.7830678889279,
117.680294085095)) ;
#157724 = CARTESIAN_POINT('Ctrl Pts',(-9.9257847579806,-12.5704752635878,
117.868146840537)) ;
#157725 = CARTESIAN_POINT('Ctrl Pts',(-9.94073149886832,-12.6293473017033,
117.913672203583)) ;
#157726 = CARTESIAN_POINT('Ctrl Pts',(-10.0145353667142,-12.6293472382111,
117.889441236294)) ;
#157727 = CARTESIAN_POINT('Ctrl Pts',(-10.0883392345601,-12.6293471747189,
117.865210269006)) ;
#157728 = CARTESIAN_POINT('Ctrl Pts',(-10.0733924936724,-12.5704751366034,
117.819684905961)) ;
#157729 = CARTESIAN_POINT('Ctrl Pts',(-10.0584457527847,-12.5116030984879,
117.774159542916)) ;
#157730 = CARTESIAN_POINT('Ctrl Pts',(-9.9846418849388,-12.5116031619801,
117.798390510204)) ;
#157731 = CARTESIAN_POINT('Ctrl Pts',(-9.91083801709289,-12.5116032254723,
117.822621477492)) ;
#157732 = CARTESIAN_POINT('Ctrl Pts',(-9.9257847579806,-12.5704752635878,
117.868146840537)) ;
#157733 = CARTESIAN_POINT('Ctrl Pts',(-10.0135422022618,-12.4206416986158,
118.100172237485)) ;
#157734 = CARTESIAN_POINT('Ctrl Pts',(-10.0231135704383,-12.490060480766,
118.129325082619)) ;
#157735 = CARTESIAN_POINT('Ctrl Pts',(-10.0969174434593,-12.4900604392227,
118.105094131093)) ;
#157736 = CARTESIAN_POINT('Ctrl Pts',(-10.1707213164804,-12.4900603976793,
118.080863179567)) ;
#157737 = CARTESIAN_POINT('Ctrl Pts',(-10.1611499483039,-12.4206416155292,
118.051710334434)) ;
#157738 = CARTESIAN_POINT('Ctrl Pts',(-10.1515785801275,-12.351222833379,
118.0225574893)) ;
#157739 = CARTESIAN_POINT('Ctrl Pts',(-10.0777747071064,-12.3512228749223,
118.046788440826)) ;
#157740 = CARTESIAN_POINT('Ctrl Pts',(-10.0039708340854,-12.3512229164656,
118.071019392351)) ;
#157741 = CARTESIAN_POINT('Ctrl Pts',(-10.0135422022618,-12.4206416986158,
118.100172237485)) ;
#157742 = CARTESIAN_POINT('Ctrl Pts',(-10.1114862816905,-12.3408954926335,
118.363002383417)) ;
#157743 = CARTESIAN_POINT('Ctrl Pts',(-10.114968062946,-12.4159838825569,
118.373607329397)) ;
#157744 = CARTESIAN_POINT('Ctrl Pts',(-10.1887719392433,-12.4159838672949,
118.34937638785)) ;
#157745 = CARTESIAN_POINT('Ctrl Pts',(-10.2625758155405,-12.4159838520328,
118.325145446303)) ;
#157746 = CARTESIAN_POINT('Ctrl Pts',(-10.259094034285,-12.3408954621094,
118.314540500324)) ;
#157747 = CARTESIAN_POINT('Ctrl Pts',(-10.2556122530295,-12.265807072186,
118.303935554344)) ;
#157748 = CARTESIAN_POINT('Ctrl Pts',(-10.1818083767322,-12.265807087448,
118.32816649589)) ;
#157749 = CARTESIAN_POINT('Ctrl Pts',(-10.1080045004349,-12.26580710271,118.352397437437)) ;
#157750 = CARTESIAN_POINT('Ctrl Pts',(-10.1114862816905,-12.3408954926335,
118.363002383417)) ;
#157751 = CARTESIAN_POINT('Ctrl Pts',(-10.2131168846024,-12.3388375024718,
118.636985267721)) ;
#157752 = CARTESIAN_POINT('Ctrl Pts',(-10.2102443248058,-12.4141806587766,
118.628235916156)) ;
#157753 = CARTESIAN_POINT('Ctrl Pts',(-10.2840482016702,-12.414180672439,
118.604004976337)) ;
#157754 = CARTESIAN_POINT('Ctrl Pts',(-10.3578520785346,-12.4141806861015,
118.579774036517)) ;
#157755 = CARTESIAN_POINT('Ctrl Pts',(-10.3607246383311,-12.3388375297967,
118.588523388082)) ;
#157756 = CARTESIAN_POINT('Ctrl Pts',(-10.3635971981277,-12.263494373492,
118.597272739647)) ;
#157757 = CARTESIAN_POINT('Ctrl Pts',(-10.2897933212633,-12.2634943598295,
118.621503679467)) ;
#157758 = CARTESIAN_POINT('Ctrl Pts',(-10.2159894443989,-12.2634943461671,
118.645734619286)) ;
#157759 = CARTESIAN_POINT('Ctrl Pts',(-10.2131168846024,-12.3388375024718,
118.636985267721)) ;
#157760 = CARTESIAN_POINT('Ctrl Pts',(-10.3111631418804,-12.413706142133,
118.900239883285)) ;
#157761 = CARTESIAN_POINT('Ctrl Pts',(-10.3021731424948,-12.4839334398815,
118.872857797784)) ;
#157762 = CARTESIAN_POINT('Ctrl Pts',(-10.3759770171298,-12.4839334817003,
118.848626851174)) ;
#157763 = CARTESIAN_POINT('Ctrl Pts',(-10.4497808917647,-12.4839335235192,
118.824395904564)) ;
#157764 = CARTESIAN_POINT('Ctrl Pts',(-10.4587708911503,-12.4137062257707,
118.851777990065)) ;
#157765 = CARTESIAN_POINT('Ctrl Pts',(-10.4677608905359,-12.3434789280223,
118.879160075566)) ;
#157766 = CARTESIAN_POINT('Ctrl Pts',(-10.3939570159009,-12.3434788862035,
118.903391022176)) ;
#157767 = CARTESIAN_POINT('Ctrl Pts',(-10.3201531412659,-12.3434788443846,
118.927621968785)) ;
#157768 = CARTESIAN_POINT('Ctrl Pts',(-10.3111631418804,-12.413706142133,
118.900239883285)) ;
#157769 = CARTESIAN_POINT('Ctrl Pts',(-10.4005037459975,-12.5617183582742,
119.136700846574)) ;
#157770 = CARTESIAN_POINT('Ctrl Pts',(-10.3860007082531,-12.6217168854957,
119.092526935736)) ;
#157771 = CARTESIAN_POINT('Ctrl Pts',(-10.4598045779934,-12.6217169518503,
119.068295974218)) ;
#157772 = CARTESIAN_POINT('Ctrl Pts',(-10.5336084477337,-12.6217170182048,
119.044065012699)) ;
#157773 = CARTESIAN_POINT('Ctrl Pts',(-10.5481114854781,-12.5617184909834,
119.088238923537)) ;
#157774 = CARTESIAN_POINT('Ctrl Pts',(-10.5626145232225,-12.501719963762,
119.132412834375)) ;
#157775 = CARTESIAN_POINT('Ctrl Pts',(-10.4888106534822,-12.5017198974074,
119.156643795893)) ;
#157776 = CARTESIAN_POINT('Ctrl Pts',(-10.4150067837419,-12.5017198310528,
119.180874757412)) ;
#157777 = CARTESIAN_POINT('Ctrl Pts',(-10.4005037459975,-12.5617183582742,
119.136700846574)) ;
#157778 = CARTESIAN_POINT('Ctrl Pts',(-10.4738998219897,-12.7688407831079,
119.325034793762)) ;
#157779 = CARTESIAN_POINT('Ctrl Pts',(-10.4549797292597,-12.8144672602671,
119.267407246099)) ;
#157780 = CARTESIAN_POINT('Ctrl Pts',(-10.5287835923174,-12.8144673453734,
119.243176264227)) ;
#157781 = CARTESIAN_POINT('Ctrl Pts',(-10.6025874553752,-12.8144674304797,
119.218945282355)) ;
#157782 = CARTESIAN_POINT('Ctrl Pts',(-10.6215075481052,-12.7688409533206,
119.276572830018)) ;
#157783 = CARTESIAN_POINT('Ctrl Pts',(-10.6404276408353,-12.7232144761614,
119.334200377682)) ;
#157784 = CARTESIAN_POINT('Ctrl Pts',(-10.5666237777775,-12.7232143910551,
119.358431359554)) ;
#157785 = CARTESIAN_POINT('Ctrl Pts',(-10.4928199147197,-12.7232143059487,
119.382662341426)) ;
#157786 = CARTESIAN_POINT('Ctrl Pts',(-10.4738998219897,-12.7688407831079,
119.325034793762)) ;
#157787 = CARTESIAN_POINT('Ctrl Pts',(-10.528497781938,-13.0241117816514,
119.455791678547)) ;
#157788 = CARTESIAN_POINT('Ctrl Pts',(-10.5064729183125,-13.0519843902153,
119.388707499628)) ;
#157789 = CARTESIAN_POINT('Ctrl Pts',(-10.580276773221,-13.0519844861314,
119.364476492934)) ;
#157790 = CARTESIAN_POINT('Ctrl Pts',(-10.6540806281294,-13.0519845820475,
119.34024548624)) ;
#157791 = CARTESIAN_POINT('Ctrl Pts',(-10.6761054917549,-13.0241119734836,
119.407329665159)) ;
#157792 = CARTESIAN_POINT('Ctrl Pts',(-10.6981303553804,-12.9962393649197,
119.474413844078)) ;
#157793 = CARTESIAN_POINT('Ctrl Pts',(-10.624326500472,-12.9962392690036,
119.498644850772)) ;
#157794 = CARTESIAN_POINT('Ctrl Pts',(-10.5505226455635,-12.9962391730874,
119.522875857466)) ;
#157795 = CARTESIAN_POINT('Ctrl Pts',(-10.528497781938,-13.0241117816514,
119.455791678547)) ;
#157796 = CARTESIAN_POINT('Ctrl Pts',(-10.5602307777131,-13.3070010234793,
119.517011250028)) ;
#157797 = CARTESIAN_POINT('Ctrl Pts',(-10.5366906221351,-13.31516473517,119.445311736237)) ;
#157798 = CARTESIAN_POINT('Ctrl Pts',(-10.6104944685515,-13.3151648334865,
119.421080703678)) ;
#157799 = CARTESIAN_POINT('Ctrl Pts',(-10.684298314968,-13.315164931803,119.396849671119)) ;
#157800 = CARTESIAN_POINT('Ctrl Pts',(-10.7078384705459,-13.3070012201123,
119.46854918491)) ;
#157801 = CARTESIAN_POINT('Ctrl Pts',(-10.7313786261238,-13.2988375084216,
119.540248698701)) ;
#157802 = CARTESIAN_POINT('Ctrl Pts',(-10.6575747797074,-13.2988374101051,
119.56447973126)) ;
#157803 = CARTESIAN_POINT('Ctrl Pts',(-10.583770933291,-13.2988373117886,
119.588710763819)) ;
#157804 = CARTESIAN_POINT('Ctrl Pts',(-10.5602307777131,-13.3070010234793,
119.517011250028)) ;
#157805 = CARTESIAN_POINT('Ctrl Pts',(-10.5678547390295,-13.5985554109386,
119.504704332823)) ;
#157806 = CARTESIAN_POINT('Ctrl Pts',(-10.5444820245611,-13.5863758262572,
119.43351481753)) ;
#157807 = CARTESIAN_POINT('Ctrl Pts',(-10.6182858629544,-13.5863759182584,
119.409283760534)) ;
#157808 = CARTESIAN_POINT('Ctrl Pts',(-10.6920897013477,-13.5863760102596,
119.385052703538)) ;
#157809 = CARTESIAN_POINT('Ctrl Pts',(-10.7154624158161,-13.5985555949411,
119.45624221883)) ;
#157810 = CARTESIAN_POINT('Ctrl Pts',(-10.7388351302845,-13.6107351796225,
119.527431734122)) ;
#157811 = CARTESIAN_POINT('Ctrl Pts',(-10.6650312918912,-13.6107350876213,
119.551662791119)) ;
#157812 = CARTESIAN_POINT('Ctrl Pts',(-10.5912274534979,-13.6107349956201,
119.575893848115)) ;
#157813 = CARTESIAN_POINT('Ctrl Pts',(-10.5678547390295,-13.5985554109386,
119.504704332823)) ;
#157814 = CARTESIAN_POINT('Ctrl Pts',(-10.5513598758863,-13.8770852609277,
119.418937728725)) ;
#157815 = CARTESIAN_POINT('Ctrl Pts',(-10.5298386410176,-13.8454408144546,
119.353387521432)) ;
#157816 = CARTESIAN_POINT('Ctrl Pts',(-10.6036424728301,-13.8454408929621,
119.329156444392)) ;
#157817 = CARTESIAN_POINT('Ctrl Pts',(-10.6774463046426,-13.8454409714697,
119.304925367352)) ;
#157818 = CARTESIAN_POINT('Ctrl Pts',(-10.6989675395113,-13.8770854179428,
119.370475574645)) ;
#157819 = CARTESIAN_POINT('Ctrl Pts',(-10.72048877438,-13.9087298644159,119.436025781938)) ;
#157820 = CARTESIAN_POINT('Ctrl Pts',(-10.6466849425675,-13.9087297859083,
119.460256858978)) ;
#157821 = CARTESIAN_POINT('Ctrl Pts',(-10.572881110755,-13.9087297074008,
119.484487936018)) ;
#157822 = CARTESIAN_POINT('Ctrl Pts',(-10.5513598758863,-13.8770852609277,
119.418937728725)) ;
#157823 = CARTESIAN_POINT('Ctrl Pts',(-10.5130330103292,-14.1214182763711,
119.266862919213)) ;
#157824 = CARTESIAN_POINT('Ctrl Pts',(-10.4948865671328,-14.0726671201406,
119.21159178272)) ;
#157825 = CARTESIAN_POINT('Ctrl Pts',(-10.5686903940646,-14.0726671815673,
119.187360690814)) ;
#157826 = CARTESIAN_POINT('Ctrl Pts',(-10.6424942209963,-14.072667242994,
119.163129598908)) ;
#157827 = CARTESIAN_POINT('Ctrl Pts',(-10.6606406641927,-14.1214183992245,
119.2184007354)) ;
#157828 = CARTESIAN_POINT('Ctrl Pts',(-10.6787871073891,-14.170169555455,
119.273671871893)) ;
#157829 = CARTESIAN_POINT('Ctrl Pts',(-10.6049832804574,-14.1701694940283,
119.297902963799)) ;
#157830 = CARTESIAN_POINT('Ctrl Pts',(-10.5311794535256,-14.1701694326015,
119.322134055705)) ;
#157831 = CARTESIAN_POINT('Ctrl Pts',(-10.5130330103292,-14.1214182763711,
119.266862919213)) ;
#157832 = CARTESIAN_POINT('Ctrl Pts',(-10.4561208615973,-14.3164119676812,
119.058063869766)) ;
#157833 = CARTESIAN_POINT('Ctrl Pts',(-10.4426541691121,-14.2539728440819,
119.017046498723)) ;
#157834 = CARTESIAN_POINT('Ctrl Pts',(-10.5164579934008,-14.2539728850066,
118.992815398767)) ;
#157835 = CARTESIAN_POINT('Ctrl Pts',(-10.5902618176896,-14.2539729259314,
118.968584298811)) ;
#157836 = CARTESIAN_POINT('Ctrl Pts',(-10.6037285101748,-14.3164120495308,
119.009601669854)) ;
#157837 = CARTESIAN_POINT('Ctrl Pts',(-10.6171952026601,-14.3788511731302,
119.050619040897)) ;
#157838 = CARTESIAN_POINT('Ctrl Pts',(-10.5433913783713,-14.3788511322054,
119.074850140853)) ;
#157839 = CARTESIAN_POINT('Ctrl Pts',(-10.4695875540826,-14.3788510912806,
119.099081240809)) ;
#157840 = CARTESIAN_POINT('Ctrl Pts',(-10.4561208615973,-14.3164119676812,
119.058063869766)) ;
#157841 = CARTESIAN_POINT('Ctrl Pts',(-10.3852189870946,-14.4472714989735,
118.806537992562)) ;
#157842 = CARTESIAN_POINT('Ctrl Pts',(-10.3774182459339,-14.3756009231922,
118.782778194882)) ;
#157843 = CARTESIAN_POINT('Ctrl Pts',(-10.4512220701755,-14.3756009434077,
118.758547094782)) ;
#157844 = CARTESIAN_POINT('Ctrl Pts',(-10.525025894417,-14.3756009636232,
118.734315994681)) ;
#157845 = CARTESIAN_POINT('Ctrl Pts',(-10.5328266355777,-14.4472715394045,
118.758075792362)) ;
#157846 = CARTESIAN_POINT('Ctrl Pts',(-10.5406273767383,-14.5189421151858,
118.781835590042)) ;
#157847 = CARTESIAN_POINT('Ctrl Pts',(-10.4668235524968,-14.5189420949703,
118.806066690143)) ;
#157848 = CARTESIAN_POINT('Ctrl Pts',(-10.3930197282553,-14.5189420747548,
118.830297790243)) ;
#157849 = CARTESIAN_POINT('Ctrl Pts',(-10.3852189870946,-14.4472714989735,
118.806537992562)) ;
#157850 = CARTESIAN_POINT('Ctrl Pts',(-10.3066385089528,-14.5039655219921,
118.531734459687)) ;
#157851 = CARTESIAN_POINT('Ctrl Pts',(-10.305046250753,-14.4282278620231,
118.526884699208)) ;
#157852 = CARTESIAN_POINT('Ctrl Pts',(-10.37885007664,-14.4282278646451,118.502653604119)) ;
#157853 = CARTESIAN_POINT('Ctrl Pts',(-10.4526539025269,-14.4282278672671,
118.47842250903)) ;
#157854 = CARTESIAN_POINT('Ctrl Pts',(-10.4542461607266,-14.5039655272361,
118.48327226951)) ;
#157855 = CARTESIAN_POINT('Ctrl Pts',(-10.4558384189264,-14.5797031872051,
118.48812202999)) ;
#157856 = CARTESIAN_POINT('Ctrl Pts',(-10.3820345930394,-14.5797031845831,
118.512353125078)) ;
#157857 = CARTESIAN_POINT('Ctrl Pts',(-10.3082307671525,-14.5797031819611,
118.536584220167)) ;
#157858 = CARTESIAN_POINT('Ctrl Pts',(-10.3066385089528,-14.5039655219921,
118.531734459687)) ;
#157859 = CARTESIAN_POINT('Ctrl Pts',(-10.2263549450695,-14.4826373105238,
118.251644902637)) ;
#157860 = CARTESIAN_POINT('Ctrl Pts',(-10.2311016200229,-14.4082736216989,
118.266102509573)) ;
#157861 = CARTESIAN_POINT('Ctrl Pts',(-10.3049054492475,-14.4082736113454,
118.24187142465)) ;
#157862 = CARTESIAN_POINT('Ctrl Pts',(-10.378709278472,-14.4082736009919,
118.217640339728)) ;
#157863 = CARTESIAN_POINT('Ctrl Pts',(-10.3739626035186,-14.4826372898169,
118.203182732792)) ;
#157864 = CARTESIAN_POINT('Ctrl Pts',(-10.3692159285652,-14.5570009786418,
118.188725125855)) ;
#157865 = CARTESIAN_POINT('Ctrl Pts',(-10.2954120993406,-14.5570009889953,
118.212956210778)) ;
#157866 = CARTESIAN_POINT('Ctrl Pts',(-10.2216082701161,-14.5570009993487,
118.237187295701)) ;
#157867 = CARTESIAN_POINT('Ctrl Pts',(-10.2263549450695,-14.4826373105238,
118.251644902637)) ;
#157868 = CARTESIAN_POINT('Ctrl Pts',(-10.1515928117172,-14.3855815012644,
117.988618093193)) ;
#157869 = CARTESIAN_POINT('Ctrl Pts',(-10.1622974516462,-14.3178820902551,
118.021222699991)) ;
#157870 = CARTESIAN_POINT('Ctrl Pts',(-10.2361012842216,-14.3178820716342,
117.996991625275)) ;
#157871 = CARTESIAN_POINT('Ctrl Pts',(-10.309905116797,-14.3178820530132,
117.972760550558)) ;
#157872 = CARTESIAN_POINT('Ctrl Pts',(-10.299200476868,-14.3855814640225,
117.94015594376)) ;
#157873 = CARTESIAN_POINT('Ctrl Pts',(-10.288495836939,-14.4532808750318,
117.907551336961)) ;
#157874 = CARTESIAN_POINT('Ctrl Pts',(-10.2146920043635,-14.4532808936528,
117.931782411678)) ;
#157875 = CARTESIAN_POINT('Ctrl Pts',(-10.1408881717881,-14.4532809122737,
117.956013486395)) ;
#157876 = CARTESIAN_POINT('Ctrl Pts',(-10.1515928117172,-14.3855815012644,
117.988618093193)) ;
#157877 = CARTESIAN_POINT('Ctrl Pts',(-10.0875742094217,-14.2190969785884,
117.758158308275)) ;
#157878 = CARTESIAN_POINT('Ctrl Pts',(-10.1034990260791,-14.1629192872983,
117.806662730949)) ;
#157879 = CARTESIAN_POINT('Ctrl Pts',(-10.1773028625826,-14.1629192658567,
117.782431668197)) ;
#157880 = CARTESIAN_POINT('Ctrl Pts',(-10.2511066990861,-14.1629192444152,
117.758200605445)) ;
#157881 = CARTESIAN_POINT('Ctrl Pts',(-10.2351818824287,-14.2190969357053,
117.709696182771)) ;
#157882 = CARTESIAN_POINT('Ctrl Pts',(-10.2192570657713,-14.2752746269954,
117.661191760097)) ;
#157883 = CARTESIAN_POINT('Ctrl Pts',(-10.1454532292678,-14.275274648437,
117.685422822849)) ;
#157884 = CARTESIAN_POINT('Ctrl Pts',(-10.0716493927643,-14.2752746698786,
117.709653885601)) ;
#157885 = CARTESIAN_POINT('Ctrl Pts',(-10.0875742094217,-14.2190969785884,
117.758158308275)) ;
#157886 = CARTESIAN_POINT('Ctrl Pts',(-10.0400271797391,-13.9949296481822,
117.577849034879)) ;
#157887 = CARTESIAN_POINT('Ctrl Pts',(-10.0600304577515,-13.9543190677503,
117.638775792622)) ;
#157888 = CARTESIAN_POINT('Ctrl Pts',(-10.1338342976265,-13.9543190483412,
117.614544740138)) ;
#157889 = CARTESIAN_POINT('Ctrl Pts',(-10.2076381375015,-13.9543190289321,
117.590313687655)) ;
#157890 = CARTESIAN_POINT('Ctrl Pts',(-10.1876348594891,-13.9949296093639,
117.529386929912)) ;
#157891 = CARTESIAN_POINT('Ctrl Pts',(-10.1676315814767,-14.0355401897957,
117.468460172169)) ;
#157892 = CARTESIAN_POINT('Ctrl Pts',(-10.0938277416017,-14.0355402092049,
117.492691224653)) ;
#157893 = CARTESIAN_POINT('Ctrl Pts',(-10.0200239017268,-14.035540228614,
117.516922277136)) ;
#157894 = CARTESIAN_POINT('Ctrl Pts',(-10.0400271797391,-13.9949296481822,
117.577849034879)) ;
#157895 = CARTESIAN_POINT('Ctrl Pts',(-10.013089520595,-13.7298783707897,
117.46036854867)) ;
#157896 = CARTESIAN_POINT('Ctrl Pts',(-10.0357371803655,-13.7077134495774,
117.529349666438)) ;
#157897 = CARTESIAN_POINT('Ctrl Pts',(-10.1095410226297,-13.7077134348718,
117.505118621232)) ;
#157898 = CARTESIAN_POINT('Ctrl Pts',(-10.1833448648939,-13.7077134201661,
117.480887576025)) ;
#157899 = CARTESIAN_POINT('Ctrl Pts',(-10.1606972051234,-13.7298783413784,
117.411906458258)) ;
#157900 = CARTESIAN_POINT('Ctrl Pts',(-10.138049545353,-13.7520432625907,
117.342925340491)) ;
#157901 = CARTESIAN_POINT('Ctrl Pts',(-10.0642457030888,-13.7520432772964,
117.367156385697)) ;
#157902 = CARTESIAN_POINT('Ctrl Pts',(-9.99044186082453,-13.752043292002,
117.391387430903)) ;
#157903 = CARTESIAN_POINT('Ctrl Pts',(-10.013089520595,-13.7298783707897,
117.46036854867)) ;
#157904 = CARTESIAN_POINT('Ctrl Pts',(-10.0095205229371,-13.4411780607526,
117.413901364897)) ;
#157905 = CARTESIAN_POINT('Ctrl Pts',(-10.033188325731,-13.4391385958436,
117.485989673571)) ;
#157906 = CARTESIAN_POINT('Ctrl Pts',(-10.1069921692462,-13.4391385881017,
117.461758632175)) ;
#157907 = CARTESIAN_POINT('Ctrl Pts',(-10.1807960127614,-13.4391385803598,
117.437527590779)) ;
#157908 = CARTESIAN_POINT('Ctrl Pts',(-10.1571282099675,-13.4411780452688,
117.365439282106)) ;
#157909 = CARTESIAN_POINT('Ctrl Pts',(-10.1334604071736,-13.4432175101778,
117.293350973432)) ;
#157910 = CARTESIAN_POINT('Ctrl Pts',(-10.0596565636584,-13.4432175179197,
117.317582014828)) ;
#157911 = CARTESIAN_POINT('Ctrl Pts',(-9.98585272014315,-13.4432175256616,
117.341813056224)) ;
#157912 = CARTESIAN_POINT('Ctrl Pts',(-10.0095205229371,-13.4411780607526,
117.413901364897)) ;
#157913 = CARTESIAN_POINT('Ctrl Pts',(-10.0300438994439,-13.1535366585443,
117.441164670617)) ;
#157914 = CARTESIAN_POINT('Ctrl Pts',(-10.0530434647087,-13.1715786657878,
117.511217635516)) ;
#157915 = CARTESIAN_POINT('Ctrl Pts',(-10.1268473085128,-13.1715786624699,
117.486986595)) ;
#157916 = CARTESIAN_POINT('Ctrl Pts',(-10.2006511523169,-13.1715786591521,
117.462755554485)) ;
#157917 = CARTESIAN_POINT('Ctrl Pts',(-10.1776515870522,-13.1535366519086,
117.392702589586)) ;
#157918 = CARTESIAN_POINT('Ctrl Pts',(-10.1546520217874,-13.1354946446651,
117.322649624687)) ;
#157919 = CARTESIAN_POINT('Ctrl Pts',(-10.0808481779833,-13.1354946479829,
117.346880665203)) ;
#157920 = CARTESIAN_POINT('Ctrl Pts',(-10.0070443341792,-13.1354946513008,
117.371111705719)) ;
#157921 = CARTESIAN_POINT('Ctrl Pts',(-10.0300438994439,-13.1535366585443,
117.441164670617)) ;
#157922 = CARTESIAN_POINT('Ctrl Pts',(-10.0745982760158,-12.8812078446008,
117.541146052817)) ;
#157923 = CARTESIAN_POINT('Ctrl Pts',(-10.0952606474382,-12.9182937200929,
117.604080302277)) ;
#157924 = CARTESIAN_POINT('Ctrl Pts',(-10.1690644906924,-12.9182937216163,
117.579849260086)) ;
#157925 = CARTESIAN_POINT('Ctrl Pts',(-10.2428683339466,-12.9182937231397,
117.555618217895)) ;
#157926 = CARTESIAN_POINT('Ctrl Pts',(-10.2222059625242,-12.8812078476476,
117.492683968435)) ;
#157927 = CARTESIAN_POINT('Ctrl Pts',(-10.2015435911017,-12.8441219721555,
117.429749718974)) ;
#157928 = CARTESIAN_POINT('Ctrl Pts',(-10.1277397478476,-12.8441219706321,
117.453980761165)) ;
#157929 = CARTESIAN_POINT('Ctrl Pts',(-10.0539359045934,-12.8441219691087,
117.478211803356)) ;
#157930 = CARTESIAN_POINT('Ctrl Pts',(-10.0745982760158,-12.8812078446008,
117.541146052817)) ;
#157931 = CARTESIAN_POINT('Ctrl Pts',(-10.1399166575301,-12.6502697095916,
117.704747539768)) ;
#157932 = CARTESIAN_POINT('Ctrl Pts',(-10.1567801601785,-12.7035365652379,
117.756111047861)) ;
#157933 = CARTESIAN_POINT('Ctrl Pts',(-10.2305840029382,-12.7035365674139,
117.731880004164)) ;
#157934 = CARTESIAN_POINT('Ctrl Pts',(-10.304387845698,-12.7035365695899,
117.707648960467)) ;
#157935 = CARTESIAN_POINT('Ctrl Pts',(-10.2875243430495,-12.6502697139436,
117.656285452374)) ;
#157936 = CARTESIAN_POINT('Ctrl Pts',(-10.2706608404011,-12.5970028582972,
117.604921944281)) ;
#157937 = CARTESIAN_POINT('Ctrl Pts',(-10.1968569976414,-12.5970028561212,
117.629152987977)) ;
#157938 = CARTESIAN_POINT('Ctrl Pts',(-10.1230531548816,-12.5970028539452,
117.653384031674)) ;
#157939 = CARTESIAN_POINT('Ctrl Pts',(-10.1399166575301,-12.6502697095916,
117.704747539768)) ;
#157940 = CARTESIAN_POINT('Ctrl Pts',(-10.2222158366404,-12.4736381112203,
117.920071829275)) ;
#157941 = CARTESIAN_POINT('Ctrl Pts',(-10.2340889281916,-12.5393175291298,
117.95623535036)) ;
#157942 = CARTESIAN_POINT('Ctrl Pts',(-10.3078927706903,-12.5393175306857,
117.932004305868)) ;
#157943 = CARTESIAN_POINT('Ctrl Pts',(-10.381696613189,-12.5393175322416,
117.907773261376)) ;
#157944 = CARTESIAN_POINT('Ctrl Pts',(-10.3698235216379,-12.473638114332,
117.871609740292)) ;
#157945 = CARTESIAN_POINT('Ctrl Pts',(-10.3579504300867,-12.4079586964224,
117.835446219207)) ;
#157946 = CARTESIAN_POINT('Ctrl Pts',(-10.284146587588,-12.4079586948666,
117.859677263699)) ;
#157947 = CARTESIAN_POINT('Ctrl Pts',(-10.2103427450893,-12.4079586933107,
117.883908308191)) ;
#157948 = CARTESIAN_POINT('Ctrl Pts',(-10.2222158366404,-12.4736381112203,
117.920071829275)) ;
#157949 = CARTESIAN_POINT('Ctrl Pts',(-10.3174784950143,-12.3636957343507,
118.174552893488)) ;
#157950 = CARTESIAN_POINT('Ctrl Pts',(-10.3234552555865,-12.4371496799271,
118.192757141833)) ;
#157951 = CARTESIAN_POINT('Ctrl Pts',(-10.397259098797,-12.4371496797509,
118.168526099509)) ;
#157952 = CARTESIAN_POINT('Ctrl Pts',(-10.4710629420074,-12.4371496795748,
118.144295057185)) ;
#157953 = CARTESIAN_POINT('Ctrl Pts',(-10.4650861814352,-12.3636957339984,
118.126090808839)) ;
#157954 = CARTESIAN_POINT('Ctrl Pts',(-10.459109420863,-12.290241788422,118.107886560494)) ;
#157955 = CARTESIAN_POINT('Ctrl Pts',(-10.3853055776525,-12.2902417885981,
118.132117602818)) ;
#157956 = CARTESIAN_POINT('Ctrl Pts',(-10.3115017344421,-12.2902417887743,
118.156348645142)) ;
#157957 = CARTESIAN_POINT('Ctrl Pts',(-10.3174784950143,-12.3636957343507,
118.174552893488)) ;
#157958 = CARTESIAN_POINT('Ctrl Pts',(-10.4179636590566,-12.3303161657527,
118.445239950958)) ;
#157959 = CARTESIAN_POINT('Ctrl Pts',(-10.4176647566625,-12.4062080741742,
118.444329542558)) ;
#157960 = CARTESIAN_POINT('Ctrl Pts',(-10.4914686010974,-12.4062080738796,
118.420098503963)) ;
#157961 = CARTESIAN_POINT('Ctrl Pts',(-10.5652724455322,-12.406208073585,
118.395867465368)) ;
#157962 = CARTESIAN_POINT('Ctrl Pts',(-10.5655713479262,-12.3303161651636,
118.396777873769)) ;
#157963 = CARTESIAN_POINT('Ctrl Pts',(-10.5658702503203,-12.2544242567421,
118.39768828217)) ;
#157964 = CARTESIAN_POINT('Ctrl Pts',(-10.4920664058854,-12.2544242570367,
118.421919320765)) ;
#157965 = CARTESIAN_POINT('Ctrl Pts',(-10.4182625614506,-12.2544242573313,
118.446150359359)) ;
#157966 = CARTESIAN_POINT('Ctrl Pts',(-10.4179636590566,-12.3303161657527,
118.445239950958)) ;
#157967 = CARTESIAN_POINT('Ctrl Pts',(-10.5180970410555,-12.3741418831008,
118.71482587813)) ;
#157968 = CARTESIAN_POINT('Ctrl Pts',(-10.511538602985,-12.4470842325009,
118.694849934126)) ;
#157969 = CARTESIAN_POINT('Ctrl Pts',(-10.5853424489065,-12.447084234237,
118.67061890006)) ;
#157970 = CARTESIAN_POINT('Ctrl Pts',(-10.6591462948279,-12.4470842359731,
118.646387865993)) ;
#157971 = CARTESIAN_POINT('Ctrl Pts',(-10.6657047328985,-12.374141886573,
118.666363809997)) ;
#157972 = CARTESIAN_POINT('Ctrl Pts',(-10.672263170969,-12.3011995371729,
118.686339754001)) ;
#157973 = CARTESIAN_POINT('Ctrl Pts',(-10.5984593250475,-12.3011995354367,
118.710570788068)) ;
#157974 = CARTESIAN_POINT('Ctrl Pts',(-10.524655479126,-12.3011995337006,
118.734801822134)) ;
#157975 = CARTESIAN_POINT('Ctrl Pts',(-10.5180970410555,-12.3741418831008,
118.71482587813)) ;
#157976 = CARTESIAN_POINT('Ctrl Pts',(-10.611946558723,-12.4937241519796,
118.965043678186)) ;
#157977 = CARTESIAN_POINT('Ctrl Pts',(-10.5995629169345,-12.5584232360499,
118.927325103705)) ;
#157978 = CARTESIAN_POINT('Ctrl Pts',(-10.6733667647407,-12.5584232440279,
118.903094075379)) ;
#157979 = CARTESIAN_POINT('Ctrl Pts',(-10.7471706125469,-12.558423252006,
118.878863047052)) ;
#157980 = CARTESIAN_POINT('Ctrl Pts',(-10.7595542543354,-12.4937241679357,
118.916581621534)) ;
#157981 = CARTESIAN_POINT('Ctrl Pts',(-10.7719378961239,-12.4290250838654,
118.954300196015)) ;
#157982 = CARTESIAN_POINT('Ctrl Pts',(-10.6981340483176,-12.4290250758873,
118.978531224342)) ;
#157983 = CARTESIAN_POINT('Ctrl Pts',(-10.6243302005114,-12.4290250679093,
119.002762252668)) ;
#157984 = CARTESIAN_POINT('Ctrl Pts',(-10.611946558723,-12.4937241519796,
118.965043678186)) ;
#157985 = CARTESIAN_POINT('Ctrl Pts',(-10.6922395149728,-12.6783961032596,
119.174263610413)) ;
#157986 = CARTESIAN_POINT('Ctrl Pts',(-10.6749630709864,-12.7302945007164,
119.121642350014)) ;
#157987 = CARTESIAN_POINT('Ctrl Pts',(-10.7487669193606,-12.7302945169849,
119.097411323418)) ;
#157988 = CARTESIAN_POINT('Ctrl Pts',(-10.8225707677349,-12.7302945332533,
119.073180296822)) ;
#157989 = CARTESIAN_POINT('Ctrl Pts',(-10.8398472117212,-12.6783961357965,
119.125801557221)) ;
#157990 = CARTESIAN_POINT('Ctrl Pts',(-10.8571236557076,-12.6264977383397,
119.17842281762)) ;
#157991 = CARTESIAN_POINT('Ctrl Pts',(-10.7833198073334,-12.6264977220713,
119.202653844216)) ;
#157992 = CARTESIAN_POINT('Ctrl Pts',(-10.7095159589592,-12.6264977058028,
119.226884870812)) ;
#157993 = CARTESIAN_POINT('Ctrl Pts',(-10.6922395149728,-12.6783961032596,
119.174263610413)) ;
#157994 = CARTESIAN_POINT('Ctrl Pts',(-10.7550368562695,-12.9163766433386,
119.330077430903)) ;
#157995 = CARTESIAN_POINT('Ctrl Pts',(-10.7340845279254,-12.951734042377,
119.266260020007)) ;
#157996 = CARTESIAN_POINT('Ctrl Pts',(-10.8078883759639,-12.9517340693484,
119.242028992389)) ;
#157997 = CARTESIAN_POINT('Ctrl Pts',(-10.8816922240024,-12.9517340963197,
119.21779796477)) ;
#157998 = CARTESIAN_POINT('Ctrl Pts',(-10.9026445523466,-12.9163766972813,
119.281615375666)) ;
#157999 = CARTESIAN_POINT('Ctrl Pts',(-10.9235968806907,-12.8810192982428,
119.345432786561)) ;
#158000 = CARTESIAN_POINT('Ctrl Pts',(-10.8497930326522,-12.8810192712715,
119.36966381418)) ;
#158001 = CARTESIAN_POINT('Ctrl Pts',(-10.7759891846136,-12.8810192443002,
119.393894841798)) ;
#158002 = CARTESIAN_POINT('Ctrl Pts',(-10.7550368562695,-12.9163766433386,
119.330077430903)) ;
#158003 = CARTESIAN_POINT('Ctrl Pts',(-10.7962673301715,-13.1903758945546,
119.420199225543)) ;
#158004 = CARTESIAN_POINT('Ctrl Pts',(-10.7731397430985,-13.2066536724704,
119.3497563277)) ;
#158005 = CARTESIAN_POINT('Ctrl Pts',(-10.8469435893136,-13.206653710727,
119.325525294528)) ;
#158006 = CARTESIAN_POINT('Ctrl Pts',(-10.9207474355287,-13.2066537489837,
119.301294261356)) ;
#158007 = CARTESIAN_POINT('Ctrl Pts',(-10.9438750226017,-13.1903759710679,
119.371737159198)) ;
#158008 = CARTESIAN_POINT('Ctrl Pts',(-10.9670026096747,-13.1740981931521,
119.442180057041)) ;
#158009 = CARTESIAN_POINT('Ctrl Pts',(-10.8931987634596,-13.1740981548955,
119.466411090213)) ;
#158010 = CARTESIAN_POINT('Ctrl Pts',(-10.8193949172445,-13.1740981166388,
119.490642123386)) ;
#158011 = CARTESIAN_POINT('Ctrl Pts',(-10.7962673301715,-13.1903758945546,
119.420199225543)) ;
#158012 = CARTESIAN_POINT('Ctrl Pts',(-10.8137492360295,-13.481432819081,
119.437894714578)) ;
#158013 = CARTESIAN_POINT('Ctrl Pts',(-10.7901032169059,-13.4774126955136,
119.365872756543)) ;
#158014 = CARTESIAN_POINT('Ctrl Pts',(-10.8639070596865,-13.4774127443564,
119.34164171291)) ;
#158015 = CARTESIAN_POINT('Ctrl Pts',(-10.9377109024671,-13.4774127931991,
119.317410669277)) ;
#158016 = CARTESIAN_POINT('Ctrl Pts',(-10.9613569215908,-13.4814329167664,
119.389432627311)) ;
#158017 = CARTESIAN_POINT('Ctrl Pts',(-10.9850029407144,-13.4854530403338,
119.461454585346)) ;
#158018 = CARTESIAN_POINT('Ctrl Pts',(-10.9111990979337,-13.4854529914911,
119.48568562898)) ;
#158019 = CARTESIAN_POINT('Ctrl Pts',(-10.8373952551531,-13.4854529426483,
119.509916672613)) ;
#158020 = CARTESIAN_POINT('Ctrl Pts',(-10.8137492360295,-13.481432819081,
119.437894714578)) ;
#158021 = CARTESIAN_POINT('Ctrl Pts',(-10.8068277964098,-13.7673558416161,
119.38132985396)) ;
#158022 = CARTESIAN_POINT('Ctrl Pts',(-10.7843650610985,-13.7433670881258,
119.312911987666)) ;
#158023 = CARTESIAN_POINT('Ctrl Pts',(-10.8581688989208,-13.7433671429839,
119.288680928931)) ;
#158024 = CARTESIAN_POINT('Ctrl Pts',(-10.9319727367432,-13.7433671978421,
119.264449870195)) ;
#158025 = CARTESIAN_POINT('Ctrl Pts',(-10.9544354720545,-13.7673559513324,
119.332867736489)) ;
#158026 = CARTESIAN_POINT('Ctrl Pts',(-10.9768982073658,-13.7913447048227,
119.401285602783)) ;
#158027 = CARTESIAN_POINT('Ctrl Pts',(-10.9030943695434,-13.7913446499646,
119.425516661519)) ;
#158028 = CARTESIAN_POINT('Ctrl Pts',(-10.8292905317211,-13.7913445951064,
119.449747720254)) ;
#158029 = CARTESIAN_POINT('Ctrl Pts',(-10.8068277964098,-13.7673558416161,
119.38132985396)) ;
#158030 = CARTESIAN_POINT('Ctrl Pts',(-10.7770884508321,-14.0271101613543,
119.255429248926)) ;
#158031 = CARTESIAN_POINT('Ctrl Pts',(-10.7574005437931,-13.9849513065541,
119.195463061969)) ;
#158032 = CARTESIAN_POINT('Ctrl Pts',(-10.8312043760563,-13.9849513605373,
119.171231986301)) ;
#158033 = CARTESIAN_POINT('Ctrl Pts',(-10.9050082083194,-13.9849514145205,
119.147000910633)) ;
#158034 = CARTESIAN_POINT('Ctrl Pts',(-10.9246961153584,-14.0271102693206,
119.206967097591)) ;
#158035 = CARTESIAN_POINT('Ctrl Pts',(-10.9443840223974,-14.0692691241208,
119.266933284548)) ;
#158036 = CARTESIAN_POINT('Ctrl Pts',(-10.8705801901342,-14.0692690701376,
119.291164360216)) ;
#158037 = CARTESIAN_POINT('Ctrl Pts',(-10.7967763578711,-14.0692690161544,
119.315395435884)) ;
#158038 = CARTESIAN_POINT('Ctrl Pts',(-10.7770884508321,-14.0271101613543,
119.255429248926)) ;
#158039 = CARTESIAN_POINT('Ctrl Pts',(-10.7271574214564,-14.2445027860115,
119.067879150203)) ;
#158040 = CARTESIAN_POINT('Ctrl Pts',(-10.7116609736876,-14.187105106811,
119.02067947205)) ;
#158041 = CARTESIAN_POINT('Ctrl Pts',(-10.785464799976,-14.1871051547693,
118.996448378184)) ;
#158042 = CARTESIAN_POINT('Ctrl Pts',(-10.8592686262643,-14.1871052027276,
118.972217284318)) ;
#158043 = CARTESIAN_POINT('Ctrl Pts',(-10.8747650740332,-14.244502881928,
119.019416962471)) ;
#158044 = CARTESIAN_POINT('Ctrl Pts',(-10.890261521802,-14.3019005611285,
119.066616640624)) ;
#158045 = CARTESIAN_POINT('Ctrl Pts',(-10.8164576955137,-14.3019005131702,
119.09084773449)) ;
#158046 = CARTESIAN_POINT('Ctrl Pts',(-10.7426538692253,-14.3019004652119,
119.115078828355)) ;
#158047 = CARTESIAN_POINT('Ctrl Pts',(-10.7271574214564,-14.2445027860115,
119.067879150203)) ;
#158048 = CARTESIAN_POINT('Ctrl Pts',(-10.6612093802085,-14.4028029107363,
118.831466877353)) ;
#158049 = CARTESIAN_POINT('Ctrl Pts',(-10.651030199486,-14.3342697574314,
118.800462736843)) ;
#158050 = CARTESIAN_POINT('Ctrl Pts',(-10.7248340200921,-14.3342697924112,
118.77623162567)) ;
#158051 = CARTESIAN_POINT('Ctrl Pts',(-10.7986378406982,-14.334269827391,
118.752000514496)) ;
#158052 = CARTESIAN_POINT('Ctrl Pts',(-10.8088170214206,-14.402802980696,
118.783004655006)) ;
#158053 = CARTESIAN_POINT('Ctrl Pts',(-10.8189962021431,-14.471336134001,
118.814008795516)) ;
#158054 = CARTESIAN_POINT('Ctrl Pts',(-10.7451923815371,-14.4713360990211,
118.838239906689)) ;
#158055 = CARTESIAN_POINT('Ctrl Pts',(-10.671388560931,-14.4713360640413,
118.862471017863)) ;
#158056 = CARTESIAN_POINT('Ctrl Pts',(-10.6612093802085,-14.4028029107363,
118.831466877353)) ;
#158057 = CARTESIAN_POINT('Ctrl Pts',(-10.5852730928227,-14.4900131921161,
118.564801583323)) ;
#158058 = CARTESIAN_POINT('Ctrl Pts',(-10.5811127826548,-14.4152919696491,
118.552129951499)) ;
#158059 = CARTESIAN_POINT('Ctrl Pts',(-10.6549165993077,-14.4152919849729,
118.527898828285)) ;
#158060 = CARTESIAN_POINT('Ctrl Pts',(-10.7287204159607,-14.4152920002968,
118.503667705072)) ;
#158061 = CARTESIAN_POINT('Ctrl Pts',(-10.7328807261286,-14.4900132227638,
118.516339336896)) ;
#158062 = CARTESIAN_POINT('Ctrl Pts',(-10.7370410362966,-14.5647344452309,
118.52901096872)) ;
#158063 = CARTESIAN_POINT('Ctrl Pts',(-10.6632372196436,-14.5647344299071,
118.553242091933)) ;
#158064 = CARTESIAN_POINT('Ctrl Pts',(-10.5894334029907,-14.5647344145832,
118.577473215147)) ;
#158065 = CARTESIAN_POINT('Ctrl Pts',(-10.5852730928227,-14.4900131921161,
118.564801583323)) ;
#158066 = CARTESIAN_POINT('Ctrl Pts',(-10.5049910429359,-14.5009049303826,
118.284799184651)) ;
#158067 = CARTESIAN_POINT('Ctrl Pts',(-10.5071637236144,-14.4253144760394,
118.29141682124)) ;
#158068 = CARTESIAN_POINT('Ctrl Pts',(-10.5809675380395,-14.4253144674804,
118.267185691241)) ;
#158069 = CARTESIAN_POINT('Ctrl Pts',(-10.6547713524647,-14.4253144589214,
118.242954561242)) ;
#158070 = CARTESIAN_POINT('Ctrl Pts',(-10.6525986717862,-14.5009049132646,
118.236336924653)) ;
#158071 = CARTESIAN_POINT('Ctrl Pts',(-10.6504259911078,-14.5764953676079,
118.229719288063)) ;
#158072 = CARTESIAN_POINT('Ctrl Pts',(-10.5766221766826,-14.5764953761669,
118.253950418063)) ;
#158073 = CARTESIAN_POINT('Ctrl Pts',(-10.5028183622575,-14.5764953847259,
118.278181548062)) ;
#158074 = CARTESIAN_POINT('Ctrl Pts',(-10.5049910429359,-14.5009049303826,
118.284799184651)) ;
#158075 = CARTESIAN_POINT('Ctrl Pts',(-10.4268806844919,-14.4337694493022,
118.011321719883)) ;
#158076 = CARTESIAN_POINT('Ctrl Pts',(-10.4352458048887,-14.3627554397417,
118.036800528817)) ;
#158077 = CARTESIAN_POINT('Ctrl Pts',(-10.5090496194382,-14.3627554046461,
118.012569399197)) ;
#158078 = CARTESIAN_POINT('Ctrl Pts',(-10.5828534339877,-14.3627553695504,
117.988338269576)) ;
#158079 = CARTESIAN_POINT('Ctrl Pts',(-10.5744883135909,-14.4337693791109,
117.962859460643)) ;
#158080 = CARTESIAN_POINT('Ctrl Pts',(-10.566123193194,-14.5047833886713,
117.937380651709)) ;
#158081 = CARTESIAN_POINT('Ctrl Pts',(-10.4923193786445,-14.504783423767,
117.961611781329)) ;
#158082 = CARTESIAN_POINT('Ctrl Pts',(-10.418515564095,-14.5047834588626,
117.98584291095)) ;
#158083 = CARTESIAN_POINT('Ctrl Pts',(-10.4268806844919,-14.4337694493022,
118.011321719883)) ;
#158084 = CARTESIAN_POINT('Ctrl Pts',(-10.3576955154029,-14.2939322119372,
117.765123850201)) ;
#158085 = CARTESIAN_POINT('Ctrl Pts',(-10.3716370706473,-14.232577073239,
117.807587580005)) ;
#158086 = CARTESIAN_POINT('Ctrl Pts',(-10.4454408881443,-14.2325770123608,
117.783356459362)) ;
#158087 = CARTESIAN_POINT('Ctrl Pts',(-10.5192447056414,-14.2325769514826,
117.759125338719)) ;
#158088 = CARTESIAN_POINT('Ctrl Pts',(-10.505303150397,-14.2939320901808,
117.716661608916)) ;
#158089 = CARTESIAN_POINT('Ctrl Pts',(-10.4913615951525,-14.3552872288789,
117.674197879113)) ;
#158090 = CARTESIAN_POINT('Ctrl Pts',(-10.4175577776555,-14.3552872897571,
117.698428999756)) ;
#158091 = CARTESIAN_POINT('Ctrl Pts',(-10.3437539601585,-14.3552873506354,
117.722660120398)) ;
#158092 = CARTESIAN_POINT('Ctrl Pts',(-10.3576955154029,-14.2939322119372,
117.765123850201)) ;
#158093 = CARTESIAN_POINT('Ctrl Pts',(-10.3029320432203,-14.0911613446941,
117.562827612356)) ;
#158094 = CARTESIAN_POINT('Ctrl Pts',(-10.3214519189372,-14.0438726639187,
117.619236167666)) ;
#158095 = CARTESIAN_POINT('Ctrl Pts',(-10.3952557418565,-14.0438725807802,
117.595005063539)) ;
#158096 = CARTESIAN_POINT('Ctrl Pts',(-10.4690595647757,-14.0438724976418,
117.570773959411)) ;
#158097 = CARTESIAN_POINT('Ctrl Pts',(-10.4505396890587,-14.0911611784172,
117.5143654041)) ;
#158098 = CARTESIAN_POINT('Ctrl Pts',(-10.4320198133418,-14.1384498591927,
117.45795684879)) ;
#158099 = CARTESIAN_POINT('Ctrl Pts',(-10.3582159904226,-14.1384499423311,
117.482187952917)) ;
#158100 = CARTESIAN_POINT('Ctrl Pts',(-10.2844121675033,-14.1384500254695,
117.506419057045)) ;
#158101 = CARTESIAN_POINT('Ctrl Pts',(-10.3029320432203,-14.0911613446941,
117.562827612356)) ;
#158102 = CARTESIAN_POINT('Ctrl Pts',(-10.2673499177128,-13.8412394795533,
117.419099337292)) ;
#158103 = CARTESIAN_POINT('Ctrl Pts',(-10.289112664957,-13.8113299936379,
117.485385156072)) ;
#158104 = CARTESIAN_POINT('Ctrl Pts',(-10.3629164952868,-13.8113298944944,
117.461154074516)) ;
#158105 = CARTESIAN_POINT('Ctrl Pts',(-10.4367203256165,-13.8113297953509,
117.436922992959)) ;
#158106 = CARTESIAN_POINT('Ctrl Pts',(-10.4149575783723,-13.8412392812663,
117.370637174179)) ;
#158107 = CARTESIAN_POINT('Ctrl Pts',(-10.393194831128,-13.8711487671817,
117.304351355399)) ;
#158108 = CARTESIAN_POINT('Ctrl Pts',(-10.3193910007983,-13.8711488663252,
117.328582436956)) ;
#158109 = CARTESIAN_POINT('Ctrl Pts',(-10.2455871704685,-13.8711489654687,
117.352813518512)) ;
#158110 = CARTESIAN_POINT('Ctrl Pts',(-10.2673499177128,-13.8412394795533,
117.419099337292)) ;
#158111 = CARTESIAN_POINT('Ctrl Pts',(-10.254056072628,-13.5592605313859,
117.343020397243)) ;
#158112 = CARTESIAN_POINT('Ctrl Pts',(-10.2775155822903,-13.5489932748768,
117.414474280592)) ;
#158113 = CARTESIAN_POINT('Ctrl Pts',(-10.3513194213136,-13.5489931673576,
117.390243225514)) ;
#158114 = CARTESIAN_POINT('Ctrl Pts',(-10.4251232603369,-13.5489930598384,
117.366012170437)) ;
#158115 = CARTESIAN_POINT('Ctrl Pts',(-10.4016637506746,-13.5592603163474,
117.294558287088)) ;
#158116 = CARTESIAN_POINT('Ctrl Pts',(-10.3782042410124,-13.5695275728564,
117.223104403739)) ;
#158117 = CARTESIAN_POINT('Ctrl Pts',(-10.3044004019891,-13.5695276803756,
117.247335458816)) ;
#158118 = CARTESIAN_POINT('Ctrl Pts',(-10.2305965629658,-13.5695277878949,
117.271566513894)) ;
#158119 = CARTESIAN_POINT('Ctrl Pts',(-10.254056072628,-13.5592605313859,
117.343020397243)) ;
#158120 = CARTESIAN_POINT('Ctrl Pts',(-10.2648180246204,-13.2696223387077,
117.34052655831)) ;
#158121 = CARTESIAN_POINT('Ctrl Pts',(-10.2882906220838,-13.279561631404,
117.412020304983)) ;
#158122 = CARTESIAN_POINT('Ctrl Pts',(-10.3620944701325,-13.2795615243136,
117.387789277396)) ;
#158123 = CARTESIAN_POINT('Ctrl Pts',(-10.4358983181812,-13.2795614172232,
117.363558249809)) ;
#158124 = CARTESIAN_POINT('Ctrl Pts',(-10.4124257207178,-13.2696221245269,
117.292064503135)) ;
#158125 = CARTESIAN_POINT('Ctrl Pts',(-10.3889531232543,-13.2596828318306,
117.220570756461)) ;
#158126 = CARTESIAN_POINT('Ctrl Pts',(-10.3151492752056,-13.259682938921,
117.244801784049)) ;
#158127 = CARTESIAN_POINT('Ctrl Pts',(-10.2413454271569,-13.2596830460114,
117.269032811636)) ;
#158128 = CARTESIAN_POINT('Ctrl Pts',(-10.2648180246204,-13.2696223387077,
117.34052655831)) ;
#158129 = CARTESIAN_POINT('Ctrl Pts',(-10.2997358790123,-12.9883139496615,
117.411316976137)) ;
#158130 = CARTESIAN_POINT('Ctrl Pts',(-10.321541507602,-13.0179078909162,
117.477733404555)) ;
#158131 = CARTESIAN_POINT('Ctrl Pts',(-10.3953453642065,-13.0179077930937,
117.453502403027)) ;
#158132 = CARTESIAN_POINT('Ctrl Pts',(-10.469149220811,-13.0179076952712,
117.4292714015)) ;
#158133 = CARTESIAN_POINT('Ctrl Pts',(-10.4473435922213,-12.9883137540165,
117.362854973081)) ;
#158134 = CARTESIAN_POINT('Ctrl Pts',(-10.4255379636317,-12.9587198127618,
117.296438544663)) ;
#158135 = CARTESIAN_POINT('Ctrl Pts',(-10.3517341070272,-12.9587199105843,
117.32066954619)) ;
#158136 = CARTESIAN_POINT('Ctrl Pts',(-10.2779302504227,-12.9587200084068,
117.344900547718)) ;
#158137 = CARTESIAN_POINT('Ctrl Pts',(-10.2997358790123,-12.9883139496615,
117.411316976137)) ;
#158138 = CARTESIAN_POINT('Ctrl Pts',(-10.3569669367904,-12.7386910562247,
117.550180832731)) ;
#158139 = CARTESIAN_POINT('Ctrl Pts',(-10.3755429712197,-12.7857570655332,
117.606760438379)) ;
#158140 = CARTESIAN_POINT('Ctrl Pts',(-10.4493468349472,-12.7857569845681,
117.582529458547)) ;
#158141 = CARTESIAN_POINT('Ctrl Pts',(-10.5231506986747,-12.785756903603,
117.558298478715)) ;
#158142 = CARTESIAN_POINT('Ctrl Pts',(-10.5045746642454,-12.7386908942945,
117.501718873067)) ;
#158143 = CARTESIAN_POINT('Ctrl Pts',(-10.4859986298161,-12.691624884986,
117.445139267419)) ;
#158144 = CARTESIAN_POINT('Ctrl Pts',(-10.4121947660886,-12.6916249659511,
117.469370247251)) ;
#158145 = CARTESIAN_POINT('Ctrl Pts',(-10.3383909023611,-12.6916250469162,
117.493601227083)) ;
#158146 = CARTESIAN_POINT('Ctrl Pts',(-10.3569669367904,-12.7386910562247,
117.550180832731)) ;
#158147 = CARTESIAN_POINT('Ctrl Pts',(-10.4331834431151,-12.5375785963018,
117.746852091262)) ;
#158148 = CARTESIAN_POINT('Ctrl Pts',(-10.4472000358455,-12.5987561417494,
117.789544373086)) ;
#158149 = CARTESIAN_POINT('Ctrl Pts',(-10.521003904621,-12.5987560832211,
117.76531340863)) ;
#158150 = CARTESIAN_POINT('Ctrl Pts',(-10.5948077733966,-12.5987560246928,
117.741082444173)) ;
#158151 = CARTESIAN_POINT('Ctrl Pts',(-10.5807911806663,-12.5375784792451,
117.698390162349)) ;
#158152 = CARTESIAN_POINT('Ctrl Pts',(-10.566774587936,-12.4764009337975,
117.655697880525)) ;
#158153 = CARTESIAN_POINT('Ctrl Pts',(-10.4929707191604,-12.4764009923258,
117.679928844982)) ;
#158154 = CARTESIAN_POINT('Ctrl Pts',(-10.4191668503848,-12.4764010508541,
117.704159809438)) ;
#158155 = CARTESIAN_POINT('Ctrl Pts',(-10.4331834431151,-12.5375785963018,
117.746852091262)) ;
#158156 = CARTESIAN_POINT('Ctrl Pts',(-10.5236752561247,-12.3995778757378,
117.98701193378)) ;
#158157 = CARTESIAN_POINT('Ctrl Pts',(-10.5321287714972,-12.4704821067912,
118.01275997948)) ;
#158158 = CARTESIAN_POINT('Ctrl Pts',(-10.6059326428365,-12.4704820736808,
117.988529022832)) ;
#158159 = CARTESIAN_POINT('Ctrl Pts',(-10.6797365141757,-12.4704820405704,
117.964298066184)) ;
#158160 = CARTESIAN_POINT('Ctrl Pts',(-10.6712829988032,-12.399577809517,
117.938550020484)) ;
#158161 = CARTESIAN_POINT('Ctrl Pts',(-10.6628294834308,-12.3286735784636,
117.912801974784)) ;
#158162 = CARTESIAN_POINT('Ctrl Pts',(-10.5890256120915,-12.328673611574,
117.937032931432)) ;
#158163 = CARTESIAN_POINT('Ctrl Pts',(-10.5152217407523,-12.3286736446844,
117.96126388808)) ;
#158164 = CARTESIAN_POINT('Ctrl Pts',(-10.5236752561247,-12.3995778757378,
117.98701193378)) ;
#158165 = CARTESIAN_POINT('Ctrl Pts',(-10.6227835579732,-12.3345174279643,
118.253393687995)) ;
#158166 = CARTESIAN_POINT('Ctrl Pts',(-10.6250645346301,-12.4100708039264,
118.26034117659)) ;
#158167 = CARTESIAN_POINT('Ctrl Pts',(-10.6988684058985,-12.4100707963706,
118.236110219726)) ;
#158168 = CARTESIAN_POINT('Ctrl Pts',(-10.7726722771668,-12.4100707888147,
118.211879262862)) ;
#158169 = CARTESIAN_POINT('Ctrl Pts',(-10.7703913005099,-12.3345174128525,
118.204931774267)) ;
#158170 = CARTESIAN_POINT('Ctrl Pts',(-10.7681103238529,-12.2589640368904,
118.197984285672)) ;
#158171 = CARTESIAN_POINT('Ctrl Pts',(-10.6943064525846,-12.2589640444462,
118.222215242536)) ;
#158172 = CARTESIAN_POINT('Ctrl Pts',(-10.6205025813162,-12.2589640520021,
118.2464461994)) ;
#158173 = CARTESIAN_POINT('Ctrl Pts',(-10.6227835579732,-12.3345174279643,
118.253393687995)) ;
#158174 = CARTESIAN_POINT('Ctrl Pts',(-10.7239238622889,-12.3471393395654,
118.526024465767)) ;
#158175 = CARTESIAN_POINT('Ctrl Pts',(-10.7198798307175,-12.4219252940087,
118.513706999714)) ;
#158176 = CARTESIAN_POINT('Ctrl Pts',(-10.7936836996938,-12.4219253092695,
118.489476035868)) ;
#158177 = CARTESIAN_POINT('Ctrl Pts',(-10.86748756867,-12.4219253245303,118.465245072023)) ;
#158178 = CARTESIAN_POINT('Ctrl Pts',(-10.8715316002415,-12.347139370087,
118.477562538076)) ;
#158179 = CARTESIAN_POINT('Ctrl Pts',(-10.8755756318129,-12.2723534156437,
118.48988000413)) ;
#158180 = CARTESIAN_POINT('Ctrl Pts',(-10.8017717628366,-12.272353400383,
118.514110967975)) ;
#158181 = CARTESIAN_POINT('Ctrl Pts',(-10.7279678938604,-12.2723533851222,
118.538341931821)) ;
#158182 = CARTESIAN_POINT('Ctrl Pts',(-10.7239238622889,-12.3471393395654,
118.526024465767)) ;
#158183 = CARTESIAN_POINT('Ctrl Pts',(-10.8207516399519,-12.4360428670471,
118.785542422515)) ;
#158184 = CARTESIAN_POINT('Ctrl Pts',(-10.8106736759998,-12.5047344738789,
118.754846571873)) ;
#158185 = CARTESIAN_POINT('Ctrl Pts',(-10.8844775408933,-12.5047345075886,
118.730615595592)) ;
#158186 = CARTESIAN_POINT('Ctrl Pts',(-10.9582814057869,-12.5047345412984,
118.706384619311)) ;
#158187 = CARTESIAN_POINT('Ctrl Pts',(-10.9683593697391,-12.4360429344666,
118.737080469954)) ;
#158188 = CARTESIAN_POINT('Ctrl Pts',(-10.9784373336912,-12.3673513276347,
118.767776320597)) ;
#158189 = CARTESIAN_POINT('Ctrl Pts',(-10.9046334687976,-12.367351293925,
118.792007296877)) ;
#158190 = CARTESIAN_POINT('Ctrl Pts',(-10.830829603904,-12.3673512602152,
118.816238273158)) ;
#158191 = CARTESIAN_POINT('Ctrl Pts',(-10.8207516399519,-12.4360428670471,
118.785542422515)) ;
#158192 = CARTESIAN_POINT('Ctrl Pts',(-10.9075644967453,-12.5962612233629,
119.014358156929)) ;
#158193 = CARTESIAN_POINT('Ctrl Pts',(-10.892146670105,-12.6538708074165,
118.967397945946)) ;
#158194 = CARTESIAN_POINT('Ctrl Pts',(-10.965950529285,-12.6538708522854,
118.943166952263)) ;
#158195 = CARTESIAN_POINT('Ctrl Pts',(-11.039754388465,-12.6538708971542,
118.918935958579)) ;
#158196 = CARTESIAN_POINT('Ctrl Pts',(-11.0551722151052,-12.5962613131006,
118.965896169562)) ;
#158197 = CARTESIAN_POINT('Ctrl Pts',(-11.0705900417455,-12.538651729047,
119.012856380545)) ;
#158198 = CARTESIAN_POINT('Ctrl Pts',(-10.9967861825655,-12.5386516841781,
119.037087374229)) ;
#158199 = CARTESIAN_POINT('Ctrl Pts',(-10.9229823233856,-12.5386516393093,
119.061318367912)) ;
#158200 = CARTESIAN_POINT('Ctrl Pts',(-10.9075644967453,-12.5962612233629,
119.014358156929)) ;
#158201 = CARTESIAN_POINT('Ctrl Pts',(-10.9778413211601,-12.8139558923281,
119.19307998567)) ;
#158202 = CARTESIAN_POINT('Ctrl Pts',(-10.9582245183943,-12.8564528958473,
119.133330370774)) ;
#158203 = CARTESIAN_POINT('Ctrl Pts',(-11.0320283721088,-12.8564529465473,
119.109099360444)) ;
#158204 = CARTESIAN_POINT('Ctrl Pts',(-11.1058322258233,-12.8564529972473,
119.084868350113)) ;
#158205 = CARTESIAN_POINT('Ctrl Pts',(-11.125449028589,-12.8139559937281,
119.144617965009)) ;
#158206 = CARTESIAN_POINT('Ctrl Pts',(-11.1450658313548,-12.7714589902089,
119.204367579904)) ;
#158207 = CARTESIAN_POINT('Ctrl Pts',(-11.0712619776403,-12.7714589395089,
119.228598590235)) ;
#158208 = CARTESIAN_POINT('Ctrl Pts',(-10.9974581239259,-12.7714588888089,
119.252829600565)) ;
#158209 = CARTESIAN_POINT('Ctrl Pts',(-10.9778413211601,-12.8139558923281,
119.19307998567)) ;
#158210 = CARTESIAN_POINT('Ctrl Pts',(-11.0282836106079,-13.0756188660845,
119.311240887642)) ;
#158211 = CARTESIAN_POINT('Ctrl Pts',(-11.0058492656937,-13.0999108300579,
119.242909493803)) ;
#158212 = CARTESIAN_POINT('Ctrl Pts',(-11.0796531139265,-13.0999108795098,
119.218678466776)) ;
#158213 = CARTESIAN_POINT('Ctrl Pts',(-11.1534569621592,-13.0999109289618,
119.194447439749)) ;
#158214 = CARTESIAN_POINT('Ctrl Pts',(-11.1758913070734,-13.0756189649884,
119.262778833588)) ;
#158215 = CARTESIAN_POINT('Ctrl Pts',(-11.1983256519876,-13.051327001015,
119.331110227428)) ;
#158216 = CARTESIAN_POINT('Ctrl Pts',(-11.1245218037548,-13.0513269515631,
119.355341254455)) ;
#158217 = CARTESIAN_POINT('Ctrl Pts',(-11.0507179555221,-13.0513269021111,
119.379572281481)) ;
#158218 = CARTESIAN_POINT('Ctrl Pts',(-11.0282836106079,-13.0756188660845,
119.311240887642)) ;
#158219 = CARTESIAN_POINT('Ctrl Pts',(-11.0555791922085,-13.3624251132735,
119.358838014228)) ;
#158220 = CARTESIAN_POINT('Ctrl Pts',(-11.0319403546085,-13.3667285784785,
119.286837929828)) ;
#158221 = CARTESIAN_POINT('Ctrl Pts',(-11.1057441984597,-13.3667286208057,
119.262606889456)) ;
#158222 = CARTESIAN_POINT('Ctrl Pts',(-11.1795480423108,-13.3667286631328,
119.238375849083)) ;
#158223 = CARTESIAN_POINT('Ctrl Pts',(-11.2031868799108,-13.3624251979278,
119.310375933482)) ;
#158224 = CARTESIAN_POINT('Ctrl Pts',(-11.2268257175108,-13.3581217327227,
119.382376017881)) ;
#158225 = CARTESIAN_POINT('Ctrl Pts',(-11.1530218736597,-13.3581216903956,
119.406607058254)) ;
#158226 = CARTESIAN_POINT('Ctrl Pts',(-11.0792180298085,-13.3581216480684,
119.430838098627)) ;
#158227 = CARTESIAN_POINT('Ctrl Pts',(-11.0555791922085,-13.3624251132735,
119.358838014228)) ;
#158228 = CARTESIAN_POINT('Ctrl Pts',(-11.0586048593759,-13.651982180129,
119.332672404455)) ;
#158229 = CARTESIAN_POINT('Ctrl Pts',(-11.0354511320318,-13.6360746304586,
119.262149887471)) ;
#158230 = CARTESIAN_POINT('Ctrl Pts',(-11.1092549728687,-13.6360746639262,
119.237918837918)) ;
#158231 = CARTESIAN_POINT('Ctrl Pts',(-11.1830588137057,-13.6360746973937,
119.213687788364)) ;
#158232 = CARTESIAN_POINT('Ctrl Pts',(-11.2062125410498,-13.651982247064,
119.284210305348)) ;
#158233 = CARTESIAN_POINT('Ctrl Pts',(-11.2293662683938,-13.6678897967344,
119.354732822331)) ;
#158234 = CARTESIAN_POINT('Ctrl Pts',(-11.1555624275569,-13.6678897632668,
119.378963871885)) ;
#158235 = CARTESIAN_POINT('Ctrl Pts',(-11.0817585867199,-13.6678897297993,
119.403194921438)) ;
#158236 = CARTESIAN_POINT('Ctrl Pts',(-11.0586048593759,-13.651982180129,
119.332672404455)) ;
#158237 = CARTESIAN_POINT('Ctrl Pts',(-11.0376843527776,-13.9268736432231,
119.23328044909)) ;
#158238 = CARTESIAN_POINT('Ctrl Pts',(-11.0166942808238,-13.8917477253801,
119.169348077124)) ;
#158239 = CARTESIAN_POINT('Ctrl Pts',(-11.0904981204884,-13.8917477464933,
119.145117023999)) ;
#158240 = CARTESIAN_POINT('Ctrl Pts',(-11.1643019601529,-13.8917477676065,
119.120885970875)) ;
#158241 = CARTESIAN_POINT('Ctrl Pts',(-11.1852920321068,-13.9268736854496,
119.184818342842)) ;
#158242 = CARTESIAN_POINT('Ctrl Pts',(-11.2062821040606,-13.9619996032926,
119.248750714809)) ;
#158243 = CARTESIAN_POINT('Ctrl Pts',(-11.132478264396,-13.9619995821794,
119.272981767933)) ;
#158244 = CARTESIAN_POINT('Ctrl Pts',(-11.0586744247314,-13.9619995610662,
119.297212821057)) ;
#158245 = CARTESIAN_POINT('Ctrl Pts',(-11.0376843527776,-13.9268736432231,
119.23328044909)) ;
#158246 = CARTESIAN_POINT('Ctrl Pts',(-10.9956210330096,-14.1624927779437,
119.069898286994)) ;
#158247 = CARTESIAN_POINT('Ctrl Pts',(-10.9782661256245,-14.1108622061885,
119.017038039656)) ;
#158248 = CARTESIAN_POINT('Ctrl Pts',(-11.052069965002,-14.1108622190925,
118.992806985658)) ;
#158249 = CARTESIAN_POINT('Ctrl Pts',(-11.1258738043794,-14.1108622319965,
118.968575931659)) ;
#158250 = CARTESIAN_POINT('Ctrl Pts',(-11.1432287117646,-14.1624928037518,
119.021436178997)) ;
#158251 = CARTESIAN_POINT('Ctrl Pts',(-11.1605836191497,-14.214123375507,
119.074296426334)) ;
#158252 = CARTESIAN_POINT('Ctrl Pts',(-11.0867797797722,-14.214123362603,
119.098527480333)) ;
#158253 = CARTESIAN_POINT('Ctrl Pts',(-11.0129759403947,-14.214123349699,
119.122758534332)) ;
#158254 = CARTESIAN_POINT('Ctrl Pts',(-10.9956210330096,-14.1624927779437,
119.069898286994)) ;
#158255 = CARTESIAN_POINT('Ctrl Pts',(-10.9354933314548,-14.3467872124729,
118.851183898762)) ;
#158256 = CARTESIAN_POINT('Ctrl Pts',(-10.9230467944216,-14.28220994504,118.813273755401)) ;
#158257 = CARTESIAN_POINT('Ctrl Pts',(-10.9968506349554,-14.2822099499131,
118.789042704924)) ;
#158258 = CARTESIAN_POINT('Ctrl Pts',(-11.0706544754893,-14.2822099547862,
118.764811654447)) ;
#158259 = CARTESIAN_POINT('Ctrl Pts',(-11.0831010125224,-14.346787222219,
118.802721797808)) ;
#158260 = CARTESIAN_POINT('Ctrl Pts',(-11.0955475495556,-14.4113644896518,
118.840631941169)) ;
#158261 = CARTESIAN_POINT('Ctrl Pts',(-11.0217437090218,-14.4113644847787,
118.864862991646)) ;
#158262 = CARTESIAN_POINT('Ctrl Pts',(-10.9479398684879,-14.4113644799057,
118.889094042122)) ;
#158263 = CARTESIAN_POINT('Ctrl Pts',(-10.9354933314548,-14.3467872124729,
118.851183898762)) ;
#158264 = CARTESIAN_POINT('Ctrl Pts',(-10.8629481065443,-14.4636106389172,
118.594821165369)) ;
#158265 = CARTESIAN_POINT('Ctrl Pts',(-10.8562810213142,-14.3907789878482,
118.574514299585)) ;
#158266 = CARTESIAN_POINT('Ctrl Pts',(-10.930084863199,-14.3907789888133,
118.550283253223)) ;
#158267 = CARTESIAN_POINT('Ctrl Pts',(-11.0038887050839,-14.3907789897784,
118.526052206862)) ;
#158268 = CARTESIAN_POINT('Ctrl Pts',(-11.0105557903141,-14.4636106408474,
118.546359072646)) ;
#158269 = CARTESIAN_POINT('Ctrl Pts',(-11.0172228755442,-14.5364422919164,
118.566665938431)) ;
#158270 = CARTESIAN_POINT('Ctrl Pts',(-10.9434190336593,-14.5364422909513,
118.590896984792)) ;
#158271 = CARTESIAN_POINT('Ctrl Pts',(-10.8696151917745,-14.5364422899862,
118.615128031154)) ;
#158272 = CARTESIAN_POINT('Ctrl Pts',(-10.8629481065443,-14.4636106389172,
118.594821165369)) ;
#158273 = CARTESIAN_POINT('Ctrl Pts',(-10.7836225816458,-14.505904926533,
118.317753204467)) ;
#158274 = CARTESIAN_POINT('Ctrl Pts',(-10.7832182997654,-14.4300107624531,
118.316521827099)) ;
#158275 = CARTESIAN_POINT('Ctrl Pts',(-10.8570221430318,-14.430010762108,
118.292290784945)) ;
#158276 = CARTESIAN_POINT('Ctrl Pts',(-10.9308259862981,-14.430010761763,
118.268059742791)) ;
#158277 = CARTESIAN_POINT('Ctrl Pts',(-10.9312302681785,-14.5059049258428,
118.26929112016)) ;
#158278 = CARTESIAN_POINT('Ctrl Pts',(-10.9316345500589,-14.5817990899227,
118.270522497528)) ;
#158279 = CARTESIAN_POINT('Ctrl Pts',(-10.8578307067925,-14.5817990902678,
118.294753539682)) ;
#158280 = CARTESIAN_POINT('Ctrl Pts',(-10.7840268635262,-14.5817990906128,
118.318984581835)) ;
#158281 = CARTESIAN_POINT('Ctrl Pts',(-10.7836225816458,-14.505904926533,
118.317753204467)) ;
#158282 = CARTESIAN_POINT('Ctrl Pts',(-10.7040268941245,-14.4703681622542,
118.039876785396)) ;
#158283 = CARTESIAN_POINT('Ctrl Pts',(-10.7099134458307,-14.3968421199682,
118.057806272054)) ;
#158284 = CARTESIAN_POINT('Ctrl Pts',(-10.7837172900055,-14.3968421204311,
118.033575232667)) ;
#158285 = CARTESIAN_POINT('Ctrl Pts',(-10.8575211341802,-14.3968421208941,
118.00934419328)) ;
#158286 = CARTESIAN_POINT('Ctrl Pts',(-10.851634582474,-14.4703681631801,
117.991414706622)) ;
#158287 = CARTESIAN_POINT('Ctrl Pts',(-10.8457480307678,-14.5438942054661,
117.973485219964)) ;
#158288 = CARTESIAN_POINT('Ctrl Pts',(-10.771944186593,-14.5438942050032,
117.997716259351)) ;
#158289 = CARTESIAN_POINT('Ctrl Pts',(-10.6981403424182,-14.5438942045402,
118.021947298738)) ;
#158290 = CARTESIAN_POINT('Ctrl Pts',(-10.7040268941245,-14.4703681622542,
118.039876785396)) ;
#158291 = CARTESIAN_POINT('Ctrl Pts',(-10.6303958446743,-14.359008640194,
117.780055371545)) ;
#158292 = CARTESIAN_POINT('Ctrl Pts',(-10.642168662501,-14.2931494608221,
117.815913475043)) ;
#158293 = CARTESIAN_POINT('Ctrl Pts',(-10.7159725068258,-14.293149462549,
117.791682436113)) ;
#158294 = CARTESIAN_POINT('Ctrl Pts',(-10.7897763511506,-14.2931494642759,
117.767451397183)) ;
#158295 = CARTESIAN_POINT('Ctrl Pts',(-10.7780035333239,-14.3590086436478,
117.731593293686)) ;
#158296 = CARTESIAN_POINT('Ctrl Pts',(-10.7662307154971,-14.4248678230197,
117.695735190188)) ;
#158297 = CARTESIAN_POINT('Ctrl Pts',(-10.6924268711723,-14.4248678212928,
117.719966229118)) ;
#158298 = CARTESIAN_POINT('Ctrl Pts',(-10.6186230268475,-14.4248678195659,
117.744197268048)) ;
#158299 = CARTESIAN_POINT('Ctrl Pts',(-10.6303958446743,-14.359008640194,
117.780055371545)) ;
#158300 = CARTESIAN_POINT('Ctrl Pts',(-10.5692768535784,-14.1808823670753,
117.558510542006)) ;
#158301 = CARTESIAN_POINT('Ctrl Pts',(-10.5860671303228,-14.1273644575797,
117.609651015829)) ;
#158302 = CARTESIAN_POINT('Ctrl Pts',(-10.6598709741343,-14.1273644591981,
117.585419975335)) ;
#158303 = CARTESIAN_POINT('Ctrl Pts',(-10.7336748179457,-14.1273644608165,
117.561188934842)) ;
#158304 = CARTESIAN_POINT('Ctrl Pts',(-10.7168845412014,-14.1808823703121,
117.510048461019)) ;
#158305 = CARTESIAN_POINT('Ctrl Pts',(-10.700094264457,-14.2344002798077,
117.458907987196)) ;
#158306 = CARTESIAN_POINT('Ctrl Pts',(-10.6262904206455,-14.2344002781893,
117.48313902769)) ;
#158307 = CARTESIAN_POINT('Ctrl Pts',(-10.552486576834,-14.2344002765709,
117.507370068183)) ;
#158308 = CARTESIAN_POINT('Ctrl Pts',(-10.5692768535784,-14.1808823670753,
117.558510542006)) ;
#158309 = CARTESIAN_POINT('Ctrl Pts',(-10.525296106505,-13.9476582149858,
117.389059170047)) ;
#158310 = CARTESIAN_POINT('Ctrl Pts',(-10.5459166163672,-13.9103470808531,
117.451865916005)) ;
#158311 = CARTESIAN_POINT('Ctrl Pts',(-10.6197204594822,-13.9103470799281,
117.42763487339)) ;
#158312 = CARTESIAN_POINT('Ctrl Pts',(-10.6935243025973,-13.910347079003,
117.403403830775)) ;
#158313 = CARTESIAN_POINT('Ctrl Pts',(-10.6729037927351,-13.9476582131357,
117.340597084818)) ;
#158314 = CARTESIAN_POINT('Ctrl Pts',(-10.6522832828729,-13.9849693472685,
117.27779033886)) ;
#158315 = CARTESIAN_POINT('Ctrl Pts',(-10.5784794397578,-13.9849693481935,
117.302021381474)) ;
#158316 = CARTESIAN_POINT('Ctrl Pts',(-10.5046755966428,-13.9849693491186,
117.326252424089)) ;
#158317 = CARTESIAN_POINT('Ctrl Pts',(-10.525296106505,-13.9476582149858,
117.389059170047)) ;
#158318 = CARTESIAN_POINT('Ctrl Pts',(-10.5026217165176,-13.6767014389998,
117.284544765499)) ;
#158319 = CARTESIAN_POINT('Ctrl Pts',(-10.52558923415,-13.6582555044241,117.35450011853)) ;
#158320 = CARTESIAN_POINT('Ctrl Pts',(-10.5993930769601,-13.6582554985914,
117.330269074987)) ;
#158321 = CARTESIAN_POINT('Ctrl Pts',(-10.6731969197703,-13.6582554927588,
117.306038031443)) ;
#158322 = CARTESIAN_POINT('Ctrl Pts',(-10.6502294021379,-13.6767014273345,
117.236082678412)) ;
#158323 = CARTESIAN_POINT('Ctrl Pts',(-10.6272618845055,-13.6951473619102,
117.16612732538)) ;
#158324 = CARTESIAN_POINT('Ctrl Pts',(-10.5534580416954,-13.6951473677429,
117.190358368924)) ;
#158325 = CARTESIAN_POINT('Ctrl Pts',(-10.4796541988852,-13.6951473735755,
117.214589412467)) ;
#158326 = CARTESIAN_POINT('Ctrl Pts',(-10.5026217165176,-13.6767014389998,
117.284544765499)) ;
#158327 = CARTESIAN_POINT('Ctrl Pts',(-10.503514877856,-13.3872299120028,
117.251810399679)) ;
#158328 = CARTESIAN_POINT('Ctrl Pts',(-10.5271871489125,-13.3889692104813,
117.323912318046)) ;
#158329 = CARTESIAN_POINT('Ctrl Pts',(-10.6009909922353,-13.388969198278,
117.299681276064)) ;
#158330 = CARTESIAN_POINT('Ctrl Pts',(-10.674794835558,-13.3889691860747,
117.275450234082)) ;
#158331 = CARTESIAN_POINT('Ctrl Pts',(-10.6511225645015,-13.3872298875961,
117.203348315715)) ;
#158332 = CARTESIAN_POINT('Ctrl Pts',(-10.627450293445,-13.3854905891176,
117.131246397348)) ;
#158333 = CARTESIAN_POINT('Ctrl Pts',(-10.5536464501223,-13.385490601321,
117.15547743933)) ;
#158334 = CARTESIAN_POINT('Ctrl Pts',(-10.4798426067995,-13.3854906135243,
117.179708481312)) ;
#158335 = CARTESIAN_POINT('Ctrl Pts',(-10.503514877856,-13.3872299120028,
117.251810399679)) ;
#158336 = CARTESIAN_POINT('Ctrl Pts',(-10.5287931159004,-13.0993467868879,
117.2932723904)) ;
#158337 = CARTESIAN_POINT('Ctrl Pts',(-10.5514700704768,-13.1211895488815,
117.362342735512)) ;
#158338 = CARTESIAN_POINT('Ctrl Pts',(-10.6252739154986,-13.1211895296054,
117.338111698705)) ;
#158339 = CARTESIAN_POINT('Ctrl Pts',(-10.6990777605203,-13.1211895103292,
117.313880661898)) ;
#158340 = CARTESIAN_POINT('Ctrl Pts',(-10.6764008059439,-13.0993467483356,
117.244810316786)) ;
#158341 = CARTESIAN_POINT('Ctrl Pts',(-10.6537238513675,-13.077503986342,
117.175739971674)) ;
#158342 = CARTESIAN_POINT('Ctrl Pts',(-10.5799200063458,-13.0775040056182,
117.199971008481)) ;
#158343 = CARTESIAN_POINT('Ctrl Pts',(-10.506116161324,-13.0775040248944,
117.224202045288)) ;
#158344 = CARTESIAN_POINT('Ctrl Pts',(-10.5287931159004,-13.0993467868879,
117.2932723904)) ;
#158345 = CARTESIAN_POINT('Ctrl Pts',(-10.5772819647789,-12.8349662721153,
117.405511188278)) ;
#158346 = CARTESIAN_POINT('Ctrl Pts',(-10.5973397474272,-12.8753001510476,
117.466603958451)) ;
#158347 = CARTESIAN_POINT('Ctrl Pts',(-10.6711435953011,-12.8753001272113,
117.442372930331)) ;
#158348 = CARTESIAN_POINT('Ctrl Pts',(-10.744947443175,-12.875300103375,117.418141902211)) ;
#158349 = CARTESIAN_POINT('Ctrl Pts',(-10.7248896605266,-12.8349662244428,
117.357049132038)) ;
#158350 = CARTESIAN_POINT('Ctrl Pts',(-10.7048318778782,-12.7946323455105,
117.295956361865)) ;
#158351 = CARTESIAN_POINT('Ctrl Pts',(-10.6310280300044,-12.7946323693468,
117.320187389985)) ;
#158352 = CARTESIAN_POINT('Ctrl Pts',(-10.5572241821305,-12.7946323931831,
117.344418418105)) ;
#158353 = CARTESIAN_POINT('Ctrl Pts',(-10.5772819647789,-12.8349662721153,
117.405511188278)) ;
#158354 = CARTESIAN_POINT('Ctrl Pts',(-10.6462390061054,-12.6123125745559,
117.580099001699)) ;
#158355 = CARTESIAN_POINT('Ctrl Pts',(-10.6622445927396,-12.6682505751424,
117.628849436791)) ;
#158356 = CARTESIAN_POINT('Ctrl Pts',(-10.7360484443089,-12.6682505503797,
117.604618419927)) ;
#158357 = CARTESIAN_POINT('Ctrl Pts',(-10.8098522958782,-12.6682505256169,
117.580387403062)) ;
#158358 = CARTESIAN_POINT('Ctrl Pts',(-10.793846709244,-12.6123125250304,
117.53163696797)) ;
#158359 = CARTESIAN_POINT('Ctrl Pts',(-10.7778411226098,-12.5563745244438,
117.482886532878)) ;
#158360 = CARTESIAN_POINT('Ctrl Pts',(-10.7040372710405,-12.5563745492066,
117.507117549743)) ;
#158361 = CARTESIAN_POINT('Ctrl Pts',(-10.6302334194712,-12.5563745739693,
117.531348566607)) ;
#158362 = CARTESIAN_POINT('Ctrl Pts',(-10.6462390061054,-12.6123125745559,
117.580099001699)) ;
#158363 = CARTESIAN_POINT('Ctrl Pts',(-10.7316789245276,-12.447065748415,
117.804830116923)) ;
#158364 = CARTESIAN_POINT('Ctrl Pts',(-10.7424769532379,-12.5146221963664,
117.83771917099)) ;
#158365 = CARTESIAN_POINT('Ctrl Pts',(-10.8162808090886,-12.5146221752964,
117.813488167166)) ;
#158366 = CARTESIAN_POINT('Ctrl Pts',(-10.8900846649393,-12.5146221542264,
117.789257163342)) ;
#158367 = CARTESIAN_POINT('Ctrl Pts',(-10.8792866362291,-12.4470657062751,
117.756368109275)) ;
#158368 = CARTESIAN_POINT('Ctrl Pts',(-10.8684886075188,-12.3795092583237,
117.723479055207)) ;
#158369 = CARTESIAN_POINT('Ctrl Pts',(-10.7946847516681,-12.3795092793937,
117.747710059031)) ;
#158370 = CARTESIAN_POINT('Ctrl Pts',(-10.7208808958174,-12.3795093004636,
117.771941062855)) ;
#158371 = CARTESIAN_POINT('Ctrl Pts',(-10.7316789245276,-12.447065748415,
117.804830116923)) ;
#158372 = CARTESIAN_POINT('Ctrl Pts',(-10.8280555786512,-12.3516677675638,
118.062896940008)) ;
#158373 = CARTESIAN_POINT('Ctrl Pts',(-10.8328744678437,-12.4259824807609,
118.077574500006)) ;
#158374 = CARTESIAN_POINT('Ctrl Pts',(-10.9066783277089,-12.4259824693785,
118.05334350841)) ;
#158375 = CARTESIAN_POINT('Ctrl Pts',(-10.980482187574,-12.425982457996,118.029112516813)) ;
#158376 = CARTESIAN_POINT('Ctrl Pts',(-10.9756632983816,-12.3516677447989,
118.014434956815)) ;
#158377 = CARTESIAN_POINT('Ctrl Pts',(-10.9708444091891,-12.2773530316018,
117.999757396817)) ;
#158378 = CARTESIAN_POINT('Ctrl Pts',(-10.897040549324,-12.2773530429843,
118.023988388413)) ;
#158379 = CARTESIAN_POINT('Ctrl Pts',(-10.8232366894588,-12.2773530543667,
118.048219380009)) ;
#158380 = CARTESIAN_POINT('Ctrl Pts',(-10.8280555786512,-12.3516677675638,
118.062896940008)) ;
#158381 = CARTESIAN_POINT('Ctrl Pts',(-10.9289420861559,-12.3325934792249,
118.334805693187)) ;
#158382 = CARTESIAN_POINT('Ctrl Pts',(-10.9274561838145,-12.4083470766961,
118.330279875596)) ;
#158383 = CARTESIAN_POINT('Ctrl Pts',(-11.00126004642,-12.4083470802209,118.306048892346)) ;
#158384 = CARTESIAN_POINT('Ctrl Pts',(-11.0750639090255,-12.4083470837456,
118.281817909096)) ;
#158385 = CARTESIAN_POINT('Ctrl Pts',(-11.0765498113669,-12.3325934862743,
118.286343726687)) ;
#158386 = CARTESIAN_POINT('Ctrl Pts',(-11.0780357137083,-12.256839888803,
118.290869544278)) ;
#158387 = CARTESIAN_POINT('Ctrl Pts',(-11.0042318511028,-12.2568398852783,
118.315100527528)) ;
#158388 = CARTESIAN_POINT('Ctrl Pts',(-10.9304279884973,-12.2568398817536,
118.339331510778)) ;
#158389 = CARTESIAN_POINT('Ctrl Pts',(-10.9289420861559,-12.3325934792249,
118.334805693187)) ;
#158390 = CARTESIAN_POINT('Ctrl Pts',(-11.0285549216706,-12.3910918553195,
118.602705295816)) ;
#158391 = CARTESIAN_POINT('Ctrl Pts',(-11.0208468030654,-12.4628709667284,
118.579227611603)) ;
#158392 = CARTESIAN_POINT('Ctrl Pts',(-11.0946506672526,-12.4628709892207,
118.554996633171)) ;
#158393 = CARTESIAN_POINT('Ctrl Pts',(-11.1684545314399,-12.4628710117129,
118.530765654739)) ;
#158394 = CARTESIAN_POINT('Ctrl Pts',(-11.176162650045,-12.3910919003041,
118.554243338952)) ;
#158395 = CARTESIAN_POINT('Ctrl Pts',(-11.1838707686502,-12.3193127888952,
118.577721023164)) ;
#158396 = CARTESIAN_POINT('Ctrl Pts',(-11.110066904463,-12.319312766403,118.601952001596)) ;
#158397 = CARTESIAN_POINT('Ctrl Pts',(-11.0362630402758,-12.3193127439107,
118.626182980028)) ;
#158398 = CARTESIAN_POINT('Ctrl Pts',(-11.0285549216706,-12.3910918553195,
118.602705295816)) ;
#158399 = CARTESIAN_POINT('Ctrl Pts',(-11.1202575355664,-12.5239274893633,
118.846436016608)) ;
#158400 = CARTESIAN_POINT('Ctrl Pts',(-11.1068720088082,-12.5865367592055,
118.805665863374)) ;
#158401 = CARTESIAN_POINT('Ctrl Pts',(-11.1806758725532,-12.5865368036991,
118.781434883595)) ;
#158402 = CARTESIAN_POINT('Ctrl Pts',(-11.2544797362982,-12.5865368481928,
118.757203903816)) ;
#158403 = CARTESIAN_POINT('Ctrl Pts',(-11.2678652630564,-12.5239275783507,
118.797974057049)) ;
#158404 = CARTESIAN_POINT('Ctrl Pts',(-11.2812507898146,-12.4613183085085,
118.838744210283)) ;
#158405 = CARTESIAN_POINT('Ctrl Pts',(-11.2074469260696,-12.4613182640148,
118.862975190062)) ;
#158406 = CARTESIAN_POINT('Ctrl Pts',(-11.1336430623246,-12.4613182195212,
118.887206169841)) ;
#158407 = CARTESIAN_POINT('Ctrl Pts',(-11.1202575355664,-12.5239274893633,
118.846436016608)) ;
#158408 = CARTESIAN_POINT('Ctrl Pts',(-11.1974790053523,-12.7192927751428,
119.046348283817)) ;
#158409 = CARTESIAN_POINT('Ctrl Pts',(-11.1794130086027,-12.7683526424801,
118.991322174291)) ;
#158410 = CARTESIAN_POINT('Ctrl Pts',(-11.2532168690804,-12.7683527070147,
118.96709118456)) ;
#158411 = CARTESIAN_POINT('Ctrl Pts',(-11.3270207295581,-12.7683527715494,
118.942860194829)) ;
#158412 = CARTESIAN_POINT('Ctrl Pts',(-11.3450867263076,-12.719292904212,
118.997886304356)) ;
#158413 = CARTESIAN_POINT('Ctrl Pts',(-11.3631527230572,-12.6702330368747,
119.052912413882)) ;
#158414 = CARTESIAN_POINT('Ctrl Pts',(-11.2893488625795,-12.67023297234,119.077143403613)) ;
#158415 = CARTESIAN_POINT('Ctrl Pts',(-11.2155450021019,-12.6702329078054,
119.101374393344)) ;
#158416 = CARTESIAN_POINT('Ctrl Pts',(-11.1974790053523,-12.7192927751428,
119.046348283817)) ;
#158417 = CARTESIAN_POINT('Ctrl Pts',(-11.256570149613,-12.9658343070978,
119.190811409268)) ;
#158418 = CARTESIAN_POINT('Ctrl Pts',(-11.2350872471003,-12.9977530103242,
119.125377956234)) ;
#158419 = CARTESIAN_POINT('Ctrl Pts',(-11.3088911024947,-12.9977530931819,
119.10114695102)) ;
#158420 = CARTESIAN_POINT('Ctrl Pts',(-11.3826949578891,-12.9977531760396,
119.076915945806)) ;
#158421 = CARTESIAN_POINT('Ctrl Pts',(-11.4041778604018,-12.9658344728131,
119.142349398841)) ;
#158422 = CARTESIAN_POINT('Ctrl Pts',(-11.4256607629145,-12.9339157695866,
119.207782851876)) ;
#158423 = CARTESIAN_POINT('Ctrl Pts',(-11.3518569075202,-12.9339156867289,
119.23201385709)) ;
#158424 = CARTESIAN_POINT('Ctrl Pts',(-11.2780530521258,-12.9339156038712,
119.256244862303)) ;
#158425 = CARTESIAN_POINT('Ctrl Pts',(-11.256570149613,-12.9658343070978,
119.190811409268)) ;
#158426 = CARTESIAN_POINT('Ctrl Pts',(-11.2934413311918,-13.2443245338218,
119.267674974483)) ;
#158427 = CARTESIAN_POINT('Ctrl Pts',(-11.2700862207604,-13.2568466102088,
119.196539078311)) ;
#158428 = CARTESIAN_POINT('Ctrl Pts',(-11.3438900691195,-13.2568467056125,
119.172308051669)) ;
#158429 = CARTESIAN_POINT('Ctrl Pts',(-11.4176939174786,-13.2568468010161,
119.148077025028)) ;
#158430 = CARTESIAN_POINT('Ctrl Pts',(-11.4410490279101,-13.2443247246291,
119.2192129212)) ;
#158431 = CARTESIAN_POINT('Ctrl Pts',(-11.4644041383415,-13.2318026482422,
119.290348817372)) ;
#158432 = CARTESIAN_POINT('Ctrl Pts',(-11.3906002899824,-13.2318025528385,
119.314579844014)) ;
#158433 = CARTESIAN_POINT('Ctrl Pts',(-11.3167964416232,-13.2318024574349,
119.338810870656)) ;
#158434 = CARTESIAN_POINT('Ctrl Pts',(-11.2934413311918,-13.2443245338218,
119.267674974483)) ;
#158435 = CARTESIAN_POINT('Ctrl Pts',(-11.3062978123674,-13.5367809605308,
119.271198329631)) ;
#158436 = CARTESIAN_POINT('Ctrl Pts',(-11.2827481298824,-13.5289033830346,
119.199469798479)) ;
#158437 = CARTESIAN_POINT('Ctrl Pts',(-11.356551969916,-13.5289034843527,
119.175238746478)) ;
#158438 = CARTESIAN_POINT('Ctrl Pts',(-11.4303558099495,-13.5289035856708,
119.151007694478)) ;
#158439 = CARTESIAN_POINT('Ctrl Pts',(-11.4539054924344,-13.536781163167,
119.222736225631)) ;
#158440 = CARTESIAN_POINT('Ctrl Pts',(-11.4774551749194,-13.5446587406632,
119.294464756783)) ;
#158441 = CARTESIAN_POINT('Ctrl Pts',(-11.4036513348859,-13.5446586393451,
119.318695808783)) ;
#158442 = CARTESIAN_POINT('Ctrl Pts',(-11.3298474948524,-13.544658538027,
119.342926860784)) ;
#158443 = CARTESIAN_POINT('Ctrl Pts',(-11.3062978123674,-13.5367809605308,
119.271198329631)) ;
#158444 = CARTESIAN_POINT('Ctrl Pts',(-11.2949986489025,-13.8179726435299,
119.201501210985)) ;
#158445 = CARTESIAN_POINT('Ctrl Pts',(-11.2729334999951,-13.790451684124,
119.134294329632)) ;
#158446 = CARTESIAN_POINT('Ctrl Pts',(-11.3467373314644,-13.7904517814122,
119.110063251546)) ;
#158447 = CARTESIAN_POINT('Ctrl Pts',(-11.4205411629338,-13.7904518787005,
119.085832173461)) ;
#158448 = CARTESIAN_POINT('Ctrl Pts',(-11.4426063118413,-13.8179728381065,
119.153039054814)) ;
#158449 = CARTESIAN_POINT('Ctrl Pts',(-11.4646714607487,-13.8454937975124,
119.220245936167)) ;
#158450 = CARTESIAN_POINT('Ctrl Pts',(-11.3908676292793,-13.8454937002241,
119.244477014252)) ;
#158451 = CARTESIAN_POINT('Ctrl Pts',(-11.3170637978099,-13.8454936029358,
119.268708092337)) ;
#158452 = CARTESIAN_POINT('Ctrl Pts',(-11.2949986489025,-13.8179726435299,
119.201501210985)) ;
#158453 = CARTESIAN_POINT('Ctrl Pts',(-11.2610571461274,-14.0724753431544,
119.062587049155)) ;
#158454 = CARTESIAN_POINT('Ctrl Pts',(-11.2420643680726,-14.0271455372004,
119.004738113744)) ;
#158455 = CARTESIAN_POINT('Ctrl Pts',(-11.315868191413,-14.0271456228523,
118.980507010899)) ;
#158456 = CARTESIAN_POINT('Ctrl Pts',(-11.3896720147534,-14.0271457085042,
118.956275908055)) ;
#158457 = CARTESIAN_POINT('Ctrl Pts',(-11.4086647928082,-14.0724755144583,
119.014124843466)) ;
#158458 = CARTESIAN_POINT('Ctrl Pts',(-11.4276575708631,-14.1178053204124,
119.071973778877)) ;
#158459 = CARTESIAN_POINT('Ctrl Pts',(-11.3538537475226,-14.1178052347605,
119.096204881721)) ;
#158460 = CARTESIAN_POINT('Ctrl Pts',(-11.2800499241822,-14.1178051491085,
119.120435984566)) ;
#158461 = CARTESIAN_POINT('Ctrl Pts',(-11.2610571461274,-14.0724753431544,
119.062587049155)) ;
#158462 = CARTESIAN_POINT('Ctrl Pts',(-11.2078251507878,-14.279096140685,
118.865063933435)) ;
#158463 = CARTESIAN_POINT('Ctrl Pts',(-11.193253085461,-14.2192740208291,
118.820679775734)) ;
#158464 = CARTESIAN_POINT('Ctrl Pts',(-11.2670569021607,-14.219274086963,
118.796448652663)) ;
#158465 = CARTESIAN_POINT('Ctrl Pts',(-11.3408607188604,-14.219274153097,
118.772217529592)) ;
#158466 = CARTESIAN_POINT('Ctrl Pts',(-11.3554327841873,-14.2790962729529,
118.816601687293)) ;
#158467 = CARTESIAN_POINT('Ctrl Pts',(-11.3700048495141,-14.3389183928089,
118.860985844993)) ;
#158468 = CARTESIAN_POINT('Ctrl Pts',(-11.2962010328144,-14.3389183266749,
118.885216968064)) ;
#158469 = CARTESIAN_POINT('Ctrl Pts',(-11.2223972161146,-14.3389182605409,
118.909448091136)) ;
#158470 = CARTESIAN_POINT('Ctrl Pts',(-11.2078251507878,-14.279096140685,
118.865063933435)) ;
#158471 = CARTESIAN_POINT('Ctrl Pts',(-11.1396467770328,-14.4248617955916,
118.621919734993)) ;
#158472 = CARTESIAN_POINT('Ctrl Pts',(-11.1305472737529,-14.3547743304939,
118.594204118298)) ;
#158473 = CARTESIAN_POINT('Ctrl Pts',(-11.2043510858454,-14.3547743715158,
118.569972981194)) ;
#158474 = CARTESIAN_POINT('Ctrl Pts',(-11.2781548979379,-14.3547744125376,
118.545741844089)) ;
#158475 = CARTESIAN_POINT('Ctrl Pts',(-11.2872544012177,-14.4248618776352,
118.573457460785)) ;
#158476 = CARTESIAN_POINT('Ctrl Pts',(-11.2963539044976,-14.4949493427329,
118.60117307748)) ;
#158477 = CARTESIAN_POINT('Ctrl Pts',(-11.2225500924051,-14.494949301711,
118.625404214584)) ;
#158478 = CARTESIAN_POINT('Ctrl Pts',(-11.1487462803127,-14.4949492606892,
118.649635351688)) ;
#158479 = CARTESIAN_POINT('Ctrl Pts',(-11.1396467770328,-14.4248617955916,
118.621919734993)) ;
#158480 = CARTESIAN_POINT('Ctrl Pts',(-11.0618371790876,-14.4982152843021,
118.349277506824)) ;
#158481 = CARTESIAN_POINT('Ctrl Pts',(-11.0588940278122,-14.4229018669145,
118.340313144982)) ;
#158482 = CARTESIAN_POINT('Ctrl Pts',(-11.132697838093,-14.4229018794509,
118.31608200236)) ;
#158483 = CARTESIAN_POINT('Ctrl Pts',(-11.2065016483738,-14.4229018919873,
118.291850859737)) ;
#158484 = CARTESIAN_POINT('Ctrl Pts',(-11.2094447996491,-14.4982153093749,
118.300815221579)) ;
#158485 = CARTESIAN_POINT('Ctrl Pts',(-11.2123879509244,-14.5735287267625,
118.309779583422)) ;
#158486 = CARTESIAN_POINT('Ctrl Pts',(-11.1385841406437,-14.5735287142261,
118.334010726044)) ;
#158487 = CARTESIAN_POINT('Ctrl Pts',(-11.0647803303629,-14.5735287016897,
118.358241868666)) ;
#158488 = CARTESIAN_POINT('Ctrl Pts',(-11.0618371790876,-14.4982152843021,
118.349277506824)) ;
#158489 = CARTESIAN_POINT('Ctrl Pts',(-10.9820685755435,-14.4941260357652,
118.071094122751)) ;
#158490 = CARTESIAN_POINT('Ctrl Pts',(-10.9854191081343,-14.4189866403318,
118.081299306452)) ;
#158491 = CARTESIAN_POINT('Ctrl Pts',(-11.0592229190619,-14.4189866245763,
118.0570681658)) ;
#158492 = CARTESIAN_POINT('Ctrl Pts',(-11.1330267299894,-14.4189866088209,
118.032837025147)) ;
#158493 = CARTESIAN_POINT('Ctrl Pts',(-11.1296761973986,-14.4941260042543,
118.022631841447)) ;
#158494 = CARTESIAN_POINT('Ctrl Pts',(-11.1263256648078,-14.5692653996877,
118.012426657746)) ;
#158495 = CARTESIAN_POINT('Ctrl Pts',(-11.0525218538802,-14.5692654154432,
118.036657798398)) ;
#158496 = CARTESIAN_POINT('Ctrl Pts',(-10.9787180429527,-14.5692654311986,
118.060888939051)) ;
#158497 = CARTESIAN_POINT('Ctrl Pts',(-10.9820685755435,-14.4941260357652,
118.071094122751)) ;
#158498 = CARTESIAN_POINT('Ctrl Pts',(-10.9049115286395,-14.4126782343137,
117.800421801026)) ;
#158499 = CARTESIAN_POINT('Ctrl Pts',(-10.9143918514831,-14.3431123024057,
117.829297336722)) ;
#158500 = CARTESIAN_POINT('Ctrl Pts',(-10.9881956660435,-14.3431122609052,
117.805066207135)) ;
#158501 = CARTESIAN_POINT('Ctrl Pts',(-11.061999480604,-14.3431122194047,
117.780835077547)) ;
#158502 = CARTESIAN_POINT('Ctrl Pts',(-11.0525191577604,-14.4126781513128,
117.751959541852)) ;
#158503 = CARTESIAN_POINT('Ctrl Pts',(-11.0430388349169,-14.4822440832209,
117.723084006156)) ;
#158504 = CARTESIAN_POINT('Ctrl Pts',(-10.9692350203564,-14.4822441247213,
117.747315135743)) ;
#158505 = CARTESIAN_POINT('Ctrl Pts',(-10.8954312057959,-14.4822441662218,
117.77154626533)) ;
#158506 = CARTESIAN_POINT('Ctrl Pts',(-10.9049115286395,-14.4126782343137,
117.800421801026)) ;
#158507 = CARTESIAN_POINT('Ctrl Pts',(-10.8381211251888,-14.2599648668114,
117.561542528994)) ;
#158508 = CARTESIAN_POINT('Ctrl Pts',(-10.8530122817742,-14.2009567428221,
117.606898591146)) ;
#158509 = CARTESIAN_POINT('Ctrl Pts',(-10.9268161018888,-14.2009566811552,
117.582667478476)) ;
#158510 = CARTESIAN_POINT('Ctrl Pts',(-11.0006199220034,-14.2009566194882,
117.558436365806)) ;
#158511 = CARTESIAN_POINT('Ctrl Pts',(-10.9857287654181,-14.2599647434775,
117.513080303654)) ;
#158512 = CARTESIAN_POINT('Ctrl Pts',(-10.9708376088328,-14.3189728674668,
117.467724241502)) ;
#158513 = CARTESIAN_POINT('Ctrl Pts',(-10.8970337887181,-14.3189729291337,
117.491955354172)) ;
#158514 = CARTESIAN_POINT('Ctrl Pts',(-10.8232299686035,-14.3189729908007,
117.516186466842)) ;
#158515 = CARTESIAN_POINT('Ctrl Pts',(-10.8381211251888,-14.2599648668114,
117.561542528994)) ;
#158516 = CARTESIAN_POINT('Ctrl Pts',(-10.7868067530969,-14.0478524029628,
117.369893536837)) ;
#158517 = CARTESIAN_POINT('Ctrl Pts',(-10.8060344417783,-14.0035651769701,
117.428457975966)) ;
#158518 = CARTESIAN_POINT('Ctrl Pts',(-10.8798382686568,-14.0035651015323,
117.404226883898)) ;
#158519 = CARTESIAN_POINT('Ctrl Pts',(-10.9536420955354,-14.0035650260945,
117.37999579183)) ;
#158520 = CARTESIAN_POINT('Ctrl Pts',(-10.934414406854,-14.0478522520872,
117.321431352701)) ;
#158521 = CARTESIAN_POINT('Ctrl Pts',(-10.9151867181727,-14.0921394780799,
117.262866913572)) ;
#158522 = CARTESIAN_POINT('Ctrl Pts',(-10.8413828912941,-14.0921395535177,
117.28709800564)) ;
#158523 = CARTESIAN_POINT('Ctrl Pts',(-10.7675790644156,-14.0921396289556,
117.311329097708)) ;
#158524 = CARTESIAN_POINT('Ctrl Pts',(-10.7868067530969,-14.0478524029628,
117.369893536837)) ;
#158525 = CARTESIAN_POINT('Ctrl Pts',(-10.7550957653846,-13.7904112840523,
117.237886359139)) ;
#158526 = CARTESIAN_POINT('Ctrl Pts',(-10.7772993131729,-13.764031497392,
117.305514784843)) ;
#158527 = CARTESIAN_POINT('Ctrl Pts',(-10.8511031475577,-13.7640314159743,
117.281283715637)) ;
#158528 = CARTESIAN_POINT('Ctrl Pts',(-10.9249069819425,-13.7640313345566,
117.257052646432)) ;
#158529 = CARTESIAN_POINT('Ctrl Pts',(-10.9027034341542,-13.7904111212169,
117.189424220728)) ;
#158530 = CARTESIAN_POINT('Ctrl Pts',(-10.8804998863659,-13.8167909078772,
117.121795795024)) ;
#158531 = CARTESIAN_POINT('Ctrl Pts',(-10.8066960519811,-13.8167909892949,
117.14602686423)) ;
#158532 = CARTESIAN_POINT('Ctrl Pts',(-10.7328922175963,-13.8167910707126,
117.170257933435)) ;
#158533 = CARTESIAN_POINT('Ctrl Pts',(-10.7550957653846,-13.7904112840523,
117.237886359139)) ;
#158534 = CARTESIAN_POINT('Ctrl Pts',(-10.7462257200646,-13.5044552055669,
117.175225916484)) ;
#158535 = CARTESIAN_POINT('Ctrl Pts',(-10.7698198062168,-13.4980004286212,
117.247089697519)) ;
#158536 = CARTESIAN_POINT('Ctrl Pts',(-10.8436236479381,-13.498000350832,
117.222858650659)) ;
#158537 = CARTESIAN_POINT('Ctrl Pts',(-10.9174274896593,-13.4980002730428,
117.198627603799)) ;
#158538 = CARTESIAN_POINT('Ctrl Pts',(-10.893833403507,-13.5044550499884,
117.126763822765)) ;
#158539 = CARTESIAN_POINT('Ctrl Pts',(-10.8702393173548,-13.5109098269341,
117.05490004173)) ;
#158540 = CARTESIAN_POINT('Ctrl Pts',(-10.7964354756336,-13.5109099047233,
117.07913108859)) ;
#158541 = CARTESIAN_POINT('Ctrl Pts',(-10.7226316339123,-13.5109099825126,
117.10336213545)) ;
#158542 = CARTESIAN_POINT('Ctrl Pts',(-10.7462257200646,-13.5044552055669,
117.175225916484)) ;
#158543 = CARTESIAN_POINT('Ctrl Pts',(-10.7617483985087,-13.2137879040768,
117.187050717025)) ;
#158544 = CARTESIAN_POINT('Ctrl Pts',(-10.7850280399954,-13.227617723032,
117.257956750195)) ;
#158545 = CARTESIAN_POINT('Ctrl Pts',(-10.8588318877171,-13.2276176541368,
117.233725721612)) ;
#158546 = CARTESIAN_POINT('Ctrl Pts',(-10.9326357354387,-13.2276175852417,
117.209494693028)) ;
#158547 = CARTESIAN_POINT('Ctrl Pts',(-10.909356093952,-13.2137877662865,
117.138588659857)) ;
#158548 = CARTESIAN_POINT('Ctrl Pts',(-10.8860764524653,-13.1999579473313,
117.067682626687)) ;
#158549 = CARTESIAN_POINT('Ctrl Pts',(-10.8122726047436,-13.1999580162265,
117.091913655271)) ;
#158550 = CARTESIAN_POINT('Ctrl Pts',(-10.738468757022,-13.1999580851216,
117.116144683854)) ;
#158551 = CARTESIAN_POINT('Ctrl Pts',(-10.7617483985087,-13.2137879040768,
117.187050717025)) ;
#158552 = CARTESIAN_POINT('Ctrl Pts',(-10.8009076226651,-12.9385963486889,
117.270982185733)) ;
#158553 = CARTESIAN_POINT('Ctrl Pts',(-10.8222196074267,-12.9716609792406,
117.335895053863)) ;
#158554 = CARTESIAN_POINT('Ctrl Pts',(-10.8960234597266,-12.9716609227663,
117.311664039224)) ;
#158555 = CARTESIAN_POINT('Ctrl Pts',(-10.9698273120265,-12.9716608662921,
117.287433024585)) ;
#158556 = CARTESIAN_POINT('Ctrl Pts',(-10.9485153272649,-12.9385962357404,
117.222520156455)) ;
#158557 = CARTESIAN_POINT('Ctrl Pts',(-10.9272033425033,-12.9055316051888,
117.157607288325)) ;
#158558 = CARTESIAN_POINT('Ctrl Pts',(-10.8533994902034,-12.905531661663,
117.181838302964)) ;
#158559 = CARTESIAN_POINT('Ctrl Pts',(-10.7795956379035,-12.9055317181373,
117.206069317603)) ;
#158560 = CARTESIAN_POINT('Ctrl Pts',(-10.8009076226651,-12.9385963486889,
117.270982185733)) ;
#158561 = CARTESIAN_POINT('Ctrl Pts',(-10.8619688891867,-12.6966955833364,
117.421502681034)) ;
#158562 = CARTESIAN_POINT('Ctrl Pts',(-10.8797836635334,-12.746700030026,
117.475763610349)) ;
#158563 = CARTESIAN_POINT('Ctrl Pts',(-10.9535875184615,-12.7466999895666,
117.451532603715)) ;
#158564 = CARTESIAN_POINT('Ctrl Pts',(-11.0273913733895,-12.7466999491071,
117.427301597081)) ;
#158565 = CARTESIAN_POINT('Ctrl Pts',(-11.0095765990428,-12.6966955024176,
117.373040667766)) ;
#158566 = CARTESIAN_POINT('Ctrl Pts',(-10.991761824696,-12.646691055728,117.31877973845)) ;
#158567 = CARTESIAN_POINT('Ctrl Pts',(-10.9179579697679,-12.6466910961874,
117.343010745084)) ;
#158568 = CARTESIAN_POINT('Ctrl Pts',(-10.8441541148399,-12.6466911366469,
117.367241751718)) ;
#158569 = CARTESIAN_POINT('Ctrl Pts',(-10.8619688891867,-12.6966955833364,
117.421502681034)) ;
#158570 = CARTESIAN_POINT('Ctrl Pts',(-10.9413222714456,-12.5064217313258,
117.627710657807)) ;
#158571 = CARTESIAN_POINT('Ctrl Pts',(-10.9543578954928,-12.5697873341699,
117.667415066251)) ;
#158572 = CARTESIAN_POINT('Ctrl Pts',(-11.0281617510148,-12.5697873098007,
117.643184061426)) ;
#158573 = CARTESIAN_POINT('Ctrl Pts',(-11.1019656065368,-12.5697872854314,
117.618953056601)) ;
#158574 = CARTESIAN_POINT('Ctrl Pts',(-11.0889299824896,-12.5064216825873,
117.579248648158)) ;
#158575 = CARTESIAN_POINT('Ctrl Pts',(-11.0758943584425,-12.4430560797432,
117.539544239714)) ;
#158576 = CARTESIAN_POINT('Ctrl Pts',(-11.0020905029204,-12.4430561041124,
117.563775244539)) ;
#158577 = CARTESIAN_POINT('Ctrl Pts',(-10.9282866473984,-12.4430561284817,
117.588006249364)) ;
#158578 = CARTESIAN_POINT('Ctrl Pts',(-10.9413222714456,-12.5064217313258,
117.627710657807)) ;
#158579 = CARTESIAN_POINT('Ctrl Pts',(-11.0338914556794,-12.3814205030376,
117.874194374824)) ;
#158580 = CARTESIAN_POINT('Ctrl Pts',(-11.0412174109701,-12.45361013115,117.896508053317)) ;
#158581 = CARTESIAN_POINT('Ctrl Pts',(-11.1150212654786,-12.4536101207451,
117.872277045405)) ;
#158582 = CARTESIAN_POINT('Ctrl Pts',(-11.1888251199871,-12.4536101103402,
117.848046037493)) ;
#158583 = CARTESIAN_POINT('Ctrl Pts',(-11.1814991646964,-12.3814204822278,
117.825732359)) ;
#158584 = CARTESIAN_POINT('Ctrl Pts',(-11.1741732094057,-12.3092308541153,
117.803418680506)) ;
#158585 = CARTESIAN_POINT('Ctrl Pts',(-11.1003693548972,-12.3092308645202,
117.827649688418)) ;
#158586 = CARTESIAN_POINT('Ctrl Pts',(-11.0265655003887,-12.3092308749251,
117.85188069633)) ;
#158587 = CARTESIAN_POINT('Ctrl Pts',(-11.0338914556794,-12.3814205030376,
117.874194374824)) ;
#158588 = CARTESIAN_POINT('Ctrl Pts',(-11.1342884555144,-12.3309490204366,
118.144369386401)) ;
#158589 = CARTESIAN_POINT('Ctrl Pts',(-11.1353525093658,-12.4067726596542,
118.147610323274)) ;
#158590 = CARTESIAN_POINT('Ctrl Pts',(-11.2091563612748,-12.4067726592374,
118.123379307444)) ;
#158591 = CARTESIAN_POINT('Ctrl Pts',(-11.2829602131838,-12.4067726588207,
118.099148291614)) ;
#158592 = CARTESIAN_POINT('Ctrl Pts',(-11.2818961593323,-12.330949019603,
118.095907354741)) ;
#158593 = CARTESIAN_POINT('Ctrl Pts',(-11.2808321054809,-12.2551253803854,
118.092666417868)) ;
#158594 = CARTESIAN_POINT('Ctrl Pts',(-11.2070282535719,-12.2551253808022,
118.116897433698)) ;
#158595 = CARTESIAN_POINT('Ctrl Pts',(-11.133224401663,-12.255125381219,118.141128449528)) ;
#158596 = CARTESIAN_POINT('Ctrl Pts',(-11.1342884555144,-12.3309490204366,
118.144369386401)) ;
#158597 = CARTESIAN_POINT('Ctrl Pts',(-11.2344352101216,-12.3579787522632,
118.414220057428)) ;
#158598 = CARTESIAN_POINT('Ctrl Pts',(-11.2292363302067,-12.4320290416833,
118.398385108464)) ;
#158599 = CARTESIAN_POINT('Ctrl Pts',(-11.303040180183,-12.4320290471933,
118.374154086748)) ;
#158600 = CARTESIAN_POINT('Ctrl Pts',(-11.3768440301593,-12.4320290527033,
118.349923065032)) ;
#158601 = CARTESIAN_POINT('Ctrl Pts',(-11.3820429100743,-12.3579787632832,
118.365758013996)) ;
#158602 = CARTESIAN_POINT('Ctrl Pts',(-11.3872417899893,-12.2839284738631,
118.38159296296)) ;
#158603 = CARTESIAN_POINT('Ctrl Pts',(-11.3134379400129,-12.2839284683531,
118.405823984676)) ;
#158604 = CARTESIAN_POINT('Ctrl Pts',(-11.2396340900366,-12.2839284628431,
118.430055006392)) ;
#158605 = CARTESIAN_POINT('Ctrl Pts',(-11.2344352101216,-12.3579787522632,
118.414220057428)) ;
#158606 = CARTESIAN_POINT('Ctrl Pts',(-11.3303750050126,-12.461461206882,
118.670792503069)) ;
#158607 = CARTESIAN_POINT('Ctrl Pts',(-11.3192068132449,-12.5283982631063,
118.636775993175)) ;
#158608 = CARTESIAN_POINT('Ctrl Pts',(-11.3930106600982,-12.5283982698858,
118.612544961947)) ;
#158609 = CARTESIAN_POINT('Ctrl Pts',(-11.4668145069516,-12.5283982766654,
118.588313930718)) ;
#158610 = CARTESIAN_POINT('Ctrl Pts',(-11.4779826987193,-12.4614612204411,
118.622330440612)) ;
#158611 = CARTESIAN_POINT('Ctrl Pts',(-11.4891508904871,-12.3945241642168,
118.656346950506)) ;
#158612 = CARTESIAN_POINT('Ctrl Pts',(-11.4153470436337,-12.3945241574372,
118.680577981735)) ;
#158613 = CARTESIAN_POINT('Ctrl Pts',(-11.3415431967804,-12.3945241506577,
118.704809012963)) ;
#158614 = CARTESIAN_POINT('Ctrl Pts',(-11.3303750050126,-12.461461206882,
118.670792503069)) ;
#158615 = CARTESIAN_POINT('Ctrl Pts',(-11.4139998494669,-12.6327579824641,
118.890139759141)) ;
#158616 = CARTESIAN_POINT('Ctrl Pts',(-11.3977074845766,-12.6878348099754,
118.840515844591)) ;
#158617 = CARTESIAN_POINT('Ctrl Pts',(-11.4715113295313,-12.6878348153818,
118.816284807579)) ;
#158618 = CARTESIAN_POINT('Ctrl Pts',(-11.5453151744861,-12.6878348207882,
118.792053770568)) ;
#158619 = CARTESIAN_POINT('Ctrl Pts',(-11.5616075393764,-12.632757993277,
118.841677685119)) ;
#158620 = CARTESIAN_POINT('Ctrl Pts',(-11.5778999042667,-12.5776811657657,
118.891301599669)) ;
#158621 = CARTESIAN_POINT('Ctrl Pts',(-11.5040960593119,-12.5776811603593,
118.91553263668)) ;
#158622 = CARTESIAN_POINT('Ctrl Pts',(-11.4302922143571,-12.5776811549529,
118.939763673692)) ;
#158623 = CARTESIAN_POINT('Ctrl Pts',(-11.4139998494669,-12.6327579824641,
118.890139759141)) ;
#158624 = CARTESIAN_POINT('Ctrl Pts',(-11.4811854191605,-12.8610649262646,
119.059239036713)) ;
#158625 = CARTESIAN_POINT('Ctrl Pts',(-11.4609125728297,-12.9002826126032,
118.997491217836)) ;
#158626 = CARTESIAN_POINT('Ctrl Pts',(-11.5347164164161,-12.9002826143644,
118.973260176657)) ;
#158627 = CARTESIAN_POINT('Ctrl Pts',(-11.6085202600025,-12.9002826161256,
118.949029135478)) ;
#158628 = CARTESIAN_POINT('Ctrl Pts',(-11.6287931063334,-12.861064929787,
119.010776954355)) ;
#158629 = CARTESIAN_POINT('Ctrl Pts',(-11.6490659526642,-12.8218472434483,
119.072524773233)) ;
#158630 = CARTESIAN_POINT('Ctrl Pts',(-11.5752621090778,-12.8218472416871,
119.096755814412)) ;
#158631 = CARTESIAN_POINT('Ctrl Pts',(-11.5014582654913,-12.8218472399259,
119.120986855591)) ;
#158632 = CARTESIAN_POINT('Ctrl Pts',(-11.4811854191605,-12.8610649262646,
119.059239036713)) ;
#158633 = CARTESIAN_POINT('Ctrl Pts',(-11.5272358980316,-13.1282120035714,
119.164129227647)) ;
#158634 = CARTESIAN_POINT('Ctrl Pts',(-11.5044492380184,-13.1488341330094,
119.094724737833)) ;
#158635 = CARTESIAN_POINT('Ctrl Pts',(-11.578253081244,-13.1488341316972,
119.070493695555)) ;
#158636 = CARTESIAN_POINT('Ctrl Pts',(-11.6520569244697,-13.148834130385,
119.046262653278)) ;
#158637 = CARTESIAN_POINT('Ctrl Pts',(-11.6748435844829,-13.1282120009471,
119.115667143091)) ;
#158638 = CARTESIAN_POINT('Ctrl Pts',(-11.6976302444961,-13.1075898715092,
119.185071632905)) ;
#158639 = CARTESIAN_POINT('Ctrl Pts',(-11.6238264012704,-13.1075898728214,
119.209302675182)) ;
#158640 = CARTESIAN_POINT('Ctrl Pts',(-11.5500225580448,-13.1075898741335,
119.23353371746)) ;
#158641 = CARTESIAN_POINT('Ctrl Pts',(-11.5272358980316,-13.1282120035714,
119.164129227647)) ;
#158642 = CARTESIAN_POINT('Ctrl Pts',(-11.550031999704,-13.4170777357306,
119.198051643061)) ;
#158643 = CARTESIAN_POINT('Ctrl Pts',(-11.5263544375705,-13.4175593372615,
119.125933609099)) ;
#158644 = CARTESIAN_POINT('Ctrl Pts',(-11.6001582809506,-13.4175593339228,
119.101702567291)) ;
#158645 = CARTESIAN_POINT('Ctrl Pts',(-11.6739621243306,-13.4175593305841,
119.077471525484)) ;
#158646 = CARTESIAN_POINT('Ctrl Pts',(-11.697639686464,-13.4170777290533,
119.149589559446)) ;
#158647 = CARTESIAN_POINT('Ctrl Pts',(-11.7213172485975,-13.4165961275224,
119.221707593408)) ;
#158648 = CARTESIAN_POINT('Ctrl Pts',(-11.6475134052175,-13.4165961308611,
119.245938635216)) ;
#158649 = CARTESIAN_POINT('Ctrl Pts',(-11.5737095618374,-13.4165961341998,
119.270169677024)) ;
#158650 = CARTESIAN_POINT('Ctrl Pts',(-11.550031999704,-13.4170777357306,
119.198051643061)) ;
#158651 = CARTESIAN_POINT('Ctrl Pts',(-11.5484863559817,-13.7056413839055,
119.157890620187)) ;
#158652 = CARTESIAN_POINT('Ctrl Pts',(-11.5256154218655,-13.6859734009019,
119.088229445024)) ;
#158653 = CARTESIAN_POINT('Ctrl Pts',(-11.5994192655733,-13.6859733981245,
119.063998404215)) ;
#158654 = CARTESIAN_POINT('Ctrl Pts',(-11.6732231092811,-13.6859733953471,
119.039767363405)) ;
#158655 = CARTESIAN_POINT('Ctrl Pts',(-11.6960940433973,-13.7056413783507,
119.109428538568)) ;
#158656 = CARTESIAN_POINT('Ctrl Pts',(-11.7189649775135,-13.7253093613543,
119.179089713731)) ;
#158657 = CARTESIAN_POINT('Ctrl Pts',(-11.6451611338057,-13.7253093641317,
119.20332075454)) ;
#158658 = CARTESIAN_POINT('Ctrl Pts',(-11.5713572900979,-13.725309366909,
119.22755179535)) ;
#158659 = CARTESIAN_POINT('Ctrl Pts',(-11.5484863559817,-13.7056413839055,
119.157890620187)) ;
#158660 = CARTESIAN_POINT('Ctrl Pts',(-11.5233022878553,-13.9747406301587,
119.04555969316)) ;
#158661 = CARTESIAN_POINT('Ctrl Pts',(-11.5028934277546,-13.9362526969778,
118.983397598257)) ;
#158662 = CARTESIAN_POINT('Ctrl Pts',(-11.5766972711998,-13.9362526974253,
118.959166556648)) ;
#158663 = CARTESIAN_POINT('Ctrl Pts',(-11.650501114645,-13.9362526978728,
118.934935515039)) ;
#158664 = CARTESIAN_POINT('Ctrl Pts',(-11.6709099747456,-13.9747406310537,
118.997097609941)) ;
#158665 = CARTESIAN_POINT('Ctrl Pts',(-11.6913188348462,-14.0132285642346,
119.059259704844)) ;
#158666 = CARTESIAN_POINT('Ctrl Pts',(-11.6175149914011,-14.0132285637871,
119.083490746453)) ;
#158667 = CARTESIAN_POINT('Ctrl Pts',(-11.5437111479559,-14.0132285633396,
119.107721788062)) ;
#158668 = CARTESIAN_POINT('Ctrl Pts',(-11.5233022878553,-13.9747406301587,
119.04555969316)) ;
#158669 = CARTESIAN_POINT('Ctrl Pts',(-11.4774772491034,-14.201974810105,
118.870644857214)) ;
#158670 = CARTESIAN_POINT('Ctrl Pts',(-11.4609696918761,-14.1475641696475,
118.820365501466)) ;
#158671 = CARTESIAN_POINT('Ctrl Pts',(-11.5347735344237,-14.1475641728961,
118.796134457123)) ;
#158672 = CARTESIAN_POINT('Ctrl Pts',(-11.6085773769713,-14.1475641761448,
118.77190341278)) ;
#158673 = CARTESIAN_POINT('Ctrl Pts',(-11.6250849341986,-14.2019748166024,
118.822182768528)) ;
#158674 = CARTESIAN_POINT('Ctrl Pts',(-11.6415924914259,-14.2563854570598,
118.872462124276)) ;
#158675 = CARTESIAN_POINT('Ctrl Pts',(-11.5677886488783,-14.2563854538112,
118.896693168619)) ;
#158676 = CARTESIAN_POINT('Ctrl Pts',(-11.4939848063307,-14.2563854505624,
118.920924212962)) ;
#158677 = CARTESIAN_POINT('Ctrl Pts',(-11.4774772491034,-14.201974810105,
118.870644857214)) ;
#158678 = CARTESIAN_POINT('Ctrl Pts',(-11.4147391200156,-14.3739130003505,
118.644102382187)) ;
#158679 = CARTESIAN_POINT('Ctrl Pts',(-11.4033218176889,-14.3074175885929,
118.609327121665)) ;
#158680 = CARTESIAN_POINT('Ctrl Pts',(-11.4771256584836,-14.3074175937146,
118.585096071983)) ;
#158681 = CARTESIAN_POINT('Ctrl Pts',(-11.5509294992783,-14.3074175988363,
118.560865022301)) ;
#158682 = CARTESIAN_POINT('Ctrl Pts',(-11.5623468016051,-14.3739130105938,
118.595640282823)) ;
#158683 = CARTESIAN_POINT('Ctrl Pts',(-11.5737641039319,-14.4404084223513,
118.630415543346)) ;
#158684 = CARTESIAN_POINT('Ctrl Pts',(-11.4999602631372,-14.4404084172297,
118.654646593028)) ;
#158685 = CARTESIAN_POINT('Ctrl Pts',(-11.4261564223424,-14.440408412108,
118.67887764271)) ;
#158686 = CARTESIAN_POINT('Ctrl Pts',(-11.4147391200156,-14.3739130003505,
118.644102382187)) ;
#158687 = CARTESIAN_POINT('Ctrl Pts',(-11.3404625025784,-14.4775305035498,
118.382452018192)) ;
#158688 = CARTESIAN_POINT('Ctrl Pts',(-11.3349477261256,-14.4037037065639,
118.365654899236)) ;
#158689 = CARTESIAN_POINT('Ctrl Pts',(-11.4087515646572,-14.403703711016,
118.341423842661)) ;
#158690 = CARTESIAN_POINT('Ctrl Pts',(-11.4825554031887,-14.4037037154681,
118.317192786086)) ;
#158691 = CARTESIAN_POINT('Ctrl Pts',(-11.4880701796416,-14.477530512454,
118.333989905042)) ;
#158692 = CARTESIAN_POINT('Ctrl Pts',(-11.4935849560945,-14.5513573094398,
118.350787023998)) ;
#158693 = CARTESIAN_POINT('Ctrl Pts',(-11.4197811175629,-14.5513573049878,
118.375018080573)) ;
#158694 = CARTESIAN_POINT('Ctrl Pts',(-11.3459772790313,-14.5513573005357,
118.399249137148)) ;
#158695 = CARTESIAN_POINT('Ctrl Pts',(-11.3404625025784,-14.4775305035498,
118.382452018192)) ;
#158696 = CARTESIAN_POINT('Ctrl Pts',(-11.2600762837107,-14.5050608269986,
118.101928838668)) ;
#158697 = CARTESIAN_POINT('Ctrl Pts',(-11.2609046322842,-14.4292041443238,
118.104451855268)) ;
#158698 = CARTESIAN_POINT('Ctrl Pts',(-11.334708467639,-14.4292041439296,
118.080220789018)) ;
#158699 = CARTESIAN_POINT('Ctrl Pts',(-11.4085123029939,-14.4292041435354,
118.055989722767)) ;
#158700 = CARTESIAN_POINT('Ctrl Pts',(-11.4076839544204,-14.5050608262101,
118.053466706166)) ;
#158701 = CARTESIAN_POINT('Ctrl Pts',(-11.4068556058469,-14.5809175088849,
118.050943689565)) ;
#158702 = CARTESIAN_POINT('Ctrl Pts',(-11.333051770492,-14.5809175092791,
118.075174755816)) ;
#158703 = CARTESIAN_POINT('Ctrl Pts',(-11.2592479351372,-14.5809175096733,
118.099405822067)) ;
#158704 = CARTESIAN_POINT('Ctrl Pts',(-11.2600762837107,-14.5050608269986,
118.101928838668)) ;
#158705 = CARTESIAN_POINT('Ctrl Pts',(-11.1816706187826,-14.4551363613954,
117.827909095909)) ;
#158706 = CARTESIAN_POINT('Ctrl Pts',(-11.1887030165374,-14.3826564737513,
117.84932864541)) ;
#158707 = CARTESIAN_POINT('Ctrl Pts',(-11.2625068504305,-14.3826564648488,
117.825097574707)) ;
#158708 = CARTESIAN_POINT('Ctrl Pts',(-11.3363106843237,-14.3826564559462,
117.800866504004)) ;
#158709 = CARTESIAN_POINT('Ctrl Pts',(-11.3292782865689,-14.4551363435903,
117.779446954503)) ;
#158710 = CARTESIAN_POINT('Ctrl Pts',(-11.3222458888142,-14.5276162312344,
117.758027405002)) ;
#158711 = CARTESIAN_POINT('Ctrl Pts',(-11.248442054921,-14.5276162401369,
117.782258475705)) ;
#158712 = CARTESIAN_POINT('Ctrl Pts',(-11.1746382210279,-14.5276162490395,
117.806489546408)) ;
#158713 = CARTESIAN_POINT('Ctrl Pts',(-11.1816706187826,-14.4551363613954,
117.827909095909)) ;
#158714 = CARTESIAN_POINT('Ctrl Pts',(-11.1096219883487,-14.3298705824412,
117.57276605832)) ;
#158715 = CARTESIAN_POINT('Ctrl Pts',(-11.122433722577,-14.2660313750253,
117.611788534437)) ;
#158716 = CARTESIAN_POINT('Ctrl Pts',(-11.1962375547277,-14.2660313525063,
117.587557458426)) ;
#158717 = CARTESIAN_POINT('Ctrl Pts',(-11.2700413868783,-14.2660313299873,
117.563326382416)) ;
#158718 = CARTESIAN_POINT('Ctrl Pts',(-11.25722965265,-14.3298705374032,117.524303906299)) ;
#158719 = CARTESIAN_POINT('Ctrl Pts',(-11.2444179184216,-14.3937097448191,
117.485281430183)) ;
#158720 = CARTESIAN_POINT('Ctrl Pts',(-11.1706140862709,-14.3937097673381,
117.509512506193)) ;
#158721 = CARTESIAN_POINT('Ctrl Pts',(-11.0968102541203,-14.3937097898571,
117.533743582204)) ;
#158722 = CARTESIAN_POINT('Ctrl Pts',(-11.1096219883487,-14.3298705824412,
117.57276605832)) ;
#158723 = CARTESIAN_POINT('Ctrl Pts',(-11.0516186729526,-14.1407879039854,
117.36082074906)) ;
#158724 = CARTESIAN_POINT('Ctrl Pts',(-11.0692285186037,-14.0900585571138,
117.41445749853)) ;
#158725 = CARTESIAN_POINT('Ctrl Pts',(-11.1430323516223,-14.090058520559,
117.390226425163)) ;
#158726 = CARTESIAN_POINT('Ctrl Pts',(-11.2168361846408,-14.0900584840042,
117.365995351797)) ;
#158727 = CARTESIAN_POINT('Ctrl Pts',(-11.1992263389897,-14.1407878308758,
117.312358602326)) ;
#158728 = CARTESIAN_POINT('Ctrl Pts',(-11.1816164933386,-14.1915171777474,
117.258721852855)) ;
#158729 = CARTESIAN_POINT('Ctrl Pts',(-11.10781266032,-14.1915172143022,117.282952926222)) ;
#158730 = CARTESIAN_POINT('Ctrl Pts',(-11.0340088273015,-14.191517250857,
117.307183999589)) ;
#158731 = CARTESIAN_POINT('Ctrl Pts',(-11.0516186729526,-14.1407879039854,
117.36082074906)) ;
#158732 = CARTESIAN_POINT('Ctrl Pts',(-11.01133249899,-13.8991517087972,117.202620381188)) ;
#158733 = CARTESIAN_POINT('Ctrl Pts',(-11.0325150051225,-13.8652196589451,
117.267138878212)) ;
#158734 = CARTESIAN_POINT('Ctrl Pts',(-11.1063188402424,-13.8652196069501,
117.242907811245)) ;
#158735 = CARTESIAN_POINT('Ctrl Pts',(-11.1801226753623,-13.865219554955,
117.218676744278)) ;
#158736 = CARTESIAN_POINT('Ctrl Pts',(-11.1589401692297,-13.8991516048072,
117.154158247255)) ;
#158737 = CARTESIAN_POINT('Ctrl Pts',(-11.1377576630972,-13.9330836546593,
117.089639750231)) ;
#158738 = CARTESIAN_POINT('Ctrl Pts',(-11.0639538279773,-13.9330837066543,
117.113870817198)) ;
#158739 = CARTESIAN_POINT('Ctrl Pts',(-10.9901499928574,-13.9330837586493,
117.138101884165)) ;
#158740 = CARTESIAN_POINT('Ctrl Pts',(-11.01133249899,-13.8991517087972,117.202620381188)) ;
#158741 = CARTESIAN_POINT('Ctrl Pts',(-10.9929531483878,-13.622377664187,
117.111093121158)) ;
#158742 = CARTESIAN_POINT('Ctrl Pts',(-11.0161851111488,-13.6077202458349,
117.18185393257)) ;
#158743 = CARTESIAN_POINT('Ctrl Pts',(-11.0899889503916,-13.6077201796241,
117.157622878161)) ;
#158744 = CARTESIAN_POINT('Ctrl Pts',(-11.1637927896344,-13.6077201134133,
117.133391823752)) ;
#158745 = CARTESIAN_POINT('Ctrl Pts',(-11.1405608268735,-13.6223775317654,
117.062631012341)) ;
#158746 = CARTESIAN_POINT('Ctrl Pts',(-11.1173288641125,-13.6370349501174,
116.991870200929)) ;
#158747 = CARTESIAN_POINT('Ctrl Pts',(-11.0435250248697,-13.6370350163283,
117.016101255338)) ;
#158748 = CARTESIAN_POINT('Ctrl Pts',(-10.9697211856269,-13.6370350825391,
117.040332309746)) ;
#158749 = CARTESIAN_POINT('Ctrl Pts',(-10.9929531483878,-13.622377664187,
117.111093121158)) ;
#158750 = CARTESIAN_POINT('Ctrl Pts',(-10.9984700935864,-13.3324243748073,
117.092526186947)) ;
#158751 = CARTESIAN_POINT('Ctrl Pts',(-11.0220823143521,-13.3379896350766,
117.164445203023)) ;
#158752 = CARTESIAN_POINT('Ctrl Pts',(-11.0958861594165,-13.3379895606869,
117.140214166346)) ;
#158753 = CARTESIAN_POINT('Ctrl Pts',(-11.1696900044808,-13.3379894862972,
117.115983129668)) ;
#158754 = CARTESIAN_POINT('Ctrl Pts',(-11.1460777837151,-13.3324242260279,
117.044064113592)) ;
#158755 = CARTESIAN_POINT('Ctrl Pts',(-11.1224655629494,-13.3268589657586,
116.972145097516)) ;
#158756 = CARTESIAN_POINT('Ctrl Pts',(-11.0486617178851,-13.3268590401483,
116.996376134193)) ;
#158757 = CARTESIAN_POINT('Ctrl Pts',(-10.9748578728207,-13.326859114538,
117.020607170871)) ;
#158758 = CARTESIAN_POINT('Ctrl Pts',(-10.9984700935864,-13.3324243748073,
117.092526186947)) ;
#158759 = CARTESIAN_POINT('Ctrl Pts',(-11.0281068838988,-13.0478498918573,
117.147341996027)) ;
#158760 = CARTESIAN_POINT('Ctrl Pts',(-11.0504177704374,-13.0732913047775,
117.215297358159)) ;
#158761 = CARTESIAN_POINT('Ctrl Pts',(-11.1242216223397,-13.073291227464,
117.191066342309)) ;
#158762 = CARTESIAN_POINT('Ctrl Pts',(-11.198025474242,-13.0732911501505,
117.166835326459)) ;
#158763 = CARTESIAN_POINT('Ctrl Pts',(-11.1757145877034,-13.0478497372302,
117.098879964327)) ;
#158764 = CARTESIAN_POINT('Ctrl Pts',(-11.1534037011648,-13.02240832431,117.030924602195)) ;
#158765 = CARTESIAN_POINT('Ctrl Pts',(-11.0795998492625,-13.0224084016235,
117.055155618045)) ;
#158766 = CARTESIAN_POINT('Ctrl Pts',(-11.0057959973602,-13.022408478937,
117.079386633895)) ;
#158767 = CARTESIAN_POINT('Ctrl Pts',(-11.0281068838988,-13.0478498918573,
117.147341996027)) ;
#158768 = CARTESIAN_POINT('Ctrl Pts',(-11.081052628238,-12.7884262570381,
117.272939564718)) ;
#158769 = CARTESIAN_POINT('Ctrl Pts',(-11.1004376583258,-12.8320168743516,
117.331983240342)) ;
#158770 = CARTESIAN_POINT('Ctrl Pts',(-11.1742415178474,-12.8320168006288,
117.3077522477)) ;
#158771 = CARTESIAN_POINT('Ctrl Pts',(-11.248045377369,-12.8320167269059,
117.283521255057)) ;
#158772 = CARTESIAN_POINT('Ctrl Pts',(-11.2286603472812,-12.7884261095925,
117.224477579433)) ;
#158773 = CARTESIAN_POINT('Ctrl Pts',(-11.2092753171935,-12.744835492279,
117.165433903809)) ;
#158774 = CARTESIAN_POINT('Ctrl Pts',(-11.1354714576718,-12.7448355660018,
117.189664896451)) ;
#158775 = CARTESIAN_POINT('Ctrl Pts',(-11.0616675981502,-12.7448356397246,
117.213895889094)) ;
#158776 = CARTESIAN_POINT('Ctrl Pts',(-11.081052628238,-12.7884262570381,
117.272939564718)) ;
#158777 = CARTESIAN_POINT('Ctrl Pts',(-11.1532846644103,-12.5764203972658,
117.457617573228)) ;
#158778 = CARTESIAN_POINT('Ctrl Pts',(-11.1683858439302,-12.6348758868913,
117.503613331312)) ;
#158779 = CARTESIAN_POINT('Ctrl Pts',(-11.2421897101441,-12.6348758265582,
117.479382359053)) ;
#158780 = CARTESIAN_POINT('Ctrl Pts',(-11.315993576358,-12.6348757662251,
117.455151386793)) ;
#158781 = CARTESIAN_POINT('Ctrl Pts',(-11.300892396838,-12.5764202765996,
117.40915562871)) ;
#158782 = CARTESIAN_POINT('Ctrl Pts',(-11.285791217318,-12.517964786974,117.363159870627)) ;
#158783 = CARTESIAN_POINT('Ctrl Pts',(-11.2119873511042,-12.5179648473072,
117.387390842886)) ;
#158784 = CARTESIAN_POINT('Ctrl Pts',(-11.1381834848903,-12.5179649076403,
117.411621815145)) ;
#158785 = CARTESIAN_POINT('Ctrl Pts',(-11.1532846644103,-12.5764203972658,
117.457617573228)) ;
#158786 = CARTESIAN_POINT('Ctrl Pts',(-11.2410864798589,-12.4236100991773,
117.689588048581)) ;
#158787 = CARTESIAN_POINT('Ctrl Pts',(-11.2508134478998,-12.4928195575656,
117.71921482572)) ;
#158788 = CARTESIAN_POINT('Ctrl Pts',(-11.3246173196788,-12.4928195167555,
117.694983870411)) ;
#158789 = CARTESIAN_POINT('Ctrl Pts',(-11.3984211914579,-12.4928194759453,
117.670752915103)) ;
#158790 = CARTESIAN_POINT('Ctrl Pts',(-11.3886942234171,-12.423610017557,
117.641126137964)) ;
#158791 = CARTESIAN_POINT('Ctrl Pts',(-11.3789672553762,-12.3544005591686,
117.611499360826)) ;
#158792 = CARTESIAN_POINT('Ctrl Pts',(-11.3051633835971,-12.3544005999788,
117.635730316134)) ;
#158793 = CARTESIAN_POINT('Ctrl Pts',(-11.2313595118181,-12.354400640789,
117.659961271443)) ;
#158794 = CARTESIAN_POINT('Ctrl Pts',(-11.2410864798589,-12.4236100991773,
117.689588048581)) ;
#158795 = CARTESIAN_POINT('Ctrl Pts',(-11.3390837070061,-12.3419562515338,
117.95250976013)) ;
#158796 = CARTESIAN_POINT('Ctrl Pts',(-11.3427190480782,-12.4169681280718,
117.963582424484)) ;
#158797 = CARTESIAN_POINT('Ctrl Pts',(-11.4165229235351,-12.4169681124147,
117.939351480377)) ;
#158798 = CARTESIAN_POINT('Ctrl Pts',(-11.4903267989919,-12.4169680967576,
117.915120536271)) ;
#158799 = CARTESIAN_POINT('Ctrl Pts',(-11.4866914579199,-12.3419562202195,
117.904047871917)) ;
#158800 = CARTESIAN_POINT('Ctrl Pts',(-11.4830561168478,-12.2669443436815,
117.892975207564)) ;
#158801 = CARTESIAN_POINT('Ctrl Pts',(-11.4092522413909,-12.2669443593386,
117.91720615167)) ;
#158802 = CARTESIAN_POINT('Ctrl Pts',(-11.3354483659341,-12.2669443749958,
117.941437095777)) ;
#158803 = CARTESIAN_POINT('Ctrl Pts',(-11.3390837070061,-12.3419562515338,
117.95250976013)) ;
#158804 = CARTESIAN_POINT('Ctrl Pts',(-11.440496530574,-12.3379525743983,
118.225901103267)) ;
#158805 = CARTESIAN_POINT('Ctrl Pts',(-11.4377914229972,-12.4133543694812,
118.217661784115)) ;
#158806 = CARTESIAN_POINT('Ctrl Pts',(-11.5115952994,-12.4133543821139,118.193430842889)) ;
#158807 = CARTESIAN_POINT('Ctrl Pts',(-11.5853991758027,-12.4133543947465,
118.169199901664)) ;
#158808 = CARTESIAN_POINT('Ctrl Pts',(-11.5881042833795,-12.3379525996635,
118.177439220816)) ;
#158809 = CARTESIAN_POINT('Ctrl Pts',(-11.5908093909563,-12.2625508045805,
118.185678539969)) ;
#158810 = CARTESIAN_POINT('Ctrl Pts',(-11.5170055145535,-12.2625507919479,
118.209909481194)) ;
#158811 = CARTESIAN_POINT('Ctrl Pts',(-11.4432016381508,-12.2625507793153,
118.23414042242)) ;
#158812 = CARTESIAN_POINT('Ctrl Pts',(-11.440496530574,-12.3379525743983,
118.225901103267)) ;
#158813 = CARTESIAN_POINT('Ctrl Pts',(-11.5383739159563,-12.4104778611719,
118.488760855449)) ;
#158814 = CARTESIAN_POINT('Ctrl Pts',(-11.529560927282,-12.4809266819483,
118.461917916001)) ;
#158815 = CARTESIAN_POINT('Ctrl Pts',(-11.6033648018396,-12.4809267225878,
118.437686969155)) ;
#158816 = CARTESIAN_POINT('Ctrl Pts',(-11.6771686763971,-12.4809267632273,
118.413456022309)) ;
#158817 = CARTESIAN_POINT('Ctrl Pts',(-11.6859816650714,-12.4104779424509,
118.440298961757)) ;
#158818 = CARTESIAN_POINT('Ctrl Pts',(-11.6947946537456,-12.3400291216744,
118.467141901205)) ;
#158819 = CARTESIAN_POINT('Ctrl Pts',(-11.6209907791881,-12.3400290810349,
118.491372848051)) ;
#158820 = CARTESIAN_POINT('Ctrl Pts',(-11.5471869046306,-12.3400290403954,
118.515603794896)) ;
#158821 = CARTESIAN_POINT('Ctrl Pts',(-11.5383739159563,-12.4104778611719,
118.488760855449)) ;
#158822 = CARTESIAN_POINT('Ctrl Pts',(-11.6278480336845,-12.5557718304403,
118.725738663281)) ;
#158823 = CARTESIAN_POINT('Ctrl Pts',(-11.6135107689349,-12.6161812209366,
118.682069670258)) ;
#158824 = CARTESIAN_POINT('Ctrl Pts',(-11.6873146391511,-12.6161812871028,
118.65783871019)) ;
#158825 = CARTESIAN_POINT('Ctrl Pts',(-11.7611185093674,-12.6161813532691,
118.633607750121)) ;
#158826 = CARTESIAN_POINT('Ctrl Pts',(-11.7754557741171,-12.5557719627728,
118.677276743144)) ;
#158827 = CARTESIAN_POINT('Ctrl Pts',(-11.7897930388667,-12.4953625722765,
118.720945736166)) ;
#158828 = CARTESIAN_POINT('Ctrl Pts',(-11.7159891686504,-12.4953625061102,
118.745176696234)) ;
#158829 = CARTESIAN_POINT('Ctrl Pts',(-11.6421852984342,-12.495362439944,
118.769407656303)) ;
#158830 = CARTESIAN_POINT('Ctrl Pts',(-11.6278480336845,-12.5557718304403,
118.725738663281)) ;
#158831 = CARTESIAN_POINT('Ctrl Pts',(-11.7021593126348,-12.7621800376528,
118.916687014316)) ;
#158832 = CARTESIAN_POINT('Ctrl Pts',(-11.6833449736774,-12.8082681507132,
118.85938157562)) ;
#158833 = CARTESIAN_POINT('Ctrl Pts',(-11.7571488373388,-12.8082682369313,
118.835150595586)) ;
#158834 = CARTESIAN_POINT('Ctrl Pts',(-11.8309527010001,-12.8082683231495,
118.810919615553)) ;
#158835 = CARTESIAN_POINT('Ctrl Pts',(-11.8497670399575,-12.7621802100891,
118.868225054249)) ;
#158836 = CARTESIAN_POINT('Ctrl Pts',(-11.8685813789148,-12.7160920970287,
118.925530492945)) ;
#158837 = CARTESIAN_POINT('Ctrl Pts',(-11.7947775152535,-12.7160920108106,
118.949761472978)) ;
#158838 = CARTESIAN_POINT('Ctrl Pts',(-11.7209736515922,-12.7160919245924,
118.973992453012)) ;
#158839 = CARTESIAN_POINT('Ctrl Pts',(-11.7021593126348,-12.7621800376528,
118.916687014316)) ;
#158840 = CARTESIAN_POINT('Ctrl Pts',(-11.7573807659036,-13.0168738808962,
119.049290511668)) ;
#158841 = CARTESIAN_POINT('Ctrl Pts',(-11.735419427469,-13.0452490763117,
118.982399820292)) ;
#158842 = CARTESIAN_POINT('Ctrl Pts',(-11.8092232829879,-13.0452491748441,
118.958168815457)) ;
#158843 = CARTESIAN_POINT('Ctrl Pts',(-11.8830271385067,-13.0452492733765,
118.933937810623)) ;
#158844 = CARTESIAN_POINT('Ctrl Pts',(-11.9049884769414,-13.0168740779611,
119.000828501999)) ;
#158845 = CARTESIAN_POINT('Ctrl Pts',(-11.926949815376,-12.9884988825456,
119.067719193375)) ;
#158846 = CARTESIAN_POINT('Ctrl Pts',(-11.8531459598571,-12.9884987840132,
119.09195019821)) ;
#158847 = CARTESIAN_POINT('Ctrl Pts',(-11.7793421043382,-12.9884986854807,
119.116181203044)) ;
#158848 = CARTESIAN_POINT('Ctrl Pts',(-11.7573807659036,-13.0168738808962,
119.049290511668)) ;
#158849 = CARTESIAN_POINT('Ctrl Pts',(-11.7896803869344,-13.2984278863564,
119.112337306604)) ;
#158850 = CARTESIAN_POINT('Ctrl Pts',(-11.7661623960868,-13.3071879031459,
119.040705303094)) ;
#158851 = CARTESIAN_POINT('Ctrl Pts',(-11.8399662429446,-13.3071880059568,
119.01647427188)) ;
#158852 = CARTESIAN_POINT('Ctrl Pts',(-11.9137700898025,-13.3071881087676,
118.992243240665)) ;
#158853 = CARTESIAN_POINT('Ctrl Pts',(-11.9372880806501,-13.2984280919781,
119.063875244175)) ;
#158854 = CARTESIAN_POINT('Ctrl Pts',(-11.9608060714977,-13.2896680751886,
119.135507247684)) ;
#158855 = CARTESIAN_POINT('Ctrl Pts',(-11.8870022246399,-13.2896679723777,
119.159738278899)) ;
#158856 = CARTESIAN_POINT('Ctrl Pts',(-11.8131983777821,-13.2896678695669,
119.183969310113)) ;
#158857 = CARTESIAN_POINT('Ctrl Pts',(-11.7896803869344,-13.2984278863564,
119.112337306604)) ;
#158858 = CARTESIAN_POINT('Ctrl Pts',(-11.7980400482597,-13.5897265030932,
119.102308017698)) ;
#158859 = CARTESIAN_POINT('Ctrl Pts',(-11.7746375625407,-13.5781620490211,
119.031027824098)) ;
#158860 = CARTESIAN_POINT('Ctrl Pts',(-11.8484414009126,-13.5781621471943,
119.006796767037)) ;
#158861 = CARTESIAN_POINT('Ctrl Pts',(-11.9222452392845,-13.5781622453675,
118.982565709975)) ;
#158862 = CARTESIAN_POINT('Ctrl Pts',(-11.9456477250035,-13.5897266994396,
119.053845903575)) ;
#158863 = CARTESIAN_POINT('Ctrl Pts',(-11.9690502107225,-13.6012911535118,
119.125126097176)) ;
#158864 = CARTESIAN_POINT('Ctrl Pts',(-11.8952463723506,-13.6012910553386,
119.149357154237)) ;
#158865 = CARTESIAN_POINT('Ctrl Pts',(-11.8214425339787,-13.6012909571654,
119.173588211298)) ;
#158866 = CARTESIAN_POINT('Ctrl Pts',(-11.7980400482597,-13.5897265030932,
119.102308017698)) ;
#158867 = CARTESIAN_POINT('Ctrl Pts',(-11.7822956103083,-13.8688372211758,
119.018847493834)) ;
#158868 = CARTESIAN_POINT('Ctrl Pts',(-11.7606918569279,-13.8377685346258,
118.953045948613)) ;
#158869 = CARTESIAN_POINT('Ctrl Pts',(-11.8344956879977,-13.8377686202372,
118.928814869311)) ;
#158870 = CARTESIAN_POINT('Ctrl Pts',(-11.9082995190675,-13.8377687058487,
118.904583790008)) ;
#158871 = CARTESIAN_POINT('Ctrl Pts',(-11.9299032724479,-13.8688373923986,
118.97038533523)) ;
#158872 = CARTESIAN_POINT('Ctrl Pts',(-11.9515070258284,-13.8999060789486,
119.036186880451)) ;
#158873 = CARTESIAN_POINT('Ctrl Pts',(-11.8777031947586,-13.8999059933372,
119.060417959753)) ;
#158874 = CARTESIAN_POINT('Ctrl Pts',(-11.8038993636888,-13.8999059077257,
119.084649039056)) ;
#158875 = CARTESIAN_POINT('Ctrl Pts',(-11.7822956103083,-13.8688372211758,
119.018847493834)) ;
#158876 = CARTESIAN_POINT('Ctrl Pts',(-11.7444566994981,-14.1152016754008,
118.868145849198)) ;
#158877 = CARTESIAN_POINT('Ctrl Pts',(-11.7261958261659,-14.0668854985442,
118.81252617712)) ;
#158878 = CARTESIAN_POINT('Ctrl Pts',(-11.7999996517436,-14.0668855661399,
118.78829508109)) ;
#158879 = CARTESIAN_POINT('Ctrl Pts',(-11.8738034773214,-14.0668856337355,
118.764063985059)) ;
#158880 = CARTESIAN_POINT('Ctrl Pts',(-11.8920643506536,-14.1152018105922,
118.819683657137)) ;
#158881 = CARTESIAN_POINT('Ctrl Pts',(-11.9103252239859,-14.1635179874488,
118.875303329215)) ;
#158882 = CARTESIAN_POINT('Ctrl Pts',(-11.8365213984081,-14.1635179198531,
118.899534425246)) ;
#158883 = CARTESIAN_POINT('Ctrl Pts',(-11.7627175728303,-14.1635178522575,
118.923765521276)) ;
#158884 = CARTESIAN_POINT('Ctrl Pts',(-11.7444566994981,-14.1152016754008,
118.868145849198)) ;
#158885 = CARTESIAN_POINT('Ctrl Pts',(-11.6880197549201,-14.3116011164225,
118.660817745576)) ;
#158886 = CARTESIAN_POINT('Ctrl Pts',(-11.6744048444867,-14.2494997572639,
118.61934892674)) ;
#158887 = CARTESIAN_POINT('Ctrl Pts',(-11.7482086667398,-14.249499803588,
118.595117820584)) ;
#158888 = CARTESIAN_POINT('Ctrl Pts',(-11.8220124889928,-14.249499849912,
118.570886714427)) ;
#158889 = CARTESIAN_POINT('Ctrl Pts',(-11.8356273994263,-14.3116012090706,
118.612355533262)) ;
#158890 = CARTESIAN_POINT('Ctrl Pts',(-11.8492423098597,-14.3737025682292,
118.653824352097)) ;
#158891 = CARTESIAN_POINT('Ctrl Pts',(-11.7754384876066,-14.3737025219051,
118.678055458254)) ;
#158892 = CARTESIAN_POINT('Ctrl Pts',(-11.7016346653535,-14.3737024755811,
118.702286564411)) ;
#158893 = CARTESIAN_POINT('Ctrl Pts',(-11.6880197549201,-14.3116011164225,
118.660817745576)) ;
#158894 = CARTESIAN_POINT('Ctrl Pts',(-11.6176369249549,-14.4442909382302,
118.410962690409)) ;
#158895 = CARTESIAN_POINT('Ctrl Pts',(-11.6096496641421,-14.3728313741273,
118.386634784156)) ;
#158896 = CARTESIAN_POINT('Ctrl Pts',(-11.6834534855113,-14.3728313982058,
118.362403675307)) ;
#158897 = CARTESIAN_POINT('Ctrl Pts',(-11.7572573068805,-14.3728314222843,
118.338172566458)) ;
#158898 = CARTESIAN_POINT('Ctrl Pts',(-11.7652445676933,-14.4442909863872,
118.362500472711)) ;
#158899 = CARTESIAN_POINT('Ctrl Pts',(-11.7732318285061,-14.5157505504901,
118.386828378965)) ;
#158900 = CARTESIAN_POINT('Ctrl Pts',(-11.6994280071369,-14.5157505264116,
118.411059487814)) ;
#158901 = CARTESIAN_POINT('Ctrl Pts',(-11.6256241857677,-14.5157505023331,
118.435290596663)) ;
#158902 = CARTESIAN_POINT('Ctrl Pts',(-11.6176369249549,-14.4442909382302,
118.410962690409)) ;
#158903 = CARTESIAN_POINT('Ctrl Pts',(-11.5390960272606,-14.5033545209173,
118.136228492371)) ;
#158904 = CARTESIAN_POINT('Ctrl Pts',(-11.5373151934807,-14.4276627971391,
118.130804361294)) ;
#158905 = CARTESIAN_POINT('Ctrl Pts',(-11.6111190162617,-14.4276628009884,
118.106573256745)) ;
#158906 = CARTESIAN_POINT('Ctrl Pts',(-11.6849228390427,-14.4276628048377,
118.082342152196)) ;
#158907 = CARTESIAN_POINT('Ctrl Pts',(-11.6867036728227,-14.5033545286159,
118.087766283273)) ;
#158908 = CARTESIAN_POINT('Ctrl Pts',(-11.6884845066026,-14.5790462523942,
118.09319041435)) ;
#158909 = CARTESIAN_POINT('Ctrl Pts',(-11.6146806838216,-14.5790462485448,
118.117421518899)) ;
#158910 = CARTESIAN_POINT('Ctrl Pts',(-11.5408768610406,-14.5790462446955,
118.141652623448)) ;
#158911 = CARTESIAN_POINT('Ctrl Pts',(-11.5390960272606,-14.5033545209173,
118.136228492371)) ;
#158912 = CARTESIAN_POINT('Ctrl Pts',(-11.4590251392824,-14.4845849990311,
117.856907062077)) ;
#158913 = CARTESIAN_POINT('Ctrl Pts',(-11.4635655267513,-14.4100891125331,
117.870736350841)) ;
#158914 = CARTESIAN_POINT('Ctrl Pts',(-11.5373693524449,-14.4100891003362,
117.846505255164)) ;
#158915 = CARTESIAN_POINT('Ctrl Pts',(-11.6111731781385,-14.4100890881394,
117.822274159486)) ;
#158916 = CARTESIAN_POINT('Ctrl Pts',(-11.6066327906697,-14.4845849746373,
117.808444870722)) ;
#158917 = CARTESIAN_POINT('Ctrl Pts',(-11.6020924032008,-14.5590808611353,
117.794615581958)) ;
#158918 = CARTESIAN_POINT('Ctrl Pts',(-11.5282885775072,-14.5590808733321,
117.818846677636)) ;
#158919 = CARTESIAN_POINT('Ctrl Pts',(-11.4544847518136,-14.559080885529,
117.843077773313)) ;
#158920 = CARTESIAN_POINT('Ctrl Pts',(-11.4590251392824,-14.4845849990311,
117.856907062077)) ;
#158921 = CARTESIAN_POINT('Ctrl Pts',(-11.383664627329,-14.3894948595566,
117.591898604544)) ;
#158922 = CARTESIAN_POINT('Ctrl Pts',(-11.3942076932912,-14.3215252408879,
117.624011083301)) ;
#158923 = CARTESIAN_POINT('Ctrl Pts',(-11.4680115230728,-14.3215252179033,
117.599780000075)) ;
#158924 = CARTESIAN_POINT('Ctrl Pts',(-11.5418153528544,-14.3215251949188,
117.575548916849)) ;
#158925 = CARTESIAN_POINT('Ctrl Pts',(-11.5312722868923,-14.3894948135875,
117.543436438092)) ;
#158926 = CARTESIAN_POINT('Ctrl Pts',(-11.52072922093,-14.4574644322562,117.511323959334)) ;
#158927 = CARTESIAN_POINT('Ctrl Pts',(-11.4469253911484,-14.4574644552408,
117.53555504256)) ;
#158928 = CARTESIAN_POINT('Ctrl Pts',(-11.3731215613668,-14.4574644782253,
117.559786125786)) ;
#158929 = CARTESIAN_POINT('Ctrl Pts',(-11.383664627329,-14.3894948595566,
117.591898604544)) ;
#158930 = CARTESIAN_POINT('Ctrl Pts',(-11.3191676650949,-14.2243477865837,
117.359917217915)) ;
#158931 = CARTESIAN_POINT('Ctrl Pts',(-11.3349653990732,-14.1678057740267,
117.40803456743)) ;
#158932 = CARTESIAN_POINT('Ctrl Pts',(-11.4087692334159,-14.1678057466232,
117.383803498096)) ;
#158933 = CARTESIAN_POINT('Ctrl Pts',(-11.4825730677585,-14.1678057192196,
117.359572428762)) ;
#158934 = CARTESIAN_POINT('Ctrl Pts',(-11.4667753337802,-14.2243477317766,
117.311455079247)) ;
#158935 = CARTESIAN_POINT('Ctrl Pts',(-11.4509775998019,-14.2808897443336,
117.263337729732)) ;
#158936 = CARTESIAN_POINT('Ctrl Pts',(-11.3771737654593,-14.2808897717371,
117.287568799066)) ;
#158937 = CARTESIAN_POINT('Ctrl Pts',(-11.3033699311166,-14.2808897991407,
117.3117998684)) ;
#158938 = CARTESIAN_POINT('Ctrl Pts',(-11.3191676650949,-14.2243477865837,
117.359917217915)) ;
#158939 = CARTESIAN_POINT('Ctrl Pts',(-11.2712397649004,-14.0022176408066,
117.178548503574)) ;
#158940 = CARTESIAN_POINT('Ctrl Pts',(-11.2911401693373,-13.9610998254784,
117.239161925192)) ;
#158941 = CARTESIAN_POINT('Ctrl Pts',(-11.3649440075334,-13.9610997980143,
117.214930867595)) ;
#158942 = CARTESIAN_POINT('Ctrl Pts',(-11.4387478457295,-13.9610997705502,
117.190699809998)) ;
#158943 = CARTESIAN_POINT('Ctrl Pts',(-11.4188474412926,-14.0022175858784,
117.13008638838)) ;
#158944 = CARTESIAN_POINT('Ctrl Pts',(-11.3989470368558,-14.0433354012065,
117.069472966763)) ;
#158945 = CARTESIAN_POINT('Ctrl Pts',(-11.3251431986597,-14.0433354286706,
117.093704024359)) ;
#158946 = CARTESIAN_POINT('Ctrl Pts',(-11.2513393604635,-14.0433354561347,
117.117935081956)) ;
#158947 = CARTESIAN_POINT('Ctrl Pts',(-11.2712397649004,-14.0022176408066,
117.178548503574)) ;
#158948 = CARTESIAN_POINT('Ctrl Pts',(-11.2436435716615,-13.738467096939,
117.059098820409)) ;
#158949 = CARTESIAN_POINT('Ctrl Pts',(-11.2662334036352,-13.7157029540504,
117.127903804218)) ;
#158950 = CARTESIAN_POINT('Ctrl Pts',(-11.3400372450378,-13.7157029304284,
117.103672756388)) ;
#158951 = CARTESIAN_POINT('Ctrl Pts',(-11.4138410864404,-13.7157029068064,
117.079441708557)) ;
#158952 = CARTESIAN_POINT('Ctrl Pts',(-11.3912512544667,-13.7384670496951,
117.010636724748)) ;
#158953 = CARTESIAN_POINT('Ctrl Pts',(-11.3686614224929,-13.7612311925838,
116.941831740939)) ;
#158954 = CARTESIAN_POINT('Ctrl Pts',(-11.2948575810903,-13.7612312162057,
116.966062788769)) ;
#158955 = CARTESIAN_POINT('Ctrl Pts',(-11.2210537396878,-13.7612312398277,
116.9902938366)) ;
#158956 = CARTESIAN_POINT('Ctrl Pts',(-11.2436435716615,-13.738467096939,
117.059098820409)) ;
#158957 = CARTESIAN_POINT('Ctrl Pts',(-11.2393171495216,-13.4497089979361,
117.010273305457)) ;
#158958 = CARTESIAN_POINT('Ctrl Pts',(-11.2629811286976,-13.4470729422015,
117.082349968154)) ;
#158959 = CARTESIAN_POINT('Ctrl Pts',(-11.336784972178,-13.4470729268746,
117.058118926652)) ;
#158960 = CARTESIAN_POINT('Ctrl Pts',(-11.4105888156583,-13.4470729115476,
117.03388788515)) ;
#158961 = CARTESIAN_POINT('Ctrl Pts',(-11.3869248364822,-13.4497089672822,
116.961811222453)) ;
#158962 = CARTESIAN_POINT('Ctrl Pts',(-11.3632608573062,-13.4523450230167,
116.889734559756)) ;
#158963 = CARTESIAN_POINT('Ctrl Pts',(-11.2894570138259,-13.4523450383437,
116.913965601258)) ;
#158964 = CARTESIAN_POINT('Ctrl Pts',(-11.2156531703456,-13.4523450536706,
116.93819664276)) ;
#158965 = CARTESIAN_POINT('Ctrl Pts',(-11.2393171495216,-13.4497089979361,
117.010273305457)) ;
#158966 = CARTESIAN_POINT('Ctrl Pts',(-11.2592549423813,-13.1612741016994,
117.035679695456)) ;
#158967 = CARTESIAN_POINT('Ctrl Pts',(-11.2822932686128,-13.1787740076572,
117.105850720125)) ;
#158968 = CARTESIAN_POINT('Ctrl Pts',(-11.3560971128853,-13.1787739983459,
117.081619681036)) ;
#158969 = CARTESIAN_POINT('Ctrl Pts',(-11.4299009571579,-13.1787739890347,
117.057388641947)) ;
#158970 = CARTESIAN_POINT('Ctrl Pts',(-11.4068626309263,-13.161274083077,
116.987217617278)) ;
#158971 = CARTESIAN_POINT('Ctrl Pts',(-11.3838243046947,-13.1437741771192,
116.917046592609)) ;
#158972 = CARTESIAN_POINT('Ctrl Pts',(-11.3100204604222,-13.1437741864305,
116.941277631698)) ;
#158973 = CARTESIAN_POINT('Ctrl Pts',(-11.2362166161497,-13.1437741957417,
116.965508670787)) ;
#158974 = CARTESIAN_POINT('Ctrl Pts',(-11.2592549423813,-13.1612741016994,
117.035679695456)) ;
#158975 = CARTESIAN_POINT('Ctrl Pts',(-11.3028442445725,-12.8897094409154,
117.132937982061)) ;
#158976 = CARTESIAN_POINT('Ctrl Pts',(-11.3236084130691,-12.9261981229531,
117.196182289087)) ;
#158977 = CARTESIAN_POINT('Ctrl Pts',(-11.3974122571748,-12.9261981199508,
117.171951249489)) ;
#158978 = CARTESIAN_POINT('Ctrl Pts',(-11.4712161012806,-12.9261981169484,
117.147720209892)) ;
#158979 = CARTESIAN_POINT('Ctrl Pts',(-11.450451932784,-12.8897094349106,
117.084475902866)) ;
#158980 = CARTESIAN_POINT('Ctrl Pts',(-11.4296877642875,-12.8532207528728,
117.02123159584)) ;
#158981 = CARTESIAN_POINT('Ctrl Pts',(-11.3558839201817,-12.8532207558752,
117.045462635438)) ;
#158982 = CARTESIAN_POINT('Ctrl Pts',(-11.282080076076,-12.8532207588776,
117.069693675035)) ;
#158983 = CARTESIAN_POINT('Ctrl Pts',(-11.3028442445725,-12.8897094409154,
117.132937982061)) ;
#158984 = CARTESIAN_POINT('Ctrl Pts',(-11.3677649574765,-12.6562456914582,
117.295185497117)) ;
#158985 = CARTESIAN_POINT('Ctrl Pts',(-11.3847614632271,-12.7090913672215,
117.346954111247)) ;
#158986 = CARTESIAN_POINT('Ctrl Pts',(-11.4585653065822,-12.7090913678115,
117.322723069363)) ;
#158987 = CARTESIAN_POINT('Ctrl Pts',(-11.5323691499374,-12.7090913684014,
117.29849202748)) ;
#158988 = CARTESIAN_POINT('Ctrl Pts',(-11.5153726441868,-12.6562456926381,
117.24672341335)) ;
#158989 = CARTESIAN_POINT('Ctrl Pts',(-11.4983761384362,-12.6034000168748,
117.19495479922)) ;
#158990 = CARTESIAN_POINT('Ctrl Pts',(-11.4245722950811,-12.6034000162848,
117.219185841103)) ;
#158991 = CARTESIAN_POINT('Ctrl Pts',(-11.3507684517259,-12.6034000156949,
117.243416882987)) ;
#158992 = CARTESIAN_POINT('Ctrl Pts',(-11.3677649574765,-12.6562456914582,
117.295185497117)) ;
#158993 = CARTESIAN_POINT('Ctrl Pts',(-11.4498623668221,-12.4776727385034,
117.509821759606)) ;
#158994 = CARTESIAN_POINT('Ctrl Pts',(-11.4618845034565,-12.5430665367951,
117.546439247975)) ;
#158995 = CARTESIAN_POINT('Ctrl Pts',(-11.5356883461067,-12.5430665383516,
117.522208203944)) ;
#158996 = CARTESIAN_POINT('Ctrl Pts',(-11.609492188757,-12.543066539908,117.497977159914)) ;
#158997 = CARTESIAN_POINT('Ctrl Pts',(-11.5974700521225,-12.4776727416163,
117.461359671545)) ;
#158998 = CARTESIAN_POINT('Ctrl Pts',(-11.585447915488,-12.4122789433245,
117.424742183177)) ;
#158999 = CARTESIAN_POINT('Ctrl Pts',(-11.5116440728378,-12.4122789417681,
117.448973227207)) ;
#159000 = CARTESIAN_POINT('Ctrl Pts',(-11.4378402301876,-12.4122789402116,
117.473204271238)) ;
#159001 = CARTESIAN_POINT('Ctrl Pts',(-11.4498623668221,-12.4776727385034,
117.509821759606)) ;
#159002 = CARTESIAN_POINT('Ctrl Pts',(-11.5443175113425,-12.3662041520314,
117.762040087288)) ;
#159003 = CARTESIAN_POINT('Ctrl Pts',(-11.5504958939717,-12.439478800866,
117.780858443836)) ;
#159004 = CARTESIAN_POINT('Ctrl Pts',(-11.6242997363917,-12.4394788016548,
117.756627399104)) ;
#159005 = CARTESIAN_POINT('Ctrl Pts',(-11.6981035788117,-12.4394788024435,
117.732396354372)) ;
#159006 = CARTESIAN_POINT('Ctrl Pts',(-11.6919251961824,-12.3662041536089,
117.713577997825)) ;
#159007 = CARTESIAN_POINT('Ctrl Pts',(-11.6857468135531,-12.2929295047743,
117.694759641277)) ;
#159008 = CARTESIAN_POINT('Ctrl Pts',(-11.6119429711331,-12.2929295039855,
117.718990686009)) ;
#159009 = CARTESIAN_POINT('Ctrl Pts',(-11.5381391287132,-12.2929295031968,
117.743221730741)) ;
#159010 = CARTESIAN_POINT('Ctrl Pts',(-11.5443175113425,-12.3662041520314,
117.762040087288)) ;
#159011 = CARTESIAN_POINT('Ctrl Pts',(-11.6448025118947,-12.3300379060018,
118.032692201155)) ;
#159012 = CARTESIAN_POINT('Ctrl Pts',(-11.6447061301734,-12.4059457816004,
118.032398637951)) ;
#159013 = CARTESIAN_POINT('Ctrl Pts',(-11.7185099730727,-12.405945781314,
118.008167594679)) ;
#159014 = CARTESIAN_POINT('Ctrl Pts',(-11.792313815972,-12.4059457810276,
117.983936551407)) ;
#159015 = CARTESIAN_POINT('Ctrl Pts',(-11.7924101976934,-12.330037905429,
117.984230114611)) ;
#159016 = CARTESIAN_POINT('Ctrl Pts',(-11.7925065794147,-12.2541300298303,
117.984523677815)) ;
#159017 = CARTESIAN_POINT('Ctrl Pts',(-11.7187027365154,-12.2541300301167,
118.008754721086)) ;
#159018 = CARTESIAN_POINT('Ctrl Pts',(-11.6448988936161,-12.2541300304032,
118.032985764358)) ;
#159019 = CARTESIAN_POINT('Ctrl Pts',(-11.6448025118947,-12.3300379060018,
118.032692201155)) ;
#159020 = CARTESIAN_POINT('Ctrl Pts',(-11.7455128333517,-12.3719948524369,
118.303864829156)) ;
#159021 = CARTESIAN_POINT('Ctrl Pts',(-11.7391201622597,-12.4450845928375,
118.284393784512)) ;
#159022 = CARTESIAN_POINT('Ctrl Pts',(-11.8129240064551,-12.4450845931213,
118.260162745188)) ;
#159023 = CARTESIAN_POINT('Ctrl Pts',(-11.8867278506504,-12.4450845934052,
118.235931705864)) ;
#159024 = CARTESIAN_POINT('Ctrl Pts',(-11.8931205217425,-12.3719948530046,
118.255402750508)) ;
#159025 = CARTESIAN_POINT('Ctrl Pts',(-11.8995131928345,-12.298905112604,
118.274873795152)) ;
#159026 = CARTESIAN_POINT('Ctrl Pts',(-11.8257093486391,-12.2989051123201,
118.299104834476)) ;
#159027 = CARTESIAN_POINT('Ctrl Pts',(-11.7519055044438,-12.2989051120363,
118.323335873801)) ;
#159028 = CARTESIAN_POINT('Ctrl Pts',(-11.7455128333517,-12.3719948524369,
118.303864829156)) ;
#159029 = CARTESIAN_POINT('Ctrl Pts',(-11.8390028851572,-12.4886302946211,
118.553235459183)) ;
#159030 = CARTESIAN_POINT('Ctrl Pts',(-11.8268052546836,-12.5536824070631,
118.516083444983)) ;
#159031 = CARTESIAN_POINT('Ctrl Pts',(-11.900609100121,-12.5536824104958,
118.491852409442)) ;
#159032 = CARTESIAN_POINT('Ctrl Pts',(-11.9744129455585,-12.5536824139286,
118.467621373901)) ;
#159033 = CARTESIAN_POINT('Ctrl Pts',(-11.9866105760321,-12.4886303014866,
118.504773388101)) ;
#159034 = CARTESIAN_POINT('Ctrl Pts',(-11.9988082065056,-12.4235781890446,
118.541925402301)) ;
#159035 = CARTESIAN_POINT('Ctrl Pts',(-11.9250043610682,-12.4235781856119,
118.566156437842)) ;
#159036 = CARTESIAN_POINT('Ctrl Pts',(-11.8512005156307,-12.4235781821791,
118.590387473383)) ;
#159037 = CARTESIAN_POINT('Ctrl Pts',(-11.8390028851572,-12.4886302946211,
118.553235459183)) ;
#159038 = CARTESIAN_POINT('Ctrl Pts',(-11.9200724717719,-12.6716133926028,
118.764723942327)) ;
#159039 = CARTESIAN_POINT('Ctrl Pts',(-11.902929845151,-12.7239835426952,
118.712510267852)) ;
#159040 = CARTESIAN_POINT('Ctrl Pts',(-11.9767336915948,-12.7239835519862,
118.688279235376)) ;
#159041 = CARTESIAN_POINT('Ctrl Pts',(-12.0505375380386,-12.7239835612772,
118.6640482029)) ;
#159042 = CARTESIAN_POINT('Ctrl Pts',(-12.0676801646595,-12.6716134111847,
118.716261877375)) ;
#159043 = CARTESIAN_POINT('Ctrl Pts',(-12.0848227912804,-12.6192432610923,
118.768475551851)) ;
#159044 = CARTESIAN_POINT('Ctrl Pts',(-12.0110189448367,-12.6192432518013,
118.792706584326)) ;
#159045 = CARTESIAN_POINT('Ctrl Pts',(-11.9372150983929,-12.6192432425104,
118.816937616802)) ;
#159046 = CARTESIAN_POINT('Ctrl Pts',(-11.9200724717719,-12.6716133926028,
118.764723942327)) ;
#159047 = CARTESIAN_POINT('Ctrl Pts',(-11.983729776495,-12.9096205473869,
118.922975846097)) ;
#159048 = CARTESIAN_POINT('Ctrl Pts',(-11.9628548652098,-12.9454485292725,
118.859394234908)) ;
#159049 = CARTESIAN_POINT('Ctrl Pts',(-12.0366587120697,-12.9454485486713,
118.835163203699)) ;
#159050 = CARTESIAN_POINT('Ctrl Pts',(-12.1104625589295,-12.9454485680701,
118.810932172491)) ;
#159051 = CARTESIAN_POINT('Ctrl Pts',(-12.1313374702147,-12.9096205861845,
118.874513783679)) ;
#159052 = CARTESIAN_POINT('Ctrl Pts',(-12.1522123814999,-12.8737926042989,
118.938095394868)) ;
#159053 = CARTESIAN_POINT('Ctrl Pts',(-12.07840853464,-12.8737925849001,118.962326426077)) ;
#159054 = CARTESIAN_POINT('Ctrl Pts',(-12.0046046877801,-12.8737925655013,
118.986557457285)) ;
#159055 = CARTESIAN_POINT('Ctrl Pts',(-11.983729776495,-12.9096205473869,
118.922975846097)) ;
#159056 = CARTESIAN_POINT('Ctrl Pts',(-12.0254107822208,-13.1819739695916,
119.014592567458)) ;
#159057 = CARTESIAN_POINT('Ctrl Pts',(-12.0023267784959,-13.1988376121803,
118.944282417269)) ;
#159058 = CARTESIAN_POINT('Ctrl Pts',(-12.0761306240772,-13.1988376406376,
118.920051382166)) ;
#159059 = CARTESIAN_POINT('Ctrl Pts',(-12.1499344696585,-13.198837669095,
118.895820347063)) ;
#159060 = CARTESIAN_POINT('Ctrl Pts',(-12.1730184733834,-13.1819740265063,
118.966130497253)) ;
#159061 = CARTESIAN_POINT('Ctrl Pts',(-12.1961024771082,-13.1651103839176,
119.036440647442)) ;
#159062 = CARTESIAN_POINT('Ctrl Pts',(-12.122298631527,-13.1651103554602,
119.060671682545)) ;
#159063 = CARTESIAN_POINT('Ctrl Pts',(-12.0484947859457,-13.1651103270029,
119.084902717648)) ;
#159064 = CARTESIAN_POINT('Ctrl Pts',(-12.0254107822208,-13.1819739695916,
119.014592567458)) ;
#159065 = CARTESIAN_POINT('Ctrl Pts',(-12.0436296355972,-13.4720244815185,
119.034627026831)) ;
#159066 = CARTESIAN_POINT('Ctrl Pts',(-12.0199739180033,-13.4686610544737,
118.962575528604)) ;
#159067 = CARTESIAN_POINT('Ctrl Pts',(-12.0937777610834,-13.4686610921263,
118.938344485883)) ;
#159068 = CARTESIAN_POINT('Ctrl Pts',(-12.1675816041635,-13.4686611297789,
118.914113443162)) ;
#159069 = CARTESIAN_POINT('Ctrl Pts',(-12.1912373217574,-13.4720245568238,
118.986164941389)) ;
#159070 = CARTESIAN_POINT('Ctrl Pts',(-12.2148930393512,-13.4753879838686,
119.058216439616)) ;
#159071 = CARTESIAN_POINT('Ctrl Pts',(-12.1410891962711,-13.475387946216,
119.082447482337)) ;
#159072 = CARTESIAN_POINT('Ctrl Pts',(-12.067285353191,-13.4753879085634,
119.106678525058)) ;
#159073 = CARTESIAN_POINT('Ctrl Pts',(-12.0436296355972,-13.4720244815185,
119.034627026831)) ;
#159074 = CARTESIAN_POINT('Ctrl Pts',(-12.0374852966316,-13.7591219512168,
118.980348270067)) ;
#159075 = CARTESIAN_POINT('Ctrl Pts',(-12.01496020499,-13.7357085596368,118.911740476252)) ;
#159076 = CARTESIAN_POINT('Ctrl Pts',(-12.0887640440176,-13.7357086049052,
118.887509421188)) ;
#159077 = CARTESIAN_POINT('Ctrl Pts',(-12.1625678830453,-13.7357086501736,
118.863278366124)) ;
#159078 = CARTESIAN_POINT('Ctrl Pts',(-12.1850929746868,-13.7591220417536,
118.931886159939)) ;
#159079 = CARTESIAN_POINT('Ctrl Pts',(-12.2076180663284,-13.7825354333337,
119.000493953753)) ;
#159080 = CARTESIAN_POINT('Ctrl Pts',(-12.1338142273008,-13.7825353880653,
119.024725008817)) ;
#159081 = CARTESIAN_POINT('Ctrl Pts',(-12.0600103882731,-13.7825353427969,
119.048956063881)) ;
#159082 = CARTESIAN_POINT('Ctrl Pts',(-12.0374852966316,-13.7591219512168,
118.980348270067)) ;
#159083 = CARTESIAN_POINT('Ctrl Pts',(-12.0081585226799,-14.0209982570872,
118.855533677512)) ;
#159084 = CARTESIAN_POINT('Ctrl Pts',(-11.9883827926061,-13.9792670582561,
118.795299995598)) ;
#159085 = CARTESIAN_POINT('Ctrl Pts',(-12.0621866264462,-13.9792671054372,
118.771068924733)) ;
#159086 = CARTESIAN_POINT('Ctrl Pts',(-12.1359904602863,-13.9792671526183,
118.746837853868)) ;
#159087 = CARTESIAN_POINT('Ctrl Pts',(-12.1557661903601,-14.0209983514494,
118.807071535783)) ;
#159088 = CARTESIAN_POINT('Ctrl Pts',(-12.1755419204339,-14.0627295502805,
118.867305217698)) ;
#159089 = CARTESIAN_POINT('Ctrl Pts',(-12.1017380865938,-14.0627295030994,
118.891536288562)) ;
#159090 = CARTESIAN_POINT('Ctrl Pts',(-12.0279342527537,-14.0627294559183,
118.915767359427)) ;
#159091 = CARTESIAN_POINT('Ctrl Pts',(-12.0081585226799,-14.0209982570872,
118.855533677512)) ;
#159092 = CARTESIAN_POINT('Ctrl Pts',(-11.9589803424424,-14.2386408615737,
118.670464829268)) ;
#159093 = CARTESIAN_POINT('Ctrl Pts',(-11.9433397158785,-14.1816542557546,
118.622826005578)) ;
#159094 = CARTESIAN_POINT('Ctrl Pts',(-12.0171435445993,-14.1816542976557,
118.598594919121)) ;
#159095 = CARTESIAN_POINT('Ctrl Pts',(-12.0909473733201,-14.1816543395568,
118.574363832664)) ;
#159096 = CARTESIAN_POINT('Ctrl Pts',(-12.1065879998839,-14.2386409453758,
118.622002656354)) ;
#159097 = CARTESIAN_POINT('Ctrl Pts',(-12.1222286264478,-14.2956275511949,
118.669641480044)) ;
#159098 = CARTESIAN_POINT('Ctrl Pts',(-12.0484247977271,-14.2956275092938,
118.693872566501)) ;
#159099 = CARTESIAN_POINT('Ctrl Pts',(-11.9746209690063,-14.2956274673927,
118.718103652958)) ;
#159100 = CARTESIAN_POINT('Ctrl Pts',(-11.9589803424424,-14.2386408615737,
118.670464829268)) ;
#159101 = CARTESIAN_POINT('Ctrl Pts',(-11.8933789786321,-14.3991847031552,
118.435064542878)) ;
#159102 = CARTESIAN_POINT('Ctrl Pts',(-11.8830321664254,-14.3309065513588,
118.403549823745)) ;
#159103 = CARTESIAN_POINT('Ctrl Pts',(-11.956835989594,-14.330906583244,118.379318720377)) ;
#159104 = CARTESIAN_POINT('Ctrl Pts',(-12.0306398127626,-14.3309066151293,
118.355087617009)) ;
#159105 = CARTESIAN_POINT('Ctrl Pts',(-12.0409866249693,-14.3991847669257,
118.386602336141)) ;
#159106 = CARTESIAN_POINT('Ctrl Pts',(-12.051333437176,-14.4674629187221,
118.418117055273)) ;
#159107 = CARTESIAN_POINT('Ctrl Pts',(-11.9775296140074,-14.4674628868368,
118.442348158641)) ;
#159108 = CARTESIAN_POINT('Ctrl Pts',(-11.9037257908388,-14.4674628549516,
118.46657926201)) ;
#159109 = CARTESIAN_POINT('Ctrl Pts',(-11.8933789786321,-14.3991847031552,
118.435064542878)) ;
#159110 = CARTESIAN_POINT('Ctrl Pts',(-11.8176447978217,-14.4885294284138,
118.169014818533)) ;
#159111 = CARTESIAN_POINT('Ctrl Pts',(-11.8133025721141,-14.4139147342441,
118.155789101172)) ;
#159112 = CARTESIAN_POINT('Ctrl Pts',(-11.8871063912677,-14.4139147488746,
118.131557985575)) ;
#159113 = CARTESIAN_POINT('Ctrl Pts',(-11.9609102104214,-14.4139147635052,
118.107326869978)) ;
#159114 = CARTESIAN_POINT('Ctrl Pts',(-11.9652524361289,-14.4885294576749,
118.120552587339)) ;
#159115 = CARTESIAN_POINT('Ctrl Pts',(-11.9695946618365,-14.5631441518446,
118.1337783047)) ;
#159116 = CARTESIAN_POINT('Ctrl Pts',(-11.8957908426829,-14.563144137214,
118.158009420297)) ;
#159117 = CARTESIAN_POINT('Ctrl Pts',(-11.8219870235292,-14.5631441225835,
118.182240535894)) ;
#159118 = CARTESIAN_POINT('Ctrl Pts',(-11.8176447978217,-14.4885294284138,
118.169014818533)) ;
#159119 = CARTESIAN_POINT('Ctrl Pts',(-11.7374057481524,-14.5016597743674,
117.889145533914)) ;
#159120 = CARTESIAN_POINT('Ctrl Pts',(-11.7393932576882,-14.4260199965907,
117.895199168941)) ;
#159121 = CARTESIAN_POINT('Ctrl Pts',(-11.8131970743123,-14.4260199894703,
117.87096804564)) ;
#159122 = CARTESIAN_POINT('Ctrl Pts',(-11.8870008909365,-14.4260199823499,
117.846736922338)) ;
#159123 = CARTESIAN_POINT('Ctrl Pts',(-11.8850133814006,-14.5016597601266,
117.84068328731)) ;
#159124 = CARTESIAN_POINT('Ctrl Pts',(-11.8830258718648,-14.5772995379034,
117.834629652282)) ;
#159125 = CARTESIAN_POINT('Ctrl Pts',(-11.8092220552407,-14.5772995450237,
117.858860775584)) ;
#159126 = CARTESIAN_POINT('Ctrl Pts',(-11.7354182386166,-14.5772995521441,
117.883091898886)) ;
#159127 = CARTESIAN_POINT('Ctrl Pts',(-11.7374057481524,-14.5016597743674,
117.889145533914)) ;
#159128 = CARTESIAN_POINT('Ctrl Pts',(-11.6592539148603,-14.437009415365,
117.615605436135)) ;
#159129 = CARTESIAN_POINT('Ctrl Pts',(-11.6674351874113,-14.3657730764766,
117.640524274072)) ;
#159130 = CARTESIAN_POINT('Ctrl Pts',(-11.7412390037029,-14.3657730444813,
117.616293149758)) ;
#159131 = CARTESIAN_POINT('Ctrl Pts',(-11.8150428199945,-14.365773012486,
117.592062025443)) ;
#159132 = CARTESIAN_POINT('Ctrl Pts',(-11.8068615474435,-14.4370093513744,
117.567143187506)) ;
#159133 = CARTESIAN_POINT('Ctrl Pts',(-11.7986802748926,-14.5082456902627,
117.54222434957)) ;
#159134 = CARTESIAN_POINT('Ctrl Pts',(-11.724876458601,-14.508245722258,117.566455473884)) ;
#159135 = CARTESIAN_POINT('Ctrl Pts',(-11.6510726423094,-14.5082457542533,
117.590686598198)) ;
#159136 = CARTESIAN_POINT('Ctrl Pts',(-11.6592539148603,-14.437009415365,
117.615605436135)) ;
#159137 = CARTESIAN_POINT('Ctrl Pts',(-11.5896054471436,-14.2988734246617,
117.367922624978)) ;
#159138 = CARTESIAN_POINT('Ctrl Pts',(-11.6033967533199,-14.2371769971241,
117.40992872027)) ;
#159139 = CARTESIAN_POINT('Ctrl Pts',(-11.6772005718606,-14.237176939765,
117.385697602806)) ;
#159140 = CARTESIAN_POINT('Ctrl Pts',(-11.7510043904013,-14.2371768824059,
117.361466485342)) ;
#159141 = CARTESIAN_POINT('Ctrl Pts',(-11.7372130842249,-14.2988733099436,
117.31946039005)) ;
#159142 = CARTESIAN_POINT('Ctrl Pts',(-11.7234217780486,-14.3605697374812,
117.277454294757)) ;
#159143 = CARTESIAN_POINT('Ctrl Pts',(-11.649617959508,-14.3605697948403,
117.301685412221)) ;
#159144 = CARTESIAN_POINT('Ctrl Pts',(-11.5758141409673,-14.3605698521993,
117.325916529686)) ;
#159145 = CARTESIAN_POINT('Ctrl Pts',(-11.5896054471436,-14.2988734246617,
117.367922624978)) ;
#159146 = CARTESIAN_POINT('Ctrl Pts',(-11.5345577224684,-14.0989764690058,
117.164944532834)) ;
#159147 = CARTESIAN_POINT('Ctrl Pts',(-11.5529430146087,-14.0511462695814,
117.220943168205)) ;
#159148 = CARTESIAN_POINT('Ctrl Pts',(-11.6267468380803,-14.0511461903864,
117.19671206576)) ;
#159149 = CARTESIAN_POINT('Ctrl Pts',(-11.700550661552,-14.0511461111915,
117.172480963314)) ;
#159150 = CARTESIAN_POINT('Ctrl Pts',(-11.6821653694116,-14.0989763106159,
117.116482327944)) ;
#159151 = CARTESIAN_POINT('Ctrl Pts',(-11.6637800772713,-14.1468065100403,
117.060483692574)) ;
#159152 = CARTESIAN_POINT('Ctrl Pts',(-11.5899762537996,-14.1468065892353,
117.084714795019)) ;
#159153 = CARTESIAN_POINT('Ctrl Pts',(-11.516172430328,-14.1468066684302,
117.108945897464)) ;
#159154 = CARTESIAN_POINT('Ctrl Pts',(-11.5345577224684,-14.0989764690058,
117.164944532834)) ;
#159155 = CARTESIAN_POINT('Ctrl Pts',(-11.4980687401448,-13.8484694868484,
117.018190484838)) ;
#159156 = CARTESIAN_POINT('Ctrl Pts',(-11.5197655262105,-13.8180580458534,
117.084275396472)) ;
#159157 = CARTESIAN_POINT('Ctrl Pts',(-11.5935693565242,-13.8180579489714,
117.060044314866)) ;
#159158 = CARTESIAN_POINT('Ctrl Pts',(-11.6673731868378,-13.8180578520894,
117.035813233261)) ;
#159159 = CARTESIAN_POINT('Ctrl Pts',(-11.645676400772,-13.8484692930843,
116.969728321627)) ;
#159160 = CARTESIAN_POINT('Ctrl Pts',(-11.6239796147063,-13.8788807340793,
116.903643409994)) ;
#159161 = CARTESIAN_POINT('Ctrl Pts',(-11.5501757843926,-13.8788808309613,
116.9278744916)) ;
#159162 = CARTESIAN_POINT('Ctrl Pts',(-11.476371954079,-13.8788809278433,
116.952105573205)) ;
#159163 = CARTESIAN_POINT('Ctrl Pts',(-11.4980687401448,-13.8484694868484,
117.018190484838)) ;
#159164 = CARTESIAN_POINT('Ctrl Pts',(-11.484185252244,-13.5679794956402,
116.940440639052)) ;
#159165 = CARTESIAN_POINT('Ctrl Pts',(-11.5076170750098,-13.5571060309524,
117.011810192564)) ;
#159166 = CARTESIAN_POINT('Ctrl Pts',(-11.5814209137794,-13.5571059245038,
116.987579136714)) ;
#159167 = CARTESIAN_POINT('Ctrl Pts',(-11.6552247525489,-13.5571058180553,
116.963348080864)) ;
#159168 = CARTESIAN_POINT('Ctrl Pts',(-11.6317929297832,-13.567979282743,
116.891978527352)) ;
#159169 = CARTESIAN_POINT('Ctrl Pts',(-11.6083611070174,-13.5788527474308,
116.820608973841)) ;
#159170 = CARTESIAN_POINT('Ctrl Pts',(-11.5345572682478,-13.5788528538794,
116.844840029691)) ;
#159171 = CARTESIAN_POINT('Ctrl Pts',(-11.4607534294783,-13.578852960328,
116.869071085541)) ;
#159172 = CARTESIAN_POINT('Ctrl Pts',(-11.484185252244,-13.5679794956402,
116.940440639052)) ;
#159173 = CARTESIAN_POINT('Ctrl Pts',(-11.4942413352023,-13.2778704302602,
116.935732247541)) ;
#159174 = CARTESIAN_POINT('Ctrl Pts',(-11.5177367482968,-13.2872353982741,
117.007295486949)) ;
#159175 = CARTESIAN_POINT('Ctrl Pts',(-11.5915405960583,-13.2872352908657,
116.983064458487)) ;
#159176 = CARTESIAN_POINT('Ctrl Pts',(-11.6653444438198,-13.2872351834573,
116.958833430025)) ;
#159177 = CARTESIAN_POINT('Ctrl Pts',(-11.6418490307253,-13.2778702154433,
116.887270190616)) ;
#159178 = CARTESIAN_POINT('Ctrl Pts',(-11.6183536176309,-13.2685052474294,
116.815706951208)) ;
#159179 = CARTESIAN_POINT('Ctrl Pts',(-11.5445497698694,-13.2685053548378,
116.83993797967)) ;
#159180 = CARTESIAN_POINT('Ctrl Pts',(-11.4707459221079,-13.2685054622462,
116.864169008132)) ;
#159181 = CARTESIAN_POINT('Ctrl Pts',(-11.4942413352023,-13.2778704302602,
116.935732247541)) ;
#159182 = CARTESIAN_POINT('Ctrl Pts',(-11.5283649580948,-12.9966579805532,
117.004198786349)) ;
#159183 = CARTESIAN_POINT('Ctrl Pts',(-11.5502466916195,-13.0256699682594,
117.070847018154)) ;
#159184 = CARTESIAN_POINT('Ctrl Pts',(-11.6240505481439,-13.025669868452,
117.046616016382)) ;
#159185 = CARTESIAN_POINT('Ctrl Pts',(-11.6978544046683,-13.0256697686447,
117.02238501461)) ;
#159186 = CARTESIAN_POINT('Ctrl Pts',(-11.6759726711435,-12.9966577809386,
116.955736782806)) ;
#159187 = CARTESIAN_POINT('Ctrl Pts',(-11.6540909376187,-12.9676457932324,
116.889088551001)) ;
#159188 = CARTESIAN_POINT('Ctrl Pts',(-11.5802870810944,-12.9676458930398,
116.913319552772)) ;
#159189 = CARTESIAN_POINT('Ctrl Pts',(-11.50648322457,-12.9676459928471,116.937550554544)) ;
#159190 = CARTESIAN_POINT('Ctrl Pts',(-11.5283649580948,-12.9966579805532,
117.004198786349)) ;
#159191 = CARTESIAN_POINT('Ctrl Pts',(-11.5851655684408,-12.7449733317735,
117.141625652285)) ;
#159192 = CARTESIAN_POINT('Ctrl Pts',(-11.6038505096671,-12.7916002389954,
117.19853697052)) ;
#159193 = CARTESIAN_POINT('Ctrl Pts',(-11.6776543737352,-12.7916001552318,
117.174305991725)) ;
#159194 = CARTESIAN_POINT('Ctrl Pts',(-11.7514582378032,-12.7916000714681,
117.15007501293)) ;
#159195 = CARTESIAN_POINT('Ctrl Pts',(-11.7327732965769,-12.7449731642463,
117.093163694695)) ;
#159196 = CARTESIAN_POINT('Ctrl Pts',(-11.7140883553506,-12.6983462570244,
117.03625237646)) ;
#159197 = CARTESIAN_POINT('Ctrl Pts',(-11.6402844912826,-12.698346340788,
117.060483355255)) ;
#159198 = CARTESIAN_POINT('Ctrl Pts',(-11.5664806272145,-12.6983464245516,
117.08471433405)) ;
#159199 = CARTESIAN_POINT('Ctrl Pts',(-11.5851655684408,-12.7449733317735,
117.141625652285)) ;
#159200 = CARTESIAN_POINT('Ctrl Pts',(-11.6608769322514,-12.5424420519023,
117.336783089927)) ;
#159201 = CARTESIAN_POINT('Ctrl Pts',(-11.6750372583365,-12.6032785791417,
117.379913160438)) ;
#159202 = CARTESIAN_POINT('Ctrl Pts',(-11.7488411279863,-12.6032785174952,
117.355682198644)) ;
#159203 = CARTESIAN_POINT('Ctrl Pts',(-11.8226449976362,-12.6032784558487,
117.33145123685)) ;
#159204 = CARTESIAN_POINT('Ctrl Pts',(-11.8084846715511,-12.5424419286094,
117.28832116634)) ;
#159205 = CARTESIAN_POINT('Ctrl Pts',(-11.794324345466,-12.48160540137,117.245191095829)) ;
#159206 = CARTESIAN_POINT('Ctrl Pts',(-11.7205204758162,-12.4816054630165,
117.269422057623)) ;
#159207 = CARTESIAN_POINT('Ctrl Pts',(-11.6467166061663,-12.481605524663,
117.293653019416)) ;
#159208 = CARTESIAN_POINT('Ctrl Pts',(-11.6608769322514,-12.5424420519023,
117.336783089927)) ;
#159209 = CARTESIAN_POINT('Ctrl Pts',(-11.751128641274,-12.4024494998622,
117.576178163021)) ;
#159210 = CARTESIAN_POINT('Ctrl Pts',(-11.7597435525524,-12.4731509953254,
117.602417794707)) ;
#159211 = CARTESIAN_POINT('Ctrl Pts',(-11.8335474252807,-12.4731509596195,
117.57818684229)) ;
#159212 = CARTESIAN_POINT('Ctrl Pts',(-11.9073512980089,-12.4731509239136,
117.553955889872)) ;
#159213 = CARTESIAN_POINT('Ctrl Pts',(-11.8987363867305,-12.4024494284505,
117.527716258186)) ;
#159214 = CARTESIAN_POINT('Ctrl Pts',(-11.8901214754521,-12.3317479329873,
117.5014766265)) ;
#159215 = CARTESIAN_POINT('Ctrl Pts',(-11.8163176027239,-12.3317479686932,
117.525707578917)) ;
#159216 = CARTESIAN_POINT('Ctrl Pts',(-11.7425137299956,-12.331748004399,
117.549938531335)) ;
#159217 = CARTESIAN_POINT('Ctrl Pts',(-11.751128641274,-12.4024494998622,
117.576178163021)) ;
#159218 = CARTESIAN_POINT('Ctrl Pts',(-11.849749431196,-12.33540698977,117.841192600071)) ;
#159219 = CARTESIAN_POINT('Ctrl Pts',(-11.8522235854152,-12.4108950254445,
117.848728476483)) ;
#159220 = CARTESIAN_POINT('Ctrl Pts',(-11.9260274587751,-12.4108950163572,
117.824497525989)) ;
#159221 = CARTESIAN_POINT('Ctrl Pts',(-11.999831332135,-12.4108950072698,
117.800266575496)) ;
#159222 = CARTESIAN_POINT('Ctrl Pts',(-11.9973571779159,-12.3354069715953,
117.792730699084)) ;
#159223 = CARTESIAN_POINT('Ctrl Pts',(-11.9948830236967,-12.2599189359207,
117.785194822671)) ;
#159224 = CARTESIAN_POINT('Ctrl Pts',(-11.9210791503368,-12.2599189450081,
117.809425773165)) ;
#159225 = CARTESIAN_POINT('Ctrl Pts',(-11.8472752769769,-12.2599189540954,
117.833656723658)) ;
#159226 = CARTESIAN_POINT('Ctrl Pts',(-11.849749431196,-12.33540698977,117.841192600071)) ;
#159227 = CARTESIAN_POINT('Ctrl Pts',(-11.9511794851965,-12.3455818235887,
118.114616538353)) ;
#159228 = CARTESIAN_POINT('Ctrl Pts',(-11.9473106410994,-12.4204731523851,
118.102832665221)) ;
#159229 = CARTESIAN_POINT('Ctrl Pts',(-12.0211145123507,-12.4204731683141,
118.078601708306)) ;
#159230 = CARTESIAN_POINT('Ctrl Pts',(-12.0949183836021,-12.4204731842432,
118.05437075139)) ;
#159231 = CARTESIAN_POINT('Ctrl Pts',(-12.0987872276992,-12.3455818554468,
118.066154624522)) ;
#159232 = CARTESIAN_POINT('Ctrl Pts',(-12.1026560717964,-12.2706905266504,
118.077938497654)) ;
#159233 = CARTESIAN_POINT('Ctrl Pts',(-12.028852200545,-12.2706905107213,
118.10216945457)) ;
#159234 = CARTESIAN_POINT('Ctrl Pts',(-11.9550483292936,-12.2706904947923,
118.126400411485)) ;
#159235 = CARTESIAN_POINT('Ctrl Pts',(-11.9511794851965,-12.3455818235887,
118.114616538353)) ;
#159236 = CARTESIAN_POINT('Ctrl Pts',(-12.048568512048,-12.433061741337,118.375702938129)) ;
#159237 = CARTESIAN_POINT('Ctrl Pts',(-12.0386297693431,-12.5019585481824,
118.345431133076)) ;
#159238 = CARTESIAN_POINT('Ctrl Pts',(-12.1124336362693,-12.5019585842902,
118.321200162986)) ;
#159239 = CARTESIAN_POINT('Ctrl Pts',(-12.1862375031954,-12.501958620398,
118.296969192897)) ;
#159240 = CARTESIAN_POINT('Ctrl Pts',(-12.1961762459003,-12.4330618135526,
118.32724099795)) ;
#159241 = CARTESIAN_POINT('Ctrl Pts',(-12.2061149886052,-12.3641650067072,
118.357512803003)) ;
#159242 = CARTESIAN_POINT('Ctrl Pts',(-12.132311121679,-12.3641649705994,
118.381743773093)) ;
#159243 = CARTESIAN_POINT('Ctrl Pts',(-12.0585072547529,-12.3641649344917,
118.405974743183)) ;
#159244 = CARTESIAN_POINT('Ctrl Pts',(-12.048568512048,-12.433061741337,118.375702938129)) ;
#159245 = CARTESIAN_POINT('Ctrl Pts',(-12.1352985452608,-12.5907670484714,
118.604444245422)) ;
#159246 = CARTESIAN_POINT('Ctrl Pts',(-12.1200223854668,-12.6487569748398,
118.557915528971)) ;
#159247 = CARTESIAN_POINT('Ctrl Pts',(-12.193826246934,-12.6487570251188,
118.533684542254)) ;
#159248 = CARTESIAN_POINT('Ctrl Pts',(-12.2676301084012,-12.6487570753977,
118.509453555537)) ;
#159249 = CARTESIAN_POINT('Ctrl Pts',(-12.2829062681952,-12.5907671490293,
118.555982271988)) ;
#159250 = CARTESIAN_POINT('Ctrl Pts',(-12.2981824279892,-12.5327772226608,
118.60251098844)) ;
#159251 = CARTESIAN_POINT('Ctrl Pts',(-12.224378566522,-12.5327771723819,
118.626741975157)) ;
#159252 = CARTESIAN_POINT('Ctrl Pts',(-12.1505747050549,-12.5327771221029,
118.650972961874)) ;
#159253 = CARTESIAN_POINT('Ctrl Pts',(-12.1352985452608,-12.5907670484714,
118.604444245422)) ;
#159254 = CARTESIAN_POINT('Ctrl Pts',(-12.2062338243243,-12.8072730343164,
118.785110454359)) ;
#159255 = CARTESIAN_POINT('Ctrl Pts',(-12.1867142471291,-12.8502341493777,
118.725656973039)) ;
#159256 = CARTESIAN_POINT('Ctrl Pts',(-12.2605181025395,-12.8502342073388,
118.701425967874)) ;
#159257 = CARTESIAN_POINT('Ctrl Pts',(-12.33432195795,-12.8502342652999,118.677194962709)) ;
#159258 = CARTESIAN_POINT('Ctrl Pts',(-12.3538415351452,-12.8072731502386,
118.73664844403)) ;
#159259 = CARTESIAN_POINT('Ctrl Pts',(-12.3733611123405,-12.7643120351774,
118.79610192535)) ;
#159260 = CARTESIAN_POINT('Ctrl Pts',(-12.29955725693,-12.7643119772163,118.820332930515)) ;
#159261 = CARTESIAN_POINT('Ctrl Pts',(-12.2257534015195,-12.7643119192552,
118.844563935679)) ;
#159262 = CARTESIAN_POINT('Ctrl Pts',(-12.2062338243243,-12.8072730343164,
118.785110454359)) ;
#159263 = CARTESIAN_POINT('Ctrl Pts',(-12.2572961681927,-13.0681776762317,
118.90514030015)) ;
#159264 = CARTESIAN_POINT('Ctrl Pts',(-12.2349163490449,-13.0929875781858,
118.836974983176)) ;
#159265 = CARTESIAN_POINT('Ctrl Pts',(-12.308720198304,-13.0929876362341,
118.812743959275)) ;
#159266 = CARTESIAN_POINT('Ctrl Pts',(-12.3825240475632,-13.0929876942824,
118.788512935374)) ;
#159267 = CARTESIAN_POINT('Ctrl Pts',(-12.4049038667109,-13.0681777923284,
118.856678252349)) ;
#159268 = CARTESIAN_POINT('Ctrl Pts',(-12.4272836858587,-13.0433678903743,
118.924843569323)) ;
#159269 = CARTESIAN_POINT('Ctrl Pts',(-12.3534798365995,-13.043367832326,
118.949074593224)) ;
#159270 = CARTESIAN_POINT('Ctrl Pts',(-12.2796759873404,-13.0433677742776,
118.973305617125)) ;
#159271 = CARTESIAN_POINT('Ctrl Pts',(-12.2572961681927,-13.0681776762317,
118.90514030015)) ;
#159272 = CARTESIAN_POINT('Ctrl Pts',(-12.2852469770119,-13.3550287065478,
118.954680417514)) ;
#159273 = CARTESIAN_POINT('Ctrl Pts',(-12.2616180631814,-13.3598480286535,
118.882710559486)) ;
#159274 = CARTESIAN_POINT('Ctrl Pts',(-12.3354219072866,-13.3598480797462,
118.858479519887)) ;
#159275 = CARTESIAN_POINT('Ctrl Pts',(-12.4092257513917,-13.3598481308389,
118.834248480288)) ;
#159276 = CARTESIAN_POINT('Ctrl Pts',(-12.4328546652223,-13.3550288087332,
118.906218338317)) ;
#159277 = CARTESIAN_POINT('Ctrl Pts',(-12.4564835790527,-13.3502094866275,
118.978188196345)) ;
#159278 = CARTESIAN_POINT('Ctrl Pts',(-12.3826797349476,-13.3502094355348,
119.002419235944)) ;
#159279 = CARTESIAN_POINT('Ctrl Pts',(-12.3088758908424,-13.3502093844422,
119.026650275543)) ;
#159280 = CARTESIAN_POINT('Ctrl Pts',(-12.2852469770119,-13.3550287065478,
118.954680417514)) ;
#159281 = CARTESIAN_POINT('Ctrl Pts',(-12.288870726614,-13.6436167217993,
118.930470264435)) ;
#159282 = CARTESIAN_POINT('Ctrl Pts',(-12.2656825372451,-13.6282936387258,
118.859842781879)) ;
#159283 = CARTESIAN_POINT('Ctrl Pts',(-12.3394863775681,-13.6282936821549,
118.83561173076)) ;
#159284 = CARTESIAN_POINT('Ctrl Pts',(-12.413290217891,-13.6282937255841,
118.811380679642)) ;
#159285 = CARTESIAN_POINT('Ctrl Pts',(-12.43647840726,-13.6436168086577,118.882008162198)) ;
#159286 = CARTESIAN_POINT('Ctrl Pts',(-12.459666596629,-13.6589398917312,
118.952635644754)) ;
#159287 = CARTESIAN_POINT('Ctrl Pts',(-12.385862756306,-13.6589398483021,
118.976866695873)) ;
#159288 = CARTESIAN_POINT('Ctrl Pts',(-12.312058915983,-13.6589398048729,
119.001097746991)) ;
#159289 = CARTESIAN_POINT('Ctrl Pts',(-12.288870726614,-13.6436167217993,
118.930470264435)) ;
#159290 = CARTESIAN_POINT('Ctrl Pts',(-12.2688371151345,-13.9180811572707,
118.833953017997)) ;
#159291 = CARTESIAN_POINT('Ctrl Pts',(-12.2477470847811,-13.8835710604602,
118.769716189091)) ;
#159292 = CARTESIAN_POINT('Ctrl Pts',(-12.3215509228609,-13.8835710916854,
118.74548513114)) ;
#159293 = CARTESIAN_POINT('Ctrl Pts',(-12.3953547609406,-13.8835711229105,
118.721254073189)) ;
#159294 = CARTESIAN_POINT('Ctrl Pts',(-12.416444791294,-13.918081219721,118.785490902094)) ;
#159295 = CARTESIAN_POINT('Ctrl Pts',(-12.4375348216475,-13.9525913165315,
118.849727730999)) ;
#159296 = CARTESIAN_POINT('Ctrl Pts',(-12.3637309835677,-13.9525912853064,
118.873958788951)) ;
#159297 = CARTESIAN_POINT('Ctrl Pts',(-12.289927145488,-13.9525912540812,
118.898189846902)) ;
#159298 = CARTESIAN_POINT('Ctrl Pts',(-12.2688371151345,-13.9180811572707,
118.833953017997)) ;
#159299 = CARTESIAN_POINT('Ctrl Pts',(-12.2271646134758,-14.156549136634,
118.671552459278)) ;
#159300 = CARTESIAN_POINT('Ctrl Pts',(-12.2096863684391,-14.1053360637856,
118.618316545524)) ;
#159301 = CARTESIAN_POINT('Ctrl Pts',(-12.2834902059413,-14.1053360831036,
118.594085485813)) ;
#159302 = CARTESIAN_POINT('Ctrl Pts',(-12.3572940434434,-14.1053361024216,
118.569854426102)) ;
#159303 = CARTESIAN_POINT('Ctrl Pts',(-12.3747722884801,-14.1565491752701,
118.623090339857)) ;
#159304 = CARTESIAN_POINT('Ctrl Pts',(-12.3922505335167,-14.2077622481185,
118.676326253611)) ;
#159305 = CARTESIAN_POINT('Ctrl Pts',(-12.3184466960146,-14.2077622288005,
118.700557313322)) ;
#159306 = CARTESIAN_POINT('Ctrl Pts',(-12.2446428585124,-14.2077622094825,
118.724788373032)) ;
#159307 = CARTESIAN_POINT('Ctrl Pts',(-12.2271646134758,-14.156549136634,
118.671552459278)) ;
#159308 = CARTESIAN_POINT('Ctrl Pts',(-12.1674566622439,-14.3423727651068,
118.454127809899)) ;
#159309 = CARTESIAN_POINT('Ctrl Pts',(-12.1548569449561,-14.2781068691163,
118.415751104352)) ;
#159310 = CARTESIAN_POINT('Ctrl Pts',(-12.2286607833888,-14.2781068782219,
118.391520047475)) ;
#159311 = CARTESIAN_POINT('Ctrl Pts',(-12.3024646218214,-14.2781068873274,
118.367288990599)) ;
#159312 = CARTESIAN_POINT('Ctrl Pts',(-12.3150643391092,-14.342372783318,
118.405665696146)) ;
#159313 = CARTESIAN_POINT('Ctrl Pts',(-12.327664056397,-14.4066386793085,
118.444042401693)) ;
#159314 = CARTESIAN_POINT('Ctrl Pts',(-12.2538602179643,-14.406638670203,
118.468273458569)) ;
#159315 = CARTESIAN_POINT('Ctrl Pts',(-12.1800563795317,-14.4066386610974,
118.492504515446)) ;
#159316 = CARTESIAN_POINT('Ctrl Pts',(-12.1674566622439,-14.3423727651068,
118.454127809899)) ;
#159317 = CARTESIAN_POINT('Ctrl Pts',(-12.0952414310603,-14.4613427108393,
118.198784751216)) ;
#159318 = CARTESIAN_POINT('Ctrl Pts',(-12.0883974197828,-14.3886728717829,
118.177938997371)) ;
#159319 = CARTESIAN_POINT('Ctrl Pts',(-12.1622012596057,-14.3886728745372,
118.153707944729)) ;
#159320 = CARTESIAN_POINT('Ctrl Pts',(-12.2360050994286,-14.3886728772916,
118.129476892087)) ;
#159321 = CARTESIAN_POINT('Ctrl Pts',(-12.242849110706,-14.461342716348,118.150322645932)) ;
#159322 = CARTESIAN_POINT('Ctrl Pts',(-12.2496931219834,-14.5340125554044,
118.171168399777)) ;
#159323 = CARTESIAN_POINT('Ctrl Pts',(-12.1758892821606,-14.5340125526501,
118.195399452419)) ;
#159324 = CARTESIAN_POINT('Ctrl Pts',(-12.1020854423377,-14.5340125498957,
118.219630505062)) ;
#159325 = CARTESIAN_POINT('Ctrl Pts',(-12.0952414310603,-14.4613427108393,
118.198784751216)) ;
#159326 = CARTESIAN_POINT('Ctrl Pts',(-12.0156536366213,-14.5057889124528,
117.920757945584)) ;
#159327 = CARTESIAN_POINT('Ctrl Pts',(-12.0150937248393,-14.4299056340327,
117.919052544731)) ;
#159328 = CARTESIAN_POINT('Ctrl Pts',(-12.088897566724,-14.4299056336396,
117.894821498369)) ;
#159329 = CARTESIAN_POINT('Ctrl Pts',(-12.1627014086088,-14.4299056332465,
117.870590452007)) ;
#159330 = CARTESIAN_POINT('Ctrl Pts',(-12.1632613203908,-14.5057889116665,
117.87229585286)) ;
#159331 = CARTESIAN_POINT('Ctrl Pts',(-12.1638212321729,-14.5816721900866,
117.874001253712)) ;
#159332 = CARTESIAN_POINT('Ctrl Pts',(-12.0900173902881,-14.5816721904797,
117.898232300074)) ;
#159333 = CARTESIAN_POINT('Ctrl Pts',(-12.0162135484033,-14.5816721908728,
117.922463346436)) ;
#159334 = CARTESIAN_POINT('Ctrl Pts',(-12.0156536366213,-14.5057889124528,
117.920757945584)) ;
#159335 = CARTESIAN_POINT('Ctrl Pts',(-11.9363592364177,-14.4724226584541,
117.643968542152)) ;
#159336 = CARTESIAN_POINT('Ctrl Pts',(-11.9420651845438,-14.3987559090156,
117.661347939515)) ;
#159337 = CARTESIAN_POINT('Ctrl Pts',(-12.0158690276237,-14.3987559084173,
117.637116896794)) ;
#159338 = CARTESIAN_POINT('Ctrl Pts',(-12.0896728707036,-14.3987559078189,
117.612885854072)) ;
#159339 = CARTESIAN_POINT('Ctrl Pts',(-12.0839669225775,-14.4724226572574,
117.595506456708)) ;
#159340 = CARTESIAN_POINT('Ctrl Pts',(-12.0782609744514,-14.5460894066958,
117.578127059344)) ;
#159341 = CARTESIAN_POINT('Ctrl Pts',(-12.0044571313715,-14.5460894072942,
117.602358102066)) ;
#159342 = CARTESIAN_POINT('Ctrl Pts',(-11.9306532882916,-14.5460894078926,
117.626589144788)) ;
#159343 = CARTESIAN_POINT('Ctrl Pts',(-11.9363592364177,-14.4724226584541,
117.643968542152)) ;
#159344 = CARTESIAN_POINT('Ctrl Pts',(-11.8623371282566,-14.3630839653471,
117.382899183667)) ;
#159345 = CARTESIAN_POINT('Ctrl Pts',(-11.8739575043683,-14.2969416918189,
117.418292974314)) ;
#159346 = CARTESIAN_POINT('Ctrl Pts',(-11.9477613484913,-14.2969416928651,
117.394061934769)) ;
#159347 = CARTESIAN_POINT('Ctrl Pts',(-12.0215651926142,-14.2969416939113,
117.369830895225)) ;
#159348 = CARTESIAN_POINT('Ctrl Pts',(-12.0099448165026,-14.3630839674395,
117.334437104578)) ;
#159349 = CARTESIAN_POINT('Ctrl Pts',(-11.9983244403909,-14.4292262409677,
117.299043313931)) ;
#159350 = CARTESIAN_POINT('Ctrl Pts',(-11.9245205962679,-14.4292262399216,
117.323274353476)) ;
#159351 = CARTESIAN_POINT('Ctrl Pts',(-11.850716752145,-14.4292262388754,
117.34750539302)) ;
#159352 = CARTESIAN_POINT('Ctrl Pts',(-11.8623371282566,-14.3630839653471,
117.382899183667)) ;
#159353 = CARTESIAN_POINT('Ctrl Pts',(-11.8008173863079,-14.1865023299291,
117.160124591948)) ;
#159354 = CARTESIAN_POINT('Ctrl Pts',(-11.8174833681576,-14.132592518795,
117.210886483552)) ;
#159355 = CARTESIAN_POINT('Ctrl Pts',(-11.8912872123,-14.1325925211688,117.186655444066)) ;
#159356 = CARTESIAN_POINT('Ctrl Pts',(-11.9650910564424,-14.1325925235426,
117.162424404581)) ;
#159357 = CARTESIAN_POINT('Ctrl Pts',(-11.9484250745928,-14.1865023346767,
117.111662512977)) ;
#159358 = CARTESIAN_POINT('Ctrl Pts',(-11.9317590927431,-14.2404121458108,
117.060900621374)) ;
#159359 = CARTESIAN_POINT('Ctrl Pts',(-11.8579552486006,-14.240412143437,
117.085131660859)) ;
#159360 = CARTESIAN_POINT('Ctrl Pts',(-11.7841514044582,-14.2404121410632,
117.109362700344)) ;
#159361 = CARTESIAN_POINT('Ctrl Pts',(-11.8008173863079,-14.1865023299291,
117.160124591948)) ;
#159362 = CARTESIAN_POINT('Ctrl Pts',(-11.7563748042704,-13.9552367476643,
116.989354134913)) ;
#159363 = CARTESIAN_POINT('Ctrl Pts',(-11.7769014328037,-13.91739633188,117.051874933419)) ;
#159364 = CARTESIAN_POINT('Ctrl Pts',(-11.8507052765402,-13.917396334111,
117.027643892697)) ;
#159365 = CARTESIAN_POINT('Ctrl Pts',(-11.9245091202767,-13.9173963363419,
117.003412851975)) ;
#159366 = CARTESIAN_POINT('Ctrl Pts',(-11.9039824917435,-13.9552367521262,
116.94089205347)) ;
#159367 = CARTESIAN_POINT('Ctrl Pts',(-11.8834558632103,-13.9930771679105,
116.878371254964)) ;
#159368 = CARTESIAN_POINT('Ctrl Pts',(-11.8096520194738,-13.9930771656796,
116.902602295686)) ;
#159369 = CARTESIAN_POINT('Ctrl Pts',(-11.7358481757372,-13.9930771634486,
116.926833336408)) ;
#159370 = CARTESIAN_POINT('Ctrl Pts',(-11.7563748042704,-13.9552367476643,
116.989354134913)) ;
#159371 = CARTESIAN_POINT('Ctrl Pts',(-11.7329833978953,-13.6844063432408,
116.882563304078)) ;
#159372 = CARTESIAN_POINT('Ctrl Pts',(-11.7559091967072,-13.6654217630373,
116.952391588213)) ;
#159373 = CARTESIAN_POINT('Ctrl Pts',(-11.8297130399375,-13.6654217622708,
116.928160545949)) ;
#159374 = CARTESIAN_POINT('Ctrl Pts',(-11.9035168831679,-13.6654217615044,
116.903929503685)) ;
#159375 = CARTESIAN_POINT('Ctrl Pts',(-11.8805910843559,-13.6844063417079,
116.834101219551)) ;
#159376 = CARTESIAN_POINT('Ctrl Pts',(-11.857665285544,-13.7033909219114,
116.764272935417)) ;
#159377 = CARTESIAN_POINT('Ctrl Pts',(-11.7838614423137,-13.7033909226779,
116.78850397768)) ;
#159378 = CARTESIAN_POINT('Ctrl Pts',(-11.7100575990833,-13.7033909234443,
116.812735019944)) ;
#159379 = CARTESIAN_POINT('Ctrl Pts',(-11.7329833978953,-13.6844063432408,
116.882563304078)) ;
#159380 = CARTESIAN_POINT('Ctrl Pts',(-11.7332475390205,-13.395616216205,
116.847967590773)) ;
#159381 = CARTESIAN_POINT('Ctrl Pts',(-11.7569209111697,-13.3967687826649,
116.920072862757)) ;
#159382 = CARTESIAN_POINT('Ctrl Pts',(-11.8307247544843,-13.3967687773501,
116.89584182075)) ;
#159383 = CARTESIAN_POINT('Ctrl Pts',(-11.9045285977989,-13.3967687720353,
116.871610778744)) ;
#159384 = CARTESIAN_POINT('Ctrl Pts',(-11.8808552256497,-13.3956162055754,
116.799505506759)) ;
#159385 = CARTESIAN_POINT('Ctrl Pts',(-11.8571818535005,-13.3944636391155,
116.727400234774)) ;
#159386 = CARTESIAN_POINT('Ctrl Pts',(-11.7833780101859,-13.3944636444303,
116.751631276781)) ;
#159387 = CARTESIAN_POINT('Ctrl Pts',(-11.7095741668713,-13.3944636497451,
116.775862318788)) ;
#159388 = CARTESIAN_POINT('Ctrl Pts',(-11.7332475390205,-13.395616216205,
116.847967590773)) ;
#159389 = CARTESIAN_POINT('Ctrl Pts',(-11.7576801957441,-13.1080920804484,
116.886949996486)) ;
#159390 = CARTESIAN_POINT('Ctrl Pts',(-11.7804153341548,-13.1293224287734,
116.956197559996)) ;
#159391 = CARTESIAN_POINT('Ctrl Pts',(-11.8542191783384,-13.1293224180304,
116.931966520636)) ;
#159392 = CARTESIAN_POINT('Ctrl Pts',(-11.9280230225219,-13.1293224072874,
116.907735481276)) ;
#159393 = CARTESIAN_POINT('Ctrl Pts',(-11.9052878841112,-13.1080920589624,
116.838487917765)) ;
#159394 = CARTESIAN_POINT('Ctrl Pts',(-11.8825527457004,-13.0868617106374,
116.769240354255)) ;
#159395 = CARTESIAN_POINT('Ctrl Pts',(-11.8087489015169,-13.0868617213805,
116.793471393615)) ;
#159396 = CARTESIAN_POINT('Ctrl Pts',(-11.7349450573333,-13.0868617321235,
116.817702432975)) ;
#159397 = CARTESIAN_POINT('Ctrl Pts',(-11.7576801957441,-13.1080920804484,
116.886949996486)) ;
#159398 = CARTESIAN_POINT('Ctrl Pts',(-11.8057887216514,-12.8414911099526,
116.997851240026)) ;
#159399 = CARTESIAN_POINT('Ctrl Pts',(-11.8259351949678,-12.8813675737048,
117.059214147502)) ;
#159400 = CARTESIAN_POINT('Ctrl Pts',(-11.8997390414271,-12.8813675568765,
117.034983115074)) ;
#159401 = CARTESIAN_POINT('Ctrl Pts',(-11.9735428878864,-12.8813675400482,
117.010752082645)) ;
#159402 = CARTESIAN_POINT('Ctrl Pts',(-11.95339641457,-12.8414910762961,116.949389175168)) ;
#159403 = CARTESIAN_POINT('Ctrl Pts',(-11.9332499412537,-12.8016146125439,
116.888026267692)) ;
#159404 = CARTESIAN_POINT('Ctrl Pts',(-11.8594460947944,-12.8016146293722,
116.912257300121)) ;
#159405 = CARTESIAN_POINT('Ctrl Pts',(-11.7856422483351,-12.8016146462005,
116.936488332549)) ;
#159406 = CARTESIAN_POINT('Ctrl Pts',(-11.8057887216514,-12.8414911099526,
116.997851240026)) ;
#159407 = CARTESIAN_POINT('Ctrl Pts',(-11.8738646701692,-12.6185827250958,
117.169942474425)) ;
#159408 = CARTESIAN_POINT('Ctrl Pts',(-11.8900165906483,-12.6740802978787,
117.219138618594)) ;
#159409 = CARTESIAN_POINT('Ctrl Pts',(-11.9638204397661,-12.6740802801009,
117.194907594263)) ;
#159410 = CARTESIAN_POINT('Ctrl Pts',(-12.037624288884,-12.674080262323,117.170676569932)) ;
#159411 = CARTESIAN_POINT('Ctrl Pts',(-12.0214723684048,-12.6185826895401,
117.121480425762)) ;
#159412 = CARTESIAN_POINT('Ctrl Pts',(-12.0053204479257,-12.5630851167572,
117.072284281593)) ;
#159413 = CARTESIAN_POINT('Ctrl Pts',(-11.9315165988079,-12.563085134535,
117.096515305924)) ;
#159414 = CARTESIAN_POINT('Ctrl Pts',(-11.85771274969,-12.5630851523128,117.120746330255)) ;
#159415 = CARTESIAN_POINT('Ctrl Pts',(-11.8738646701692,-12.6185827250958,
117.169942474425)) ;
#159416 = CARTESIAN_POINT('Ctrl Pts',(-11.959020038101,-12.4509854490646,
117.393736018184)) ;
#159417 = CARTESIAN_POINT('Ctrl Pts',(-11.969985920216,-12.518265407944,117.427136326441)) ;
#159418 = CARTESIAN_POINT('Ctrl Pts',(-12.0437897731662,-12.5182653912533,
117.402905313782)) ;
#159419 = CARTESIAN_POINT('Ctrl Pts',(-12.1175936261163,-12.5182653745627,
117.378674301124)) ;
#159420 = CARTESIAN_POINT('Ctrl Pts',(-12.1066277440013,-12.4509854156833,
117.345273992867)) ;
#159421 = CARTESIAN_POINT('Ctrl Pts',(-12.0956618618863,-12.383705456804,
117.311873684609)) ;
#159422 = CARTESIAN_POINT('Ctrl Pts',(-12.0218580089361,-12.3837054734946,
117.336104697268)) ;
#159423 = CARTESIAN_POINT('Ctrl Pts',(-11.948054155986,-12.3837054901852,
117.360335709926)) ;
#159424 = CARTESIAN_POINT('Ctrl Pts',(-11.959020038101,-12.4509854490646,
117.393736018184)) ;
#159425 = CARTESIAN_POINT('Ctrl Pts',(-12.0550313167262,-12.3534810644787,
117.650738776618)) ;
#159426 = CARTESIAN_POINT('Ctrl Pts',(-12.0600427070521,-12.427665920119,
117.666002663801)) ;
#159427 = CARTESIAN_POINT('Ctrl Pts',(-12.1338465636051,-12.4276659104835,
117.641771662116)) ;
#159428 = CARTESIAN_POINT('Ctrl Pts',(-12.2076504201582,-12.4276659008479,
117.617540660431)) ;
#159429 = CARTESIAN_POINT('Ctrl Pts',(-12.2026390298322,-12.3534810452076,
117.602276773248)) ;
#159430 = CARTESIAN_POINT('Ctrl Pts',(-12.1976276395063,-12.2792961895673,
117.587012886065)) ;
#159431 = CARTESIAN_POINT('Ctrl Pts',(-12.1238237829533,-12.2792961992029,
117.61124388775)) ;
#159432 = CARTESIAN_POINT('Ctrl Pts',(-12.0500199264003,-12.2792962088384,
117.635474889435)) ;
#159433 = CARTESIAN_POINT('Ctrl Pts',(-12.0550313167262,-12.3534810644787,
117.650738776618)) ;
#159434 = CARTESIAN_POINT('Ctrl Pts',(-12.1561839108002,-12.3320089256095,
117.923345972253)) ;
#159435 = CARTESIAN_POINT('Ctrl Pts',(-12.1548744716883,-12.407800207037,
117.919357633003)) ;
#159436 = CARTESIAN_POINT('Ctrl Pts',(-12.2286783313457,-12.407800209429,
117.895126640774)) ;
#159437 = CARTESIAN_POINT('Ctrl Pts',(-12.302482191003,-12.4078002118209,
117.870895648545)) ;
#159438 = CARTESIAN_POINT('Ctrl Pts',(-12.303791630115,-12.3320089303934,
117.874883987795)) ;
#159439 = CARTESIAN_POINT('Ctrl Pts',(-12.305101069227,-12.2562176489658,
117.878872327045)) ;
#159440 = CARTESIAN_POINT('Ctrl Pts',(-12.2312972095696,-12.2562176465738,
117.903103319274)) ;
#159441 = CARTESIAN_POINT('Ctrl Pts',(-12.1574933499122,-12.2562176441819,
117.927334311503)) ;
#159442 = CARTESIAN_POINT('Ctrl Pts',(-12.1561839108002,-12.3320089256095,
117.923345972253)) ;
#159443 = CARTESIAN_POINT('Ctrl Pts',(-12.2558122040571,-12.3884256006082,
118.1913322941)) ;
#159444 = CARTESIAN_POINT('Ctrl Pts',(-12.2482788311864,-12.4603875127443,
118.168386857015)) ;
#159445 = CARTESIAN_POINT('Ctrl Pts',(-12.3220826926037,-12.4603875316984,
118.144155870146)) ;
#159446 = CARTESIAN_POINT('Ctrl Pts',(-12.3958865540209,-12.4603875506525,
118.119924883277)) ;
#159447 = CARTESIAN_POINT('Ctrl Pts',(-12.4034199268916,-12.3884256385165,
118.142870320362)) ;
#159448 = CARTESIAN_POINT('Ctrl Pts',(-12.4109532997624,-12.3164637263805,
118.165815757446)) ;
#159449 = CARTESIAN_POINT('Ctrl Pts',(-12.3371494383451,-12.3164637074263,
118.190046744315)) ;
#159450 = CARTESIAN_POINT('Ctrl Pts',(-12.2633455769279,-12.3164636884722,
118.214277731184)) ;
#159451 = CARTESIAN_POINT('Ctrl Pts',(-12.2558122040571,-12.3884256006082,
118.1913322941)) ;
#159452 = CARTESIAN_POINT('Ctrl Pts',(-12.3475394657345,-12.5185566369419,
118.43526353432)) ;
#159453 = CARTESIAN_POINT('Ctrl Pts',(-12.3343246291813,-12.5815371501028,
118.395013275716)) ;
#159454 = CARTESIAN_POINT('Ctrl Pts',(-12.4081284904738,-12.5815371883386,
118.370782288467)) ;
#159455 = CARTESIAN_POINT('Ctrl Pts',(-12.4819323517663,-12.5815372265744,
118.346551301219)) ;
#159456 = CARTESIAN_POINT('Ctrl Pts',(-12.4951471883196,-12.5185567134136,
118.386801559822)) ;
#159457 = CARTESIAN_POINT('Ctrl Pts',(-12.5083620248728,-12.4555762002527,
118.427051818425)) ;
#159458 = CARTESIAN_POINT('Ctrl Pts',(-12.4345581635803,-12.4555761620169,
118.451282805674)) ;
#159459 = CARTESIAN_POINT('Ctrl Pts',(-12.3607543022878,-12.4555761237811,
118.475513792923)) ;
#159460 = CARTESIAN_POINT('Ctrl Pts',(-12.3475394657345,-12.5185566369419,
118.43526353432)) ;
#159461 = CARTESIAN_POINT('Ctrl Pts',(-12.4255960408986,-12.7128146761132,
118.637581654736)) ;
#159462 = CARTESIAN_POINT('Ctrl Pts',(-12.4076454894822,-12.7623237651114,
118.582907172911)) ;
#159463 = CARTESIAN_POINT('Ctrl Pts',(-12.4814493485287,-12.7623238229043,
118.558676178821)) ;
#159464 = CARTESIAN_POINT('Ctrl Pts',(-12.5552532075751,-12.7623238806971,
118.534445184731)) ;
#159465 = CARTESIAN_POINT('Ctrl Pts',(-12.5732037589916,-12.7128147916989,
118.589119666556)) ;
#159466 = CARTESIAN_POINT('Ctrl Pts',(-12.591154310408,-12.6633057027007,
118.643794148382)) ;
#159467 = CARTESIAN_POINT('Ctrl Pts',(-12.5173504513616,-12.6633056449079,
118.668025142472)) ;
#159468 = CARTESIAN_POINT('Ctrl Pts',(-12.4435465923151,-12.663305587115,
118.692256136562)) ;
#159469 = CARTESIAN_POINT('Ctrl Pts',(-12.4255960408986,-12.7128146761132,
118.637581654736)) ;
#159470 = CARTESIAN_POINT('Ctrl Pts',(-12.4854118400066,-12.9591843124397,
118.784128401409)) ;
#159471 = CARTESIAN_POINT('Ctrl Pts',(-12.4639964600509,-12.9915649142031,
118.718900611066)) ;
#159472 = CARTESIAN_POINT('Ctrl Pts',(-12.537800314808,-12.9915649910661,
118.694669603911)) ;
#159473 = CARTESIAN_POINT('Ctrl Pts',(-12.6116041695651,-12.9915650679292,
118.670438596757)) ;
#159474 = CARTESIAN_POINT('Ctrl Pts',(-12.6330195495208,-12.9591844661657,
118.735666387099)) ;
#159475 = CARTESIAN_POINT('Ctrl Pts',(-12.6544349294764,-12.9268038644023,
118.800894177441)) ;
#159476 = CARTESIAN_POINT('Ctrl Pts',(-12.5806310747193,-12.9268037875393,
118.825125184596)) ;
#159477 = CARTESIAN_POINT('Ctrl Pts',(-12.5068272199622,-12.9268037106763,
118.849356191751)) ;
#159478 = CARTESIAN_POINT('Ctrl Pts',(-12.4854118400066,-12.9591843124397,
118.784128401409)) ;
#159479 = CARTESIAN_POINT('Ctrl Pts',(-12.5227062774273,-13.2359003760254,
118.862430198041)) ;
#159480 = CARTESIAN_POINT('Ctrl Pts',(-12.4993863439673,-13.2490083473187,
118.791401445121)) ;
#159481 = CARTESIAN_POINT('Ctrl Pts',(-12.5731901922074,-13.24900843612,118.767170418116)) ;
#159482 = CARTESIAN_POINT('Ctrl Pts',(-12.6469940404474,-13.2490085249213,
118.742939391112)) ;
#159483 = CARTESIAN_POINT('Ctrl Pts',(-12.6703139739074,-13.235900553628,
118.813968144031)) ;
#159484 = CARTESIAN_POINT('Ctrl Pts',(-12.6936339073674,-13.2227925823347,
118.884996896951)) ;
#159485 = CARTESIAN_POINT('Ctrl Pts',(-12.6198300591273,-13.2227924935334,
118.909227923956)) ;
#159486 = CARTESIAN_POINT('Ctrl Pts',(-12.5460262108872,-13.2227924047321,
118.93345895096)) ;
#159487 = CARTESIAN_POINT('Ctrl Pts',(-12.5227062774273,-13.2359003760254,
118.862430198041)) ;
#159488 = CARTESIAN_POINT('Ctrl Pts',(-12.5363357220994,-13.5269168879405,
118.86847314923)) ;
#159489 = CARTESIAN_POINT('Ctrl Pts',(-12.5127641692558,-13.5197262961672,
118.796678004376)) ;
#159490 = CARTESIAN_POINT('Ctrl Pts',(-12.5865680098084,-13.5197263915446,
118.772446953957)) ;
#159491 = CARTESIAN_POINT('Ctrl Pts',(-12.6603718503611,-13.5197264869221,
118.748215903538)) ;
#159492 = CARTESIAN_POINT('Ctrl Pts',(-12.6839434032046,-13.5269170786954,
118.820011048392)) ;
#159493 = CARTESIAN_POINT('Ctrl Pts',(-12.7075149560482,-13.5341076704686,
118.891806193245)) ;
#159494 = CARTESIAN_POINT('Ctrl Pts',(-12.6337111154956,-13.5341075750912,
118.916037243664)) ;
#159495 = CARTESIAN_POINT('Ctrl Pts',(-12.559907274943,-13.5341074797137,
118.940268294084)) ;
#159496 = CARTESIAN_POINT('Ctrl Pts',(-12.5363357220994,-13.5269168879405,
118.86847314923)) ;
#159497 = CARTESIAN_POINT('Ctrl Pts',(-12.5257513802662,-13.8100818853549,
118.80078051953)) ;
#159498 = CARTESIAN_POINT('Ctrl Pts',(-12.5036179456418,-13.7831112951298,
118.733365650822)) ;
#159499 = CARTESIAN_POINT('Ctrl Pts',(-12.5774217778562,-13.7831113889682,
118.709134575006)) ;
#159500 = CARTESIAN_POINT('Ctrl Pts',(-12.6512256100705,-13.7831114828066,
118.68490349919)) ;
#159501 = CARTESIAN_POINT('Ctrl Pts',(-12.6733590446949,-13.8100820730318,
118.752318367897)) ;
#159502 = CARTESIAN_POINT('Ctrl Pts',(-12.6954924793192,-13.837052663257,
118.819733236605)) ;
#159503 = CARTESIAN_POINT('Ctrl Pts',(-12.6216886471049,-13.8370525694185,
118.843964312421)) ;
#159504 = CARTESIAN_POINT('Ctrl Pts',(-12.5478848148905,-13.8370524755801,
118.868195388238)) ;
#159505 = CARTESIAN_POINT('Ctrl Pts',(-12.5257513802662,-13.8100818853549,
118.80078051953)) ;
#159506 = CARTESIAN_POINT('Ctrl Pts',(-12.4923757936398,-14.0658493622321,
118.663565106864)) ;
#159507 = CARTESIAN_POINT('Ctrl Pts',(-12.4732757223142,-14.0209825335161,
118.60538937341)) ;
#159508 = CARTESIAN_POINT('Ctrl Pts',(-12.5470795463847,-14.0209826175788,
118.581158272789)) ;
#159509 = CARTESIAN_POINT('Ctrl Pts',(-12.6208833704551,-14.0209827016415,
118.556927172168)) ;
#159510 = CARTESIAN_POINT('Ctrl Pts',(-12.6399834417808,-14.0658495303575,
118.615102905622)) ;
#159511 = CARTESIAN_POINT('Ctrl Pts',(-12.6590835131064,-14.1107163590735,
118.673278639076)) ;
#159512 = CARTESIAN_POINT('Ctrl Pts',(-12.5852796890359,-14.1107162750108,
118.697509739697)) ;
#159513 = CARTESIAN_POINT('Ctrl Pts',(-12.5114758649654,-14.1107161909481,
118.721740840318)) ;
#159514 = CARTESIAN_POINT('Ctrl Pts',(-12.4923757936398,-14.0658493622321,
118.663565106864)) ;
#159515 = CARTESIAN_POINT('Ctrl Pts',(-12.4395119409733,-14.2744004374724,
118.467090668042)) ;
#159516 = CARTESIAN_POINT('Ctrl Pts',(-12.4248082411244,-14.2149073780421,
118.4223055728)) ;
#159517 = CARTESIAN_POINT('Ctrl Pts',(-12.4986120583206,-14.2149074440193,
118.398074451241)) ;
#159518 = CARTESIAN_POINT('Ctrl Pts',(-12.5724158755168,-14.2149075099964,
118.373843329682)) ;
#159519 = CARTESIAN_POINT('Ctrl Pts',(-12.5871195753657,-14.2744005694268,
118.418628424924)) ;
#159520 = CARTESIAN_POINT('Ctrl Pts',(-12.6018232752146,-14.3338936288571,
118.463413520166)) ;
#159521 = CARTESIAN_POINT('Ctrl Pts',(-12.5280194580184,-14.3338935628799,
118.487644641725)) ;
#159522 = CARTESIAN_POINT('Ctrl Pts',(-12.4542156408222,-14.3338934969028,
118.511875763284)) ;
#159523 = CARTESIAN_POINT('Ctrl Pts',(-12.4395119409733,-14.2744004374724,
118.467090668042)) ;
#159524 = CARTESIAN_POINT('Ctrl Pts',(-12.371795140951,-14.4215076088756,
118.225429654782)) ;
#159525 = CARTESIAN_POINT('Ctrl Pts',(-12.362530137544,-14.3516564443396,
118.197209951397)) ;
#159526 = CARTESIAN_POINT('Ctrl Pts',(-12.4363339498473,-14.3516564861261,
118.172978814935)) ;
#159527 = CARTESIAN_POINT('Ctrl Pts',(-12.5101377621506,-14.3516565279127,
118.148747678473)) ;
#159528 = CARTESIAN_POINT('Ctrl Pts',(-12.5194027655576,-14.4215076924487,
118.176967381858)) ;
#159529 = CARTESIAN_POINT('Ctrl Pts',(-12.5286677689646,-14.4913588569847,
118.205187085244)) ;
#159530 = CARTESIAN_POINT('Ctrl Pts',(-12.4548639566613,-14.4913588151982,
118.229418221706)) ;
#159531 = CARTESIAN_POINT('Ctrl Pts',(-12.381060144358,-14.4913587734116,
118.253649358168)) ;
#159532 = CARTESIAN_POINT('Ctrl Pts',(-12.371795140951,-14.4215076088756,
118.225429654782)) ;
#159533 = CARTESIAN_POINT('Ctrl Pts',(-12.2946403903294,-14.4970287487176,
117.954986337942)) ;
#159534 = CARTESIAN_POINT('Ctrl Pts',(-12.2914816993358,-14.421801684016,
117.945365476924)) ;
#159535 = CARTESIAN_POINT('Ctrl Pts',(-12.3652855092019,-14.42180169783,117.921134333039)) ;
#159536 = CARTESIAN_POINT('Ctrl Pts',(-12.4390893190681,-14.421801711644,
117.896903189154)) ;
#159537 = CARTESIAN_POINT('Ctrl Pts',(-12.4422480100617,-14.4970287763456,
117.906524050172)) ;
#159538 = CARTESIAN_POINT('Ctrl Pts',(-12.4454067010553,-14.5722558410471,
117.91614491119)) ;
#159539 = CARTESIAN_POINT('Ctrl Pts',(-12.3716028911892,-14.5722558272332,
117.940376055076)) ;
#159540 = CARTESIAN_POINT('Ctrl Pts',(-12.297799081323,-14.5722558134192,
117.964607198961)) ;
#159541 = CARTESIAN_POINT('Ctrl Pts',(-12.2946403903294,-14.4970287487176,
117.954986337942)) ;
#159542 = CARTESIAN_POINT('Ctrl Pts',(-12.2142494904348,-14.495364180026,
117.674634887753)) ;
#159543 = CARTESIAN_POINT('Ctrl Pts',(-12.2174331076008,-14.420141562785,
117.684331674045)) ;
#159544 = CARTESIAN_POINT('Ctrl Pts',(-12.2912369177925,-14.4201415475385,
117.660100531151)) ;
#159545 = CARTESIAN_POINT('Ctrl Pts',(-12.3650407279842,-14.420141532292,
117.635869388258)) ;
#159546 = CARTESIAN_POINT('Ctrl Pts',(-12.3618571108181,-14.495364149533,
117.626172601966)) ;
#159547 = CARTESIAN_POINT('Ctrl Pts',(-12.3586734936521,-14.570586766774,
117.616475815674)) ;
#159548 = CARTESIAN_POINT('Ctrl Pts',(-12.2848696834604,-14.5705867820204,
117.640706958568)) ;
#159549 = CARTESIAN_POINT('Ctrl Pts',(-12.2110658732687,-14.5705867972669,
117.664938101461)) ;
#159550 = CARTESIAN_POINT('Ctrl Pts',(-12.2142494904348,-14.495364180026,
117.674634887753)) ;
#159551 = CARTESIAN_POINT('Ctrl Pts',(-12.1371207254048,-14.4159600881982,
117.404140731358)) ;
#159552 = CARTESIAN_POINT('Ctrl Pts',(-12.1464300057665,-14.3461687677575,
117.432495299325)) ;
#159553 = CARTESIAN_POINT('Ctrl Pts',(-12.2202338191202,-14.346168725633,
117.408264166062)) ;
#159554 = CARTESIAN_POINT('Ctrl Pts',(-12.294037632474,-14.3461686835086,
117.3840330328)) ;
#159555 = CARTESIAN_POINT('Ctrl Pts',(-12.2847283521122,-14.4159600039494,
117.355678464832)) ;
#159556 = CARTESIAN_POINT('Ctrl Pts',(-12.2754190717505,-14.4857513243901,
117.327323896865)) ;
#159557 = CARTESIAN_POINT('Ctrl Pts',(-12.2016152583968,-14.4857513665145,
117.351555030128)) ;
#159558 = CARTESIAN_POINT('Ctrl Pts',(-12.1278114450431,-14.485751408639,
117.37578616339)) ;
#159559 = CARTESIAN_POINT('Ctrl Pts',(-12.1371207254048,-14.4159600881982,
117.404140731358)) ;
#159560 = CARTESIAN_POINT('Ctrl Pts',(-12.0701819932153,-14.2660479877099,
117.164946413806)) ;
#159561 = CARTESIAN_POINT('Ctrl Pts',(-12.0849092529423,-14.2066193411526,
117.209803272681)) ;
#159562 = CARTESIAN_POINT('Ctrl Pts',(-12.1587130714868,-14.206619276698,
117.185572155228)) ;
#159563 = CARTESIAN_POINT('Ctrl Pts',(-12.2325168900312,-14.2066192122434,
117.161341037776)) ;
#159564 = CARTESIAN_POINT('Ctrl Pts',(-12.2177896303041,-14.2660478588008,
117.1164841789)) ;
#159565 = CARTESIAN_POINT('Ctrl Pts',(-12.2030623705771,-14.3254765053581,
117.071627320025)) ;
#159566 = CARTESIAN_POINT('Ctrl Pts',(-12.1292585520327,-14.3254765698126,
117.095858437478)) ;
#159567 = CARTESIAN_POINT('Ctrl Pts',(-12.0554547334883,-14.3254766342672,
117.12008955493)) ;
#159568 = CARTESIAN_POINT('Ctrl Pts',(-12.0701819932153,-14.2660479877099,
117.164946413806)) ;
#159569 = CARTESIAN_POINT('Ctrl Pts',(-12.0180738968896,-14.0549162780305,
116.970748910434)) ;
#159570 = CARTESIAN_POINT('Ctrl Pts',(-12.0371954975587,-14.010139153776,
117.028990222714)) ;
#159571 = CARTESIAN_POINT('Ctrl Pts',(-12.1109993231329,-14.0101390737133,
117.004759126673)) ;
#159572 = CARTESIAN_POINT('Ctrl Pts',(-12.184803148707,-14.0101389936507,
116.980528030632)) ;
#159573 = CARTESIAN_POINT('Ctrl Pts',(-12.1656815480379,-14.0549161179053,
116.922286718351)) ;
#159574 = CARTESIAN_POINT('Ctrl Pts',(-12.1465599473688,-14.0996932421598,
116.864045406071)) ;
#159575 = CARTESIAN_POINT('Ctrl Pts',(-12.0727561217947,-14.0996933222224,
116.888276502112)) ;
#159576 = CARTESIAN_POINT('Ctrl Pts',(-11.9989522962205,-14.0996934022851,
116.912507598153)) ;
#159577 = CARTESIAN_POINT('Ctrl Pts',(-12.0180738968896,-14.0549162780305,
116.970748910434)) ;
#159578 = CARTESIAN_POINT('Ctrl Pts',(-11.9857272141969,-13.7973888984154,
116.836670452939)) ;
#159579 = CARTESIAN_POINT('Ctrl Pts',(-12.0078717114481,-13.7705242930268,
116.904119020354)) ;
#159580 = CARTESIAN_POINT('Ctrl Pts',(-12.0816755449335,-13.7705242060614,
116.87988794841)) ;
#159581 = CARTESIAN_POINT('Ctrl Pts',(-12.155479378419,-13.770524119096,116.855656876465)) ;
#159582 = CARTESIAN_POINT('Ctrl Pts',(-12.1333348811679,-13.7973887244846,
116.78820830905)) ;
#159583 = CARTESIAN_POINT('Ctrl Pts',(-12.1111903839167,-13.8242533298732,
116.720759741635)) ;
#159584 = CARTESIAN_POINT('Ctrl Pts',(-12.0373865504313,-13.8242534168386,
116.744990813579)) ;
#159585 = CARTESIAN_POINT('Ctrl Pts',(-11.9635827169458,-13.824253503804,
116.769221885524)) ;
#159586 = CARTESIAN_POINT('Ctrl Pts',(-11.9857272141969,-13.7973888984154,
116.836670452939)) ;
#159587 = CARTESIAN_POINT('Ctrl Pts',(-11.9762272551923,-13.5143192821472,
116.772389751235)) ;
#159588 = CARTESIAN_POINT('Ctrl Pts',(-11.999799643485,-13.5071778533561,
116.844187444272)) ;
#159589 = CARTESIAN_POINT('Ctrl Pts',(-12.0736034846683,-13.507177766311,
116.819956395774)) ;
#159590 = CARTESIAN_POINT('Ctrl Pts',(-12.1474073258517,-13.5071776792659,
116.795725347276)) ;
#159591 = CARTESIAN_POINT('Ctrl Pts',(-12.1238349375591,-13.514319108057,
116.723927654239)) ;
#159592 = CARTESIAN_POINT('Ctrl Pts',(-12.1002625492664,-13.5214605368481,
116.652129961202)) ;
#159593 = CARTESIAN_POINT('Ctrl Pts',(-12.0264587080831,-13.5214606238932,
116.6763610097)) ;
#159594 = CARTESIAN_POINT('Ctrl Pts',(-11.9526548668997,-13.5214607109383,
116.700592058198)) ;
#159595 = CARTESIAN_POINT('Ctrl Pts',(-11.9762272551923,-13.5143192821472,
116.772389751235)) ;
#159596 = CARTESIAN_POINT('Ctrl Pts',(-11.9909277151902,-13.2228141005811,
116.78161966851)) ;
#159597 = CARTESIAN_POINT('Ctrl Pts',(-12.0142449048521,-13.236014362639,
116.85264006755)) ;
#159598 = CARTESIAN_POINT('Ctrl Pts',(-12.0880487529386,-13.2360142841561,
116.828409040078)) ;
#159599 = CARTESIAN_POINT('Ctrl Pts',(-12.1618526010251,-13.2360142056732,
116.804178012605)) ;
#159600 = CARTESIAN_POINT('Ctrl Pts',(-12.1385354113632,-13.2228139436153,
116.733157613566)) ;
#159601 = CARTESIAN_POINT('Ctrl Pts',(-12.1152182217013,-13.2096136815574,
116.662137214526)) ;
#159602 = CARTESIAN_POINT('Ctrl Pts',(-12.0414143736148,-13.2096137600403,
116.686368241999)) ;
#159603 = CARTESIAN_POINT('Ctrl Pts',(-11.9676105255282,-13.2096138385232,
116.710599269471)) ;
#159604 = CARTESIAN_POINT('Ctrl Pts',(-11.9909277151902,-13.2228141005811,
116.78161966851)) ;
#159605 = CARTESIAN_POINT('Ctrl Pts',(-12.0294614824962,-12.9463122499942,
116.863581031885)) ;
#159606 = CARTESIAN_POINT('Ctrl Pts',(-12.0508561203109,-12.9788376519378,
116.928745648064)) ;
#159607 = CARTESIAN_POINT('Ctrl Pts',(-12.1246599737822,-12.978837586653,
116.904514636993)) ;
#159608 = CARTESIAN_POINT('Ctrl Pts',(-12.1984638272535,-12.9788375213682,
116.880283625922)) ;
#159609 = CARTESIAN_POINT('Ctrl Pts',(-12.1770691894388,-12.9463121194246,
116.815119009743)) ;
#159610 = CARTESIAN_POINT('Ctrl Pts',(-12.1556745516242,-12.913786717481,
116.749954393564)) ;
#159611 = CARTESIAN_POINT('Ctrl Pts',(-12.0818706981529,-12.9137867827658,
116.774185404635)) ;
#159612 = CARTESIAN_POINT('Ctrl Pts',(-12.0080668446816,-12.9137868480506,
116.798416415706)) ;
#159613 = CARTESIAN_POINT('Ctrl Pts',(-12.0294614824962,-12.9463122499942,
116.863581031885)) ;
#159614 = CARTESIAN_POINT('Ctrl Pts',(-12.0901776028958,-12.7025112775513,
117.012934916738)) ;
#159615 = CARTESIAN_POINT('Ctrl Pts',(-12.1081017353665,-12.7521082971811,
117.067528933426)) ;
#159616 = CARTESIAN_POINT('Ctrl Pts',(-12.1819055920202,-12.7521082496802,
117.043297932048)) ;
#159617 = CARTESIAN_POINT('Ctrl Pts',(-12.255709448674,-12.7521082021794,
117.01906693067)) ;
#159618 = CARTESIAN_POINT('Ctrl Pts',(-12.2377853162033,-12.7025111825496,
116.964472913982)) ;
#159619 = CARTESIAN_POINT('Ctrl Pts',(-12.2198611837327,-12.6529141629198,
116.909878897294)) ;
#159620 = CARTESIAN_POINT('Ctrl Pts',(-12.1460573270789,-12.6529142104206,
116.934109898672)) ;
#159621 = CARTESIAN_POINT('Ctrl Pts',(-12.0722534704252,-12.6529142579215,
116.958340900049)) ;
#159622 = CARTESIAN_POINT('Ctrl Pts',(-12.0901776028958,-12.7025112775513,
117.012934916738)) ;
#159623 = CARTESIAN_POINT('Ctrl Pts',(-12.1687375174296,-12.5113386435153,
117.216879767183)) ;
#159624 = CARTESIAN_POINT('Ctrl Pts',(-12.1819348220533,-12.5743584257443,
117.25707662878)) ;
#159625 = CARTESIAN_POINT('Ctrl Pts',(-12.2557386802607,-12.5743583951879,
117.232845632134)) ;
#159626 = CARTESIAN_POINT('Ctrl Pts',(-12.3295425384681,-12.5743583646314,
117.208614635489)) ;
#159627 = CARTESIAN_POINT('Ctrl Pts',(-12.3163452338444,-12.5113385824024,
117.168417773891)) ;
#159628 = CARTESIAN_POINT('Ctrl Pts',(-12.3031479292207,-12.4483188001733,
117.128220912294)) ;
#159629 = CARTESIAN_POINT('Ctrl Pts',(-12.2293440710133,-12.4483188307298,
117.15245190894)) ;
#159630 = CARTESIAN_POINT('Ctrl Pts',(-12.1555402128059,-12.4483188612862,
117.176682905585)) ;
#159631 = CARTESIAN_POINT('Ctrl Pts',(-12.1687375174296,-12.5113386435153,
117.216879767183)) ;
#159632 = CARTESIAN_POINT('Ctrl Pts',(-12.2612290461381,-12.3839986409936,
117.463033125205)) ;
#159633 = CARTESIAN_POINT('Ctrl Pts',(-12.2687243980064,-12.45600534241,117.48586275853)) ;
#159634 = CARTESIAN_POINT('Ctrl Pts',(-12.3425282553788,-12.4560053286552,
117.461631759341)) ;
#159635 = CARTESIAN_POINT('Ctrl Pts',(-12.4163321127512,-12.4560053149005,
117.437400760152)) ;
#159636 = CARTESIAN_POINT('Ctrl Pts',(-12.408836760883,-12.3839986134842,
117.414571126827)) ;
#159637 = CARTESIAN_POINT('Ctrl Pts',(-12.4013414090147,-12.3119919120679,
117.391741493502)) ;
#159638 = CARTESIAN_POINT('Ctrl Pts',(-12.3275375516422,-12.3119919258226,
117.415972492691)) ;
#159639 = CARTESIAN_POINT('Ctrl Pts',(-12.2537336942698,-12.3119919395773,
117.44020349188)) ;
#159640 = CARTESIAN_POINT('Ctrl Pts',(-12.2612290461381,-12.3839986409936,
117.463033125205)) ;
#159641 = CARTESIAN_POINT('Ctrl Pts',(-12.3609719875208,-12.3313598679509,
117.731405074504)) ;
#159642 = CARTESIAN_POINT('Ctrl Pts',(-12.3622475504806,-12.4071510797427,
117.735290234212)) ;
#159643 = CARTESIAN_POINT('Ctrl Pts',(-12.4360514058846,-12.4071510785913,
117.711059229027)) ;
#159644 = CARTESIAN_POINT('Ctrl Pts',(-12.5098552612885,-12.4071510774399,
117.686828223842)) ;
#159645 = CARTESIAN_POINT('Ctrl Pts',(-12.5085796983286,-12.3313598656482,
117.682943064135)) ;
#159646 = CARTESIAN_POINT('Ctrl Pts',(-12.5073041353688,-12.2555686538564,
117.679057904427)) ;
#159647 = CARTESIAN_POINT('Ctrl Pts',(-12.4335002799649,-12.2555686550078,
117.703288909611)) ;
#159648 = CARTESIAN_POINT('Ctrl Pts',(-12.3596964245609,-12.2555686561592,
117.727519914796)) ;
#159649 = CARTESIAN_POINT('Ctrl Pts',(-12.3609719875208,-12.3313598679509,
117.731405074504)) ;
#159650 = CARTESIAN_POINT('Ctrl Pts',(-12.4619148744611,-12.3561484752169,
118.003421771831)) ;
#159651 = CARTESIAN_POINT('Ctrl Pts',(-12.4568776202729,-12.4303237529548,
117.988079108915)) ;
#159652 = CARTESIAN_POINT('Ctrl Pts',(-12.5306814728019,-12.4303237603732,
117.963848094974)) ;
#159653 = CARTESIAN_POINT('Ctrl Pts',(-12.6044853253309,-12.4303237677915,
117.939617081032)) ;
#159654 = CARTESIAN_POINT('Ctrl Pts',(-12.6095225795191,-12.3561484900536,
117.954959743949)) ;
#159655 = CARTESIAN_POINT('Ctrl Pts',(-12.6145598337073,-12.2819732123158,
117.970302406865)) ;
#159656 = CARTESIAN_POINT('Ctrl Pts',(-12.5407559811783,-12.2819732048974,
117.994533420806)) ;
#159657 = CARTESIAN_POINT('Ctrl Pts',(-12.4669521286493,-12.2819731974791,
118.018764434748)) ;
#159658 = CARTESIAN_POINT('Ctrl Pts',(-12.4619148744611,-12.3561484752169,
118.003421771831)) ;
#159659 = CARTESIAN_POINT('Ctrl Pts',(-12.558035703025,-12.4578681360596,
118.260559283857)) ;
#159660 = CARTESIAN_POINT('Ctrl Pts',(-12.5470165166241,-12.5250537220818,
118.226996620417)) ;
#159661 = CARTESIAN_POINT('Ctrl Pts',(-12.6208203656014,-12.5250537323896,
118.202765595658)) ;
#159662 = CARTESIAN_POINT('Ctrl Pts',(-12.6946242145786,-12.5250537426973,
118.178534570898)) ;
#159663 = CARTESIAN_POINT('Ctrl Pts',(-12.7056434009795,-12.4578681566752,
118.212097234338)) ;
#159664 = CARTESIAN_POINT('Ctrl Pts',(-12.7166625873804,-12.390682570653,
118.245659897778)) ;
#159665 = CARTESIAN_POINT('Ctrl Pts',(-12.6428587384032,-12.3906825603452,
118.269890922537)) ;
#159666 = CARTESIAN_POINT('Ctrl Pts',(-12.5690548894259,-12.3906825500374,
118.294121947297)) ;
#159667 = CARTESIAN_POINT('Ctrl Pts',(-12.558035703025,-12.4578681360596,
118.260559283857)) ;
#159668 = CARTESIAN_POINT('Ctrl Pts',(-12.6418650591551,-12.6270814220524,
118.480600547495)) ;
#159669 = CARTESIAN_POINT('Ctrl Pts',(-12.6257062539618,-12.6825528988753,
118.431383434374)) ;
#159670 = CARTESIAN_POINT('Ctrl Pts',(-12.6995101005983,-12.6825529093536,
118.407152402485)) ;
#159671 = CARTESIAN_POINT('Ctrl Pts',(-12.7733139472347,-12.6825529198319,
118.382921370596)) ;
#159672 = CARTESIAN_POINT('Ctrl Pts',(-12.7894727524281,-12.627081443009,
118.432138483717)) ;
#159673 = CARTESIAN_POINT('Ctrl Pts',(-12.8056315576213,-12.5716099661861,
118.481355596837)) ;
#159674 = CARTESIAN_POINT('Ctrl Pts',(-12.7318277109849,-12.5716099557078,
118.505586628726)) ;
#159675 = CARTESIAN_POINT('Ctrl Pts',(-12.6580238643484,-12.5716099452296,
118.529817660615)) ;
#159676 = CARTESIAN_POINT('Ctrl Pts',(-12.6418650591551,-12.6270814220524,
118.480600547495)) ;
#159677 = CARTESIAN_POINT('Ctrl Pts',(-12.709500616301,-12.8533401319523,
118.65115248197)) ;
#159678 = CARTESIAN_POINT('Ctrl Pts',(-12.68932847821,-12.8930967028274,118.589711404264)) ;
#159679 = CARTESIAN_POINT('Ctrl Pts',(-12.763132322778,-12.8930967101103,
118.565480366075)) ;
#159680 = CARTESIAN_POINT('Ctrl Pts',(-12.8369361673461,-12.8930967173931,
118.541249327886)) ;
#159681 = CARTESIAN_POINT('Ctrl Pts',(-12.8571083054371,-12.853340146518,
118.602690405592)) ;
#159682 = CARTESIAN_POINT('Ctrl Pts',(-12.8772804435281,-12.8135835756429,
118.664131483297)) ;
#159683 = CARTESIAN_POINT('Ctrl Pts',(-12.80347659896,-12.8135835683601,118.688362521486)) ;
#159684 = CARTESIAN_POINT('Ctrl Pts',(-12.729672754392,-12.8135835610772,
118.712593559675)) ;
#159685 = CARTESIAN_POINT('Ctrl Pts',(-12.709500616301,-12.8533401319523,
118.65115248197)) ;
#159686 = CARTESIAN_POINT('Ctrl Pts',(-12.7564269379405,-13.1210491167834,
118.758518890216)) ;
#159687 = CARTESIAN_POINT('Ctrl Pts',(-12.7336836205255,-13.1421721692445,
118.689246415035)) ;
#159688 = CARTESIAN_POINT('Ctrl Pts',(-12.8074874639998,-13.1421721715333,
118.665015373515)) ;
#159689 = CARTESIAN_POINT('Ctrl Pts',(-12.8812913074742,-13.1421721738222,
118.640784331994)) ;
#159690 = CARTESIAN_POINT('Ctrl Pts',(-12.9040346248891,-13.121049121361,
118.710056807176)) ;
#159691 = CARTESIAN_POINT('Ctrl Pts',(-12.926777942304,-13.0999260688999,
118.779329282357)) ;
#159692 = CARTESIAN_POINT('Ctrl Pts',(-12.8529740988297,-13.0999260666111,
118.803560323877)) ;
#159693 = CARTESIAN_POINT('Ctrl Pts',(-12.7791702553554,-13.0999260643223,
118.827791365398)) ;
#159694 = CARTESIAN_POINT('Ctrl Pts',(-12.7564269379405,-13.1210491167834,
118.758518890216)) ;
#159695 = CARTESIAN_POINT('Ctrl Pts',(-12.7797729830741,-13.40900770729,118.794199282391)) ;
#159696 = CARTESIAN_POINT('Ctrl Pts',(-12.756098640465,-13.410054885097,118.722091054621)) ;
#159697 = CARTESIAN_POINT('Ctrl Pts',(-12.8299024838005,-13.4100548838608,
118.697860012678)) ;
#159698 = CARTESIAN_POINT('Ctrl Pts',(-12.903706327136,-13.4100548826247,
118.673628970735)) ;
#159699 = CARTESIAN_POINT('Ctrl Pts',(-12.9273806697451,-13.4090077048177,
118.745737198505)) ;
#159700 = CARTESIAN_POINT('Ctrl Pts',(-12.9510550123542,-13.4079605270107,
118.817845426275)) ;
#159701 = CARTESIAN_POINT('Ctrl Pts',(-12.8772511690187,-13.4079605282469,
118.842076468218)) ;
#159702 = CARTESIAN_POINT('Ctrl Pts',(-12.8034473256832,-13.407960529483,
118.866307510161)) ;
#159703 = CARTESIAN_POINT('Ctrl Pts',(-12.7797729830741,-13.40900770729,118.794199282391)) ;
#159704 = CARTESIAN_POINT('Ctrl Pts',(-12.7789054138412,-13.6972694862933,
118.756166722536)) ;
#159705 = CARTESIAN_POINT('Ctrl Pts',(-12.7559888438116,-13.6781895282422,
118.686366547741)) ;
#159706 = CARTESIAN_POINT('Ctrl Pts',(-12.8297926874375,-13.6781895252059,
118.662135506682)) ;
#159707 = CARTESIAN_POINT('Ctrl Pts',(-12.9035965310634,-13.6781895221696,
118.637904465624)) ;
#159708 = CARTESIAN_POINT('Ctrl Pts',(-12.926513101093,-13.6972694802207,
118.707704640419)) ;
#159709 = CARTESIAN_POINT('Ctrl Pts',(-12.9494296711225,-13.7163494382719,
118.777504815214)) ;
#159710 = CARTESIAN_POINT('Ctrl Pts',(-12.8756258274966,-13.7163494413082,
118.801735856273)) ;
#159711 = CARTESIAN_POINT('Ctrl Pts',(-12.8018219838707,-13.7163494443445,
118.825966897331)) ;
#159712 = CARTESIAN_POINT('Ctrl Pts',(-12.7789054138412,-13.6972694862933,
118.756166722536)) ;
#159713 = CARTESIAN_POINT('Ctrl Pts',(-12.7545947470765,-13.9663054532962,
118.646647736907)) ;
#159714 = CARTESIAN_POINT('Ctrl Pts',(-12.7340759482531,-13.9284104742122,
118.584150786325)) ;
#159715 = CARTESIAN_POINT('Ctrl Pts',(-12.8078797922052,-13.9284104715145,
118.55991974626)) ;
#159716 = CARTESIAN_POINT('Ctrl Pts',(-12.8816836361573,-13.9284104688168,
118.535688706195)) ;
#159717 = CARTESIAN_POINT('Ctrl Pts',(-12.9022024349807,-13.9663054479008,
118.598185656777)) ;
#159718 = CARTESIAN_POINT('Ctrl Pts',(-12.9227212338041,-14.0042004269848,
118.660682607359)) ;
#159719 = CARTESIAN_POINT('Ctrl Pts',(-12.848917389852,-14.0042004296825,
118.684913647424)) ;
#159720 = CARTESIAN_POINT('Ctrl Pts',(-12.7751135458999,-14.0042004323802,
118.709144687489)) ;
#159721 = CARTESIAN_POINT('Ctrl Pts',(-12.7545947470765,-13.9663054532962,
118.646647736907)) ;
#159722 = CARTESIAN_POINT('Ctrl Pts',(-12.708953623995,-14.1969043333081,
118.471990317947)) ;
#159723 = CARTESIAN_POINT('Ctrl Pts',(-12.692329221625,-14.1428507400375,
118.421355070661)) ;
#159724 = CARTESIAN_POINT('Ctrl Pts',(-12.7661330651514,-14.1428507401224,
118.3971240293)) ;
#159725 = CARTESIAN_POINT('Ctrl Pts',(-12.8399369086778,-14.1428507402074,
118.372892987938)) ;
#159726 = CARTESIAN_POINT('Ctrl Pts',(-12.8565613110478,-14.196904333478,
118.423528235223)) ;
#159727 = CARTESIAN_POINT('Ctrl Pts',(-12.8731857134178,-14.2509579267487,
118.474163482509)) ;
#159728 = CARTESIAN_POINT('Ctrl Pts',(-12.7993818698914,-14.2509579266637,
118.498394523871)) ;
#159729 = CARTESIAN_POINT('Ctrl Pts',(-12.725578026365,-14.2509579265788,
118.522625565232)) ;
#159730 = CARTESIAN_POINT('Ctrl Pts',(-12.708953623995,-14.1969043333081,
118.471990317947)) ;
#159731 = CARTESIAN_POINT('Ctrl Pts',(-12.6467531532713,-14.3698914257013,
118.24719675644)) ;
#159732 = CARTESIAN_POINT('Ctrl Pts',(-12.6351790212959,-14.3036801668695,
118.211943817991)) ;
#159733 = CARTESIAN_POINT('Ctrl Pts',(-12.7089828637962,-14.3036801689092,
118.187712773504)) ;
#159734 = CARTESIAN_POINT('Ctrl Pts',(-12.7827867062965,-14.303680170949,
118.163481729016)) ;
#159735 = CARTESIAN_POINT('Ctrl Pts',(-12.7943608382718,-14.3698914297808,
118.198734667466)) ;
#159736 = CARTESIAN_POINT('Ctrl Pts',(-12.8059349702472,-14.4361026886127,
118.233987605915)) ;
#159737 = CARTESIAN_POINT('Ctrl Pts',(-12.7321311277469,-14.4361026865729,
118.258218650402)) ;
#159738 = CARTESIAN_POINT('Ctrl Pts',(-12.6583272852466,-14.4361026845332,
118.282449694889)) ;
#159739 = CARTESIAN_POINT('Ctrl Pts',(-12.6467531532713,-14.3698914257013,
118.24719675644)) ;
#159740 = CARTESIAN_POINT('Ctrl Pts',(-12.5727418641631,-14.4755193866787,
117.986353001203)) ;
#159741 = CARTESIAN_POINT('Ctrl Pts',(-12.5670515910477,-14.4018362726686,
117.969021347583)) ;
#159742 = CARTESIAN_POINT('Ctrl Pts',(-12.6408554318707,-14.4018362752404,
117.944790297987)) ;
#159743 = CARTESIAN_POINT('Ctrl Pts',(-12.7146592726937,-14.4018362778122,
117.920559248391)) ;
#159744 = CARTESIAN_POINT('Ctrl Pts',(-12.7203495458091,-14.4755193918222,
117.937890902011)) ;
#159745 = CARTESIAN_POINT('Ctrl Pts',(-12.7260398189245,-14.5492025058322,
117.955222555631)) ;
#159746 = CARTESIAN_POINT('Ctrl Pts',(-12.6522359781016,-14.5492025032605,
117.979453605227)) ;
#159747 = CARTESIAN_POINT('Ctrl Pts',(-12.5784321372786,-14.5492025006887,
118.003684654823)) ;
#159748 = CARTESIAN_POINT('Ctrl Pts',(-12.5727418641631,-14.4755193866787,
117.986353001203)) ;
#159749 = CARTESIAN_POINT('Ctrl Pts',(-12.4928027634597,-14.5054697818126,
117.707363787146)) ;
#159750 = CARTESIAN_POINT('Ctrl Pts',(-12.4934206488961,-14.4295881889502,
117.709245766793)) ;
#159751 = CARTESIAN_POINT('Ctrl Pts',(-12.5672244874137,-14.4295881891086,
117.685014710175)) ;
#159752 = CARTESIAN_POINT('Ctrl Pts',(-12.6410283259312,-14.429588189267,
117.660783653557)) ;
#159753 = CARTESIAN_POINT('Ctrl Pts',(-12.6404104404947,-14.5054697821294,
117.65890167391)) ;
#159754 = CARTESIAN_POINT('Ctrl Pts',(-12.6397925550582,-14.5813513749918,
117.657019694263)) ;
#159755 = CARTESIAN_POINT('Ctrl Pts',(-12.5659887165407,-14.5813513748333,
117.681250750881)) ;
#159756 = CARTESIAN_POINT('Ctrl Pts',(-12.4921848780232,-14.5813513746749,
117.705481807498)) ;
#159757 = CARTESIAN_POINT('Ctrl Pts',(-12.4928027634597,-14.5054697818126,
117.707363787146)) ;
#159758 = CARTESIAN_POINT('Ctrl Pts',(-12.4137352350169,-14.4574393177702,
117.431077181479)) ;
#159759 = CARTESIAN_POINT('Ctrl Pts',(-12.4206084727546,-14.384801335134,
117.452011955084)) ;
#159760 = CARTESIAN_POINT('Ctrl Pts',(-12.4944123091801,-14.384801328945,
117.427780892094)) ;
#159761 = CARTESIAN_POINT('Ctrl Pts',(-12.5682161456056,-14.384801322756,
117.403549829104)) ;
#159762 = CARTESIAN_POINT('Ctrl Pts',(-12.5613429078678,-14.4574393053923,
117.382615055499)) ;
#159763 = CARTESIAN_POINT('Ctrl Pts',(-12.5544696701301,-14.5300772880285,
117.361680281894)) ;
#159764 = CARTESIAN_POINT('Ctrl Pts',(-12.4806658337047,-14.5300772942175,
117.385911344884)) ;
#159765 = CARTESIAN_POINT('Ctrl Pts',(-12.4068619972792,-14.5300773004065,
117.410142407874)) ;
#159766 = CARTESIAN_POINT('Ctrl Pts',(-12.4137352350169,-14.4574393177702,
117.431077181479)) ;
#159767 = CARTESIAN_POINT('Ctrl Pts',(-12.3418324266654,-14.3349211938034,
117.176601530105)) ;
#159768 = CARTESIAN_POINT('Ctrl Pts',(-12.3544699690229,-14.2707324518497,
117.215093445674)) ;
#159769 = CARTESIAN_POINT('Ctrl Pts',(-12.4282738040413,-14.2707324355109,
117.190862378399)) ;
#159770 = CARTESIAN_POINT('Ctrl Pts',(-12.5020776390596,-14.2707324191721,
117.166631311123)) ;
#159771 = CARTESIAN_POINT('Ctrl Pts',(-12.4894400967021,-14.3349211611258,
117.128139395553)) ;
#159772 = CARTESIAN_POINT('Ctrl Pts',(-12.4768025543446,-14.3991099030794,
117.089647479984)) ;
#159773 = CARTESIAN_POINT('Ctrl Pts',(-12.4029987193263,-14.3991099194182,
117.11387854726)) ;
#159774 = CARTESIAN_POINT('Ctrl Pts',(-12.3291948843079,-14.399109935757,
117.138109614536)) ;
#159775 = CARTESIAN_POINT('Ctrl Pts',(-12.3418324266654,-14.3349211938034,
117.176601530105)) ;
#159776 = CARTESIAN_POINT('Ctrl Pts',(-12.2830970975097,-14.1470800055845,
116.962290261975)) ;
#159777 = CARTESIAN_POINT('Ctrl Pts',(-12.3005865815552,-14.0959137214437,
117.015560409224)) ;
#159778 = CARTESIAN_POINT('Ctrl Pts',(-12.3743904165327,-14.0959136926008,
116.991329341823)) ;
#159779 = CARTESIAN_POINT('Ctrl Pts',(-12.4481942515102,-14.095913663758,
116.967098274423)) ;
#159780 = CARTESIAN_POINT('Ctrl Pts',(-12.4307047674647,-14.1470799478988,
116.913828127174)) ;
#159781 = CARTESIAN_POINT('Ctrl Pts',(-12.4132152834192,-14.1982462320397,
116.860557979926)) ;
#159782 = CARTESIAN_POINT('Ctrl Pts',(-12.3394114484417,-14.1982462608825,
116.884789047326)) ;
#159783 = CARTESIAN_POINT('Ctrl Pts',(-12.2656076134642,-14.1982462897254,
116.909020114726)) ;
#159784 = CARTESIAN_POINT('Ctrl Pts',(-12.2830970975097,-14.1470800055845,
116.962290261975)) ;
#159785 = CARTESIAN_POINT('Ctrl Pts',(-12.2422554856577,-13.9065331674936,
116.80239048803)) ;
#159786 = CARTESIAN_POINT('Ctrl Pts',(-12.2633564495242,-13.8720877275132,
116.866660620279)) ;
#159787 = CARTESIAN_POINT('Ctrl Pts',(-12.3371602858923,-13.8720876844338,
116.842429557115)) ;
#159788 = CARTESIAN_POINT('Ctrl Pts',(-12.4109641222604,-13.8720876413544,
116.81819849395)) ;
#159789 = CARTESIAN_POINT('Ctrl Pts',(-12.3898631583939,-13.9065330813348,
116.753928361701)) ;
#159790 = CARTESIAN_POINT('Ctrl Pts',(-12.3687621945274,-13.9409785213152,
116.689658229452)) ;
#159791 = CARTESIAN_POINT('Ctrl Pts',(-12.2949583581593,-13.9409785643945,
116.713889292616)) ;
#159792 = CARTESIAN_POINT('Ctrl Pts',(-12.2211545217912,-13.9409786074739,
116.738120355781)) ;
#159793 = CARTESIAN_POINT('Ctrl Pts',(-12.2422554856577,-13.9065331674936,
116.80239048803)) ;
#159794 = CARTESIAN_POINT('Ctrl Pts',(-12.2232261811748,-13.630738678715,
116.708912567899)) ;
#159795 = CARTESIAN_POINT('Ctrl Pts',(-12.2464212316731,-13.6154990346672,
116.779560950327)) ;
#159796 = CARTESIAN_POINT('Ctrl Pts',(-12.3202250713423,-13.6154989781254,
116.755329897217)) ;
#159797 = CARTESIAN_POINT('Ctrl Pts',(-12.3940289110116,-13.6154989215836,
116.731098844107)) ;
#159798 = CARTESIAN_POINT('Ctrl Pts',(-12.3708338605132,-13.6307385656315,
116.660450461679)) ;
#159799 = CARTESIAN_POINT('Ctrl Pts',(-12.3476388100149,-13.6459782096793,
116.589802079252)) ;
#159800 = CARTESIAN_POINT('Ctrl Pts',(-12.2738349703457,-13.6459782662211,
116.614033132362)) ;
#159801 = CARTESIAN_POINT('Ctrl Pts',(-12.2000311306764,-13.6459783227629,
116.638264185472)) ;
#159802 = CARTESIAN_POINT('Ctrl Pts',(-12.2232261811748,-13.630738678715,
116.708912567899)) ;
#159803 = CARTESIAN_POINT('Ctrl Pts',(-12.2280126456687,-13.3408270196336,
116.688112612688)) ;
#159804 = CARTESIAN_POINT('Ctrl Pts',(-12.2516390316777,-13.3458064636332,
116.760074773632)) ;
#159805 = CARTESIAN_POINT('Ctrl Pts',(-12.3254428763228,-13.3458063983403,
116.735843735678)) ;
#159806 = CARTESIAN_POINT('Ctrl Pts',(-12.3992467209678,-13.3458063330474,
116.711612697724)) ;
#159807 = CARTESIAN_POINT('Ctrl Pts',(-12.3756203349588,-13.3408268890478,
116.639650536779)) ;
#159808 = CARTESIAN_POINT('Ctrl Pts',(-12.3519939489498,-13.3358474450482,
116.567688375835)) ;
#159809 = CARTESIAN_POINT('Ctrl Pts',(-12.2781901043047,-13.3358475103411,
116.591919413789)) ;
#159810 = CARTESIAN_POINT('Ctrl Pts',(-12.2043862596596,-13.335847575634,
116.616150451744)) ;
#159811 = CARTESIAN_POINT('Ctrl Pts',(-12.2280126456687,-13.3408270196336,
116.688112612688)) ;
#159812 = CARTESIAN_POINT('Ctrl Pts',(-12.2570791816381,-13.0553492265632,
116.741127681574)) ;
#159813 = CARTESIAN_POINT('Ctrl Pts',(-12.2794453818278,-13.0802672240232,
116.809251520007)) ;
#159814 = CARTESIAN_POINT('Ctrl Pts',(-12.3532492327196,-13.0802671541192,
116.785020501079)) ;
#159815 = CARTESIAN_POINT('Ctrl Pts',(-12.4270530836114,-13.0802670842153,
116.760789482151)) ;
#159816 = CARTESIAN_POINT('Ctrl Pts',(-12.4046868834218,-13.0553490867554,
116.692665643718)) ;
#159817 = CARTESIAN_POINT('Ctrl Pts',(-12.3823206832321,-13.0304310892955,
116.624541805285)) ;
#159818 = CARTESIAN_POINT('Ctrl Pts',(-12.3085168323402,-13.0304311591994,
116.648772824213)) ;
#159819 = CARTESIAN_POINT('Ctrl Pts',(-12.2347129814484,-13.0304312291033,
116.673003843141)) ;
#159820 = CARTESIAN_POINT('Ctrl Pts',(-12.2570791816381,-13.0553492265632,
116.741127681574)) ;
#159821 = CARTESIAN_POINT('Ctrl Pts',(-12.3090343418545,-12.7963986353394,
116.863927628217)) ;
#159822 = CARTESIAN_POINT('Ctrl Pts',(-12.3285390631052,-12.8394319369363,
116.923335863641)) ;
#159823 = CARTESIAN_POINT('Ctrl Pts',(-12.4023429208373,-12.8394318699613,
116.899104865548)) ;
#159824 = CARTESIAN_POINT('Ctrl Pts',(-12.4761467785694,-12.8394318029862,
116.874873867454)) ;
#159825 = CARTESIAN_POINT('Ctrl Pts',(-12.4566420573186,-12.7963985013893,
116.815465632031)) ;
#159826 = CARTESIAN_POINT('Ctrl Pts',(-12.4371373360679,-12.7533651997924,
116.756057396607)) ;
#159827 = CARTESIAN_POINT('Ctrl Pts',(-12.3633334783358,-12.7533652667675,
116.7802883947)) ;
#159828 = CARTESIAN_POINT('Ctrl Pts',(-12.2895296206037,-12.7533653337425,
116.804519392794)) ;
#159829 = CARTESIAN_POINT('Ctrl Pts',(-12.3090343418545,-12.7963986353394,
116.863927628217)) ;
#159830 = CARTESIAN_POINT('Ctrl Pts',(-12.3809755753915,-12.581755675213,
117.047570548939)) ;
#159831 = CARTESIAN_POINT('Ctrl Pts',(-12.3962200578774,-12.6398371824031,
117.094002784605)) ;
#159832 = CARTESIAN_POINT('Ctrl Pts',(-12.4700239222921,-12.6398371256695,
117.069771806866)) ;
#159833 = CARTESIAN_POINT('Ctrl Pts',(-12.5438277867068,-12.639837068936,
117.045540829126)) ;
#159834 = CARTESIAN_POINT('Ctrl Pts',(-12.5285833042209,-12.581755561746,
116.999108593461)) ;
#159835 = CARTESIAN_POINT('Ctrl Pts',(-12.5133388217349,-12.5236740545559,
116.952676357795)) ;
#159836 = CARTESIAN_POINT('Ctrl Pts',(-12.4395349573202,-12.5236741112895,
116.976907335534)) ;
#159837 = CARTESIAN_POINT('Ctrl Pts',(-12.3657310929056,-12.523674168023,
117.001138313273)) ;
#159838 = CARTESIAN_POINT('Ctrl Pts',(-12.3809755753915,-12.581755675213,
117.047570548939)) ;
#159839 = CARTESIAN_POINT('Ctrl Pts',(-12.4684134110327,-12.4271874700909,
117.278442488482)) ;
#159840 = CARTESIAN_POINT('Ctrl Pts',(-12.478308991434,-12.4961449438695,
117.308582831552)) ;
#159841 = CARTESIAN_POINT('Ctrl Pts',(-12.5521128614542,-12.4961449047111,
117.284351870886)) ;
#159842 = CARTESIAN_POINT('Ctrl Pts',(-12.6259167314744,-12.4961448655528,
117.26012091022)) ;
#159843 = CARTESIAN_POINT('Ctrl Pts',(-12.6160211510731,-12.4271873917741,
117.22998056715)) ;
#159844 = CARTESIAN_POINT('Ctrl Pts',(-12.6061255706718,-12.3582299179955,
117.199840224079)) ;
#159845 = CARTESIAN_POINT('Ctrl Pts',(-12.5323217006516,-12.3582299571538,
117.224071184745)) ;
#159846 = CARTESIAN_POINT('Ctrl Pts',(-12.4585178306314,-12.3582299963122,
117.248302145411)) ;
#159847 = CARTESIAN_POINT('Ctrl Pts',(-12.4684134110327,-12.4271874700909,
117.278442488482)) ;
#159848 = CARTESIAN_POINT('Ctrl Pts',(-12.5658597005341,-12.3434882644401,
117.539803720469)) ;
#159849 = CARTESIAN_POINT('Ctrl Pts',(-12.5696997847096,-12.4183899253302,
117.551499999181)) ;
#159850 = CARTESIAN_POINT('Ctrl Pts',(-12.6435036585378,-12.4183899094731,
117.527269050114)) ;
#159851 = CARTESIAN_POINT('Ctrl Pts',(-12.717307532366,-12.418389893616,117.503038101047)) ;
#159852 = CARTESIAN_POINT('Ctrl Pts',(-12.7134674481905,-12.3434882327259,
117.491341822334)) ;
#159853 = CARTESIAN_POINT('Ctrl Pts',(-12.709627364015,-12.2685865718357,
117.479645543622)) ;
#159854 = CARTESIAN_POINT('Ctrl Pts',(-12.6358234901868,-12.2685865876929,
117.503876492689)) ;
#159855 = CARTESIAN_POINT('Ctrl Pts',(-12.5620196163586,-12.26858660355,117.528107441756)) ;
#159856 = CARTESIAN_POINT('Ctrl Pts',(-12.5658597005341,-12.3434882644401,
117.539803720469)) ;
#159857 = CARTESIAN_POINT('Ctrl Pts',(-12.6672936908425,-12.3367187774922,
117.813250325772)) ;
#159858 = CARTESIAN_POINT('Ctrl Pts',(-12.6647923438579,-12.412202858538,
117.805631628438)) ;
#159859 = CARTESIAN_POINT('Ctrl Pts',(-12.7385962192158,-12.4122028696992,
117.781400684031)) ;
#159860 = CARTESIAN_POINT('Ctrl Pts',(-12.8124000945738,-12.4122028808603,
117.757169739623)) ;
#159861 = CARTESIAN_POINT('Ctrl Pts',(-12.8149014415584,-12.3367187998145,
117.764788436956)) ;
#159862 = CARTESIAN_POINT('Ctrl Pts',(-12.8174027885431,-12.2612347187686,
117.772407134289)) ;
#159863 = CARTESIAN_POINT('Ctrl Pts',(-12.7435989131851,-12.2612347076075,
117.796638078697)) ;
#159864 = CARTESIAN_POINT('Ctrl Pts',(-12.6697950378272,-12.2612346964463,
117.820869023105)) ;
#159865 = CARTESIAN_POINT('Ctrl Pts',(-12.6672936908425,-12.3367187774922,
117.813250325772)) ;
#159866 = CARTESIAN_POINT('Ctrl Pts',(-12.765948884936,-12.4076100218016,
118.078256939231)) ;
#159867 = CARTESIAN_POINT('Ctrl Pts',(-12.7572902976169,-12.478255694811,
118.051884281362)) ;
#159868 = CARTESIAN_POINT('Ctrl Pts',(-12.8310941717384,-12.4782557339545,
118.027653333189)) ;
#159869 = CARTESIAN_POINT('Ctrl Pts',(-12.90489804586,-12.4782557730979,118.003422385015)) ;
#159870 = CARTESIAN_POINT('Ctrl Pts',(-12.9135566331791,-12.4076101000885,
118.029795042883)) ;
#159871 = CARTESIAN_POINT('Ctrl Pts',(-12.9222152204983,-12.3369644270791,
118.056167700752)) ;
#159872 = CARTESIAN_POINT('Ctrl Pts',(-12.8484113463767,-12.3369643879356,
118.080398648925)) ;
#159873 = CARTESIAN_POINT('Ctrl Pts',(-12.7746074722552,-12.3369643487922,
118.104629597099)) ;
#159874 = CARTESIAN_POINT('Ctrl Pts',(-12.765948884936,-12.4076100218016,
118.078256939231)) ;
#159875 = CARTESIAN_POINT('Ctrl Pts',(-12.8553355026567,-12.5503272886106,
118.315139856333)) ;
#159876 = CARTESIAN_POINT('Ctrl Pts',(-12.8411554877371,-12.6111127645847,
118.271949820905)) ;
#159877 = CARTESIAN_POINT('Ctrl Pts',(-12.9149593579354,-12.6111128294537,
118.247718860782)) ;
#159878 = CARTESIAN_POINT('Ctrl Pts',(-12.9887632281337,-12.6111128943226,
118.223487900658)) ;
#159879 = CARTESIAN_POINT('Ctrl Pts',(-13.0029432430532,-12.5503274183485,
118.266677936086)) ;
#159880 = CARTESIAN_POINT('Ctrl Pts',(-13.0171232579728,-12.4895419423743,
118.309867971514)) ;
#159881 = CARTESIAN_POINT('Ctrl Pts',(-12.9433193877745,-12.4895418775054,
118.334098931637)) ;
#159882 = CARTESIAN_POINT('Ctrl Pts',(-12.8695155175762,-12.4895418126364,
118.358329891761)) ;
#159883 = CARTESIAN_POINT('Ctrl Pts',(-12.8553355026567,-12.5503272886106,
118.315139856333)) ;
#159884 = CARTESIAN_POINT('Ctrl Pts',(-12.9304176070875,-12.7556871760659,
118.508319195545)) ;
#159885 = CARTESIAN_POINT('Ctrl Pts',(-12.9117094172772,-12.8022252144536,
118.451337070035)) ;
#159886 = CARTESIAN_POINT('Ctrl Pts',(-12.9855132812814,-12.8022253005655,
118.427106091045)) ;
#159887 = CARTESIAN_POINT('Ctrl Pts',(-13.0593171452855,-12.8022253866775,
118.402875112056)) ;
#159888 = CARTESIAN_POINT('Ctrl Pts',(-13.0780253350958,-12.7556873482899,
118.459857237566)) ;
#159889 = CARTESIAN_POINT('Ctrl Pts',(-13.0967335249062,-12.7091493099022,
118.516839363076)) ;
#159890 = CARTESIAN_POINT('Ctrl Pts',(-13.022929660902,-12.7091492237902,
118.541070342065)) ;
#159891 = CARTESIAN_POINT('Ctrl Pts',(-12.9491257968979,-12.7091491376783,
118.565301321055)) ;
#159892 = CARTESIAN_POINT('Ctrl Pts',(-12.9304176070875,-12.7556871760659,
118.508319195545)) ;
#159893 = CARTESIAN_POINT('Ctrl Pts',(-12.9861723417227,-13.0091921750313,
118.642571963292)) ;
#159894 = CARTESIAN_POINT('Ctrl Pts',(-12.964279676432,-13.038100701856,118.575890439269)) ;
#159895 = CARTESIAN_POINT('Ctrl Pts',(-13.0380835324484,-13.03810080188,118.551659435951)) ;
#159896 = CARTESIAN_POINT('Ctrl Pts',(-13.1118873884648,-13.038100901904,
118.527428432632)) ;
#159897 = CARTESIAN_POINT('Ctrl Pts',(-13.1337800537556,-13.0091923750794,
118.594109956654)) ;
#159898 = CARTESIAN_POINT('Ctrl Pts',(-13.1556727190464,-12.9802838482547,
118.660791480676)) ;
#159899 = CARTESIAN_POINT('Ctrl Pts',(-13.08186886303,-12.9802837482307,118.685022483995)) ;
#159900 = CARTESIAN_POINT('Ctrl Pts',(-13.0080650070135,-12.9802836482067,
118.709253487314)) ;
#159901 = CARTESIAN_POINT('Ctrl Pts',(-12.9861723417227,-13.0091921750313,
118.642571963292)) ;
#159902 = CARTESIAN_POINT('Ctrl Pts',(-13.0191734609878,-13.2902503547293,
118.707745845769)) ;
#159903 = CARTESIAN_POINT('Ctrl Pts',(-12.9956755887425,-13.2995791016308,
118.636175120335)) ;
#159904 = CARTESIAN_POINT('Ctrl Pts',(-13.0694794359814,-13.2995792074157,
118.611944090282)) ;
#159905 = CARTESIAN_POINT('Ctrl Pts',(-13.1432832832204,-13.2995793132006,
118.587713060228)) ;
#159906 = CARTESIAN_POINT('Ctrl Pts',(-13.1667811554657,-13.2902505662991,
118.659283785661)) ;
#159907 = CARTESIAN_POINT('Ctrl Pts',(-13.190279027711,-13.2809218193976,
118.730854511095)) ;
#159908 = CARTESIAN_POINT('Ctrl Pts',(-13.1164751804721,-13.2809217136127,
118.755085541148)) ;
#159909 = CARTESIAN_POINT('Ctrl Pts',(-13.0426713332331,-13.2809216078278,
118.779316571202)) ;
#159910 = CARTESIAN_POINT('Ctrl Pts',(-13.0191734609878,-13.2902503547293,
118.707745845769)) ;
#159911 = CARTESIAN_POINT('Ctrl Pts',(-13.028209715569,-13.5823834440121,
118.699683255514)) ;
#159912 = CARTESIAN_POINT('Ctrl Pts',(-13.0047821035049,-13.5713305139235,
118.628326531197)) ;
#159913 = CARTESIAN_POINT('Ctrl Pts',(-13.0785859419211,-13.5713306161393,
118.604095474271)) ;
#159914 = CARTESIAN_POINT('Ctrl Pts',(-13.1523897803373,-13.5713307183552,
118.579864417345)) ;
#159915 = CARTESIAN_POINT('Ctrl Pts',(-13.1758173924015,-13.5823836484438,
118.651221141661)) ;
#159916 = CARTESIAN_POINT('Ctrl Pts',(-13.1992450044656,-13.5934365785324,
118.722577865978)) ;
#159917 = CARTESIAN_POINT('Ctrl Pts',(-13.1254411660494,-13.5934364763166,
118.746808922905)) ;
#159918 = CARTESIAN_POINT('Ctrl Pts',(-13.0516373276332,-13.5934363741007,
118.771039979831)) ;
#159919 = CARTESIAN_POINT('Ctrl Pts',(-13.028209715569,-13.5823834440121,
118.699683255514)) ;
#159920 = CARTESIAN_POINT('Ctrl Pts',(-13.0130366717192,-13.8618181146796,
118.617988137292)) ;
#159921 = CARTESIAN_POINT('Ctrl Pts',(-12.9913674586558,-13.8312391943693,
118.551987212537)) ;
#159922 = CARTESIAN_POINT('Ctrl Pts',(-13.0651712893114,-13.8312392849538,
118.527756131973)) ;
#159923 = CARTESIAN_POINT('Ctrl Pts',(-13.138975119967,-13.8312393755383,
118.503525051408)) ;
#159924 = CARTESIAN_POINT('Ctrl Pts',(-13.1606443330303,-13.8618182958485,
118.569525976164)) ;
#159925 = CARTESIAN_POINT('Ctrl Pts',(-13.1823135460937,-13.8923972161587,
118.635526900919)) ;
#159926 = CARTESIAN_POINT('Ctrl Pts',(-13.1085097154381,-13.8923971255743,
118.659757981483)) ;
#159927 = CARTESIAN_POINT('Ctrl Pts',(-13.0347058847825,-13.8923970349898,
118.683989062047)) ;
#159928 = CARTESIAN_POINT('Ctrl Pts',(-13.0130366717192,-13.8618181146796,
118.617988137292)) ;
#159929 = CARTESIAN_POINT('Ctrl Pts',(-12.9759659852745,-14.1083106024044,
118.469780251358)) ;
#159930 = CARTESIAN_POINT('Ctrl Pts',(-12.957582964321,-14.0604763693046,
118.413788537469)) ;
#159931 = CARTESIAN_POINT('Ctrl Pts',(-13.0313867887157,-14.0604764428427,
118.389557437835)) ;
#159932 = CARTESIAN_POINT('Ctrl Pts',(-13.1051906131104,-14.0604765163808,
118.365326338202)) ;
#159933 = CARTESIAN_POINT('Ctrl Pts',(-13.1235736340638,-14.1083107494807,
118.42131805209)) ;
#159934 = CARTESIAN_POINT('Ctrl Pts',(-13.1419566550173,-14.1561449825805,
118.477309765979)) ;
#159935 = CARTESIAN_POINT('Ctrl Pts',(-13.0681528306226,-14.1561449090424,
118.501540865613)) ;
#159936 = CARTESIAN_POINT('Ctrl Pts',(-12.994349006228,-14.1561448355042,
118.525771965247)) ;
#159937 = CARTESIAN_POINT('Ctrl Pts',(-12.9759659852745,-14.1083106024044,
118.469780251358)) ;
#159938 = CARTESIAN_POINT('Ctrl Pts',(-12.9198792403032,-14.3070623418306,
118.263416505571)) ;
#159939 = CARTESIAN_POINT('Ctrl Pts',(-12.906119592085,-14.2452796350311,
118.221506838939)) ;
#159940 = CARTESIAN_POINT('Ctrl Pts',(-12.9799234125691,-14.2452796860699,
118.197275727394)) ;
#159941 = CARTESIAN_POINT('Ctrl Pts',(-13.0537272330532,-14.2452797371086,
118.173044615849)) ;
#159942 = CARTESIAN_POINT('Ctrl Pts',(-13.0674868812713,-14.3070624439081,
118.214954282482)) ;
#159943 = CARTESIAN_POINT('Ctrl Pts',(-13.0812465294895,-14.3688451507076,
118.256863949114)) ;
#159944 = CARTESIAN_POINT('Ctrl Pts',(-13.0074427090054,-14.3688450996689,
118.281095060659)) ;
#159945 = CARTESIAN_POINT('Ctrl Pts',(-12.9336388885213,-14.3688450486301,
118.305326172203)) ;
#159946 = CARTESIAN_POINT('Ctrl Pts',(-12.9198792403032,-14.3070623418306,
118.263416505571)) ;
#159947 = CARTESIAN_POINT('Ctrl Pts',(-12.849560606782,-14.4418892785907,
118.013651989613)) ;
#159948 = CARTESIAN_POINT('Ctrl Pts',(-12.8414260041814,-14.370599628049,
117.988875304187)) ;
#159949 = CARTESIAN_POINT('Ctrl Pts',(-12.9152298234765,-14.3705996550827,
117.964644189021)) ;
#159950 = CARTESIAN_POINT('Ctrl Pts',(-12.9890336427715,-14.3705996821164,
117.940413073854)) ;
#159951 = CARTESIAN_POINT('Ctrl Pts',(-12.9971682453721,-14.4418893326581,
117.96518975928)) ;
#159952 = CARTESIAN_POINT('Ctrl Pts',(-13.0053028479727,-14.5131789831999,
117.989966444705)) ;
#159953 = CARTESIAN_POINT('Ctrl Pts',(-12.9314990286777,-14.5131789561661,
118.014197559872)) ;
#159954 = CARTESIAN_POINT('Ctrl Pts',(-12.8576952093826,-14.5131789291324,
118.038428675038)) ;
#159955 = CARTESIAN_POINT('Ctrl Pts',(-12.849560606782,-14.4418892785907,
118.013651989613)) ;
#159956 = CARTESIAN_POINT('Ctrl Pts',(-12.7712938037721,-14.502692884587,
117.739819479159)) ;
#159957 = CARTESIAN_POINT('Ctrl Pts',(-12.7693448921635,-14.4270502382033,
117.733883410297)) ;
#159958 = CARTESIAN_POINT('Ctrl Pts',(-12.8431487123452,-14.4270502433144,
117.709652297831)) ;
#159959 = CARTESIAN_POINT('Ctrl Pts',(-12.9169525325268,-14.4270502484255,
117.685421185365)) ;
#159960 = CARTESIAN_POINT('Ctrl Pts',(-12.9189014441354,-14.5026928948091,
117.691357254227)) ;
#159961 = CARTESIAN_POINT('Ctrl Pts',(-12.920850355744,-14.5783355411928,
117.697293323088)) ;
#159962 = CARTESIAN_POINT('Ctrl Pts',(-12.8470465355624,-14.5783355360817,
117.721524435554)) ;
#159963 = CARTESIAN_POINT('Ctrl Pts',(-12.7732427153807,-14.5783355309706,
117.74575554802)) ;
#159964 = CARTESIAN_POINT('Ctrl Pts',(-12.7712938037721,-14.502692884587,
117.739819479159)) ;
#159965 = CARTESIAN_POINT('Ctrl Pts',(-12.691443150556,-14.4862255258319,
117.461283982672)) ;
#159966 = CARTESIAN_POINT('Ctrl Pts',(-12.6957973956779,-14.4116185668452,
117.474546312073)) ;
#159967 = CARTESIAN_POINT('Ctrl Pts',(-12.7696012182988,-14.4116185533067,
117.450315207036)) ;
#159968 = CARTESIAN_POINT('Ctrl Pts',(-12.8434050409197,-14.4116185397681,
117.426084102)) ;
#159969 = CARTESIAN_POINT('Ctrl Pts',(-12.8390507957978,-14.4862254987549,
117.412821772599)) ;
#159970 = CARTESIAN_POINT('Ctrl Pts',(-12.8346965506758,-14.5608324577416,
117.399559443198)) ;
#159971 = CARTESIAN_POINT('Ctrl Pts',(-12.7608927280549,-14.5608324712802,
117.423790548234)) ;
#159972 = CARTESIAN_POINT('Ctrl Pts',(-12.687088905434,-14.5608324848187,
117.448021653271)) ;
#159973 = CARTESIAN_POINT('Ctrl Pts',(-12.691443150556,-14.4862255258319,
117.461283982672)) ;
#159974 = CARTESIAN_POINT('Ctrl Pts',(-12.6158746315244,-14.3934141564473,
117.195652815533)) ;
#159975 = CARTESIAN_POINT('Ctrl Pts',(-12.6262454854695,-14.3251742595679,
117.227240764473)) ;
#159976 = CARTESIAN_POINT('Ctrl Pts',(-12.700049312281,-14.325174232371,117.203009672201)) ;
#159977 = CARTESIAN_POINT('Ctrl Pts',(-12.7738531390925,-14.3251742051741,
117.178778579928)) ;
#159978 = CARTESIAN_POINT('Ctrl Pts',(-12.7634822851474,-14.3934141020535,
117.147190630988)) ;
#159979 = CARTESIAN_POINT('Ctrl Pts',(-12.7531114312024,-14.4616539989329,
117.115602682048)) ;
#159980 = CARTESIAN_POINT('Ctrl Pts',(-12.6793076043909,-14.4616540261298,
117.139833774321)) ;
#159981 = CARTESIAN_POINT('Ctrl Pts',(-12.6055037775794,-14.4616540533267,
117.164064866593)) ;
#159982 = CARTESIAN_POINT('Ctrl Pts',(-12.6158746315244,-14.3934141564473,
117.195652815533)) ;
#159983 = CARTESIAN_POINT('Ctrl Pts',(-12.5509163096876,-14.2302607448999,
116.962257398382)) ;
#159984 = CARTESIAN_POINT('Ctrl Pts',(-12.5665738753727,-14.1733086335148,
117.009947818093)) ;
#159985 = CARTESIAN_POINT('Ctrl Pts',(-12.6403777072618,-14.1733085993244,
116.985716741286)) ;
#159986 = CARTESIAN_POINT('Ctrl Pts',(-12.7141815391508,-14.173308565134,
116.961485664479)) ;
#159987 = CARTESIAN_POINT('Ctrl Pts',(-12.6985239734657,-14.2302606765191,
116.913795244768)) ;
#159988 = CARTESIAN_POINT('Ctrl Pts',(-12.6828664077805,-14.2872127879042,
116.866104825057)) ;
#159989 = CARTESIAN_POINT('Ctrl Pts',(-12.6090625758915,-14.2872128220946,
116.890335901864)) ;
#159990 = CARTESIAN_POINT('Ctrl Pts',(-12.5352587440024,-14.287212856285,
116.914566978671)) ;
#159991 = CARTESIAN_POINT('Ctrl Pts',(-12.5509163096876,-14.2302607448999,
116.962257398382)) ;
#159992 = CARTESIAN_POINT('Ctrl Pts',(-12.5022332898898,-14.0081666908763,
116.778385267356)) ;
#159993 = CARTESIAN_POINT('Ctrl Pts',(-12.5220503757503,-13.9666350467411,
116.838744914192)) ;
#159994 = CARTESIAN_POINT('Ctrl Pts',(-12.5958542125087,-13.9666350124539,
116.814513852216)) ;
#159995 = CARTESIAN_POINT('Ctrl Pts',(-12.6696580492672,-13.9666349781666,
116.790282790241)) ;
#159996 = CARTESIAN_POINT('Ctrl Pts',(-12.6498409634067,-14.0081666223018,
116.729923143405)) ;
#159997 = CARTESIAN_POINT('Ctrl Pts',(-12.6300238775463,-14.0496982664369,
116.669563496569)) ;
#159998 = CARTESIAN_POINT('Ctrl Pts',(-12.5562200407878,-14.0496983007242,
116.693794558544)) ;
#159999 = CARTESIAN_POINT('Ctrl Pts',(-12.4824162040293,-14.0496983350115,
116.71802562052)) ;
#160000 = CARTESIAN_POINT('Ctrl Pts',(-12.5022332898898,-14.0081666908763,
116.778385267356)) ;
#160001 = CARTESIAN_POINT('Ctrl Pts',(-12.4742506823548,-13.7466548362381,
116.657950049822)) ;
#160002 = CARTESIAN_POINT('Ctrl Pts',(-12.4967799149851,-13.7233199580348,
116.726570457999)) ;
#160003 = CARTESIAN_POINT('Ctrl Pts',(-12.5705837553633,-13.7233199251522,
116.702339407048)) ;
#160004 = CARTESIAN_POINT('Ctrl Pts',(-12.6443875957415,-13.7233198922696,
116.678108356097)) ;
#160005 = CARTESIAN_POINT('Ctrl Pts',(-12.6218583631112,-13.7466547704729,
116.609487947921)) ;
#160006 = CARTESIAN_POINT('Ctrl Pts',(-12.5993291304809,-13.7699896486762,
116.540867539744)) ;
#160007 = CARTESIAN_POINT('Ctrl Pts',(-12.5255252901027,-13.7699896815587,
116.565098590695)) ;
#160008 = CARTESIAN_POINT('Ctrl Pts',(-12.4517214497245,-13.7699897144413,
116.589329641646)) ;
#160009 = CARTESIAN_POINT('Ctrl Pts',(-12.4742506823548,-13.7466548362381,
116.657950049822)) ;
#160010 = CARTESIAN_POINT('Ctrl Pts',(-12.4691100549571,-13.4587847124533,
116.606699386214)) ;
#160011 = CARTESIAN_POINT('Ctrl Pts',(-12.4927690498238,-13.4555144548359,
116.678760867692)) ;
#160012 = CARTESIAN_POINT('Ctrl Pts',(-12.5665728932212,-13.4555144300918,
116.654529825937)) ;
#160013 = CARTESIAN_POINT('Ctrl Pts',(-12.6403767366186,-13.4555144053477,
116.630298784182)) ;
#160014 = CARTESIAN_POINT('Ctrl Pts',(-12.6167177417518,-13.4587846629652,
116.558237302705)) ;
#160015 = CARTESIAN_POINT('Ctrl Pts',(-12.5930587468851,-13.4620549205826,
116.486175821228)) ;
#160016 = CARTESIAN_POINT('Ctrl Pts',(-12.5192549034877,-13.4620549453267,
116.510406862983)) ;
#160017 = CARTESIAN_POINT('Ctrl Pts',(-12.4454510600903,-13.4620549700708,
116.534637904737)) ;
#160018 = CARTESIAN_POINT('Ctrl Pts',(-12.4691100549571,-13.4587847124533,
116.606699386214)) ;
#160019 = CARTESIAN_POINT('Ctrl Pts',(-12.4885192361608,-13.1685102080527,
116.630294437279)) ;
#160020 = CARTESIAN_POINT('Ctrl Pts',(-12.5115939319546,-13.1855034690251,
116.700576237899)) ;
#160021 = CARTESIAN_POINT('Ctrl Pts',(-12.5853977767225,-13.1855034529917,
116.676345200319)) ;
#160022 = CARTESIAN_POINT('Ctrl Pts',(-12.6592016214903,-13.1855034369582,
116.652114162738)) ;
#160023 = CARTESIAN_POINT('Ctrl Pts',(-12.6361269256965,-13.1685101759858,
116.581832362118)) ;
#160024 = CARTESIAN_POINT('Ctrl Pts',(-12.6130522299027,-13.1515169150133,
116.511550561497)) ;
#160025 = CARTESIAN_POINT('Ctrl Pts',(-12.5392483851348,-13.1515169310468,
116.535781599078)) ;
#160026 = CARTESIAN_POINT('Ctrl Pts',(-12.465444540367,-13.1515169470802,
116.560012636658)) ;
#160027 = CARTESIAN_POINT('Ctrl Pts',(-12.4885192361608,-13.1685102080527,
116.630294437279)) ;
#160028 = CARTESIAN_POINT('Ctrl Pts',(-12.5312093541707,-12.8978336872395,
116.725034238603)) ;
#160029 = CARTESIAN_POINT('Ctrl Pts',(-12.5520681509441,-12.9337522455578,
116.788566768234)) ;
#160030 = CARTESIAN_POINT('Ctrl Pts',(-12.6258719961565,-12.9337522361366,
116.764335732008)) ;
#160031 = CARTESIAN_POINT('Ctrl Pts',(-12.6996758413689,-12.9337522267154,
116.740104695781)) ;
#160032 = CARTESIAN_POINT('Ctrl Pts',(-12.6788170445955,-12.897833668397,
116.67657216615)) ;
#160033 = CARTESIAN_POINT('Ctrl Pts',(-12.657958247822,-12.8619151100786,
116.613039636519)) ;
#160034 = CARTESIAN_POINT('Ctrl Pts',(-12.5841544026096,-12.8619151194999,
116.637270672746)) ;
#160035 = CARTESIAN_POINT('Ctrl Pts',(-12.5103505573972,-12.8619151289211,
116.661501708972)) ;
#160036 = CARTESIAN_POINT('Ctrl Pts',(-12.5312093541707,-12.8978336872395,
116.725034238603)) ;
#160037 = CARTESIAN_POINT('Ctrl Pts',(-12.5957395733222,-12.6619537350285,
116.885954892402)) ;
#160038 = CARTESIAN_POINT('Ctrl Pts',(-12.612861275193,-12.7143974709413,
116.938104833802)) ;
#160039 = CARTESIAN_POINT('Ctrl Pts',(-12.6866651195987,-12.714397468419,
116.913873795118)) ;
#160040 = CARTESIAN_POINT('Ctrl Pts',(-12.7604689640043,-12.7143974658967,
116.889642756435)) ;
#160041 = CARTESIAN_POINT('Ctrl Pts',(-12.7433472621335,-12.6619537299839,
116.837492815035)) ;
#160042 = CARTESIAN_POINT('Ctrl Pts',(-12.7262255602627,-12.6095099940711,
116.785342873635)) ;
#160043 = CARTESIAN_POINT('Ctrl Pts',(-12.652421715857,-12.6095099965934,
116.809573912318)) ;
#160044 = CARTESIAN_POINT('Ctrl Pts',(-12.5786178714514,-12.6095099991157,
116.833804951002)) ;
#160045 = CARTESIAN_POINT('Ctrl Pts',(-12.5957395733222,-12.6619537350285,
116.885954892402)) ;
#160046 = CARTESIAN_POINT('Ctrl Pts',(-12.6776143419512,-12.4816257056073,
117.099854766256)) ;
#160047 = CARTESIAN_POINT('Ctrl Pts',(-12.6897787676254,-12.5467399887244,
117.136905644134)) ;
#160048 = CARTESIAN_POINT('Ctrl Pts',(-12.7635826110348,-12.5467399890346,
117.112674602415)) ;
#160049 = CARTESIAN_POINT('Ctrl Pts',(-12.8373864544442,-12.5467399893448,
117.088443560697)) ;
#160050 = CARTESIAN_POINT('Ctrl Pts',(-12.8252220287701,-12.4816257062277,
117.051392682819)) ;
#160051 = CARTESIAN_POINT('Ctrl Pts',(-12.8130576030959,-12.4165114231106,
117.014341804942)) ;
#160052 = CARTESIAN_POINT('Ctrl Pts',(-12.7392537596865,-12.4165114228005,
117.03857284666)) ;
#160053 = CARTESIAN_POINT('Ctrl Pts',(-12.6654499162771,-12.4165114224903,
117.062803888378)) ;
#160054 = CARTESIAN_POINT('Ctrl Pts',(-12.6776143419512,-12.4816257056073,
117.099854766256)) ;
#160055 = CARTESIAN_POINT('Ctrl Pts',(-12.7713529617644,-12.3684889471066,
117.350055385643)) ;
#160056 = CARTESIAN_POINT('Ctrl Pts',(-12.7777208023874,-12.441600008621,
117.369450800684)) ;
#160057 = CARTESIAN_POINT('Ctrl Pts',(-12.8515246450419,-12.441600009445,
117.345219756667)) ;
#160058 = CARTESIAN_POINT('Ctrl Pts',(-12.9253284876963,-12.4416000102689,
117.320988712649)) ;
#160059 = CARTESIAN_POINT('Ctrl Pts',(-12.9189606470733,-12.3684889487544,
117.301593297608)) ;
#160060 = CARTESIAN_POINT('Ctrl Pts',(-12.9125928064503,-12.2953778872399,
117.282197882567)) ;
#160061 = CARTESIAN_POINT('Ctrl Pts',(-12.8387889637959,-12.295377886416,
117.306428926584)) ;
#160062 = CARTESIAN_POINT('Ctrl Pts',(-12.7649851211414,-12.2953778855921,
117.330659970602)) ;
#160063 = CARTESIAN_POINT('Ctrl Pts',(-12.7713529617644,-12.3684889471066,
117.350055385643)) ;
#160064 = CARTESIAN_POINT('Ctrl Pts',(-12.8723202400041,-12.3299903879882,
117.621972650026)) ;
#160065 = CARTESIAN_POINT('Ctrl Pts',(-12.8723839341267,-12.4058988295515,
117.622166651981)) ;
#160066 = CARTESIAN_POINT('Ctrl Pts',(-12.9461877764825,-12.4058988295036,
117.597935607054)) ;
#160067 = CARTESIAN_POINT('Ctrl Pts',(-13.0199916188383,-12.4058988294557,
117.573704562126)) ;
#160068 = CARTESIAN_POINT('Ctrl Pts',(-13.0199279247158,-12.3299903878923,
117.573510560171)) ;
#160069 = CARTESIAN_POINT('Ctrl Pts',(-13.0198642305932,-12.254081946329,
117.573316558216)) ;
#160070 = CARTESIAN_POINT('Ctrl Pts',(-12.9460603882374,-12.2540819463769,
117.597547603144)) ;
#160071 = CARTESIAN_POINT('Ctrl Pts',(-12.8722565458816,-12.2540819464249,
117.621778648071)) ;
#160072 = CARTESIAN_POINT('Ctrl Pts',(-12.8723202400041,-12.3299903879882,
117.621972650026)) ;
#160073 = CARTESIAN_POINT('Ctrl Pts',(-12.9724385289638,-12.3696139932957,
117.891584408557)) ;
#160074 = CARTESIAN_POINT('Ctrl Pts',(-12.9662425210927,-12.4428670872802,
117.872712368267)) ;
#160075 = CARTESIAN_POINT('Ctrl Pts',(-13.040046363953,-12.4428670865975,
117.848481324877)) ;
#160076 = CARTESIAN_POINT('Ctrl Pts',(-13.1138502068133,-12.4428670859149,
117.824250281486)) ;
#160077 = CARTESIAN_POINT('Ctrl Pts',(-13.1200462146844,-12.3696139919303,
117.843122321775)) ;
#160078 = CARTESIAN_POINT('Ctrl Pts',(-13.1262422225556,-12.2963608979458,
117.861994362065)) ;
#160079 = CARTESIAN_POINT('Ctrl Pts',(-13.0524383796953,-12.2963608986285,
117.886225405455)) ;
#160080 = CARTESIAN_POINT('Ctrl Pts',(-12.978634536835,-12.2963608993112,
117.910456448846)) ;
#160081 = CARTESIAN_POINT('Ctrl Pts',(-12.9724385289638,-12.3696139932957,
117.891584408557)) ;
#160082 = CARTESIAN_POINT('Ctrl Pts',(-13.0664515487238,-12.4839372794238,
118.142479880966)) ;
#160083 = CARTESIAN_POINT('Ctrl Pts',(-13.0544155149314,-12.5493150647165,
118.105820064064)) ;
#160084 = CARTESIAN_POINT('Ctrl Pts',(-13.1282193587287,-12.5493150649477,
118.081589023527)) ;
#160085 = CARTESIAN_POINT('Ctrl Pts',(-13.2020232025261,-12.549315065179,
118.057357982991)) ;
#160086 = CARTESIAN_POINT('Ctrl Pts',(-13.2140592363185,-12.4839372798862,
118.094017799893)) ;
#160087 = CARTESIAN_POINT('Ctrl Pts',(-13.2260952701109,-12.4185594945934,
118.130677616795)) ;
#160088 = CARTESIAN_POINT('Ctrl Pts',(-13.1522914263136,-12.4185594943622,
118.154908657331)) ;
#160089 = CARTESIAN_POINT('Ctrl Pts',(-13.0784875825162,-12.418559494131,
118.179139697867)) ;
#160090 = CARTESIAN_POINT('Ctrl Pts',(-13.0664515487238,-12.4839372794238,
118.142479880966)) ;
#160091 = CARTESIAN_POINT('Ctrl Pts',(-13.1484405032608,-12.6667316342934,
118.356525775525)) ;
#160092 = CARTESIAN_POINT('Ctrl Pts',(-13.1314001129427,-12.7194414647668,
118.304623496218)) ;
#160093 = CARTESIAN_POINT('Ctrl Pts',(-13.2052039581057,-12.7194414698136,
118.280392459841)) ;
#160094 = CARTESIAN_POINT('Ctrl Pts',(-13.2790078032687,-12.7194414748605,
118.256161423465)) ;
#160095 = CARTESIAN_POINT('Ctrl Pts',(-13.2960481935868,-12.6667316443871,
118.308063702771)) ;
#160096 = CARTESIAN_POINT('Ctrl Pts',(-13.3130885839048,-12.6140218139138,
118.359965982077)) ;
#160097 = CARTESIAN_POINT('Ctrl Pts',(-13.2392847387418,-12.6140218088669,
118.384197018454)) ;
#160098 = CARTESIAN_POINT('Ctrl Pts',(-13.1654808935788,-12.6140218038201,
118.408428054831)) ;
#160099 = CARTESIAN_POINT('Ctrl Pts',(-13.1484405032608,-12.6667316342934,
118.356525775525)) ;
#160100 = CARTESIAN_POINT('Ctrl Pts',(-13.2121850011556,-12.9020313562946,
118.515277498017)) ;
#160101 = CARTESIAN_POINT('Ctrl Pts',(-13.191401639139,-12.9383882322268,
118.45197473096)) ;
#160102 = CARTESIAN_POINT('Ctrl Pts',(-13.265205484716,-12.9383882439588,
118.427743695844)) ;
#160103 = CARTESIAN_POINT('Ctrl Pts',(-13.3390093302929,-12.9383882556908,
118.403512660728)) ;
#160104 = CARTESIAN_POINT('Ctrl Pts',(-13.3597926923095,-12.9020313797586,
118.466815427784)) ;
#160105 = CARTESIAN_POINT('Ctrl Pts',(-13.3805760543261,-12.8656745038264,
118.530118194841)) ;
#160106 = CARTESIAN_POINT('Ctrl Pts',(-13.3067722087492,-12.8656744920944,
118.554349229957)) ;
#160107 = CARTESIAN_POINT('Ctrl Pts',(-13.2329683631722,-12.8656744803624,
118.578580265073)) ;
#160108 = CARTESIAN_POINT('Ctrl Pts',(-13.2121850011556,-12.9020313562946,
118.515277498017)) ;
#160109 = CARTESIAN_POINT('Ctrl Pts',(-13.2546371352095,-13.1740426154344,
118.609174623203)) ;
#160110 = CARTESIAN_POINT('Ctrl Pts',(-13.2315922119599,-13.1914596717363,
118.538983505663)) ;
#160111 = CARTESIAN_POINT('Ctrl Pts',(-13.3053960569823,-13.1914596914773,
118.514752468858)) ;
#160112 = CARTESIAN_POINT('Ctrl Pts',(-13.3791999020048,-13.1914597112182,
118.490521432053)) ;
#160113 = CARTESIAN_POINT('Ctrl Pts',(-13.4022448252544,-13.1740426549163,
118.560712549593)) ;
#160114 = CARTESIAN_POINT('Ctrl Pts',(-13.4252897485041,-13.1566255986144,
118.630903667132)) ;
#160115 = CARTESIAN_POINT('Ctrl Pts',(-13.3514859034817,-13.1566255788734,
118.655134703937)) ;
#160116 = CARTESIAN_POINT('Ctrl Pts',(-13.2776820584592,-13.1566255591325,
118.679365740742)) ;
#160117 = CARTESIAN_POINT('Ctrl Pts',(-13.2546371352095,-13.1740426154344,
118.609174623203)) ;
#160118 = CARTESIAN_POINT('Ctrl Pts',(-13.2734900958146,-13.4634545824485,
118.631199247328)) ;
#160119 = CARTESIAN_POINT('Ctrl Pts',(-13.2498280242855,-13.4606896668886,
118.559128395849)) ;
#160120 = CARTESIAN_POINT('Ctrl Pts',(-13.3236318675582,-13.4606896946661,
118.534897353714)) ;
#160121 = CARTESIAN_POINT('Ctrl Pts',(-13.3974357108309,-13.4606897224437,
118.51066631158)) ;
#160122 = CARTESIAN_POINT('Ctrl Pts',(-13.42109778236,-13.4634546380036,118.58273716306)) ;
#160123 = CARTESIAN_POINT('Ctrl Pts',(-13.4447598538892,-13.4662195535635,
118.654808014539)) ;
#160124 = CARTESIAN_POINT('Ctrl Pts',(-13.3709560106164,-13.466219525786,
118.679039056674)) ;
#160125 = CARTESIAN_POINT('Ctrl Pts',(-13.2971521673437,-13.4662194980085,
118.703270098808)) ;
#160126 = CARTESIAN_POINT('Ctrl Pts',(-13.2734900958146,-13.4634545824485,
118.631199247328)) ;
#160127 = CARTESIAN_POINT('Ctrl Pts',(-13.2680796257058,-13.7505708131454,
118.579201045788)) ;
#160128 = CARTESIAN_POINT('Ctrl Pts',(-13.245496029926,-13.7277551955946,
118.510415057603)) ;
#160129 = CARTESIAN_POINT('Ctrl Pts',(-13.3192998700676,-13.7277552307989,
118.486184005931)) ;
#160130 = CARTESIAN_POINT('Ctrl Pts',(-13.3931037102092,-13.7277552660031,
118.46195295426)) ;
#160131 = CARTESIAN_POINT('Ctrl Pts',(-13.415687305989,-13.7505708835539,
118.530738942446)) ;
#160132 = CARTESIAN_POINT('Ctrl Pts',(-13.4382709017688,-13.7733865011047,
118.599524930632)) ;
#160133 = CARTESIAN_POINT('Ctrl Pts',(-13.3644670616272,-13.7733864659004,
118.623755982303)) ;
#160134 = CARTESIAN_POINT('Ctrl Pts',(-13.2906632214856,-13.7733864306961,
118.647987033974)) ;
#160135 = CARTESIAN_POINT('Ctrl Pts',(-13.2680796257058,-13.7505708131454,
118.579201045788)) ;
#160136 = CARTESIAN_POINT('Ctrl Pts',(-13.2394962360415,-14.0133363300327,
118.456684613439)) ;
#160137 = CARTESIAN_POINT('Ctrl Pts',(-13.2196093760611,-13.9721415095329,
118.396112447548)) ;
#160138 = CARTESIAN_POINT('Ctrl Pts',(-13.2934132119228,-13.9721415478717,
118.371881382841)) ;
#160139 = CARTESIAN_POINT('Ctrl Pts',(-13.3672170477845,-13.9721415862106,
118.347650318134)) ;
#160140 = CARTESIAN_POINT('Ctrl Pts',(-13.3871039077648,-14.0133364067105,
118.408222484025)) ;
#160141 = CARTESIAN_POINT('Ctrl Pts',(-13.4069907677452,-14.0545312272103,
118.468794649916)) ;
#160142 = CARTESIAN_POINT('Ctrl Pts',(-13.3331869318835,-14.0545311888715,
118.493025714623)) ;
#160143 = CARTESIAN_POINT('Ctrl Pts',(-13.2593830960218,-14.0545311505326,
118.51725677933)) ;
#160144 = CARTESIAN_POINT('Ctrl Pts',(-13.2394962360415,-14.0133363300327,
118.456684613439)) ;
#160145 = CARTESIAN_POINT('Ctrl Pts',(-13.1905999974754,-14.2335678065818,
118.272293478368)) ;
#160146 = CARTESIAN_POINT('Ctrl Pts',(-13.1748320592631,-14.1769371406859,
118.224266883765)) ;
#160147 = CARTESIAN_POINT('Ctrl Pts',(-13.2486358902102,-14.1769371770333,
118.200035804088)) ;
#160148 = CARTESIAN_POINT('Ctrl Pts',(-13.3224397211572,-14.1769372133807,
118.175804724412)) ;
#160149 = CARTESIAN_POINT('Ctrl Pts',(-13.3382076593695,-14.2335678792767,
118.223831319015)) ;
#160150 = CARTESIAN_POINT('Ctrl Pts',(-13.3539755975818,-14.2901985451726,
118.271857913619)) ;
#160151 = CARTESIAN_POINT('Ctrl Pts',(-13.2801717666348,-14.2901985088252,
118.296088993295)) ;
#160152 = CARTESIAN_POINT('Ctrl Pts',(-13.2063679356877,-14.2901984724778,
118.320320072971)) ;
#160153 = CARTESIAN_POINT('Ctrl Pts',(-13.1905999974754,-14.2335678065818,
118.272293478368)) ;
#160154 = CARTESIAN_POINT('Ctrl Pts',(-13.1253712311633,-14.3958087768564,
118.038043104771)) ;
#160155 = CARTESIAN_POINT('Ctrl Pts',(-13.114870684948,-14.3277685970779,
118.006060136485)) ;
#160156 = CARTESIAN_POINT('Ctrl Pts',(-13.1886745106335,-14.3277686257104,
117.981829040783)) ;
#160157 = CARTESIAN_POINT('Ctrl Pts',(-13.2624783363189,-14.327768654343,
117.957597945081)) ;
#160158 = CARTESIAN_POINT('Ctrl Pts',(-13.2729788825342,-14.3958088341215,
117.989580913366)) ;
#160159 = CARTESIAN_POINT('Ctrl Pts',(-13.2834794287496,-14.4638490139001,
118.021563881652)) ;
#160160 = CARTESIAN_POINT('Ctrl Pts',(-13.2096756030641,-14.4638489852675,
118.045794977354)) ;
#160161 = CARTESIAN_POINT('Ctrl Pts',(-13.1358717773787,-14.463848956635,
118.070026073057)) ;
#160162 = CARTESIAN_POINT('Ctrl Pts',(-13.1253712311633,-14.3958087768564,
118.038043104771)) ;
#160163 = CARTESIAN_POINT('Ctrl Pts',(-13.0496091296525,-14.4872051600084,
117.771802663667)) ;
#160164 = CARTESIAN_POINT('Ctrl Pts',(-13.0451171023842,-14.4126853477426,
117.758120674782)) ;
#160165 = CARTESIAN_POINT('Ctrl Pts',(-13.1189209238047,-14.4126853615341,
117.73388956609)) ;
#160166 = CARTESIAN_POINT('Ctrl Pts',(-13.1927247452252,-14.4126853753255,
117.709658457397)) ;
#160167 = CARTESIAN_POINT('Ctrl Pts',(-13.1972167724935,-14.4872051875913,
117.723340446282)) ;
#160168 = CARTESIAN_POINT('Ctrl Pts',(-13.2017087997618,-14.561724999857,
117.737022435167)) ;
#160169 = CARTESIAN_POINT('Ctrl Pts',(-13.1279049783413,-14.5617249860656,
117.761253543859)) ;
#160170 = CARTESIAN_POINT('Ctrl Pts',(-13.0541011569208,-14.5617249722742,
117.785484652552)) ;
#160171 = CARTESIAN_POINT('Ctrl Pts',(-13.0496091296525,-14.4872051600084,
117.771802663667)) ;
#160172 = CARTESIAN_POINT('Ctrl Pts',(-12.9697977471393,-14.5023836342265,
117.493417412762)) ;
#160173 = CARTESIAN_POINT('Ctrl Pts',(-12.9716017236427,-14.4266966491582,
117.498912035629)) ;
#160174 = CARTESIAN_POINT('Ctrl Pts',(-13.0454055427674,-14.4266966434283,
117.474680919943)) ;
#160175 = CARTESIAN_POINT('Ctrl Pts',(-13.119209361892,-14.4266966376984,
117.450449804258)) ;
#160176 = CARTESIAN_POINT('Ctrl Pts',(-13.1174053853887,-14.5023836227667,
117.444955181391)) ;
#160177 = CARTESIAN_POINT('Ctrl Pts',(-13.1156014088854,-14.5780706078349,
117.439460558524)) ;
#160178 = CARTESIAN_POINT('Ctrl Pts',(-13.0417975897607,-14.5780706135648,
117.463691674209)) ;
#160179 = CARTESIAN_POINT('Ctrl Pts',(-12.967993770636,-14.5780706192947,
117.487922789895)) ;
#160180 = CARTESIAN_POINT('Ctrl Pts',(-12.9697977471393,-14.5023836342265,
117.493417412762)) ;
#160181 = CARTESIAN_POINT('Ctrl Pts',(-12.8911729784752,-14.4395233841403,
117.218279983479)) ;
#160182 = CARTESIAN_POINT('Ctrl Pts',(-12.8992067287691,-14.3681145695168,
117.242749492307)) ;
#160183 = CARTESIAN_POINT('Ctrl Pts',(-12.9730105467516,-14.3681145402781,
117.218518373143)) ;
#160184 = CARTESIAN_POINT('Ctrl Pts',(-13.046814364734,-14.3681145110395,
117.194287253978)) ;
#160185 = CARTESIAN_POINT('Ctrl Pts',(-13.0387806144401,-14.4395233256629,
117.16981774515)) ;
#160186 = CARTESIAN_POINT('Ctrl Pts',(-13.0307468641462,-14.5109321402864,
117.145348236322)) ;
#160187 = CARTESIAN_POINT('Ctrl Pts',(-12.9569430461637,-14.510932169525,
117.169579355486)) ;
#160188 = CARTESIAN_POINT('Ctrl Pts',(-12.8831392281813,-14.5109321987637,
117.193810474651)) ;
#160189 = CARTESIAN_POINT('Ctrl Pts',(-12.8911729784752,-14.4395233841403,
117.218279983479)) ;
#160190 = CARTESIAN_POINT('Ctrl Pts',(-12.8215722521092,-14.3038981389521,
116.970926660863)) ;
#160191 = CARTESIAN_POINT('Ctrl Pts',(-12.8352086467856,-14.2418546197311,
117.0124609206)) ;
#160192 = CARTESIAN_POINT('Ctrl Pts',(-12.9090124667695,-14.2418545666607,
116.988229807532)) ;
#160193 = CARTESIAN_POINT('Ctrl Pts',(-12.9828162867534,-14.2418545135903,
116.963998694464)) ;
#160194 = CARTESIAN_POINT('Ctrl Pts',(-12.969179892077,-14.3038980328113,
116.922464434726)) ;
#160195 = CARTESIAN_POINT('Ctrl Pts',(-12.9555434974006,-14.3659415520323,
116.880930174989)) ;
#160196 = CARTESIAN_POINT('Ctrl Pts',(-12.8817396774167,-14.3659416051027,
116.905161288057)) ;
#160197 = CARTESIAN_POINT('Ctrl Pts',(-12.8079358574328,-14.3659416581731,
116.929392401125)) ;
#160198 = CARTESIAN_POINT('Ctrl Pts',(-12.8215722521092,-14.3038981389521,
116.970926660863)) ;
#160199 = CARTESIAN_POINT('Ctrl Pts',(-12.765908924504,-14.1052991872385,
116.765996341192)) ;
#160200 = CARTESIAN_POINT('Ctrl Pts',(-12.7841836185283,-14.057030828904,
116.821658112453)) ;
#160201 = CARTESIAN_POINT('Ctrl Pts',(-12.8579874427366,-14.0570307540221,
116.797427012251)) ;
#160202 = CARTESIAN_POINT('Ctrl Pts',(-12.9317912669448,-14.0570306791401,
116.77319591205)) ;
#160203 = CARTESIAN_POINT('Ctrl Pts',(-12.9135165729205,-14.1052990374745,
116.717534140789)) ;
#160204 = CARTESIAN_POINT('Ctrl Pts',(-12.8952418788962,-14.1535673958089,
116.661872369529)) ;
#160205 = CARTESIAN_POINT('Ctrl Pts',(-12.821438054688,-14.1535674706909,
116.68610346973)) ;
#160206 = CARTESIAN_POINT('Ctrl Pts',(-12.7476342304797,-14.1535675455729,
116.710334569932)) ;
#160207 = CARTESIAN_POINT('Ctrl Pts',(-12.765908924504,-14.1052991872385,
116.765996341192)) ;
#160208 = CARTESIAN_POINT('Ctrl Pts',(-12.7289194558588,-13.8563431079666,
116.617783489361)) ;
#160209 = CARTESIAN_POINT('Ctrl Pts',(-12.7505389533844,-13.8253850611036,
116.683632992497)) ;
#160210 = CARTESIAN_POINT('Ctrl Pts',(-12.8243427839167,-13.8253849680989,
116.659401911558)) ;
#160211 = CARTESIAN_POINT('Ctrl Pts',(-12.8981466144491,-13.8253848750942,
116.635170830618)) ;
#160212 = CARTESIAN_POINT('Ctrl Pts',(-12.8765271169234,-13.8563429219572,
116.569321327482)) ;
#160213 = CARTESIAN_POINT('Ctrl Pts',(-12.8549076193978,-13.8873009688202,
116.503471824345)) ;
#160214 = CARTESIAN_POINT('Ctrl Pts',(-12.7811037888655,-13.8873010618249,
116.527702905285)) ;
#160215 = CARTESIAN_POINT('Ctrl Pts',(-12.7072999583332,-13.8873011548297,
116.551933986224)) ;
#160216 = CARTESIAN_POINT('Ctrl Pts',(-12.7289194558588,-13.8563431079666,
116.617783489361)) ;
#160217 = CARTESIAN_POINT('Ctrl Pts',(-12.7143046569284,-13.5768529523028,
116.537845772707)) ;
#160218 = CARTESIAN_POINT('Ctrl Pts',(-12.7377091514829,-13.5653624857166,
116.609132088846)) ;
#160219 = CARTESIAN_POINT('Ctrl Pts',(-12.8115129900551,-13.56536238196,116.584901032395)) ;
#160220 = CARTESIAN_POINT('Ctrl Pts',(-12.8853168286273,-13.5653622782034,
116.560669975944)) ;
#160221 = CARTESIAN_POINT('Ctrl Pts',(-12.8619123340728,-13.5768527447896,
116.489383659805)) ;
#160222 = CARTESIAN_POINT('Ctrl Pts',(-12.8385078395183,-13.5883432113757,
116.418097343665)) ;
#160223 = CARTESIAN_POINT('Ctrl Pts',(-12.7647040009461,-13.5883433151323,
116.442328400117)) ;
#160224 = CARTESIAN_POINT('Ctrl Pts',(-12.6909001623739,-13.5883434188889,
116.466559456568)) ;
#160225 = CARTESIAN_POINT('Ctrl Pts',(-12.7143046569284,-13.5768529523028,
116.537845772707)) ;
#160226 = CARTESIAN_POINT('Ctrl Pts',(-12.7237017190187,-13.2855121533732,
116.530980294664)) ;
#160227 = CARTESIAN_POINT('Ctrl Pts',(-12.7472188965232,-13.2943449974089,
116.602609824933)) ;
#160228 = CARTESIAN_POINT('Ctrl Pts',(-12.8210227439731,-13.2943448909631,
116.578378795522)) ;
#160229 = CARTESIAN_POINT('Ctrl Pts',(-12.894826591423,-13.2943447845173,
116.554147766111)) ;
#160230 = CARTESIAN_POINT('Ctrl Pts',(-12.8713094139185,-13.2855119404815,
116.482518235842)) ;
#160231 = CARTESIAN_POINT('Ctrl Pts',(-12.847792236414,-13.2766790964458,
116.410888705573)) ;
#160232 = CARTESIAN_POINT('Ctrl Pts',(-12.7739883889641,-13.2766792028916,
116.435119734985)) ;
#160233 = CARTESIAN_POINT('Ctrl Pts',(-12.7001845415141,-13.2766793093374,
116.459350764396)) ;
#160234 = CARTESIAN_POINT('Ctrl Pts',(-12.7237017190187,-13.2855121533732,
116.530980294664)) ;
#160235 = CARTESIAN_POINT('Ctrl Pts',(-12.7572168622974,-13.0041275578471,
116.597631042541)) ;
#160236 = CARTESIAN_POINT('Ctrl Pts',(-12.7791619438715,-13.0326186796293,
116.664472222282)) ;
#160237 = CARTESIAN_POINT('Ctrl Pts',(-12.8529658001272,-13.0326185795002,
116.640241219692)) ;
#160238 = CARTESIAN_POINT('Ctrl Pts',(-12.9267696563828,-13.0326184793711,
116.616010217102)) ;
#160239 = CARTESIAN_POINT('Ctrl Pts',(-12.9048245748087,-13.0041273575889,
116.54916903736)) ;
#160240 = CARTESIAN_POINT('Ctrl Pts',(-12.8828794932346,-12.9756362358068,
116.482327857619)) ;
#160241 = CARTESIAN_POINT('Ctrl Pts',(-12.809075636979,-12.9756363359359,
116.506558860209)) ;
#160242 = CARTESIAN_POINT('Ctrl Pts',(-12.7352717807234,-12.975636436065,
116.5307898628)) ;
#160243 = CARTESIAN_POINT('Ctrl Pts',(-12.7572168622974,-13.0041275578471,
116.597631042541)) ;
#160244 = CARTESIAN_POINT('Ctrl Pts',(-12.8130794083186,-12.7524010633512,
116.732371814801)) ;
#160245 = CARTESIAN_POINT('Ctrl Pts',(-12.8318894471127,-12.798508919761,
116.789664160074)) ;
#160246 = CARTESIAN_POINT('Ctrl Pts',(-12.9056933112272,-12.798508834093,
116.765433181421)) ;
#160247 = CARTESIAN_POINT('Ctrl Pts',(-12.9794971753417,-12.7985087484251,
116.741202202767)) ;
#160248 = CARTESIAN_POINT('Ctrl Pts',(-12.9606871365476,-12.7524008920153,
116.683909857494)) ;
#160249 = CARTESIAN_POINT('Ctrl Pts',(-12.9418770977535,-12.7062930356055,
116.626617512222)) ;
#160250 = CARTESIAN_POINT('Ctrl Pts',(-12.868073233639,-12.7062931212734,
116.650848490875)) ;
#160251 = CARTESIAN_POINT('Ctrl Pts',(-12.7942693695245,-12.7062932069414,
116.675079469529)) ;
#160252 = CARTESIAN_POINT('Ctrl Pts',(-12.8130794083186,-12.7524010633512,
116.732371814801)) ;
#160253 = CARTESIAN_POINT('Ctrl Pts',(-12.88854761512,-12.5474082659178,116.92665451824)) ;
#160254 = CARTESIAN_POINT('Ctrl Pts',(-12.9028530268849,-12.6078966446447,
116.970226496376)) ;
#160255 = CARTESIAN_POINT('Ctrl Pts',(-12.9766568970565,-12.6078965805878,
116.945995536171)) ;
#160256 = CARTESIAN_POINT('Ctrl Pts',(-13.050460767228,-12.6078965165309,
116.921764575967)) ;
#160257 = CARTESIAN_POINT('Ctrl Pts',(-13.036155355463,-12.5474081378039,
116.878192597831)) ;
#160258 = CARTESIAN_POINT('Ctrl Pts',(-13.0218499436981,-12.4869197590769,
116.834620619695)) ;
#160259 = CARTESIAN_POINT('Ctrl Pts',(-12.9480460735266,-12.4869198231338,
116.8588515799)) ;
#160260 = CARTESIAN_POINT('Ctrl Pts',(-12.874242203355,-12.4869198871908,
116.883082540105)) ;
#160261 = CARTESIAN_POINT('Ctrl Pts',(-12.88854761512,-12.5474082659178,116.92665451824)) ;
#160262 = CARTESIAN_POINT('Ctrl Pts',(-12.9782123177536,-12.4057612857423,
117.164359360981)) ;
#160263 = CARTESIAN_POINT('Ctrl Pts',(-12.9870113646885,-12.4762290506085,
117.191159840251)) ;
#160264 = CARTESIAN_POINT('Ctrl Pts',(-13.0608152385725,-12.4762290124344,
117.166928891354)) ;
#160265 = CARTESIAN_POINT('Ctrl Pts',(-13.1346191124565,-12.4762289742604,
117.142697942457)) ;
#160266 = CARTESIAN_POINT('Ctrl Pts',(-13.1258200655216,-12.4057612093942,
117.115897463187)) ;
#160267 = CARTESIAN_POINT('Ctrl Pts',(-13.1170210185867,-12.3352934445281,
117.089096983917)) ;
#160268 = CARTESIAN_POINT('Ctrl Pts',(-13.0432171447027,-12.3352934827021,
117.113327932814)) ;
#160269 = CARTESIAN_POINT('Ctrl Pts',(-12.9694132708188,-12.3352935208762,
117.137558881711)) ;
#160270 = CARTESIAN_POINT('Ctrl Pts',(-12.9782123177536,-12.4057612857423,
117.164359360981)) ;
#160271 = CARTESIAN_POINT('Ctrl Pts',(-13.0770064791105,-12.3361751661113,
117.429775138385)) ;
#160272 = CARTESIAN_POINT('Ctrl Pts',(-13.0796556464204,-12.4116066467127,
117.43784407653)) ;
#160273 = CARTESIAN_POINT('Ctrl Pts',(-13.1534595213048,-12.4116066363173,
117.41361313068)) ;
#160274 = CARTESIAN_POINT('Ctrl Pts',(-13.2272633961891,-12.4116066259219,
117.38938218483)) ;
#160275 = CARTESIAN_POINT('Ctrl Pts',(-13.2246142288792,-12.3361751453206,
117.381313246685)) ;
#160276 = CARTESIAN_POINT('Ctrl Pts',(-13.2219650615692,-12.2607436647193,
117.37324430854)) ;
#160277 = CARTESIAN_POINT('Ctrl Pts',(-13.1481611866849,-12.2607436751146,
117.39747525439)) ;
#160278 = CARTESIAN_POINT('Ctrl Pts',(-13.0743573118005,-12.26074368551,117.42170620024)) ;
#160279 = CARTESIAN_POINT('Ctrl Pts',(-13.0770064791105,-12.3361751661113,
117.429775138385)) ;
#160280 = CARTESIAN_POINT('Ctrl Pts',(-13.1783190413846,-12.3442704255669,
117.702890794258)) ;
#160281 = CARTESIAN_POINT('Ctrl Pts',(-13.1746326472494,-12.4192498359007,
117.691662634393)) ;
#160282 = CARTESIAN_POINT('Ctrl Pts',(-13.2484365204859,-12.4192498519891,
117.667431683524)) ;
#160283 = CARTESIAN_POINT('Ctrl Pts',(-13.3222403937224,-12.4192498680774,
117.643200732654)) ;
#160284 = CARTESIAN_POINT('Ctrl Pts',(-13.3259267878576,-12.3442704577436,
117.654428892519)) ;
#160285 = CARTESIAN_POINT('Ctrl Pts',(-13.3296131819927,-12.2692910474097,
117.665657052383)) ;
#160286 = CARTESIAN_POINT('Ctrl Pts',(-13.2558093087563,-12.2692910313214,
117.689888003252)) ;
#160287 = CARTESIAN_POINT('Ctrl Pts',(-13.1820054355198,-12.269291015233,
117.714118954122)) ;
#160288 = CARTESIAN_POINT('Ctrl Pts',(-13.1783190413846,-12.3442704255669,
117.702890794258)) ;
#160289 = CARTESIAN_POINT('Ctrl Pts',(-13.2756527267231,-12.4291570429794,
117.963909021848)) ;
#160290 = CARTESIAN_POINT('Ctrl Pts',(-13.2658985708581,-12.4983225025168,
117.934199438683)) ;
#160291 = CARTESIAN_POINT('Ctrl Pts',(-13.3397024401949,-12.4983225412537,
117.909968475935)) ;
#160292 = CARTESIAN_POINT('Ctrl Pts',(-13.4135063095318,-12.4983225799905,
117.885737513188)) ;
#160293 = CARTESIAN_POINT('Ctrl Pts',(-13.4232604653967,-12.429157120453,
117.915447096353)) ;
#160294 = CARTESIAN_POINT('Ctrl Pts',(-13.4330146212616,-12.3599916609156,
117.945156679518)) ;
#160295 = CARTESIAN_POINT('Ctrl Pts',(-13.3592107519248,-12.3599916221787,
117.969387642266)) ;
#160296 = CARTESIAN_POINT('Ctrl Pts',(-13.285406882588,-12.3599915834419,
117.993618605013)) ;
#160297 = CARTESIAN_POINT('Ctrl Pts',(-13.2756527267231,-12.4291570429794,
117.963909021848)) ;
#160298 = CARTESIAN_POINT('Ctrl Pts',(-13.36292678935,-12.5849331529663,118.194259899517)) ;
#160299 = CARTESIAN_POINT('Ctrl Pts',(-13.3477985856065,-12.6433268351206,
118.148181833491)) ;
#160300 = CARTESIAN_POINT('Ctrl Pts',(-13.4216024492848,-12.6433268905322,
118.123950853509)) ;
#160301 = CARTESIAN_POINT('Ctrl Pts',(-13.495406312963,-12.6433269459438,
118.099719873526)) ;
#160302 = CARTESIAN_POINT('Ctrl Pts',(-13.5105345167065,-12.5849332637895,
118.145797939552)) ;
#160303 = CARTESIAN_POINT('Ctrl Pts',(-13.52566272045,-12.5265395816352,118.191876005578)) ;
#160304 = CARTESIAN_POINT('Ctrl Pts',(-13.4518588567717,-12.5265395262236,
118.21610698556)) ;
#160305 = CARTESIAN_POINT('Ctrl Pts',(-13.3780549930935,-12.526539470812,
118.240337965542)) ;
#160306 = CARTESIAN_POINT('Ctrl Pts',(-13.36292678935,-12.5849331529663,118.194259899517)) ;
#160307 = CARTESIAN_POINT('Ctrl Pts',(-13.4345794652228,-12.8005108515807,
118.377018028647)) ;
#160308 = CARTESIAN_POINT('Ctrl Pts',(-13.4151599387072,-12.8439413739947,
118.317869285721)) ;
#160309 = CARTESIAN_POINT('Ctrl Pts',(-13.4889637957772,-12.8439414387627,
118.293638285611)) ;
#160310 = CARTESIAN_POINT('Ctrl Pts',(-13.5627676528473,-12.8439415035308,
118.269407285501)) ;
#160311 = CARTESIAN_POINT('Ctrl Pts',(-13.5821871793629,-12.8005109811168,
118.328556028427)) ;
#160312 = CARTESIAN_POINT('Ctrl Pts',(-13.6016067058785,-12.7570804587029,
118.387704771354)) ;
#160313 = CARTESIAN_POINT('Ctrl Pts',(-13.5278028488085,-12.7570803939349,
118.411935771464)) ;
#160314 = CARTESIAN_POINT('Ctrl Pts',(-13.4539989917384,-12.7570803291668,
118.436166771574)) ;
#160315 = CARTESIAN_POINT('Ctrl Pts',(-13.4345794652228,-12.8005108515807,
118.377018028647)) ;
#160316 = CARTESIAN_POINT('Ctrl Pts',(-13.4861674949149,-13.060269126664,
118.498676029101)) ;
#160317 = CARTESIAN_POINT('Ctrl Pts',(-13.4638507023729,-13.0856291470037,
118.43070268118)) ;
#160318 = CARTESIAN_POINT('Ctrl Pts',(-13.537654552795,-13.0856292137402,
118.406471660822)) ;
#160319 = CARTESIAN_POINT('Ctrl Pts',(-13.6114584032172,-13.0856292804768,
118.382240640464)) ;
#160320 = CARTESIAN_POINT('Ctrl Pts',(-13.6337751957592,-13.0602692601371,
118.450213988385)) ;
#160321 = CARTESIAN_POINT('Ctrl Pts',(-13.6560919883012,-13.0349092397974,
118.518187336306)) ;
#160322 = CARTESIAN_POINT('Ctrl Pts',(-13.582288137879,-13.0349091730608,
118.542418356664)) ;
#160323 = CARTESIAN_POINT('Ctrl Pts',(-13.5084842874569,-13.0349091063243,
118.566649377022)) ;
#160324 = CARTESIAN_POINT('Ctrl Pts',(-13.4861674949149,-13.060269126664,
118.498676029101)) ;
#160325 = CARTESIAN_POINT('Ctrl Pts',(-13.5147933718825,-13.3453693583979,
118.550429429881)) ;
#160326 = CARTESIAN_POINT('Ctrl Pts',(-13.4911774012882,-13.3508620232142,
118.478498995081)) ;
#160327 = CARTESIAN_POINT('Ctrl Pts',(-13.5649812457546,-13.3508620856039,
118.454267956582)) ;
#160328 = CARTESIAN_POINT('Ctrl Pts',(-13.638785090221,-13.3508621479936,
118.430036918084)) ;
#160329 = CARTESIAN_POINT('Ctrl Pts',(-13.6624010608153,-13.3453694831773,
118.501967352883)) ;
#160330 = CARTESIAN_POINT('Ctrl Pts',(-13.6860170314095,-13.3398768183609,
118.573897787683)) ;
#160331 = CARTESIAN_POINT('Ctrl Pts',(-13.6122131869431,-13.3398767559712,
118.598128826182)) ;
#160332 = CARTESIAN_POINT('Ctrl Pts',(-13.5384093424767,-13.3398766935815,
118.62235986468)) ;
#160333 = CARTESIAN_POINT('Ctrl Pts',(-13.5147933718825,-13.3453693583979,
118.550429429881)) ;
#160334 = CARTESIAN_POINT('Ctrl Pts',(-13.5191703640909,-13.6361640667827,
118.528261672456)) ;
#160335 = CARTESIAN_POINT('Ctrl Pts',(-13.4959475223528,-13.6213614987656,
118.457528644549)) ;
#160336 = CARTESIAN_POINT('Ctrl Pts',(-13.5697513621746,-13.6213615511211,
118.433297591904)) ;
#160337 = CARTESIAN_POINT('Ctrl Pts',(-13.6435552019965,-13.6213616034766,
118.409066539259)) ;
#160338 = CARTESIAN_POINT('Ctrl Pts',(-13.6667780437346,-13.6361641714938,
118.479799567165)) ;
#160339 = CARTESIAN_POINT('Ctrl Pts',(-13.6900008854728,-13.6509667395109,
118.550532595072)) ;
#160340 = CARTESIAN_POINT('Ctrl Pts',(-13.6161970456509,-13.6509666871554,
118.574763647717)) ;
#160341 = CARTESIAN_POINT('Ctrl Pts',(-13.542393205829,-13.6509666347999,
118.598994700362)) ;
#160342 = CARTESIAN_POINT('Ctrl Pts',(-13.5191703640909,-13.6361640667827,
118.528261672456)) ;
#160343 = CARTESIAN_POINT('Ctrl Pts',(-13.4997846887976,-13.9104324089111,
118.433833737107)) ;
#160344 = CARTESIAN_POINT('Ctrl Pts',(-13.478612399891,-13.8764575771015,
118.369346362117)) ;
#160345 = CARTESIAN_POINT('Ctrl Pts',(-13.5524162366454,-13.8764576175232,
118.345115300128)) ;
#160346 = CARTESIAN_POINT('Ctrl Pts',(-13.6262200733997,-13.8764576579448,
118.32088423814)) ;
#160347 = CARTESIAN_POINT('Ctrl Pts',(-13.6473923623063,-13.9104324897545,
118.38537161313)) ;
#160348 = CARTESIAN_POINT('Ctrl Pts',(-13.6685646512129,-13.9444073215641,
118.44985898812)) ;
#160349 = CARTESIAN_POINT('Ctrl Pts',(-13.5947608144585,-13.9444072811424,
118.474090050108)) ;
#160350 = CARTESIAN_POINT('Ctrl Pts',(-13.5209569777042,-13.9444072407208,
118.498321112097)) ;
#160351 = CARTESIAN_POINT('Ctrl Pts',(-13.4997846887976,-13.9104324089111,
118.433833737107)) ;
#160352 = CARTESIAN_POINT('Ctrl Pts',(-13.4587413574297,-14.1501784561149,
118.27335686083)) ;
#160353 = CARTESIAN_POINT('Ctrl Pts',(-13.4411365754914,-14.0994124816197,
118.219735536282)) ;
#160354 = CARTESIAN_POINT('Ctrl Pts',(-13.5149404109386,-14.0994125084155,
118.195504470312)) ;
#160355 = CARTESIAN_POINT('Ctrl Pts',(-13.5887442463858,-14.0994125352114,
118.171273404342)) ;
#160356 = CARTESIAN_POINT('Ctrl Pts',(-13.6063490283242,-14.1501785097066,
118.22489472889)) ;
#160357 = CARTESIAN_POINT('Ctrl Pts',(-13.6239538102625,-14.2009444842018,
118.278516053439)) ;
#160358 = CARTESIAN_POINT('Ctrl Pts',(-13.5501499748153,-14.200944457406,
118.302747119408)) ;
#160359 = CARTESIAN_POINT('Ctrl Pts',(-13.4763461393681,-14.2009444306102,
118.326978185378)) ;
#160360 = CARTESIAN_POINT('Ctrl Pts',(-13.4587413574297,-14.1501784561149,
118.27335686083)) ;
#160361 = CARTESIAN_POINT('Ctrl Pts',(-13.39950930923,-14.3377944456025,118.057390334685)) ;
#160362 = CARTESIAN_POINT('Ctrl Pts',(-13.3867493283457,-14.273851283079,
118.018525492262)) ;
#160363 = CARTESIAN_POINT('Ctrl Pts',(-13.4605531643258,-14.2738512972119,
117.994294427915)) ;
#160364 = CARTESIAN_POINT('Ctrl Pts',(-13.5343570003059,-14.2738513113447,
117.970063363569)) ;
#160365 = CARTESIAN_POINT('Ctrl Pts',(-13.5471169811902,-14.3377944738682,
118.008928205992)) ;
#160366 = CARTESIAN_POINT('Ctrl Pts',(-13.5598769620745,-14.4017376363917,
118.047793048415)) ;
#160367 = CARTESIAN_POINT('Ctrl Pts',(-13.4860731260944,-14.4017376222589,
118.072024112762)) ;
#160368 = CARTESIAN_POINT('Ctrl Pts',(-13.4122692901143,-14.4017376081261,
118.096255177108)) ;
#160369 = CARTESIAN_POINT('Ctrl Pts',(-13.39950930923,-14.3377944456025,118.057390334685)) ;
#160370 = CARTESIAN_POINT('Ctrl Pts',(-13.32749153125,-14.4588735568458,117.802602901111)) ;
#160371 = CARTESIAN_POINT('Ctrl Pts',(-13.3204740636633,-14.3863794182977,
117.781228827494)) ;
#160372 = CARTESIAN_POINT('Ctrl Pts',(-13.3942779010377,-14.3863794234914,
117.756997767394)) ;
#160373 = CARTESIAN_POINT('Ctrl Pts',(-13.468081738412,-14.3863794286851,
117.732766707294)) ;
#160374 = CARTESIAN_POINT('Ctrl Pts',(-13.4750992059987,-14.4588735672332,
117.754140780912)) ;
#160375 = CARTESIAN_POINT('Ctrl Pts',(-13.4821166735854,-14.5313677057812,
117.775514854529)) ;
#160376 = CARTESIAN_POINT('Ctrl Pts',(-13.408312836211,-14.5313677005875,
117.799745914629)) ;
#160377 = CARTESIAN_POINT('Ctrl Pts',(-13.3345089988367,-14.5313676953939,
117.823976974729)) ;
#160378 = CARTESIAN_POINT('Ctrl Pts',(-13.32749153125,-14.4588735568458,117.802602901111)) ;
#160379 = CARTESIAN_POINT('Ctrl Pts',(-13.2483458924945,-14.5056122473976,
117.526071610546)) ;
#160380 = CARTESIAN_POINT('Ctrl Pts',(-13.2475781043464,-14.4297450127553,
117.523733051975)) ;
#160381 = CARTESIAN_POINT('Ctrl Pts',(-13.3213819437732,-14.4297450124761,
117.499501998127)) ;
#160382 = CARTESIAN_POINT('Ctrl Pts',(-13.3951857832,-14.4297450121969,117.475270944278)) ;
#160383 = CARTESIAN_POINT('Ctrl Pts',(-13.3959535713481,-14.5056122468393,
117.477609502849)) ;
#160384 = CARTESIAN_POINT('Ctrl Pts',(-13.3967213594963,-14.5814794814817,
117.479948061419)) ;
#160385 = CARTESIAN_POINT('Ctrl Pts',(-13.3229175200695,-14.5814794817608,
117.504179115268)) ;
#160386 = CARTESIAN_POINT('Ctrl Pts',(-13.2491136806427,-14.58147948204,117.528410169116)) ;
#160387 = CARTESIAN_POINT('Ctrl Pts',(-13.2483458924945,-14.5056122473976,
117.526071610546)) ;
#160388 = CARTESIAN_POINT('Ctrl Pts',(-13.1685437749415,-14.4743736272664,
117.247539732196)) ;
#160389 = CARTESIAN_POINT('Ctrl Pts',(-13.1740810712629,-14.4005733067483,
117.264405443477)) ;
#160390 = CARTESIAN_POINT('Ctrl Pts',(-13.2478849127416,-14.4005733047048,
117.240174395878)) ;
#160391 = CARTESIAN_POINT('Ctrl Pts',(-13.3216887542203,-14.4005733026613,
117.21594334828)) ;
#160392 = CARTESIAN_POINT('Ctrl Pts',(-13.3161514578989,-14.4743736231794,
117.199077636998)) ;
#160393 = CARTESIAN_POINT('Ctrl Pts',(-13.3106141615776,-14.5481739436975,
117.182211925717)) ;
#160394 = CARTESIAN_POINT('Ctrl Pts',(-13.2368103200988,-14.548173945741,
117.206442973316)) ;
#160395 = CARTESIAN_POINT('Ctrl Pts',(-13.1630064786201,-14.5481739477846,
117.230674020914)) ;
#160396 = CARTESIAN_POINT('Ctrl Pts',(-13.1685437749415,-14.4743736272664,
117.247539732196)) ;
#160397 = CARTESIAN_POINT('Ctrl Pts',(-13.0946020226361,-14.3676054099568,
116.986884001878)) ;
#160398 = CARTESIAN_POINT('Ctrl Pts',(-13.1060441801812,-14.3011495694392,
117.021734967606)) ;
#160399 = CARTESIAN_POINT('Ctrl Pts',(-13.1798480232085,-14.3011495683314,
116.997503924724)) ;
#160400 = CARTESIAN_POINT('Ctrl Pts',(-13.2536518662359,-14.3011495672236,
116.973272881842)) ;
#160401 = CARTESIAN_POINT('Ctrl Pts',(-13.2422097086908,-14.3676054077411,
116.938421916114)) ;
#160402 = CARTESIAN_POINT('Ctrl Pts',(-13.2307675511457,-14.4340612482587,
116.903570950386)) ;
#160403 = CARTESIAN_POINT('Ctrl Pts',(-13.1569637081184,-14.4340612493665,
116.927801993268)) ;
#160404 = CARTESIAN_POINT('Ctrl Pts',(-13.0831598650911,-14.4340612504743,
116.95203303615)) ;
#160405 = CARTESIAN_POINT('Ctrl Pts',(-13.0946020226361,-14.3676054099568,
116.986884001878)) ;
#160406 = CARTESIAN_POINT('Ctrl Pts',(-13.0324910029511,-14.1926642104704,
116.762231273457)) ;
#160407 = CARTESIAN_POINT('Ctrl Pts',(-13.0490214672177,-14.1383247775165,
116.812580400398)) ;
#160408 = CARTESIAN_POINT('Ctrl Pts',(-13.1228253110723,-14.1383247785838,
116.788349360036)) ;
#160409 = CARTESIAN_POINT('Ctrl Pts',(-13.1966291549269,-14.1383247796511,
116.764118319674)) ;
#160410 = CARTESIAN_POINT('Ctrl Pts',(-13.1800986906603,-14.192664212605,
116.713769192732)) ;
#160411 = CARTESIAN_POINT('Ctrl Pts',(-13.1635682263937,-14.2470036455589,
116.663420065791)) ;
#160412 = CARTESIAN_POINT('Ctrl Pts',(-13.0897643825391,-14.2470036444916,
116.687651106153)) ;
#160413 = CARTESIAN_POINT('Ctrl Pts',(-13.0159605386845,-14.2470036434243,
116.711882146515)) ;
#160414 = CARTESIAN_POINT('Ctrl Pts',(-13.0324910029511,-14.1926642104704,
116.762231273457)) ;
#160415 = CARTESIAN_POINT('Ctrl Pts',(-12.9874746142067,-13.9629645552833,
116.589736773677)) ;
#160416 = CARTESIAN_POINT('Ctrl Pts',(-13.0079052715445,-13.9245838600997,
116.651965259386)) ;
#160417 = CARTESIAN_POINT('Ctrl Pts',(-13.0817091155005,-13.9245838630912,
116.627734219333)) ;
#160418 = CARTESIAN_POINT('Ctrl Pts',(-13.1555129594564,-13.9245838660827,
116.603503179279)) ;
#160419 = CARTESIAN_POINT('Ctrl Pts',(-13.1350823021187,-13.9629645612662,
116.54127469357)) ;
#160420 = CARTESIAN_POINT('Ctrl Pts',(-13.1146516447809,-14.0013452564497,
116.47904620786)) ;
#160421 = CARTESIAN_POINT('Ctrl Pts',(-13.040847800825,-14.0013452534583,
116.503277247914)) ;
#160422 = CARTESIAN_POINT('Ctrl Pts',(-12.967043956869,-14.0013452504668,
116.527508287967)) ;
#160423 = CARTESIAN_POINT('Ctrl Pts',(-12.9874746142067,-13.9629645552833,
116.589736773677)) ;
#160424 = CARTESIAN_POINT('Ctrl Pts',(-12.9633562559811,-13.6916669453695,
116.48056065792)) ;
#160425 = CARTESIAN_POINT('Ctrl Pts',(-12.9862407299605,-13.6721744570857,
116.55026307322)) ;
#160426 = CARTESIAN_POINT('Ctrl Pts',(-13.0600445735023,-13.6721744593942,
116.526032031905)) ;
#160427 = CARTESIAN_POINT('Ctrl Pts',(-13.1338484170441,-13.6721744617026,
116.50180099059)) ;
#160428 = CARTESIAN_POINT('Ctrl Pts',(-13.1109639430647,-13.6916669499864,
116.43209857529)) ;
#160429 = CARTESIAN_POINT('Ctrl Pts',(-13.0880794690853,-13.7111594382702,
116.36239615999)) ;
#160430 = CARTESIAN_POINT('Ctrl Pts',(-13.0142756255436,-13.7111594359618,
116.386627201305)) ;
#160431 = CARTESIAN_POINT('Ctrl Pts',(-12.9404717820018,-13.7111594336534,
116.41085824262)) ;
#160432 = CARTESIAN_POINT('Ctrl Pts',(-12.9633562559811,-13.6916669453695,
116.48056065792)) ;
#160433 = CARTESIAN_POINT('Ctrl Pts',(-12.9629691653421,-13.4042886281479,
116.444129256868)) ;
#160434 = CARTESIAN_POINT('Ctrl Pts',(-12.9866435826147,-13.4048339669214,
116.516237712028)) ;
#160435 = CARTESIAN_POINT('Ctrl Pts',(-13.0604474259364,-13.4048339668837,
116.492006670043)) ;
#160436 = CARTESIAN_POINT('Ctrl Pts',(-13.1342512692581,-13.404833966846,
116.467775628057)) ;
#160437 = CARTESIAN_POINT('Ctrl Pts',(-13.1105768519855,-13.4042886280725,
116.395667172897)) ;
#160438 = CARTESIAN_POINT('Ctrl Pts',(-13.0869024347129,-13.403743289299,
116.323558717737)) ;
#160439 = CARTESIAN_POINT('Ctrl Pts',(-13.0130985913912,-13.4037432893367,
116.347789759722)) ;
#160440 = CARTESIAN_POINT('Ctrl Pts',(-12.9392947480694,-13.4037432893744,
116.372020801708)) ;
#160441 = CARTESIAN_POINT('Ctrl Pts',(-12.9629691653421,-13.4042886281479,
116.444129256868)) ;
#160442 = CARTESIAN_POINT('Ctrl Pts',(-12.9867239596031,-13.1160881842174,
116.481000353099)) ;
#160443 = CARTESIAN_POINT('Ctrl Pts',(-13.0095086248234,-13.1367582104912,
116.550398767152)) ;
#160444 = CARTESIAN_POINT('Ctrl Pts',(-13.08331246846,-13.1367582061789,116.526167726126)) ;
#160445 = CARTESIAN_POINT('Ctrl Pts',(-13.1571163120967,-13.1367582018666,
116.5019366851)) ;
#160446 = CARTESIAN_POINT('Ctrl Pts',(-13.1343316468764,-13.1160881755929,
116.432538271047)) ;
#160447 = CARTESIAN_POINT('Ctrl Pts',(-13.1115469816561,-13.0954181493191,
116.363139856994)) ;
#160448 = CARTESIAN_POINT('Ctrl Pts',(-13.0377431380194,-13.0954181536314,
116.38737089802)) ;
#160449 = CARTESIAN_POINT('Ctrl Pts',(-12.9639392943828,-13.0954181579436,
116.411601939046)) ;
#160450 = CARTESIAN_POINT('Ctrl Pts',(-12.9867239596031,-13.1160881842174,
116.481000353099)) ;
#160451 = CARTESIAN_POINT('Ctrl Pts',(-13.0339690435015,-12.8495738757798,
116.589413701142)) ;
#160452 = CARTESIAN_POINT('Ctrl Pts',(-13.0542224194139,-12.8888833461409,
116.651102216502)) ;
#160453 = CARTESIAN_POINT('Ctrl Pts',(-13.1280262643834,-12.8888833370438,
116.626871179536)) ;
#160454 = CARTESIAN_POINT('Ctrl Pts',(-13.2018301093529,-12.8888833279467,
116.602640142569)) ;
#160455 = CARTESIAN_POINT('Ctrl Pts',(-13.1815767334405,-12.8495738575856,
116.540951627209)) ;
#160456 = CARTESIAN_POINT('Ctrl Pts',(-13.1613233575281,-12.8102643872246,
116.479263111849)) ;
#160457 = CARTESIAN_POINT('Ctrl Pts',(-13.0875195125586,-12.8102643963217,
116.503494148816)) ;
#160458 = CARTESIAN_POINT('Ctrl Pts',(-13.0137156675891,-12.8102644054188,
116.527725185782)) ;
#160459 = CARTESIAN_POINT('Ctrl Pts',(-13.0339690435015,-12.8495738757798,
116.589413701142)) ;
#160460 = CARTESIAN_POINT('Ctrl Pts',(-13.1016362988514,-12.6242652876755,
116.76014561289)) ;
#160461 = CARTESIAN_POINT('Ctrl Pts',(-13.1179262753709,-12.6793633695142,
116.809762253308)) ;
#160462 = CARTESIAN_POINT('Ctrl Pts',(-13.1917301223629,-12.6793633576824,
116.785531222502)) ;
#160463 = CARTESIAN_POINT('Ctrl Pts',(-13.2655339693549,-12.6793633458506,
116.761300191696)) ;
#160464 = CARTESIAN_POINT('Ctrl Pts',(-13.2492439928354,-12.6242652640119,
116.711683551278)) ;
#160465 = CARTESIAN_POINT('Ctrl Pts',(-13.2329540163159,-12.5691671821732,
116.66206691086)) ;
#160466 = CARTESIAN_POINT('Ctrl Pts',(-13.1591501693239,-12.569167194005,
116.686297941666)) ;
#160467 = CARTESIAN_POINT('Ctrl Pts',(-13.0853463223319,-12.5691672058369,
116.710528972472)) ;
#160468 = CARTESIAN_POINT('Ctrl Pts',(-13.1016362988514,-12.6242652876755,
116.76014561289)) ;
#160469 = CARTESIAN_POINT('Ctrl Pts',(-13.1868381515301,-12.4543477917217,
116.98391806025)) ;
#160470 = CARTESIAN_POINT('Ctrl Pts',(-13.1979423963532,-12.5213905408383,
117.017739798833)) ;
#160471 = CARTESIAN_POINT('Ctrl Pts',(-13.2717462470113,-12.5213905278412,
116.993508779193)) ;
#160472 = CARTESIAN_POINT('Ctrl Pts',(-13.3455500976693,-12.521390514844,
116.969277759554)) ;
#160473 = CARTESIAN_POINT('Ctrl Pts',(-13.3344458528461,-12.4543477657274,
116.93545602097)) ;
#160474 = CARTESIAN_POINT('Ctrl Pts',(-13.323341608023,-12.3873050166108,
116.901634282387)) ;
#160475 = CARTESIAN_POINT('Ctrl Pts',(-13.2495377573649,-12.387305029608,
116.925865302027)) ;
#160476 = CARTESIAN_POINT('Ctrl Pts',(-13.1757339067069,-12.3873050426051,
116.950096321667)) ;
#160477 = CARTESIAN_POINT('Ctrl Pts',(-13.1868381515301,-12.4543477917217,
116.98391806025)) ;
#160478 = CARTESIAN_POINT('Ctrl Pts',(-13.282130994495,-12.3553371823295,
117.238917231087)) ;
#160479 = CARTESIAN_POINT('Ctrl Pts',(-13.2873271899244,-12.4293892510952,
117.254744004599)) ;
#160480 = CARTESIAN_POINT('Ctrl Pts',(-13.3611310433399,-12.4293892433542,
117.230512993358)) ;
#160481 = CARTESIAN_POINT('Ctrl Pts',(-13.4349348967555,-12.4293892356132,
117.206281982117)) ;
#160482 = CARTESIAN_POINT('Ctrl Pts',(-13.4297387013261,-12.3553371668475,
117.190455208605)) ;
#160483 = CARTESIAN_POINT('Ctrl Pts',(-13.4245425058967,-12.2812850980819,
117.174628435093)) ;
#160484 = CARTESIAN_POINT('Ctrl Pts',(-13.3507386524812,-12.2812851058229,
117.198859446334)) ;
#160485 = CARTESIAN_POINT('Ctrl Pts',(-13.2769347990657,-12.2812851135639,
117.223090457575)) ;
#160486 = CARTESIAN_POINT('Ctrl Pts',(-13.282130994495,-12.3553371823295,
117.238917231087)) ;
#160487 = CARTESIAN_POINT('Ctrl Pts',(-13.3835527278556,-12.3315537600446,
117.512226746283)) ;
#160488 = CARTESIAN_POINT('Ctrl Pts',(-13.3824119200247,-12.4073738615737,
117.508752030529)) ;
#160489 = CARTESIAN_POINT('Ctrl Pts',(-13.456215776812,-12.4073738630853,
117.484521029558)) ;
#160490 = CARTESIAN_POINT('Ctrl Pts',(-13.5300196335994,-12.4073738645969,
117.460290028587)) ;
#160491 = CARTESIAN_POINT('Ctrl Pts',(-13.5311604414304,-12.3315537630678,
117.463764744342)) ;
#160492 = CARTESIAN_POINT('Ctrl Pts',(-13.5323012492613,-12.2557336615386,
117.467239460096)) ;
#160493 = CARTESIAN_POINT('Ctrl Pts',(-13.4584973924739,-12.255733660027,
117.491470461067)) ;
#160494 = CARTESIAN_POINT('Ctrl Pts',(-13.3846935356866,-12.2557336585155,
117.515701462038)) ;
#160495 = CARTESIAN_POINT('Ctrl Pts',(-13.3835527278556,-12.3315537600446,
117.512226746283)) ;
#160496 = CARTESIAN_POINT('Ctrl Pts',(-13.4828912406925,-12.3856473127391,
117.779479511165)) ;
#160497 = CARTESIAN_POINT('Ctrl Pts',(-13.4755438357451,-12.4577997306566,
117.757100502165)) ;
#160498 = CARTESIAN_POINT('Ctrl Pts',(-13.549347694077,-12.4577997458788,
117.732869505898)) ;
#160499 = CARTESIAN_POINT('Ctrl Pts',(-13.6231515524089,-12.457799761101,
117.708638509632)) ;
#160500 = CARTESIAN_POINT('Ctrl Pts',(-13.6304989573563,-12.3856473431835,
117.731017518632)) ;
#160501 = CARTESIAN_POINT('Ctrl Pts',(-13.6378463623037,-12.3134949252661,
117.753396527632)) ;
#160502 = CARTESIAN_POINT('Ctrl Pts',(-13.5640425039718,-12.3134949100439,
117.777627523899)) ;
#160503 = CARTESIAN_POINT('Ctrl Pts',(-13.4902386456399,-12.3134948948217,
117.801858520165)) ;
#160504 = CARTESIAN_POINT('Ctrl Pts',(-13.4828912406925,-12.3856473127391,
117.779479511165)) ;
#160505 = CARTESIAN_POINT('Ctrl Pts',(-13.5751280064643,-12.513656004823,
118.024906933845)) ;
#160506 = CARTESIAN_POINT('Ctrl Pts',(-13.5620649402894,-12.5769754722421,
117.98511894314)) ;
#160507 = CARTESIAN_POINT('Ctrl Pts',(-13.6358687992258,-12.5769755044901,
117.960887948714)) ;
#160508 = CARTESIAN_POINT('Ctrl Pts',(-13.7096726581622,-12.576975536738,
117.936656954289)) ;
#160509 = CARTESIAN_POINT('Ctrl Pts',(-13.7227357243371,-12.5136560693188,
117.976444944994)) ;
#160510 = CARTESIAN_POINT('Ctrl Pts',(-13.7357987905121,-12.4503366018996,
118.016232935699)) ;
#160511 = CARTESIAN_POINT('Ctrl Pts',(-13.6619949315757,-12.4503365696517,
118.040463930124)) ;
#160512 = CARTESIAN_POINT('Ctrl Pts',(-13.5881910726393,-12.4503365374038,
118.06469492455)) ;
#160513 = CARTESIAN_POINT('Ctrl Pts',(-13.5751280064643,-12.513656004823,
118.024906933845)) ;
#160514 = CARTESIAN_POINT('Ctrl Pts',(-13.6539134068514,-12.707439556573,
118.229281918463)) ;
#160515 = CARTESIAN_POINT('Ctrl Pts',(-13.6360672125102,-12.7573213774984,
118.174925291302)) ;
#160516 = CARTESIAN_POINT('Ctrl Pts',(-13.7098710700878,-12.7573214291752,
118.150694292738)) ;
#160517 = CARTESIAN_POINT('Ctrl Pts',(-13.7836749276654,-12.7573214808521,
118.126463294174)) ;
#160518 = CARTESIAN_POINT('Ctrl Pts',(-13.8015211220067,-12.7074396599266,
118.180819921335)) ;
#160519 = CARTESIAN_POINT('Ctrl Pts',(-13.8193673163479,-12.6575578390012,
118.235176548496)) ;
#160520 = CARTESIAN_POINT('Ctrl Pts',(-13.7455634587703,-12.6575577873243,
118.25940754706)) ;
#160521 = CARTESIAN_POINT('Ctrl Pts',(-13.6717596011927,-12.6575577356475,
118.283638545624)) ;
#160522 = CARTESIAN_POINT('Ctrl Pts',(-13.6539134068514,-12.707439556573,
118.229281918463)) ;
#160523 = CARTESIAN_POINT('Ctrl Pts',(-13.7137234776106,-12.9500051005904,
118.376179984501)) ;
#160524 = CARTESIAN_POINT('Ctrl Pts',(-13.6924056592633,-12.9830234168188,
118.31124935088)) ;
#160525 = CARTESIAN_POINT('Ctrl Pts',(-13.7662095128799,-12.9830234842415,
118.287018340252)) ;
#160526 = CARTESIAN_POINT('Ctrl Pts',(-13.8400133664964,-12.9830235516642,
118.262787329623)) ;
#160527 = CARTESIAN_POINT('Ctrl Pts',(-13.8613311848437,-12.9500052354358,
118.327717963243)) ;
#160528 = CARTESIAN_POINT('Ctrl Pts',(-13.8826490031911,-12.9169869192073,
118.392648596863)) ;
#160529 = CARTESIAN_POINT('Ctrl Pts',(-13.8088451495745,-12.9169868517846,
118.416879607492)) ;
#160530 = CARTESIAN_POINT('Ctrl Pts',(-13.735041295958,-12.9169867843619,
118.441110618121)) ;
#160531 = CARTESIAN_POINT('Ctrl Pts',(-13.7137234776106,-12.9500051005904,
118.376179984501)) ;
#160532 = CARTESIAN_POINT('Ctrl Pts',(-13.7520689708624,-13.2274462581565,
118.457479335507)) ;
#160533 = CARTESIAN_POINT('Ctrl Pts',(-13.7287774968662,-13.2411424706592,
118.386537265376)) ;
#160534 = CARTESIAN_POINT('Ctrl Pts',(-13.8025813449987,-13.2411425518727,
118.362306238044)) ;
#160535 = CARTESIAN_POINT('Ctrl Pts',(-13.8763851931311,-13.2411426330862,
118.338075210711)) ;
#160536 = CARTESIAN_POINT('Ctrl Pts',(-13.8996766671273,-13.2274464205834,
118.409017280842)) ;
#160537 = CARTESIAN_POINT('Ctrl Pts',(-13.9229681411235,-13.2137502080807,
118.479959350972)) ;
#160538 = CARTESIAN_POINT('Ctrl Pts',(-13.8491642929911,-13.2137501268672,
118.504190378305)) ;
#160539 = CARTESIAN_POINT('Ctrl Pts',(-13.7753604448586,-13.2137500456537,
118.528421405637)) ;
#160540 = CARTESIAN_POINT('Ctrl Pts',(-13.7520689708624,-13.2274462581565,
118.457479335507)) ;
#160541 = CARTESIAN_POINT('Ctrl Pts',(-13.7663393260749,-13.5192262317475,
118.465377287378)) ;
#160542 = CARTESIAN_POINT('Ctrl Pts',(-13.7427535201405,-13.5125713400262,
118.393538729794)) ;
#160543 = CARTESIAN_POINT('Ctrl Pts',(-13.8165573610894,-13.5125714295465,
118.369307680582)) ;
#160544 = CARTESIAN_POINT('Ctrl Pts',(-13.8903612020383,-13.5125715190667,
118.34507663137)) ;
#160545 = CARTESIAN_POINT('Ctrl Pts',(-13.9139470079727,-13.519226410788,
118.416915188953)) ;
#160546 = CARTESIAN_POINT('Ctrl Pts',(-13.9375328139072,-13.5258813025093,
118.488753746537)) ;
#160547 = CARTESIAN_POINT('Ctrl Pts',(-13.8637289729583,-13.525881212989,
118.512984795749)) ;
#160548 = CARTESIAN_POINT('Ctrl Pts',(-13.7899251320094,-13.5258811234688,
118.537215844962)) ;
#160549 = CARTESIAN_POINT('Ctrl Pts',(-13.7663393260749,-13.5192262317475,
118.465377287378)) ;
#160550 = CARTESIAN_POINT('Ctrl Pts',(-13.7564573176797,-13.8018769048648,
118.399949096535)) ;
#160551 = CARTESIAN_POINT('Ctrl Pts',(-13.7342582218036,-13.7754786172954,
118.332334234138)) ;
#160552 = CARTESIAN_POINT('Ctrl Pts',(-13.8080620549042,-13.7754787060709,
118.308103161021)) ;
#160553 = CARTESIAN_POINT('Ctrl Pts',(-13.8818658880047,-13.7754787948464,
118.283872087904)) ;
#160554 = CARTESIAN_POINT('Ctrl Pts',(-13.9040649838808,-13.8018770824157,
118.351486950301)) ;
#160555 = CARTESIAN_POINT('Ctrl Pts',(-13.9262640797569,-13.8282753699851,
118.419101812698)) ;
#160556 = CARTESIAN_POINT('Ctrl Pts',(-13.8524602466564,-13.8282752812096,
118.443332885815)) ;
#160557 = CARTESIAN_POINT('Ctrl Pts',(-13.7786564135558,-13.8282751924341,
118.467563958932)) ;
#160558 = CARTESIAN_POINT('Ctrl Pts',(-13.7564573176797,-13.8018769048648,
118.399949096535)) ;
#160559 = CARTESIAN_POINT('Ctrl Pts',(-13.7237468055255,-14.058784271986,
118.264759363062)) ;
#160560 = CARTESIAN_POINT('Ctrl Pts',(-13.7045346643817,-14.0144111213973,
118.20624228294)) ;
#160561 = CARTESIAN_POINT('Ctrl Pts',(-13.7783384894998,-14.0144112025132,
118.18201118551)) ;
#160562 = CARTESIAN_POINT('Ctrl Pts',(-13.8521423146179,-14.014411283629,
118.157780088079)) ;
#160563 = CARTESIAN_POINT('Ctrl Pts',(-13.8713544557617,-14.0587844342176,
118.216297168201)) ;
#160564 = CARTESIAN_POINT('Ctrl Pts',(-13.8905665969056,-14.1031575848063,
118.274814248324)) ;
#160565 = CARTESIAN_POINT('Ctrl Pts',(-13.8167627717875,-14.1031575036904,
118.299045345754)) ;
#160566 = CARTESIAN_POINT('Ctrl Pts',(-13.7429589466694,-14.1031574225746,
118.323276443184)) ;
#160567 = CARTESIAN_POINT('Ctrl Pts',(-13.7237468055255,-14.058784271986,
118.264759363062)) ;
#160568 = CARTESIAN_POINT('Ctrl Pts',(-13.6714025576082,-14.2690401451517,
118.069862285334)) ;
#160569 = CARTESIAN_POINT('Ctrl Pts',(-13.6565505498238,-14.2099227100526,
118.024625467992)) ;
#160570 = CARTESIAN_POINT('Ctrl Pts',(-13.7303543679443,-14.2099227749143,
118.000394349248)) ;
#160571 = CARTESIAN_POINT('Ctrl Pts',(-13.8041581860649,-14.209922839776,
117.976163230505)) ;
#160572 = CARTESIAN_POINT('Ctrl Pts',(-13.8190101938493,-14.2690402748751,
118.021400047847)) ;
#160573 = CARTESIAN_POINT('Ctrl Pts',(-13.8338622016338,-14.3281577099741,
118.066636865189)) ;
#160574 = CARTESIAN_POINT('Ctrl Pts',(-13.7600583835132,-14.3281576451124,
118.090867983933)) ;
#160575 = CARTESIAN_POINT('Ctrl Pts',(-13.6862545653926,-14.3281575802507,
118.115099102677)) ;
#160576 = CARTESIAN_POINT('Ctrl Pts',(-13.6714025576082,-14.2690401451517,
118.069862285334)) ;
#160577 = CARTESIAN_POINT('Ctrl Pts',(-13.6038901489006,-14.418345814643,
117.828744781992)) ;
#160578 = CARTESIAN_POINT('Ctrl Pts',(-13.5944639944471,-14.3487174926443,
117.80003423849)) ;
#160579 = CARTESIAN_POINT('Ctrl Pts',(-13.6682678073288,-14.3487175346435,
117.77580310379)) ;
#160580 = CARTESIAN_POINT('Ctrl Pts',(-13.7420716202107,-14.3487175766427,
117.751571969089)) ;
#160581 = CARTESIAN_POINT('Ctrl Pts',(-13.7514977746642,-14.4183458986414,
117.780282512592)) ;
#160582 = CARTESIAN_POINT('Ctrl Pts',(-13.7609239291177,-14.48797422064,117.808993056095)) ;
#160583 = CARTESIAN_POINT('Ctrl Pts',(-13.6871201162359,-14.4879741786408,
117.833224190795)) ;
#160584 = CARTESIAN_POINT('Ctrl Pts',(-13.6133163033541,-14.4879741366417,
117.857455325495)) ;
#160585 = CARTESIAN_POINT('Ctrl Pts',(-13.6038901489006,-14.418345814643,
117.828744781992)) ;
#160586 = CARTESIAN_POINT('Ctrl Pts',(-13.5270066699605,-14.4960013207205,
117.559173432525)) ;
#160587 = CARTESIAN_POINT('Ctrl Pts',(-13.5236667615923,-14.4208489309484,
117.549000612615)) ;
#160588 = CARTESIAN_POINT('Ctrl Pts',(-13.5974705716151,-14.4208489456351,
117.524769469207)) ;
#160589 = CARTESIAN_POINT('Ctrl Pts',(-13.6712743816379,-14.4208489603219,
117.500538325799)) ;
#160590 = CARTESIAN_POINT('Ctrl Pts',(-13.6746142900061,-14.496001350094,
117.510711145709)) ;
#160591 = CARTESIAN_POINT('Ctrl Pts',(-13.6779541983743,-14.5711537398661,
117.520883965618)) ;
#160592 = CARTESIAN_POINT('Ctrl Pts',(-13.6041503883515,-14.5711537251794,
117.545115109027)) ;
#160593 = CARTESIAN_POINT('Ctrl Pts',(-13.5303465783287,-14.5711537104926,
117.569346252435)) ;
#160594 = CARTESIAN_POINT('Ctrl Pts',(-13.5270066699605,-14.4960013207205,
117.559173432525)) ;
#160595 = CARTESIAN_POINT('Ctrl Pts',(-13.4463172125483,-14.4962457299704,
117.277772265082)) ;
#160596 = CARTESIAN_POINT('Ctrl Pts',(-13.4493430518799,-14.4209645456079,
117.286988485564)) ;
#160597 = CARTESIAN_POINT('Ctrl Pts',(-13.5231468617819,-14.4209645311187,
117.262757341788)) ;
#160598 = CARTESIAN_POINT('Ctrl Pts',(-13.5969506716839,-14.4209645166296,
117.238526198012)) ;
#160599 = CARTESIAN_POINT('Ctrl Pts',(-13.5939248323523,-14.4962457009921,
117.22930997753)) ;
#160600 = CARTESIAN_POINT('Ctrl Pts',(-13.5908989930207,-14.5715268853546,
117.220093757049)) ;
#160601 = CARTESIAN_POINT('Ctrl Pts',(-13.5170951831187,-14.5715268998438,
117.244324900825)) ;
#160602 = CARTESIAN_POINT('Ctrl Pts',(-13.4432913732167,-14.5715269143329,
117.268556044601)) ;
#160603 = CARTESIAN_POINT('Ctrl Pts',(-13.4463172125483,-14.4962457299704,
117.277772265082)) ;
#160604 = CARTESIAN_POINT('Ctrl Pts',(-13.3696988473351,-14.4198799151553,
117.009166760654)) ;
#160605 = CARTESIAN_POINT('Ctrl Pts',(-13.3788075758718,-14.3498193552219,
117.036910480173)) ;
#160606 = CARTESIAN_POINT('Ctrl Pts',(-13.4526113883286,-14.3498193130492,
117.012679344178)) ;
#160607 = CARTESIAN_POINT('Ctrl Pts',(-13.5264152007854,-14.3498192708765,
116.988448208184)) ;
#160608 = CARTESIAN_POINT('Ctrl Pts',(-13.5173064722488,-14.4198798308098,
116.960704488665)) ;
#160609 = CARTESIAN_POINT('Ctrl Pts',(-13.5081977437121,-14.4899403907432,
116.932960769146)) ;
#160610 = CARTESIAN_POINT('Ctrl Pts',(-13.4343939312553,-14.4899404329159,
116.957191905141)) ;
#160611 = CARTESIAN_POINT('Ctrl Pts',(-13.3605901187985,-14.4899404750886,
116.981423041135)) ;
#160612 = CARTESIAN_POINT('Ctrl Pts',(-13.3696988473351,-14.4198799151553,
117.009166760654)) ;
#160613 = CARTESIAN_POINT('Ctrl Pts',(-13.3017866089322,-14.2709014086462,
116.76670550127)) ;
#160614 = CARTESIAN_POINT('Ctrl Pts',(-13.3163871564839,-14.2111372247694,
116.811176415367)) ;
#160615 = CARTESIAN_POINT('Ctrl Pts',(-13.390190974086,-14.2111371588843,
116.786945295044)) ;
#160616 = CARTESIAN_POINT('Ctrl Pts',(-13.4639947916881,-14.2111370929992,
116.762714174722)) ;
#160617 = CARTESIAN_POINT('Ctrl Pts',(-13.4493942441364,-14.270901276876,
116.718243260625)) ;
#160618 = CARTESIAN_POINT('Ctrl Pts',(-13.4347936965847,-14.3306654607528,
116.673772346528)) ;
#160619 = CARTESIAN_POINT('Ctrl Pts',(-13.3609898789826,-14.3306655266379,
116.698003466851)) ;
#160620 = CARTESIAN_POINT('Ctrl Pts',(-13.2871860613805,-14.330665592523,
116.722234587174)) ;
#160621 = CARTESIAN_POINT('Ctrl Pts',(-13.3017866089322,-14.2709014086462,
116.76670550127)) ;
#160622 = CARTESIAN_POINT('Ctrl Pts',(-13.2493889815294,-14.0614284920593,
116.571702252918)) ;
#160623 = CARTESIAN_POINT('Ctrl Pts',(-13.2684022387902,-14.016200017183,
116.629613568744)) ;
#160624 = CARTESIAN_POINT('Ctrl Pts',(-13.342206063304,-14.01619993407,116.605382469473)) ;
#160625 = CARTESIAN_POINT('Ctrl Pts',(-13.4160098878178,-14.016199850957,
116.581151370202)) ;
#160626 = CARTESIAN_POINT('Ctrl Pts',(-13.396996630557,-14.0614283258333,
116.523240054376)) ;
#160627 = CARTESIAN_POINT('Ctrl Pts',(-13.3779833732962,-14.1066568007097,
116.46532873855)) ;
#160628 = CARTESIAN_POINT('Ctrl Pts',(-13.3041795487824,-14.1066568838226,
116.48955983782)) ;
#160629 = CARTESIAN_POINT('Ctrl Pts',(-13.2303757242686,-14.1066569669356,
116.513790937091)) ;
#160630 = CARTESIAN_POINT('Ctrl Pts',(-13.2493889815294,-14.0614284920593,
116.571702252918)) ;
#160631 = CARTESIAN_POINT('Ctrl Pts',(-13.2164243628667,-13.8059370930909,
116.435853274894)) ;
#160632 = CARTESIAN_POINT('Ctrl Pts',(-13.23850096586,-13.778478597832,116.503095047478)) ;
#160633 = CARTESIAN_POINT('Ctrl Pts',(-13.3123047984058,-13.7784785051367,
116.478863972672)) ;
#160634 = CARTESIAN_POINT('Ctrl Pts',(-13.3861086309516,-13.7784784124414,
116.454632897865)) ;
#160635 = CARTESIAN_POINT('Ctrl Pts',(-13.3640320279583,-13.8059369077003,
116.38739112528)) ;
#160636 = CARTESIAN_POINT('Ctrl Pts',(-13.3419554249649,-13.8333954029592,
116.320149352695)) ;
#160637 = CARTESIAN_POINT('Ctrl Pts',(-13.2681515924191,-13.8333954956545,
116.344380427502)) ;
#160638 = CARTESIAN_POINT('Ctrl Pts',(-13.1943477598733,-13.8333955883498,
116.368611502309)) ;
#160639 = CARTESIAN_POINT('Ctrl Pts',(-13.2164243628667,-13.8059370930909,
116.435853274894)) ;
#160640 = CARTESIAN_POINT('Ctrl Pts',(-13.2062477246467,-13.5211628984478,
116.369237660814)) ;
#160641 = CARTESIAN_POINT('Ctrl Pts',(-13.2298051727491,-13.5135452087457,
116.44098984855)) ;
#160642 = CARTESIAN_POINT('Ctrl Pts',(-13.3036090135613,-13.5135451161284,
116.416758798922)) ;
#160643 = CARTESIAN_POINT('Ctrl Pts',(-13.3774128543735,-13.513545023511,
116.392527749293)) ;
#160644 = CARTESIAN_POINT('Ctrl Pts',(-13.3538554062711,-13.5211627132132,
116.320775561557)) ;
#160645 = CARTESIAN_POINT('Ctrl Pts',(-13.3302979581687,-13.5287804029153,
116.24902337382)) ;
#160646 = CARTESIAN_POINT('Ctrl Pts',(-13.2564941173566,-13.5287804955326,
116.273254423449)) ;
#160647 = CARTESIAN_POINT('Ctrl Pts',(-13.1826902765444,-13.52878058815,116.297485473077)) ;
#160648 = CARTESIAN_POINT('Ctrl Pts',(-13.2062477246467,-13.5211628984478,
116.369237660814)) ;
#160649 = CARTESIAN_POINT('Ctrl Pts',(-13.2201829843462,-13.2317212421624,
116.376408413708)) ;
#160650 = CARTESIAN_POINT('Ctrl Pts',(-13.2435326740826,-13.244300576159,
116.447527802893)) ;
#160651 = CARTESIAN_POINT('Ctrl Pts',(-13.3173365223856,-13.2443004892996,
116.42329677608)) ;
#160652 = CARTESIAN_POINT('Ctrl Pts',(-13.3911403706885,-13.2443004024403,
116.399065749266)) ;
#160653 = CARTESIAN_POINT('Ctrl Pts',(-13.367790680952,-13.2317210684437,
116.327946360081)) ;
#160654 = CARTESIAN_POINT('Ctrl Pts',(-13.3444409912156,-13.2191417344471,
116.256826970896)) ;
#160655 = CARTESIAN_POINT('Ctrl Pts',(-13.2706371429126,-13.2191418213064,
116.281057997709)) ;
#160656 = CARTESIAN_POINT('Ctrl Pts',(-13.1968332946097,-13.2191419081658,
116.305289024523)) ;
#160657 = CARTESIAN_POINT('Ctrl Pts',(-13.2201829843462,-13.2317212421624,
116.376408413708)) ;
#160658 = CARTESIAN_POINT('Ctrl Pts',(-13.2582351273943,-12.953209842425,
116.456720631326)) ;
#160659 = CARTESIAN_POINT('Ctrl Pts',(-13.2796998255669,-12.9852534588735,
116.522098640202)) ;
#160660 = CARTESIAN_POINT('Ctrl Pts',(-13.3535036799056,-12.9852533862488,
116.497867631773)) ;
#160661 = CARTESIAN_POINT('Ctrl Pts',(-13.4273075342443,-12.9852533136241,
116.473636623344)) ;
#160662 = CARTESIAN_POINT('Ctrl Pts',(-13.4058428360717,-12.9532096971755,
116.408258614468)) ;
#160663 = CARTESIAN_POINT('Ctrl Pts',(-13.384378137899,-12.921166080727,116.342880605593)) ;
#160664 = CARTESIAN_POINT('Ctrl Pts',(-13.3105742835603,-12.9211661533517,
116.367111614022)) ;
#160665 = CARTESIAN_POINT('Ctrl Pts',(-13.2367704292216,-12.9211662259765,
116.391342622451)) ;
#160666 = CARTESIAN_POINT('Ctrl Pts',(-13.2582351273943,-12.953209842425,
116.456720631326)) ;
#160667 = CARTESIAN_POINT('Ctrl Pts',(-13.3179987777289,-12.7094642616823,
116.60338316649)) ;
#160668 = CARTESIAN_POINT('Ctrl Pts',(-13.336055040414,-12.7585743721417,
116.658379630691)) ;
#160669 = CARTESIAN_POINT('Ctrl Pts',(-13.4098588990292,-12.7585743165694,
116.634148635288)) ;
#160670 = CARTESIAN_POINT('Ctrl Pts',(-13.4836627576445,-12.7585742609971,
116.609917639884)) ;
#160671 = CARTESIAN_POINT('Ctrl Pts',(-13.4656064949594,-12.7094641505378,
116.554921175684)) ;
#160672 = CARTESIAN_POINT('Ctrl Pts',(-13.4475502322743,-12.6603540400784,
116.499924711483)) ;
#160673 = CARTESIAN_POINT('Ctrl Pts',(-13.3737463736591,-12.6603540956507,
116.524155706886)) ;
#160674 = CARTESIAN_POINT('Ctrl Pts',(-13.2999425150438,-12.660354151223,
116.54838670229)) ;
#160675 = CARTESIAN_POINT('Ctrl Pts',(-13.3179987777289,-12.7094642616823,
116.60338316649)) ;
#160676 = CARTESIAN_POINT('Ctrl Pts',(-13.3968395702768,-12.5150572905195,
116.807856696789)) ;
#160677 = CARTESIAN_POINT('Ctrl Pts',(-13.4101566106701,-12.5778156836835,
116.848418254369)) ;
#160678 = CARTESIAN_POINT('Ctrl Pts',(-13.4839604707963,-12.5778156484991,
116.824187263567)) ;
#160679 = CARTESIAN_POINT('Ctrl Pts',(-13.5577643309226,-12.5778156133148,
116.799956272766)) ;
#160680 = CARTESIAN_POINT('Ctrl Pts',(-13.5444472905293,-12.5150572201508,
116.759394715186)) ;
#160681 = CARTESIAN_POINT('Ctrl Pts',(-13.531130250136,-12.4522988269869,
116.718833157607)) ;
#160682 = CARTESIAN_POINT('Ctrl Pts',(-13.4573263900098,-12.4522988621712,
116.743064148408)) ;
#160683 = CARTESIAN_POINT('Ctrl Pts',(-13.3835225298836,-12.4522988973556,
116.767295139209)) ;
#160684 = CARTESIAN_POINT('Ctrl Pts',(-13.3968395702768,-12.5150572905195,
116.807856696789)) ;
#160685 = CARTESIAN_POINT('Ctrl Pts',(-13.4880657336334,-12.3871819681861,
117.050541251165)) ;
#160686 = CARTESIAN_POINT('Ctrl Pts',(-13.4957612186245,-12.4589631112732,
117.073980457915)) ;
#160687 = CARTESIAN_POINT('Ctrl Pts',(-13.5695650793503,-12.4589630933021,
117.049749468939)) ;
#160688 = CARTESIAN_POINT('Ctrl Pts',(-13.6433689400761,-12.458963075331,
117.025518479964)) ;
#160689 = CARTESIAN_POINT('Ctrl Pts',(-13.635673455085,-12.3871819322439,
117.002079273215)) ;
#160690 = CARTESIAN_POINT('Ctrl Pts',(-13.6279779700939,-12.3154007891568,
116.978640066466)) ;
#160691 = CARTESIAN_POINT('Ctrl Pts',(-13.5541741093681,-12.3154008071279,
117.002871055441)) ;
#160692 = CARTESIAN_POINT('Ctrl Pts',(-13.4803702486423,-12.315400825099,
117.027102044416)) ;
#160693 = CARTESIAN_POINT('Ctrl Pts',(-13.4880657336334,-12.3871819681861,
117.050541251165)) ;
#160694 = CARTESIAN_POINT('Ctrl Pts',(-13.5882207279045,-12.3316884564228,
117.319958997263)) ;
#160695 = CARTESIAN_POINT('Ctrl Pts',(-13.5896724457049,-12.4074536121107,
117.324380696378)) ;
#160696 = CARTESIAN_POINT('Ctrl Pts',(-13.663476304107,-12.4074536102533,
117.300149700326)) ;
#160697 = CARTESIAN_POINT('Ctrl Pts',(-13.7372801625091,-12.407453608396,
117.275918704273)) ;
#160698 = CARTESIAN_POINT('Ctrl Pts',(-13.7358284447087,-12.3316884527082,
117.271497005158)) ;
#160699 = CARTESIAN_POINT('Ctrl Pts',(-13.7343767269083,-12.2559232970203,
117.267075306043)) ;
#160700 = CARTESIAN_POINT('Ctrl Pts',(-13.6605728685062,-12.2559232988777,
117.291306302096)) ;
#160701 = CARTESIAN_POINT('Ctrl Pts',(-13.5867690101041,-12.255923300735,
117.315537298149)) ;
#160702 = CARTESIAN_POINT('Ctrl Pts',(-13.5882207279045,-12.3316884564228,
117.319958997263)) ;
#160703 = CARTESIAN_POINT('Ctrl Pts',(-13.6888941607603,-12.3542922095437,
117.591275254107)) ;
#160704 = CARTESIAN_POINT('Ctrl Pts',(-13.6840497212975,-12.4285936621951,
117.576519873938)) ;
#160705 = CARTESIAN_POINT('Ctrl Pts',(-13.7578535770702,-12.428593671534,
117.552288869877)) ;
#160706 = CARTESIAN_POINT('Ctrl Pts',(-13.831657432843,-12.428593680873,117.528057865815)) ;
#160707 = CARTESIAN_POINT('Ctrl Pts',(-13.8365018723058,-12.3542922282216,
117.542813245984)) ;
#160708 = CARTESIAN_POINT('Ctrl Pts',(-13.8413463117686,-12.2799907755701,
117.557568626153)) ;
#160709 = CARTESIAN_POINT('Ctrl Pts',(-13.7675424559959,-12.2799907662312,
117.581799630214)) ;
#160710 = CARTESIAN_POINT('Ctrl Pts',(-13.6937386002231,-12.2799907568923,
117.606030634276)) ;
#160711 = CARTESIAN_POINT('Ctrl Pts',(-13.6888941607603,-12.3542922095437,
117.591275254107)) ;
#160712 = CARTESIAN_POINT('Ctrl Pts',(-13.7853698113562,-12.4537268763868,
117.849457635997)) ;
#160713 = CARTESIAN_POINT('Ctrl Pts',(-13.774519802585,-12.5211987643482,
117.816410260506)) ;
#160714 = CARTESIAN_POINT('Ctrl Pts',(-13.8483236542404,-12.5211987790939,
117.792179243904)) ;
#160715 = CARTESIAN_POINT('Ctrl Pts',(-13.9221275058957,-12.5211987938395,
117.767948227302)) ;
#160716 = CARTESIAN_POINT('Ctrl Pts',(-13.932977514667,-12.4537269058781,
117.800995602792)) ;
#160717 = CARTESIAN_POINT('Ctrl Pts',(-13.9438275234382,-12.3862550179166,
117.834042978283)) ;
#160718 = CARTESIAN_POINT('Ctrl Pts',(-13.8700236717828,-12.386255003171,
117.858273994885)) ;
#160719 = CARTESIAN_POINT('Ctrl Pts',(-13.7962198201275,-12.3862549884253,
117.882505011487)) ;
#160720 = CARTESIAN_POINT('Ctrl Pts',(-13.7853698113562,-12.4537268763868,
117.849457635997)) ;
#160721 = CARTESIAN_POINT('Ctrl Pts',(-13.8696982601704,-12.6212675456056,
118.070986029358)) ;
#160722 = CARTESIAN_POINT('Ctrl Pts',(-13.8536747152405,-12.6771429779521,
118.022180897344)) ;
#160723 = CARTESIAN_POINT('Ctrl Pts',(-13.9274785638659,-12.6771429943205,
117.997949871512)) ;
#160724 = CARTESIAN_POINT('Ctrl Pts',(-14.0012824124912,-12.6771430106889,
117.973718845681)) ;
#160725 = CARTESIAN_POINT('Ctrl Pts',(-14.017305957421,-12.6212675783423,
118.022523977695)) ;
#160726 = CARTESIAN_POINT('Ctrl Pts',(-14.0333295023509,-12.5653921459958,
118.07132910971)) ;
#160727 = CARTESIAN_POINT('Ctrl Pts',(-13.9595256537255,-12.5653921296274,
118.095560135541)) ;
#160728 = CARTESIAN_POINT('Ctrl Pts',(-13.8857218051002,-12.565392113259,
118.119791161372)) ;
#160729 = CARTESIAN_POINT('Ctrl Pts',(-13.8696982601704,-12.6212675456056,
118.070986029358)) ;
#160730 = CARTESIAN_POINT('Ctrl Pts',(-13.9378798134609,-12.846192059173,
118.243189707452)) ;
#160731 = CARTESIAN_POINT('Ctrl Pts',(-13.917805231475,-12.8864467914097,
118.18204577005)) ;
#160732 = CARTESIAN_POINT('Ctrl Pts',(-13.9916090772929,-12.8864468052169,
118.157814735668)) ;
#160733 = CARTESIAN_POINT('Ctrl Pts',(-14.0654129231109,-12.8864468190241,
118.133583701286)) ;
#160734 = CARTESIAN_POINT('Ctrl Pts',(-14.0854875050968,-12.8461920867874,
118.194727638688)) ;
#160735 = CARTESIAN_POINT('Ctrl Pts',(-14.1055620870827,-12.8059373545508,
118.25587157609)) ;
#160736 = CARTESIAN_POINT('Ctrl Pts',(-14.0317582412647,-12.8059373407436,
118.280102610472)) ;
#160737 = CARTESIAN_POINT('Ctrl Pts',(-13.9579543954468,-12.8059373269364,
118.304333644854)) ;
#160738 = CARTESIAN_POINT('Ctrl Pts',(-13.9378798134609,-12.846192059173,
118.243189707452)) ;
#160739 = CARTESIAN_POINT('Ctrl Pts',(-13.9854016724836,-13.1124184461725,
118.352441492381)) ;
#160740 = CARTESIAN_POINT('Ctrl Pts',(-13.9627130007129,-13.1341445509028,
118.283335459142)) ;
#160741 = CARTESIAN_POINT('Ctrl Pts',(-14.0365168447199,-13.1341445595333,
118.259104419244)) ;
#160742 = CARTESIAN_POINT('Ctrl Pts',(-14.1103206887269,-13.1341445681639,
118.234873379346)) ;
#160743 = CARTESIAN_POINT('Ctrl Pts',(-14.1330093604975,-13.1124184634336,
118.303979412585)) ;
#160744 = CARTESIAN_POINT('Ctrl Pts',(-14.1556980322682,-13.0906923587033,
118.373085445824)) ;
#160745 = CARTESIAN_POINT('Ctrl Pts',(-14.0818941882612,-13.0906923500727,
118.397316485722)) ;
#160746 = CARTESIAN_POINT('Ctrl Pts',(-14.0080903442542,-13.0906923414422,
118.42154752562)) ;
#160747 = CARTESIAN_POINT('Ctrl Pts',(-13.9854016724836,-13.1124184461725,
118.352441492381)) ;
#160748 = CARTESIAN_POINT('Ctrl Pts',(-14.0095130072085,-13.400879749144,
118.390345126407)) ;
#160749 = CARTESIAN_POINT('Ctrl Pts',(-13.9858419287106,-13.4024961126535,
118.318246840676)) ;
#160750 = CARTESIAN_POINT('Ctrl Pts',(-14.059645772004,-13.4024961156936,
118.294015798605)) ;
#160751 = CARTESIAN_POINT('Ctrl Pts',(-14.1334496152975,-13.4024961187337,
118.269784756533)) ;
#160752 = CARTESIAN_POINT('Ctrl Pts',(-14.1571206937954,-13.4008797552242,
118.341883042265)) ;
#160753 = CARTESIAN_POINT('Ctrl Pts',(-14.1807917722932,-13.3992633917147,
118.413981327996)) ;
#160754 = CARTESIAN_POINT('Ctrl Pts',(-14.1069879289998,-13.3992633886746,
118.438212370068)) ;
#160755 = CARTESIAN_POINT('Ctrl Pts',(-14.0331840857064,-13.3992633856344,
118.462443412139)) ;
#160756 = CARTESIAN_POINT('Ctrl Pts',(-14.0095130072085,-13.400879749144,
118.390345126407)) ;
#160757 = CARTESIAN_POINT('Ctrl Pts',(-14.0093724892591,-13.6891262166377,
118.354574264124)) ;
#160758 = CARTESIAN_POINT('Ctrl Pts',(-13.9864072579121,-13.6706178186388,
118.284625874855)) ;
#160759 = CARTESIAN_POINT('Ctrl Pts',(-14.0602111012856,-13.6706178179427,
118.260394833028)) ;
#160760 = CARTESIAN_POINT('Ctrl Pts',(-14.1340149446592,-13.6706178172465,
118.236163791201)) ;
#160761 = CARTESIAN_POINT('Ctrl Pts',(-14.1569801760062,-13.6891262152454,
118.30611218047)) ;
#160762 = CARTESIAN_POINT('Ctrl Pts',(-14.1799454073532,-13.7076346132443,
118.376060569739)) ;
#160763 = CARTESIAN_POINT('Ctrl Pts',(-14.1061415639797,-13.7076346139405,
118.400291611566)) ;
#160764 = CARTESIAN_POINT('Ctrl Pts',(-14.0323377206061,-13.7076346146366,
118.424522653393)) ;
#160765 = CARTESIAN_POINT('Ctrl Pts',(-14.0093724892591,-13.6891262166377,
118.354574264124)) ;
#160766 = CARTESIAN_POINT('Ctrl Pts',(-13.985414910218,-13.9605413879786,
118.245894494186)) ;
#160767 = CARTESIAN_POINT('Ctrl Pts',(-13.9648272415158,-13.9230519796462,
118.183187777064)) ;
#160768 = CARTESIAN_POINT('Ctrl Pts',(-14.0386310853959,-13.9230519767635,
118.15895673678)) ;
#160769 = CARTESIAN_POINT('Ctrl Pts',(-14.1124349292761,-13.9230519738809,
118.134725696495)) ;
#160770 = CARTESIAN_POINT('Ctrl Pts',(-14.1330225979783,-13.9605413822133,
118.197432413617)) ;
#160771 = CARTESIAN_POINT('Ctrl Pts',(-14.1536102666806,-13.9980307905457,
118.260139130739)) ;
#160772 = CARTESIAN_POINT('Ctrl Pts',(-14.0798064228004,-13.9980307934284,
118.284370171023)) ;
#160773 = CARTESIAN_POINT('Ctrl Pts',(-14.0060025789203,-13.9980307963111,
118.308601211307)) ;
#160774 = CARTESIAN_POINT('Ctrl Pts',(-13.985414910218,-13.9605413879786,
118.245894494186)) ;
#160775 = CARTESIAN_POINT('Ctrl Pts',(-13.9409451108123,-14.1894540736428,
118.075288407443)) ;
#160776 = CARTESIAN_POINT('Ctrl Pts',(-13.9241599655485,-14.1359254038344,
118.02416356318)) ;
#160777 = CARTESIAN_POINT('Ctrl Pts',(-13.9979638096976,-14.1359254016367,
117.999932523715)) ;
#160778 = CARTESIAN_POINT('Ctrl Pts',(-14.0717676538467,-14.135925399439,
117.97570148425)) ;
#160779 = CARTESIAN_POINT('Ctrl Pts',(-14.0885527991105,-14.1894540692474,
118.026826328513)) ;
#160780 = CARTESIAN_POINT('Ctrl Pts',(-14.1053379443743,-14.2429827390558,
118.077951172775)) ;
#160781 = CARTESIAN_POINT('Ctrl Pts',(-14.0315341002252,-14.2429827412535,
118.10218221224)) ;
#160782 = CARTESIAN_POINT('Ctrl Pts',(-13.9577302560761,-14.2429827434512,
118.126413251706)) ;
#160783 = CARTESIAN_POINT('Ctrl Pts',(-13.9409451108123,-14.1894540736428,
118.075288407443)) ;
#160784 = CARTESIAN_POINT('Ctrl Pts',(-13.8788030525502,-14.3660067048925,
117.850395877402)) ;
#160785 = CARTESIAN_POINT('Ctrl Pts',(-13.8670695405437,-14.3000702425711,
117.814657493004)) ;
#160786 = CARTESIAN_POINT('Ctrl Pts',(-13.9408733842996,-14.3000702422313,
117.790426452341)) ;
#160787 = CARTESIAN_POINT('Ctrl Pts',(-14.0146772280555,-14.3000702418915,
117.766195411678)) ;
#160788 = CARTESIAN_POINT('Ctrl Pts',(-14.026410740062,-14.3660067042129,
117.801933796077)) ;
#160789 = CARTESIAN_POINT('Ctrl Pts',(-14.0381442520685,-14.4319431665342,
117.837672180475)) ;
#160790 = CARTESIAN_POINT('Ctrl Pts',(-13.9643404083126,-14.431943166874,
117.861903221138)) ;
#160791 = CARTESIAN_POINT('Ctrl Pts',(-13.8905365645568,-14.4319431672138,
117.886134261801)) ;
#160792 = CARTESIAN_POINT('Ctrl Pts',(-13.8788030525502,-14.3660067048925,
117.850395877402)) ;
#160793 = CARTESIAN_POINT('Ctrl Pts',(-13.805049295041,-14.4734792612079,
117.590360278057)) ;
#160794 = CARTESIAN_POINT('Ctrl Pts',(-13.7991810058367,-14.3999420243742,
117.572486416034)) ;
#160795 = CARTESIAN_POINT('Ctrl Pts',(-13.8729848485188,-14.3999420254069,
117.548255372101)) ;
#160796 = CARTESIAN_POINT('Ctrl Pts',(-13.9467886912009,-14.3999420264397,
117.524024328167)) ;
#160797 = CARTESIAN_POINT('Ctrl Pts',(-13.9526569804052,-14.4734792632734,
117.54189819019)) ;
#160798 = CARTESIAN_POINT('Ctrl Pts',(-13.9585252696096,-14.5470165001072,
117.559772052213)) ;
#160799 = CARTESIAN_POINT('Ctrl Pts',(-13.8847214269275,-14.5470164990744,
117.584003096146)) ;
#160800 = CARTESIAN_POINT('Ctrl Pts',(-13.8109175842454,-14.5470164980416,
117.60823414008)) ;
#160801 = CARTESIAN_POINT('Ctrl Pts',(-13.805049295041,-14.4734792612079,
117.590360278057)) ;
#160802 = CARTESIAN_POINT('Ctrl Pts',(-13.7251059804211,-14.5056975632985,
117.311316857951)) ;
#160803 = CARTESIAN_POINT('Ctrl Pts',(-13.7255468602542,-14.4298031115965,
117.312659706948)) ;
#160804 = CARTESIAN_POINT('Ctrl Pts',(-13.7993507010675,-14.4298031119292,
117.288428657322)) ;
#160805 = CARTESIAN_POINT('Ctrl Pts',(-13.8731545418808,-14.4298031122619,
117.264197607697)) ;
#160806 = CARTESIAN_POINT('Ctrl Pts',(-13.8727136620476,-14.5056975639639,
117.2628547587)) ;
#160807 = CARTESIAN_POINT('Ctrl Pts',(-13.8722727822144,-14.5815920156659,
117.261511909703)) ;
#160808 = CARTESIAN_POINT('Ctrl Pts',(-13.7984689414012,-14.5815920153332,
117.285742959328)) ;
#160809 = CARTESIAN_POINT('Ctrl Pts',(-13.7246651005879,-14.5815920150005,
117.309974008954)) ;
#160810 = CARTESIAN_POINT('Ctrl Pts',(-13.7251059804211,-14.5056975632985,
117.311316857951)) ;
#160811 = CARTESIAN_POINT('Ctrl Pts',(-13.6460687434891,-14.4599236721213,
117.035189019244)) ;
#160812 = CARTESIAN_POINT('Ctrl Pts',(-13.6527613166628,-14.387115192455,
117.055573517566)) ;
#160813 = CARTESIAN_POINT('Ctrl Pts',(-13.7265651557173,-14.3871151888849,
117.031342462584)) ;
#160814 = CARTESIAN_POINT('Ctrl Pts',(-13.8003689947718,-14.3871151853148,
117.007111407601)) ;
#160815 = CARTESIAN_POINT('Ctrl Pts',(-13.7936764215981,-14.4599236649811,
116.986726909279)) ;
#160816 = CARTESIAN_POINT('Ctrl Pts',(-13.7869838484244,-14.5327321446473,
116.966342410956)) ;
#160817 = CARTESIAN_POINT('Ctrl Pts',(-13.7131800093699,-14.5327321482174,
116.990573465939)) ;
#160818 = CARTESIAN_POINT('Ctrl Pts',(-13.6393761703155,-14.5327321517875,
117.014804520921)) ;
#160819 = CARTESIAN_POINT('Ctrl Pts',(-13.6460687434891,-14.4599236721213,
117.035189019244)) ;
#160820 = CARTESIAN_POINT('Ctrl Pts',(-13.5738853047407,-14.3395761921465,
116.779866121718)) ;
#160821 = CARTESIAN_POINT('Ctrl Pts',(-13.5863614796708,-14.27506508821,116.817866537953)) ;
#160822 = CARTESIAN_POINT('Ctrl Pts',(-13.660165317222,-14.2750650771765,
116.793635478392)) ;
#160823 = CARTESIAN_POINT('Ctrl Pts',(-13.7339691547732,-14.2750650661431,
116.76940441883)) ;
#160824 = CARTESIAN_POINT('Ctrl Pts',(-13.7214929798432,-14.3395761700796,
116.731404002596)) ;
#160825 = CARTESIAN_POINT('Ctrl Pts',(-13.7090168049131,-14.4040872740161,
116.693403586361)) ;
#160826 = CARTESIAN_POINT('Ctrl Pts',(-13.6352129673619,-14.4040872850496,
116.717634645922)) ;
#160827 = CARTESIAN_POINT('Ctrl Pts',(-13.5614091298106,-14.404087296083,
116.741865705483)) ;
#160828 = CARTESIAN_POINT('Ctrl Pts',(-13.5738853047407,-14.3395761921465,
116.779866121718)) ;
#160829 = CARTESIAN_POINT('Ctrl Pts',(-13.5146382184193,-14.1535350418836,
116.563988746602)) ;
#160830 = CARTESIAN_POINT('Ctrl Pts',(-13.5320020882261,-14.101920284912,
116.616876292952)) ;
#160831 = CARTESIAN_POINT('Ctrl Pts',(-13.6058059252282,-14.1019202637606,
116.592645231719)) ;
#160832 = CARTESIAN_POINT('Ctrl Pts',(-13.6796097622303,-14.1019202426092,
116.568414170485)) ;
#160833 = CARTESIAN_POINT('Ctrl Pts',(-13.6622458924235,-14.1535349995808,
116.515526624135)) ;
#160834 = CARTESIAN_POINT('Ctrl Pts',(-13.6448820226168,-14.2051497565524,
116.462639077784)) ;
#160835 = CARTESIAN_POINT('Ctrl Pts',(-13.5710781856146,-14.2051497777038,
116.486870139018)) ;
#160836 = CARTESIAN_POINT('Ctrl Pts',(-13.4972743486125,-14.2051497988552,
116.511101200251)) ;
#160837 = CARTESIAN_POINT('Ctrl Pts',(-13.5146382184193,-14.1535350418836,
116.563988746602)) ;
#160838 = CARTESIAN_POINT('Ctrl Pts',(-13.4731069605417,-13.9130985111844,
116.401832242531)) ;
#160839 = CARTESIAN_POINT('Ctrl Pts',(-13.4941337169664,-13.8781962453412,
116.465876350717)) ;
#160840 = CARTESIAN_POINT('Ctrl Pts',(-13.5679375545039,-13.8781962102056,
116.441645291114)) ;
#160841 = CARTESIAN_POINT('Ctrl Pts',(-13.6417413920414,-13.87819617507,116.417414231511)) ;
#160842 = CARTESIAN_POINT('Ctrl Pts',(-13.6207146356167,-13.9130984409133,
116.353370123325)) ;
#160843 = CARTESIAN_POINT('Ctrl Pts',(-13.5996878791919,-13.9480007067565,
116.28932601514)) ;
#160844 = CARTESIAN_POINT('Ctrl Pts',(-13.5258840416544,-13.9480007418921,
116.313557074743)) ;
#160845 = CARTESIAN_POINT('Ctrl Pts',(-13.452080204117,-13.9480007770277,
116.337788134346)) ;
#160846 = CARTESIAN_POINT('Ctrl Pts',(-13.4731069605417,-13.9130985111844,
116.401832242531)) ;
#160847 = CARTESIAN_POINT('Ctrl Pts',(-13.4535360973529,-13.6395736822347,
116.306908957539)) ;
#160848 = CARTESIAN_POINT('Ctrl Pts',(-13.4766902515202,-13.6237185301076,
116.377432776133)) ;
#160849 = CARTESIAN_POINT('Ctrl Pts',(-13.5504940917278,-13.6237184841126,
116.353201724663)) ;
#160850 = CARTESIAN_POINT('Ctrl Pts',(-13.6242979319354,-13.6237184381175,
116.328970673193)) ;
#160851 = CARTESIAN_POINT('Ctrl Pts',(-13.6011437777682,-13.6395735902447,
116.258446854598)) ;
#160852 = CARTESIAN_POINT('Ctrl Pts',(-13.577989623601,-13.6554287423718,
116.187923036004)) ;
#160853 = CARTESIAN_POINT('Ctrl Pts',(-13.5041857833933,-13.6554287883668,
116.212154087474)) ;
#160854 = CARTESIAN_POINT('Ctrl Pts',(-13.4303819431857,-13.6554288343619,
116.236385138944)) ;
#160855 = CARTESIAN_POINT('Ctrl Pts',(-13.4535360973529,-13.6395736822347,
116.306908957539)) ;
#160856 = CARTESIAN_POINT('Ctrl Pts',(-13.4576157743933,-13.3487006076146,
116.283814176628)) ;
#160857 = CARTESIAN_POINT('Ctrl Pts',(-13.4812536077164,-13.3531309210736,
116.355811204069)) ;
#160858 = CARTESIAN_POINT('Ctrl Pts',(-13.5550574520074,-13.3531308648212,
116.331580165036)) ;
#160859 = CARTESIAN_POINT('Ctrl Pts',(-13.6288612962983,-13.3531308085687,
116.307349126003)) ;
#160860 = CARTESIAN_POINT('Ctrl Pts',(-13.6052234629752,-13.3487004951098,
116.235352098562)) ;
#160861 = CARTESIAN_POINT('Ctrl Pts',(-13.5815856296521,-13.3442701816508,
116.163355071121)) ;
#160862 = CARTESIAN_POINT('Ctrl Pts',(-13.5077817853611,-13.3442702379032,
116.187586110155)) ;
#160863 = CARTESIAN_POINT('Ctrl Pts',(-13.4339779410702,-13.3442702941557,
116.211817149188)) ;
#160864 = CARTESIAN_POINT('Ctrl Pts',(-13.4576157743933,-13.3487006076146,
116.283814176628)) ;
#160865 = CARTESIAN_POINT('Ctrl Pts',(-13.4859406302875,-13.0636371844073,
116.334679965118)) ;
#160866 = CARTESIAN_POINT('Ctrl Pts',(-13.5083676426488,-13.0879765100876,
116.402989027427)) ;
#160867 = CARTESIAN_POINT('Ctrl Pts',(-13.5821714923869,-13.0879764491053,
116.378758004986)) ;
#160868 = CARTESIAN_POINT('Ctrl Pts',(-13.655975342125,-13.0879763881229,
116.354526982544)) ;
#160869 = CARTESIAN_POINT('Ctrl Pts',(-13.6335483297638,-13.0636370624426,
116.286217920235)) ;
#160870 = CARTESIAN_POINT('Ctrl Pts',(-13.6111213174025,-13.0392977367622,
116.217908857925)) ;
#160871 = CARTESIAN_POINT('Ctrl Pts',(-13.5373174676644,-13.0392977977446,
116.242139880367)) ;
#160872 = CARTESIAN_POINT('Ctrl Pts',(-13.4635136179263,-13.0392978587269,
116.266370902809)) ;
#160873 = CARTESIAN_POINT('Ctrl Pts',(-13.4859406302875,-13.0636371844073,
116.334679965118)) ;
#160874 = CARTESIAN_POINT('Ctrl Pts',(-13.537302484578,-12.803286823163,116.455624512449)) ;
#160875 = CARTESIAN_POINT('Ctrl Pts',(-13.5569104932401,-12.8458384350668,
116.515347344498)) ;
#160876 = CARTESIAN_POINT('Ctrl Pts',(-13.6307143492738,-12.8458383747554,
116.491116341231)) ;
#160877 = CARTESIAN_POINT('Ctrl Pts',(-13.7045182053075,-12.8458383144439,
116.466885337965)) ;
#160878 = CARTESIAN_POINT('Ctrl Pts',(-13.6849101966454,-12.8032867025401,
116.407162505917)) ;
#160879 = CARTESIAN_POINT('Ctrl Pts',(-13.6653021879832,-12.7607350906363,
116.347439673868)) ;
#160880 = CARTESIAN_POINT('Ctrl Pts',(-13.5914983319496,-12.7607351509478,
116.371670677135)) ;
#160881 = CARTESIAN_POINT('Ctrl Pts',(-13.5176944759159,-12.7607352112592,
116.395901680401)) ;
#160882 = CARTESIAN_POINT('Ctrl Pts',(-13.537302484578,-12.803286823163,116.455624512449)) ;
#160883 = CARTESIAN_POINT('Ctrl Pts',(-13.6086911430819,-12.5872505028287,
116.637604570861)) ;
#160884 = CARTESIAN_POINT('Ctrl Pts',(-13.6240771137081,-12.644946835435,
116.68446775642)) ;
#160885 = CARTESIAN_POINT('Ctrl Pts',(-13.697880976079,-12.6449467832351,
116.660236772456)) ;
#160886 = CARTESIAN_POINT('Ctrl Pts',(-13.7716848384499,-12.6449467310352,
116.636005788491)) ;
#160887 = CARTESIAN_POINT('Ctrl Pts',(-13.7562988678237,-12.5872503984288,
116.589142602933)) ;
#160888 = CARTESIAN_POINT('Ctrl Pts',(-13.7409128971974,-12.5295540658224,
116.542279417374)) ;
#160889 = CARTESIAN_POINT('Ctrl Pts',(-13.6671090348266,-12.5295541180224,
116.566510401338)) ;
#160890 = CARTESIAN_POINT('Ctrl Pts',(-13.5933051724557,-12.5295541702223,
116.590741385303)) ;
#160891 = CARTESIAN_POINT('Ctrl Pts',(-13.6086911430819,-12.5872505028287,
116.637604570861)) ;
#160892 = CARTESIAN_POINT('Ctrl Pts',(-13.6958832608641,-12.4304809457012,
116.867672531912)) ;
#160893 = CARTESIAN_POINT('Ctrl Pts',(-13.705938807208,-12.4992062995871,
116.898300105306)) ;
#160894 = CARTESIAN_POINT('Ctrl Pts',(-13.7797426752621,-12.4992062624081,
116.874069138652)) ;
#160895 = CARTESIAN_POINT('Ctrl Pts',(-13.8535465433162,-12.4992062252292,
116.849838171998)) ;
#160896 = CARTESIAN_POINT('Ctrl Pts',(-13.8434909969723,-12.4304808713433,
116.819210598604)) ;
#160897 = CARTESIAN_POINT('Ctrl Pts',(-13.8334354506284,-12.3617555174574,
116.788583025209)) ;
#160898 = CARTESIAN_POINT('Ctrl Pts',(-13.7596315825743,-12.3617555546364,
116.812813991863)) ;
#160899 = CARTESIAN_POINT('Ctrl Pts',(-13.6858277145202,-12.3617555918153,
116.837044958517)) ;
#160900 = CARTESIAN_POINT('Ctrl Pts',(-13.6958832608641,-12.4304809457012,
116.867672531912)) ;
#160901 = CARTESIAN_POINT('Ctrl Pts',(-13.7933144950255,-12.3447676693836,
117.128927982332)) ;
#160902 = CARTESIAN_POINT('Ctrl Pts',(-13.7973170359522,-12.4195774199376,
117.141119077995)) ;
#160903 = CARTESIAN_POINT('Ctrl Pts',(-13.8711209081213,-12.4195774042201,
117.116888123875)) ;
#160904 = CARTESIAN_POINT('Ctrl Pts',(-13.9449247802904,-12.4195773885026,
117.092657169754)) ;
#160905 = CARTESIAN_POINT('Ctrl Pts',(-13.9409222393638,-12.3447676379485,
117.080466074092)) ;
#160906 = CARTESIAN_POINT('Ctrl Pts',(-13.9369196984371,-12.2699578873945,
117.068274978429)) ;
#160907 = CARTESIAN_POINT('Ctrl Pts',(-13.863115826268,-12.269957903112,117.092505932549)) ;
#160908 = CARTESIAN_POINT('Ctrl Pts',(-13.7893119540988,-12.2699579188295,
117.11673688667)) ;
#160909 = CARTESIAN_POINT('Ctrl Pts',(-13.7933144950255,-12.3447676693836,
117.128927982332)) ;
#160910 = CARTESIAN_POINT('Ctrl Pts',(-13.8942106173158,-12.3358385329225,
117.400917482378)) ;
#160911 = CARTESIAN_POINT('Ctrl Pts',(-13.8919056550011,-12.4113804397121,
117.393896940963)) ;
#160912 = CARTESIAN_POINT('Ctrl Pts',(-13.965709528786,-12.4113804494303,
117.369665991764)) ;
#160913 = CARTESIAN_POINT('Ctrl Pts',(-14.039513402571,-12.4113804591485,
117.345435042565)) ;
#160914 = CARTESIAN_POINT('Ctrl Pts',(-14.0418183648857,-12.335838552359,
117.35245558398)) ;
#160915 = CARTESIAN_POINT('Ctrl Pts',(-14.0441233272004,-12.2602966455695,
117.359476125395)) ;
#160916 = CARTESIAN_POINT('Ctrl Pts',(-13.9703194534154,-12.2602966358513,
117.383707074594)) ;
#160917 = CARTESIAN_POINT('Ctrl Pts',(-13.8965155796305,-12.260296626133,
117.407938023793)) ;
#160918 = CARTESIAN_POINT('Ctrl Pts',(-13.8942106173158,-12.3358385329225,
117.400917482378)) ;
#160919 = CARTESIAN_POINT('Ctrl Pts',(-13.9931058830893,-12.4042599768703,
117.666636589428)) ;
#160920 = CARTESIAN_POINT('Ctrl Pts',(-13.9846276244577,-12.4751356263476,
117.640813183575)) ;
#160921 = CARTESIAN_POINT('Ctrl Pts',(-14.0584314976336,-12.4751356632063,
117.616582232521)) ;
#160922 = CARTESIAN_POINT('Ctrl Pts',(-14.1322353708096,-12.4751357000651,
117.592351281467)) ;
#160923 = CARTESIAN_POINT('Ctrl Pts',(-14.1407136294413,-12.4042600505878,
117.61817468732)) ;
#160924 = CARTESIAN_POINT('Ctrl Pts',(-14.1491918880729,-12.3333844011106,
117.643998093173)) ;
#160925 = CARTESIAN_POINT('Ctrl Pts',(-14.0753880148969,-12.3333843642518,
117.668229044227)) ;
#160926 = CARTESIAN_POINT('Ctrl Pts',(-14.0015841417209,-12.3333843273931,
117.692459995281)) ;
#160927 = CARTESIAN_POINT('Ctrl Pts',(-13.9931058830893,-12.4042599768703,
117.666636589428)) ;
#160928 = CARTESIAN_POINT('Ctrl Pts',(-14.0830802598219,-12.5454038835963,
117.905215825566)) ;
#160929 = CARTESIAN_POINT('Ctrl Pts',(-14.0690417835344,-12.6065294802411,
117.862456893932)) ;
#160930 = CARTESIAN_POINT('Ctrl Pts',(-14.1428456533588,-12.6065295430782,
117.83822593267)) ;
#160931 = CARTESIAN_POINT('Ctrl Pts',(-14.2166495231833,-12.6065296059152,
117.813994971409)) ;
#160932 = CARTESIAN_POINT('Ctrl Pts',(-14.2306879994708,-12.5454040092703,
117.856753903043)) ;
#160933 = CARTESIAN_POINT('Ctrl Pts',(-14.2447264757583,-12.4842784126255,
117.899512834677)) ;
#160934 = CARTESIAN_POINT('Ctrl Pts',(-14.1709226059339,-12.4842783497885,
117.923743795939)) ;
#160935 = CARTESIAN_POINT('Ctrl Pts',(-14.0971187361094,-12.4842782869515,
117.9479747572)) ;
#160936 = CARTESIAN_POINT('Ctrl Pts',(-14.0830802598219,-12.5454038835963,
117.905215825566)) ;
#160937 = CARTESIAN_POINT('Ctrl Pts',(-14.1585388443987,-12.7490645526663,
118.099576579279)) ;
#160938 = CARTESIAN_POINT('Ctrl Pts',(-14.1399454760981,-12.796061398436,
118.042944181542)) ;
#160939 = CARTESIAN_POINT('Ctrl Pts',(-14.2137493401466,-12.7960614831609,
118.018713202688)) ;
#160940 = CARTESIAN_POINT('Ctrl Pts',(-14.2875532041952,-12.7960615678859,
117.994482223833)) ;
#160941 = CARTESIAN_POINT('Ctrl Pts',(-14.3061465724958,-12.7490647221162,
118.05111462157)) ;
#160942 = CARTESIAN_POINT('Ctrl Pts',(-14.3247399407963,-12.7020678763465,
118.107747019307)) ;
#160943 = CARTESIAN_POINT('Ctrl Pts',(-14.2509360767478,-12.7020677916216,
118.131977998162)) ;
#160944 = CARTESIAN_POINT('Ctrl Pts',(-14.1771322126992,-12.7020677068967,
118.156208977016)) ;
#160945 = CARTESIAN_POINT('Ctrl Pts',(-14.1585388443987,-12.7490645526663,
118.099576579279)) ;
#160946 = CARTESIAN_POINT('Ctrl Pts',(-14.2147792241185,-13.0004109945635,
118.235435558541)) ;
#160947 = CARTESIAN_POINT('Ctrl Pts',(-14.1929652259204,-13.0299291555683,
118.168993641801)) ;
#160948 = CARTESIAN_POINT('Ctrl Pts',(-14.2667690823032,-13.0299292556675,
118.144762639597)) ;
#160949 = CARTESIAN_POINT('Ctrl Pts',(-14.340572938686,-13.0299293557667,
118.120531637394)) ;
#160950 = CARTESIAN_POINT('Ctrl Pts',(-14.362386936884,-13.0004111947619,
118.186973554135)) ;
#160951 = CARTESIAN_POINT('Ctrl Pts',(-14.384200935082,-12.9708930337571,
118.253415470876)) ;
#160952 = CARTESIAN_POINT('Ctrl Pts',(-14.3103970786992,-12.9708929336578,
118.277646473079)) ;
#160953 = CARTESIAN_POINT('Ctrl Pts',(-14.2365932223165,-12.9708928335586,
118.301877475282)) ;
#160954 = CARTESIAN_POINT('Ctrl Pts',(-14.2147792241185,-13.0004109945635,
118.235435558541)) ;
#160955 = CARTESIAN_POINT('Ctrl Pts',(-14.2486273894212,-13.281956740539,
118.303050309436)) ;
#160956 = CARTESIAN_POINT('Ctrl Pts',(-14.2251520583296,-13.2918622013087,
118.231548240752)) ;
#160957 = CARTESIAN_POINT('Ctrl Pts',(-14.2989559059233,-13.2918623086419,
118.207317211779)) ;
#160958 = CARTESIAN_POINT('Ctrl Pts',(-14.372759753517,-13.2918624159751,
118.183086182806)) ;
#160959 = CARTESIAN_POINT('Ctrl Pts',(-14.3962350846086,-13.2819569552054,
118.25458825149)) ;
#160960 = CARTESIAN_POINT('Ctrl Pts',(-14.4197104157001,-13.2720514944356,
118.326090320173)) ;
#160961 = CARTESIAN_POINT('Ctrl Pts',(-14.3459065681064,-13.2720513871025,
118.350321349146)) ;
#160962 = CARTESIAN_POINT('Ctrl Pts',(-14.2721027205127,-13.2720512797693,
118.37455237812)) ;
#160963 = CARTESIAN_POINT('Ctrl Pts',(-14.2486273894212,-13.281956740539,
118.303050309436)) ;
#160964 = CARTESIAN_POINT('Ctrl Pts',(-14.2583346166308,-13.573019683806,
118.297166121252)) ;
#160965 = CARTESIAN_POINT('Ctrl Pts',(-14.234880205577,-13.5626188486144,
118.225727771601)) ;
#160966 = CARTESIAN_POINT('Ctrl Pts',(-14.3086840441726,-13.5626189543087,
118.201496715222)) ;
#160967 = CARTESIAN_POINT('Ctrl Pts',(-14.3824878827682,-13.5626190600031,
118.177265658842)) ;
#160968 = CARTESIAN_POINT('Ctrl Pts',(-14.405942293822,-13.5730198951947,
118.248704008492)) ;
#160969 = CARTESIAN_POINT('Ctrl Pts',(-14.4293967048758,-13.5834207303863,
118.320142358142)) ;
#160970 = CARTESIAN_POINT('Ctrl Pts',(-14.3555928662802,-13.583420624692,
118.344373414522)) ;
#160971 = CARTESIAN_POINT('Ctrl Pts',(-14.2817890276846,-13.5834205189976,
118.368604470902)) ;
#160972 = CARTESIAN_POINT('Ctrl Pts',(-14.2583346166308,-13.573019683806,
118.297166121252)) ;
#160973 = CARTESIAN_POINT('Ctrl Pts',(-14.2439797697,-13.8532505028034,118.217957846964)) ;
#160974 = CARTESIAN_POINT('Ctrl Pts',(-14.222226824094,-13.823269355178,118.151701886488)) ;
#160975 = CARTESIAN_POINT('Ctrl Pts',(-14.2960306544012,-13.823269450611,
118.127470804863)) ;
#160976 = CARTESIAN_POINT('Ctrl Pts',(-14.3698344847084,-13.8232695460439,
118.103239723238)) ;
#160977 = CARTESIAN_POINT('Ctrl Pts',(-14.3915874303144,-13.8532506936693,
118.169495683714)) ;
#160978 = CARTESIAN_POINT('Ctrl Pts',(-14.4133403759204,-13.8832318412947,
118.23575164419)) ;
#160979 = CARTESIAN_POINT('Ctrl Pts',(-14.3395365456132,-13.8832317458617,
118.259982725815)) ;
#160980 = CARTESIAN_POINT('Ctrl Pts',(-14.265732715306,-13.8832316504288,
118.28421380744)) ;
#160981 = CARTESIAN_POINT('Ctrl Pts',(-14.2439797697,-13.8532505028034,118.217957846964)) ;
#160982 = CARTESIAN_POINT('Ctrl Pts',(-14.2073259241701,-14.1021597581384,
118.070845549194)) ;
#160983 = CARTESIAN_POINT('Ctrl Pts',(-14.1888334456528,-14.0547556097992,
118.014520445326)) ;
#160984 = CARTESIAN_POINT('Ctrl Pts',(-14.262637269227,-14.0547556877835,
117.990289343193)) ;
#160985 = CARTESIAN_POINT('Ctrl Pts',(-14.3364410928012,-14.0547557657678,
117.96605824106)) ;
#160986 = CARTESIAN_POINT('Ctrl Pts',(-14.3549335713185,-14.102159914107,
118.022383344929)) ;
#160987 = CARTESIAN_POINT('Ctrl Pts',(-14.3734260498358,-14.1495640624461,
118.078708448797)) ;
#160988 = CARTESIAN_POINT('Ctrl Pts',(-14.2996222262616,-14.1495639844619,
118.10293955093)) ;
#160989 = CARTESIAN_POINT('Ctrl Pts',(-14.2258184026873,-14.1495639064776,
118.127170653063)) ;
#160990 = CARTESIAN_POINT('Ctrl Pts',(-14.2073259241701,-14.1021597581384,
118.070845549194)) ;
#160991 = CARTESIAN_POINT('Ctrl Pts',(-14.1518319080389,-14.3018608409922,
117.866383830764)) ;
#160992 = CARTESIAN_POINT('Ctrl Pts',(-14.1379194094146,-14.240442969134,
117.824008606587)) ;
#160993 = CARTESIAN_POINT('Ctrl Pts',(-14.2117232283738,-14.2404430248273,
117.799777490397)) ;
#160994 = CARTESIAN_POINT('Ctrl Pts',(-14.285527047333,-14.2404430805207,
117.775546374208)) ;
#160995 = CARTESIAN_POINT('Ctrl Pts',(-14.2994395459573,-14.3018609523788,
117.817921598386)) ;
#160996 = CARTESIAN_POINT('Ctrl Pts',(-14.3133520445816,-14.3632788242369,
117.860296822564)) ;
#160997 = CARTESIAN_POINT('Ctrl Pts',(-14.2395482256223,-14.3632787685436,
117.884527938753)) ;
#160998 = CARTESIAN_POINT('Ctrl Pts',(-14.1657444066631,-14.3632787128503,
117.908759054942)) ;
#160999 = CARTESIAN_POINT('Ctrl Pts',(-14.1518319080389,-14.3018608409922,
117.866383830764)) ;
#161000 = CARTESIAN_POINT('Ctrl Pts',(-14.0821691837154,-14.4384983198451,
117.618753194085)) ;
#161001 = CARTESIAN_POINT('Ctrl Pts',(-14.0738329886517,-14.3674483770308,
117.593362490715)) ;
#161002 = CARTESIAN_POINT('Ctrl Pts',(-14.147636805446,-14.3674484079295,
117.569131367932)) ;
#161003 = CARTESIAN_POINT('Ctrl Pts',(-14.2214406222404,-14.3674484388281,
117.544900245149)) ;
#161004 = CARTESIAN_POINT('Ctrl Pts',(-14.2297768173042,-14.4384983816424,
117.570290948519)) ;
#161005 = CARTESIAN_POINT('Ctrl Pts',(-14.2381130123679,-14.5095483244567,
117.59568165189)) ;
#161006 = CARTESIAN_POINT('Ctrl Pts',(-14.1643091955736,-14.509548293558,
117.619912774673)) ;
#161007 = CARTESIAN_POINT('Ctrl Pts',(-14.0905053787792,-14.5095482626594,
117.644143897456)) ;
#161008 = CARTESIAN_POINT('Ctrl Pts',(-14.0821691837154,-14.4384983198451,
117.618753194085)) ;
#161009 = CARTESIAN_POINT('Ctrl Pts',(-14.0038053646086,-14.5020770602936,
117.344502812886)) ;
#161010 = CARTESIAN_POINT('Ctrl Pts',(-14.0016637496419,-14.4264807176174,
117.33797980086)) ;
#161011 = CARTESIAN_POINT('Ctrl Pts',(-14.0754675670679,-14.4264807240547,
117.313748680001)) ;
#161012 = CARTESIAN_POINT('Ctrl Pts',(-14.1492713844939,-14.426480730492,
117.289517559142)) ;
#161013 = CARTESIAN_POINT('Ctrl Pts',(-14.1514129994607,-14.5020770731682,
117.296040571168)) ;
#161014 = CARTESIAN_POINT('Ctrl Pts',(-14.1535546144274,-14.5776734158445,
117.302563583194)) ;
#161015 = CARTESIAN_POINT('Ctrl Pts',(-14.0797507970014,-14.5776734094072,
117.326794704053)) ;
#161016 = CARTESIAN_POINT('Ctrl Pts',(-14.0059469795754,-14.5776734029699,
117.351025824912)) ;
#161017 = CARTESIAN_POINT('Ctrl Pts',(-14.0038053646086,-14.5020770602936,
117.344502812886)) ;
#161018 = CARTESIAN_POINT('Ctrl Pts',(-13.9237302084394,-14.48777877411,117.065203884427)) ;
#161019 = CARTESIAN_POINT('Ctrl Pts',(-13.927908724164,-14.4130666847603,
117.077930970607)) ;
#161020 = CARTESIAN_POINT('Ctrl Pts',(-14.0017125440559,-14.413066670136,
117.053699857259)) ;
#161021 = CARTESIAN_POINT('Ctrl Pts',(-14.0755163639479,-14.4130666555116,
117.029468743911)) ;
#161022 = CARTESIAN_POINT('Ctrl Pts',(-14.0713378482233,-14.4877787448612,
117.01674165773)) ;
#161023 = CARTESIAN_POINT('Ctrl Pts',(-14.0671593324987,-14.5624908342109,
117.004014571549)) ;
#161024 = CARTESIAN_POINT('Ctrl Pts',(-13.9933555126067,-14.5624908488352,
117.028245684898)) ;
#161025 = CARTESIAN_POINT('Ctrl Pts',(-13.9195516927148,-14.5624908634596,
117.052476798246)) ;
#161026 = CARTESIAN_POINT('Ctrl Pts',(-13.9237302084394,-14.48777877411,117.065203884427)) ;
#161027 = CARTESIAN_POINT('Ctrl Pts',(-13.8479693987333,-14.3970097456745,
116.798993617263)) ;
#161028 = CARTESIAN_POINT('Ctrl Pts',(-13.8581774849074,-14.3285220925645,
116.830085802016)) ;
#161029 = CARTESIAN_POINT('Ctrl Pts',(-13.9319813090122,-14.3285220617789,
116.805854701499)) ;
#161030 = CARTESIAN_POINT('Ctrl Pts',(-14.005785133117,-14.3285220309933,
116.781623600983)) ;
#161031 = CARTESIAN_POINT('Ctrl Pts',(-13.995577046943,-14.3970096841033,
116.75053141623)) ;
#161032 = CARTESIAN_POINT('Ctrl Pts',(-13.9853689607689,-14.4654973372134,
116.719439231476)) ;
#161033 = CARTESIAN_POINT('Ctrl Pts',(-13.9115651366641,-14.465497367999,
116.743670331993)) ;
#161034 = CARTESIAN_POINT('Ctrl Pts',(-13.8377613125592,-14.4654973987846,
116.76790143251)) ;
#161035 = CARTESIAN_POINT('Ctrl Pts',(-13.8479693987333,-14.3970097456745,
116.798993617263)) ;
#161036 = CARTESIAN_POINT('Ctrl Pts',(-13.782799826033,-14.2362612997962,
116.5650573821)) ;
#161037 = CARTESIAN_POINT('Ctrl Pts',(-13.7983068769087,-14.1788934065685,
116.612289358194)) ;
#161038 = CARTESIAN_POINT('Ctrl Pts',(-13.8721107061698,-14.1788933656858,
116.588058273383)) ;
#161039 = CARTESIAN_POINT('Ctrl Pts',(-13.9459145354309,-14.178893324803,
116.563827188572)) ;
#161040 = CARTESIAN_POINT('Ctrl Pts',(-13.9304074845553,-14.2362612180308,
116.516595212478)) ;
#161041 = CARTESIAN_POINT('Ctrl Pts',(-13.9149004336796,-14.2936291112585,
116.469363236383)) ;
#161042 = CARTESIAN_POINT('Ctrl Pts',(-13.8410966044185,-14.2936291521412,
116.493594321195)) ;
#161043 = CARTESIAN_POINT('Ctrl Pts',(-13.7672927751574,-14.293629193024,
116.517825406006)) ;
#161044 = CARTESIAN_POINT('Ctrl Pts',(-13.782799826033,-14.2362612997962,
116.5650573821)) ;
#161045 = CARTESIAN_POINT('Ctrl Pts',(-13.733518100292,-14.0159101115065,
116.379369583749)) ;
#161046 = CARTESIAN_POINT('Ctrl Pts',(-13.7532259903904,-13.973840125215,
116.439396638124)) ;
#161047 = CARTESIAN_POINT('Ctrl Pts',(-13.8270298252004,-13.97384008191,116.415165570213)) ;
#161048 = CARTESIAN_POINT('Ctrl Pts',(-13.9008336600105,-13.973840038605,
116.390934502303)) ;
#161049 = CARTESIAN_POINT('Ctrl Pts',(-13.8811257699121,-14.0159100248966,
116.330907447928)) ;
#161050 = CARTESIAN_POINT('Ctrl Pts',(-13.8614178798137,-14.0579800111881,
116.270880393553)) ;
#161051 = CARTESIAN_POINT('Ctrl Pts',(-13.7876140450037,-14.0579800544931,
116.295111461463)) ;
#161052 = CARTESIAN_POINT('Ctrl Pts',(-13.7138102101937,-14.0579800977981,
116.319342529374)) ;
#161053 = CARTESIAN_POINT('Ctrl Pts',(-13.733518100292,-14.0159101115065,
116.379369583749)) ;
#161054 = CARTESIAN_POINT('Ctrl Pts',(-13.7047590259111,-13.7543350935969,
116.256429298379)) ;
#161055 = CARTESIAN_POINT('Ctrl Pts',(-13.7272361212088,-13.7304650573216,
116.324890904835)) ;
#161056 = CARTESIAN_POINT('Ctrl Pts',(-13.8010399606436,-13.730465015473,
116.300659851011)) ;
#161057 = CARTESIAN_POINT('Ctrl Pts',(-13.8748438000783,-13.7304649736245,
116.276428797187)) ;
#161058 = CARTESIAN_POINT('Ctrl Pts',(-13.8523667047806,-13.7543350098997,
116.20796719073)) ;
#161059 = CARTESIAN_POINT('Ctrl Pts',(-13.8298896094828,-13.778205046175,
116.139505584273)) ;
#161060 = CARTESIAN_POINT('Ctrl Pts',(-13.7560857700481,-13.7782050880236,
116.163736638098)) ;
#161061 = CARTESIAN_POINT('Ctrl Pts',(-13.6822819306134,-13.7782051298721,
116.187967691922)) ;
#161062 = CARTESIAN_POINT('Ctrl Pts',(-13.7047590259111,-13.7543350935969,
116.256429298379)) ;
#161063 = CARTESIAN_POINT('Ctrl Pts',(-13.699032750653,-13.4665595551094,
116.203361929234)) ;
#161064 = CARTESIAN_POINT('Ctrl Pts',(-13.7226811442359,-13.4627465020412,
116.275391121082)) ;
#161065 = CARTESIAN_POINT('Ctrl Pts',(-13.7964849874278,-13.4627464684725,
116.251160078701)) ;
#161066 = CARTESIAN_POINT('Ctrl Pts',(-13.8702888306197,-13.4627464349037,
116.22692903632)) ;
#161067 = CARTESIAN_POINT('Ctrl Pts',(-13.8466404370368,-13.4665594879718,
116.154899844473)) ;
#161068 = CARTESIAN_POINT('Ctrl Pts',(-13.822992043454,-13.4703725410399,
116.082870652625)) ;
#161069 = CARTESIAN_POINT('Ctrl Pts',(-13.749188200262,-13.4703725746087,
116.107101695006)) ;
#161070 = CARTESIAN_POINT('Ctrl Pts',(-13.6753843570701,-13.4703726081775,
116.131332737386)) ;
#161071 = CARTESIAN_POINT('Ctrl Pts',(-13.699032750653,-13.4665595551094,
116.203361929234)) ;
#161072 = CARTESIAN_POINT('Ctrl Pts',(-13.7175768117472,-13.1776643244991,
116.224521765399)) ;
#161073 = CARTESIAN_POINT('Ctrl Pts',(-13.7406970529322,-13.1940170948714,
116.294942290125)) ;
#161074 = CARTESIAN_POINT('Ctrl Pts',(-13.8145008983678,-13.1940170691323,
116.270711254578)) ;
#161075 = CARTESIAN_POINT('Ctrl Pts',(-13.8883047438033,-13.1940170433932,
116.246480219032)) ;
#161076 = CARTESIAN_POINT('Ctrl Pts',(-13.8651845026183,-13.1776642730209,
116.176059694306)) ;
#161077 = CARTESIAN_POINT('Ctrl Pts',(-13.8420642614332,-13.1613115026485,
116.10563916958)) ;
#161078 = CARTESIAN_POINT('Ctrl Pts',(-13.7682604159977,-13.1613115283877,
116.129870205127)) ;
#161079 = CARTESIAN_POINT('Ctrl Pts',(-13.6944565705621,-13.1613115541268,
116.154101240673)) ;
#161080 = CARTESIAN_POINT('Ctrl Pts',(-13.7175768117472,-13.1776643244991,
116.224521765399)) ;
#161081 = CARTESIAN_POINT('Ctrl Pts',(-13.7598364090687,-12.90467088677,116.317749177515)) ;
#161082 = CARTESIAN_POINT('Ctrl Pts',(-13.7807753175707,-12.9401099840166,
116.381525714689)) ;
#161083 = CARTESIAN_POINT('Ctrl Pts',(-13.8545791638935,-12.9401099680248,
116.357294681845)) ;
#161084 = CARTESIAN_POINT('Ctrl Pts',(-13.9283830102164,-12.9401099520331,
116.333063649001)) ;
#161085 = CARTESIAN_POINT('Ctrl Pts',(-13.9074441017143,-12.9046708547865,
116.269287111826)) ;
#161086 = CARTESIAN_POINT('Ctrl Pts',(-13.8865051932123,-12.86923175754,116.205510574652)) ;
#161087 = CARTESIAN_POINT('Ctrl Pts',(-13.8127013468894,-12.8692317735317,
116.229741607496)) ;
#161088 = CARTESIAN_POINT('Ctrl Pts',(-13.7388975005666,-12.8692317895235,
116.253972640341)) ;
#161089 = CARTESIAN_POINT('Ctrl Pts',(-13.7598364090687,-12.90467088677,116.317749177515)) ;
#161090 = CARTESIAN_POINT('Ctrl Pts',(-13.8234518415385,-12.6688603640825,
116.476089051097)) ;
#161091 = CARTESIAN_POINT('Ctrl Pts',(-13.8407134383904,-12.7208184006723,
116.528665090186)) ;
#161092 = CARTESIAN_POINT('Ctrl Pts',(-13.9145172844529,-12.7208183925847,
116.504434056549)) ;
#161093 = CARTESIAN_POINT('Ctrl Pts',(-13.9883211305155,-12.7208183844972,
116.480203022912)) ;
#161094 = CARTESIAN_POINT('Ctrl Pts',(-13.9710595336636,-12.6688603479075,
116.427626983823)) ;
#161095 = CARTESIAN_POINT('Ctrl Pts',(-13.9537979368117,-12.6169023113178,
116.375050944734)) ;
#161096 = CARTESIAN_POINT('Ctrl Pts',(-13.8799940907491,-12.6169023194053,
116.399281978371)) ;
#161097 = CARTESIAN_POINT('Ctrl Pts',(-13.8061902446866,-12.6169023274928,
116.423513012008)) ;
#161098 = CARTESIAN_POINT('Ctrl Pts',(-13.8234518415385,-12.6688603640825,
116.476089051097)) ;
#161099 = CARTESIAN_POINT('Ctrl Pts',(-13.9049557333608,-12.48602188738,116.688787580776)) ;
#161100 = CARTESIAN_POINT('Ctrl Pts',(-13.9172879290513,-12.5508253721629,
116.726349459155)) ;
#161101 = CARTESIAN_POINT('Ctrl Pts',(-13.9910917739091,-12.5508253699932,
116.702118421849)) ;
#161102 = CARTESIAN_POINT('Ctrl Pts',(-14.0648956187668,-12.5508253678235,
116.677887384542)) ;
#161103 = CARTESIAN_POINT('Ctrl Pts',(-14.0525634230762,-12.4860218830405,
116.640325506162)) ;
#161104 = CARTESIAN_POINT('Ctrl Pts',(-14.0402312273857,-12.4212183982575,
116.602763627783)) ;
#161105 = CARTESIAN_POINT('Ctrl Pts',(-13.966427382528,-12.4212184004273,
116.62699466509)) ;
#161106 = CARTESIAN_POINT('Ctrl Pts',(-13.8926235376703,-12.421218402597,
116.651225702396)) ;
#161107 = CARTESIAN_POINT('Ctrl Pts',(-13.9049557333608,-12.48602188738,116.688787580776)) ;
#161108 = CARTESIAN_POINT('Ctrl Pts',(-13.9989576689692,-12.3704601308902,
116.939602004027)) ;
#161109 = CARTESIAN_POINT('Ctrl Pts',(-14.0054791232532,-12.4434303508523,
116.95946530155)) ;
#161110 = CARTESIAN_POINT('Ctrl Pts',(-14.0792829667969,-12.4434303510562,
116.935234260241)) ;
#161111 = CARTESIAN_POINT('Ctrl Pts',(-14.1530868103407,-12.4434303512601,
116.911003218932)) ;
#161112 = CARTESIAN_POINT('Ctrl Pts',(-14.1465653560567,-12.370460131298,
116.891139921409)) ;
#161113 = CARTESIAN_POINT('Ctrl Pts',(-14.1400439017728,-12.297489911336,
116.871276623886)) ;
#161114 = CARTESIAN_POINT('Ctrl Pts',(-14.066240058229,-12.2974899111321,
116.895507665195)) ;
#161115 = CARTESIAN_POINT('Ctrl Pts',(-13.9924362146853,-12.2974899109282,
116.919738706504)) ;
#161116 = CARTESIAN_POINT('Ctrl Pts',(-13.9989576689692,-12.3704601308902,
116.939602004027)) ;
#161117 = CARTESIAN_POINT('Ctrl Pts',(-14.0992273955684,-12.3301504850153,
117.209607062401)) ;
#161118 = CARTESIAN_POINT('Ctrl Pts',(-14.0994895791475,-12.406044193393,
117.210405631236)) ;
#161119 = CARTESIAN_POINT('Ctrl Pts',(-14.1732934218532,-12.4060441935951,
117.186174587374)) ;
#161120 = CARTESIAN_POINT('Ctrl Pts',(-14.2470972645588,-12.4060441937972,
117.161943543513)) ;
#161121 = CARTESIAN_POINT('Ctrl Pts',(-14.2468350809797,-12.3301504854195,
117.161144974677)) ;
#161122 = CARTESIAN_POINT('Ctrl Pts',(-14.2465728974006,-12.2542567770418,
117.160346405842)) ;
#161123 = CARTESIAN_POINT('Ctrl Pts',(-14.1727690546949,-12.2542567768397,
117.184577449703)) ;
#161124 = CARTESIAN_POINT('Ctrl Pts',(-14.0989652119893,-12.2542567766376,
117.208808493565)) ;
#161125 = CARTESIAN_POINT('Ctrl Pts',(-14.0992273955684,-12.3301504850153,
117.209607062401)) ;
#161126 = CARTESIAN_POINT('Ctrl Pts',(-14.1995620772837,-12.3670848663884,
117.479845083354)) ;
#161127 = CARTESIAN_POINT('Ctrl Pts',(-14.1935503460574,-12.440512077599,
117.461534319959)) ;
#161128 = CARTESIAN_POINT('Ctrl Pts',(-14.2673541883964,-12.4405120766493,
117.43730327498)) ;
#161129 = CARTESIAN_POINT('Ctrl Pts',(-14.3411580307353,-12.4405120756996,
117.413072230002)) ;
#161130 = CARTESIAN_POINT('Ctrl Pts',(-14.3471697619617,-12.367084864489,
117.431382993397)) ;
#161131 = CARTESIAN_POINT('Ctrl Pts',(-14.353181493188,-12.2936576532783,
117.449693756792)) ;
#161132 = CARTESIAN_POINT('Ctrl Pts',(-14.279377650849,-12.293657654228,117.47392480177)) ;
#161133 = CARTESIAN_POINT('Ctrl Pts',(-14.2055738085101,-12.2936576551777,
117.498155846749)) ;
#161134 = CARTESIAN_POINT('Ctrl Pts',(-14.1995620772837,-12.3670848663884,
117.479845083354)) ;
#161135 = CARTESIAN_POINT('Ctrl Pts',(-14.2945308343906,-12.4806961242678,
117.733368848111)) ;
#161136 = CARTESIAN_POINT('Ctrl Pts',(-14.2826179068284,-12.5462988180666,
117.697083992866)) ;
#161137 = CARTESIAN_POINT('Ctrl Pts',(-14.3564217497902,-12.5462988169735,
117.672852949784)) ;
#161138 = CARTESIAN_POINT('Ctrl Pts',(-14.4302255927519,-12.5462988158804,
117.648621906703)) ;
#161139 = CARTESIAN_POINT('Ctrl Pts',(-14.4421385203141,-12.4806961220815,
117.684906761948)) ;
#161140 = CARTESIAN_POINT('Ctrl Pts',(-14.4540514478763,-12.4150934282827,
117.721191617193)) ;
#161141 = CARTESIAN_POINT('Ctrl Pts',(-14.3802476049145,-12.4150934293758,
117.745422660274)) ;
#161142 = CARTESIAN_POINT('Ctrl Pts',(-14.3064437619527,-12.415093430469,
117.769653703356)) ;
#161143 = CARTESIAN_POINT('Ctrl Pts',(-14.2945308343906,-12.4806961242678,
117.733368848111)) ;
#161144 = CARTESIAN_POINT('Ctrl Pts',(-14.3760228392886,-12.659847054779,
117.946296624332)) ;
#161145 = CARTESIAN_POINT('Ctrl Pts',(-14.3591324954954,-12.7130362017687,
117.894851362404)) ;
#161146 = CARTESIAN_POINT('Ctrl Pts',(-14.4329363392067,-12.7130362022566,
117.870620321606)) ;
#161147 = CARTESIAN_POINT('Ctrl Pts',(-14.5067401829181,-12.7130362027444,
117.846389280807)) ;
#161148 = CARTESIAN_POINT('Ctrl Pts',(-14.5236305267113,-12.6598470557547,
117.897834542735)) ;
#161149 = CARTESIAN_POINT('Ctrl Pts',(-14.5405208705045,-12.606657908765,
117.949279804662)) ;
#161150 = CARTESIAN_POINT('Ctrl Pts',(-14.4667170267932,-12.6066579082772,
117.973510845461)) ;
#161151 = CARTESIAN_POINT('Ctrl Pts',(-14.3929131830819,-12.6066579077893,
117.997741886259)) ;
#161152 = CARTESIAN_POINT('Ctrl Pts',(-14.3760228392886,-12.659847054779,
117.946296624332)) ;
#161153 = CARTESIAN_POINT('Ctrl Pts',(-14.4406901314542,-12.8944266812495,
118.107719161995)) ;
#161154 = CARTESIAN_POINT('Ctrl Pts',(-14.4199951352374,-12.9313139586903,
118.044685542764)) ;
#161155 = CARTESIAN_POINT('Ctrl Pts',(-14.4937989797123,-12.9313139638645,
118.020454504291)) ;
#161156 = CARTESIAN_POINT('Ctrl Pts',(-14.5676028241872,-12.9313139690387,
117.996223465819)) ;
#161157 = CARTESIAN_POINT('Ctrl Pts',(-14.5882978204039,-12.8944266915978,
118.05925708505)) ;
#161158 = CARTESIAN_POINT('Ctrl Pts',(-14.6089928166207,-12.8575394141569,
118.122290704281)) ;
#161159 = CARTESIAN_POINT('Ctrl Pts',(-14.5351889721458,-12.8575394089827,
118.146521742754)) ;
#161160 = CARTESIAN_POINT('Ctrl Pts',(-14.4613851276709,-12.8575394038086,
118.170752781227)) ;
#161161 = CARTESIAN_POINT('Ctrl Pts',(-14.4406901314542,-12.8944266812495,
118.107719161995)) ;
#161162 = CARTESIAN_POINT('Ctrl Pts',(-14.4837690484985,-13.1656332510844,
118.203535687924)) ;
#161163 = CARTESIAN_POINT('Ctrl Pts',(-14.4607685127247,-13.183637429578,
118.13347976731)) ;
#161164 = CARTESIAN_POINT('Ctrl Pts',(-14.5345723571586,-13.1836374410536,
118.109248728713)) ;
#161165 = CARTESIAN_POINT('Ctrl Pts',(-14.6083762015924,-13.1836374525291,
118.085017690115)) ;
#161166 = CARTESIAN_POINT('Ctrl Pts',(-14.6313767373662,-13.1656332740355,
118.155073610728)) ;
#161167 = CARTESIAN_POINT('Ctrl Pts',(-14.65437727314,-13.1476290955419,118.225129531342)) ;
#161168 = CARTESIAN_POINT('Ctrl Pts',(-14.5805734287061,-13.1476290840664,
118.24936056994)) ;
#161169 = CARTESIAN_POINT('Ctrl Pts',(-14.5067695842722,-13.1476290725908,
118.273591608538)) ;
#161170 = CARTESIAN_POINT('Ctrl Pts',(-14.4837690484985,-13.1656332510844,
118.203535687924)) ;
#161171 = CARTESIAN_POINT('Ctrl Pts',(-14.5033674776862,-13.455130793988,
118.227791066086)) ;
#161172 = CARTESIAN_POINT('Ctrl Pts',(-14.479698496056,-13.4529475727115,
118.155699167379)) ;
#161173 = CARTESIAN_POINT('Ctrl Pts',(-14.5535023394862,-13.452947591497,
118.131468125724)) ;
#161174 = CARTESIAN_POINT('Ctrl Pts',(-14.6273061829163,-13.4529476102826,
118.107237084069)) ;
#161175 = CARTESIAN_POINT('Ctrl Pts',(-14.6509751645465,-13.4551308315591,
118.179328982776)) ;
#161176 = CARTESIAN_POINT('Ctrl Pts',(-14.6746441461766,-13.4573140528355,
118.251420881482)) ;
#161177 = CARTESIAN_POINT('Ctrl Pts',(-14.6008403027464,-13.45731403405,118.275651923137)) ;
#161178 = CARTESIAN_POINT('Ctrl Pts',(-14.5270364593163,-13.4573140152645,
118.299882964792)) ;
#161179 = CARTESIAN_POINT('Ctrl Pts',(-14.5033674776862,-13.455130793988,
118.227791066086)) ;
#161180 = CARTESIAN_POINT('Ctrl Pts',(-14.4986092754277,-13.7427936624919,
118.177758141915)) ;
#161181 = CARTESIAN_POINT('Ctrl Pts',(-14.4759736082191,-13.7205220170914,
118.108813552378)) ;
#161182 = CARTESIAN_POINT('Ctrl Pts',(-14.549777449295,-13.7205220434154,
118.084582503552)) ;
#161183 = CARTESIAN_POINT('Ctrl Pts',(-14.6235812903709,-13.7205220697394,
118.060351454727)) ;
#161184 = CARTESIAN_POINT('Ctrl Pts',(-14.6462169575795,-13.7427937151399,
118.129296044264)) ;
#161185 = CARTESIAN_POINT('Ctrl Pts',(-14.6688526247881,-13.7650653605404,
118.198240633801)) ;
#161186 = CARTESIAN_POINT('Ctrl Pts',(-14.5950487837123,-13.7650653342164,
118.222471682627)) ;
#161187 = CARTESIAN_POINT('Ctrl Pts',(-14.5212449426364,-13.7650653078924,
118.246702731452)) ;
#161188 = CARTESIAN_POINT('Ctrl Pts',(-14.4986092754277,-13.7427936624919,
118.177758141915)) ;
#161189 = CARTESIAN_POINT('Ctrl Pts',(-14.4707221810934,-14.0059776158613,
118.057435006683)) ;
#161190 = CARTESIAN_POINT('Ctrl Pts',(-14.4507331312598,-13.9652981717702,
117.996551586788)) ;
#161191 = CARTESIAN_POINT('Ctrl Pts',(-14.5245369689501,-13.9652982015733,
117.97232052765)) ;
#161192 = CARTESIAN_POINT('Ctrl Pts',(-14.5983408066405,-13.9652982313764,
117.948089468513)) ;
#161193 = CARTESIAN_POINT('Ctrl Pts',(-14.6183298564741,-14.0059776754674,
118.008972888409)) ;
#161194 = CARTESIAN_POINT('Ctrl Pts',(-14.6383189063077,-14.0466571195585,
118.069856308304)) ;
#161195 = CARTESIAN_POINT('Ctrl Pts',(-14.5645150686173,-14.0466570897554,
118.094087367441)) ;
#161196 = CARTESIAN_POINT('Ctrl Pts',(-14.4907112309269,-14.0466570599524,
118.118318426579)) ;
#161197 = CARTESIAN_POINT('Ctrl Pts',(-14.4707221810934,-14.0059776158613,
118.057435006683)) ;
#161198 = CARTESIAN_POINT('Ctrl Pts',(-14.422360755841,-14.2279037819529,
117.874652010575)) ;
#161199 = CARTESIAN_POINT('Ctrl Pts',(-14.4064536010254,-14.1716706622332,
117.826201384463)) ;
#161200 = CARTESIAN_POINT('Ctrl Pts',(-14.4802574344402,-14.1716706921349,
117.801970312303)) ;
#161201 = CARTESIAN_POINT('Ctrl Pts',(-14.5540612678551,-14.1716707220365,
117.777739240143)) ;
#161202 = CARTESIAN_POINT('Ctrl Pts',(-14.5699684226707,-14.2279038417561,
117.826189866255)) ;
#161203 = CARTESIAN_POINT('Ctrl Pts',(-14.5858755774864,-14.2841369614758,
117.874640492367)) ;
#161204 = CARTESIAN_POINT('Ctrl Pts',(-14.5120717440715,-14.2841369315741,
117.898871564527)) ;
#161205 = CARTESIAN_POINT('Ctrl Pts',(-14.4382679106566,-14.2841369016725,
117.923102636686)) ;
#161206 = CARTESIAN_POINT('Ctrl Pts',(-14.422360755841,-14.2279037819529,
117.874652010575)) ;
#161207 = CARTESIAN_POINT('Ctrl Pts',(-14.3575106947756,-14.3919406672911,
117.641551257708)) ;
#161208 = CARTESIAN_POINT('Ctrl Pts',(-14.3468444592662,-14.3241730854154,
117.609063626374)) ;
#161209 = CARTESIAN_POINT('Ctrl Pts',(-14.4206482878016,-14.3241731099825,
117.584832539352)) ;
#161210 = CARTESIAN_POINT('Ctrl Pts',(-14.494452116337,-14.3241731345496,
117.560601452331)) ;
#161211 = CARTESIAN_POINT('Ctrl Pts',(-14.5051183518464,-14.3919407164252,
117.593089083665)) ;
#161212 = CARTESIAN_POINT('Ctrl Pts',(-14.5157845873559,-14.4597082983009,
117.625576714999)) ;
#161213 = CARTESIAN_POINT('Ctrl Pts',(-14.4419807588204,-14.4597082737338,
117.649807802021)) ;
#161214 = CARTESIAN_POINT('Ctrl Pts',(-14.368176930285,-14.4597082491667,
117.674038889043)) ;
#161215 = CARTESIAN_POINT('Ctrl Pts',(-14.3575106947756,-14.3919406672911,
117.641551257708)) ;
#161216 = CARTESIAN_POINT('Ctrl Pts',(-14.2822303298045,-14.4855253459423,
117.376890300863)) ;
#161217 = CARTESIAN_POINT('Ctrl Pts',(-14.2775365285705,-14.4111261442654,
117.36259374083)) ;
#161218 = CARTESIAN_POINT('Ctrl Pts',(-14.3513403532585,-14.4111261567896,
117.33836264209)) ;
#161219 = CARTESIAN_POINT('Ctrl Pts',(-14.4251441779466,-14.4111261693137,
117.31413154335)) ;
#161220 = CARTESIAN_POINT('Ctrl Pts',(-14.4298379791805,-14.4855253709906,
117.328428103382)) ;
#161221 = CARTESIAN_POINT('Ctrl Pts',(-14.4345317804145,-14.5599245726675,
117.342724663414)) ;
#161222 = CARTESIAN_POINT('Ctrl Pts',(-14.3607279557265,-14.5599245601434,
117.366955762154)) ;
#161223 = CARTESIAN_POINT('Ctrl Pts',(-14.2869241310384,-14.5599245476192,
117.391186860895)) ;
#161224 = CARTESIAN_POINT('Ctrl Pts',(-14.2822303298045,-14.4855253459423,
117.376890300863)) ;
#161225 = CARTESIAN_POINT('Ctrl Pts',(-14.2019505143216,-14.5029122651219,
117.09684616291)) ;
#161226 = CARTESIAN_POINT('Ctrl Pts',(-14.203589948758,-14.4271913157213,
117.101839617036)) ;
#161227 = CARTESIAN_POINT('Ctrl Pts',(-14.2773937703637,-14.4271913111352,
117.077608508907)) ;
#161228 = CARTESIAN_POINT('Ctrl Pts',(-14.3511975919692,-14.427191306549,
117.053377400778)) ;
#161229 = CARTESIAN_POINT('Ctrl Pts',(-14.3495581575327,-14.5029122559496,
117.048383946652)) ;
#161230 = CARTESIAN_POINT('Ctrl Pts',(-14.3479187230963,-14.5786332053501,
117.043390492526)) ;
#161231 = CARTESIAN_POINT('Ctrl Pts',(-14.2741149014907,-14.5786332099363,
117.067621600655)) ;
#161232 = CARTESIAN_POINT('Ctrl Pts',(-14.2003110798851,-14.5786332145224,
117.091852708784)) ;
#161233 = CARTESIAN_POINT('Ctrl Pts',(-14.2019505143216,-14.5029122651219,
117.09684616291)) ;
#161234 = CARTESIAN_POINT('Ctrl Pts',(-14.1238906002577,-14.4429567945224,
116.823764513881)) ;
#161235 = CARTESIAN_POINT('Ctrl Pts',(-14.131713252239,-14.3713125211074,
116.847591051117)) ;
#161236 = CARTESIAN_POINT('Ctrl Pts',(-14.2055170730593,-14.3713124959872,
116.823359940596)) ;
#161237 = CARTESIAN_POINT('Ctrl Pts',(-14.2793208938797,-14.371312470867,
116.799128830075)) ;
#161238 = CARTESIAN_POINT('Ctrl Pts',(-14.2714982418984,-14.4429567442819,
116.77530229284)) ;
#161239 = CARTESIAN_POINT('Ctrl Pts',(-14.2636755899171,-14.5146010176969,
116.751475755604)) ;
#161240 = CARTESIAN_POINT('Ctrl Pts',(-14.1898717690967,-14.5146010428171,
116.775706866125)) ;
#161241 = CARTESIAN_POINT('Ctrl Pts',(-14.1160679482764,-14.5146010679373,
116.799937976645)) ;
#161242 = CARTESIAN_POINT('Ctrl Pts',(-14.1238906002577,-14.4429567945224,
116.823764513881)) ;
#161243 = CARTESIAN_POINT('Ctrl Pts',(-14.0534400115056,-14.3088313127917,
116.573580387455)) ;
#161244 = CARTESIAN_POINT('Ctrl Pts',(-14.0669293704049,-14.2464468463962,
116.614666799803)) ;
#161245 = CARTESIAN_POINT('Ctrl Pts',(-14.1407331920325,-14.2464467981566,
116.590435691741)) ;
#161246 = CARTESIAN_POINT('Ctrl Pts',(-14.2145370136601,-14.2464467499169,
116.566204583679)) ;
#161247 = CARTESIAN_POINT('Ctrl Pts',(-14.2010476547608,-14.3088312163124,
116.525118171332)) ;
#161248 = CARTESIAN_POINT('Ctrl Pts',(-14.1875582958615,-14.3712156827079,
116.484031758984)) ;
#161249 = CARTESIAN_POINT('Ctrl Pts',(-14.1137544742339,-14.3712157309476,
116.508262867046)) ;
#161250 = CARTESIAN_POINT('Ctrl Pts',(-14.0399506526063,-14.3712157791872,
116.532493975107)) ;
#161251 = CARTESIAN_POINT('Ctrl Pts',(-14.0534400115056,-14.3088313127917,
116.573580387455)) ;
#161252 = CARTESIAN_POINT('Ctrl Pts',(-13.9973344587926,-14.1118280044828,
116.36732016952)) ;
#161253 = CARTESIAN_POINT('Ctrl Pts',(-14.0154923901431,-14.0631071534286,
116.422626300394)) ;
#161254 = CARTESIAN_POINT('Ctrl Pts',(-14.0892962154004,-14.0631070839309,
116.398395203387)) ;
#161255 = CARTESIAN_POINT('Ctrl Pts',(-14.1631000406576,-14.0631070144332,
116.374164106381)) ;
#161256 = CARTESIAN_POINT('Ctrl Pts',(-14.1449421093071,-14.1118278654874,
116.318857975507)) ;
#161257 = CARTESIAN_POINT('Ctrl Pts',(-14.1267841779565,-14.1605487165416,
116.263551844633)) ;
#161258 = CARTESIAN_POINT('Ctrl Pts',(-14.0529803526993,-14.1605487860393,
116.28778294164)) ;
#161259 = CARTESIAN_POINT('Ctrl Pts',(-13.979176527442,-14.160548855537,116.312014038646)) ;
#161260 = CARTESIAN_POINT('Ctrl Pts',(-13.9973344587926,-14.1118280044828,
116.36732016952)) ;
#161261 = CARTESIAN_POINT('Ctrl Pts',(-13.9596840563562,-13.8633524569287,
116.216996890361)) ;
#161262 = CARTESIAN_POINT('Ctrl Pts',(-13.9812347707687,-13.8319077248758,
116.282636891145)) ;
#161263 = CARTESIAN_POINT('Ctrl Pts',(-14.055038601653,-13.8319076363894,
116.258405811277)) ;
#161264 = CARTESIAN_POINT('Ctrl Pts',(-14.1288424325373,-13.8319075479029,
116.23417473141)) ;
#161265 = CARTESIAN_POINT('Ctrl Pts',(-14.1072917181249,-13.8633522799557,
116.168534730626)) ;
#161266 = CARTESIAN_POINT('Ctrl Pts',(-14.0857410037124,-13.8947970120086,
116.102894729843)) ;
#161267 = CARTESIAN_POINT('Ctrl Pts',(-14.0119371728281,-13.894797100495,
116.12712580971)) ;
#161268 = CARTESIAN_POINT('Ctrl Pts',(-13.9381333419438,-13.8947971889815,
116.151356889577)) ;
#161269 = CARTESIAN_POINT('Ctrl Pts',(-13.9596840563562,-13.8633524569287,
116.216996890361)) ;
#161270 = CARTESIAN_POINT('Ctrl Pts',(-13.9444872281656,-13.5856086171591,
116.135434675017)) ;
#161271 = CARTESIAN_POINT('Ctrl Pts',(-13.967860187308,-13.5735093381459,
116.206624939297)) ;
#161272 = CARTESIAN_POINT('Ctrl Pts',(-14.0416640258029,-13.5735092387167,
116.18239388261)) ;
#161273 = CARTESIAN_POINT('Ctrl Pts',(-14.1154678642979,-13.5735091392875,
116.158162825924)) ;
#161274 = CARTESIAN_POINT('Ctrl Pts',(-14.0920949051554,-13.5856084183006,
116.086972561643)) ;
#161275 = CARTESIAN_POINT('Ctrl Pts',(-14.068721946013,-13.5977076973138,
116.015782297363)) ;
#161276 = CARTESIAN_POINT('Ctrl Pts',(-13.9949181075181,-13.597707796743,
116.04001335405)) ;
#161277 = CARTESIAN_POINT('Ctrl Pts',(-13.9211142690232,-13.5977078961722,
116.064244410736)) ;
#161278 = CARTESIAN_POINT('Ctrl Pts',(-13.9444872281656,-13.5856086171591,
116.135434675017)) ;
#161279 = CARTESIAN_POINT('Ctrl Pts',(-13.9531206776375,-13.29429050433,116.126236655127)) ;
#161280 = CARTESIAN_POINT('Ctrl Pts',(-13.9766595960887,-13.3025120940468,
116.197932404757)) ;
#161281 = CARTESIAN_POINT('Ctrl Pts',(-14.0504634431248,-13.3025119902988,
116.173701374085)) ;
#161282 = CARTESIAN_POINT('Ctrl Pts',(-14.1242672901609,-13.3025118865508,
116.149470343414)) ;
#161283 = CARTESIAN_POINT('Ctrl Pts',(-14.1007283717097,-13.294290296834,
116.077774593784)) ;
#161284 = CARTESIAN_POINT('Ctrl Pts',(-14.0771894532585,-13.2860687071171,
116.006078844155)) ;
#161285 = CARTESIAN_POINT('Ctrl Pts',(-14.0033856062224,-13.2860688108651,
116.030309874826)) ;
#161286 = CARTESIAN_POINT('Ctrl Pts',(-13.9295817591863,-13.2860689146131,
116.054540905498)) ;
#161287 = CARTESIAN_POINT('Ctrl Pts',(-13.9531206776375,-13.29429050433,116.126236655127)) ;
#161288 = CARTESIAN_POINT('Ctrl Pts',(-13.9859156053883,-13.0122145331766,
116.19068657179)) ;
#161289 = CARTESIAN_POINT('Ctrl Pts',(-14.0079327694877,-13.0401416634717,
116.257747303244)) ;
#161290 = CARTESIAN_POINT('Ctrl Pts',(-14.0817366252876,-13.0401415643198,
116.233516299266)) ;
#161291 = CARTESIAN_POINT('Ctrl Pts',(-14.1555404810876,-13.0401414651678,
116.209285295287)) ;
#161292 = CARTESIAN_POINT('Ctrl Pts',(-14.1335233169882,-13.0122143348728,
116.142224563833)) ;
#161293 = CARTESIAN_POINT('Ctrl Pts',(-14.1115061528888,-12.9842872045777,
116.075163832378)) ;
#161294 = CARTESIAN_POINT('Ctrl Pts',(-14.0377022970889,-12.9842873037296,
116.099394836357)) ;
#161295 = CARTESIAN_POINT('Ctrl Pts',(-13.963898441289,-12.9842874028816,
116.123625840335)) ;
#161296 = CARTESIAN_POINT('Ctrl Pts',(-13.9859156053883,-13.0122145331766,
116.19068657179)) ;
#161297 = CARTESIAN_POINT('Ctrl Pts',(-14.0414265852797,-12.7583429519339,
116.324206721183)) ;
#161298 = CARTESIAN_POINT('Ctrl Pts',(-14.0603365111948,-12.8040356004971,
116.381803306508)) ;
#161299 = CARTESIAN_POINT('Ctrl Pts',(-14.1341403750837,-12.8040355143443,
116.357572327168)) ;
#161300 = CARTESIAN_POINT('Ctrl Pts',(-14.2079442389726,-12.8040354281915,
116.333341347827)) ;
#161301 = CARTESIAN_POINT('Ctrl Pts',(-14.1890343130574,-12.7583427796283,
116.275744762501)) ;
#161302 = CARTESIAN_POINT('Ctrl Pts',(-14.1701243871423,-12.7126501310651,
116.218148177176)) ;
#161303 = CARTESIAN_POINT('Ctrl Pts',(-14.0963205232534,-12.7126502172179,
116.242379156517)) ;
#161304 = CARTESIAN_POINT('Ctrl Pts',(-14.0225166593645,-12.7126503033707,
116.266610135857)) ;
#161305 = CARTESIAN_POINT('Ctrl Pts',(-14.0414265852797,-12.7583429519339,
116.324206721183)) ;
#161306 = CARTESIAN_POINT('Ctrl Pts',(-14.1163566701285,-12.5522896132778,
116.516904433369)) ;
#161307 = CARTESIAN_POINT('Ctrl Pts',(-14.1307984259442,-12.6124359304363,
116.560891693508)) ;
#161308 = CARTESIAN_POINT('Ctrl Pts',(-14.2046022962474,-12.6124358649261,
116.536660733704)) ;
#161309 = CARTESIAN_POINT('Ctrl Pts',(-14.2784061665505,-12.6124357994159,
116.5124297739)) ;
#161310 = CARTESIAN_POINT('Ctrl Pts',(-14.2639644107349,-12.5522894822574,
116.468442513761)) ;
#161311 = CARTESIAN_POINT('Ctrl Pts',(-14.2495226549191,-12.4921431650989,
116.424455253623)) ;
#161312 = CARTESIAN_POINT('Ctrl Pts',(-14.175718784616,-12.4921432306091,
116.448686213427)) ;
#161313 = CARTESIAN_POINT('Ctrl Pts',(-14.1019149143128,-12.4921432961193,
116.47291717323)) ;
#161314 = CARTESIAN_POINT('Ctrl Pts',(-14.1163566701285,-12.5522896132778,
116.516904433369)) ;
#161315 = CARTESIAN_POINT('Ctrl Pts',(-14.2054208500919,-12.4090180636989,
116.75287655481)) ;
#161316 = CARTESIAN_POINT('Ctrl Pts',(-14.2143962414437,-12.4792560944464,
116.78021415077)) ;
#161317 = CARTESIAN_POINT('Ctrl Pts',(-14.2882001159623,-12.4792560544209,
116.755983203806)) ;
#161318 = CARTESIAN_POINT('Ctrl Pts',(-14.3620039904809,-12.4792560143955,
116.731752256842)) ;
#161319 = CARTESIAN_POINT('Ctrl Pts',(-14.3530285991291,-12.409017983648,
116.704414660881)) ;
#161320 = CARTESIAN_POINT('Ctrl Pts',(-14.3440532077773,-12.3387799529005,
116.67707706492)) ;
#161321 = CARTESIAN_POINT('Ctrl Pts',(-14.2702493332587,-12.3387799929259,
116.701308011885)) ;
#161322 = CARTESIAN_POINT('Ctrl Pts',(-14.1964454587401,-12.3387800329514,
116.725538958849)) ;
#161323 = CARTESIAN_POINT('Ctrl Pts',(-14.2054208500919,-12.4090180636989,
116.75287655481)) ;
#161324 = CARTESIAN_POINT('Ctrl Pts',(-14.3041315741692,-12.3371174607651,
117.018003366661)) ;
#161325 = CARTESIAN_POINT('Ctrl Pts',(-14.306963905046,-12.4124801362831,
117.026630191551)) ;
#161326 = CARTESIAN_POINT('Ctrl Pts',(-14.3807677810887,-12.4124801245382,
117.002399249229)) ;
#161327 = CARTESIAN_POINT('Ctrl Pts',(-14.4545716571313,-12.4124801127933,
116.978168306907)) ;
#161328 = CARTESIAN_POINT('Ctrl Pts',(-14.4517393262545,-12.3371174372753,
116.969541482016)) ;
#161329 = CARTESIAN_POINT('Ctrl Pts',(-14.4489069953776,-12.2617547617574,
116.960914657126)) ;
#161330 = CARTESIAN_POINT('Ctrl Pts',(-14.375103119335,-12.2617547735023,
116.985145599448)) ;
#161331 = CARTESIAN_POINT('Ctrl Pts',(-14.3012992432923,-12.2617547852472,
117.009376541771)) ;
#161332 = CARTESIAN_POINT('Ctrl Pts',(-14.3041315741692,-12.3371174607651,
117.018003366661)) ;
#161333 = CARTESIAN_POINT('Ctrl Pts',(-14.4053499510961,-12.3428658905722,
117.290874128105)) ;
#161334 = CARTESIAN_POINT('Ctrl Pts',(-14.40185271617,-12.4179397314328,117.280222116772)) ;
#161335 = CARTESIAN_POINT('Ctrl Pts',(-14.4756565910603,-12.4179397474679,
117.25599117094)) ;
#161336 = CARTESIAN_POINT('Ctrl Pts',(-14.5494604659506,-12.4179397635031,
117.231760225108)) ;
#161337 = CARTESIAN_POINT('Ctrl Pts',(-14.5529577008767,-12.3428659226425,
117.242412236441)) ;
#161338 = CARTESIAN_POINT('Ctrl Pts',(-14.5564549358029,-12.267792081782,
117.253064247774)) ;
#161339 = CARTESIAN_POINT('Ctrl Pts',(-14.4826510609126,-12.2677920657468,
117.277295193606)) ;
#161340 = CARTESIAN_POINT('Ctrl Pts',(-14.4088471860223,-12.2677920497116,
117.301526139438)) ;
#161341 = CARTESIAN_POINT('Ctrl Pts',(-14.4053499510961,-12.3428658905722,
117.290874128105)) ;
#161342 = CARTESIAN_POINT('Ctrl Pts',(-14.5030362331871,-12.4257351119528,
117.55290734156)) ;
#161343 = CARTESIAN_POINT('Ctrl Pts',(-14.4934481825595,-12.4951358678153,
117.523703688264)) ;
#161344 = CARTESIAN_POINT('Ctrl Pts',(-14.5672520537253,-12.4951359082695,
117.499472731088)) ;
#161345 = CARTESIAN_POINT('Ctrl Pts',(-14.6410559248911,-12.4951359487237,
117.475241773911)) ;
#161346 = CARTESIAN_POINT('Ctrl Pts',(-14.6506439755188,-12.4257351928613,
117.504445427208)) ;
#161347 = CARTESIAN_POINT('Ctrl Pts',(-14.6602320261464,-12.3563344369988,
117.533649080504)) ;
#161348 = CARTESIAN_POINT('Ctrl Pts',(-14.5864281549806,-12.3563343965446,
117.557880037681)) ;
#161349 = CARTESIAN_POINT('Ctrl Pts',(-14.5126242838148,-12.3563343560904,
117.582110994857)) ;
#161350 = CARTESIAN_POINT('Ctrl Pts',(-14.5030362331871,-12.4257351119528,
117.55290734156)) ;
#161351 = CARTESIAN_POINT('Ctrl Pts',(-14.5904621270827,-12.5790185234623,
117.783826332769)) ;
#161352 = CARTESIAN_POINT('Ctrl Pts',(-14.5754876103016,-12.6378213476739,
117.738216372584)) ;
#161353 = CARTESIAN_POINT('Ctrl Pts',(-14.6492914760003,-12.6378214074388,
117.713985398756)) ;
#161354 = CARTESIAN_POINT('Ctrl Pts',(-14.7230953416989,-12.6378214672038,
117.689754424927)) ;
#161355 = CARTESIAN_POINT('Ctrl Pts',(-14.7380698584799,-12.5790186429921,
117.735364385112)) ;
#161356 = CARTESIAN_POINT('Ctrl Pts',(-14.753044375261,-12.5202158187805,
117.780974345297)) ;
#161357 = CARTESIAN_POINT('Ctrl Pts',(-14.6792405095624,-12.5202157590156,
117.805205319126)) ;
#161358 = CARTESIAN_POINT('Ctrl Pts',(-14.6054366438637,-12.5202156992507,
117.829436292955)) ;
#161359 = CARTESIAN_POINT('Ctrl Pts',(-14.5904621270827,-12.5790185234623,
117.783826332769)) ;
#161360 = CARTESIAN_POINT('Ctrl Pts',(-14.6629652552051,-12.7940406828703,
117.969008479269)) ;
#161361 = CARTESIAN_POINT('Ctrl Pts',(-14.6436437278103,-12.837920143464,
117.910158225998)) ;
#161362 = CARTESIAN_POINT('Ctrl Pts',(-14.717447586395,-12.8379202140664,
117.885927230502)) ;
#161363 = CARTESIAN_POINT('Ctrl Pts',(-14.7912514449796,-12.8379202846688,
117.861696235005)) ;
#161364 = CARTESIAN_POINT('Ctrl Pts',(-14.8105729723744,-12.7940408240752,
117.920546488276)) ;
#161365 = CARTESIAN_POINT('Ctrl Pts',(-14.8298944997692,-12.7501613634815,
117.979396741547)) ;
#161366 = CARTESIAN_POINT('Ctrl Pts',(-14.7560906411845,-12.7501612928791,
118.003627737044)) ;
#161367 = CARTESIAN_POINT('Ctrl Pts',(-14.6822867825999,-12.7501612222767,
118.02785873254)) ;
#161368 = CARTESIAN_POINT('Ctrl Pts',(-14.6629652552051,-12.7940406828703,
117.969008479269)) ;
#161369 = CARTESIAN_POINT('Ctrl Pts',(-14.7149782729242,-13.0518842131347,
118.092091883262)) ;
#161370 = CARTESIAN_POINT('Ctrl Pts',(-14.6927274213406,-13.0778272755866,
118.02431938104)) ;
#161371 = CARTESIAN_POINT('Ctrl Pts',(-14.7665312729268,-13.0778273508396,
118.000088364228)) ;
#161372 = CARTESIAN_POINT('Ctrl Pts',(-14.840335124513,-13.0778274260925,
117.975857347415)) ;
#161373 = CARTESIAN_POINT('Ctrl Pts',(-14.8625859760966,-13.0518843636406,
118.043629849637)) ;
#161374 = CARTESIAN_POINT('Ctrl Pts',(-14.8848368276802,-13.0259413011886,
118.111402351858)) ;
#161375 = CARTESIAN_POINT('Ctrl Pts',(-14.811032976094,-13.0259412259357,
118.135633368671)) ;
#161376 = CARTESIAN_POINT('Ctrl Pts',(-14.7372291245078,-13.0259411506828,
118.159864385484)) ;
#161377 = CARTESIAN_POINT('Ctrl Pts',(-14.7149782729242,-13.0518842131347,
118.092091883262)) ;
#161378 = CARTESIAN_POINT('Ctrl Pts',(-14.7443671066665,-13.3370763555055,
118.146092536195)) ;
#161379 = CARTESIAN_POINT('Ctrl Pts',(-14.7207654994872,-13.343146769627,
118.074205850219)) ;
#161380 = CARTESIAN_POINT('Ctrl Pts',(-14.7945693443435,-13.3431468412151,
118.049974812908)) ;
#161381 = CARTESIAN_POINT('Ctrl Pts',(-14.8683731891997,-13.3431469128033,
118.025743775596)) ;
#161382 = CARTESIAN_POINT('Ctrl Pts',(-14.891974796379,-13.3370764986818,
118.097630461573)) ;
#161383 = CARTESIAN_POINT('Ctrl Pts',(-14.9155764035582,-13.3310060845603,
118.16951714755)) ;
#161384 = CARTESIAN_POINT('Ctrl Pts',(-14.8417725587019,-13.3310060129721,
118.193748184861)) ;
#161385 = CARTESIAN_POINT('Ctrl Pts',(-14.7679687138457,-13.3310059413839,
118.217979222172)) ;
#161386 = CARTESIAN_POINT('Ctrl Pts',(-14.7443671066665,-13.3370763555055,
118.146092536195)) ;
#161387 = CARTESIAN_POINT('Ctrl Pts',(-14.7494764883566,-13.6270297095458,
118.126281327732)) ;
#161388 = CARTESIAN_POINT('Ctrl Pts',(-14.7262144515455,-13.6128647269904,
118.055428918166)) ;
#161389 = CARTESIAN_POINT('Ctrl Pts',(-14.8000182908552,-13.6128647900771,
118.031197863962)) ;
#161390 = CARTESIAN_POINT('Ctrl Pts',(-14.8738221301649,-13.6128648531639,
118.006966809757)) ;
#161391 = CARTESIAN_POINT('Ctrl Pts',(-14.897084166976,-13.6270298357193,
118.077819219322)) ;
#161392 = CARTESIAN_POINT('Ctrl Pts',(-14.9203462037872,-13.6411948182747,
118.148671628887)) ;
#161393 = CARTESIAN_POINT('Ctrl Pts',(-14.8465423644775,-13.6411947551879,
118.172902683092)) ;
#161394 = CARTESIAN_POINT('Ctrl Pts',(-14.7727385251678,-13.6411946921012,
118.197133737297)) ;
#161395 = CARTESIAN_POINT('Ctrl Pts',(-14.7494764883566,-13.6270297095458,
118.126281327732)) ;
#161396 = CARTESIAN_POINT('Ctrl Pts',(-14.7306708206297,-13.9038567932623,
118.033390708072)) ;
#161397 = CARTESIAN_POINT('Ctrl Pts',(-14.7094232936479,-13.8703419963818,
117.968674170216)) ;
#161398 = CARTESIAN_POINT('Ctrl Pts',(-14.7832271292031,-13.8703420447739,
117.944443104575)) ;
#161399 = CARTESIAN_POINT('Ctrl Pts',(-14.8570309647582,-13.8703420931661,
117.920212038934)) ;
#161400 = CARTESIAN_POINT('Ctrl Pts',(-14.87827849174,-13.9038568900467,117.98492857679)) ;
#161401 = CARTESIAN_POINT('Ctrl Pts',(-14.8995260187217,-13.9373716869272,
118.049645114647)) ;
#161402 = CARTESIAN_POINT('Ctrl Pts',(-14.8257221831665,-13.9373716385351,
118.073876180288)) ;
#161403 = CARTESIAN_POINT('Ctrl Pts',(-14.7519183476114,-13.9373715901429,
118.098107245928)) ;
#161404 = CARTESIAN_POINT('Ctrl Pts',(-14.7306708206297,-13.9038567932623,
118.033390708072)) ;
#161405 = CARTESIAN_POINT('Ctrl Pts',(-14.690027558541,-14.1447030861545,
117.874109045323)) ;
#161406 = CARTESIAN_POINT('Ctrl Pts',(-14.6723199395305,-14.0943210410225,
117.820174495812)) ;
#161407 = CARTESIAN_POINT('Ctrl Pts',(-14.7461237732829,-14.0943210744769,
117.79594342468)) ;
#161408 = CARTESIAN_POINT('Ctrl Pts',(-14.8199276070354,-14.0943211079313,
117.771712353549)) ;
#161409 = CARTESIAN_POINT('Ctrl Pts',(-14.8376352260459,-14.1447031530633,
117.82564690306)) ;
#161410 = CARTESIAN_POINT('Ctrl Pts',(-14.8553428450565,-14.1950851981953,
117.879581452572)) ;
#161411 = CARTESIAN_POINT('Ctrl Pts',(-14.781539011304,-14.1950851647409,
117.903812523703)) ;
#161412 = CARTESIAN_POINT('Ctrl Pts',(-14.7077351775515,-14.1950851312865,
117.928043594835)) ;
#161413 = CARTESIAN_POINT('Ctrl Pts',(-14.690027558541,-14.1447030861545,
117.874109045323)) ;
#161414 = CARTESIAN_POINT('Ctrl Pts',(-14.6316472186503,-14.332817774621,
117.660971076182)) ;
#161415 = CARTESIAN_POINT('Ctrl Pts',(-14.6187199695823,-14.2692250612684,
117.621596762065)) ;
#161416 = CARTESIAN_POINT('Ctrl Pts',(-14.6925238028212,-14.2692250813647,
117.597365689369)) ;
#161417 = CARTESIAN_POINT('Ctrl Pts',(-14.76632763606,-14.269225101461,117.573134616673)) ;
#161418 = CARTESIAN_POINT('Ctrl Pts',(-14.7792548851279,-14.3328178148136,
117.61250893079)) ;
#161419 = CARTESIAN_POINT('Ctrl Pts',(-14.7921821341959,-14.3964105281663,
117.651883244906)) ;
#161420 = CARTESIAN_POINT('Ctrl Pts',(-14.718378300957,-14.3964105080699,
117.676114317602)) ;
#161421 = CARTESIAN_POINT('Ctrl Pts',(-14.6445744677182,-14.3964104879736,
117.700345390298)) ;
#161422 = CARTESIAN_POINT('Ctrl Pts',(-14.6316472186503,-14.332817774621,
117.660971076182)) ;
#161423 = CARTESIAN_POINT('Ctrl Pts',(-14.5597455784243,-14.45646682902,117.406433016193)) ;
#161424 = CARTESIAN_POINT('Ctrl Pts',(-14.5525544833958,-14.3841439170352,
117.384530101578)) ;
#161425 = CARTESIAN_POINT('Ctrl Pts',(-14.6263583180638,-14.3841439249686,
117.360299033234)) ;
#161426 = CARTESIAN_POINT('Ctrl Pts',(-14.7001621527318,-14.3841439329019,
117.336067964891)) ;
#161427 = CARTESIAN_POINT('Ctrl Pts',(-14.7073532477603,-14.4564668448866,
117.357970879507)) ;
#161428 = CARTESIAN_POINT('Ctrl Pts',(-14.7145443427888,-14.5287897568713,
117.379873794122)) ;
#161429 = CARTESIAN_POINT('Ctrl Pts',(-14.6407405081208,-14.528789748938,
117.404104862465)) ;
#161430 = CARTESIAN_POINT('Ctrl Pts',(-14.5669366734528,-14.5287897410047,
117.428335930808)) ;
#161431 = CARTESIAN_POINT('Ctrl Pts',(-14.5597455784243,-14.45646682902,117.406433016193)) ;
#161432 = CARTESIAN_POINT('Ctrl Pts',(-14.4807629365922,-14.5053560860543,
117.130424369544)) ;
#161433 = CARTESIAN_POINT('Ctrl Pts',(-14.4798092245676,-14.4295100560536,
117.127519517009)) ;
#161434 = CARTESIAN_POINT('Ctrl Pts',(-14.5536130613439,-14.4295100560703,
117.103288455087)) ;
#161435 = CARTESIAN_POINT('Ctrl Pts',(-14.6274168981201,-14.429510056087,
117.079057393166)) ;
#161436 = CARTESIAN_POINT('Ctrl Pts',(-14.6283706101447,-14.5053560860877,
117.081962245701)) ;
#161437 = CARTESIAN_POINT('Ctrl Pts',(-14.6293243221693,-14.5812021160883,
117.084867098236)) ;
#161438 = CARTESIAN_POINT('Ctrl Pts',(-14.5555204853931,-14.5812021160717,
117.109098160158)) ;
#161439 = CARTESIAN_POINT('Ctrl Pts',(-14.4817166486168,-14.581202116055,
117.133329222079)) ;
#161440 = CARTESIAN_POINT('Ctrl Pts',(-14.4807629365922,-14.5053560860543,
117.130424369544)) ;
#161441 = CARTESIAN_POINT('Ctrl Pts',(-14.4006764355962,-14.4762759602464,
116.850932976369)) ;
#161442 = CARTESIAN_POINT('Ctrl Pts',(-14.4060492486959,-14.4023454887856,
116.867297698424)) ;
#161443 = CARTESIAN_POINT('Ctrl Pts',(-14.4798530881773,-14.4023454850915,
116.843066644742)) ;
#161444 = CARTESIAN_POINT('Ctrl Pts',(-14.5536569276586,-14.4023454813974,
116.818835591059)) ;
#161445 = CARTESIAN_POINT('Ctrl Pts',(-14.5482841145589,-14.4762759528582,
116.802470869005)) ;
#161446 = CARTESIAN_POINT('Ctrl Pts',(-14.5429113014591,-14.5502064243191,
116.78610614695)) ;
#161447 = CARTESIAN_POINT('Ctrl Pts',(-14.4691074619778,-14.5502064280132,
116.810337200632)) ;
#161448 = CARTESIAN_POINT('Ctrl Pts',(-14.3953036224965,-14.5502064317073,
116.834568254315)) ;
#161449 = CARTESIAN_POINT('Ctrl Pts',(-14.4006764355962,-14.4762759602464,
116.850932976369)) ;
#161450 = CARTESIAN_POINT('Ctrl Pts',(-14.3265390078925,-14.3712943997113,
116.589686458049)) ;
#161451 = CARTESIAN_POINT('Ctrl Pts',(-14.3378299538683,-14.3045830394382,
116.624076857841)) ;
#161452 = CARTESIAN_POINT('Ctrl Pts',(-14.4116337954084,-14.3045830356426,
116.599845810429)) ;
#161453 = CARTESIAN_POINT('Ctrl Pts',(-14.4854376369484,-14.3045830318471,
116.575614763017)) ;
#161454 = CARTESIAN_POINT('Ctrl Pts',(-14.4741466909726,-14.3712943921201,
116.541224363225)) ;
#161455 = CARTESIAN_POINT('Ctrl Pts',(-14.4628557449968,-14.4380057523932,
116.506833963433)) ;
#161456 = CARTESIAN_POINT('Ctrl Pts',(-14.3890519034567,-14.4380057561888,
116.531065010845)) ;
#161457 = CARTESIAN_POINT('Ctrl Pts',(-14.3152480619167,-14.4380057599843,
116.555296058257)) ;
#161458 = CARTESIAN_POINT('Ctrl Pts',(-14.3265390078925,-14.3712943997113,
116.589686458049)) ;
#161459 = CARTESIAN_POINT('Ctrl Pts',(-14.2642291252365,-14.1990455522355,
116.364581017991)) ;
#161460 = CARTESIAN_POINT('Ctrl Pts',(-14.2806187025119,-14.1442616573657,
116.414501025975)) ;
#161461 = CARTESIAN_POINT('Ctrl Pts',(-14.3544225454209,-14.1442616552479,
116.390269982733)) ;
#161462 = CARTESIAN_POINT('Ctrl Pts',(-14.4282263883299,-14.1442616531301,
116.36603893949)) ;
#161463 = CARTESIAN_POINT('Ctrl Pts',(-14.4118368110544,-14.1990455479999,
116.316118931507)) ;
#161464 = CARTESIAN_POINT('Ctrl Pts',(-14.3954472337789,-14.2538294428697,
116.266198923523)) ;
#161465 = CARTESIAN_POINT('Ctrl Pts',(-14.3216433908699,-14.2538294449875,
116.290429966766)) ;
#161466 = CARTESIAN_POINT('Ctrl Pts',(-14.247839547961,-14.2538294471053,
116.314661010008)) ;
#161467 = CARTESIAN_POINT('Ctrl Pts',(-14.2642291252365,-14.1990455522355,
116.364581017991)) ;
#161468 = CARTESIAN_POINT('Ctrl Pts',(-14.2184481514674,-13.969268231171,
116.189542795207)) ;
#161469 = CARTESIAN_POINT('Ctrl Pts',(-14.2387958666726,-13.9304471194496,
116.251518652599)) ;
#161470 = CARTESIAN_POINT('Ctrl Pts',(-14.312599710417,-13.9304471207081,
116.227287611902)) ;
#161471 = CARTESIAN_POINT('Ctrl Pts',(-14.3864035541614,-13.9304471219666,
116.203056571204)) ;
#161472 = CARTESIAN_POINT('Ctrl Pts',(-14.3660558389563,-13.9692682336881,
116.141080713812)) ;
#161473 = CARTESIAN_POINT('Ctrl Pts',(-14.3457081237511,-14.0080893454095,
116.07910485642)) ;
#161474 = CARTESIAN_POINT('Ctrl Pts',(-14.2719042800067,-14.008089344151,
116.103335897118)) ;
#161475 = CARTESIAN_POINT('Ctrl Pts',(-14.1981004362623,-14.0080893428925,
116.127566937816)) ;
#161476 = CARTESIAN_POINT('Ctrl Pts',(-14.2184481514674,-13.969268231171,
116.189542795207)) ;
#161477 = CARTESIAN_POINT('Ctrl Pts',(-14.1938561787033,-13.7012052922517,
116.079239578809)) ;
#161478 = CARTESIAN_POINT('Ctrl Pts',(-14.2166839653933,-13.6810448607135,
116.148769333753)) ;
#161479 = CARTESIAN_POINT('Ctrl Pts',(-14.2904878090818,-13.6810448639026,
116.124538292885)) ;
#161480 = CARTESIAN_POINT('Ctrl Pts',(-14.3642916527704,-13.6810448670916,
116.100307252017)) ;
#161481 = CARTESIAN_POINT('Ctrl Pts',(-14.3414638660804,-13.7012052986298,
116.030777497073)) ;
#161482 = CARTESIAN_POINT('Ctrl Pts',(-14.3186360793905,-13.7213657301679,
115.961247742129)) ;
#161483 = CARTESIAN_POINT('Ctrl Pts',(-14.2448322357019,-13.7213657269789,
115.985478782997)) ;
#161484 = CARTESIAN_POINT('Ctrl Pts',(-14.1710283920134,-13.7213657237898,
116.009709823865)) ;
#161485 = CARTESIAN_POINT('Ctrl Pts',(-14.1938561787033,-13.7012052922517,
116.079239578809)) ;
#161486 = CARTESIAN_POINT('Ctrl Pts',(-14.1927076708075,-13.4115854195081,
116.040169663763)) ;
#161487 = CARTESIAN_POINT('Ctrl Pts',(-14.2163857118218,-13.4116194662379,
116.112289156201)) ;
#161488 = CARTESIAN_POINT('Ctrl Pts',(-14.2901895551865,-13.4116194689939,
116.088058114347)) ;
#161489 = CARTESIAN_POINT('Ctrl Pts',(-14.3639933985512,-13.41161947175,116.063827072493)) ;
#161490 = CARTESIAN_POINT('Ctrl Pts',(-14.3403153575369,-13.4115854250202,
115.991707580054)) ;
#161491 = CARTESIAN_POINT('Ctrl Pts',(-14.3166373165225,-13.4115513782904,
115.919588087615)) ;
#161492 = CARTESIAN_POINT('Ctrl Pts',(-14.2428334731578,-13.4115513755344,
115.94381912947)) ;
#161493 = CARTESIAN_POINT('Ctrl Pts',(-14.1690296297931,-13.4115513727784,
115.968050171324)) ;
#161494 = CARTESIAN_POINT('Ctrl Pts',(-14.1927076708075,-13.4115854195081,
116.040169663763)) ;
#161495 = CARTESIAN_POINT('Ctrl Pts',(-14.2158186831131,-13.1240520278943,
116.075200920001)) ;
#161496 = CARTESIAN_POINT('Ctrl Pts',(-14.238649448497,-13.1441635924048,
116.144739747623)) ;
#161497 = CARTESIAN_POINT('Ctrl Pts',(-14.3124532917785,-13.144163592711,
116.120508705515)) ;
#161498 = CARTESIAN_POINT('Ctrl Pts',(-14.38625713506,-13.1441635930171,116.096277663407)) ;
#161499 = CARTESIAN_POINT('Ctrl Pts',(-14.3634263696761,-13.1240520285066,
116.026738835786)) ;
#161500 = CARTESIAN_POINT('Ctrl Pts',(-14.3405956042921,-13.103940463996,
115.957200008165)) ;
#161501 = CARTESIAN_POINT('Ctrl Pts',(-14.2667917610107,-13.1039404636899,
115.981431050272)) ;
#161502 = CARTESIAN_POINT('Ctrl Pts',(-14.1929879177292,-13.1039404633837,
116.00566209238)) ;
#161503 = CARTESIAN_POINT('Ctrl Pts',(-14.2158186831131,-13.1240520278943,
116.075200920001)) ;
#161504 = CARTESIAN_POINT('Ctrl Pts',(-14.2623847117566,-12.8565945311091,
116.181543563239)) ;
#161505 = CARTESIAN_POINT('Ctrl Pts',(-14.2827318296291,-12.895411134357,
116.243517601359)) ;
#161506 = CARTESIAN_POINT('Ctrl Pts',(-14.3565356735563,-12.8954111308149,
116.219286561218)) ;
#161507 = CARTESIAN_POINT('Ctrl Pts',(-14.4303395174835,-12.8954111272728,
116.195055521077)) ;
#161508 = CARTESIAN_POINT('Ctrl Pts',(-14.409992399611,-12.8565945240249,
116.133081482957)) ;
#161509 = CARTESIAN_POINT('Ctrl Pts',(-14.3896452817385,-12.817777920777,
116.071107444837)) ;
#161510 = CARTESIAN_POINT('Ctrl Pts',(-14.3158414378113,-12.8177779243191,
116.095338484978)) ;
#161511 = CARTESIAN_POINT('Ctrl Pts',(-14.2420375938841,-12.8177779278612,
116.119569525119)) ;
#161512 = CARTESIAN_POINT('Ctrl Pts',(-14.2623847117566,-12.8565945311091,
116.181543563239)) ;
#161513 = CARTESIAN_POINT('Ctrl Pts',(-14.3295805648497,-12.6299321000607,
116.350826699486)) ;
#161514 = CARTESIAN_POINT('Ctrl Pts',(-14.345997626373,-12.6846316848106,
116.400830420177)) ;
#161515 = CARTESIAN_POINT('Ctrl Pts',(-14.4198014716913,-12.6846316781894,
116.376599384273)) ;
#161516 = CARTESIAN_POINT('Ctrl Pts',(-14.4936053170096,-12.6846316715683,
116.352368348369)) ;
#161517 = CARTESIAN_POINT('Ctrl Pts',(-14.4771882554863,-12.6299320868185,
116.302364627678)) ;
#161518 = CARTESIAN_POINT('Ctrl Pts',(-14.460771193963,-12.5752325020687,
116.252360906988)) ;
#161519 = CARTESIAN_POINT('Ctrl Pts',(-14.3869673486447,-12.5752325086898,
116.276591942892)) ;
#161520 = CARTESIAN_POINT('Ctrl Pts',(-14.3131635033265,-12.5752325153109,
116.300822978795)) ;
#161521 = CARTESIAN_POINT('Ctrl Pts',(-14.3295805648497,-12.6299321000607,
116.350826699486)) ;
#161522 = CARTESIAN_POINT('Ctrl Pts',(-14.4139535876279,-12.458754218581,
116.572235100756)) ;
#161523 = CARTESIAN_POINT('Ctrl Pts',(-14.425239560756,-12.5254858902144,
116.60661035424)) ;
#161524 = CARTESIAN_POINT('Ctrl Pts',(-14.4990434086302,-12.5254858817945,
116.582379326121)) ;
#161525 = CARTESIAN_POINT('Ctrl Pts',(-14.5728472565044,-12.5254858733746,
116.558148298002)) ;
#161526 = CARTESIAN_POINT('Ctrl Pts',(-14.5615612833762,-12.4587542017412,
116.523773044517)) ;
#161527 = CARTESIAN_POINT('Ctrl Pts',(-14.550275310248,-12.3920225301078,
116.489397791033)) ;
#161528 = CARTESIAN_POINT('Ctrl Pts',(-14.4764714623738,-12.3920225385277,
116.513628819152)) ;
#161529 = CARTESIAN_POINT('Ctrl Pts',(-14.4026676144997,-12.3920225469476,
116.537859847271)) ;
#161530 = CARTESIAN_POINT('Ctrl Pts',(-14.4139535876279,-12.458754218581,
116.572235100756)) ;
#161531 = CARTESIAN_POINT('Ctrl Pts',(-14.5094836498744,-12.3569969390507,
116.827772100287)) ;
#161532 = CARTESIAN_POINT('Ctrl Pts',(-14.5148490608815,-12.4309301429408,
116.844114276972)) ;
#161533 = CARTESIAN_POINT('Ctrl Pts',(-14.5886529115489,-12.4309301369064,
116.819883257361)) ;
#161534 = CARTESIAN_POINT('Ctrl Pts',(-14.6624567622163,-12.430930130872,
116.795652237749)) ;
#161535 = CARTESIAN_POINT('Ctrl Pts',(-14.6570913512092,-12.356996926982,
116.779310061064)) ;
#161536 = CARTESIAN_POINT('Ctrl Pts',(-14.6517259402021,-12.283063723092,
116.762967884378)) ;
#161537 = CARTESIAN_POINT('Ctrl Pts',(-14.5779220895347,-12.2830637291264,
116.787198903989)) ;
#161538 = CARTESIAN_POINT('Ctrl Pts',(-14.5041182388673,-12.2830637351607,
116.811429923601)) ;
#161539 = CARTESIAN_POINT('Ctrl Pts',(-14.5094836498744,-12.3569969390507,
116.827772100287)) ;
#161540 = CARTESIAN_POINT('Ctrl Pts',(-14.6106904064239,-12.3311725454961,
117.10048536176)) ;
#161541 = CARTESIAN_POINT('Ctrl Pts',(-14.6097327538528,-12.4070160661621,
117.097568507183)) ;
#161542 = CARTESIAN_POINT('Ctrl Pts',(-14.6835366075574,-12.4070160669481,
117.073337496822)) ;
#161543 = CARTESIAN_POINT('Ctrl Pts',(-14.7573404612619,-12.4070160677341,
117.049106486462)) ;
#161544 = CARTESIAN_POINT('Ctrl Pts',(-14.7582981138329,-12.3311725470681,
117.052023341038)) ;
#161545 = CARTESIAN_POINT('Ctrl Pts',(-14.759255766404,-12.2553290264021,
117.054940195615)) ;
#161546 = CARTESIAN_POINT('Ctrl Pts',(-14.6854519126995,-12.2553290256161,
117.079171205975)) ;
#161547 = CARTESIAN_POINT('Ctrl Pts',(-14.611648058995,-12.2553290248301,
117.103402216336)) ;
#161548 = CARTESIAN_POINT('Ctrl Pts',(-14.6106904064239,-12.3311725454961,
117.10048536176)) ;
#161549 = CARTESIAN_POINT('Ctrl Pts',(-14.7103650458112,-12.3830921654557,
117.368691273652)) ;
#161550 = CARTESIAN_POINT('Ctrl Pts',(-14.7031789791306,-12.4554200435771,
117.3468036748)) ;
#161551 = CARTESIAN_POINT('Ctrl Pts',(-14.7769828347535,-12.4554200554495,
117.322572670283)) ;
#161552 = CARTESIAN_POINT('Ctrl Pts',(-14.8507866903763,-12.4554200673219,
117.298341665765)) ;
#161553 = CARTESIAN_POINT('Ctrl Pts',(-14.8579727570569,-12.3830921892004,
117.320229264616)) ;
#161554 = CARTESIAN_POINT('Ctrl Pts',(-14.8651588237375,-12.310764311079,
117.342116863467)) ;
#161555 = CARTESIAN_POINT('Ctrl Pts',(-14.7913549681146,-12.3107642992066,
117.366347867985)) ;
#161556 = CARTESIAN_POINT('Ctrl Pts',(-14.7175511124917,-12.3107642873342,
117.390578872503)) ;
#161557 = CARTESIAN_POINT('Ctrl Pts',(-14.7103650458112,-12.3830921654557,
117.368691273652)) ;
#161558 = CARTESIAN_POINT('Ctrl Pts',(-14.8029787361383,-12.5097082549453,
117.615209351864)) ;
#161559 = CARTESIAN_POINT('Ctrl Pts',(-14.790052001847,-12.5733006688363,
117.575836605912)) ;
#161560 = CARTESIAN_POINT('Ctrl Pts',(-14.8638558585522,-12.5733006960963,
117.55160560469)) ;
#161561 = CARTESIAN_POINT('Ctrl Pts',(-14.9376597152575,-12.5733007233563,
117.527374603469)) ;
#161562 = CARTESIAN_POINT('Ctrl Pts',(-14.9505864495488,-12.5097083094653,
117.566747349422)) ;
#161563 = CARTESIAN_POINT('Ctrl Pts',(-14.9635131838401,-12.4461158955744,
117.606120095374)) ;
#161564 = CARTESIAN_POINT('Ctrl Pts',(-14.8897093271349,-12.4461158683144,
117.630351096595)) ;
#161565 = CARTESIAN_POINT('Ctrl Pts',(-14.8159054704297,-12.4461158410544,
117.654582097816)) ;
#161566 = CARTESIAN_POINT('Ctrl Pts',(-14.8029787361383,-12.5097082549453,
117.615209351864)) ;
#161567 = CARTESIAN_POINT('Ctrl Pts',(-14.8815949767115,-12.6999655173835,
117.819379893254)) ;
#161568 = CARTESIAN_POINT('Ctrl Pts',(-14.8638908473129,-12.7503658770991,
117.765455972768)) ;
#161569 = CARTESIAN_POINT('Ctrl Pts',(-14.9376947027237,-12.7503659198469,
117.741224967604)) ;
#161570 = CARTESIAN_POINT('Ctrl Pts',(-15.0114985581344,-12.7503659625947,
117.71699396244)) ;
#161571 = CARTESIAN_POINT('Ctrl Pts',(-15.029202687533,-12.699965602879,117.770917882926)) ;
#161572 = CARTESIAN_POINT('Ctrl Pts',(-15.0469068169316,-12.6495652431633,
117.824841803413)) ;
#161573 = CARTESIAN_POINT('Ctrl Pts',(-14.9731029615209,-12.6495652004156,
117.849072808577)) ;
#161574 = CARTESIAN_POINT('Ctrl Pts',(-14.8992991061101,-12.6495651576678,
117.873303813741)) ;
#161575 = CARTESIAN_POINT('Ctrl Pts',(-14.8815949767115,-12.6999655173835,
117.819379893254)) ;
#161576 = CARTESIAN_POINT('Ctrl Pts',(-14.9425172204992,-12.9431519741363,
117.969375033027)) ;
#161577 = CARTESIAN_POINT('Ctrl Pts',(-14.9212698376286,-12.9766466266446,
117.904658934347)) ;
#161578 = CARTESIAN_POINT('Ctrl Pts',(-14.9950736903222,-12.9766466864281,
117.880427920907)) ;
#161579 = CARTESIAN_POINT('Ctrl Pts',(-15.0688775430157,-12.9766467462115,
117.856196907467)) ;
#161580 = CARTESIAN_POINT('Ctrl Pts',(-15.0901249258863,-12.9431520937032,
117.920913006147)) ;
#161581 = CARTESIAN_POINT('Ctrl Pts',(-15.1113723087568,-12.9096574411949,
117.985629104826)) ;
#161582 = CARTESIAN_POINT('Ctrl Pts',(-15.0375684560633,-12.9096573814114,
118.009860118267)) ;
#161583 = CARTESIAN_POINT('Ctrl Pts',(-14.9637646033697,-12.9096573216279,
118.034091131707)) ;
#161584 = CARTESIAN_POINT('Ctrl Pts',(-14.9425172204992,-12.9431519741363,
117.969375033027)) ;
#161585 = CARTESIAN_POINT('Ctrl Pts',(-14.9812992054159,-13.2187420743147,
118.052168315938)) ;
#161586 = CARTESIAN_POINT('Ctrl Pts',(-14.9580445655685,-13.233044020348,
117.981338436508)) ;
#161587 = CARTESIAN_POINT('Ctrl Pts',(-15.0318484133956,-13.2330440926295,
117.957107408245)) ;
#161588 = CARTESIAN_POINT('Ctrl Pts',(-15.1056522612227,-13.2330441649111,
117.932876379983)) ;
#161589 = CARTESIAN_POINT('Ctrl Pts',(-15.1289069010701,-13.2187422188778,
118.003706259413)) ;
#161590 = CARTESIAN_POINT('Ctrl Pts',(-15.1521615409175,-13.2044402728445,
118.074536138843)) ;
#161591 = CARTESIAN_POINT('Ctrl Pts',(-15.0783576930904,-13.204440200563,
118.098767167106)) ;
#161592 = CARTESIAN_POINT('Ctrl Pts',(-15.0045538452633,-13.2044401282814,
118.122998195368)) ;
#161593 = CARTESIAN_POINT('Ctrl Pts',(-14.9812992054159,-13.2187420743147,
118.052168315938)) ;
#161594 = CARTESIAN_POINT('Ctrl Pts',(-14.9963500333539,-13.5111774969548,
118.062342681364)) ;
#161595 = CARTESIAN_POINT('Ctrl Pts',(-14.9727486985028,-13.505083397222,
117.990456825067)) ;
#161596 = CARTESIAN_POINT('Ctrl Pts',(-15.046552539892,-13.5050834796266,
117.966225777196)) ;
#161597 = CARTESIAN_POINT('Ctrl Pts',(-15.1203563812812,-13.5050835620312,
117.941994729324)) ;
#161598 = CARTESIAN_POINT('Ctrl Pts',(-15.1439577161323,-13.511177661764,
118.013880585621)) ;
#161599 = CARTESIAN_POINT('Ctrl Pts',(-15.1675590509834,-13.5172717614969,
118.085766441919)) ;
#161600 = CARTESIAN_POINT('Ctrl Pts',(-15.0937552095942,-13.5172716790923,
118.10999748979)) ;
#161601 = CARTESIAN_POINT('Ctrl Pts',(-15.019951368205,-13.5172715966877,
118.134228537661)) ;
#161602 = CARTESIAN_POINT('Ctrl Pts',(-14.9963500333539,-13.5111774969548,
118.062342681364)) ;
#161603 = CARTESIAN_POINT('Ctrl Pts',(-14.9871457345053,-13.7940494918521,
117.999019373326)) ;
#161604 = CARTESIAN_POINT('Ctrl Pts',(-14.9648830646108,-13.7681973144643,
117.931210874597)) ;
#161605 = CARTESIAN_POINT('Ctrl Pts',(-15.0386868986759,-13.7681973972875,
117.906979804418)) ;
#161606 = CARTESIAN_POINT('Ctrl Pts',(-15.112490732741,-13.7681974801107,
117.882748734239)) ;
#161607 = CARTESIAN_POINT('Ctrl Pts',(-15.1347534026356,-13.7940496574985,
117.950557232967)) ;
#161608 = CARTESIAN_POINT('Ctrl Pts',(-15.1570160725302,-13.8199018348862,
118.018365731696)) ;
#161609 = CARTESIAN_POINT('Ctrl Pts',(-15.0832122384651,-13.819901752063,
118.042596801875)) ;
#161610 = CARTESIAN_POINT('Ctrl Pts',(-15.0094084043999,-13.8199016692398,
118.066827872054)) ;
#161611 = CARTESIAN_POINT('Ctrl Pts',(-14.9871457345053,-13.7940494918521,
117.999019373326)) ;
#161612 = CARTESIAN_POINT('Ctrl Pts',(-14.9548742901699,-14.0529110285333,
117.865026253004)) ;
#161613 = CARTESIAN_POINT('Ctrl Pts',(-14.9355706975565,-14.0089483158053,
117.806230626371)) ;
#161614 = CARTESIAN_POINT('Ctrl Pts',(-15.0093745237244,-14.0089483935527,
117.781999532138)) ;
#161615 = CARTESIAN_POINT('Ctrl Pts',(-15.0831783498923,-14.0089484713001,
117.757768437906)) ;
#161616 = CARTESIAN_POINT('Ctrl Pts',(-15.1024819425057,-14.0529111840282,
117.816564064539)) ;
#161617 = CARTESIAN_POINT('Ctrl Pts',(-15.1217855351191,-14.0968738967562,
117.875359691172)) ;
#161618 = CARTESIAN_POINT('Ctrl Pts',(-15.0479817089512,-14.0968738190088,
117.899590785405)) ;
#161619 = CARTESIAN_POINT('Ctrl Pts',(-14.9741778827833,-14.0968737412614,
117.923821879638)) ;
#161620 = CARTESIAN_POINT('Ctrl Pts',(-14.9548742901699,-14.0529110285333,
117.865026253004)) ;
#161621 = CARTESIAN_POINT('Ctrl Pts',(-14.9032500009219,-14.2634870650102,
117.672503574574)) ;
#161622 = CARTESIAN_POINT('Ctrl Pts',(-14.8882526660298,-14.2047586746315,
117.62682411422)) ;
#161623 = CARTESIAN_POINT('Ctrl Pts',(-14.9620564854445,-14.2047587372463,
117.602592999418)) ;
#161624 = CARTESIAN_POINT('Ctrl Pts',(-15.0358603048591,-14.204758799861,
117.578361884616)) ;
#161625 = CARTESIAN_POINT('Ctrl Pts',(-15.0508576397512,-14.2634871902397,
117.62404134497)) ;
#161626 = CARTESIAN_POINT('Ctrl Pts',(-15.0658549746433,-14.3222155806184,
117.669720805323)) ;
#161627 = CARTESIAN_POINT('Ctrl Pts',(-14.9920511552287,-14.3222155180036,
117.693951920125)) ;
#161628 = CARTESIAN_POINT('Ctrl Pts',(-14.918247335814,-14.3222154553889,
117.718183034927)) ;
#161629 = CARTESIAN_POINT('Ctrl Pts',(-14.9032500009219,-14.2634870650102,
117.672503574574)) ;
#161630 = CARTESIAN_POINT('Ctrl Pts',(-14.8361924144871,-14.4148461022599,
117.432794192959)) ;
#161631 = CARTESIAN_POINT('Ctrl Pts',(-14.8265885875091,-14.3454644446965,
117.40354248755)) ;
#161632 = CARTESIAN_POINT('Ctrl Pts',(-14.9003924014718,-14.3454644862781,
117.379311356142)) ;
#161633 = CARTESIAN_POINT('Ctrl Pts',(-14.9741962154345,-14.3454645278597,
117.355080224734)) ;
#161634 = CARTESIAN_POINT('Ctrl Pts',(-14.9838000424125,-14.414846185423,
117.384331930144)) ;
#161635 = CARTESIAN_POINT('Ctrl Pts',(-14.9934038693905,-14.4842278429864,
117.413583635553)) ;
#161636 = CARTESIAN_POINT('Ctrl Pts',(-14.9196000554278,-14.4842278014048,
117.437814766961)) ;
#161637 = CARTESIAN_POINT('Ctrl Pts',(-14.8457962414651,-14.4842277598232,
117.462045898369)) ;
#161638 = CARTESIAN_POINT('Ctrl Pts',(-14.8361924144871,-14.4148461022599,
117.432794192959)) ;
#161639 = CARTESIAN_POINT('Ctrl Pts',(-14.7594134311292,-14.494780073978,
117.16350011444)) ;
#161640 = CARTESIAN_POINT('Ctrl Pts',(-14.7558891680831,-14.4197159016166,
117.152765779888)) ;
#161641 = CARTESIAN_POINT('Ctrl Pts',(-14.8296929787699,-14.4197159169921,
117.128534638503)) ;
#161642 = CARTESIAN_POINT('Ctrl Pts',(-14.9034967894568,-14.4197159323676,
117.104303497117)) ;
#161643 = CARTESIAN_POINT('Ctrl Pts',(-14.9070210525029,-14.4947801047291,
117.115037831669)) ;
#161644 = CARTESIAN_POINT('Ctrl Pts',(-14.910545315549,-14.5698442770905,
117.125772166221)) ;
#161645 = CARTESIAN_POINT('Ctrl Pts',(-14.8367415048621,-14.5698442617149,
117.150003307607)) ;
#161646 = CARTESIAN_POINT('Ctrl Pts',(-14.7629376941752,-14.5698442463394,
117.174234448992)) ;
#161647 = CARTESIAN_POINT('Ctrl Pts',(-14.7594134311292,-14.494780073978,
117.16350011444)) ;
#161648 = CARTESIAN_POINT('Ctrl Pts',(-14.6788165394104,-14.4974507314962,
116.882424493313)) ;
#161649 = CARTESIAN_POINT('Ctrl Pts',(-14.6816504035553,-14.4220890720825,
116.891055988342)) ;
#161650 = CARTESIAN_POINT('Ctrl Pts',(-14.7554542135507,-14.4220890586317,
116.866824844851)) ;
#161651 = CARTESIAN_POINT('Ctrl Pts',(-14.8292580235462,-14.4220890451809,
116.842593701359)) ;
#161652 = CARTESIAN_POINT('Ctrl Pts',(-14.8264241594014,-14.4974507045946,
116.83396220633)) ;
#161653 = CARTESIAN_POINT('Ctrl Pts',(-14.8235902952566,-14.5728123640084,
116.825330711301)) ;
#161654 = CARTESIAN_POINT('Ctrl Pts',(-14.7497864852611,-14.5728123774592,
116.849561854792)) ;
#161655 = CARTESIAN_POINT('Ctrl Pts',(-14.6759826752656,-14.57281239091,116.873792998283)) ;
#161656 = CARTESIAN_POINT('Ctrl Pts',(-14.6788165394104,-14.4974507314962,
116.882424493313)) ;
#161657 = CARTESIAN_POINT('Ctrl Pts',(-14.6018098242213,-14.4229495346006,
116.612531368624)) ;
#161658 = CARTESIAN_POINT('Ctrl Pts',(-14.6107555369899,-14.3526782474262,
116.639778568426)) ;
#161659 = CARTESIAN_POINT('Ctrl Pts',(-14.6845593491738,-14.3526782058987,
116.615547431601)) ;
#161660 = CARTESIAN_POINT('Ctrl Pts',(-14.7583631613577,-14.3526781643712,
116.591316294775)) ;
#161661 = CARTESIAN_POINT('Ctrl Pts',(-14.7494174485891,-14.4229494515456,
116.564069094973)) ;
#161662 = CARTESIAN_POINT('Ctrl Pts',(-14.7404717358206,-14.49322073872,116.53682189517)) ;
#161663 = CARTESIAN_POINT('Ctrl Pts',(-14.6666679236366,-14.4932207802475,
116.561053031996)) ;
#161664 = CARTESIAN_POINT('Ctrl Pts',(-14.5928641114527,-14.493220821775,
116.585284168822)) ;
#161665 = CARTESIAN_POINT('Ctrl Pts',(-14.6018098242213,-14.4229495346006,
116.612531368624)) ;
#161666 = CARTESIAN_POINT('Ctrl Pts',(-14.5338249366433,-14.2768020033666,
116.370022693878)) ;
#161667 = CARTESIAN_POINT('Ctrl Pts',(-14.5482635939486,-14.2166300695752,
116.414000516451)) ;
#161668 = CARTESIAN_POINT('Ctrl Pts',(-14.6220674107796,-14.2166300030693,
116.389769393779)) ;
#161669 = CARTESIAN_POINT('Ctrl Pts',(-14.6958712276106,-14.2166299365633,
116.365538271108)) ;
#161670 = CARTESIAN_POINT('Ctrl Pts',(-14.6814325703052,-14.2768018703547,
116.321560448536)) ;
#161671 = CARTESIAN_POINT('Ctrl Pts',(-14.6669939129999,-14.336973804146,
116.277582625963)) ;
#161672 = CARTESIAN_POINT('Ctrl Pts',(-14.5931900961689,-14.336973870652,
116.301813748635)) ;
#161673 = CARTESIAN_POINT('Ctrl Pts',(-14.5193862793379,-14.3369739371579,
116.326044871306)) ;
#161674 = CARTESIAN_POINT('Ctrl Pts',(-14.5338249366433,-14.2768020033666,
116.370022693878)) ;
#161675 = CARTESIAN_POINT('Ctrl Pts',(-14.4805103340185,-14.0672719747909,
116.171945276152)) ;
#161676 = CARTESIAN_POINT('Ctrl Pts',(-14.4994313031301,-14.0216384576254,
116.229575497223)) ;
#161677 = CARTESIAN_POINT('Ctrl Pts',(-14.5732351268998,-14.0216383725684,
116.205344395686)) ;
#161678 = CARTESIAN_POINT('Ctrl Pts',(-14.6470389506695,-14.0216382875114,
116.181113294149)) ;
#161679 = CARTESIAN_POINT('Ctrl Pts',(-14.628117981558,-14.067271804677,116.123483073077)) ;
#161680 = CARTESIAN_POINT('Ctrl Pts',(-14.6091970124464,-14.1129053218425,
116.065852852006)) ;
#161681 = CARTESIAN_POINT('Ctrl Pts',(-14.5353931886767,-14.1129054068995,
116.090083953543)) ;
#161682 = CARTESIAN_POINT('Ctrl Pts',(-14.4615893649069,-14.1129054919565,
116.11431505508)) ;
#161683 = CARTESIAN_POINT('Ctrl Pts',(-14.4805103340185,-14.0672719747909,
116.171945276152)) ;
#161684 = CARTESIAN_POINT('Ctrl Pts',(-14.4472092133991,-13.8140437794069,
116.035263380737)) ;
#161685 = CARTESIAN_POINT('Ctrl Pts',(-14.4692127086449,-13.786022349902,
116.102282479007)) ;
#161686 = CARTESIAN_POINT('Ctrl Pts',(-14.5430165403838,-13.7860222533108,
116.078051401742)) ;
#161687 = CARTESIAN_POINT('Ctrl Pts',(-14.6168203721226,-13.7860221567197,
116.053820324478)) ;
#161688 = CARTESIAN_POINT('Ctrl Pts',(-14.5948168768768,-13.8140435862246,
115.986801226207)) ;
#161689 = CARTESIAN_POINT('Ctrl Pts',(-14.5728133816309,-13.8420650157295,
115.919782127937)) ;
#161690 = CARTESIAN_POINT('Ctrl Pts',(-14.4990095498921,-13.8420651123206,
115.944013205202)) ;
#161691 = CARTESIAN_POINT('Ctrl Pts',(-14.4252057181532,-13.8420652089118,
115.968244282466)) ;
#161692 = CARTESIAN_POINT('Ctrl Pts',(-14.4472092133991,-13.8140437794069,
116.035263380737)) ;
#161693 = CARTESIAN_POINT('Ctrl Pts',(-14.4362486432515,-13.5305545368903,
115.96633944488)) ;
#161694 = CARTESIAN_POINT('Ctrl Pts',(-14.4597857472441,-13.5222834200997,
116.038029667866)) ;
#161695 = CARTESIAN_POINT('Ctrl Pts',(-14.5335895875712,-13.5222833210965,
116.01379861676)) ;
#161696 = CARTESIAN_POINT('Ctrl Pts',(-14.6073934278984,-13.5222832220932,
115.989567565655)) ;
#161697 = CARTESIAN_POINT('Ctrl Pts',(-14.5838563239058,-13.5305543388838,
115.917877342668)) ;
#161698 = CARTESIAN_POINT('Ctrl Pts',(-14.5603192199132,-13.5388254556744,
115.846187119682)) ;
#161699 = CARTESIAN_POINT('Ctrl Pts',(-14.486515379586,-13.5388255546776,
115.870418170788)) ;
#161700 = CARTESIAN_POINT('Ctrl Pts',(-14.4127115392589,-13.5388256536809,
115.894649221894)) ;
#161701 = CARTESIAN_POINT('Ctrl Pts',(-14.4362486432515,-13.5305545368903,
115.96633944488)) ;
#161702 = CARTESIAN_POINT('Ctrl Pts',(-14.449486240473,-13.2400469135056,
115.971266296655)) ;
#161703 = CARTESIAN_POINT('Ctrl Pts',(-14.4728667368979,-13.2520460162367,
116.042479518172)) ;
#161704 = CARTESIAN_POINT('Ctrl Pts',(-14.5466705853202,-13.2520459225966,
116.018248491723)) ;
#161705 = CARTESIAN_POINT('Ctrl Pts',(-14.6204744337425,-13.2520458289565,
115.994017465274)) ;
#161706 = CARTESIAN_POINT('Ctrl Pts',(-14.5970939373175,-13.2400467262255,
115.922804243756)) ;
#161707 = CARTESIAN_POINT('Ctrl Pts',(-14.5737134408926,-13.2280476234944,
115.851591022239)) ;
#161708 = CARTESIAN_POINT('Ctrl Pts',(-14.4999095924703,-13.2280477171344,
115.875822048688)) ;
#161709 = CARTESIAN_POINT('Ctrl Pts',(-14.426105744048,-13.2280478107745,
115.900053075137)) ;
#161710 = CARTESIAN_POINT('Ctrl Pts',(-14.449486240473,-13.2400469135056,
115.971266296655)) ;
#161711 = CARTESIAN_POINT('Ctrl Pts',(-14.4868824566312,-12.9607801917685,
116.04957346963)) ;
#161712 = CARTESIAN_POINT('Ctrl Pts',(-14.5084238912217,-12.9922952069383,
116.115185205403)) ;
#161713 = CARTESIAN_POINT('Ctrl Pts',(-14.5822277463875,-12.9922951270176,
116.090954199492)) ;
#161714 = CARTESIAN_POINT('Ctrl Pts',(-14.6560316015532,-12.9922950470968,
116.066723193582)) ;
#161715 = CARTESIAN_POINT('Ctrl Pts',(-14.6344901669627,-12.960780031927,
116.00111145781)) ;
#161716 = CARTESIAN_POINT('Ctrl Pts',(-14.6129487323722,-12.9292650167572,
115.935499722038)) ;
#161717 = CARTESIAN_POINT('Ctrl Pts',(-14.5391448772065,-12.929265096678,
115.959730727948)) ;
#161718 = CARTESIAN_POINT('Ctrl Pts',(-14.4653410220408,-12.9292651765987,
115.983961733858)) ;
#161719 = CARTESIAN_POINT('Ctrl Pts',(-14.4868824566312,-12.9607801917685,
116.04957346963)) ;
#161720 = CARTESIAN_POINT('Ctrl Pts',(-14.5461400633249,-12.7157522020321,
116.194666581357)) ;
#161721 = CARTESIAN_POINT('Ctrl Pts',(-14.5643090647105,-12.7644222769748,
116.250006429608)) ;
#161722 = CARTESIAN_POINT('Ctrl Pts',(-14.6381129248079,-12.7644222146516,
116.225775438719)) ;
#161723 = CARTESIAN_POINT('Ctrl Pts',(-14.7119167849052,-12.7644221523283,
116.20154444783)) ;
#161724 = CARTESIAN_POINT('Ctrl Pts',(-14.6937477835196,-12.7157520773856,
116.146204599579)) ;
#161725 = CARTESIAN_POINT('Ctrl Pts',(-14.675578782134,-12.6670820024428,
116.090864751328)) ;
#161726 = CARTESIAN_POINT('Ctrl Pts',(-14.6017749220366,-12.6670820647661,
116.115095742217)) ;
#161727 = CARTESIAN_POINT('Ctrl Pts',(-14.5279710619392,-12.6670821270893,
116.139326733106)) ;
#161728 = CARTESIAN_POINT('Ctrl Pts',(-14.5461400633249,-12.7157522020321,
116.194666581357)) ;
#161729 = CARTESIAN_POINT('Ctrl Pts',(-14.6240444846692,-12.5205021117526,
116.396478689841)) ;
#161730 = CARTESIAN_POINT('Ctrl Pts',(-14.6375357271718,-12.5828779756765,
116.437570839145)) ;
#161731 = CARTESIAN_POINT('Ctrl Pts',(-14.7113395899329,-12.5828779339693,
116.413339856369)) ;
#161732 = CARTESIAN_POINT('Ctrl Pts',(-14.785143452694,-12.582877892262,116.389108873593)) ;
#161733 = CARTESIAN_POINT('Ctrl Pts',(-14.7716522101914,-12.5205020283381,
116.348016724289)) ;
#161734 = CARTESIAN_POINT('Ctrl Pts',(-14.7581609676887,-12.4581261644142,
116.306924574986)) ;
#161735 = CARTESIAN_POINT('Ctrl Pts',(-14.6843571049276,-12.4581262061215,
116.331155557762)) ;
#161736 = CARTESIAN_POINT('Ctrl Pts',(-14.6105532421665,-12.4581262478287,
116.355386540537)) ;
#161737 = CARTESIAN_POINT('Ctrl Pts',(-14.6240444846692,-12.5205021117526,
116.396478689841)) ;
#161738 = CARTESIAN_POINT('Ctrl Pts',(-14.7155078962198,-12.3896091910669,
116.639659815513)) ;
#161739 = CARTESIAN_POINT('Ctrl Pts',(-14.7233661315669,-12.4612182427459,
116.663594733761)) ;
#161740 = CARTESIAN_POINT('Ctrl Pts',(-14.7971699949239,-12.4612182215385,
116.6393637528)) ;
#161741 = CARTESIAN_POINT('Ctrl Pts',(-14.8709738582809,-12.461218200331,
116.615132771839)) ;
#161742 = CARTESIAN_POINT('Ctrl Pts',(-14.8631156229337,-12.389609148652,
116.591197853591)) ;
#161743 = CARTESIAN_POINT('Ctrl Pts',(-14.8552573875865,-12.318000096973,
116.567262935343)) ;
#161744 = CARTESIAN_POINT('Ctrl Pts',(-14.7814535242296,-12.3180001181804,
116.591493916304)) ;
#161745 = CARTESIAN_POINT('Ctrl Pts',(-14.7076496608726,-12.3180001393879,
116.615724897265)) ;
#161746 = CARTESIAN_POINT('Ctrl Pts',(-14.7155078962198,-12.3896091910669,
116.639659815513)) ;
#161747 = CARTESIAN_POINT('Ctrl Pts',(-14.8155283401331,-12.3322116649338,
116.908678402663)) ;
#161748 = CARTESIAN_POINT('Ctrl Pts',(-14.817152276422,-12.4079372852091,
116.913624651688)) ;
#161749 = CARTESIAN_POINT('Ctrl Pts',(-14.8909561377333,-12.4079372823359,
116.889393664496)) ;
#161750 = CARTESIAN_POINT('Ctrl Pts',(-14.9647599990446,-12.4079372794628,
116.865162677304)) ;
#161751 = CARTESIAN_POINT('Ctrl Pts',(-14.9631360627557,-12.3322116591875,
116.860216428279)) ;
#161752 = CARTESIAN_POINT('Ctrl Pts',(-14.9615121264668,-12.2564860389122,
116.855270179255)) ;
#161753 = CARTESIAN_POINT('Ctrl Pts',(-14.8877082651555,-12.2564860417854,
116.879501166446)) ;
#161754 = CARTESIAN_POINT('Ctrl Pts',(-14.8139044038442,-12.2564860446585,
116.903732153638)) ;
#161755 = CARTESIAN_POINT('Ctrl Pts',(-14.8155283401331,-12.3322116649338,
116.908678402663)) ;
#161756 = CARTESIAN_POINT('Ctrl Pts',(-14.9160696924354,-12.3526193896652,
117.179651593861)) ;
#161757 = CARTESIAN_POINT('Ctrl Pts',(-14.9114057877124,-12.4270343562084,
117.165446093574)) ;
#161758 = CARTESIAN_POINT('Ctrl Pts',(-14.9852096465855,-12.4270343671983,
117.141215098956)) ;
#161759 = CARTESIAN_POINT('Ctrl Pts',(-15.0590135054586,-12.4270343781882,
117.116984104338)) ;
#161760 = CARTESIAN_POINT('Ctrl Pts',(-15.0636774101816,-12.352619411645,
117.131189604624)) ;
#161761 = CARTESIAN_POINT('Ctrl Pts',(-15.0683413149046,-12.2782044451017,
117.145395104911)) ;
#161762 = CARTESIAN_POINT('Ctrl Pts',(-14.9945374560315,-12.2782044341118,
117.169626099529)) ;
#161763 = CARTESIAN_POINT('Ctrl Pts',(-14.9207335971584,-12.2782044231219,
117.193857094147)) ;
#161764 = CARTESIAN_POINT('Ctrl Pts',(-14.9160696924354,-12.3526193896652,
117.179651593861)) ;
#161765 = CARTESIAN_POINT('Ctrl Pts',(-15.0126074976825,-12.4495335034968,
117.438097138294)) ;
#161766 = CARTESIAN_POINT('Ctrl Pts',(-15.0019325703686,-12.5172950398371,
117.405583032877)) ;
#161767 = CARTESIAN_POINT('Ctrl Pts',(-15.075736424986,-12.517295059255,117.381352025297)) ;
#161768 = CARTESIAN_POINT('Ctrl Pts',(-15.1495402796035,-12.5172950786729,
117.357121017717)) ;
#161769 = CARTESIAN_POINT('Ctrl Pts',(-15.1602152069174,-12.4495335423326,
117.389635123133)) ;
#161770 = CARTESIAN_POINT('Ctrl Pts',(-15.1708901342314,-12.3817720059923,
117.42214922855)) ;
#161771 = CARTESIAN_POINT('Ctrl Pts',(-15.0970862796139,-12.3817719865744,
117.44638023613)) ;
#161772 = CARTESIAN_POINT('Ctrl Pts',(-15.0232824249965,-12.3817719671566,
117.47061124371)) ;
#161773 = CARTESIAN_POINT('Ctrl Pts',(-15.0126074976825,-12.4495335034968,
117.438097138294)) ;
#161774 = CARTESIAN_POINT('Ctrl Pts',(-15.0977303726993,-12.6159519111974,
117.661885772396)) ;
#161775 = CARTESIAN_POINT('Ctrl Pts',(-15.0818299469695,-12.6721964554001,
117.613455641767)) ;
#161776 = CARTESIAN_POINT('Ctrl Pts',(-15.1556337975825,-12.6721964775936,
117.58922462199)) ;
#161777 = CARTESIAN_POINT('Ctrl Pts',(-15.2294376481955,-12.6721964997871,
117.564993602213)) ;
#161778 = CARTESIAN_POINT('Ctrl Pts',(-15.2453380739253,-12.6159519555843,
117.613423732842)) ;
#161779 = CARTESIAN_POINT('Ctrl Pts',(-15.2612384996551,-12.5597074113816,
117.661853863472)) ;
#161780 = CARTESIAN_POINT('Ctrl Pts',(-15.1874346490421,-12.5597073891882,
117.686084883249)) ;
#161781 = CARTESIAN_POINT('Ctrl Pts',(-15.1136307984291,-12.5597073669947,
117.710315903026)) ;
#161782 = CARTESIAN_POINT('Ctrl Pts',(-15.0977303726993,-12.6159519111974,
117.661885772396)) ;
#161783 = CARTESIAN_POINT('Ctrl Pts',(-15.1663307990368,-12.8395609374739,
117.835382986547)) ;
#161784 = CARTESIAN_POINT('Ctrl Pts',(-15.1463499196944,-12.8802774256323,
117.774524452437)) ;
#161785 = CARTESIAN_POINT('Ctrl Pts',(-15.2201537669202,-12.8802774463099,
117.750293422343)) ;
#161786 = CARTESIAN_POINT('Ctrl Pts',(-15.293957614146,-12.8802774669874,
117.726062392249)) ;
#161787 = CARTESIAN_POINT('Ctrl Pts',(-15.3139384934884,-12.839560978829,
117.786920926359)) ;
#161788 = CARTESIAN_POINT('Ctrl Pts',(-15.3339193728309,-12.7988444906705,
117.847779460469)) ;
#161789 = CARTESIAN_POINT('Ctrl Pts',(-15.260115525605,-12.798844469993,117.872010490563)) ;
#161790 = CARTESIAN_POINT('Ctrl Pts',(-15.1863116783792,-12.7988444493154,
117.896241520657)) ;
#161791 = CARTESIAN_POINT('Ctrl Pts',(-15.1663307990368,-12.8395609374739,
117.835382986547)) ;
#161792 = CARTESIAN_POINT('Ctrl Pts',(-15.2143261495517,-13.1036924153161,
117.946224932861)) ;
#161793 = CARTESIAN_POINT('Ctrl Pts',(-15.1916953168761,-13.126027690226,
117.877295068337)) ;
#161794 = CARTESIAN_POINT('Ctrl Pts',(-15.265499161631,-13.1260277069746,
117.853064030717)) ;
#161795 = CARTESIAN_POINT('Ctrl Pts',(-15.3393030063859,-13.1260277237232,
117.828832993097)) ;
#161796 = CARTESIAN_POINT('Ctrl Pts',(-15.3619338390615,-13.1036924488133,
117.897762857621)) ;
#161797 = CARTESIAN_POINT('Ctrl Pts',(-15.3845646717372,-13.0813571739034,
117.966692722145)) ;
#161798 = CARTESIAN_POINT('Ctrl Pts',(-15.3107608269823,-13.0813571571548,
117.990923759765)) ;
#161799 = CARTESIAN_POINT('Ctrl Pts',(-15.2369569822274,-13.0813571404062,
118.015154797385)) ;
#161800 = CARTESIAN_POINT('Ctrl Pts',(-15.2143261495517,-13.1036924153161,
117.946224932861)) ;
#161801 = CARTESIAN_POINT('Ctrl Pts',(-15.2392646854199,-13.3927905140901,
117.986526462558)) ;
#161802 = CARTESIAN_POINT('Ctrl Pts',(-15.2155960469045,-13.3949729390862,
117.914435608735)) ;
#161803 = CARTESIAN_POINT('Ctrl Pts',(-15.2893998901954,-13.3949729481192,
117.890204566656)) ;
#161804 = CARTESIAN_POINT('Ctrl Pts',(-15.3632037334863,-13.3949729571521,
117.865973524577)) ;
#161805 = CARTESIAN_POINT('Ctrl Pts',(-15.3868723720017,-13.392790532156,
117.9380643784)) ;
#161806 = CARTESIAN_POINT('Ctrl Pts',(-15.4105410105172,-13.3906081071599,
118.010155232223)) ;
#161807 = CARTESIAN_POINT('Ctrl Pts',(-15.3367371672263,-13.390608098127,
118.034386274302)) ;
#161808 = CARTESIAN_POINT('Ctrl Pts',(-15.2629333239354,-13.3906080890941,
118.058617316381)) ;
#161809 = CARTESIAN_POINT('Ctrl Pts',(-15.2392646854199,-13.3927905140901,
117.986526462558)) ;
#161810 = CARTESIAN_POINT('Ctrl Pts',(-15.2397192982517,-13.6807940128297,
117.9526185938)) ;
#161811 = CARTESIAN_POINT('Ctrl Pts',(-15.2167138279062,-13.6628697332101,
117.882547643134)) ;
#161812 = CARTESIAN_POINT('Ctrl Pts',(-15.2905176708599,-13.6628697375112,
117.858316600028)) ;
#161813 = CARTESIAN_POINT('Ctrl Pts',(-15.3643215138137,-13.6628697418123,
117.834085556922)) ;
#161814 = CARTESIAN_POINT('Ctrl Pts',(-15.3873269841592,-13.680794021432,
117.904156507587)) ;
#161815 = CARTESIAN_POINT('Ctrl Pts',(-15.4103324545046,-13.6987183010517,
117.974227458253)) ;
#161816 = CARTESIAN_POINT('Ctrl Pts',(-15.3365286115509,-13.6987182967505,
117.998458501359)) ;
#161817 = CARTESIAN_POINT('Ctrl Pts',(-15.2627247685972,-13.6987182924494,
118.022689544465)) ;
#161818 = CARTESIAN_POINT('Ctrl Pts',(-15.2397192982517,-13.6807940128297,
117.9526185938)) ;
#161819 = CARTESIAN_POINT('Ctrl Pts',(-15.2167475033035,-13.9516407801447,
117.847166620473)) ;
#161820 = CARTESIAN_POINT('Ctrl Pts',(-15.1960458684568,-13.9147771638665,
117.784112780923)) ;
#161821 = CARTESIAN_POINT('Ctrl Pts',(-15.2698497117907,-13.9147771635359,
117.759881738975)) ;
#161822 = CARTESIAN_POINT('Ctrl Pts',(-15.3436535551245,-13.9147771632054,
117.735650697027)) ;
#161823 = CARTESIAN_POINT('Ctrl Pts',(-15.3643551899713,-13.9516407794836,
117.798704536577)) ;
#161824 = CARTESIAN_POINT('Ctrl Pts',(-15.3850568248181,-13.9885043957617,
117.861758376127)) ;
#161825 = CARTESIAN_POINT('Ctrl Pts',(-15.3112529814842,-13.9885043960923,
117.885989418075)) ;
#161826 = CARTESIAN_POINT('Ctrl Pts',(-15.2374491381503,-13.9885043964229,
117.910220460023)) ;
#161827 = CARTESIAN_POINT('Ctrl Pts',(-15.2167475033035,-13.9516407801447,
117.847166620473)) ;
#161828 = CARTESIAN_POINT('Ctrl Pts',(-15.1722328786369,-14.1848191645832,
117.675959254401)) ;
#161829 = CARTESIAN_POINT('Ctrl Pts',(-15.1553459389584,-14.1316174193291,
117.62452436078)) ;
#161830 = CARTESIAN_POINT('Ctrl Pts',(-15.2291497829877,-14.1316174171336,
117.600293320951)) ;
#161831 = CARTESIAN_POINT('Ctrl Pts',(-15.3029536270171,-14.1316174149382,
117.576062281121)) ;
#161832 = CARTESIAN_POINT('Ctrl Pts',(-15.3198405666957,-14.1848191601922,
117.627497174741)) ;
#161833 = CARTESIAN_POINT('Ctrl Pts',(-15.3367275063742,-14.2380209054463,
117.678932068361)) ;
#161834 = CARTESIAN_POINT('Ctrl Pts',(-15.2629236623449,-14.2380209076418,
117.703163108191)) ;
#161835 = CARTESIAN_POINT('Ctrl Pts',(-15.1891198183155,-14.2380209098372,
117.727394148021)) ;
#161836 = CARTESIAN_POINT('Ctrl Pts',(-15.1722328786369,-14.1848191645832,
117.675959254401)) ;
#161837 = CARTESIAN_POINT('Ctrl Pts',(-15.1111116959615,-14.3611535147467,
117.45455531879)) ;
#161838 = CARTESIAN_POINT('Ctrl Pts',(-15.0991970488396,-14.2955603830771,
117.418265226013)) ;
#161839 = CARTESIAN_POINT('Ctrl Pts',(-15.173000893171,-14.2955603814556,
117.394034187103)) ;
#161840 = CARTESIAN_POINT('Ctrl Pts',(-15.2468047375024,-14.2955603798341,
117.369803148193)) ;
#161841 = CARTESIAN_POINT('Ctrl Pts',(-15.2587193846242,-14.3611535115037,
117.40609324097)) ;
#161842 = CARTESIAN_POINT('Ctrl Pts',(-15.2706340317462,-14.4267466431733,
117.442383333747)) ;
#161843 = CARTESIAN_POINT('Ctrl Pts',(-15.1968301874148,-14.4267466447948,
117.466614372657)) ;
#161844 = CARTESIAN_POINT('Ctrl Pts',(-15.1230263430834,-14.4267466464163,
117.490845411567)) ;
#161845 = CARTESIAN_POINT('Ctrl Pts',(-15.1111116959615,-14.3611535147467,
117.45455531879)) ;
#161846 = CARTESIAN_POINT('Ctrl Pts',(-15.03716340119,-14.4717132500286,117.193678534081)) ;
#161847 = CARTESIAN_POINT('Ctrl Pts',(-15.0311325532717,-14.3983025037114,
117.175309544367)) ;
#161848 = CARTESIAN_POINT('Ctrl Pts',(-15.1049363971596,-14.3983025035885,
117.151078504106)) ;
#161849 = CARTESIAN_POINT('Ctrl Pts',(-15.1787402410475,-14.3983025034657,
117.126847463845)) ;
#161850 = CARTESIAN_POINT('Ctrl Pts',(-15.1847710889657,-14.4717132497829,
117.14521645356)) ;
#161851 = CARTESIAN_POINT('Ctrl Pts',(-15.190801936884,-14.5451239961002,
117.163585443274)) ;
#161852 = CARTESIAN_POINT('Ctrl Pts',(-15.1169980929961,-14.545123996223,
117.187816483535)) ;
#161853 = CARTESIAN_POINT('Ctrl Pts',(-15.0431942491082,-14.5451239963458,
117.212047523796)) ;
#161854 = CARTESIAN_POINT('Ctrl Pts',(-15.03716340119,-14.4717132500286,117.193678534081)) ;
#161855 = CARTESIAN_POINT('Ctrl Pts',(-14.9574931202988,-14.5058049610956,
116.91556782578)) ;
#161856 = CARTESIAN_POINT('Ctrl Pts',(-14.9577501226259,-14.4299061959812,
116.916350613445)) ;
#161857 = CARTESIAN_POINT('Ctrl Pts',(-15.031553965324,-14.4299061963414,
116.892119569561)) ;
#161858 = CARTESIAN_POINT('Ctrl Pts',(-15.105357808022,-14.4299061967016,
116.867888525676)) ;
#161859 = CARTESIAN_POINT('Ctrl Pts',(-15.1051008056949,-14.505804961816,
116.86710573801)) ;
#161860 = CARTESIAN_POINT('Ctrl Pts',(-15.1048438033677,-14.5817037269304,
116.866322950345)) ;
#161861 = CARTESIAN_POINT('Ctrl Pts',(-15.0310399606696,-14.5817037265702,
116.89055399423)) ;
#161862 = CARTESIAN_POINT('Ctrl Pts',(-14.9572361179716,-14.58170372621,116.914785038115)) ;
#161863 = CARTESIAN_POINT('Ctrl Pts',(-14.9574931202988,-14.5058049610956,
116.91556782578)) ;
#161864 = CARTESIAN_POINT('Ctrl Pts',(-14.8782558620267,-14.4622432474708,
116.638782637704)) ;
#161865 = CARTESIAN_POINT('Ctrl Pts',(-14.8847794043709,-14.389275462024,
116.658652295255)) ;
#161866 = CARTESIAN_POINT('Ctrl Pts',(-14.9585832455578,-14.3892754604599,
116.634421246768)) ;
#161867 = CARTESIAN_POINT('Ctrl Pts',(-15.0323870867446,-14.3892754588959,
116.61019019828)) ;
#161868 = CARTESIAN_POINT('Ctrl Pts',(-15.0258635444004,-14.4622432443427,
116.590320540728)) ;
#161869 = CARTESIAN_POINT('Ctrl Pts',(-15.0193400020562,-14.5352110297894,
116.570450883177)) ;
#161870 = CARTESIAN_POINT('Ctrl Pts',(-14.9455361608693,-14.5352110313535,
116.594681931664)) ;
#161871 = CARTESIAN_POINT('Ctrl Pts',(-14.8717323196825,-14.5352110329176,
116.618912980152)) ;
#161872 = CARTESIAN_POINT('Ctrl Pts',(-14.8782558620267,-14.4622432474708,
116.638782637704)) ;
#161873 = CARTESIAN_POINT('Ctrl Pts',(-14.8058079691528,-14.343914063795,
116.382668771781)) ;
#161874 = CARTESIAN_POINT('Ctrl Pts',(-14.8181331615164,-14.2791023763225,
116.42020931932)) ;
#161875 = CARTESIAN_POINT('Ctrl Pts',(-14.8919370012243,-14.2791023697226,
116.395978266328)) ;
#161876 = CARTESIAN_POINT('Ctrl Pts',(-14.9657408409322,-14.2791023631227,
116.371747213336)) ;
#161877 = CARTESIAN_POINT('Ctrl Pts',(-14.9534156485687,-14.3439140505953,
116.334206665797)) ;
#161878 = CARTESIAN_POINT('Ctrl Pts',(-14.9410904562051,-14.4087257380679,
116.296666118258)) ;
#161879 = CARTESIAN_POINT('Ctrl Pts',(-14.8672866164972,-14.4087257446678,
116.32089717125)) ;
#161880 = CARTESIAN_POINT('Ctrl Pts',(-14.7934827767893,-14.4087257512676,
116.345128224242)) ;
#161881 = CARTESIAN_POINT('Ctrl Pts',(-14.8058079691528,-14.343914063795,
116.382668771781)) ;
#161882 = CARTESIAN_POINT('Ctrl Pts',(-14.7461096383968,-14.1592285094383,
116.165376277947)) ;
#161883 = CARTESIAN_POINT('Ctrl Pts',(-14.7633548151318,-14.1072180552491,
116.217902304186)) ;
#161884 = CARTESIAN_POINT('Ctrl Pts',(-14.8371586539576,-14.1072180404113,
116.193671248507)) ;
#161885 = CARTESIAN_POINT('Ctrl Pts',(-14.9109624927834,-14.1072180255735,
116.169440192828)) ;
#161886 = CARTESIAN_POINT('Ctrl Pts',(-14.8937173160483,-14.1592284797627,
116.116914166588)) ;
#161887 = CARTESIAN_POINT('Ctrl Pts',(-14.8764721393133,-14.2112389339519,
116.064388140349)) ;
#161888 = CARTESIAN_POINT('Ctrl Pts',(-14.8026683004875,-14.2112389487897,
116.088619196028)) ;
#161889 = CARTESIAN_POINT('Ctrl Pts',(-14.7288644616617,-14.2112389636275,
116.112850251707)) ;
#161890 = CARTESIAN_POINT('Ctrl Pts',(-14.7461096383968,-14.1592285094383,
116.165376277947)) ;
#161891 = CARTESIAN_POINT('Ctrl Pts',(-14.7042341925757,-13.9218383285055,
116.002418128098)) ;
#161892 = CARTESIAN_POINT('Ctrl Pts',(-14.725160890206,-13.8863275964736,
116.066157473119)) ;
#161893 = CARTESIAN_POINT('Ctrl Pts',(-14.7989647293144,-13.8863275716233,
116.0419264183)) ;
#161894 = CARTESIAN_POINT('Ctrl Pts',(-14.8727685684227,-13.886327546773,
116.017695363482)) ;
#161895 = CARTESIAN_POINT('Ctrl Pts',(-14.8518418707924,-13.9218382788049,
115.953956018461)) ;
#161896 = CARTESIAN_POINT('Ctrl Pts',(-14.8309151731621,-13.9573490108368,
115.89021667344)) ;
#161897 = CARTESIAN_POINT('Ctrl Pts',(-14.7571113340538,-13.9573490356871,
115.914447728259)) ;
#161898 = CARTESIAN_POINT('Ctrl Pts',(-14.6833074949454,-13.9573490605374,
115.938678783077)) ;
#161899 = CARTESIAN_POINT('Ctrl Pts',(-14.7042341925757,-13.9218383285055,
116.002418128098)) ;
#161900 = CARTESIAN_POINT('Ctrl Pts',(-14.6838147453501,-13.6477929587425,
115.904727451076)) ;
#161901 = CARTESIAN_POINT('Ctrl Pts',(-14.7069319501639,-13.6313648712608,
115.97513872771)) ;
#161902 = CARTESIAN_POINT('Ctrl Pts',(-14.7807357908862,-13.6313648350965,
115.950907677807)) ;
#161903 = CARTESIAN_POINT('Ctrl Pts',(-14.8545396316085,-13.6313647989322,
115.926676627904)) ;
#161904 = CARTESIAN_POINT('Ctrl Pts',(-14.8314224267947,-13.6477928864138,
115.85626535127)) ;
#161905 = CARTESIAN_POINT('Ctrl Pts',(-14.8083052219809,-13.6642209738955,
115.785854074636)) ;
#161906 = CARTESIAN_POINT('Ctrl Pts',(-14.7345013812586,-13.6642210100599,
115.810085124539)) ;
#161907 = CARTESIAN_POINT('Ctrl Pts',(-14.6606975405363,-13.6642210462242,
115.834316174442)) ;
#161908 = CARTESIAN_POINT('Ctrl Pts',(-14.6838147453501,-13.6477929587425,
115.904727451076)) ;
#161909 = CARTESIAN_POINT('Ctrl Pts',(-14.6872087463539,-13.3573882946602,
115.879587299227)) ;
#161910 = CARTESIAN_POINT('Ctrl Pts',(-14.7108565242422,-13.3612124494826,
115.951614616009)) ;
#161911 = CARTESIAN_POINT('Ctrl Pts',(-14.7846603682144,-13.3612124035114,
115.927383576005)) ;
#161912 = CARTESIAN_POINT('Ctrl Pts',(-14.8584642121865,-13.3612123575402,
115.903152536001)) ;
#161913 = CARTESIAN_POINT('Ctrl Pts',(-14.8348164342983,-13.3573882027177,
115.83112521922)) ;
#161914 = CARTESIAN_POINT('Ctrl Pts',(-14.81116865641,-13.3535640478952,115.759097902438)) ;
#161915 = CARTESIAN_POINT('Ctrl Pts',(-14.7373648124378,-13.3535640938664,
115.783328942442)) ;
#161916 = CARTESIAN_POINT('Ctrl Pts',(-14.6635609684656,-13.3535641398377,
115.807559982446)) ;
#161917 = CARTESIAN_POINT('Ctrl Pts',(-14.6872087463539,-13.3573882946602,
115.879587299227)) ;
#161918 = CARTESIAN_POINT('Ctrl Pts',(-14.7148769500706,-13.0713760146383,
115.928387341854)) ;
#161919 = CARTESIAN_POINT('Ctrl Pts',(-14.7373611554509,-13.0951747720227,
115.996870604688)) ;
#161920 = CARTESIAN_POINT('Ctrl Pts',(-14.8111650040805,-13.0951747198527,
115.97263957887)) ;
#161921 = CARTESIAN_POINT('Ctrl Pts',(-14.8849688527101,-13.0951746676827,
115.948408553052)) ;
#161922 = CARTESIAN_POINT('Ctrl Pts',(-14.8624846473298,-13.0713759102982,
115.879925290218)) ;
#161923 = CARTESIAN_POINT('Ctrl Pts',(-14.8400004419496,-13.0475771529138,
115.811442027384)) ;
#161924 = CARTESIAN_POINT('Ctrl Pts',(-14.76619659332,-13.0475772050838,115.835673053202)) ;
#161925 = CARTESIAN_POINT('Ctrl Pts',(-14.6923927446904,-13.0475772572539,
115.859904079021)) ;
#161926 = CARTESIAN_POINT('Ctrl Pts',(-14.7148769500706,-13.0713760146383,
115.928387341854)) ;
#161927 = CARTESIAN_POINT('Ctrl Pts',(-14.7656221631295,-12.8101300373193,
116.047465559082)) ;
#161928 = CARTESIAN_POINT('Ctrl Pts',(-14.785330177933,-12.852202961782,116.107492993524)) ;
#161929 = CARTESIAN_POINT('Ctrl Pts',(-14.8591340322195,-12.8522029087301,
116.083261984936)) ;
#161930 = CARTESIAN_POINT('Ctrl Pts',(-14.9329378865061,-12.8522028556782,
116.059030976348)) ;
#161931 = CARTESIAN_POINT('Ctrl Pts',(-14.9132298717026,-12.8101299312156,
115.999003541906)) ;
#161932 = CARTESIAN_POINT('Ctrl Pts',(-14.8935218568992,-12.7680570067529,
115.938976107465)) ;
#161933 = CARTESIAN_POINT('Ctrl Pts',(-14.8197180026126,-12.7680570598048,
115.963207116053)) ;
#161934 = CARTESIAN_POINT('Ctrl Pts',(-14.745914148326,-12.7680571128567,
115.987438124641)) ;
#161935 = CARTESIAN_POINT('Ctrl Pts',(-14.7656221631295,-12.8101300373193,
116.047465559082)) ;
#161936 = CARTESIAN_POINT('Ctrl Pts',(-14.836499389826,-12.5926203368979,
116.227885615043)) ;
#161937 = CARTESIAN_POINT('Ctrl Pts',(-14.8520211846851,-12.6499401722223,
116.275162499135)) ;
#161938 = CARTESIAN_POINT('Ctrl Pts',(-14.9258250448979,-12.6499401250942,
116.250931508597)) ;
#161939 = CARTESIAN_POINT('Ctrl Pts',(-14.9996289051108,-12.6499400779661,
116.22670051806)) ;
#161940 = CARTESIAN_POINT('Ctrl Pts',(-14.9841071102517,-12.5926202426416,
116.179423633968)) ;
#161941 = CARTESIAN_POINT('Ctrl Pts',(-14.9685853153926,-12.5353004073172,
116.132146749876)) ;
#161942 = CARTESIAN_POINT('Ctrl Pts',(-14.8947814551798,-12.5353004544453,
116.156377740414)) ;
#161943 = CARTESIAN_POINT('Ctrl Pts',(-14.820977594967,-12.5353005015734,
116.180608730951)) ;
#161944 = CARTESIAN_POINT('Ctrl Pts',(-14.836499389826,-12.5926203368979,
116.227885615043)) ;
#161945 = CARTESIAN_POINT('Ctrl Pts',(-14.9232190242914,-12.4341144288436,
116.456553356206)) ;
#161946 = CARTESIAN_POINT('Ctrl Pts',(-14.9334426620929,-12.5025837722115,
116.487692908903)) ;
#161947 = CARTESIAN_POINT('Ctrl Pts',(-15.0072465277716,-12.5025837377898,
116.463461935014)) ;
#161948 = CARTESIAN_POINT('Ctrl Pts',(-15.0810503934502,-12.502583703368,
116.439230961124)) ;
#161949 = CARTESIAN_POINT('Ctrl Pts',(-15.0708267556487,-12.4341143600001,
116.408091408427)) ;
#161950 = CARTESIAN_POINT('Ctrl Pts',(-15.0606031178471,-12.3656450166321,
116.37695185573)) ;
#161951 = CARTESIAN_POINT('Ctrl Pts',(-14.9867992521685,-12.3656450510539,
116.40118282962)) ;
#161952 = CARTESIAN_POINT('Ctrl Pts',(-14.9129953864899,-12.3656450854756,
116.425413803509)) ;
#161953 = CARTESIAN_POINT('Ctrl Pts',(-14.9232190242914,-12.4341144288436,
116.456553356206)) ;
#161954 = CARTESIAN_POINT('Ctrl Pts',(-15.0204191933641,-12.346259851331,
116.717108536912)) ;
#161955 = CARTESIAN_POINT('Ctrl Pts',(-15.0246060505222,-12.4209624752005,
116.729861029938)) ;
#161956 = CARTESIAN_POINT('Ctrl Pts',(-15.0984099204493,-12.4209624599237,
116.705630068989)) ;
#161957 = CARTESIAN_POINT('Ctrl Pts',(-15.1722137903763,-12.4209624446469,
116.681399108039)) ;
#161958 = CARTESIAN_POINT('Ctrl Pts',(-15.1680269332182,-12.3462598207773,
116.668646615013)) ;
#161959 = CARTESIAN_POINT('Ctrl Pts',(-15.1638400760601,-12.2715571969078,
116.655894121986)) ;
#161960 = CARTESIAN_POINT('Ctrl Pts',(-15.090036206133,-12.2715572121846,
116.680125082936)) ;
#161961 = CARTESIAN_POINT('Ctrl Pts',(-15.016232336206,-12.2715572274614,
116.704356043885)) ;
#161962 = CARTESIAN_POINT('Ctrl Pts',(-15.0204191933641,-12.346259851331,
116.717108536912)) ;
#161963 = CARTESIAN_POINT('Ctrl Pts',(-15.1212516203235,-12.3348158852733,
116.98892332195)) ;
#161964 = CARTESIAN_POINT('Ctrl Pts',(-15.1191352709603,-12.4104256805368,
116.982477265032)) ;
#161965 = CARTESIAN_POINT('Ctrl Pts',(-15.1929391428361,-12.4104256886821,
116.958246310018)) ;
#161966 = CARTESIAN_POINT('Ctrl Pts',(-15.266743014712,-12.4104256968275,
116.934015355004)) ;
#161967 = CARTESIAN_POINT('Ctrl Pts',(-15.2688593640751,-12.334815901564,
116.940461411923)) ;
#161968 = CARTESIAN_POINT('Ctrl Pts',(-15.2709757134383,-12.2592061063006,
116.946907468841)) ;
#161969 = CARTESIAN_POINT('Ctrl Pts',(-15.1971718415625,-12.2592060981552,
116.971138423855)) ;
#161970 = CARTESIAN_POINT('Ctrl Pts',(-15.1233679696867,-12.2592060900098,
116.995369378869)) ;
#161971 = CARTESIAN_POINT('Ctrl Pts',(-15.1212516203235,-12.3348158852733,
116.98892332195)) ;
#161972 = CARTESIAN_POINT('Ctrl Pts',(-15.2210253617375,-12.4019396871859,
117.257046128186)) ;
#161973 = CARTESIAN_POINT('Ctrl Pts',(-15.2126803008155,-12.4729745049504,
117.231628420995)) ;
#161974 = CARTESIAN_POINT('Ctrl Pts',(-15.2864841729896,-12.4729745398318,
117.207397466889)) ;
#161975 = CARTESIAN_POINT('Ctrl Pts',(-15.3602880451638,-12.4729745747131,
117.183166512784)) ;
#161976 = CARTESIAN_POINT('Ctrl Pts',(-15.3686331060857,-12.4019397569486,
117.208584219976)) ;
#161977 = CARTESIAN_POINT('Ctrl Pts',(-15.3769781670076,-12.330904939184,
117.234001927168)) ;
#161978 = CARTESIAN_POINT('Ctrl Pts',(-15.3031742948335,-12.3309049043027,
117.258232881273)) ;
#161979 = CARTESIAN_POINT('Ctrl Pts',(-15.2293704226594,-12.3309048694214,
117.282463835378)) ;
#161980 = CARTESIAN_POINT('Ctrl Pts',(-15.2210253617375,-12.4019396871859,
117.257046128186)) ;
#161981 = CARTESIAN_POINT('Ctrl Pts',(-15.3104774186011,-12.5400212389952,
117.494364772624)) ;
#161982 = CARTESIAN_POINT('Ctrl Pts',(-15.2966020261323,-12.6015185806479,
117.452102567907)) ;
#161983 = CARTESIAN_POINT('Ctrl Pts',(-15.3704058950722,-12.6015186402617,
117.427871603951)) ;
#161984 = CARTESIAN_POINT('Ctrl Pts',(-15.4442097640122,-12.6015186998755,
117.403640639995)) ;
#161985 = CARTESIAN_POINT('Ctrl Pts',(-15.458085156481,-12.5400213582228,
117.445902844712)) ;
#161986 = CARTESIAN_POINT('Ctrl Pts',(-15.4719605489497,-12.4785240165702,
117.488165049428)) ;
#161987 = CARTESIAN_POINT('Ctrl Pts',(-15.3981566800098,-12.4785239569564,
117.512396013384)) ;
#161988 = CARTESIAN_POINT('Ctrl Pts',(-15.3243528110698,-12.4785238973426,
117.53662697734)) ;
#161989 = CARTESIAN_POINT('Ctrl Pts',(-15.3104774186011,-12.5400212389952,
117.494364772624)) ;
#161990 = CARTESIAN_POINT('Ctrl Pts',(-15.386781464252,-12.7426569389483,
117.691155444074)) ;
#161991 = CARTESIAN_POINT('Ctrl Pts',(-15.368295445562,-12.790097789664,117.634850015886)) ;
#161992 = CARTESIAN_POINT('Ctrl Pts',(-15.4420993094136,-12.7900978720305,
117.610619036432)) ;
#161993 = CARTESIAN_POINT('Ctrl Pts',(-15.5159031732653,-12.790097954397,
117.586388056978)) ;
#161994 = CARTESIAN_POINT('Ctrl Pts',(-15.5343891919552,-12.7426571036813,
117.642693485165)) ;
#161995 = CARTESIAN_POINT('Ctrl Pts',(-15.5528752106452,-12.6952162529655,
117.698998913352)) ;
#161996 = CARTESIAN_POINT('Ctrl Pts',(-15.4790713467936,-12.695216170599,
117.723229892807)) ;
#161997 = CARTESIAN_POINT('Ctrl Pts',(-15.405267482942,-12.6952160882325,
117.747460872261)) ;
#161998 = CARTESIAN_POINT('Ctrl Pts',(-15.386781464252,-12.7426569389483,
117.691155444074)) ;
#161999 = CARTESIAN_POINT('Ctrl Pts',(-15.4435452552671,-12.9928209893326,
117.828633943598)) ;
#162000 = CARTESIAN_POINT('Ctrl Pts',(-15.4218018018575,-13.0228660525859,
117.762406894878)) ;
#162001 = CARTESIAN_POINT('Ctrl Pts',(-15.4956056583648,-13.0228661512881,
117.738175893054)) ;
#162002 = CARTESIAN_POINT('Ctrl Pts',(-15.569409514872,-13.0228662499903,
117.71394489123)) ;
#162003 = CARTESIAN_POINT('Ctrl Pts',(-15.5911529682816,-12.992821186737,
117.78017193995)) ;
#162004 = CARTESIAN_POINT('Ctrl Pts',(-15.6128964216912,-12.9627761234838,
117.846398988669)) ;
#162005 = CARTESIAN_POINT('Ctrl Pts',(-15.5390925651839,-12.9627760247816,
117.870629990493)) ;
#162006 = CARTESIAN_POINT('Ctrl Pts',(-15.4652887086767,-12.9627759260794,
117.894860992317)) ;
#162007 = CARTESIAN_POINT('Ctrl Pts',(-15.4435452552671,-12.9928209893326,
117.828633943598)) ;
#162008 = CARTESIAN_POINT('Ctrl Pts',(-15.4780991318046,-13.274121349933,
117.89835399274)) ;
#162009 = CARTESIAN_POINT('Ctrl Pts',(-15.454646181204,-13.2845716251807,
117.826920091425)) ;
#162010 = CARTESIAN_POINT('Ctrl Pts',(-15.5284500290858,-13.2845717326201,
117.80268906333)) ;
#162011 = CARTESIAN_POINT('Ctrl Pts',(-15.6022538769677,-13.2845718400594,
117.778458035234)) ;
#162012 = CARTESIAN_POINT('Ctrl Pts',(-15.6257068275682,-13.2741215648117,
117.849891936549)) ;
#162013 = CARTESIAN_POINT('Ctrl Pts',(-15.6491597781688,-13.263671289564,
117.921325837863)) ;
#162014 = CARTESIAN_POINT('Ctrl Pts',(-15.5753559302869,-13.2636711821247,
117.945556865959)) ;
#162015 = CARTESIAN_POINT('Ctrl Pts',(-15.5015520824051,-13.2636710746853,
117.969787894055)) ;
#162016 = CARTESIAN_POINT('Ctrl Pts',(-15.4780991318046,-13.274121349933,
117.89835399274)) ;
#162017 = CARTESIAN_POINT('Ctrl Pts',(-15.4884434105682,-13.5650423075934,
117.894429498399)) ;
#162018 = CARTESIAN_POINT('Ctrl Pts',(-15.4649666718816,-13.5551969668732,
117.822923142409)) ;
#162019 = CARTESIAN_POINT('Ctrl Pts',(-15.5387705106964,-13.555197074088,
117.798692086697)) ;
#162020 = CARTESIAN_POINT('Ctrl Pts',(-15.6125743495112,-13.5551971813029,
117.774461030985)) ;
#162021 = CARTESIAN_POINT('Ctrl Pts',(-15.6360510881978,-13.5650425220231,
117.845967386975)) ;
#162022 = CARTESIAN_POINT('Ctrl Pts',(-15.6595278268843,-13.5748878627432,
117.917473742965)) ;
#162023 = CARTESIAN_POINT('Ctrl Pts',(-15.5857239880695,-13.5748877555284,
117.941704798677)) ;
#162024 = CARTESIAN_POINT('Ctrl Pts',(-15.5119201492547,-13.5748876483136,
117.965935854389)) ;
#162025 = CARTESIAN_POINT('Ctrl Pts',(-15.4884434105682,-13.5650423075934,
117.894429498399)) ;
#162026 = CARTESIAN_POINT('Ctrl Pts',(-15.4747873042015,-13.8454220244642,
117.817406765733)) ;
#162027 = CARTESIAN_POINT('Ctrl Pts',(-15.4529622075996,-13.8159869229919,
117.750931045019)) ;
#162028 = CARTESIAN_POINT('Ctrl Pts',(-15.5267660378298,-13.8159870213789,
117.72669996316)) ;
#162029 = CARTESIAN_POINT('Ctrl Pts',(-15.60056986806,-13.8159871197658,117.7024688813)) ;
#162030 = CARTESIAN_POINT('Ctrl Pts',(-15.622394964662,-13.8454222212381,
117.768944602014)) ;
#162031 = CARTESIAN_POINT('Ctrl Pts',(-15.644220061264,-13.8748573227103,
117.835420322728)) ;
#162032 = CARTESIAN_POINT('Ctrl Pts',(-15.5704162310338,-13.8748572243234,
117.859651404588)) ;
#162033 = CARTESIAN_POINT('Ctrl Pts',(-15.4966124008035,-13.8748571259364,
117.883882486447)) ;
#162034 = CARTESIAN_POINT('Ctrl Pts',(-15.4747873042015,-13.8454220244642,
117.817406765733)) ;
#162035 = CARTESIAN_POINT('Ctrl Pts',(-15.4387248228193,-14.095635489283,
117.672076552588)) ;
#162036 = CARTESIAN_POINT('Ctrl Pts',(-15.4201192687897,-14.0486874017416,
117.615407039032)) ;
#162037 = CARTESIAN_POINT('Ctrl Pts',(-15.4939230917936,-14.0486874834364,
117.591175935163)) ;
#162038 = CARTESIAN_POINT('Ctrl Pts',(-15.5677269147975,-14.0486875651311,
117.566944831293)) ;
#162039 = CARTESIAN_POINT('Ctrl Pts',(-15.5863324688271,-14.0956356526725,
117.623614344849)) ;
#162040 = CARTESIAN_POINT('Ctrl Pts',(-15.6049380228566,-14.1425837402138,
117.680283858405)) ;
#162041 = CARTESIAN_POINT('Ctrl Pts',(-15.5311341998527,-14.1425836585191,
117.704514962275)) ;
#162042 = CARTESIAN_POINT('Ctrl Pts',(-15.4573303768488,-14.1425835768243,
117.728746066145)) ;
#162043 = CARTESIAN_POINT('Ctrl Pts',(-15.4387248228193,-14.095635489283,
117.672076552588)) ;
#162044 = CARTESIAN_POINT('Ctrl Pts',(-15.3836965141025,-14.2970558104585,
117.469021551389)) ;
#162045 = CARTESIAN_POINT('Ctrl Pts',(-15.3696385446302,-14.2359749683573,
117.426203246579)) ;
#162046 = CARTESIAN_POINT('Ctrl Pts',(-15.4434423624372,-14.2359750277231,
117.40197212688)) ;
#162047 = CARTESIAN_POINT('Ctrl Pts',(-15.5172461802443,-14.2359750870889,
117.377741007182)) ;
#162048 = CARTESIAN_POINT('Ctrl Pts',(-15.5313041497167,-14.2970559291901,
117.420559311992)) ;
#162049 = CARTESIAN_POINT('Ctrl Pts',(-15.545362119189,-14.3581367712912,
117.463377616802)) ;
#162050 = CARTESIAN_POINT('Ctrl Pts',(-15.471558301382,-14.3581367119255,
117.487608736501)) ;
#162051 = CARTESIAN_POINT('Ctrl Pts',(-15.3977544835749,-14.3581366525597,
117.511839856199)) ;
#162052 = CARTESIAN_POINT('Ctrl Pts',(-15.3836965141025,-14.2970558104585,
117.469021551389)) ;
#162053 = CARTESIAN_POINT('Ctrl Pts',(-15.3141371945857,-14.4359480747077,
117.221601988843)) ;
#162054 = CARTESIAN_POINT('Ctrl Pts',(-15.3056501747108,-14.3650783452255,
117.195751897542)) ;
#162055 = CARTESIAN_POINT('Ctrl Pts',(-15.3794539899394,-14.3650783787337,
117.17152076999)) ;
#162056 = CARTESIAN_POINT('Ctrl Pts',(-15.453257805168,-14.3650784122419,
117.147289642437)) ;
#162057 = CARTESIAN_POINT('Ctrl Pts',(-15.4617448250429,-14.4359481417242,
117.173139733739)) ;
#162058 = CARTESIAN_POINT('Ctrl Pts',(-15.4702318449178,-14.5068178712064,
117.19898982504)) ;
#162059 = CARTESIAN_POINT('Ctrl Pts',(-15.3964280296892,-14.5068178376981,
117.223220952592)) ;
#162060 = CARTESIAN_POINT('Ctrl Pts',(-15.3226242144606,-14.5068178041899,
117.247452080144)) ;
#162061 = CARTESIAN_POINT('Ctrl Pts',(-15.3141371945857,-14.4359480747077,
117.221601988843)) ;
#162062 = CARTESIAN_POINT('Ctrl Pts',(-15.2359817859273,-14.501304829004,
116.948020668741)) ;
#162063 = CARTESIAN_POINT('Ctrl Pts',(-15.2336738762587,-14.4257651981435,
116.940991150015)) ;
#162064 = CARTESIAN_POINT('Ctrl Pts',(-15.3074776916091,-14.4257652059426,
116.916760022834)) ;
#162065 = CARTESIAN_POINT('Ctrl Pts',(-15.3812815069595,-14.4257652137418,
116.892528895653)) ;
#162066 = CARTESIAN_POINT('Ctrl Pts',(-15.3835894166281,-14.5013048446024,
116.899558414379)) ;
#162067 = CARTESIAN_POINT('Ctrl Pts',(-15.3858973262967,-14.576844475463,
116.906587933104)) ;
#162068 = CARTESIAN_POINT('Ctrl Pts',(-15.3120935109463,-14.5768444676638,
116.930819060286)) ;
#162069 = CARTESIAN_POINT('Ctrl Pts',(-15.2382896955959,-14.5768444598646,
116.955050187467)) ;
#162070 = CARTESIAN_POINT('Ctrl Pts',(-15.2359817859273,-14.501304829004,
116.948020668741)) ;
#162071 = CARTESIAN_POINT('Ctrl Pts',(-15.1561240539043,-14.4893139259723,
116.669494222094)) ;
#162072 = CARTESIAN_POINT('Ctrl Pts',(-15.1601185367574,-14.4144981524163,
116.681660774003)) ;
#162073 = CARTESIAN_POINT('Ctrl Pts',(-15.2339223540431,-14.4144981369881,
116.657429652717)) ;
#162074 = CARTESIAN_POINT('Ctrl Pts',(-15.3077261713288,-14.4144981215599,
116.63319853143)) ;
#162075 = CARTESIAN_POINT('Ctrl Pts',(-15.3037316884757,-14.4893138951159,
116.621031979521)) ;
#162076 = CARTESIAN_POINT('Ctrl Pts',(-15.2997372056226,-14.564129668672,
116.608865427612)) ;
#162077 = CARTESIAN_POINT('Ctrl Pts',(-15.2259333883369,-14.5641296841002,
116.633096548898)) ;
#162078 = CARTESIAN_POINT('Ctrl Pts',(-15.1521295710511,-14.5641296995284,
116.657327670185)) ;
#162079 = CARTESIAN_POINT('Ctrl Pts',(-15.1561240539043,-14.4893139259723,
116.669494222094)) ;
#162080 = CARTESIAN_POINT('Ctrl Pts',(-15.0799694117837,-14.4004454436412,
116.401998946719)) ;
#162081 = CARTESIAN_POINT('Ctrl Pts',(-15.090022382406,-14.3317211347541,
116.432618674691)) ;
#162082 = CARTESIAN_POINT('Ctrl Pts',(-15.1638262040758,-14.331721100851,
116.408387566758)) ;
#162083 = CARTESIAN_POINT('Ctrl Pts',(-15.2376300257455,-14.331721066948,
116.384156458824)) ;
#162084 = CARTESIAN_POINT('Ctrl Pts',(-15.2275770551231,-14.4004453758351,
116.353536730852)) ;
#162085 = CARTESIAN_POINT('Ctrl Pts',(-15.2175240845008,-14.4691696847222,
116.322917002879)) ;
#162086 = CARTESIAN_POINT('Ctrl Pts',(-15.143720262831,-14.4691697186253,
116.347148110813)) ;
#162087 = CARTESIAN_POINT('Ctrl Pts',(-15.0699164411613,-14.4691697525284,
116.371379218746)) ;
#162088 = CARTESIAN_POINT('Ctrl Pts',(-15.0799694117837,-14.4004454436412,
116.401998946719)) ;
#162089 = CARTESIAN_POINT('Ctrl Pts',(-15.0146075791838,-14.2418718140722,
116.167568446909)) ;
#162090 = CARTESIAN_POINT('Ctrl Pts',(-15.0299707183661,-14.1841154082224,
116.214362091392)) ;
#162091 = CARTESIAN_POINT('Ctrl Pts',(-15.1037745452079,-14.1841153614757,
116.190130999212)) ;
#162092 = CARTESIAN_POINT('Ctrl Pts',(-15.1775783720496,-14.1841153147289,
116.165899907032)) ;
#162093 = CARTESIAN_POINT('Ctrl Pts',(-15.1622152328674,-14.2418717205788,
116.119106262548)) ;
#162094 = CARTESIAN_POINT('Ctrl Pts',(-15.1468520936851,-14.2996281264286,
116.072312618065)) ;
#162095 = CARTESIAN_POINT('Ctrl Pts',(-15.0730482668433,-14.2996281731753,
116.096543710245)) ;
#162096 = CARTESIAN_POINT('Ctrl Pts',(-14.9992444400016,-14.299628219922,
116.120774802425)) ;
#162097 = CARTESIAN_POINT('Ctrl Pts',(-15.0146075791838,-14.2418718140722,
116.167568446909)) ;
#162098 = CARTESIAN_POINT('Ctrl Pts',(-14.9647824826636,-14.0233785235775,
115.98025836275)) ;
#162099 = CARTESIAN_POINT('Ctrl Pts',(-14.9843833842169,-13.9807896305814,
116.039959547481)) ;
#162100 = CARTESIAN_POINT('Ctrl Pts',(-15.0581872171145,-13.9807895787785,
116.015728473746)) ;
#162101 = CARTESIAN_POINT('Ctrl Pts',(-15.1319910500122,-13.9807895269757,
115.991497400011)) ;
#162102 = CARTESIAN_POINT('Ctrl Pts',(-15.1123901484589,-14.0233784199718,
115.93179621528)) ;
#162103 = CARTESIAN_POINT('Ctrl Pts',(-15.0927892469056,-14.0659673129679,
115.872095030548)) ;
#162104 = CARTESIAN_POINT('Ctrl Pts',(-15.018985414008,-14.0659673647708,
115.896326104283)) ;
#162105 = CARTESIAN_POINT('Ctrl Pts',(-14.9451815811103,-14.0659674165736,
115.920557178019)) ;
#162106 = CARTESIAN_POINT('Ctrl Pts',(-14.9647824826636,-14.0233785235775,
115.98025836275)) ;
#162107 = CARTESIAN_POINT('Ctrl Pts',(-14.9353130383132,-13.7618917263419,
115.855036424513)) ;
#162108 = CARTESIAN_POINT('Ctrl Pts',(-14.9577350844152,-13.7374955038548,
115.923330360184)) ;
#162109 = CARTESIAN_POINT('Ctrl Pts',(-15.0315389228224,-13.7374954531261,
115.89909930323)) ;
#162110 = CARTESIAN_POINT('Ctrl Pts',(-15.1053427612296,-13.7374954023974,
115.874868246276)) ;
#162111 = CARTESIAN_POINT('Ctrl Pts',(-15.0829207151276,-13.7618916248845,
115.806574310605)) ;
#162112 = CARTESIAN_POINT('Ctrl Pts',(-15.0604986690256,-13.7862878473716,
115.738280374933)) ;
#162113 = CARTESIAN_POINT('Ctrl Pts',(-14.9866948306184,-13.7862878981003,
115.762511431887)) ;
#162114 = CARTESIAN_POINT('Ctrl Pts',(-14.9128909922112,-13.786287948829,
115.786742488841)) ;
#162115 = CARTESIAN_POINT('Ctrl Pts',(-14.9353130383132,-13.7618917263419,
115.855036424513)) ;
#162116 = CARTESIAN_POINT('Ctrl Pts',(-14.9289325059808,-13.4754623735639,
115.800094097423)) ;
#162117 = CARTESIAN_POINT('Ctrl Pts',(-14.9525688879762,-13.471028133492,
115.872086704117)) ;
#162118 = CARTESIAN_POINT('Ctrl Pts',(-15.0263727308896,-13.4710280894286,
115.847855660888)) ;
#162119 = CARTESIAN_POINT('Ctrl Pts',(-15.100176573803,-13.4710280453652,
115.823624617659)) ;
#162120 = CARTESIAN_POINT('Ctrl Pts',(-15.0765401918076,-13.4754622854371,
115.751632010965)) ;
#162121 = CARTESIAN_POINT('Ctrl Pts',(-15.0529038098122,-13.479896525509,
115.679639404272)) ;
#162122 = CARTESIAN_POINT('Ctrl Pts',(-14.9790999668988,-13.4798965695724,
115.703870447501)) ;
#162123 = CARTESIAN_POINT('Ctrl Pts',(-14.9052961239854,-13.4798966136358,
115.728101490729)) ;
#162124 = CARTESIAN_POINT('Ctrl Pts',(-14.9289325059808,-13.4754623735639,
115.800094097423)) ;
#162125 = CARTESIAN_POINT('Ctrl Pts',(-14.9467156400316,-13.1862230579374,
115.818918808621)) ;
#162126 = CARTESIAN_POINT('Ctrl Pts',(-14.9698774007745,-13.2019774295457,
115.889465795415)) ;
#162127 = CARTESIAN_POINT('Ctrl Pts',(-15.0436812468443,-13.2019773939464,
115.8652347618)) ;
#162128 = CARTESIAN_POINT('Ctrl Pts',(-15.1174850929142,-13.2019773583471,
115.841003728185)) ;
#162129 = CARTESIAN_POINT('Ctrl Pts',(-15.0943233321713,-13.1862229867387,
115.770456741391)) ;
#162130 = CARTESIAN_POINT('Ctrl Pts',(-15.0711615714284,-13.1704686151304,
115.699909754597)) ;
#162131 = CARTESIAN_POINT('Ctrl Pts',(-14.9973577253585,-13.1704686507297,
115.724140788212)) ;
#162132 = CARTESIAN_POINT('Ctrl Pts',(-14.9235538792887,-13.170468686329,
115.748371821826)) ;
#162133 = CARTESIAN_POINT('Ctrl Pts',(-14.9467156400316,-13.1862230579374,
115.818918808621)) ;
#162134 = CARTESIAN_POINT('Ctrl Pts',(-14.9883696704994,-12.9121173454345,
115.910257352319)) ;
#162135 = CARTESIAN_POINT('Ctrl Pts',(-15.0093934840061,-12.9470346448942,
115.974292496613)) ;
#162136 = CARTESIAN_POINT('Ctrl Pts',(-15.0831973316234,-12.947034620835,
115.950061467711)) ;
#162137 = CARTESIAN_POINT('Ctrl Pts',(-15.1570011792406,-12.9470345967758,
115.925830438809)) ;
#162138 = CARTESIAN_POINT('Ctrl Pts',(-15.1359773657339,-12.9121172973162,
115.861795294515)) ;
#162139 = CARTESIAN_POINT('Ctrl Pts',(-15.1149535522271,-12.8771999978565,
115.797760150221)) ;
#162140 = CARTESIAN_POINT('Ctrl Pts',(-15.0411497046099,-12.8772000219157,
115.821991179123)) ;
#162141 = CARTESIAN_POINT('Ctrl Pts',(-14.9673458569927,-12.8772000459749,
115.846222208024)) ;
#162142 = CARTESIAN_POINT('Ctrl Pts',(-14.9883696704994,-12.9121173454345,
115.910257352319)) ;
#162143 = CARTESIAN_POINT('Ctrl Pts',(-15.0514075082548,-12.6748571224349,
116.066831542999)) ;
#162144 = CARTESIAN_POINT('Ctrl Pts',(-15.0687947514386,-12.7263936809792,
116.119790280699)) ;
#162145 = CARTESIAN_POINT('Ctrl Pts',(-15.1425985992495,-12.7263936670357,
116.095559252388)) ;
#162146 = CARTESIAN_POINT('Ctrl Pts',(-15.2164024470604,-12.7263936530922,
116.071328224076)) ;
#162147 = CARTESIAN_POINT('Ctrl Pts',(-15.1990152038766,-12.6748570945479,
116.018369486375)) ;
#162148 = CARTESIAN_POINT('Ctrl Pts',(-15.1816279606928,-12.6233205360036,
115.965410748675)) ;
#162149 = CARTESIAN_POINT('Ctrl Pts',(-15.1078241128819,-12.6233205499471,
115.989641776987)) ;
#162150 = CARTESIAN_POINT('Ctrl Pts',(-15.034020265071,-12.6233205638906,
116.013872805299)) ;
#162151 = CARTESIAN_POINT('Ctrl Pts',(-15.0514075082548,-12.6748571224349,
116.066831542999)) ;
#162152 = CARTESIAN_POINT('Ctrl Pts',(-15.1328444729729,-12.4898752939566,
116.279188009529)) ;
#162153 = CARTESIAN_POINT('Ctrl Pts',(-15.1453102034931,-12.5544068109691,
116.317156613569)) ;
#162154 = CARTESIAN_POINT('Ctrl Pts',(-15.2191140499375,-12.5544068057079,
116.292925581095)) ;
#162155 = CARTESIAN_POINT('Ctrl Pts',(-15.2929178963818,-12.5544068004467,
116.26869454862)) ;
#162156 = CARTESIAN_POINT('Ctrl Pts',(-15.2804521658616,-12.4898752834342,
116.230725944581)) ;
#162157 = CARTESIAN_POINT('Ctrl Pts',(-15.2679864353413,-12.4253437664217,
116.192757340541)) ;
#162158 = CARTESIAN_POINT('Ctrl Pts',(-15.194182588897,-12.4253437716829,
116.216988373016)) ;
#162159 = CARTESIAN_POINT('Ctrl Pts',(-15.1203787424527,-12.4253437769441,
116.24121940549)) ;
#162160 = CARTESIAN_POINT('Ctrl Pts',(-15.1328444729729,-12.4898752939566,
116.279188009529)) ;
#162161 = CARTESIAN_POINT('Ctrl Pts',(-15.2258152326025,-12.3730682967797,
116.527146434279)) ;
#162162 = CARTESIAN_POINT('Ctrl Pts',(-15.2325367436392,-12.4458523869168,
116.547619072512)) ;
#162163 = CARTESIAN_POINT('Ctrl Pts',(-15.3063405890483,-12.4458523855329,
116.523388036884)) ;
#162164 = CARTESIAN_POINT('Ctrl Pts',(-15.3801444344574,-12.445852384149,
116.499157001257)) ;
#162165 = CARTESIAN_POINT('Ctrl Pts',(-15.3734229234207,-12.3730682940119,
116.478684363024)) ;
#162166 = CARTESIAN_POINT('Ctrl Pts',(-15.366701412384,-12.3002842038747,
116.458211724791)) ;
#162167 = CARTESIAN_POINT('Ctrl Pts',(-15.2928975669749,-12.3002842052586,
116.482442760418)) ;
#162168 = CARTESIAN_POINT('Ctrl Pts',(-15.2190937215657,-12.3002842066425,
116.506673796046)) ;
#162169 = CARTESIAN_POINT('Ctrl Pts',(-15.2258152326025,-12.3730682967797,
116.527146434279)) ;
#162170 = CARTESIAN_POINT('Ctrl Pts',(-15.3267957548085,-12.330125354393,
116.799022433184)) ;
#162171 = CARTESIAN_POINT('Ctrl Pts',(-15.327214765721,-12.4060180175289,
116.800298672828)) ;
#162172 = CARTESIAN_POINT('Ctrl Pts',(-15.4010186093175,-12.4060180179283,
116.77606763168)) ;
#162173 = CARTESIAN_POINT('Ctrl Pts',(-15.474822452914,-12.4060180183277,
116.751836590531)) ;
#162174 = CARTESIAN_POINT('Ctrl Pts',(-15.4744034420016,-12.3301253551918,
116.750560350888)) ;
#162175 = CARTESIAN_POINT('Ctrl Pts',(-15.4739844310891,-12.2542326920559,
116.749284111245)) ;
#162176 = CARTESIAN_POINT('Ctrl Pts',(-15.4001805874926,-12.2542326916565,
116.773515152393)) ;
#162177 = CARTESIAN_POINT('Ctrl Pts',(-15.326376743896,-12.2542326912571,
116.797746193541)) ;
#162178 = CARTESIAN_POINT('Ctrl Pts',(-15.3267957548085,-12.330125354393,
116.799022433184)) ;
#162179 = CARTESIAN_POINT('Ctrl Pts',(-15.4267371080215,-12.3650026478225,
117.068234016832)) ;
#162180 = CARTESIAN_POINT('Ctrl Pts',(-15.4209065945382,-12.4385726507877,
117.050475213478)) ;
#162181 = CARTESIAN_POINT('Ctrl Pts',(-15.4947104373962,-12.4385726504867,
117.02624417008)) ;
#162182 = CARTESIAN_POINT('Ctrl Pts',(-15.5685142802541,-12.4385726501857,
117.002013126682)) ;
#162183 = CARTESIAN_POINT('Ctrl Pts',(-15.5743447937374,-12.3650026472205,
117.019771930036)) ;
#162184 = CARTESIAN_POINT('Ctrl Pts',(-15.5801753072207,-12.2914326442552,
117.037530733391)) ;
#162185 = CARTESIAN_POINT('Ctrl Pts',(-15.5063714643627,-12.2914326445563,
117.061761776789)) ;
#162186 = CARTESIAN_POINT('Ctrl Pts',(-15.4325676215048,-12.2914326448573,
117.085992820186)) ;
#162187 = CARTESIAN_POINT('Ctrl Pts',(-15.4267371080215,-12.3650026478225,
117.068234016832)) ;
#162188 = CARTESIAN_POINT('Ctrl Pts',(-15.5220396277674,-12.4764750890778,
117.322748096145)) ;
#162189 = CARTESIAN_POINT('Ctrl Pts',(-15.5102853182541,-12.5423709931459,
117.286946365851)) ;
#162190 = CARTESIAN_POINT('Ctrl Pts',(-15.5840891607112,-12.5423709914641,
117.262715321232)) ;
#162191 = CARTESIAN_POINT('Ctrl Pts',(-15.6578930031683,-12.5423709897823,
117.238484276613)) ;
#162192 = CARTESIAN_POINT('Ctrl Pts',(-15.6696473126816,-12.4764750857142,
117.274286006907)) ;
#162193 = CARTESIAN_POINT('Ctrl Pts',(-15.6814016221949,-12.410579181646,
117.310087737201)) ;
#162194 = CARTESIAN_POINT('Ctrl Pts',(-15.6075977797378,-12.4105791833278,
117.33431878182)) ;
#162195 = CARTESIAN_POINT('Ctrl Pts',(-15.5337939372807,-12.4105791850096,
117.358549826438)) ;
#162196 = CARTESIAN_POINT('Ctrl Pts',(-15.5220396277674,-12.4764750890778,
117.322748096145)) ;
#162197 = CARTESIAN_POINT('Ctrl Pts',(-15.6038717305927,-12.6535586984017,
117.536764515105)) ;
#162198 = CARTESIAN_POINT('Ctrl Pts',(-15.5871151861937,-12.7071860625279,
117.485726784475)) ;
#162199 = CARTESIAN_POINT('Ctrl Pts',(-15.6609190290941,-12.7071860605199,
117.461495741206)) ;
#162200 = CARTESIAN_POINT('Ctrl Pts',(-15.7347228719945,-12.7071860585118,
117.437264697938)) ;
#162201 = CARTESIAN_POINT('Ctrl Pts',(-15.7514794163935,-12.6535586943856,
117.488302428568)) ;
#162202 = CARTESIAN_POINT('Ctrl Pts',(-15.7682359607925,-12.5999313302593,
117.539340159199)) ;
#162203 = CARTESIAN_POINT('Ctrl Pts',(-15.6944321178921,-12.5999313322674,
117.563571202468)) ;
#162204 = CARTESIAN_POINT('Ctrl Pts',(-15.6206282749917,-12.5999313342754,
117.587802245736)) ;
#162205 = CARTESIAN_POINT('Ctrl Pts',(-15.6038717305927,-12.6535586984017,
117.536764515105)) ;
#162206 = CARTESIAN_POINT('Ctrl Pts',(-15.6692705920402,-12.8875907025722,
117.700299247988)) ;
#162207 = CARTESIAN_POINT('Ctrl Pts',(-15.648660558624,-12.9249550568961,
117.637524411639)) ;
#162208 = CARTESIAN_POINT('Ctrl Pts',(-15.7224644022642,-12.9249550576415,
117.613293370624)) ;
#162209 = CARTESIAN_POINT('Ctrl Pts',(-15.7962682459044,-12.9249550583868,
117.589062329609)) ;
#162210 = CARTESIAN_POINT('Ctrl Pts',(-15.8168782793206,-12.887590704063,
117.651837165958)) ;
#162211 = CARTESIAN_POINT('Ctrl Pts',(-15.8374883127368,-12.8502263497391,
117.714612002307)) ;
#162212 = CARTESIAN_POINT('Ctrl Pts',(-15.7636844690966,-12.8502263489938,
117.738843043322)) ;
#162213 = CARTESIAN_POINT('Ctrl Pts',(-15.6898806254564,-12.8502263482484,
117.763074084338)) ;
#162214 = CARTESIAN_POINT('Ctrl Pts',(-15.6692705920402,-12.8875907025722,
117.700299247988)) ;
#162215 = CARTESIAN_POINT('Ctrl Pts',(-15.7128057696858,-13.1564738506933,
117.797702690961)) ;
#162216 = CARTESIAN_POINT('Ctrl Pts',(-15.6898544161461,-13.1751180004759,
117.727796571349)) ;
#162217 = CARTESIAN_POINT('Ctrl Pts',(-15.7636582600179,-13.1751180045343,
117.703565531039)) ;
#162218 = CARTESIAN_POINT('Ctrl Pts',(-15.8374621038898,-13.1751180085928,
117.67933449073)) ;
#162219 = CARTESIAN_POINT('Ctrl Pts',(-15.8604134574295,-13.1564738588101,
117.749240610342)) ;
#162220 = CARTESIAN_POINT('Ctrl Pts',(-15.8833648109692,-13.1378297090275,
117.819146729954)) ;
#162221 = CARTESIAN_POINT('Ctrl Pts',(-15.8095609670974,-13.1378297049691,
117.843377770263)) ;
#162222 = CARTESIAN_POINT('Ctrl Pts',(-15.7357571232256,-13.1378297009107,
117.867608810573)) ;
#162223 = CARTESIAN_POINT('Ctrl Pts',(-15.7128057696858,-13.1564738506933,
117.797702690961)) ;
#162224 = CARTESIAN_POINT('Ctrl Pts',(-15.7332548587096,-13.4476180482474,
117.824312090504)) ;
#162225 = CARTESIAN_POINT('Ctrl Pts',(-15.709580261815,-13.4459601626287,
117.752203088467)) ;
#162226 = CARTESIAN_POINT('Ctrl Pts',(-15.7833841053314,-13.4459601740975,
117.727972047075)) ;
#162227 = CARTESIAN_POINT('Ctrl Pts',(-15.8571879488478,-13.4459601855664,
117.703741005682)) ;
#162228 = CARTESIAN_POINT('Ctrl Pts',(-15.8808625457424,-13.4476180711851,
117.77585000772)) ;
#162229 = CARTESIAN_POINT('Ctrl Pts',(-15.904537142637,-13.4492759568038,
117.847959009757)) ;
#162230 = CARTESIAN_POINT('Ctrl Pts',(-15.8307332991206,-13.4492759453349,
117.872190051149)) ;
#162231 = CARTESIAN_POINT('Ctrl Pts',(-15.7569294556042,-13.4492759338661,
117.896421092541)) ;
#162232 = CARTESIAN_POINT('Ctrl Pts',(-15.7332548587096,-13.4476180482474,
117.824312090504)) ;
#162233 = CARTESIAN_POINT('Ctrl Pts',(-15.7291353924876,-13.7346448783816,
117.776350799521)) ;
#162234 = CARTESIAN_POINT('Ctrl Pts',(-15.7064469536668,-13.7129435340765,
117.707245475991)) ;
#162235 = CARTESIAN_POINT('Ctrl Pts',(-15.7802507956075,-13.7129435517169,
117.6830144298)) ;
#162236 = CARTESIAN_POINT('Ctrl Pts',(-15.8540546375481,-13.7129435693573,
117.658783383608)) ;
#162237 = CARTESIAN_POINT('Ctrl Pts',(-15.8767430763689,-13.7346449136625,
117.727888707137)) ;
#162238 = CARTESIAN_POINT('Ctrl Pts',(-15.8994315151896,-13.7563462579677,
117.796994030667)) ;
#162239 = CARTESIAN_POINT('Ctrl Pts',(-15.8256276732489,-13.7563462403272,
117.821225076858)) ;
#162240 = CARTESIAN_POINT('Ctrl Pts',(-15.7518238313083,-13.7563462226868,
117.84545612305)) ;
#162241 = CARTESIAN_POINT('Ctrl Pts',(-15.7291353924876,-13.7346448783816,
117.776350799521)) ;
#162242 = CARTESIAN_POINT('Ctrl Pts',(-15.7018297830167,-13.9993799399049,
117.657715317448)) ;
#162243 = CARTESIAN_POINT('Ctrl Pts',(-15.6817489265485,-13.9591628378215,
117.596552269184)) ;
#162244 = CARTESIAN_POINT('Ctrl Pts',(-15.7555527657976,-13.9591628601971,
117.572321214794)) ;
#162245 = CARTESIAN_POINT('Ctrl Pts',(-15.8293566050468,-13.9591628825727,
117.548090160405)) ;
#162246 = CARTESIAN_POINT('Ctrl Pts',(-15.849437461515,-13.9993799846561,
117.609253208669)) ;
#162247 = CARTESIAN_POINT('Ctrl Pts',(-15.8695183179831,-14.0395970867396,
117.670416256934)) ;
#162248 = CARTESIAN_POINT('Ctrl Pts',(-15.795714478734,-14.0395970643639,
117.694647311323)) ;
#162249 = CARTESIAN_POINT('Ctrl Pts',(-15.7219106394849,-14.0395970419883,
117.718878365713)) ;
#162250 = CARTESIAN_POINT('Ctrl Pts',(-15.7018297830167,-13.9993799399049,
117.657715317448)) ;
#162251 = CARTESIAN_POINT('Ctrl Pts',(-15.6540905337258,-14.2219559568416,
117.476929036007)) ;
#162252 = CARTESIAN_POINT('Ctrl Pts',(-15.6380460071677,-14.1661403968853,
117.428059997535)) ;
#162253 = CARTESIAN_POINT('Ctrl Pts',(-15.7118498429771,-14.1661404199882,
117.403828932668)) ;
#162254 = CARTESIAN_POINT('Ctrl Pts',(-15.7856536787865,-14.166140443091,
117.379597867802)) ;
#162255 = CARTESIAN_POINT('Ctrl Pts',(-15.8016982053447,-14.2219560030472,
117.428466906274)) ;
#162256 = CARTESIAN_POINT('Ctrl Pts',(-15.8177427319028,-14.2777715630035,
117.477335944747)) ;
#162257 = CARTESIAN_POINT('Ctrl Pts',(-15.7439388960934,-14.2777715399007,
117.501567009613)) ;
#162258 = CARTESIAN_POINT('Ctrl Pts',(-15.6701350602839,-14.2777715167979,
117.525798074479)) ;
#162259 = CARTESIAN_POINT('Ctrl Pts',(-15.6540905337258,-14.2219559568416,
117.476929036007)) ;
#162260 = CARTESIAN_POINT('Ctrl Pts',(-15.5899295337492,-14.3877271051732,
117.246044868715)) ;
#162261 = CARTESIAN_POINT('Ctrl Pts',(-15.5790752953713,-14.3202567503196,
117.212984610756)) ;
#162262 = CARTESIAN_POINT('Ctrl Pts',(-15.652879127185,-14.3202567702551,
117.188753533719)) ;
#162263 = CARTESIAN_POINT('Ctrl Pts',(-15.7266829589986,-14.3202567901906,
117.164522456682)) ;
#162264 = CARTESIAN_POINT('Ctrl Pts',(-15.7375371973765,-14.3877271450442,
117.197582714642)) ;
#162265 = CARTESIAN_POINT('Ctrl Pts',(-15.7483914357544,-14.4551974998978,
117.230642972601)) ;
#162266 = CARTESIAN_POINT('Ctrl Pts',(-15.6745876039407,-14.4551974799623,
117.254874049638)) ;
#162267 = CARTESIAN_POINT('Ctrl Pts',(-15.6007837721271,-14.4551974600268,
117.279105126675)) ;
#162268 = CARTESIAN_POINT('Ctrl Pts',(-15.5899295337492,-14.3877271051732,
117.246044868715)) ;
#162269 = CARTESIAN_POINT('Ctrl Pts',(-15.5142887883934,-14.4840522417127,
116.980008252819)) ;
#162270 = CARTESIAN_POINT('Ctrl Pts',(-15.5094376169318,-14.4097585017527,
116.965232368298)) ;
#162271 = CARTESIAN_POINT('Ctrl Pts',(-15.583241444289,-14.4097585129656,
116.941001277688)) ;
#162272 = CARTESIAN_POINT('Ctrl Pts',(-15.6570452716462,-14.4097585241785,
116.916770187077)) ;
#162273 = CARTESIAN_POINT('Ctrl Pts',(-15.6618964431078,-14.4840522641385,
116.931546071598)) ;
#162274 = CARTESIAN_POINT('Ctrl Pts',(-15.6667476145694,-14.5583460040984,
116.946321956118)) ;
#162275 = CARTESIAN_POINT('Ctrl Pts',(-15.5929437872122,-14.5583459928856,
116.970553046728)) ;
#162276 = CARTESIAN_POINT('Ctrl Pts',(-15.519139959855,-14.5583459816727,
116.994784137339)) ;
#162277 = CARTESIAN_POINT('Ctrl Pts',(-15.5142887883934,-14.4840522417127,
116.980008252819)) ;
#162278 = CARTESIAN_POINT('Ctrl Pts',(-15.4346677192972,-14.5035551456864,
116.702251625481)) ;
#162279 = CARTESIAN_POINT('Ctrl Pts',(-15.4360978653644,-14.4277930448145,
116.706607620791)) ;
#162280 = CARTESIAN_POINT('Ctrl Pts',(-15.5099016903547,-14.4277930415592,
116.682376522971)) ;
#162281 = CARTESIAN_POINT('Ctrl Pts',(-15.583705515345,-14.427793038304,116.658145425152)) ;
#162282 = CARTESIAN_POINT('Ctrl Pts',(-15.5822753692777,-14.503555139176,
116.653789429841)) ;
#162283 = CARTESIAN_POINT('Ctrl Pts',(-15.5808452232104,-14.579317240048,
116.649433434531)) ;
#162284 = CARTESIAN_POINT('Ctrl Pts',(-15.5070413982202,-14.5793172433032,
116.673664532351)) ;
#162285 = CARTESIAN_POINT('Ctrl Pts',(-15.4332375732299,-14.5793172465584,
116.69789563017)) ;
#162286 = CARTESIAN_POINT('Ctrl Pts',(-15.4346677192972,-14.5035551456864,
116.702251625481)) ;
#162287 = CARTESIAN_POINT('Ctrl Pts',(-15.3559292275796,-14.4455933724693,
116.426856756554)) ;
#162288 = CARTESIAN_POINT('Ctrl Pts',(-15.3635948048506,-14.3737681183539,
116.450204869409)) ;
#162289 = CARTESIAN_POINT('Ctrl Pts',(-15.4373986280072,-14.3737680965987,
116.425973766004)) ;
#162290 = CARTESIAN_POINT('Ctrl Pts',(-15.5112024511638,-14.3737680748436,
116.4017426626)) ;
#162291 = CARTESIAN_POINT('Ctrl Pts',(-15.5035368738929,-14.445593328959,
116.378394549745)) ;
#162292 = CARTESIAN_POINT('Ctrl Pts',(-15.4958712966219,-14.5174185830743,
116.355046436891)) ;
#162293 = CARTESIAN_POINT('Ctrl Pts',(-15.4220674734653,-14.5174186048295,
116.379277540295)) ;
#162294 = CARTESIAN_POINT('Ctrl Pts',(-15.3482636503086,-14.5174186265847,
116.4035086437)) ;
#162295 = CARTESIAN_POINT('Ctrl Pts',(-15.3559292275796,-14.4455933724693,
116.426856756554)) ;
#162296 = CARTESIAN_POINT('Ctrl Pts',(-15.285414304366,-14.3137077173971,
116.176599635695)) ;
#162297 = CARTESIAN_POINT('Ctrl Pts',(-15.2987483150693,-14.2509862906075,
116.21721288234)) ;
#162298 = CARTESIAN_POINT('Ctrl Pts',(-15.3725521387493,-14.2509862477117,
116.192981780529)) ;
#162299 = CARTESIAN_POINT('Ctrl Pts',(-15.4463559624294,-14.2509862048158,
116.168750678719)) ;
#162300 = CARTESIAN_POINT('Ctrl Pts',(-15.4330219517261,-14.3137076316054,
116.128137432075)) ;
#162301 = CARTESIAN_POINT('Ctrl Pts',(-15.4196879410228,-14.3764290583951,
116.08752418543)) ;
#162302 = CARTESIAN_POINT('Ctrl Pts',(-15.3458841173428,-14.3764291012909,
116.111755287241)) ;
#162303 = CARTESIAN_POINT('Ctrl Pts',(-15.2720802936627,-14.3764291441867,
116.135986389051)) ;
#162304 = CARTESIAN_POINT('Ctrl Pts',(-15.285414304366,-14.3137077173971,
116.176599635695)) ;
#162305 = CARTESIAN_POINT('Ctrl Pts',(-15.2287932761951,-14.118290994482,
115.968741900664)) ;
#162306 = CARTESIAN_POINT('Ctrl Pts',(-15.2468321761194,-14.0691221426053,
116.023685480875)) ;
#162307 = CARTESIAN_POINT('Ctrl Pts',(-15.3206360026981,-14.0691220793387,
115.999454387893)) ;
#162308 = CARTESIAN_POINT('Ctrl Pts',(-15.3944398292768,-14.0691220160722,
115.975223294912)) ;
#162309 = CARTESIAN_POINT('Ctrl Pts',(-15.3764009293525,-14.1182908679489,
115.920279714701)) ;
#162310 = CARTESIAN_POINT('Ctrl Pts',(-15.3583620294282,-14.1674597198256,
115.865336134491)) ;
#162311 = CARTESIAN_POINT('Ctrl Pts',(-15.2845582028495,-14.1674597830921,
115.889567227472)) ;
#162312 = CARTESIAN_POINT('Ctrl Pts',(-15.2107543762708,-14.1674598463587,
115.913798320454)) ;
#162313 = CARTESIAN_POINT('Ctrl Pts',(-15.2287932761951,-14.118290994482,
115.968741900664)) ;
#162314 = CARTESIAN_POINT('Ctrl Pts',(-15.190662017011,-13.8721339097932,
115.817104400349)) ;
#162315 = CARTESIAN_POINT('Ctrl Pts',(-15.2121238291066,-13.840079359465,
115.882473618878)) ;
#162316 = CARTESIAN_POINT('Ctrl Pts',(-15.2859276606813,-13.8400792780125,
115.858242541114)) ;
#162317 = CARTESIAN_POINT('Ctrl Pts',(-15.3597314922561,-13.8400791965599,
115.83401146335)) ;
#162318 = CARTESIAN_POINT('Ctrl Pts',(-15.3382696801605,-13.872133746888,
115.76864224482)) ;
#162319 = CARTESIAN_POINT('Ctrl Pts',(-15.316807868065,-13.9041882972162,
115.703273026291)) ;
#162320 = CARTESIAN_POINT('Ctrl Pts',(-15.2430040364902,-13.9041883786687,
115.727504104055)) ;
#162321 = CARTESIAN_POINT('Ctrl Pts',(-15.1692002049154,-13.9041884601213,
115.75173518182)) ;
#162322 = CARTESIAN_POINT('Ctrl Pts',(-15.190662017011,-13.8721339097932,
115.817104400349)) ;
#162323 = CARTESIAN_POINT('Ctrl Pts',(-15.1746169230128,-13.5943341067766,
115.732853741077)) ;
#162324 = CARTESIAN_POINT('Ctrl Pts',(-15.1979622079392,-13.5816279445403,
115.803959714053)) ;
#162325 = CARTESIAN_POINT('Ctrl Pts',(-15.2717660463982,-13.5816278507647,
115.779728657256)) ;
#162326 = CARTESIAN_POINT('Ctrl Pts',(-15.3455698848571,-13.5816277569891,
115.75549760046)) ;
#162327 = CARTESIAN_POINT('Ctrl Pts',(-15.3222245999306,-13.5943339192254,
115.684391627484)) ;
#162328 = CARTESIAN_POINT('Ctrl Pts',(-15.2988793150042,-13.6070400814617,
115.613285654508)) ;
#162329 = CARTESIAN_POINT('Ctrl Pts',(-15.2250754765453,-13.6070401752373,
115.637516711305)) ;
#162330 = CARTESIAN_POINT('Ctrl Pts',(-15.1512716380863,-13.6070402690129,
115.661747768101)) ;
#162331 = CARTESIAN_POINT('Ctrl Pts',(-15.1746169230128,-13.5943341067766,
115.732853741077)) ;
#162332 = CARTESIAN_POINT('Ctrl Pts',(-15.1826673766295,-13.3016132059809,
115.721705106696)) ;
#162333 = CARTESIAN_POINT('Ctrl Pts',(-15.2062229726213,-13.309324862532,
115.793451653354)) ;
#162334 = CARTESIAN_POINT('Ctrl Pts',(-15.2800268192901,-13.3093247622356,
115.769220621564)) ;
#162335 = CARTESIAN_POINT('Ctrl Pts',(-15.3538306659589,-13.3093246619392,
115.744989589774)) ;
#162336 = CARTESIAN_POINT('Ctrl Pts',(-15.3302750699671,-13.3016130053881,
115.673243043115)) ;
#162337 = CARTESIAN_POINT('Ctrl Pts',(-15.3067194739753,-13.293901348837,
115.601496496456)) ;
#162338 = CARTESIAN_POINT('Ctrl Pts',(-15.2329156273065,-13.2939014491334,
115.625727528247)) ;
#162339 = CARTESIAN_POINT('Ctrl Pts',(-15.1591117806377,-13.2939015494298,
115.649958560037)) ;
#162340 = CARTESIAN_POINT('Ctrl Pts',(-15.1826673766295,-13.3016132059809,
115.721705106696)) ;
#162341 = CARTESIAN_POINT('Ctrl Pts',(-15.2146933752457,-13.0203974601351,
115.783981898111)) ;
#162342 = CARTESIAN_POINT('Ctrl Pts',(-15.2367771372747,-13.0477539673653,
115.851245476052)) ;
#162343 = CARTESIAN_POINT('Ctrl Pts',(-15.3105809924454,-13.0477538708474,
115.827014470158)) ;
#162344 = CARTESIAN_POINT('Ctrl Pts',(-15.3843848476162,-13.0477537743296,
115.802783464263)) ;
#162345 = CARTESIAN_POINT('Ctrl Pts',(-15.3623010855873,-13.0203972670994,
115.735519886322)) ;
#162346 = CARTESIAN_POINT('Ctrl Pts',(-15.3402173235583,-12.9930407598692,
115.668256308381)) ;
#162347 = CARTESIAN_POINT('Ctrl Pts',(-15.2664134683876,-12.9930408563871,
115.692487314276)) ;
#162348 = CARTESIAN_POINT('Ctrl Pts',(-15.1926096132168,-12.9930409529049,
115.71671832017)) ;
#162349 = CARTESIAN_POINT('Ctrl Pts',(-15.2146933752457,-13.0203974601351,
115.783981898111)) ;
#162350 = CARTESIAN_POINT('Ctrl Pts',(-15.269404025713,-12.7657619407627,
115.915129891759)) ;
#162351 = CARTESIAN_POINT('Ctrl Pts',(-15.2884349716493,-12.8109362194434,
115.973095084508)) ;
#162352 = CARTESIAN_POINT('Ctrl Pts',(-15.362238834935,-12.8109361340697,
115.948864103331)) ;
#162353 = CARTESIAN_POINT('Ctrl Pts',(-15.4360426982208,-12.810936048696,
115.924633122153)) ;
#162354 = CARTESIAN_POINT('Ctrl Pts',(-15.4170117522845,-12.7657617700153,
115.866667929404)) ;
#162355 = CARTESIAN_POINT('Ctrl Pts',(-15.3979808063481,-12.7205874913346,
115.808702736655)) ;
#162356 = CARTESIAN_POINT('Ctrl Pts',(-15.3241769430624,-12.7205875767083,
115.832933717832)) ;
#162357 = CARTESIAN_POINT('Ctrl Pts',(-15.2503730797767,-12.720587662082,
115.85716469901)) ;
#162358 = CARTESIAN_POINT('Ctrl Pts',(-15.269404025713,-12.7657619407627,
115.915129891759)) ;
#162359 = CARTESIAN_POINT('Ctrl Pts',(-15.3438708491905,-12.5577255499837,
116.10637631446)) ;
#162360 = CARTESIAN_POINT('Ctrl Pts',(-15.3584669209644,-12.6174909098253,
116.150833596105)) ;
#162361 = CARTESIAN_POINT('Ctrl Pts',(-15.4322707910339,-12.6174908436088,
116.12660263559)) ;
#162362 = CARTESIAN_POINT('Ctrl Pts',(-15.5060746611033,-12.6174907773923,
116.102371675074)) ;
#162363 = CARTESIAN_POINT('Ctrl Pts',(-15.4914785893295,-12.5577254175507,
116.057914393429)) ;
#162364 = CARTESIAN_POINT('Ctrl Pts',(-15.4768825175556,-12.497960057709,
116.013457111784)) ;
#162365 = CARTESIAN_POINT('Ctrl Pts',(-15.4030786474862,-12.4979601239256,
116.0376880723)) ;
#162366 = CARTESIAN_POINT('Ctrl Pts',(-15.3292747774167,-12.4979601901421,
116.061919032815)) ;
#162367 = CARTESIAN_POINT('Ctrl Pts',(-15.3438708491905,-12.5577255499837,
116.10637631446)) ;
#162368 = CARTESIAN_POINT('Ctrl Pts',(-15.4327636159981,-12.4120606642955,
116.34175086754)) ;
#162369 = CARTESIAN_POINT('Ctrl Pts',(-15.4419070935897,-12.4820840248362,
116.369600427087)) ;
#162370 = CARTESIAN_POINT('Ctrl Pts',(-15.5157109682969,-12.482083983576,
116.345369480697)) ;
#162371 = CARTESIAN_POINT('Ctrl Pts',(-15.5895148430041,-12.4820839423157,
116.321138534307)) ;
#162372 = CARTESIAN_POINT('Ctrl Pts',(-15.5803713654125,-12.412060581775,
116.293288974761)) ;
#162373 = CARTESIAN_POINT('Ctrl Pts',(-15.5712278878209,-12.3420372212343,
116.265439415215)) ;
#162374 = CARTESIAN_POINT('Ctrl Pts',(-15.4974240131137,-12.3420372624946,
116.289670361605)) ;
#162375 = CARTESIAN_POINT('Ctrl Pts',(-15.4236201384065,-12.3420373037548,
116.313901307994)) ;
#162376 = CARTESIAN_POINT('Ctrl Pts',(-15.4327636159981,-12.4120606642955,
116.34175086754)) ;
#162377 = CARTESIAN_POINT('Ctrl Pts',(-15.5316685213714,-12.3380220880362,
116.60734315125)) ;
#162378 = CARTESIAN_POINT('Ctrl Pts',(-15.5346582890961,-12.4133190427032,
116.616449503417)) ;
#162379 = CARTESIAN_POINT('Ctrl Pts',(-15.6084621657583,-12.4133190298849,
116.592218562982)) ;
#162380 = CARTESIAN_POINT('Ctrl Pts',(-15.6822660424204,-12.4133190170666,
116.567987622547)) ;
#162381 = CARTESIAN_POINT('Ctrl Pts',(-15.6792762746957,-12.3380220623996,
116.558881270379)) ;
#162382 = CARTESIAN_POINT('Ctrl Pts',(-15.676286506971,-12.2627251077326,
116.549774918212)) ;
#162383 = CARTESIAN_POINT('Ctrl Pts',(-15.6024826303088,-12.2627251205509,
116.574005858647)) ;
#162384 = CARTESIAN_POINT('Ctrl Pts',(-15.5286787536467,-12.2627251333692,
116.598236799083)) ;
#162385 = CARTESIAN_POINT('Ctrl Pts',(-15.5316685213714,-12.3380220880362,
116.60734315125)) ;
#162386 = CARTESIAN_POINT('Ctrl Pts',(-15.6323103361434,-12.3416277493325,
116.878663222145)) ;
#162387 = CARTESIAN_POINT('Ctrl Pts',(-15.629006691363,-12.4167843477481,
116.868600855232)) ;
#162388 = CARTESIAN_POINT('Ctrl Pts',(-15.7028105674402,-12.4167843633384,
116.844369913015)) ;
#162389 = CARTESIAN_POINT('Ctrl Pts',(-15.7766144435173,-12.4167843789286,
116.820138970798)) ;
#162390 = CARTESIAN_POINT('Ctrl Pts',(-15.7799180882977,-12.3416277805131,
116.830201337711)) ;
#162391 = CARTESIAN_POINT('Ctrl Pts',(-15.7832217330782,-12.2664711820975,
116.840263704625)) ;
#162392 = CARTESIAN_POINT('Ctrl Pts',(-15.709417857001,-12.2664711665072,
116.864494646842)) ;
#162393 = CARTESIAN_POINT('Ctrl Pts',(-15.6356139809238,-12.266471150917,
116.888725589059)) ;
#162394 = CARTESIAN_POINT('Ctrl Pts',(-15.6323103361434,-12.3416277493325,
116.878663222145)) ;
#162395 = CARTESIAN_POINT('Ctrl Pts',(-15.7303191792415,-12.4221117178776,
117.141642652826)) ;
#162396 = CARTESIAN_POINT('Ctrl Pts',(-15.7209033300313,-12.4917616411482,
117.112963497359)) ;
#162397 = CARTESIAN_POINT('Ctrl Pts',(-15.7947072027341,-12.4917616828604,
117.088732544865)) ;
#162398 = CARTESIAN_POINT('Ctrl Pts',(-15.868511075437,-12.4917617245726,
117.06450159237)) ;
#162399 = CARTESIAN_POINT('Ctrl Pts',(-15.8779269246473,-12.422111801302,
117.093180747837)) ;
#162400 = CARTESIAN_POINT('Ctrl Pts',(-15.8873427738576,-12.3524618780314,
117.121859903304)) ;
#162401 = CARTESIAN_POINT('Ctrl Pts',(-15.8135389011547,-12.3524618363192,
117.146090855799)) ;
#162402 = CARTESIAN_POINT('Ctrl Pts',(-15.7397350284518,-12.3524617946069,
117.170321808294)) ;
#162403 = CARTESIAN_POINT('Ctrl Pts',(-15.7303191792415,-12.4221117178776,
117.141642652826)) ;
#162404 = CARTESIAN_POINT('Ctrl Pts',(-15.818253094992,-12.5739000669618,
117.37404115853)) ;
#162405 = CARTESIAN_POINT('Ctrl Pts',(-15.8034170204807,-12.6330567654726,
117.32885287127)) ;
#162406 = CARTESIAN_POINT('Ctrl Pts',(-15.8772208877114,-12.6330568281404,
117.304621902107)) ;
#162407 = CARTESIAN_POINT('Ctrl Pts',(-15.951024754942,-12.6330568908083,
117.280390932945)) ;
#162408 = CARTESIAN_POINT('Ctrl Pts',(-15.9658608294533,-12.5739001922976,
117.325579220205)) ;
#162409 = CARTESIAN_POINT('Ctrl Pts',(-15.9806969039645,-12.5147434937868,
117.370767507466)) ;
#162410 = CARTESIAN_POINT('Ctrl Pts',(-15.9068930367339,-12.5147434311189,
117.394998476628)) ;
#162411 = CARTESIAN_POINT('Ctrl Pts',(-15.8330891695033,-12.5147433684511,
117.41922944579)) ;
#162412 = CARTESIAN_POINT('Ctrl Pts',(-15.818253094992,-12.5739000669618,
117.37404115853)) ;
#162413 = CARTESIAN_POINT('Ctrl Pts',(-15.8910677122169,-12.7865530350162,
117.560294460758)) ;
#162414 = CARTESIAN_POINT('Ctrl Pts',(-15.8718607305365,-12.830951855475,
117.5017930954)) ;
#162415 = CARTESIAN_POINT('Ctrl Pts',(-15.9456645907029,-12.8309519318751,
117.477562104721)) ;
#162416 = CARTESIAN_POINT('Ctrl Pts',(-16.0194684508694,-12.8309520082752,
117.453331114042)) ;
#162417 = CARTESIAN_POINT('Ctrl Pts',(-16.0386754325498,-12.7865531878164,
117.511832479401)) ;
#162418 = CARTESIAN_POINT('Ctrl Pts',(-16.0578824142302,-12.7421543673576,
117.57033384476)) ;
#162419 = CARTESIAN_POINT('Ctrl Pts',(-15.9840785540637,-12.7421542909575,
117.594564835438)) ;
#162420 = CARTESIAN_POINT('Ctrl Pts',(-15.9102746938973,-12.7421542145574,
117.618795826117)) ;
#162421 = CARTESIAN_POINT('Ctrl Pts',(-15.8910677122169,-12.7865530350162,
117.560294460758)) ;
#162422 = CARTESIAN_POINT('Ctrl Pts',(-15.943961350988,-13.044698151263,117.685874037695)) ;
#162423 = CARTESIAN_POINT('Ctrl Pts',(-15.921767547098,-13.071140713464,117.618275293682)) ;
#162424 = CARTESIAN_POINT('Ctrl Pts',(-15.9955713996357,-13.0711407952517,
117.594044279767)) ;
#162425 = CARTESIAN_POINT('Ctrl Pts',(-16.0693752521733,-13.0711408770393,
117.569813265852)) ;
#162426 = CARTESIAN_POINT('Ctrl Pts',(-16.0915690560633,-13.0446983148383,
117.637412009865)) ;
#162427 = CARTESIAN_POINT('Ctrl Pts',(-16.1137628599533,-13.0182557526373,
117.705010753878)) ;
#162428 = CARTESIAN_POINT('Ctrl Pts',(-16.0399590074156,-13.0182556708497,
117.729241767793)) ;
#162429 = CARTESIAN_POINT('Ctrl Pts',(-15.966155154878,-13.018255589062,117.753472781708)) ;
#162430 = CARTESIAN_POINT('Ctrl Pts',(-15.943961350988,-13.044698151263,117.685874037695)) ;
#162431 = CARTESIAN_POINT('Ctrl Pts',(-15.973861910085,-13.328059924083,117.741608955228)) ;
#162432 = CARTESIAN_POINT('Ctrl Pts',(-15.9502783076643,-13.33475818736,117.669777109021)) ;
#162433 = CARTESIAN_POINT('Ctrl Pts',(-16.024082152983,-13.3347582681445,
117.645546073119)) ;
#162434 = CARTESIAN_POINT('Ctrl Pts',(-16.0978859983017,-13.334758348929,
117.621315037216)) ;
#162435 = CARTESIAN_POINT('Ctrl Pts',(-16.1214696007224,-13.328060085652,
117.693146883423)) ;
#162436 = CARTESIAN_POINT('Ctrl Pts',(-16.145053203143,-13.321361822375,117.764978729631)) ;
#162437 = CARTESIAN_POINT('Ctrl Pts',(-16.0712493578243,-13.3213617415905,
117.789209765533)) ;
#162438 = CARTESIAN_POINT('Ctrl Pts',(-15.9974455125056,-13.321361660806,
117.813440801436)) ;
#162439 = CARTESIAN_POINT('Ctrl Pts',(-15.973861910085,-13.328059924083,117.741608955228)) ;
#162440 = CARTESIAN_POINT('Ctrl Pts',(-15.9797490331987,-13.6187777866059,
117.724086355187)) ;
#162441 = CARTESIAN_POINT('Ctrl Pts',(-15.9564523748508,-13.6051885128316,
117.653128494185)) ;
#162442 = CARTESIAN_POINT('Ctrl Pts',(-16.0302562137773,-13.6051885851199,
117.628897438813)) ;
#162443 = CARTESIAN_POINT('Ctrl Pts',(-16.1040600527037,-13.6051886574082,
117.604666383441)) ;
#162444 = CARTESIAN_POINT('Ctrl Pts',(-16.1273567110516,-13.6187779311824,
117.675624244442)) ;
#162445 = CARTESIAN_POINT('Ctrl Pts',(-16.1506533693995,-13.6323672049567,
117.746582105443)) ;
#162446 = CARTESIAN_POINT('Ctrl Pts',(-16.0768495304731,-13.6323671326684,
117.770813160816)) ;
#162447 = CARTESIAN_POINT('Ctrl Pts',(-16.0030456915466,-13.6323670603802,
117.795044216188)) ;
#162448 = CARTESIAN_POINT('Ctrl Pts',(-15.9797490331987,-13.6187777866059,
117.724086355187)) ;
#162449 = CARTESIAN_POINT('Ctrl Pts',(-15.9616058932464,-13.8959727795492,
117.633255070877)) ;
#162450 = CARTESIAN_POINT('Ctrl Pts',(-15.9402766412006,-13.863009115872,
117.568289611858)) ;
#162451 = CARTESIAN_POINT('Ctrl Pts',(-16.0140804755236,-13.8630091736306,
117.544058542464)) ;
#162452 = CARTESIAN_POINT('Ctrl Pts',(-16.0878843098467,-13.8630092313891,
117.519827473071)) ;
#162453 = CARTESIAN_POINT('Ctrl Pts',(-16.1092135618925,-13.8959728950663,
117.58479293209)) ;
#162454 = CARTESIAN_POINT('Ctrl Pts',(-16.1305428139384,-13.9289365587434,
117.64975839111)) ;
#162455 = CARTESIAN_POINT('Ctrl Pts',(-16.0567389796153,-13.9289365009848,
117.673989460503)) ;
#162456 = CARTESIAN_POINT('Ctrl Pts',(-15.9829351452922,-13.9289364432263,
117.698220529897)) ;
#162457 = CARTESIAN_POINT('Ctrl Pts',(-15.9616058932464,-13.8959727795492,
117.633255070877)) ;
#162458 = CARTESIAN_POINT('Ctrl Pts',(-15.92165968614,-14.1380897314584,117.476125293794)) ;
#162459 = CARTESIAN_POINT('Ctrl Pts',(-15.9038209335532,-14.0881713161907,
117.421791332774)) ;
#162460 = CARTESIAN_POINT('Ctrl Pts',(-15.9776247651568,-14.0881713577831,
117.397560255097)) ;
#162461 = CARTESIAN_POINT('Ctrl Pts',(-16.0514285967603,-14.0881713993755,
117.37332917742)) ;
#162462 = CARTESIAN_POINT('Ctrl Pts',(-16.0692673493471,-14.1380898146432,
117.427663138441)) ;
#162463 = CARTESIAN_POINT('Ctrl Pts',(-16.0871061019338,-14.1880082299108,
117.481997099461)) ;
#162464 = CARTESIAN_POINT('Ctrl Pts',(-16.0133022703303,-14.1880081883184,
117.506228177138)) ;
#162465 = CARTESIAN_POINT('Ctrl Pts',(-15.9394984387268,-14.188008146726,
117.530459254814)) ;
#162466 = CARTESIAN_POINT('Ctrl Pts',(-15.92165968614,-14.1380897314584,117.476125293794)) ;
#162467 = CARTESIAN_POINT('Ctrl Pts',(-15.8633008249773,-14.3289912800735,
117.262814844311)) ;
#162468 = CARTESIAN_POINT('Ctrl Pts',(-15.8502454740091,-14.2656678675504,
117.223050352636)) ;
#162469 = CARTESIAN_POINT('Ctrl Pts',(-15.9240493051082,-14.2656678924027,
117.198819273423)) ;
#162470 = CARTESIAN_POINT('Ctrl Pts',(-15.9978531362073,-14.2656679172549,
117.17458819421)) ;
#162471 = CARTESIAN_POINT('Ctrl Pts',(-16.0109084871756,-14.3289913297781,
117.214352685885)) ;
#162472 = CARTESIAN_POINT('Ctrl Pts',(-16.0239638381439,-14.3923147423012,
117.25411717756)) ;
#162473 = CARTESIAN_POINT('Ctrl Pts',(-15.9501600070448,-14.3923147174489,
117.278348256773)) ;
#162474 = CARTESIAN_POINT('Ctrl Pts',(-15.8763561759456,-14.3923146925966,
117.302579335987)) ;
#162475 = CARTESIAN_POINT('Ctrl Pts',(-15.8633008249773,-14.3289912800735,
117.262814844311)) ;
#162476 = CARTESIAN_POINT('Ctrl Pts',(-15.7921118917969,-14.4536834307714,
117.01067142375)) ;
#162477 = CARTESIAN_POINT('Ctrl Pts',(-15.7847381201067,-14.3815580790825,
116.988212105697)) ;
#162478 = CARTESIAN_POINT('Ctrl Pts',(-15.8585419517498,-14.381558090492,
116.963981028141)) ;
#162479 = CARTESIAN_POINT('Ctrl Pts',(-15.9323457833928,-14.3815581019016,
116.939749950584)) ;
#162480 = CARTESIAN_POINT('Ctrl Pts',(-15.9397195550829,-14.4536834535906,
116.962209268637)) ;
#162481 = CARTESIAN_POINT('Ctrl Pts',(-15.947093326773,-14.5258088052795,
116.984668586689)) ;
#162482 = CARTESIAN_POINT('Ctrl Pts',(-15.87328949513,-14.52580879387,117.008899664246)) ;
#162483 = CARTESIAN_POINT('Ctrl Pts',(-15.799485663487,-14.5258087824604,
117.033130741802)) ;
#162484 = CARTESIAN_POINT('Ctrl Pts',(-15.7921118917969,-14.4536834307714,
117.01067142375)) ;
#162485 = CARTESIAN_POINT('Ctrl Pts',(-15.7132086075603,-14.5050447602448,
116.734875307883)) ;
#162486 = CARTESIAN_POINT('Ctrl Pts',(-15.7120668798563,-14.4292238155188,
116.731397790109)) ;
#162487 = CARTESIAN_POINT('Ctrl Pts',(-15.7858707136532,-14.4292238160263,
116.707166719113)) ;
#162488 = CARTESIAN_POINT('Ctrl Pts',(-15.8596745474501,-14.4292238165338,
116.682935648117)) ;
#162489 = CARTESIAN_POINT('Ctrl Pts',(-15.8608162751541,-14.5050447612597,
116.686413165891)) ;
#162490 = CARTESIAN_POINT('Ctrl Pts',(-15.8619580028581,-14.5808657059856,
116.689890683665)) ;
#162491 = CARTESIAN_POINT('Ctrl Pts',(-15.7881541690612,-14.5808657054781,
116.714121754661)) ;
#162492 = CARTESIAN_POINT('Ctrl Pts',(-15.7143503352643,-14.5808657049707,
116.738352825657)) ;
#162493 = CARTESIAN_POINT('Ctrl Pts',(-15.7132086075603,-14.5050447602448,
116.734875307883)) ;
#162494 = CARTESIAN_POINT('Ctrl Pts',(-15.6332196110999,-14.4782940097224,
116.455753006044)) ;
#162495 = CARTESIAN_POINT('Ctrl Pts',(-15.6383957039192,-14.4042259752822,
116.471518550047)) ;
#162496 = CARTESIAN_POINT('Ctrl Pts',(-15.7121995405475,-14.4042259695799,
116.447287487674)) ;
#162497 = CARTESIAN_POINT('Ctrl Pts',(-15.7860033771757,-14.4042259638776,
116.423056425302)) ;
#162498 = CARTESIAN_POINT('Ctrl Pts',(-15.7808272843565,-14.4782939983178,
116.4072908813)) ;
#162499 = CARTESIAN_POINT('Ctrl Pts',(-15.7756511915372,-14.552362032758,
116.391525337298)) ;
#162500 = CARTESIAN_POINT('Ctrl Pts',(-15.7018473549089,-14.5523620384603,
116.41575639967)) ;
#162501 = CARTESIAN_POINT('Ctrl Pts',(-15.6280435182807,-14.5523620441626,
116.439987462042)) ;
#162502 = CARTESIAN_POINT('Ctrl Pts',(-15.6332196110999,-14.4782940097224,
116.455753006044)) ;
#162503 = CARTESIAN_POINT('Ctrl Pts',(-15.5587696998728,-14.3758709565101,
116.193557985972)) ;
#162504 = CARTESIAN_POINT('Ctrl Pts',(-15.5698852741414,-14.3088425929799,
116.227414231996)) ;
#162505 = CARTESIAN_POINT('Ctrl Pts',(-15.6436891134963,-14.3088425851836,
116.203183177928)) ;
#162506 = CARTESIAN_POINT('Ctrl Pts',(-15.7174929528511,-14.3088425773873,
116.17895212386)) ;
#162507 = CARTESIAN_POINT('Ctrl Pts',(-15.7063773785825,-14.3758709409175,
116.145095877837)) ;
#162508 = CARTESIAN_POINT('Ctrl Pts',(-15.6952618043138,-14.4428993044478,
116.111239631813)) ;
#162509 = CARTESIAN_POINT('Ctrl Pts',(-15.621457964959,-14.442899312244,116.13547068588)) ;
#162510 = CARTESIAN_POINT('Ctrl Pts',(-15.5476541256042,-14.4428993200403,
116.159701739948)) ;
#162511 = CARTESIAN_POINT('Ctrl Pts',(-15.5587696998728,-14.3758709565101,
116.193557985972)) ;
#162512 = CARTESIAN_POINT('Ctrl Pts',(-15.4956323923376,-14.2038414128419,
115.965654894124)) ;
#162513 = CARTESIAN_POINT('Ctrl Pts',(-15.5119101272549,-14.1487238719563,
116.015234248429)) ;
#162514 = CARTESIAN_POINT('Ctrl Pts',(-15.5857139690308,-14.1487238662438,
115.991003201736)) ;
#162515 = CARTESIAN_POINT('Ctrl Pts',(-15.6595178108066,-14.1487238605313,
115.966772155042)) ;
#162516 = CARTESIAN_POINT('Ctrl Pts',(-15.6432400758893,-14.2038414014169,
115.917192800737)) ;
#162517 = CARTESIAN_POINT('Ctrl Pts',(-15.6269623409719,-14.2589589423024,
115.867613446432)) ;
#162518 = CARTESIAN_POINT('Ctrl Pts',(-15.553158499196,-14.2589589480149,
115.891844493126)) ;
#162519 = CARTESIAN_POINT('Ctrl Pts',(-15.4793546574202,-14.2589589537274,
115.91607553982)) ;
#162520 = CARTESIAN_POINT('Ctrl Pts',(-15.4956323923376,-14.2038414128419,
115.965654894124)) ;
#162521 = CARTESIAN_POINT('Ctrl Pts',(-15.4497236558171,-13.9777022974474,
115.790578372436)) ;
#162522 = CARTESIAN_POINT('Ctrl Pts',(-15.469960680649,-13.9382924680263,
115.85221708491)) ;
#162523 = CARTESIAN_POINT('Ctrl Pts',(-15.5437645236048,-13.9382924647888,
115.827986041811)) ;
#162524 = CARTESIAN_POINT('Ctrl Pts',(-15.6175683665605,-13.9382924615514,
115.803754998711)) ;
#162525 = CARTESIAN_POINT('Ctrl Pts',(-15.5973313417286,-13.9777022909725,
115.742116286236)) ;
#162526 = CARTESIAN_POINT('Ctrl Pts',(-15.5770943168967,-14.0171121203935,
115.680477573762)) ;
#162527 = CARTESIAN_POINT('Ctrl Pts',(-15.503290473941,-14.017112123631,115.704708616861)) ;
#162528 = CARTESIAN_POINT('Ctrl Pts',(-15.4294866309852,-14.0171121268685,
115.728939659961)) ;
#162529 = CARTESIAN_POINT('Ctrl Pts',(-15.4497236558171,-13.9777022974474,
115.790578372436)) ;
#162530 = CARTESIAN_POINT('Ctrl Pts',(-15.4242298945828,-13.7081471730545,
115.677198196239)) ;
#162531 = CARTESIAN_POINT('Ctrl Pts',(-15.4470171331945,-13.6875008672276,
115.746604448313)) ;
#162532 = CARTESIAN_POINT('Ctrl Pts',(-15.5208209768319,-13.6875008686463,
115.722373407289)) ;
#162533 = CARTESIAN_POINT('Ctrl Pts',(-15.5946248204693,-13.687500870065,
115.698142366266)) ;
#162534 = CARTESIAN_POINT('Ctrl Pts',(-15.5718375818576,-13.7081471758919,
115.628736114192)) ;
#162535 = CARTESIAN_POINT('Ctrl Pts',(-15.5490503432458,-13.7287934817188,
115.559329862118)) ;
#162536 = CARTESIAN_POINT('Ctrl Pts',(-15.4752464996084,-13.7287934803001,
115.583560903142)) ;
#162537 = CARTESIAN_POINT('Ctrl Pts',(-15.401442655971,-13.7287934788814,
115.607791944166)) ;
#162538 = CARTESIAN_POINT('Ctrl Pts',(-15.4242298945828,-13.7081471730545,
115.677198196239)) ;
#162539 = CARTESIAN_POINT('Ctrl Pts',(-15.4224756486748,-13.4207218926891,
115.636530543552)) ;
#162540 = CARTESIAN_POINT('Ctrl Pts',(-15.4461502225077,-13.4201152017274,
115.70863947551)) ;
#162541 = CARTESIAN_POINT('Ctrl Pts',(-15.5199540659324,-13.4201152047761,
115.684408433839)) ;
#162542 = CARTESIAN_POINT('Ctrl Pts',(-15.593757909357,-13.4201152078248,
115.660177392167)) ;
#162543 = CARTESIAN_POINT('Ctrl Pts',(-15.5700833355241,-13.4207218987865,
115.588068460209)) ;
#162544 = CARTESIAN_POINT('Ctrl Pts',(-15.5464087616913,-13.4213285897482,
115.515959528251)) ;
#162545 = CARTESIAN_POINT('Ctrl Pts',(-15.4726049182666,-13.4213285866995,
115.540190569923)) ;
#162546 = CARTESIAN_POINT('Ctrl Pts',(-15.398801074842,-13.4213285836508,
115.564421611594)) ;
#162547 = CARTESIAN_POINT('Ctrl Pts',(-15.4224756486748,-13.4207218926891,
115.636530543552)) ;
#162548 = CARTESIAN_POINT('Ctrl Pts',(-15.4448455283626,-13.1323473586493,
115.669233043994)) ;
#162549 = CARTESIAN_POINT('Ctrl Pts',(-15.4677263606914,-13.1518767361785,
115.738924367398)) ;
#162550 = CARTESIAN_POINT('Ctrl Pts',(-15.541530203822,-13.1518767392038,
115.714693324831)) ;
#162551 = CARTESIAN_POINT('Ctrl Pts',(-15.6153340469527,-13.1518767422291,
115.690462282264)) ;
#162552 = CARTESIAN_POINT('Ctrl Pts',(-15.592453214624,-13.1323473646999,
115.62077095886)) ;
#162553 = CARTESIAN_POINT('Ctrl Pts',(-15.5695723822952,-13.1128179871707,
115.551079635456)) ;
#162554 = CARTESIAN_POINT('Ctrl Pts',(-15.4957685391646,-13.1128179841454,
115.575310678023)) ;
#162555 = CARTESIAN_POINT('Ctrl Pts',(-15.4219646960339,-13.1128179811201,
115.59954172059)) ;
#162556 = CARTESIAN_POINT('Ctrl Pts',(-15.4448455283626,-13.1323473586493,
115.669233043994)) ;
#162557 = CARTESIAN_POINT('Ctrl Pts',(-15.4907259221535,-12.8640039527127,
115.773502605509)) ;
#162558 = CARTESIAN_POINT('Ctrl Pts',(-15.5111708603039,-12.9022999989721,
115.835774588317)) ;
#162559 = CARTESIAN_POINT('Ctrl Pts',(-15.5849747034648,-12.9022999996752,
115.811543545842)) ;
#162560 = CARTESIAN_POINT('Ctrl Pts',(-15.6587785466256,-12.9023000003783,
115.787312503367)) ;
#162561 = CARTESIAN_POINT('Ctrl Pts',(-15.6383336084751,-12.8640039541189,
115.725040520558)) ;
#162562 = CARTESIAN_POINT('Ctrl Pts',(-15.6178886703247,-12.8257079078595,
115.66276853775)) ;
#162563 = CARTESIAN_POINT('Ctrl Pts',(-15.5440848271639,-12.8257079071564,
115.686999580226)) ;
#162564 = CARTESIAN_POINT('Ctrl Pts',(-15.4702809840031,-12.8257079064533,
115.711230622701)) ;
#162565 = CARTESIAN_POINT('Ctrl Pts',(-15.4907259221535,-12.8640039527127,
115.773502605509)) ;
#162566 = CARTESIAN_POINT('Ctrl Pts',(-15.5576964345495,-12.6351955964259,
115.941952413121)) ;
#162567 = CARTESIAN_POINT('Ctrl Pts',(-15.5742303280639,-12.6895248162975,
115.992311985098)) ;
#162568 = CARTESIAN_POINT('Ctrl Pts',(-15.6480341721483,-12.6895248136964,
115.968080945436)) ;
#162569 = CARTESIAN_POINT('Ctrl Pts',(-15.7218380162327,-12.6895248110954,
115.943849905773)) ;
#162570 = CARTESIAN_POINT('Ctrl Pts',(-15.7053041227182,-12.6351955912238,
115.893490333797)) ;
#162571 = CARTESIAN_POINT('Ctrl Pts',(-15.6887702292038,-12.5808663713523,
115.84313076182)) ;
#162572 = CARTESIAN_POINT('Ctrl Pts',(-15.6149663851194,-12.5808663739533,
115.867361801483)) ;
#162573 = CARTESIAN_POINT('Ctrl Pts',(-15.541162541035,-12.5808663765543,
115.891592841145)) ;
#162574 = CARTESIAN_POINT('Ctrl Pts',(-15.5576964345495,-12.6351955964259,
115.941952413121)) ;
#162575 = CARTESIAN_POINT('Ctrl Pts',(-15.6410494594336,-12.4633049543151,
116.160508256525)) ;
#162576 = CARTESIAN_POINT('Ctrl Pts',(-15.6525183306037,-12.5297151872054,
116.195440587766)) ;
#162577 = CARTESIAN_POINT('Ctrl Pts',(-15.7263221760862,-12.5297151829142,
116.171209552362)) ;
#162578 = CARTESIAN_POINT('Ctrl Pts',(-15.8001260215687,-12.529715178623,
116.146978516958)) ;
#162579 = CARTESIAN_POINT('Ctrl Pts',(-15.7886571503986,-12.4633049457328,
116.112046185718)) ;
#162580 = CARTESIAN_POINT('Ctrl Pts',(-15.7771882792285,-12.3968947128425,
116.077113854477)) ;
#162581 = CARTESIAN_POINT('Ctrl Pts',(-15.703384433746,-12.3968947171337,
116.101344889881)) ;
#162582 = CARTESIAN_POINT('Ctrl Pts',(-15.6295805882636,-12.3968947214249,
116.125575925284)) ;
#162583 = CARTESIAN_POINT('Ctrl Pts',(-15.6410494594336,-12.4633049543151,
116.160508256525)) ;
#162584 = CARTESIAN_POINT('Ctrl Pts',(-15.73692924491,-12.3586842738095,116.416876897232)) ;
#162585 = CARTESIAN_POINT('Ctrl Pts',(-15.7424581639716,-12.4324967253125,
116.433717092915)) ;
#162586 = CARTESIAN_POINT('Ctrl Pts',(-15.8162620121878,-12.432496720994,
116.409486065837)) ;
#162587 = CARTESIAN_POINT('Ctrl Pts',(-15.890065860404,-12.4324967166755,
116.38525503876)) ;
#162588 = CARTESIAN_POINT('Ctrl Pts',(-15.8845369413424,-12.3586842651726,
116.368414843077)) ;
#162589 = CARTESIAN_POINT('Ctrl Pts',(-15.8790080222809,-12.2848718136696,
116.351574647394)) ;
#162590 = CARTESIAN_POINT('Ctrl Pts',(-15.8052041740647,-12.284871817988,
116.375805674472)) ;
#162591 = CARTESIAN_POINT('Ctrl Pts',(-15.7314003258485,-12.2848718223065,
116.400036701549)) ;
#162592 = CARTESIAN_POINT('Ctrl Pts',(-15.73692924491,-12.3586842738095,116.416876897232)) ;
#162593 = CARTESIAN_POINT('Ctrl Pts',(-15.837547597677,-12.3308701665295,
116.687989713795)) ;
#162594 = CARTESIAN_POINT('Ctrl Pts',(-15.8367907309467,-12.4067313032611,
116.685684420293)) ;
#162595 = CARTESIAN_POINT('Ctrl Pts',(-15.9105945814395,-12.4067313035056,
116.66145340015)) ;
#162596 = CARTESIAN_POINT('Ctrl Pts',(-15.9843984319324,-12.4067313037501,
116.637222380007)) ;
#162597 = CARTESIAN_POINT('Ctrl Pts',(-15.9851552986627,-12.3308701670186,
116.639527673509)) ;
#162598 = CARTESIAN_POINT('Ctrl Pts',(-15.985912165393,-12.2550090302871,
116.641832967011)) ;
#162599 = CARTESIAN_POINT('Ctrl Pts',(-15.9121083149001,-12.2550090300425,
116.666063987154)) ;
#162600 = CARTESIAN_POINT('Ctrl Pts',(-15.8383044644072,-12.255009029798,
116.690295007297)) ;
#162601 = CARTESIAN_POINT('Ctrl Pts',(-15.837547597677,-12.3308701665295,
116.687989713795)) ;
#162602 = CARTESIAN_POINT('Ctrl Pts',(-15.9375214249544,-12.3804185210795,
116.95704231323)) ;
#162603 = CARTESIAN_POINT('Ctrl Pts',(-15.930516766912,-12.4529298980233,
116.935707255623)) ;
#162604 = CARTESIAN_POINT('Ctrl Pts',(-16.0043206195212,-12.452929906521,
116.911476241926)) ;
#162605 = CARTESIAN_POINT('Ctrl Pts',(-16.0781244721304,-12.4529299150187,
116.887245228229)) ;
#162606 = CARTESIAN_POINT('Ctrl Pts',(-16.0851291301728,-12.380418538075,
116.908580285836)) ;
#162607 = CARTESIAN_POINT('Ctrl Pts',(-16.0921337882152,-12.3079071611312,
116.929915343443)) ;
#162608 = CARTESIAN_POINT('Ctrl Pts',(-16.018329935606,-12.3079071526335,
116.95414635714)) ;
#162609 = CARTESIAN_POINT('Ctrl Pts',(-15.9445260829967,-12.3079071441357,
116.978377370836)) ;
#162610 = CARTESIAN_POINT('Ctrl Pts',(-15.9375214249544,-12.3804185210795,
116.95704231323)) ;
#162611 = CARTESIAN_POINT('Ctrl Pts',(-16.0302559090412,-12.5045865657479,
117.204009987315)) ;
#162612 = CARTESIAN_POINT('Ctrl Pts',(-16.0175006624101,-12.5685333529208,
117.165159564891)) ;
#162613 = CARTESIAN_POINT('Ctrl Pts',(-16.0913045162659,-12.5685333737573,
117.14092855499)) ;
#162614 = CARTESIAN_POINT('Ctrl Pts',(-16.1651083701216,-12.5685333945939,
117.11669754509)) ;
#162615 = CARTESIAN_POINT('Ctrl Pts',(-16.1778636167527,-12.504586607421,
117.155547967515)) ;
#162616 = CARTESIAN_POINT('Ctrl Pts',(-16.1906188633838,-12.4406398202481,
117.194398389939)) ;
#162617 = CARTESIAN_POINT('Ctrl Pts',(-16.1168150095281,-12.4406397994116,
117.218629399839)) ;
#162618 = CARTESIAN_POINT('Ctrl Pts',(-16.0430111556723,-12.440639778575,
117.242860409739)) ;
#162619 = CARTESIAN_POINT('Ctrl Pts',(-16.0302559090412,-12.5045865657479,
117.204009987315)) ;
#162620 = CARTESIAN_POINT('Ctrl Pts',(-16.1096439036277,-12.6936012415773,
117.410410771102)) ;
#162621 = CARTESIAN_POINT('Ctrl Pts',(-16.0920599995317,-12.7444433865652,
117.356853037297)) ;
#162622 = CARTESIAN_POINT('Ctrl Pts',(-16.165863853018,-12.7444434214993,
117.332622026272)) ;
#162623 = CARTESIAN_POINT('Ctrl Pts',(-16.2396677065044,-12.7444434564334,
117.308391015246)) ;
#162624 = CARTESIAN_POINT('Ctrl Pts',(-16.2572516106004,-12.6936013114455,
117.361948749051)) ;
#162625 = CARTESIAN_POINT('Ctrl Pts',(-16.2748355146964,-12.6427591664577,
117.415506482856)) ;
#162626 = CARTESIAN_POINT('Ctrl Pts',(-16.20103166121,-12.6427591315236,117.439737493882)) ;
#162627 = CARTESIAN_POINT('Ctrl Pts',(-16.1272278077237,-12.6427590965895,
117.463968504907)) ;
#162628 = CARTESIAN_POINT('Ctrl Pts',(-16.1096439036277,-12.6936012415773,
117.410410771102)) ;
#162629 = CARTESIAN_POINT('Ctrl Pts',(-16.1712738995267,-12.9362801376937,
117.56247016244)) ;
#162630 = CARTESIAN_POINT('Ctrl Pts',(-16.1500992985322,-12.9702525737982,
117.497975745442)) ;
#162631 = CARTESIAN_POINT('Ctrl Pts',(-16.2239031501781,-12.9702526255318,
117.473744728811)) ;
#162632 = CARTESIAN_POINT('Ctrl Pts',(-16.297707001824,-12.9702526772653,
117.44951371218)) ;
#162633 = CARTESIAN_POINT('Ctrl Pts',(-16.3188816028185,-12.9362802411607,
117.514008129178)) ;
#162634 = CARTESIAN_POINT('Ctrl Pts',(-16.340056203813,-12.9023078050562,
117.578502546175)) ;
#162635 = CARTESIAN_POINT('Ctrl Pts',(-16.2662523521671,-12.9023077533226,
117.602733562806)) ;
#162636 = CARTESIAN_POINT('Ctrl Pts',(-16.1924485005212,-12.9023077015891,
117.626964579437)) ;
#162637 = CARTESIAN_POINT('Ctrl Pts',(-16.1712738995267,-12.9362801376937,
117.56247016244)) ;
#162638 = CARTESIAN_POINT('Ctrl Pts',(-16.2106239956556,-13.2112926431605,
117.646987028832)) ;
#162639 = CARTESIAN_POINT('Ctrl Pts',(-16.1874027324492,-13.2261131719055,
117.576258809104)) ;
#162640 = CARTESIAN_POINT('Ctrl Pts',(-16.2612065799304,-13.2261132359039,
117.552027779788)) ;
#162641 = CARTESIAN_POINT('Ctrl Pts',(-16.3350104274116,-13.2261132999022,
117.527796750472)) ;
#162642 = CARTESIAN_POINT('Ctrl Pts',(-16.358231690618,-13.2112927711572,
117.5985249702)) ;
#162643 = CARTESIAN_POINT('Ctrl Pts',(-16.3814529538244,-13.1964722424121,
117.669253189928)) ;
#162644 = CARTESIAN_POINT('Ctrl Pts',(-16.3076491063432,-13.1964721784138,
117.693484219244)) ;
#162645 = CARTESIAN_POINT('Ctrl Pts',(-16.233845258862,-13.1964721144154,
117.71771524856)) ;
#162646 = CARTESIAN_POINT('Ctrl Pts',(-16.2106239956556,-13.2112926431605,
117.646987028832)) ;
#162647 = CARTESIAN_POINT('Ctrl Pts',(-16.2263302334408,-13.5026318637497,
117.659280382526)) ;
#162648 = CARTESIAN_POINT('Ctrl Pts',(-16.2027142030157,-13.4971333433814,
117.587349765715)) ;
#162649 = CARTESIAN_POINT('Ctrl Pts',(-16.2765180448406,-13.4971334172492,
117.563118719171)) ;
#162650 = CARTESIAN_POINT('Ctrl Pts',(-16.3503218866654,-13.4971334911169,
117.538887672627)) ;
#162651 = CARTESIAN_POINT('Ctrl Pts',(-16.3739379170905,-13.5026320114853,
117.610818289438)) ;
#162652 = CARTESIAN_POINT('Ctrl Pts',(-16.3975539475155,-13.5081305318536,
117.682748906249)) ;
#162653 = CARTESIAN_POINT('Ctrl Pts',(-16.3237501056907,-13.5081304579859,
117.706979952793)) ;
#162654 = CARTESIAN_POINT('Ctrl Pts',(-16.2499462638658,-13.5081303841181,
117.731210999337)) ;
#162655 = CARTESIAN_POINT('Ctrl Pts',(-16.2263302334408,-13.5026318637497,
117.659280382526)) ;
#162656 = CARTESIAN_POINT('Ctrl Pts',(-16.2177424879971,-13.7865927515763,
117.59774844092)) ;
#162657 = CARTESIAN_POINT('Ctrl Pts',(-16.1954238427971,-13.7612608950297,
117.529769450301)) ;
#162658 = CARTESIAN_POINT('Ctrl Pts',(-16.2692276778268,-13.7612609711619,
117.50553838306)) ;
#162659 = CARTESIAN_POINT('Ctrl Pts',(-16.3430315128565,-13.7612610472941,
117.481307315818)) ;
#162660 = CARTESIAN_POINT('Ctrl Pts',(-16.3653501580564,-13.7865929038406,
117.549286306437)) ;
#162661 = CARTESIAN_POINT('Ctrl Pts',(-16.3876688032563,-13.8119247603871,
117.617265297056)) ;
#162662 = CARTESIAN_POINT('Ctrl Pts',(-16.3138649682267,-13.811924684255,
117.641496364297)) ;
#162663 = CARTESIAN_POINT('Ctrl Pts',(-16.240061133197,-13.8119246081228,
117.665727431539)) ;
#162664 = CARTESIAN_POINT('Ctrl Pts',(-16.2177424879971,-13.7865927515763,
117.59774844092)) ;
#162665 = CARTESIAN_POINT('Ctrl Pts',(-16.1863917194238,-14.0445932154009,
117.466837858413)) ;
#162666 = CARTESIAN_POINT('Ctrl Pts',(-16.1669624264012,-14.0012118501805,
117.407659368456)) ;
#162667 = CARTESIAN_POINT('Ctrl Pts',(-16.2407662542766,-14.001211921774,
117.383428279424)) ;
#162668 = CARTESIAN_POINT('Ctrl Pts',(-16.3145700821519,-14.0012119933675,
117.359197190392)) ;
#162669 = CARTESIAN_POINT('Ctrl Pts',(-16.3339993751745,-14.0445933585879,
117.418375680349)) ;
#162670 = CARTESIAN_POINT('Ctrl Pts',(-16.3534286681971,-14.0879747238084,
117.477554170305)) ;
#162671 = CARTESIAN_POINT('Ctrl Pts',(-16.2796248403217,-14.0879746522149,
117.501785259337)) ;
#162672 = CARTESIAN_POINT('Ctrl Pts',(-16.2058210124464,-14.0879745806213,
117.526016348369)) ;
#162673 = CARTESIAN_POINT('Ctrl Pts',(-16.1863917194238,-14.0445932154009,
117.466837858413)) ;
#162674 = CARTESIAN_POINT('Ctrl Pts',(-16.1351369456625,-14.2581092551482,
117.275260073732)) ;
#162675 = CARTESIAN_POINT('Ctrl Pts',(-16.1199915913662,-14.199757820622,
117.229129770043)) ;
#162676 = CARTESIAN_POINT('Ctrl Pts',(-16.1937954124028,-14.199757880284,
117.204898660181)) ;
#162677 = CARTESIAN_POINT('Ctrl Pts',(-16.2675992334394,-14.199757939946,
117.180667550319)) ;
#162678 = CARTESIAN_POINT('Ctrl Pts',(-16.2827445877356,-14.2581093744722,
117.226797854008)) ;
#162679 = CARTESIAN_POINT('Ctrl Pts',(-16.2978899420319,-14.3164608089984,
117.272928157698)) ;
#162680 = CARTESIAN_POINT('Ctrl Pts',(-16.2240861209953,-14.3164607493364,
117.29715926756)) ;
#162681 = CARTESIAN_POINT('Ctrl Pts',(-16.1502822999588,-14.3164606896743,
117.321390377422)) ;
#162682 = CARTESIAN_POINT('Ctrl Pts',(-16.1351369456625,-14.2581092551482,
117.275260073732)) ;
#162683 = CARTESIAN_POINT('Ctrl Pts',(-16.0682061521682,-14.4117380229187,
117.035830487134)) ;
#162684 = CARTESIAN_POINT('Ctrl Pts',(-16.0584474319418,-14.3425754066096,
117.0061070018)) ;
#162685 = CARTESIAN_POINT('Ctrl Pts',(-16.1322512472086,-14.3425754472621,
116.981875874365)) ;
#162686 = CARTESIAN_POINT('Ctrl Pts',(-16.2060550624755,-14.3425754879145,
116.957644746929)) ;
#162687 = CARTESIAN_POINT('Ctrl Pts',(-16.2158137827019,-14.4117381042236,
116.987368232263)) ;
#162688 = CARTESIAN_POINT('Ctrl Pts',(-16.2255725029284,-14.4809007205327,
117.017091717597)) ;
#162689 = CARTESIAN_POINT('Ctrl Pts',(-16.1517686876615,-14.4809006798802,
117.041322845032)) ;
#162690 = CARTESIAN_POINT('Ctrl Pts',(-16.0779648723947,-14.4809006392278,
117.065553972468)) ;
#162691 = CARTESIAN_POINT('Ctrl Pts',(-16.0682061521682,-14.4117380229187,
117.035830487134)) ;
#162692 = CARTESIAN_POINT('Ctrl Pts',(-15.9915317982417,-14.4936441507055,
116.76682264577)) ;
#162693 = CARTESIAN_POINT('Ctrl Pts',(-15.9878458146668,-14.4186618661927,
116.755595736523)) ;
#162694 = CARTESIAN_POINT('Ctrl Pts',(-16.0616496263278,-14.4186618819305,
116.731364598104)) ;
#162695 = CARTESIAN_POINT('Ctrl Pts',(-16.1354534379888,-14.4186618976683,
116.707133459686)) ;
#162696 = CARTESIAN_POINT('Ctrl Pts',(-16.1391394215636,-14.4936441821811,
116.718360368933)) ;
#162697 = CARTESIAN_POINT('Ctrl Pts',(-16.1428254051384,-14.5686264666939,
116.729587278181)) ;
#162698 = CARTESIAN_POINT('Ctrl Pts',(-16.0690215934775,-14.5686264509561,
116.753818416599)) ;
#162699 = CARTESIAN_POINT('Ctrl Pts',(-15.9952177818165,-14.5686264352184,
116.778049555018)) ;
#162700 = CARTESIAN_POINT('Ctrl Pts',(-15.9915317982417,-14.4936441507055,
116.76682264577)) ;
#162701 = CARTESIAN_POINT('Ctrl Pts',(-15.9111646098176,-14.4983888239063,
116.486541384417)) ;
#162702 = CARTESIAN_POINT('Ctrl Pts',(-15.9138185855326,-14.422965043811,
116.494624968275)) ;
#162703 = CARTESIAN_POINT('Ctrl Pts',(-15.9876223961134,-14.4229650315207,
116.470393826567)) ;
#162704 = CARTESIAN_POINT('Ctrl Pts',(-16.0614262066943,-14.4229650192305,
116.446162684859)) ;
#162705 = CARTESIAN_POINT('Ctrl Pts',(-16.0587722309793,-14.4983887993257,
116.438079101)) ;
#162706 = CARTESIAN_POINT('Ctrl Pts',(-16.0561182552643,-14.573812579421,
116.429995517142)) ;
#162707 = CARTESIAN_POINT('Ctrl Pts',(-15.9823144446834,-14.5738125917113,
116.45422665885)) ;
#162708 = CARTESIAN_POINT('Ctrl Pts',(-15.9085106341026,-14.5738126040015,
116.478457800559)) ;
#162709 = CARTESIAN_POINT('Ctrl Pts',(-15.9111646098176,-14.4983888239063,
116.486541384417)) ;
#162710 = CARTESIAN_POINT('Ctrl Pts',(-15.8339367194652,-14.426207251784,
116.215966892118)) ;
#162711 = CARTESIAN_POINT('Ctrl Pts',(-15.8427178234298,-14.3557121733631,
116.242712720049)) ;
#162712 = CARTESIAN_POINT('Ctrl Pts',(-15.9165216357164,-14.355712132954,
116.218481583536)) ;
#162713 = CARTESIAN_POINT('Ctrl Pts',(-15.9903254480029,-14.3557120925449,
116.194250447023)) ;
#162714 = CARTESIAN_POINT('Ctrl Pts',(-15.9815443440383,-14.4262071709657,
116.167504619092)) ;
#162715 = CARTESIAN_POINT('Ctrl Pts',(-15.9727632400736,-14.4967022493866,
116.140758791161)) ;
#162716 = CARTESIAN_POINT('Ctrl Pts',(-15.8989594277871,-14.4967022897957,
116.164989927674)) ;
#162717 = CARTESIAN_POINT('Ctrl Pts',(-15.8251556155005,-14.4967023302048,
116.189221064187)) ;
#162718 = CARTESIAN_POINT('Ctrl Pts',(-15.8339367194652,-14.426207251784,
116.215966892118)) ;
#162719 = CARTESIAN_POINT('Ctrl Pts',(-15.7654080575456,-14.2809809264381,
115.971651595224)) ;
#162720 = CARTESIAN_POINT('Ctrl Pts',(-15.7797229341676,-14.2205203869784,
116.015252401813)) ;
#162721 = CARTESIAN_POINT('Ctrl Pts',(-15.8535267507502,-14.2205203209335,
115.991021278385)) ;
#162722 = CARTESIAN_POINT('Ctrl Pts',(-15.9273305673328,-14.2205202548886,
115.966790154957)) ;
#162723 = CARTESIAN_POINT('Ctrl Pts',(-15.9130156907108,-14.2809807943484,
115.923189348368)) ;
#162724 = CARTESIAN_POINT('Ctrl Pts',(-15.8987008140888,-14.3414413338082,
115.879588541778)) ;
#162725 = CARTESIAN_POINT('Ctrl Pts',(-15.8248969975061,-14.3414413998531,
115.903819665206)) ;
#162726 = CARTESIAN_POINT('Ctrl Pts',(-15.7510931809235,-14.3414414658979,
115.928050788634)) ;
#162727 = CARTESIAN_POINT('Ctrl Pts',(-15.7654080575456,-14.2809809264381,
115.971651595224)) ;
#162728 = CARTESIAN_POINT('Ctrl Pts',(-15.7121638592197,-14.0755731076895,
115.774205354296)) ;
#162729 = CARTESIAN_POINT('Ctrl Pts',(-15.7309470596531,-14.0293643773253,
115.831415954248)) ;
#162730 = CARTESIAN_POINT('Ctrl Pts',(-15.8047508827093,-14.0293642911148,
115.807184850537)) ;
#162731 = CARTESIAN_POINT('Ctrl Pts',(-15.8785547057655,-14.0293642049043,
115.782953746827)) ;
#162732 = CARTESIAN_POINT('Ctrl Pts',(-15.8597715053321,-14.0755729352685,
115.725743146875)) ;
#162733 = CARTESIAN_POINT('Ctrl Pts',(-15.8409883048986,-14.1217816656326,
115.668532546923)) ;
#162734 = CARTESIAN_POINT('Ctrl Pts',(-15.7671844818424,-14.1217817518431,
115.692763650634)) ;
#162735 = CARTESIAN_POINT('Ctrl Pts',(-15.6933806587863,-14.1217818380536,
115.716994754344)) ;
#162736 = CARTESIAN_POINT('Ctrl Pts',(-15.7121638592197,-14.0755731076895,
115.774205354296)) ;
#162737 = CARTESIAN_POINT('Ctrl Pts',(-15.6778558958867,-13.8214647968314,
115.634145099666)) ;
#162738 = CARTESIAN_POINT('Ctrl Pts',(-15.699798207312,-13.7929280082953,
115.700977841948)) ;
#162739 = CARTESIAN_POINT('Ctrl Pts',(-15.7736020384604,-13.7929279092314,
115.676746762885)) ;
#162740 = CARTESIAN_POINT('Ctrl Pts',(-15.8474058696088,-13.7929278101675,
115.652515683822)) ;
#162741 = CARTESIAN_POINT('Ctrl Pts',(-15.8254635581835,-13.8214645987035,
115.58568294154)) ;
#162742 = CARTESIAN_POINT('Ctrl Pts',(-15.8035212467582,-13.8500013872396,
115.518850199258)) ;
#162743 = CARTESIAN_POINT('Ctrl Pts',(-15.7297174156098,-13.8500014863035,
115.543081278321)) ;
#162744 = CARTESIAN_POINT('Ctrl Pts',(-15.6559135844614,-13.8500015853674,
115.567312357384)) ;
#162745 = CARTESIAN_POINT('Ctrl Pts',(-15.6778558958867,-13.8214647968314,
115.634145099666)) ;
#162746 = CARTESIAN_POINT('Ctrl Pts',(-15.6663008904224,-13.5390721929965,
115.563497706539)) ;
#162747 = CARTESIAN_POINT('Ctrl Pts',(-15.6898162477156,-13.5302086359891,
115.635121692674)) ;
#162748 = CARTESIAN_POINT('Ctrl Pts',(-15.7636200876184,-13.5302085326853,
115.610890640275)) ;
#162749 = CARTESIAN_POINT('Ctrl Pts',(-15.8374239275211,-13.5302084293816,
115.586659587877)) ;
#162750 = CARTESIAN_POINT('Ctrl Pts',(-15.8139085702279,-13.539071986389,
115.515035601742)) ;
#162751 = CARTESIAN_POINT('Ctrl Pts',(-15.7903932129347,-13.5479355433964,
115.443411615607)) ;
#162752 = CARTESIAN_POINT('Ctrl Pts',(-15.7165893730319,-13.5479356467002,
115.467642668006)) ;
#162753 = CARTESIAN_POINT('Ctrl Pts',(-15.6427855331292,-13.5479357500039,
115.491873720405)) ;
#162754 = CARTESIAN_POINT('Ctrl Pts',(-15.6663008904224,-13.5390721929965,
115.563497706539)) ;
#162755 = CARTESIAN_POINT('Ctrl Pts',(-15.6788710235298,-13.2479213210197,
115.566312381468)) ;
#162756 = CARTESIAN_POINT('Ctrl Pts',(-15.7022779391019,-13.2593718199025,
115.637606071544)) ;
#162757 = CARTESIAN_POINT('Ctrl Pts',(-15.7760817875237,-13.2593717210079,
115.613375045094)) ;
#162758 = CARTESIAN_POINT('Ctrl Pts',(-15.8498856359456,-13.2593716221134,
115.589144018643)) ;
#162759 = CARTESIAN_POINT('Ctrl Pts',(-15.8264787203735,-13.2479211232306,
115.517850328566)) ;
#162760 = CARTESIAN_POINT('Ctrl Pts',(-15.8030718048014,-13.2364706243478,
115.446556638489)) ;
#162761 = CARTESIAN_POINT('Ctrl Pts',(-15.7292679563796,-13.2364707232423,
115.47078766494)) ;
#162762 = CARTESIAN_POINT('Ctrl Pts',(-15.6554641079578,-13.2364708221369,
115.495018691391)) ;
#162763 = CARTESIAN_POINT('Ctrl Pts',(-15.6788710235298,-13.2479213210197,
115.566312381468)) ;
#162764 = CARTESIAN_POINT('Ctrl Pts',(-15.7154570310451,-12.9689956696526,
115.642283838143)) ;
#162765 = CARTESIAN_POINT('Ctrl Pts',(-15.7370785345889,-12.9999372691398,
115.708139451166)) ;
#162766 = CARTESIAN_POINT('Ctrl Pts',(-15.8108823904318,-12.9999371823959,
115.683908447318)) ;
#162767 = CARTESIAN_POINT('Ctrl Pts',(-15.8846862462746,-12.9999370956519,
115.65967744347)) ;
#162768 = CARTESIAN_POINT('Ctrl Pts',(-15.8630647427309,-12.9689954961647,
115.593821830448)) ;
#162769 = CARTESIAN_POINT('Ctrl Pts',(-15.8414432391871,-12.9380538966775,
115.527966217425)) ;
#162770 = CARTESIAN_POINT('Ctrl Pts',(-15.7676393833442,-12.9380539834215,
115.552197221273)) ;
#162771 = CARTESIAN_POINT('Ctrl Pts',(-15.6938355275013,-12.9380540701654,
115.57642822512)) ;
#162772 = CARTESIAN_POINT('Ctrl Pts',(-15.7154570310451,-12.9689956696526,
115.642283838143)) ;
#162773 = CARTESIAN_POINT('Ctrl Pts',(-15.7742309880506,-12.7220961737177,
115.785813685881)) ;
#162774 = CARTESIAN_POINT('Ctrl Pts',(-15.7925158427138,-12.7703223930981,
115.841506404667)) ;
#162775 = CARTESIAN_POINT('Ctrl Pts',(-15.8663197041459,-12.7703223245763,
115.817275417843)) ;
#162776 = CARTESIAN_POINT('Ctrl Pts',(-15.9401235655779,-12.7703222560545,
115.793044431019)) ;
#162777 = CARTESIAN_POINT('Ctrl Pts',(-15.9218387109147,-12.7220960366741,
115.737351712233)) ;
#162778 = CARTESIAN_POINT('Ctrl Pts',(-15.9035538562515,-12.6738698172937,
115.681658993447)) ;
#162779 = CARTESIAN_POINT('Ctrl Pts',(-15.8297499948195,-12.6738698858155,
115.705889980271)) ;
#162780 = CARTESIAN_POINT('Ctrl Pts',(-15.7559461333875,-12.6738699543374,
115.730120967095)) ;
#162781 = CARTESIAN_POINT('Ctrl Pts',(-15.7742309880506,-12.7220961737177,
115.785813685881)) ;
#162782 = CARTESIAN_POINT('Ctrl Pts',(-15.8515784407682,-12.5254520180373,
115.985975276655)) ;
#162783 = CARTESIAN_POINT('Ctrl Pts',(-15.8652235858158,-12.5874803484278,
116.027536188445)) ;
#162784 = CARTESIAN_POINT('Ctrl Pts',(-15.9390274506629,-12.5874803012304,
116.003305212022)) ;
#162785 = CARTESIAN_POINT('Ctrl Pts',(-16.0128313155099,-12.5874802540331,
115.9790742356)) ;
#162786 = CARTESIAN_POINT('Ctrl Pts',(-15.9991861704623,-12.5254519236426,
115.93751332381)) ;
#162787 = CARTESIAN_POINT('Ctrl Pts',(-15.9855410254147,-12.463423593252,
115.89595241202)) ;
#162788 = CARTESIAN_POINT('Ctrl Pts',(-15.9117371605676,-12.4634236404494,
115.920183388442)) ;
#162789 = CARTESIAN_POINT('Ctrl Pts',(-15.8379332957206,-12.4634236876467,
115.944414364864)) ;
#162790 = CARTESIAN_POINT('Ctrl Pts',(-15.8515784407682,-12.5254520180373,
115.985975276655)) ;
#162791 = CARTESIAN_POINT('Ctrl Pts',(-15.94270937751,-12.3924871288094,116.22814157512)) ;
#162792 = CARTESIAN_POINT('Ctrl Pts',(-15.9507450204375,-12.4638924990082,
116.252616848413)) ;
#162793 = CARTESIAN_POINT('Ctrl Pts',(-16.0245488864703,-12.4638924741093,
116.228385875602)) ;
#162794 = CARTESIAN_POINT('Ctrl Pts',(-16.0983527525031,-12.4638924492103,
116.204154902791)) ;
#162795 = CARTESIAN_POINT('Ctrl Pts',(-16.0903171095756,-12.3924870790115,
116.179679629498)) ;
#162796 = CARTESIAN_POINT('Ctrl Pts',(-16.0822814666481,-12.3210817088127,
116.155204356205)) ;
#162797 = CARTESIAN_POINT('Ctrl Pts',(-16.0084776006153,-12.3210817337116,
116.179435329016)) ;
#162798 = CARTESIAN_POINT('Ctrl Pts',(-15.9346737345826,-12.3210817586106,
116.203666301827)) ;
#162799 = CARTESIAN_POINT('Ctrl Pts',(-15.94270937751,-12.3924871288094,116.22814157512)) ;
#162800 = CARTESIAN_POINT('Ctrl Pts',(-16.0425166341127,-12.3327720085306,
116.496536154784)) ;
#162801 = CARTESIAN_POINT('Ctrl Pts',(-16.0443326725553,-12.4084551705648,
116.502067516169)) ;
#162802 = CARTESIAN_POINT('Ctrl Pts',(-16.1181365370123,-12.4084551665108,
116.477836538559)) ;
#162803 = CARTESIAN_POINT('Ctrl Pts',(-16.1919404014694,-12.4084551624567,
116.453605560949)) ;
#162804 = CARTESIAN_POINT('Ctrl Pts',(-16.1901243630268,-12.3327720004226,
116.448074199563)) ;
#162805 = CARTESIAN_POINT('Ctrl Pts',(-16.1883083245843,-12.2570888383885,
116.442542838178)) ;
#162806 = CARTESIAN_POINT('Ctrl Pts',(-16.1145044601272,-12.2570888424425,
116.466773815788)) ;
#162807 = CARTESIAN_POINT('Ctrl Pts',(-16.0407005956702,-12.2570888464965,
116.491004793398)) ;
#162808 = CARTESIAN_POINT('Ctrl Pts',(-16.0425166341127,-12.3327720085306,
116.496536154784)) ;
#162809 = CARTESIAN_POINT('Ctrl Pts',(-16.1432965454572,-12.3509988977752,
116.768165464397)) ;
#162810 = CARTESIAN_POINT('Ctrl Pts',(-16.1388098877865,-12.4255237330698,
116.754499830221)) ;
#162811 = CARTESIAN_POINT('Ctrl Pts',(-16.2126137496675,-12.4255237455323,
116.730268844765)) ;
#162812 = CARTESIAN_POINT('Ctrl Pts',(-16.2864176115484,-12.4255237579948,
116.706037859308)) ;
#162813 = CARTESIAN_POINT('Ctrl Pts',(-16.2909042692191,-12.3509989227002,
116.719703493484)) ;
#162814 = CARTESIAN_POINT('Ctrl Pts',(-16.2953909268898,-12.2764740874057,
116.733369127659)) ;
#162815 = CARTESIAN_POINT('Ctrl Pts',(-16.2215870650088,-12.2764740749432,
116.757600113116)) ;
#162816 = CARTESIAN_POINT('Ctrl Pts',(-16.1477832031279,-12.2764740624807,
116.781831098573)) ;
#162817 = CARTESIAN_POINT('Ctrl Pts',(-16.1432965454572,-12.3509988977752,
116.768165464397)) ;
#162818 = CARTESIAN_POINT('Ctrl Pts',(-16.2397734663179,-12.4453838611795,
117.026540426964)) ;
#162819 = CARTESIAN_POINT('Ctrl Pts',(-16.2292780482387,-12.5134317382336,
116.994573077925)) ;
#162820 = CARTESIAN_POINT('Ctrl Pts',(-16.3030819059699,-12.5134317622461,
116.970342079829)) ;
#162821 = CARTESIAN_POINT('Ctrl Pts',(-16.3768857637012,-12.5134317862586,
116.946111081733)) ;
#162822 = CARTESIAN_POINT('Ctrl Pts',(-16.3873811817803,-12.4453839092044,
116.978078430772)) ;
#162823 = CARTESIAN_POINT('Ctrl Pts',(-16.3978765998595,-12.3773360321503,
117.01004577981)) ;
#162824 = CARTESIAN_POINT('Ctrl Pts',(-16.3240727421283,-12.3773360081379,
117.034276777906)) ;
#162825 = CARTESIAN_POINT('Ctrl Pts',(-16.2502688843971,-12.3773359841254,
117.058507776003)) ;
#162826 = CARTESIAN_POINT('Ctrl Pts',(-16.2397734663179,-12.4453838611795,
117.026540426964)) ;
#162827 = CARTESIAN_POINT('Ctrl Pts',(-16.3254447848863,-12.6100760699984,
117.251940625839)) ;
#162828 = CARTESIAN_POINT('Ctrl Pts',(-16.3096871062923,-12.6667282433853,
117.203945280152)) ;
#162829 = CARTESIAN_POINT('Ctrl Pts',(-16.3834909593544,-12.6667282722992,
117.179714267834)) ;
#162830 = CARTESIAN_POINT('Ctrl Pts',(-16.4572948124166,-12.6667283012131,
117.155483255517)) ;
#162831 = CARTESIAN_POINT('Ctrl Pts',(-16.4730524910106,-12.6100761278262,
117.203478601204)) ;
#162832 = CARTESIAN_POINT('Ctrl Pts',(-16.4888101696046,-12.5534239544393,
117.251473946891)) ;
#162833 = CARTESIAN_POINT('Ctrl Pts',(-16.4150063165425,-12.5534239255254,
117.275704959209)) ;
#162834 = CARTESIAN_POINT('Ctrl Pts',(-16.3412024634803,-12.5534238966115,
117.299935971526)) ;
#162835 = CARTESIAN_POINT('Ctrl Pts',(-16.3254447848863,-12.6100760699984,
117.251940625839)) ;
#162836 = CARTESIAN_POINT('Ctrl Pts',(-16.3945559404646,-12.8316470477012,
117.427060764436)) ;
#162837 = CARTESIAN_POINT('Ctrl Pts',(-16.3746810642588,-12.8729143960197,
117.366525098979)) ;
#162838 = CARTESIAN_POINT('Ctrl Pts',(-16.4484849132355,-12.8729144255077,
117.342294074218)) ;
#162839 = CARTESIAN_POINT('Ctrl Pts',(-16.5222887622122,-12.8729144549957,
117.318063049457)) ;
#162840 = CARTESIAN_POINT('Ctrl Pts',(-16.542163638418,-12.8316471066773,
117.378598714914)) ;
#162841 = CARTESIAN_POINT('Ctrl Pts',(-16.5620385146238,-12.7903797583588,
117.439134380371)) ;
#162842 = CARTESIAN_POINT('Ctrl Pts',(-16.4882346656471,-12.7903797288708,
117.463365405132)) ;
#162843 = CARTESIAN_POINT('Ctrl Pts',(-16.4144308166704,-12.7903796993828,
117.487596429893)) ;
#162844 = CARTESIAN_POINT('Ctrl Pts',(-16.3945559404646,-12.8316470477012,
117.427060764436)) ;
#162845 = CARTESIAN_POINT('Ctrl Pts',(-16.4435312853677,-13.0973555362981,
117.540560244616)) ;
#162846 = CARTESIAN_POINT('Ctrl Pts',(-16.4209446285881,-13.1201328482756,
117.471764932878)) ;
#162847 = CARTESIAN_POINT('Ctrl Pts',(-16.4947484740099,-13.1201328716907,
117.44753389729)) ;
#162848 = CARTESIAN_POINT('Ctrl Pts',(-16.5685523194317,-13.1201328951058,
117.423302861701)) ;
#162849 = CARTESIAN_POINT('Ctrl Pts',(-16.5911389762113,-13.0973555831283,
117.492098173439)) ;
#162850 = CARTESIAN_POINT('Ctrl Pts',(-16.6137256329909,-13.0745782711508,
117.560893485177)) ;
#162851 = CARTESIAN_POINT('Ctrl Pts',(-16.5399217875691,-13.0745782477357,
117.585124520766)) ;
#162852 = CARTESIAN_POINT('Ctrl Pts',(-16.4661179421473,-13.0745782243206,
117.609355556355)) ;
#162853 = CARTESIAN_POINT('Ctrl Pts',(-16.4435312853677,-13.0973555362981,
117.540560244616)) ;
#162854 = CARTESIAN_POINT('Ctrl Pts',(-16.4688621130792,-13.3829827267331,
117.582449970111)) ;
#162855 = CARTESIAN_POINT('Ctrl Pts',(-16.4452025092137,-13.3858507921175,
117.510386634553)) ;
#162856 = CARTESIAN_POINT('Ctrl Pts',(-16.5190063526211,-13.3858508103817,
117.486155592829)) ;
#162857 = CARTESIAN_POINT('Ctrl Pts',(-16.5928101960284,-13.3858508286459,
117.461924551104)) ;
#162858 = CARTESIAN_POINT('Ctrl Pts',(-16.6164697998939,-13.3829827632615,
117.533987886662)) ;
#162859 = CARTESIAN_POINT('Ctrl Pts',(-16.6401294037594,-13.380114697877,
117.60605122222)) ;
#162860 = CARTESIAN_POINT('Ctrl Pts',(-16.566325560352,-13.3801146796128,
117.630282263945)) ;
#162861 = CARTESIAN_POINT('Ctrl Pts',(-16.4925217169447,-13.3801146613487,
117.654513305669)) ;
#162862 = CARTESIAN_POINT('Ctrl Pts',(-16.4688621130792,-13.3829827267331,
117.582449970111)) ;
#162863 = CARTESIAN_POINT('Ctrl Pts',(-16.470124542703,-13.6735145155205,
117.550719313167)) ;
#162864 = CARTESIAN_POINT('Ctrl Pts',(-16.4470771654852,-13.6561003398034,
117.480520721043)) ;
#162865 = CARTESIAN_POINT('Ctrl Pts',(-16.5208810079376,-13.6561003497692,
117.45628967641)) ;
#162866 = CARTESIAN_POINT('Ctrl Pts',(-16.5946848503899,-13.656100359735,
117.432058631777)) ;
#162867 = CARTESIAN_POINT('Ctrl Pts',(-16.6177322276078,-13.673514535452,
117.502257223901)) ;
#162868 = CARTESIAN_POINT('Ctrl Pts',(-16.6407796048256,-13.690928711169,
117.572455816025)) ;
#162869 = CARTESIAN_POINT('Ctrl Pts',(-16.5669757623732,-13.6909287012033,
117.596686860658)) ;
#162870 = CARTESIAN_POINT('Ctrl Pts',(-16.4931719199208,-13.6909286912375,
117.620917905291)) ;
#162871 = CARTESIAN_POINT('Ctrl Pts',(-16.470124542703,-13.6735145155205,
117.550719313167)) ;
#162872 = CARTESIAN_POINT('Ctrl Pts',(-16.4477134830108,-13.9443960540442,
117.447059781621)) ;
#162873 = CARTESIAN_POINT('Ctrl Pts',(-16.4269288979224,-13.9080411308625,
117.383753289118)) ;
#162874 = CARTESIAN_POINT('Ctrl Pts',(-16.5007327404672,-13.9080411350017,
117.359522244767)) ;
#162875 = CARTESIAN_POINT('Ctrl Pts',(-16.574536583012,-13.9080411391408,
117.335291200415)) ;
#162876 = CARTESIAN_POINT('Ctrl Pts',(-16.5953211681005,-13.9443960623225,
117.398597692918)) ;
#162877 = CARTESIAN_POINT('Ctrl Pts',(-16.616105753189,-13.9807509855041,
117.461904185421)) ;
#162878 = CARTESIAN_POINT('Ctrl Pts',(-16.5423019106441,-13.980750981365,
117.486135229772)) ;
#162879 = CARTESIAN_POINT('Ctrl Pts',(-16.4684980680993,-13.9807509772258,
117.510366274124)) ;
#162880 = CARTESIAN_POINT('Ctrl Pts',(-16.4477134830108,-13.9443960540442,
117.447059781621)) ;
#162881 = CARTESIAN_POINT('Ctrl Pts',(-16.4040416496053,-14.1780473237906,
117.278577420489)) ;
#162882 = CARTESIAN_POINT('Ctrl Pts',(-16.3870093108388,-14.125322660068,
117.226699664773)) ;
#162883 = CARTESIAN_POINT('Ctrl Pts',(-16.460813154071,-14.12532266015,117.202468622515)) ;
#162884 = CARTESIAN_POINT('Ctrl Pts',(-16.5346169973033,-14.1253226602321,
117.178237580257)) ;
#162885 = CARTESIAN_POINT('Ctrl Pts',(-16.5516493360698,-14.1780473239547,
117.230115335974)) ;
#162886 = CARTESIAN_POINT('Ctrl Pts',(-16.5686816748364,-14.2307719876773,
117.28199309169)) ;
#162887 = CARTESIAN_POINT('Ctrl Pts',(-16.4948778316041,-14.2307719875953,
117.306224133948)) ;
#162888 = CARTESIAN_POINT('Ctrl Pts',(-16.4210739883719,-14.2307719875132,
117.330455176205)) ;
#162889 = CARTESIAN_POINT('Ctrl Pts',(-16.4040416496053,-14.1780473237906,
117.278577420489)) ;
#162890 = CARTESIAN_POINT('Ctrl Pts',(-16.3431014881368,-14.3571729772058,
117.057559267268)) ;
#162891 = CARTESIAN_POINT('Ctrl Pts',(-16.3310317024854,-14.2918617658065,
117.020796647579)) ;
#162892 = CARTESIAN_POINT('Ctrl Pts',(-16.4048355465375,-14.2918617643923,
116.996565607819)) ;
#162893 = CARTESIAN_POINT('Ctrl Pts',(-16.4786393905896,-14.291861762978,
116.972334568058)) ;
#162894 = CARTESIAN_POINT('Ctrl Pts',(-16.4907091762409,-14.3571729743773,
117.009097187747)) ;
#162895 = CARTESIAN_POINT('Ctrl Pts',(-16.5027789618923,-14.4224841857766,
117.045859807437)) ;
#162896 = CARTESIAN_POINT('Ctrl Pts',(-16.4289751178402,-14.4224841871909,
117.070090847197)) ;
#162897 = CARTESIAN_POINT('Ctrl Pts',(-16.3551712737882,-14.4224841886051,
117.094321886958)) ;
#162898 = CARTESIAN_POINT('Ctrl Pts',(-16.3431014881368,-14.3571729772058,
117.057559267268)) ;
#162899 = CARTESIAN_POINT('Ctrl Pts',(-16.2692843220695,-14.4697035049953,
116.797034589842)) ;
#162900 = CARTESIAN_POINT('Ctrl Pts',(-16.2630899618578,-14.3964364704153,
116.778167568028)) ;
#162901 = CARTESIAN_POINT('Ctrl Pts',(-16.3368938062969,-14.3964364695808,
116.753936529446)) ;
#162902 = CARTESIAN_POINT('Ctrl Pts',(-16.410697650736,-14.3964364687462,
116.729705490864)) ;
#162903 = CARTESIAN_POINT('Ctrl Pts',(-16.4168920109476,-14.4697035033262,
116.748572512678)) ;
#162904 = CARTESIAN_POINT('Ctrl Pts',(-16.4230863711593,-14.5429705379062,
116.767439534492)) ;
#162905 = CARTESIAN_POINT('Ctrl Pts',(-16.3492825267203,-14.5429705387408,
116.791670573074)) ;
#162906 = CARTESIAN_POINT('Ctrl Pts',(-16.2754786822812,-14.5429705395753,
116.815901611656)) ;
#162907 = CARTESIAN_POINT('Ctrl Pts',(-16.2692843220695,-14.4697035049953,
116.797034589842)) ;
#162908 = CARTESIAN_POINT('Ctrl Pts',(-16.189974204939,-14.5058316151569,
116.520142021784)) ;
#162909 = CARTESIAN_POINT('Ctrl Pts',(-16.1900398398108,-14.4299343068103,
116.520341934979)) ;
#162910 = CARTESIAN_POINT('Ctrl Pts',(-16.2638436837928,-14.4299343070279,
116.496110895004)) ;
#162911 = CARTESIAN_POINT('Ctrl Pts',(-16.3376475277747,-14.4299343072455,
116.47187985503)) ;
#162912 = CARTESIAN_POINT('Ctrl Pts',(-16.3375818929029,-14.5058316155922,
116.471679941836)) ;
#162913 = CARTESIAN_POINT('Ctrl Pts',(-16.3375162580311,-14.5817289239388,
116.471480028642)) ;
#162914 = CARTESIAN_POINT('Ctrl Pts',(-16.2637124140491,-14.5817289237212,
116.495711068616)) ;
#162915 = CARTESIAN_POINT('Ctrl Pts',(-16.1899085700672,-14.5817289235035,
116.51994210859)) ;
#162916 = CARTESIAN_POINT('Ctrl Pts',(-16.189974204939,-14.5058316151569,
116.520142021784)) ;
#162917 = CARTESIAN_POINT('Ctrl Pts',(-16.1107202304642,-14.4647781183691,
116.243348321315)) ;
#162918 = CARTESIAN_POINT('Ctrl Pts',(-16.1170525275077,-14.3916362177671,
116.262635476418)) ;
#162919 = CARTESIAN_POINT('Ctrl Pts',(-16.1908563705672,-14.3916362178144,
116.238404433634)) ;
#162920 = CARTESIAN_POINT('Ctrl Pts',(-16.2646602136268,-14.3916362178617,
116.21417339085)) ;
#162921 = CARTESIAN_POINT('Ctrl Pts',(-16.2583279165833,-14.4647781184637,
116.194886235748)) ;
#162922 = CARTESIAN_POINT('Ctrl Pts',(-16.2519956195399,-14.5379200190658,
116.175599080645)) ;
#162923 = CARTESIAN_POINT('Ctrl Pts',(-16.1781917764803,-14.5379200190184,
116.199830123429)) ;
#162924 = CARTESIAN_POINT('Ctrl Pts',(-16.1043879334208,-14.5379200189711,
116.224061166212)) ;
#162925 = CARTESIAN_POINT('Ctrl Pts',(-16.1107202304642,-14.4647781183691,
116.243348321315)) ;
#162926 = CARTESIAN_POINT('Ctrl Pts',(-16.03788617739,-14.3484987257117,115.986015587949)) ;
#162927 = CARTESIAN_POINT('Ctrl Pts',(-16.0500479103369,-14.2833691759875,
116.023058264334)) ;
#162928 = CARTESIAN_POINT('Ctrl Pts',(-16.1238517520509,-14.2833691732841,
115.998827217452)) ;
#162929 = CARTESIAN_POINT('Ctrl Pts',(-16.1976555937649,-14.2833691705807,
115.97459617057)) ;
#162930 = CARTESIAN_POINT('Ctrl Pts',(-16.1854938608181,-14.3484987203049,
115.937553494185)) ;
#162931 = CARTESIAN_POINT('Ctrl Pts',(-16.1733321278713,-14.4136282700291,
115.9005108178)) ;
#162932 = CARTESIAN_POINT('Ctrl Pts',(-16.0995282861572,-14.4136282727325,
115.924741864682)) ;
#162933 = CARTESIAN_POINT('Ctrl Pts',(-16.0257244444432,-14.4136282754358,
115.948972911564)) ;
#162934 = CARTESIAN_POINT('Ctrl Pts',(-16.03788617739,-14.3484987257117,115.986015587949)) ;
#162935 = CARTESIAN_POINT('Ctrl Pts',(-15.9776687836141,-14.1655053892491,
115.767116814539)) ;
#162936 = CARTESIAN_POINT('Ctrl Pts',(-15.994787213724,-14.1130583565086,
115.819256790845)) ;
#162937 = CARTESIAN_POINT('Ctrl Pts',(-16.0685910543299,-14.1130583479537,
115.795025740588)) ;
#162938 = CARTESIAN_POINT('Ctrl Pts',(-16.1423948949358,-14.1130583393988,
115.77079469033)) ;
#162939 = CARTESIAN_POINT('Ctrl Pts',(-16.1252764648259,-14.1655053721393,
115.718654714025)) ;
#162940 = CARTESIAN_POINT('Ctrl Pts',(-16.1081580347159,-14.2179524048798,
115.666514737719)) ;
#162941 = CARTESIAN_POINT('Ctrl Pts',(-16.0343541941101,-14.2179524134347,
115.690745787976)) ;
#162942 = CARTESIAN_POINT('Ctrl Pts',(-15.9605503535042,-14.2179524219896,
115.714976838234)) ;
#162943 = CARTESIAN_POINT('Ctrl Pts',(-15.9776687836141,-14.1655053892491,
115.767116814539)) ;
#162944 = CARTESIAN_POINT('Ctrl Pts',(-15.9351536436701,-13.9286208259661,
115.602105173613)) ;
#162945 = CARTESIAN_POINT('Ctrl Pts',(-15.9560004743455,-13.8926376196403,
115.665601256615)) ;
#162946 = CARTESIAN_POINT('Ctrl Pts',(-16.0298043146523,-13.8926376022121,
115.641370205447)) ;
#162947 = CARTESIAN_POINT('Ctrl Pts',(-16.1036081549591,-13.8926375847838,
115.617139154278)) ;
#162948 = CARTESIAN_POINT('Ctrl Pts',(-16.0827613242837,-13.9286207911095,
115.553643071277)) ;
#162949 = CARTESIAN_POINT('Ctrl Pts',(-16.0619144936083,-13.9646039974353,
115.490146988275)) ;
#162950 = CARTESIAN_POINT('Ctrl Pts',(-15.9881106533015,-13.9646040148635,
115.514378039444)) ;
#162951 = CARTESIAN_POINT('Ctrl Pts',(-15.9143068129948,-13.9646040322918,
115.538609090612)) ;
#162952 = CARTESIAN_POINT('Ctrl Pts',(-15.9351536436701,-13.9286208259661,
115.602105173613)) ;
#162953 = CARTESIAN_POINT('Ctrl Pts',(-15.9141622270948,-13.6565946963034,
115.502836000379)) ;
#162954 = CARTESIAN_POINT('Ctrl Pts',(-15.9372359188981,-13.6395527561257,
115.573114743203)) ;
#162955 = CARTESIAN_POINT('Ctrl Pts',(-16.0110397602486,-13.6395527301396,
115.548883695214)) ;
#162956 = CARTESIAN_POINT('Ctrl Pts',(-16.0848436015992,-13.6395527041535,
115.524652647225)) ;
#162957 = CARTESIAN_POINT('Ctrl Pts',(-16.0617699097959,-13.6565946443312,
115.454373904401)) ;
#162958 = CARTESIAN_POINT('Ctrl Pts',(-16.0386962179926,-13.6736365845089,
115.384095161576)) ;
#162959 = CARTESIAN_POINT('Ctrl Pts',(-15.9648923766421,-13.673636610495,
115.408326209565)) ;
#162960 = CARTESIAN_POINT('Ctrl Pts',(-15.8910885352915,-13.6736366364811,
115.432557257555)) ;
#162961 = CARTESIAN_POINT('Ctrl Pts',(-15.9141622270948,-13.6565946963034,
115.502836000379)) ;
#162962 = CARTESIAN_POINT('Ctrl Pts',(-15.9168400704658,-13.3650274692435,
115.475347116262)) ;
#162963 = CARTESIAN_POINT('Ctrl Pts',(-15.9404979400582,-13.3683183370286,
115.547405170571)) ;
#162964 = CARTESIAN_POINT('Ctrl Pts',(-16.0143017837554,-13.368318300107,
115.52317412973)) ;
#162965 = CARTESIAN_POINT('Ctrl Pts',(-16.0881056274526,-13.3683182631854,
115.498943088888)) ;
#162966 = CARTESIAN_POINT('Ctrl Pts',(-16.0644477578601,-13.3650273954003,
115.426885034579)) ;
#162967 = CARTESIAN_POINT('Ctrl Pts',(-16.0407898882677,-13.3617365276153,
115.35482698027)) ;
#162968 = CARTESIAN_POINT('Ctrl Pts',(-15.9669860445706,-13.3617365645369,
115.379058021112)) ;
#162969 = CARTESIAN_POINT('Ctrl Pts',(-15.8931822008734,-13.3617366014585,
115.403289061953)) ;
#162970 = CARTESIAN_POINT('Ctrl Pts',(-15.9168400704658,-13.3650274692435,
115.475347116262)) ;
#162971 = CARTESIAN_POINT('Ctrl Pts',(-15.943917468856,-13.0788343995772,
115.522370330454)) ;
#162972 = CARTESIAN_POINT('Ctrl Pts',(-15.9664525229632,-13.1021119946019,
115.591008470126)) ;
#162973 = CARTESIAN_POINT('Ctrl Pts',(-16.0402563706024,-13.1021119511676,
115.566777441291)) ;
#162974 = CARTESIAN_POINT('Ctrl Pts',(-16.1140602182415,-13.1021119077334,
115.542546412456)) ;
#162975 = CARTESIAN_POINT('Ctrl Pts',(-16.0915251641342,-13.0788343127088,
115.473908272784)) ;
#162976 = CARTESIAN_POINT('Ctrl Pts',(-16.068990110027,-13.0555567176841,
115.405270133111)) ;
#162977 = CARTESIAN_POINT('Ctrl Pts',(-15.9951862623878,-13.0555567611183,
115.429501161946)) ;
#162978 = CARTESIAN_POINT('Ctrl Pts',(-15.9213824147487,-13.0555568045526,
115.453732190781)) ;
#162979 = CARTESIAN_POINT('Ctrl Pts',(-15.943917468856,-13.0788343995772,
115.522370330454)) ;
#162980 = CARTESIAN_POINT('Ctrl Pts',(-15.9938421820601,-12.8175211583994,
115.639074782229)) ;
#162981 = CARTESIAN_POINT('Ctrl Pts',(-16.0136556516188,-12.8590768776832,
115.699423414641)) ;
#162982 = CARTESIAN_POINT('Ctrl Pts',(-16.0874595039968,-12.8590768329722,
115.67519240024)) ;
#162983 = CARTESIAN_POINT('Ctrl Pts',(-16.1612633563749,-12.8590767882613,
115.650961385839)) ;
#162984 = CARTESIAN_POINT('Ctrl Pts',(-16.1414498868162,-12.8175210689774,
115.590612753427)) ;
#162985 = CARTESIAN_POINT('Ctrl Pts',(-16.1216364172575,-12.7759653496935,
115.530264121016)) ;
#162986 = CARTESIAN_POINT('Ctrl Pts',(-16.0478325648795,-12.7759653944045,
115.554495135417)) ;
#162987 = CARTESIAN_POINT('Ctrl Pts',(-15.9740287125014,-12.7759654391155,
115.578726149818)) ;
#162988 = CARTESIAN_POINT('Ctrl Pts',(-15.9938421820601,-12.8175211583994,
115.639074782229)) ;
#162989 = CARTESIAN_POINT('Ctrl Pts',(-16.0641439891467,-12.5984995679009,
115.817749196681)) ;
#162990 = CARTESIAN_POINT('Ctrl Pts',(-16.0798113378379,-12.6554070787726,
115.865469414067)) ;
#162991 = CARTESIAN_POINT('Ctrl Pts',(-16.1536151955778,-12.6554070377801,
115.841238415998)) ;
#162992 = CARTESIAN_POINT('Ctrl Pts',(-16.2274190533178,-12.6554069967877,
115.817007417928)) ;
#162993 = CARTESIAN_POINT('Ctrl Pts',(-16.2117517046266,-12.5984994859161,
115.769287200542)) ;
#162994 = CARTESIAN_POINT('Ctrl Pts',(-16.1960843559353,-12.5415919750444,
115.721566983155)) ;
#162995 = CARTESIAN_POINT('Ctrl Pts',(-16.1222804981954,-12.5415920160368,
115.745797981225)) ;
#162996 = CARTESIAN_POINT('Ctrl Pts',(-16.0484766404554,-12.5415920570292,
115.770028979294)) ;
#162997 = CARTESIAN_POINT('Ctrl Pts',(-16.0641439891467,-12.5984995679009,
115.817749196681)) ;
#162998 = CARTESIAN_POINT('Ctrl Pts',(-16.1502868270294,-12.4381081950322,
116.044719588303)) ;
#162999 = CARTESIAN_POINT('Ctrl Pts',(-16.1606951475451,-12.5062960463662,
116.076421654558)) ;
#163000 = CARTESIAN_POINT('Ctrl Pts',(-16.2344990103366,-12.5062960154841,
116.052190671875)) ;
#163001 = CARTESIAN_POINT('Ctrl Pts',(-16.3083028731281,-12.506295984602,
116.027959689191)) ;
#163002 = CARTESIAN_POINT('Ctrl Pts',(-16.2978945526124,-12.4381081332681,
115.996257622937)) ;
#163003 = CARTESIAN_POINT('Ctrl Pts',(-16.2874862320967,-12.3699202819341,
115.964555556682)) ;
#163004 = CARTESIAN_POINT('Ctrl Pts',(-16.2136823693052,-12.3699203128162,
115.988786539365)) ;
#163005 = CARTESIAN_POINT('Ctrl Pts',(-16.1398785065137,-12.3699203436983,
116.013017522048)) ;
#163006 = CARTESIAN_POINT('Ctrl Pts',(-16.1502868270294,-12.4381081950322,
116.044719588303)) ;
#163007 = CARTESIAN_POINT('Ctrl Pts',(-16.2478432903342,-12.3474840033873,
116.306149605933)) ;
#163008 = CARTESIAN_POINT('Ctrl Pts',(-16.2521946188714,-12.4220984887537,
116.319403052103)) ;
#163009 = CARTESIAN_POINT('Ctrl Pts',(-16.3259984865435,-12.4220984739895,
116.295172084286)) ;
#163010 = CARTESIAN_POINT('Ctrl Pts',(-16.3998023542157,-12.4220984592253,
116.270941116468)) ;
#163011 = CARTESIAN_POINT('Ctrl Pts',(-16.3954510256785,-12.3474839738589,
116.257687670298)) ;
#163012 = CARTESIAN_POINT('Ctrl Pts',(-16.3910996971414,-12.2728694884925,
116.244434224128)) ;
#163013 = CARTESIAN_POINT('Ctrl Pts',(-16.3172958294692,-12.2728695032567,
116.268665191945)) ;
#163014 = CARTESIAN_POINT('Ctrl Pts',(-16.243491961797,-12.2728695180209,
116.292896159763)) ;
#163015 = CARTESIAN_POINT('Ctrl Pts',(-16.2478432903342,-12.3474840033873,
116.306149605933)) ;
#163016 = CARTESIAN_POINT('Ctrl Pts',(-16.3485101468529,-12.3342746176406,
116.577507728098)) ;
#163017 = CARTESIAN_POINT('Ctrl Pts',(-16.3465689953954,-12.4099190416296,
116.571595295596)) ;
#163018 = CARTESIAN_POINT('Ctrl Pts',(-16.4203728650902,-12.4099190485564,
116.547364333939)) ;
#163019 = CARTESIAN_POINT('Ctrl Pts',(-16.4941767347851,-12.4099190554831,
116.523133372282)) ;
#163020 = CARTESIAN_POINT('Ctrl Pts',(-16.4961178862426,-12.3342746314941,
116.529045804785)) ;
#163021 = CARTESIAN_POINT('Ctrl Pts',(-16.4980590377001,-12.2586302075051,
116.534958237287)) ;
#163022 = CARTESIAN_POINT('Ctrl Pts',(-16.4242551680053,-12.2586302005783,
116.559189198944)) ;
#163023 = CARTESIAN_POINT('Ctrl Pts',(-16.3504512983104,-12.2586301936515,
116.5834201606)) ;
#163024 = CARTESIAN_POINT('Ctrl Pts',(-16.3485101468529,-12.3342746176406,
116.577507728098)) ;
#163025 = CARTESIAN_POINT('Ctrl Pts',(-16.4477907403322,-12.3983523506611,
116.844372055818)) ;
#163026 = CARTESIAN_POINT('Ctrl Pts',(-16.4396504910612,-12.4696333213927,
116.819578171729)) ;
#163027 = CARTESIAN_POINT('Ctrl Pts',(-16.513454361231,-12.4696333527669,
116.795347211519)) ;
#163028 = CARTESIAN_POINT('Ctrl Pts',(-16.5872582314008,-12.4696333841411,
116.771116251309)) ;
#163029 = CARTESIAN_POINT('Ctrl Pts',(-16.5953984806718,-12.3983524134095,
116.795910135398)) ;
#163030 = CARTESIAN_POINT('Ctrl Pts',(-16.6035387299428,-12.3270714426779,
116.820704019487)) ;
#163031 = CARTESIAN_POINT('Ctrl Pts',(-16.529734859773,-12.3270714113037,
116.844934979697)) ;
#163032 = CARTESIAN_POINT('Ctrl Pts',(-16.4559309896032,-12.3270713799295,
116.869165939907)) ;
#163033 = CARTESIAN_POINT('Ctrl Pts',(-16.4477907403322,-12.3983523506611,
116.844372055818)) ;
#163034 = CARTESIAN_POINT('Ctrl Pts',(-16.5383794781962,-12.5353914606374,
117.084853142342)) ;
#163035 = CARTESIAN_POINT('Ctrl Pts',(-16.5246360542602,-12.5972087494759,
117.042992892395)) ;
#163036 = CARTESIAN_POINT('Ctrl Pts',(-16.5984399222197,-12.5972088056809,
117.018761925452)) ;
#163037 = CARTESIAN_POINT('Ctrl Pts',(-16.6722437901792,-12.5972088618859,
116.99453095851)) ;
#163038 = CARTESIAN_POINT('Ctrl Pts',(-16.6859872141153,-12.5353915730474,
117.036391208458)) ;
#163039 = CARTESIAN_POINT('Ctrl Pts',(-16.6997306380514,-12.4735742842089,
117.078251458405)) ;
#163040 = CARTESIAN_POINT('Ctrl Pts',(-16.6259267700919,-12.4735742280039,
117.102482425347)) ;
#163041 = CARTESIAN_POINT('Ctrl Pts',(-16.5521229021323,-12.4735741717989,
117.12671339229)) ;
#163042 = CARTESIAN_POINT('Ctrl Pts',(-16.5383794781962,-12.5353914606374,
117.084853142342)) ;
#163043 = CARTESIAN_POINT('Ctrl Pts',(-16.6151024200091,-12.7368848040207,
117.282902758644)) ;
#163044 = CARTESIAN_POINT('Ctrl Pts',(-16.5967196831152,-12.7847255574639,
117.226911910079)) ;
#163045 = CARTESIAN_POINT('Ctrl Pts',(-16.6705235464973,-12.7847256367286,
117.202680929194)) ;
#163046 = CARTESIAN_POINT('Ctrl Pts',(-16.7443274098794,-12.7847257159933,
117.17844994831)) ;
#163047 = CARTESIAN_POINT('Ctrl Pts',(-16.7627101467733,-12.7368849625501,
117.234440796876)) ;
#163048 = CARTESIAN_POINT('Ctrl Pts',(-16.7810928836672,-12.6890442091069,
117.290431645442)) ;
#163049 = CARTESIAN_POINT('Ctrl Pts',(-16.7072890202851,-12.6890441298422,
117.314662626326)) ;
#163050 = CARTESIAN_POINT('Ctrl Pts',(-16.633485156903,-12.6890440505775,
117.33889360721)) ;
#163051 = CARTESIAN_POINT('Ctrl Pts',(-16.6151024200091,-12.7368848040207,
117.282902758644)) ;
#163052 = CARTESIAN_POINT('Ctrl Pts',(-16.6722339594684,-12.9849643669818,
117.421634700217)) ;
#163053 = CARTESIAN_POINT('Ctrl Pts',(-16.6505656858349,-13.0155548424745,
117.355636636913)) ;
#163054 = CARTESIAN_POINT('Ctrl Pts',(-16.7243695422743,-13.0155549383142,
117.331405634882)) ;
#163055 = CARTESIAN_POINT('Ctrl Pts',(-16.7981733987138,-13.0155550341539,
117.307174632852)) ;
#163056 = CARTESIAN_POINT('Ctrl Pts',(-16.8198416723473,-12.9849645586612,
117.373172696156)) ;
#163057 = CARTESIAN_POINT('Ctrl Pts',(-16.8415099459808,-12.9543740831685,
117.43917075946)) ;
#163058 = CARTESIAN_POINT('Ctrl Pts',(-16.7677060895413,-12.9543739873288,
117.46340176149)) ;
#163059 = CARTESIAN_POINT('Ctrl Pts',(-16.6939022331019,-12.9543738914891,
117.487632763521)) ;
#163060 = CARTESIAN_POINT('Ctrl Pts',(-16.6722339594684,-12.9849643669818,
117.421634700217)) ;
#163061 = CARTESIAN_POINT('Ctrl Pts',(-16.7074953741335,-13.2657001242146,
117.493501410732)) ;
#163062 = CARTESIAN_POINT('Ctrl Pts',(-16.6840686069065,-13.2767359206685,
117.422147259724)) ;
#163063 = CARTESIAN_POINT('Ctrl Pts',(-16.7578724550329,-13.2767360267194,
117.397916232373)) ;
#163064 = CARTESIAN_POINT('Ctrl Pts',(-16.8316763031593,-13.2767361327703,
117.373685205023)) ;
#163065 = CARTESIAN_POINT('Ctrl Pts',(-16.8551030703862,-13.2657003363164,
117.445039356031)) ;
#163066 = CARTESIAN_POINT('Ctrl Pts',(-16.8785298376132,-13.2546645398624,
117.516393507038)) ;
#163067 = CARTESIAN_POINT('Ctrl Pts',(-16.8047259894868,-13.2546644338116,
117.540624534389)) ;
#163068 = CARTESIAN_POINT('Ctrl Pts',(-16.7309221413604,-13.2546643277607,
117.56485556174)) ;
#163069 = CARTESIAN_POINT('Ctrl Pts',(-16.7074953741335,-13.2657001242146,
117.493501410732)) ;
#163070 = CARTESIAN_POINT('Ctrl Pts',(-16.7185435095042,-13.5562446654925,
117.491765214544)) ;
#163071 = CARTESIAN_POINT('Ctrl Pts',(-16.6950431078555,-13.5470119024509,
117.420186784989)) ;
#163072 = CARTESIAN_POINT('Ctrl Pts',(-16.7688469469812,-13.5470120097675,
117.395955730224)) ;
#163073 = CARTESIAN_POINT('Ctrl Pts',(-16.842650786107,-13.5470121170841,
117.371724675459)) ;
#163074 = CARTESIAN_POINT('Ctrl Pts',(-16.8661511877557,-13.5562448801257,
117.443303105014)) ;
#163075 = CARTESIAN_POINT('Ctrl Pts',(-16.8896515894044,-13.5654776431673,
117.514881534569)) ;
#163076 = CARTESIAN_POINT('Ctrl Pts',(-16.8158477502786,-13.5654775358507,
117.539112589334)) ;
#163077 = CARTESIAN_POINT('Ctrl Pts',(-16.7420439111529,-13.5654774285341,
117.5633436441)) ;
#163078 = CARTESIAN_POINT('Ctrl Pts',(-16.7185435095042,-13.5562446654925,
117.491765214544)) ;
#163079 = CARTESIAN_POINT('Ctrl Pts',(-16.7056071827156,-13.837740260252,
117.416879374421)) ;
#163080 = CARTESIAN_POINT('Ctrl Pts',(-16.6837093500279,-13.8088409661864,
117.350182111352)) ;
#163081 = CARTESIAN_POINT('Ctrl Pts',(-16.7575131803557,-13.8088410662031,
117.32595102979)) ;
#163082 = CARTESIAN_POINT('Ctrl Pts',(-16.8313170106835,-13.8088411662199,
117.301719948228)) ;
#163083 = CARTESIAN_POINT('Ctrl Pts',(-16.8532148433712,-13.8377404602855,
117.368417211296)) ;
#163084 = CARTESIAN_POINT('Ctrl Pts',(-16.8751126760589,-13.8666397543512,
117.435114474365)) ;
#163085 = CARTESIAN_POINT('Ctrl Pts',(-16.8013088457311,-13.8666396543344,
117.459345555927)) ;
#163086 = CARTESIAN_POINT('Ctrl Pts',(-16.7275050154033,-13.8666395543177,
117.483576637489)) ;
#163087 = CARTESIAN_POINT('Ctrl Pts',(-16.7056071827156,-13.837740260252,
117.416879374421)) ;
#163088 = CARTESIAN_POINT('Ctrl Pts',(-16.6698983566585,-14.0900089023239,
117.272469305418)) ;
#163089 = CARTESIAN_POINT('Ctrl Pts',(-16.6511984458618,-14.0434540249531,
117.215512396418)) ;
#163090 = CARTESIAN_POINT('Ctrl Pts',(-16.7250022686231,-14.0434541089459,
117.191281291809)) ;
#163091 = CARTESIAN_POINT('Ctrl Pts',(-16.7988060913844,-14.0434541929387,
117.167050187201)) ;
#163092 = CARTESIAN_POINT('Ctrl Pts',(-16.8175060021811,-14.0900090703095,
117.224007096201)) ;
#163093 = CARTESIAN_POINT('Ctrl Pts',(-16.8362059129778,-14.1365639476803,
117.280964005202)) ;
#163094 = CARTESIAN_POINT('Ctrl Pts',(-16.7624020902165,-14.1365638636875,
117.30519510981)) ;
#163095 = CARTESIAN_POINT('Ctrl Pts',(-16.6885982674552,-14.1365637796947,
117.329426214419)) ;
#163096 = CARTESIAN_POINT('Ctrl Pts',(-16.6698983566585,-14.0900089023239,
117.272469305418)) ;
#163097 = CARTESIAN_POINT('Ctrl Pts',(-16.615678314691,-14.2916996646196,
117.072102717414)) ;
#163098 = CARTESIAN_POINT('Ctrl Pts',(-16.6014650259406,-14.2309943169081,
117.028811335221)) ;
#163099 = CARTESIAN_POINT('Ctrl Pts',(-16.6752688429158,-14.230994379438,
117.004580212989)) ;
#163100 = CARTESIAN_POINT('Ctrl Pts',(-16.749072659891,-14.2309944419679,
116.980349090757)) ;
#163101 = CARTESIAN_POINT('Ctrl Pts',(-16.7632859486414,-14.2916997896794,
117.023640472949)) ;
#163102 = CARTESIAN_POINT('Ctrl Pts',(-16.7774992373917,-14.3524051373909,
117.066931855141)) ;
#163103 = CARTESIAN_POINT('Ctrl Pts',(-16.7036954204165,-14.352405074861,
117.091162977374)) ;
#163104 = CARTESIAN_POINT('Ctrl Pts',(-16.6298916034414,-14.352405012331,
117.115394099606)) ;
#163105 = CARTESIAN_POINT('Ctrl Pts',(-16.615678314691,-14.2916996646196,
117.072102717414)) ;
#163106 = CARTESIAN_POINT('Ctrl Pts',(-16.5462715072985,-14.4330905333239,
116.82503637481)) ;
#163107 = CARTESIAN_POINT('Ctrl Pts',(-16.5376205247406,-14.362422601594,
116.798686879729)) ;
#163108 = CARTESIAN_POINT('Ctrl Pts',(-16.6114243386022,-14.3624226376889,
116.774455748013)) ;
#163109 = CARTESIAN_POINT('Ctrl Pts',(-16.6852281524637,-14.3624226737838,
116.750224616297)) ;
#163110 = CARTESIAN_POINT('Ctrl Pts',(-16.6938791350216,-14.4330906055137,
116.776574111379)) ;
#163111 = CARTESIAN_POINT('Ctrl Pts',(-16.7025301175795,-14.5037585372437,
116.80292360646)) ;
#163112 = CARTESIAN_POINT('Ctrl Pts',(-16.628726303718,-14.5037585011487,
116.827154738176)) ;
#163113 = CARTESIAN_POINT('Ctrl Pts',(-16.5549224898564,-14.5037584650538,
116.851385869892)) ;
#163114 = CARTESIAN_POINT('Ctrl Pts',(-16.5462715072985,-14.4330905333239,
116.82503637481)) ;
#163115 = CARTESIAN_POINT('Ctrl Pts',(-16.4684461424741,-14.5004556458798,
116.552546390901)) ;
#163116 = CARTESIAN_POINT('Ctrl Pts',(-16.4659492440457,-14.424978464963,
116.544941243033)) ;
#163117 = CARTESIAN_POINT('Ctrl Pts',(-16.5397530573826,-14.4249784742085,
116.520710109719)) ;
#163118 = CARTESIAN_POINT('Ctrl Pts',(-16.6135568707195,-14.4249784834539,
116.496478976405)) ;
#163119 = CARTESIAN_POINT('Ctrl Pts',(-16.6160537691479,-14.5004556643706,
116.504084124273)) ;
#163120 = CARTESIAN_POINT('Ctrl Pts',(-16.6185506675763,-14.5759328452874,
116.51168927214)) ;
#163121 = CARTESIAN_POINT('Ctrl Pts',(-16.5447468542394,-14.5759328360419,
116.535920405454)) ;
#163122 = CARTESIAN_POINT('Ctrl Pts',(-16.4709430409025,-14.5759328267965,
116.560151538768)) ;
#163123 = CARTESIAN_POINT('Ctrl Pts',(-16.4684461424741,-14.5004556458798,
116.552546390901)) ;
#163124 = CARTESIAN_POINT('Ctrl Pts',(-16.3884429132822,-14.4906784452632,
116.273515768952)) ;
#163125 = CARTESIAN_POINT('Ctrl Pts',(-16.3922594977658,-14.4157707960699,
116.285140471267)) ;
#163126 = CARTESIAN_POINT('Ctrl Pts',(-16.4660633128443,-14.4157707802425,
116.260909343258)) ;
#163127 = CARTESIAN_POINT('Ctrl Pts',(-16.5398671279229,-14.4157707644151,
116.236678215249)) ;
#163128 = CARTESIAN_POINT('Ctrl Pts',(-16.5360505434393,-14.4906784136084,
116.225053512934)) ;
#163129 = CARTESIAN_POINT('Ctrl Pts',(-16.5322339589558,-14.5655860628017,
116.213428810619)) ;
#163130 = CARTESIAN_POINT('Ctrl Pts',(-16.4584301438772,-14.5655860786291,
116.237659938628)) ;
#163131 = CARTESIAN_POINT('Ctrl Pts',(-16.3846263287987,-14.5655860944565,
116.261891066637)) ;
#163132 = CARTESIAN_POINT('Ctrl Pts',(-16.3884429132822,-14.4906784452632,
116.273515768952)) ;
#163133 = CARTESIAN_POINT('Ctrl Pts',(-16.3122978006783,-14.4044504861589,
116.006169416252)) ;
#163134 = CARTESIAN_POINT('Ctrl Pts',(-16.3221693671015,-14.3354504116019,
116.036236616476)) ;
#163135 = CARTESIAN_POINT('Ctrl Pts',(-16.3959731861657,-14.3354503745246,
116.012005500606)) ;
#163136 = CARTESIAN_POINT('Ctrl Pts',(-16.4697770052299,-14.3354503374474,
115.987774384737)) ;
#163137 = CARTESIAN_POINT('Ctrl Pts',(-16.4599054388067,-14.4044504120043,
115.957707184513)) ;
#163138 = CARTESIAN_POINT('Ctrl Pts',(-16.4500338723836,-14.4734504865613,
115.92763998429)) ;
#163139 = CARTESIAN_POINT('Ctrl Pts',(-16.3762300533194,-14.4734505236385,
115.95187110016)) ;
#163140 = CARTESIAN_POINT('Ctrl Pts',(-16.3024262342552,-14.4734505607158,
115.976102216029)) ;
#163141 = CARTESIAN_POINT('Ctrl Pts',(-16.3122978006783,-14.4044504861589,
116.006169416252)) ;
#163142 = CARTESIAN_POINT('Ctrl Pts',(-16.2460229579914,-14.2464177648016,
115.768663223049)) ;
#163143 = CARTESIAN_POINT('Ctrl Pts',(-16.2612742676278,-14.1883465874269,
115.815116252918)) ;
#163144 = CARTESIAN_POINT('Ctrl Pts',(-16.3350780926779,-14.1883465362759,
115.790885155281)) ;
#163145 = CARTESIAN_POINT('Ctrl Pts',(-16.4088819177281,-14.1883464851249,
115.766654057644)) ;
#163146 = CARTESIAN_POINT('Ctrl Pts',(-16.3936306080916,-14.2464176624996,
115.720201027774)) ;
#163147 = CARTESIAN_POINT('Ctrl Pts',(-16.3783792984552,-14.3044888398743,
115.673747997904)) ;
#163148 = CARTESIAN_POINT('Ctrl Pts',(-16.304575473405,-14.3044888910253,
115.697979095542)) ;
#163149 = CARTESIAN_POINT('Ctrl Pts',(-16.2307716483549,-14.3044889421763,
115.722210193179)) ;
#163150 = CARTESIAN_POINT('Ctrl Pts',(-16.2460229579914,-14.2464177648016,
115.768663223049)) ;
#163151 = CARTESIAN_POINT('Ctrl Pts',(-16.1959322208732,-14.0296079395376,
115.58064014647)) ;
#163152 = CARTESIAN_POINT('Ctrl Pts',(-16.2154375855199,-13.9865865421538,
115.640050341363)) ;
#163153 = CARTESIAN_POINT('Ctrl Pts',(-16.2892414167736,-13.9865864836806,
115.615819262621)) ;
#163154 = CARTESIAN_POINT('Ctrl Pts',(-16.3630452480274,-13.9865864252074,
115.591588183879)) ;
#163155 = CARTESIAN_POINT('Ctrl Pts',(-16.3435398833807,-14.0296078225912,
115.532177988986)) ;
#163156 = CARTESIAN_POINT('Ctrl Pts',(-16.324034518734,-14.072629219975,115.472767794093)) ;
#163157 = CARTESIAN_POINT('Ctrl Pts',(-16.2502306874803,-14.0726292784482,
115.496998872835)) ;
#163158 = CARTESIAN_POINT('Ctrl Pts',(-16.1764268562265,-14.0726293369214,
115.521229951577)) ;
#163159 = CARTESIAN_POINT('Ctrl Pts',(-16.1959322208732,-14.0296079395376,
115.58064014647)) ;
#163160 = CARTESIAN_POINT('Ctrl Pts',(-16.1659524449804,-13.7700542634679,
115.453985376571)) ;
#163161 = CARTESIAN_POINT('Ctrl Pts',(-16.1883117544927,-13.7450900092007,
115.522088226907)) ;
#163162 = CARTESIAN_POINT('Ctrl Pts',(-16.2621155917233,-13.7450899491233,
115.497857166369)) ;
#163163 = CARTESIAN_POINT('Ctrl Pts',(-16.3359194289538,-13.7450898890458,
115.473626105831)) ;
#163164 = CARTESIAN_POINT('Ctrl Pts',(-16.3135601194414,-13.7700541433129,
115.405523255495)) ;
#163165 = CARTESIAN_POINT('Ctrl Pts',(-16.2912008099291,-13.79501839758,115.337420405159)) ;
#163166 = CARTESIAN_POINT('Ctrl Pts',(-16.2173969726985,-13.7950184576575,
115.361651465697)) ;
#163167 = CARTESIAN_POINT('Ctrl Pts',(-16.143593135468,-13.795018517735,115.385882526235)) ;
#163168 = CARTESIAN_POINT('Ctrl Pts',(-16.1659524449804,-13.7700542634679,
115.453985376571)) ;
#163169 = CARTESIAN_POINT('Ctrl Pts',(-16.1588094450499,-13.4844393542531,
115.396766680954)) ;
#163170 = CARTESIAN_POINT('Ctrl Pts',(-16.1824352013854,-13.4793790766449,
115.468726923808)) ;
#163171 = CARTESIAN_POINT('Ctrl Pts',(-16.2562390440075,-13.4793790219259,
115.444495879692)) ;
#163172 = CARTESIAN_POINT('Ctrl Pts',(-16.3300428866296,-13.479378967207,
115.420264835576)) ;
#163173 = CARTESIAN_POINT('Ctrl Pts',(-16.3064171302942,-13.4844392448151,
115.348304592722)) ;
#163174 = CARTESIAN_POINT('Ctrl Pts',(-16.2827913739587,-13.4894995224233,
115.276344349867)) ;
#163175 = CARTESIAN_POINT('Ctrl Pts',(-16.2089875313366,-13.4894995771423,
115.300575393983)) ;
#163176 = CARTESIAN_POINT('Ctrl Pts',(-16.1351836887144,-13.4894996318613,
115.324806438099)) ;
#163177 = CARTESIAN_POINT('Ctrl Pts',(-16.1588094450499,-13.4844393542531,
115.396766680954)) ;
#163178 = CARTESIAN_POINT('Ctrl Pts',(-16.1759899887603,-13.1938467066394,
115.413606223146)) ;
#163179 = CARTESIAN_POINT('Ctrl Pts',(-16.1991864289273,-13.2090684129076,
115.484258838048)) ;
#163180 = CARTESIAN_POINT('Ctrl Pts',(-16.27299027552,-13.2090683682137,115.460027806026)) ;
#163181 = CARTESIAN_POINT('Ctrl Pts',(-16.3467941221126,-13.2090683235198,
115.435796774003)) ;
#163182 = CARTESIAN_POINT('Ctrl Pts',(-16.3235976819456,-13.1938466172516,
115.365144159101)) ;
#163183 = CARTESIAN_POINT('Ctrl Pts',(-16.3004012417786,-13.1786249109835,
115.294491544198)) ;
#163184 = CARTESIAN_POINT('Ctrl Pts',(-16.226597395186,-13.1786249556774,
115.318722576221)) ;
#163185 = CARTESIAN_POINT('Ctrl Pts',(-16.1527935485933,-13.1786250003713,
115.342953608243)) ;
#163186 = CARTESIAN_POINT('Ctrl Pts',(-16.1759899887603,-13.1938467066394,
115.413606223146)) ;
#163187 = CARTESIAN_POINT('Ctrl Pts',(-16.2169131908586,-12.9193998282655,
115.502784611301)) ;
#163188 = CARTESIAN_POINT('Ctrl Pts',(-16.2380214175388,-12.9538071121124,
115.567076864686)) ;
#163189 = CARTESIAN_POINT('Ctrl Pts',(-16.3118252664966,-12.9538070795867,
115.542845839867)) ;
#163190 = CARTESIAN_POINT('Ctrl Pts',(-16.3856291154545,-12.9538070470611,
115.518614815049)) ;
#163191 = CARTESIAN_POINT('Ctrl Pts',(-16.3645208887744,-12.9193997632142,
115.454322561664)) ;
#163192 = CARTESIAN_POINT('Ctrl Pts',(-16.3434126620942,-12.8849924793673,
115.39003030828)) ;
#163193 = CARTESIAN_POINT('Ctrl Pts',(-16.2696088131364,-12.884992511893,
115.414261333098)) ;
#163194 = CARTESIAN_POINT('Ctrl Pts',(-16.1958049641785,-12.8849925444186,
115.438492357917)) ;
#163195 = CARTESIAN_POINT('Ctrl Pts',(-16.2169131908586,-12.9193998282655,
115.502784611301)) ;
#163196 = CARTESIAN_POINT('Ctrl Pts',(-16.2798288449759,-12.679977460876,
115.658797492625)) ;
#163197 = CARTESIAN_POINT('Ctrl Pts',(-16.2973132491563,-12.7311545599109,
115.712052167187)) ;
#163198 = CARTESIAN_POINT('Ctrl Pts',(-16.371117098481,-12.7311545403401,
115.687821143486)) ;
#163199 = CARTESIAN_POINT('Ctrl Pts',(-16.4449209478057,-12.7311545207693,
115.663590119785)) ;
#163200 = CARTESIAN_POINT('Ctrl Pts',(-16.4274365436253,-12.6799774217345,
115.610335445223)) ;
#163201 = CARTESIAN_POINT('Ctrl Pts',(-16.4099521394449,-12.6288003226997,
115.557080770662)) ;
#163202 = CARTESIAN_POINT('Ctrl Pts',(-16.3361482901202,-12.6288003422704,
115.581311794363)) ;
#163203 = CARTESIAN_POINT('Ctrl Pts',(-16.2623444407955,-12.6288003618412,
115.605542818064)) ;
#163204 = CARTESIAN_POINT('Ctrl Pts',(-16.2798288449759,-12.679977460876,
115.658797492625)) ;
#163205 = CARTESIAN_POINT('Ctrl Pts',(-16.3596321413727,-12.4956043021029,
115.866685267832)) ;
#163206 = CARTESIAN_POINT('Ctrl Pts',(-16.3722987255031,-12.5597317655866,
115.905265639768)) ;
#163207 = CARTESIAN_POINT('Ctrl Pts',(-16.4461025747697,-12.5597317545878,
115.88103461589)) ;
#163208 = CARTESIAN_POINT('Ctrl Pts',(-16.5199064240364,-12.5597317435889,
115.856803592012)) ;
#163209 = CARTESIAN_POINT('Ctrl Pts',(-16.507239839906,-12.4956042801052,
115.818223220076)) ;
#163210 = CARTESIAN_POINT('Ctrl Pts',(-16.4945732557756,-12.4314768166214,
115.77964284814)) ;
#163211 = CARTESIAN_POINT('Ctrl Pts',(-16.420769406509,-12.4314768276203,
115.803873872018)) ;
#163212 = CARTESIAN_POINT('Ctrl Pts',(-16.3469655572423,-12.4314768386191,
115.828104895896)) ;
#163213 = CARTESIAN_POINT('Ctrl Pts',(-16.3596321413727,-12.4956043021029,
115.866685267832)) ;
#163214 = CARTESIAN_POINT('Ctrl Pts',(-16.4533735886139,-12.3751190535725,
116.11656191809)) ;
#163215 = CARTESIAN_POINT('Ctrl Pts',(-16.4602515014048,-12.4477568900421,
116.137510930954)) ;
#163216 = CARTESIAN_POINT('Ctrl Pts',(-16.5340553487443,-12.4477568870231,
116.113279901206)) ;
#163217 = CARTESIAN_POINT('Ctrl Pts',(-16.6078591960839,-12.4477568840041,
116.089048871459)) ;
#163218 = CARTESIAN_POINT('Ctrl Pts',(-16.6009812832931,-12.3751190475345,
116.068099858596)) ;
#163219 = CARTESIAN_POINT('Ctrl Pts',(-16.5941033705022,-12.3024812110649,
116.047150845732)) ;
#163220 = CARTESIAN_POINT('Ctrl Pts',(-16.5202995231627,-12.3024812140839,
116.07138187548)) ;
#163221 = CARTESIAN_POINT('Ctrl Pts',(-16.4464956758231,-12.3024812171029,
116.095612905227)) ;
#163222 = CARTESIAN_POINT('Ctrl Pts',(-16.4533735886139,-12.3751190535725,
116.11656191809)) ;
#163223 = CARTESIAN_POINT('Ctrl Pts',(-16.5533514223054,-12.3303020351126,
116.385717677923)) ;
#163224 = CARTESIAN_POINT('Ctrl Pts',(-16.5539904411733,-12.4061784488461,
116.387664026431)) ;
#163225 = CARTESIAN_POINT('Ctrl Pts',(-16.627794286868,-12.4061784491626,
116.363432991674)) ;
#163226 = CARTESIAN_POINT('Ctrl Pts',(-16.7015981325627,-12.4061784494791,
116.339201956916)) ;
#163227 = CARTESIAN_POINT('Ctrl Pts',(-16.7009591136948,-12.3303020357456,
116.337255608408)) ;
#163228 = CARTESIAN_POINT('Ctrl Pts',(-16.7003200948268,-12.2544256220122,
116.335309259899)) ;
#163229 = CARTESIAN_POINT('Ctrl Pts',(-16.6265162491321,-12.2544256216956,
116.359540294657)) ;
#163230 = CARTESIAN_POINT('Ctrl Pts',(-16.5527124034374,-12.2544256213791,
116.383771329414)) ;
#163231 = CARTESIAN_POINT('Ctrl Pts',(-16.5533514223054,-12.3303020351126,
116.385717677923)) ;
#163232 = CARTESIAN_POINT('Ctrl Pts',(-16.6543061351395,-12.3631774170788,
116.657672551658)) ;
#163233 = CARTESIAN_POINT('Ctrl Pts',(-16.6486321491688,-12.4368724586972,
116.64039050592)) ;
#163234 = CARTESIAN_POINT('Ctrl Pts',(-16.7224359930919,-12.4368724595397,
116.616159465767)) ;
#163235 = CARTESIAN_POINT('Ctrl Pts',(-16.796239837015,-12.4368724603823,
116.591928425613)) ;
#163236 = CARTESIAN_POINT('Ctrl Pts',(-16.8019138229856,-12.363177418764,
116.609210471351)) ;
#163237 = CARTESIAN_POINT('Ctrl Pts',(-16.8075878089563,-12.2894823771457,
116.626492517088)) ;
#163238 = CARTESIAN_POINT('Ctrl Pts',(-16.7337839650332,-12.2894823763031,
116.650723557242)) ;
#163239 = CARTESIAN_POINT('Ctrl Pts',(-16.6599801211101,-12.2894823754605,
116.674954597395)) ;
#163240 = CARTESIAN_POINT('Ctrl Pts',(-16.6543061351395,-12.3631774170788,
116.657672551658)) ;
#163241 = CARTESIAN_POINT('Ctrl Pts',(-16.7488808914051,-12.4713342743348,
116.91035898593)) ;
#163242 = CARTESIAN_POINT('Ctrl Pts',(-16.7373265919045,-12.5375870378766,
116.875166453904)) ;
#163243 = CARTESIAN_POINT('Ctrl Pts',(-16.8111304348947,-12.5375870373685,
116.850935410909)) ;
#163244 = CARTESIAN_POINT('Ctrl Pts',(-16.884934277885,-12.5375870368604,
116.826704367914)) ;
#163245 = CARTESIAN_POINT('Ctrl Pts',(-16.8964885773856,-12.4713342733185,
116.861896899941)) ;
#163246 = CARTESIAN_POINT('Ctrl Pts',(-16.9080428768862,-12.4050815097766,
116.897089431967)) ;
#163247 = CARTESIAN_POINT('Ctrl Pts',(-16.8342390338959,-12.4050815102848,
116.921320474962)) ;
#163248 = CARTESIAN_POINT('Ctrl Pts',(-16.7604351909057,-12.4050815107929,
116.945551517957)) ;
#163249 = CARTESIAN_POINT('Ctrl Pts',(-16.7488808914051,-12.4713342743348,
116.91035898593)) ;
#163250 = CARTESIAN_POINT('Ctrl Pts',(-16.8318207118205,-12.6476404276989,
117.12747273466)) ;
#163251 = CARTESIAN_POINT('Ctrl Pts',(-16.8151924034807,-12.7016806543081,
117.07682559036)) ;
#163252 = CARTESIAN_POINT('Ctrl Pts',(-16.8889962461316,-12.7016806520052,
117.052594546332)) ;
#163253 = CARTESIAN_POINT('Ctrl Pts',(-16.9628000887825,-12.7016806497023,
117.028363502303)) ;
#163254 = CARTESIAN_POINT('Ctrl Pts',(-16.9794283971223,-12.6476404230932,
117.079010646603)) ;
#163255 = CARTESIAN_POINT('Ctrl Pts',(-16.9960567054621,-12.5936001964841,
117.129657790903)) ;
#163256 = CARTESIAN_POINT('Ctrl Pts',(-16.9222528628112,-12.5936001987869,
117.153888834932)) ;
#163257 = CARTESIAN_POINT('Ctrl Pts',(-16.8484490201604,-12.5936002010898,
117.17811987896)) ;
#163258 = CARTESIAN_POINT('Ctrl Pts',(-16.8318207118205,-12.6476404276989,
117.12747273466)) ;
#163259 = CARTESIAN_POINT('Ctrl Pts',(-16.8975001296176,-12.8790215196565,
117.292056197982)) ;
#163260 = CARTESIAN_POINT('Ctrl Pts',(-16.8769948136313,-12.9169844114343,
117.229600313953)) ;
#163261 = CARTESIAN_POINT('Ctrl Pts',(-16.9507986566424,-12.916984408831,
117.205369271022)) ;
#163262 = CARTESIAN_POINT('Ctrl Pts',(-17.0246024996535,-12.9169844062277,
117.18113822809)) ;
#163263 = CARTESIAN_POINT('Ctrl Pts',(-17.0451078156398,-12.87902151445,117.24359411212)) ;
#163264 = CARTESIAN_POINT('Ctrl Pts',(-17.0656131316261,-12.8410586226723,
117.306049996149)) ;
#163265 = CARTESIAN_POINT('Ctrl Pts',(-16.991809288615,-12.8410586252756,
117.330281039081)) ;
#163266 = CARTESIAN_POINT('Ctrl Pts',(-16.9180054456039,-12.8410586278788,
117.354512082012)) ;
#163267 = CARTESIAN_POINT('Ctrl Pts',(-16.8975001296176,-12.8790215196565,
117.292056197982)) ;
#163268 = CARTESIAN_POINT('Ctrl Pts',(-16.942134561038,-13.1499133657009,
117.392426703096)) ;
#163269 = CARTESIAN_POINT('Ctrl Pts',(-16.9192185652055,-13.1690162421117,
117.322628277277)) ;
#163270 = CARTESIAN_POINT('Ctrl Pts',(-16.9930224087252,-13.1690162422106,
117.298397235895)) ;
#163271 = CARTESIAN_POINT('Ctrl Pts',(-17.0668262522449,-13.1690162423095,
117.274166194512)) ;
#163272 = CARTESIAN_POINT('Ctrl Pts',(-17.0897422480774,-13.1499133658987,
117.343964620332)) ;
#163273 = CARTESIAN_POINT('Ctrl Pts',(-17.1126582439099,-13.1308104894879,
117.413763046152)) ;
#163274 = CARTESIAN_POINT('Ctrl Pts',(-17.0388544003902,-13.130810489389,
117.437994087534)) ;
#163275 = CARTESIAN_POINT('Ctrl Pts',(-16.9650505568705,-13.1308104892901,
117.462225128916)) ;
#163276 = CARTESIAN_POINT('Ctrl Pts',(-16.942134561038,-13.1499133657009,
117.392426703096)) ;
#163277 = CARTESIAN_POINT('Ctrl Pts',(-16.9630233535542,-13.4386144880716,
117.420658950536)) ;
#163278 = CARTESIAN_POINT('Ctrl Pts',(-16.9393477399357,-13.437586579743,
117.348546851583)) ;
#163279 = CARTESIAN_POINT('Ctrl Pts',(-17.0131515834676,-13.4375865840391,
117.324315810238)) ;
#163280 = CARTESIAN_POINT('Ctrl Pts',(-17.0869554269994,-13.4375865883353,
117.300084768893)) ;
#163281 = CARTESIAN_POINT('Ctrl Pts',(-17.1106310406178,-13.438614496664,
117.372196867845)) ;
#163282 = CARTESIAN_POINT('Ctrl Pts',(-17.1343066542363,-13.4396424049927,
117.444308966798)) ;
#163283 = CARTESIAN_POINT('Ctrl Pts',(-17.0605028107044,-13.4396424006965,
117.468540008143)) ;
#163284 = CARTESIAN_POINT('Ctrl Pts',(-16.9866989671726,-13.4396423964003,
117.492771049488)) ;
#163285 = CARTESIAN_POINT('Ctrl Pts',(-16.9630233535542,-13.4386144880716,
117.420658950536)) ;
#163286 = CARTESIAN_POINT('Ctrl Pts',(-16.9596443378371,-13.7268235527867,
117.37484372471)) ;
#163287 = CARTESIAN_POINT('Ctrl Pts',(-16.9369052317055,-13.7056699529127,
117.305584076576)) ;
#163288 = CARTESIAN_POINT('Ctrl Pts',(-17.0107090743469,-13.7056699630902,
117.281353032519)) ;
#163289 = CARTESIAN_POINT('Ctrl Pts',(-17.0845129169883,-13.7056699732676,
117.257121988462)) ;
#163290 = CARTESIAN_POINT('Ctrl Pts',(-17.10725202312,-13.7268235731417,117.326381636595)) ;
#163291 = CARTESIAN_POINT('Ctrl Pts',(-17.1299911292516,-13.7479771730157,
117.395641284728)) ;
#163292 = CARTESIAN_POINT('Ctrl Pts',(-17.0561872866102,-13.7479771628382,
117.419872328786)) ;
#163293 = CARTESIAN_POINT('Ctrl Pts',(-16.9823834439688,-13.7479771526607,
117.444103372843)) ;
#163294 = CARTESIAN_POINT('Ctrl Pts',(-16.9596443378371,-13.7268235527867,
117.37484372471)) ;
#163295 = CARTESIAN_POINT('Ctrl Pts',(-16.9330916364897,-13.9914324144424,
117.258649259076)) ;
#163296 = CARTESIAN_POINT('Ctrl Pts',(-16.912904485559,-13.9517725540924,
117.197162454839)) ;
#163297 = CARTESIAN_POINT('Ctrl Pts',(-16.9867083264563,-13.9517725681727,
117.17293140547)) ;
#163298 = CARTESIAN_POINT('Ctrl Pts',(-17.0605121673537,-13.9517725822531,
117.148700356101)) ;
#163299 = CARTESIAN_POINT('Ctrl Pts',(-17.0806993182844,-13.9914324426031,
117.210187160338)) ;
#163300 = CARTESIAN_POINT('Ctrl Pts',(-17.1008864692151,-14.0310923029532,
117.271673964574)) ;
#163301 = CARTESIAN_POINT('Ctrl Pts',(-17.0270826283177,-14.0310922888728,
117.295905013944)) ;
#163302 = CARTESIAN_POINT('Ctrl Pts',(-16.9532787874204,-14.0310922747924,
117.320136063313)) ;
#163303 = CARTESIAN_POINT('Ctrl Pts',(-16.9330916364897,-13.9914324144424,
117.258649259076)) ;
#163304 = CARTESIAN_POINT('Ctrl Pts',(-16.8858015410838,-14.2164140691066,
117.079108171634)) ;
#163305 = CARTESIAN_POINT('Ctrl Pts',(-16.8696216727807,-14.1609879110475,
117.029826903861)) ;
#163306 = CARTESIAN_POINT('Ctrl Pts',(-16.9434255108324,-14.1609879280051,
117.005595845824)) ;
#163307 = CARTESIAN_POINT('Ctrl Pts',(-17.0172293488841,-14.1609879449628,
116.981364787787)) ;
#163308 = CARTESIAN_POINT('Ctrl Pts',(-17.0334092171872,-14.2164141030218,
117.03064605556)) ;
#163309 = CARTESIAN_POINT('Ctrl Pts',(-17.0495890854903,-14.2718402610809,
117.079927323333)) ;
#163310 = CARTESIAN_POINT('Ctrl Pts',(-16.9757852474386,-14.2718402441232,
117.10415838137)) ;
#163311 = CARTESIAN_POINT('Ctrl Pts',(-16.9019814093869,-14.2718402271656,
117.128389439407)) ;
#163312 = CARTESIAN_POINT('Ctrl Pts',(-16.8858015410838,-14.2164140691066,
117.079108171634)) ;
#163313 = CARTESIAN_POINT('Ctrl Pts',(-16.8218713013157,-14.384032579335,
116.848865519025)) ;
#163314 = CARTESIAN_POINT('Ctrl Pts',(-16.8108667298453,-14.3168227397863,
116.815347370544)) ;
#163315 = CARTESIAN_POINT('Ctrl Pts',(-16.8846705642333,-14.3168227556033,
116.791116301349)) ;
#163316 = CARTESIAN_POINT('Ctrl Pts',(-16.9584743986213,-14.3168227714204,
116.766885232153)) ;
#163317 = CARTESIAN_POINT('Ctrl Pts',(-16.9694789700917,-14.3840326109691,
116.800403380634)) ;
#163318 = CARTESIAN_POINT('Ctrl Pts',(-16.9804835415621,-14.4512424505178,
116.833921529114)) ;
#163319 = CARTESIAN_POINT('Ctrl Pts',(-16.906679707174,-14.4512424347008,
116.85815259831)) ;
#163320 = CARTESIAN_POINT('Ctrl Pts',(-16.832875872786,-14.4512424188837,
116.882383667506)) ;
#163321 = CARTESIAN_POINT('Ctrl Pts',(-16.8218713013157,-14.384032579335,
116.848865519025)) ;
#163322 = CARTESIAN_POINT('Ctrl Pts',(-16.7469781937031,-14.4820529544929,
116.585338242812)) ;
#163323 = CARTESIAN_POINT('Ctrl Pts',(-16.7419196115825,-14.40790231883,116.569930618666)) ;
#163324 = CARTESIAN_POINT('Ctrl Pts',(-16.8157234425129,-14.4079023280758,
116.545699538938)) ;
#163325 = CARTESIAN_POINT('Ctrl Pts',(-16.8895272734432,-14.4079023373216,
116.521468459211)) ;
#163326 = CARTESIAN_POINT('Ctrl Pts',(-16.8945858555639,-14.4820529729845,
116.536876083358)) ;
#163327 = CARTESIAN_POINT('Ctrl Pts',(-16.8996444376845,-14.5562036086474,
116.552283707504)) ;
#163328 = CARTESIAN_POINT('Ctrl Pts',(-16.8258406067541,-14.5562035994016,
116.576514787232)) ;
#163329 = CARTESIAN_POINT('Ctrl Pts',(-16.7520367758238,-14.5562035901558,
116.600745866959)) ;
#163330 = CARTESIAN_POINT('Ctrl Pts',(-16.7469781937031,-14.4820529544929,
116.585338242812)) ;
#163331 = CARTESIAN_POINT('Ctrl Pts',(-16.6668754248099,-14.5042250600488,
116.305877110692)) ;
#163332 = CARTESIAN_POINT('Ctrl Pts',(-16.668136431742,-14.4284191898376,
116.309717935311)) ;
#163333 = CARTESIAN_POINT('Ctrl Pts',(-16.7419402595713,-14.4284191877868,
116.285486846138)) ;
#163334 = CARTESIAN_POINT('Ctrl Pts',(-16.8157440874006,-14.428419185736,
116.261255756966)) ;
#163335 = CARTESIAN_POINT('Ctrl Pts',(-16.8144830804684,-14.5042250559472,
116.257414932347)) ;
#163336 = CARTESIAN_POINT('Ctrl Pts',(-16.8132220735362,-14.5800309261584,
116.253574107729)) ;
#163337 = CARTESIAN_POINT('Ctrl Pts',(-16.739418245707,-14.5800309282092,
116.277805196901)) ;
#163338 = CARTESIAN_POINT('Ctrl Pts',(-16.6656144178777,-14.58003093026,116.302036286074)) ;
#163339 = CARTESIAN_POINT('Ctrl Pts',(-16.6668754248099,-14.5042250600488,
116.305877110692)) ;
#163340 = CARTESIAN_POINT('Ctrl Pts',(-16.5879598850496,-14.4479097103847,
116.029910236852)) ;
#163341 = CARTESIAN_POINT('Ctrl Pts',(-16.5954692147568,-14.3759257111989,
116.052782444672)) ;
#163342 = CARTESIAN_POINT('Ctrl Pts',(-16.6692730404099,-14.3759256925376,
116.028551348871)) ;
#163343 = CARTESIAN_POINT('Ctrl Pts',(-16.743076866063,-14.3759256738764,
116.00432025307)) ;
#163344 = CARTESIAN_POINT('Ctrl Pts',(-16.7355675363558,-14.4479096730622,
115.98144804525)) ;
#163345 = CARTESIAN_POINT('Ctrl Pts',(-16.7280582066486,-14.519893672248,
115.95857583743)) ;
#163346 = CARTESIAN_POINT('Ctrl Pts',(-16.6542543809955,-14.5198936909092,
115.982806933231)) ;
#163347 = CARTESIAN_POINT('Ctrl Pts',(-16.5804505553424,-14.5198937095705,
116.007038029031)) ;
#163348 = CARTESIAN_POINT('Ctrl Pts',(-16.5879598850496,-14.4479097103847,
116.029910236852)) ;
#163349 = CARTESIAN_POINT('Ctrl Pts',(-16.5174994343308,-14.3189148106109,
115.780020371028)) ;
#163350 = CARTESIAN_POINT('Ctrl Pts',(-16.5306689565097,-14.2558334084202,
115.820132611976)) ;
#163351 = CARTESIAN_POINT('Ctrl Pts',(-16.6044727826075,-14.2558333716659,
115.79590151753)) ;
#163352 = CARTESIAN_POINT('Ctrl Pts',(-16.6782766087053,-14.2558333349115,
115.771670423084)) ;
#163353 = CARTESIAN_POINT('Ctrl Pts',(-16.6651070865265,-14.3189147371022,
115.731558182136)) ;
#163354 = CARTESIAN_POINT('Ctrl Pts',(-16.6519375643476,-14.3819961392929,
115.691445941188)) ;
#163355 = CARTESIAN_POINT('Ctrl Pts',(-16.5781337382498,-14.3819961760472,
115.715677035634)) ;
#163356 = CARTESIAN_POINT('Ctrl Pts',(-16.504329912152,-14.3819962128016,
115.73990813008)) ;
#163357 = CARTESIAN_POINT('Ctrl Pts',(-16.5174994343308,-14.3189148106109,
115.780020371028)) ;
#163358 = CARTESIAN_POINT('Ctrl Pts',(-16.4601033314479,-14.1239822238445,
115.569589941592)) ;
#163359 = CARTESIAN_POINT('Ctrl Pts',(-16.4780361084618,-14.0744187665949,
115.624210288398)) ;
#163360 = CARTESIAN_POINT('Ctrl Pts',(-16.5518399363937,-14.074418709394,
115.599979199538)) ;
#163361 = CARTESIAN_POINT('Ctrl Pts',(-16.6256437643256,-14.0744186521931,
115.575748110678)) ;
#163362 = CARTESIAN_POINT('Ctrl Pts',(-16.6077109873116,-14.1239821094427,
115.521127763872)) ;
#163363 = CARTESIAN_POINT('Ctrl Pts',(-16.5897782102976,-14.1735455666924,
115.466507417066)) ;
#163364 = CARTESIAN_POINT('Ctrl Pts',(-16.5159743823658,-14.1735456238933,
115.490738505926)) ;
#163365 = CARTESIAN_POINT('Ctrl Pts',(-16.4421705544339,-14.1735456810942,
115.514969594786)) ;
#163366 = CARTESIAN_POINT('Ctrl Pts',(-16.4601033314479,-14.1239822238445,
115.569589941592)) ;
#163367 = CARTESIAN_POINT('Ctrl Pts',(-16.4215747130303,-13.8804446676162,
115.416952493218)) ;
#163368 = CARTESIAN_POINT('Ctrl Pts',(-16.4429534477659,-13.8478127953866,
115.482068671354)) ;
#163369 = CARTESIAN_POINT('Ctrl Pts',(-16.5167572801787,-13.8478127217154,
115.457837596143)) ;
#163370 = CARTESIAN_POINT('Ctrl Pts',(-16.5905611125915,-13.8478126480443,
115.433606520931)) ;
#163371 = CARTESIAN_POINT('Ctrl Pts',(-16.5691823778558,-13.8804445202739,
115.368490342794)) ;
#163372 = CARTESIAN_POINT('Ctrl Pts',(-16.5478036431202,-13.9130763925035,
115.303374164658)) ;
#163373 = CARTESIAN_POINT('Ctrl Pts',(-16.4739998107074,-13.9130764661746,
115.32760523987)) ;
#163374 = CARTESIAN_POINT('Ctrl Pts',(-16.4001959782946,-13.9130765398458,
115.351836315081)) ;
#163375 = CARTESIAN_POINT('Ctrl Pts',(-16.4215747130303,-13.8804446676162,
115.416952493218)) ;
#163376 = CARTESIAN_POINT('Ctrl Pts',(-16.4047818629355,-13.6007259227713,
115.330092652858)) ;
#163377 = CARTESIAN_POINT('Ctrl Pts',(-16.4281032255851,-13.5875751539527,
115.401125762342)) ;
#163378 = CARTESIAN_POINT('Ctrl Pts',(-16.5019070640968,-13.5875750652436,
115.376894705707)) ;
#163379 = CARTESIAN_POINT('Ctrl Pts',(-16.5757109026085,-13.5875749765345,
115.352663649072)) ;
#163380 = CARTESIAN_POINT('Ctrl Pts',(-16.5523895399589,-13.6007257453531,
115.281630539587)) ;
#163381 = CARTESIAN_POINT('Ctrl Pts',(-16.5290681773093,-13.6138765141717,
115.210597430103)) ;
#163382 = CARTESIAN_POINT('Ctrl Pts',(-16.4552643387976,-13.6138766028808,
115.234828486739)) ;
#163383 = CARTESIAN_POINT('Ctrl Pts',(-16.3814605002859,-13.6138766915899,
115.259059543374)) ;
#163384 = CARTESIAN_POINT('Ctrl Pts',(-16.4047818629355,-13.6007259227713,
115.330092652858)) ;
#163385 = CARTESIAN_POINT('Ctrl Pts',(-16.4121369550956,-13.310886389785,
115.317177989403)) ;
#163386 = CARTESIAN_POINT('Ctrl Pts',(-16.4357094306014,-13.3179522424612,
115.38897594822)) ;
#163387 = CARTESIAN_POINT('Ctrl Pts',(-16.5095132768189,-13.3179521481175,
115.364744915055)) ;
#163388 = CARTESIAN_POINT('Ctrl Pts',(-16.5833171230364,-13.3179520537738,
115.34051388189)) ;
#163389 = CARTESIAN_POINT('Ctrl Pts',(-16.5597446475305,-13.3108862010977,
115.268715923073)) ;
#163390 = CARTESIAN_POINT('Ctrl Pts',(-16.5361721720247,-13.3038203484215,
115.196917964256)) ;
#163391 = CARTESIAN_POINT('Ctrl Pts',(-16.4623683258072,-13.3038204427652,
115.221148997421)) ;
#163392 = CARTESIAN_POINT('Ctrl Pts',(-16.3885644795897,-13.3038205371088,
115.245380030586)) ;
#163393 = CARTESIAN_POINT('Ctrl Pts',(-16.4121369550956,-13.310886389785,
115.317177989403)) ;
#163394 = CARTESIAN_POINT('Ctrl Pts',(-16.4435486385353,-13.0275729196668,
115.377389997303)) ;
#163395 = CARTESIAN_POINT('Ctrl Pts',(-16.4656962766156,-13.0544289037497,
115.444848131314)) ;
#163396 = CARTESIAN_POINT('Ctrl Pts',(-16.539500131069,-13.0544288105617,
115.420617123234)) ;
#163397 = CARTESIAN_POINT('Ctrl Pts',(-16.6133039855224,-13.0544287173738,
115.396386115154)) ;
#163398 = CARTESIAN_POINT('Ctrl Pts',(-16.5911563474421,-13.0275727332909,
115.328927981143)) ;
#163399 = CARTESIAN_POINT('Ctrl Pts',(-16.5690087093617,-13.000716749208,
115.261469847132)) ;
#163400 = CARTESIAN_POINT('Ctrl Pts',(-16.4952048549083,-13.000716842396,
115.285700855212)) ;
#163401 = CARTESIAN_POINT('Ctrl Pts',(-16.4214010004549,-13.000716935584,
115.309931863291)) ;
#163402 = CARTESIAN_POINT('Ctrl Pts',(-16.4435486385353,-13.0275729196668,
115.377389997303)) ;
#163403 = CARTESIAN_POINT('Ctrl Pts',(-16.4978834158618,-12.7715214711428,
115.507323795441)) ;
#163404 = CARTESIAN_POINT('Ctrl Pts',(-16.5170059842238,-12.8162933310401,
115.565568055265)) ;
#163405 = CARTESIAN_POINT('Ctrl Pts',(-16.5908098468287,-12.8162932472945,
115.541337072013)) ;
#163406 = CARTESIAN_POINT('Ctrl Pts',(-16.6646137094336,-12.8162931635489,
115.517106088762)) ;
#163407 = CARTESIAN_POINT('Ctrl Pts',(-16.6454911410716,-12.7715213036516,
115.458861828938)) ;
#163408 = CARTESIAN_POINT('Ctrl Pts',(-16.6263685727096,-12.7267494437543,
115.400617569114)) ;
#163409 = CARTESIAN_POINT('Ctrl Pts',(-16.5525647101047,-12.7267495274999,
115.424848552366)) ;
#163410 = CARTESIAN_POINT('Ctrl Pts',(-16.4787608474998,-12.7267496112455,
115.449079535617)) ;
#163411 = CARTESIAN_POINT('Ctrl Pts',(-16.4978834158618,-12.7715214711428,
115.507323795441)) ;
#163412 = CARTESIAN_POINT('Ctrl Pts',(-16.5717603357923,-12.5625540682405,
115.696844987537)) ;
#163413 = CARTESIAN_POINT('Ctrl Pts',(-16.5864877055185,-12.6219811291845,
115.74170218153)) ;
#163414 = CARTESIAN_POINT('Ctrl Pts',(-16.6602915750344,-12.6219810632867,
115.717471219328)) ;
#163415 = CARTESIAN_POINT('Ctrl Pts',(-16.7340954445502,-12.6219809973889,
115.693240257126)) ;
#163416 = CARTESIAN_POINT('Ctrl Pts',(-16.7193680748241,-12.5625539364449,
115.648383063133)) ;
#163417 = CARTESIAN_POINT('Ctrl Pts',(-16.7046407050979,-12.5031268755009,
115.603525869141)) ;
#163418 = CARTESIAN_POINT('Ctrl Pts',(-16.630836835582,-12.5031269413987,
115.627756831343)) ;
#163419 = CARTESIAN_POINT('Ctrl Pts',(-16.5570329660662,-12.5031270072965,
115.651987793545)) ;
#163420 = CARTESIAN_POINT('Ctrl Pts',(-16.5717603357923,-12.5625540682405,
115.696844987537)) ;
#163421 = CARTESIAN_POINT('Ctrl Pts',(-16.6600063471763,-12.4155360311479,
115.930369190556)) ;
#163422 = CARTESIAN_POINT('Ctrl Pts',(-16.6693238142624,-12.4853145096468,
115.958748694017)) ;
#163423 = CARTESIAN_POINT('Ctrl Pts',(-16.7431276886547,-12.4853144677288,
115.934517746667)) ;
#163424 = CARTESIAN_POINT('Ctrl Pts',(-16.8169315630469,-12.4853144258108,
115.910286799318)) ;
#163425 = CARTESIAN_POINT('Ctrl Pts',(-16.8076140959607,-12.4155359473118,
115.881907295858)) ;
#163426 = CARTESIAN_POINT('Ctrl Pts',(-16.7982966288746,-12.3457574688128,
115.853527792397)) ;
#163427 = CARTESIAN_POINT('Ctrl Pts',(-16.7244927544824,-12.3457575107309,
115.877758739747)) ;
#163428 = CARTESIAN_POINT('Ctrl Pts',(-16.6506888800901,-12.3457575526489,
115.901989687096)) ;
#163429 = CARTESIAN_POINT('Ctrl Pts',(-16.6600063471763,-12.4155360311479,
115.930369190556)) ;
#163430 = CARTESIAN_POINT('Ctrl Pts',(-16.7583961657612,-12.339199302571,
116.194502768036)) ;
#163431 = CARTESIAN_POINT('Ctrl Pts',(-16.7615937653379,-12.4144106897109,
116.204242142512)) ;
#163432 = CARTESIAN_POINT('Ctrl Pts',(-16.835397642295,-12.41441067568,116.180011202975)) ;
#163433 = CARTESIAN_POINT('Ctrl Pts',(-16.909201519252,-12.4144106616491,
116.155780263438)) ;
#163434 = CARTESIAN_POINT('Ctrl Pts',(-16.9060039196752,-12.3391992745091,
116.146040888962)) ;
#163435 = CARTESIAN_POINT('Ctrl Pts',(-16.9028063200983,-12.2639878873692,
116.136301514485)) ;
#163436 = CARTESIAN_POINT('Ctrl Pts',(-16.8290024431413,-12.2639879014001,
116.160532454023)) ;
#163437 = CARTESIAN_POINT('Ctrl Pts',(-16.7551985661843,-12.2639879154311,
116.18476339356)) ;
#163438 = CARTESIAN_POINT('Ctrl Pts',(-16.7583961657612,-12.339199302571,
116.194502768036)) ;
#163439 = CARTESIAN_POINT('Ctrl Pts',(-16.8595422687567,-12.3403409953756,
116.467185667784)) ;
#163440 = CARTESIAN_POINT('Ctrl Pts',(-16.8564152393437,-12.4155840268561,
116.457661242822)) ;
#163441 = CARTESIAN_POINT('Ctrl Pts',(-16.9302191160928,-12.4155840418634,
116.433430302651)) ;
#163442 = CARTESIAN_POINT('Ctrl Pts',(-17.0040229928419,-12.4155840568707,
116.409199362481)) ;
#163443 = CARTESIAN_POINT('Ctrl Pts',(-17.0071500222549,-12.3403410253901,
116.418723787443)) ;
#163444 = CARTESIAN_POINT('Ctrl Pts',(-17.0102770516679,-12.2650979939095,
116.428248212404)) ;
#163445 = CARTESIAN_POINT('Ctrl Pts',(-16.9364731749188,-12.2650979789023,
116.452479152575)) ;
#163446 = CARTESIAN_POINT('Ctrl Pts',(-16.8626692981697,-12.265097963895,
116.476710092745)) ;
#163447 = CARTESIAN_POINT('Ctrl Pts',(-16.8595422687567,-12.3403409953756,
116.467185667784)) ;
#163448 = CARTESIAN_POINT('Ctrl Pts',(-16.9578689738167,-12.4190382667156,
116.731080805892)) ;
#163449 = CARTESIAN_POINT('Ctrl Pts',(-16.9486089308596,-12.488899337021,
116.702876211193)) ;
#163450 = CARTESIAN_POINT('Ctrl Pts',(-17.0224128045713,-12.488899379198,
116.678645261771)) ;
#163451 = CARTESIAN_POINT('Ctrl Pts',(-17.096216678283,-12.488899421375,116.654414312349)) ;
#163452 = CARTESIAN_POINT('Ctrl Pts',(-17.1054767212401,-12.4190383510696,
116.682618907047)) ;
#163453 = CARTESIAN_POINT('Ctrl Pts',(-17.1147367641971,-12.3491772807642,
116.710823501746)) ;
#163454 = CARTESIAN_POINT('Ctrl Pts',(-17.0409328904855,-12.3491772385872,
116.735054451168)) ;
#163455 = CARTESIAN_POINT('Ctrl Pts',(-16.9671290167738,-12.3491771964102,
116.75928540059)) ;
#163456 = CARTESIAN_POINT('Ctrl Pts',(-16.9578689738167,-12.4190382667156,
116.731080805892)) ;
#163457 = CARTESIAN_POINT('Ctrl Pts',(-17.0458999041783,-12.5685297170459,
116.963876177155)) ;
#163458 = CARTESIAN_POINT('Ctrl Pts',(-17.0312110845687,-12.6280576016783,
116.919136404655)) ;
#163459 = CARTESIAN_POINT('Ctrl Pts',(-17.105014953103,-12.6280576665216,
116.894905439464)) ;
#163460 = CARTESIAN_POINT('Ctrl Pts',(-17.1788188216374,-12.6280577313649,
116.870674474273)) ;
#163461 = CARTESIAN_POINT('Ctrl Pts',(-17.1935076412471,-12.5685298467324,
116.915414246773)) ;
#163462 = CARTESIAN_POINT('Ctrl Pts',(-17.2081964608567,-12.5090019621,116.960154019273)) ;
#163463 = CARTESIAN_POINT('Ctrl Pts',(-17.1343925923223,-12.5090018972567,
116.984384984464)) ;
#163464 = CARTESIAN_POINT('Ctrl Pts',(-17.0605887237879,-12.5090018324134,
117.008615949655)) ;
#163465 = CARTESIAN_POINT('Ctrl Pts',(-17.0458999041783,-12.5685297170459,
116.963876177155)) ;
#163466 = CARTESIAN_POINT('Ctrl Pts',(-17.1191748552296,-12.7793086778933,
117.151568386626)) ;
#163467 = CARTESIAN_POINT('Ctrl Pts',(-17.1000825757091,-12.8242097756673,
117.093416385657)) ;
#163468 = CARTESIAN_POINT('Ctrl Pts',(-17.1738864372224,-12.8242098564781,
117.069185399081)) ;
#163469 = CARTESIAN_POINT('Ctrl Pts',(-17.2476902987357,-12.8242099372889,
117.044954412505)) ;
#163470 = CARTESIAN_POINT('Ctrl Pts',(-17.2667825782563,-12.7793088395149,
117.103106413474)) ;
#163471 = CARTESIAN_POINT('Ctrl Pts',(-17.2858748577768,-12.7344077417409,
117.161258414442)) ;
#163472 = CARTESIAN_POINT('Ctrl Pts',(-17.2120709962635,-12.7344076609301,
117.185489401019)) ;
#163473 = CARTESIAN_POINT('Ctrl Pts',(-17.1382671347501,-12.7344075801193,
117.209720387595)) ;
#163474 = CARTESIAN_POINT('Ctrl Pts',(-17.1191748552296,-12.7793086778933,
117.151568386626)) ;
#163475 = CARTESIAN_POINT('Ctrl Pts',(-17.1727252854914,-13.0361487300971,
117.279168850677)) ;
#163476 = CARTESIAN_POINT('Ctrl Pts',(-17.1506002151848,-13.0631853690337,
117.211779458213)) ;
#163477 = CARTESIAN_POINT('Ctrl Pts',(-17.2244040687652,-13.0631854575266,
117.187548447474)) ;
#163478 = CARTESIAN_POINT('Ctrl Pts',(-17.2982079223455,-13.0631855460195,
117.163317436735)) ;
#163479 = CARTESIAN_POINT('Ctrl Pts',(-17.320332992652,-13.0361489070829,
117.230706829199)) ;
#163480 = CARTESIAN_POINT('Ctrl Pts',(-17.3424580629586,-13.0091122681464,
117.298096221663)) ;
#163481 = CARTESIAN_POINT('Ctrl Pts',(-17.2686542093782,-13.0091121796535,
117.322327232402)) ;
#163482 = CARTESIAN_POINT('Ctrl Pts',(-17.1948503557979,-13.0091120911606,
117.346558243141)) ;
#163483 = CARTESIAN_POINT('Ctrl Pts',(-17.1727252854914,-13.0361487300971,
117.279168850677)) ;
#163484 = CARTESIAN_POINT('Ctrl Pts',(-17.2034288318534,-13.3199156358865,
117.337236471295)) ;
#163485 = CARTESIAN_POINT('Ctrl Pts',(-17.1798603419687,-13.3271808481679,
117.265450655579)) ;
#163486 = CARTESIAN_POINT('Ctrl Pts',(-17.2536641876918,-13.3271809363831,
117.241219620908)) ;
#163487 = CARTESIAN_POINT('Ctrl Pts',(-17.3274680334149,-13.3271810245983,
117.216988586238)) ;
#163488 = CARTESIAN_POINT('Ctrl Pts',(-17.3510365232996,-13.3199158123169,
117.288774401953)) ;
#163489 = CARTESIAN_POINT('Ctrl Pts',(-17.3746050131842,-13.3126506000355,
117.360560217669)) ;
#163490 = CARTESIAN_POINT('Ctrl Pts',(-17.3008011674611,-13.3126505118203,
117.38479125234)) ;
#163491 = CARTESIAN_POINT('Ctrl Pts',(-17.226997321738,-13.312650423605,117.409022287011)) ;
#163492 = CARTESIAN_POINT('Ctrl Pts',(-17.2034288318534,-13.3199156358865,
117.337236471295)) ;
#163493 = CARTESIAN_POINT('Ctrl Pts',(-17.2099599842142,-13.61053350134,117.321699031089)) ;
#163494 = CARTESIAN_POINT('Ctrl Pts',(-17.1866331051387,-13.5975190949255,
117.250649122791)) ;
#163495 = CARTESIAN_POINT('Ctrl Pts',(-17.2604369438178,-13.5975191756466,
117.226418066665)) ;
#163496 = CARTESIAN_POINT('Ctrl Pts',(-17.334240782497,-13.5975192563676,
117.20218701054)) ;
#163497 = CARTESIAN_POINT('Ctrl Pts',(-17.3575676615725,-13.6105336627821,
117.273236918838)) ;
#163498 = CARTESIAN_POINT('Ctrl Pts',(-17.3808945406481,-13.6235480691965,
117.344286827137)) ;
#163499 = CARTESIAN_POINT('Ctrl Pts',(-17.3070907019689,-13.6235479884755,
117.368517883263)) ;
#163500 = CARTESIAN_POINT('Ctrl Pts',(-17.2332868632897,-13.6235479077544,
117.392748939388)) ;
#163501 = CARTESIAN_POINT('Ctrl Pts',(-17.2099599842142,-13.61053350134,117.321699031089)) ;
#163502 = CARTESIAN_POINT('Ctrl Pts',(-17.1925797786754,-13.8877845324202,
117.233281417969)) ;
#163503 = CARTESIAN_POINT('Ctrl Pts',(-17.1711652640745,-13.8553930149523,
117.168056263156)) ;
#163504 = CARTESIAN_POINT('Ctrl Pts',(-17.24496909722,-13.8553930819553,117.143825190176)) ;
#163505 = CARTESIAN_POINT('Ctrl Pts',(-17.3187729303654,-13.8553931489583,
117.119594117196)) ;
#163506 = CARTESIAN_POINT('Ctrl Pts',(-17.3401874449663,-13.8877846664262,
117.184819272008)) ;
#163507 = CARTESIAN_POINT('Ctrl Pts',(-17.3616019595672,-13.9201761838941,
117.250044426821)) ;
#163508 = CARTESIAN_POINT('Ctrl Pts',(-17.2877981264218,-13.9201761168911,
117.274275499801)) ;
#163509 = CARTESIAN_POINT('Ctrl Pts',(-17.2139942932763,-13.9201760498881,
117.298506572782)) ;
#163510 = CARTESIAN_POINT('Ctrl Pts',(-17.1925797786754,-13.8877845324202,
117.233281417969)) ;
#163511 = CARTESIAN_POINT('Ctrl Pts',(-17.1531888988296,-14.1315208949384,
117.077791857519)) ;
#163512 = CARTESIAN_POINT('Ctrl Pts',(-17.135227002644,-14.0820626171462,
117.023082821159)) ;
#163513 = CARTESIAN_POINT('Ctrl Pts',(-17.2090308323232,-14.0820626666498,
116.998851737621)) ;
#163514 = CARTESIAN_POINT('Ctrl Pts',(-17.2828346620024,-14.0820627161535,
116.974620654083)) ;
#163515 = CARTESIAN_POINT('Ctrl Pts',(-17.300796558188,-14.1315209939457,
117.029329690443)) ;
#163516 = CARTESIAN_POINT('Ctrl Pts',(-17.3187584543736,-14.1809792717379,
117.084038726803)) ;
#163517 = CARTESIAN_POINT('Ctrl Pts',(-17.2449546246944,-14.1809792222342,
117.108269810341)) ;
#163518 = CARTESIAN_POINT('Ctrl Pts',(-17.1711507950152,-14.1809791727306,
117.132500893879)) ;
#163519 = CARTESIAN_POINT('Ctrl Pts',(-17.1531888988296,-14.1315208949384,
117.077791857519)) ;
#163520 = CARTESIAN_POINT('Ctrl Pts',(-17.0955345319982,-14.3236676354294,
116.866747533545)) ;
#163521 = CARTESIAN_POINT('Ctrl Pts',(-17.0823042094018,-14.2607186290668,
116.826450106743)) ;
#163522 = CARTESIAN_POINT('Ctrl Pts',(-17.1561080375986,-14.260718660624,
116.80221901869)) ;
#163523 = CARTESIAN_POINT('Ctrl Pts',(-17.2299118657954,-14.2607186921811,
116.777987930637)) ;
#163524 = CARTESIAN_POINT('Ctrl Pts',(-17.2431421883918,-14.3236676985437,
116.818285357438)) ;
#163525 = CARTESIAN_POINT('Ctrl Pts',(-17.2563725109882,-14.3866167049062,
116.85858278424)) ;
#163526 = CARTESIAN_POINT('Ctrl Pts',(-17.1825686827914,-14.3866166733491,
116.882813872293)) ;
#163527 = CARTESIAN_POINT('Ctrl Pts',(-17.1087648545946,-14.3866166417919,
116.907044960346)) ;
#163528 = CARTESIAN_POINT('Ctrl Pts',(-17.0955345319982,-14.3236676354294,
116.866747533545)) ;
#163529 = CARTESIAN_POINT('Ctrl Pts',(-17.0243702739968,-14.451213086268,
116.614520189238)) ;
#163530 = CARTESIAN_POINT('Ctrl Pts',(-17.016822677996,-14.3792631912131,
116.591531430573)) ;
#163531 = CARTESIAN_POINT('Ctrl Pts',(-17.0906265067015,-14.3792632058746,
116.567300344069)) ;
#163532 = CARTESIAN_POINT('Ctrl Pts',(-17.164430335407,-14.3792632205361,
116.543069257566)) ;
#163533 = CARTESIAN_POINT('Ctrl Pts',(-17.1719779314079,-14.451213115591,
116.56605801623)) ;
#163534 = CARTESIAN_POINT('Ctrl Pts',(-17.1795255274087,-14.5231630106458,
116.589046774895)) ;
#163535 = CARTESIAN_POINT('Ctrl Pts',(-17.1057216987032,-14.5231629959843,
116.613277861399)) ;
#163536 = CARTESIAN_POINT('Ctrl Pts',(-17.0319178699977,-14.5231629813228,
116.637508947902)) ;
#163537 = CARTESIAN_POINT('Ctrl Pts',(-17.0243702739968,-14.451213086268,
116.614520189238)) ;
#163538 = CARTESIAN_POINT('Ctrl Pts',(-16.9454296666756,-14.5046478984509,
116.338545787343)) ;
#163539 = CARTESIAN_POINT('Ctrl Pts',(-16.9441177229474,-14.4288576762163,
116.3345498192)) ;
#163540 = CARTESIAN_POINT('Ctrl Pts',(-17.0179215539013,-14.4288576774106,
116.310318739545)) ;
#163541 = CARTESIAN_POINT('Ctrl Pts',(-17.0917253848553,-14.4288576786049,
116.286087659889)) ;
#163542 = CARTESIAN_POINT('Ctrl Pts',(-17.0930373285836,-14.5046479008395,
116.290083628032)) ;
#163543 = CARTESIAN_POINT('Ctrl Pts',(-17.0943492723118,-14.5804381230741,
116.294079596175)) ;
#163544 = CARTESIAN_POINT('Ctrl Pts',(-17.0205454413578,-14.5804381218798,
116.318310675831)) ;
#163545 = CARTESIAN_POINT('Ctrl Pts',(-16.9467416104039,-14.5804381206855,
116.342541755486)) ;
#163546 = CARTESIAN_POINT('Ctrl Pts',(-16.9454296666756,-14.5046478984509,
116.338545787343)) ;
#163547 = CARTESIAN_POINT('Ctrl Pts',(-16.8656122340257,-14.4801334339684,
116.060046712965)) ;
#163548 = CARTESIAN_POINT('Ctrl Pts',(-16.8706036868272,-14.4059401882447,
116.075249873451)) ;
#163549 = CARTESIAN_POINT('Ctrl Pts',(-16.9444075204913,-14.405940180657,
116.051018802051)) ;
#163550 = CARTESIAN_POINT('Ctrl Pts',(-17.0182113541555,-14.4059401730692,
116.02678773065)) ;
#163551 = CARTESIAN_POINT('Ctrl Pts',(-17.013219901354,-14.4801334187929,
116.011584570164)) ;
#163552 = CARTESIAN_POINT('Ctrl Pts',(-17.0082284485525,-14.5543266645165,
115.996381409677)) ;
#163553 = CARTESIAN_POINT('Ctrl Pts',(-16.9344246148884,-14.5543266721042,
116.020612481078)) ;
#163554 = CARTESIAN_POINT('Ctrl Pts',(-16.8606207812242,-14.554326679692,
116.044843552478)) ;
#163555 = CARTESIAN_POINT('Ctrl Pts',(-16.8656122340257,-14.4801334339684,
116.060046712965)) ;
#163556 = CARTESIAN_POINT('Ctrl Pts',(-16.790980956793,-14.3800974324411,
115.797335713982)) ;
#163557 = CARTESIAN_POINT('Ctrl Pts',(-16.801923417816,-14.3127767665056,
115.830664685171)) ;
#163558 = CARTESIAN_POINT('Ctrl Pts',(-16.8757272545943,-14.3127767543614,
115.806433623256)) ;
#163559 = CARTESIAN_POINT('Ctrl Pts',(-16.9495310913725,-14.3127767422172,
115.78220256134)) ;
#163560 = CARTESIAN_POINT('Ctrl Pts',(-16.9385886303495,-14.3800974081526,
115.748873590151)) ;
#163561 = CARTESIAN_POINT('Ctrl Pts',(-16.9276461693265,-14.4474180740881,
115.715544618961)) ;
#163562 = CARTESIAN_POINT('Ctrl Pts',(-16.8538423325482,-14.4474180862324,
115.739775680876)) ;
#163563 = CARTESIAN_POINT('Ctrl Pts',(-16.78003849577,-14.4474180983766,115.764006742792)) ;
#163564 = CARTESIAN_POINT('Ctrl Pts',(-16.790980956793,-14.3800974324411,
115.797335713982)) ;
#163565 = CARTESIAN_POINT('Ctrl Pts',(-16.7272992435064,-14.2097836883392,
115.567723704897)) ;
#163566 = CARTESIAN_POINT('Ctrl Pts',(-16.7434426567899,-14.1542529210645,
115.616893937324)) ;
#163567 = CARTESIAN_POINT('Ctrl Pts',(-16.8172464968672,-14.1542529100711,
115.592662885457)) ;
#163568 = CARTESIAN_POINT('Ctrl Pts',(-16.8910503369444,-14.1542528990776,
115.568431833589)) ;
#163569 = CARTESIAN_POINT('Ctrl Pts',(-16.8749069236608,-14.2097836663522,
115.519261601162)) ;
#163570 = CARTESIAN_POINT('Ctrl Pts',(-16.8587635103773,-14.2653144336269,
115.470091368735)) ;
#163571 = CARTESIAN_POINT('Ctrl Pts',(-16.7849596703,-14.2653144446203,115.494322420602)) ;
#163572 = CARTESIAN_POINT('Ctrl Pts',(-16.7111558302228,-14.2653144556138,
115.518553472469)) ;
#163573 = CARTESIAN_POINT('Ctrl Pts',(-16.7272992435064,-14.2097836883392,
115.567723704897)) ;
#163574 = CARTESIAN_POINT('Ctrl Pts',(-16.6808108315259,-13.9844447661634,
115.3908060488)) ;
#163575 = CARTESIAN_POINT('Ctrl Pts',(-16.7009554993096,-13.944564790948,
115.452163456727)) ;
#163576 = CARTESIAN_POINT('Ctrl Pts',(-16.7747593412743,-13.9445647824093,
115.427932410608)) ;
#163577 = CARTESIAN_POINT('Ctrl Pts',(-16.848563183239,-13.9445647738706,
115.40370136449)) ;
#163578 = CARTESIAN_POINT('Ctrl Pts',(-16.8284185154553,-13.984444749086,
115.342343956563)) ;
#163579 = CARTESIAN_POINT('Ctrl Pts',(-16.8082738476717,-14.0243247243014,
115.280986548637)) ;
#163580 = CARTESIAN_POINT('Ctrl Pts',(-16.734470005707,-14.0243247328401,
115.305217594755)) ;
#163581 = CARTESIAN_POINT('Ctrl Pts',(-16.6606661637423,-14.0243247413788,
115.329448640873)) ;
#163582 = CARTESIAN_POINT('Ctrl Pts',(-16.6808108315259,-13.9844447661634,
115.3908060488)) ;
#163583 = CARTESIAN_POINT('Ctrl Pts',(-16.6547738612727,-13.7175338810347,
115.275995973862)) ;
#163584 = CARTESIAN_POINT('Ctrl Pts',(-16.6775017259514,-13.6962312533339,
115.345221382617)) ;
#163585 = CARTESIAN_POINT('Ctrl Pts',(-16.7513055691903,-13.6962312496336,
115.32099034038)) ;
#163586 = CARTESIAN_POINT('Ctrl Pts',(-16.8251094124292,-13.6962312459334,
115.296759298142)) ;
#163587 = CARTESIAN_POINT('Ctrl Pts',(-16.8023815477505,-13.7175338736341,
115.227533889387)) ;
#163588 = CARTESIAN_POINT('Ctrl Pts',(-16.7796536830717,-13.7388365013348,
115.158308480631)) ;
#163589 = CARTESIAN_POINT('Ctrl Pts',(-16.7058498398329,-13.7388365050351,
115.182539522869)) ;
#163590 = CARTESIAN_POINT('Ctrl Pts',(-16.632045996594,-13.7388365087354,
115.206770565106)) ;
#163591 = CARTESIAN_POINT('Ctrl Pts',(-16.6547738612727,-13.7175338810347,
115.275995973862)) ;
#163592 = CARTESIAN_POINT('Ctrl Pts',(-16.6522344647069,-13.4290941380284,
115.232763303442)) ;
#163593 = CARTESIAN_POINT('Ctrl Pts',(-16.6759083668004,-13.42790072271,115.304870189438)) ;
#163594 = CARTESIAN_POINT('Ctrl Pts',(-16.7497122103021,-13.4279007232461,
115.280639148001)) ;
#163595 = CARTESIAN_POINT('Ctrl Pts',(-16.8235160538039,-13.4279007237822,
115.256408106565)) ;
#163596 = CARTESIAN_POINT('Ctrl Pts',(-16.7998421517105,-13.4290941391006,
115.184301220568)) ;
#163597 = CARTESIAN_POINT('Ctrl Pts',(-16.7761682496171,-13.430287554419,
115.112194334572)) ;
#163598 = CARTESIAN_POINT('Ctrl Pts',(-16.7023644061153,-13.4302875538829,
115.136425376008)) ;
#163599 = CARTESIAN_POINT('Ctrl Pts',(-16.6285605626135,-13.4302875533468,
115.160656417445)) ;
#163600 = CARTESIAN_POINT('Ctrl Pts',(-16.6522344647069,-13.4290941380284,
115.232763303442)) ;
#163601 = CARTESIAN_POINT('Ctrl Pts',(-16.6738872742428,-13.1407025280343,
115.263323344163)) ;
#163602 = CARTESIAN_POINT('Ctrl Pts',(-16.6968168802155,-13.1596450179659,
115.333163224222)) ;
#163603 = CARTESIAN_POINT('Ctrl Pts',(-16.7706207234299,-13.1596450208018,
115.30893218191)) ;
#163604 = CARTESIAN_POINT('Ctrl Pts',(-16.8444245666443,-13.1596450236377,
115.284701139598)) ;
#163605 = CARTESIAN_POINT('Ctrl Pts',(-16.8214949606715,-13.1407025337061,
115.214861259539)) ;
#163606 = CARTESIAN_POINT('Ctrl Pts',(-16.7985653546987,-13.1217600437745,
115.14502137948)) ;
#163607 = CARTESIAN_POINT('Ctrl Pts',(-16.7247615114844,-13.1217600409386,
115.169252421792)) ;
#163608 = CARTESIAN_POINT('Ctrl Pts',(-16.65095766827,-13.1217600381026,115.193483464104)) ;
#163609 = CARTESIAN_POINT('Ctrl Pts',(-16.6738872742428,-13.1407025280343,
115.263323344163)) ;
#163610 = CARTESIAN_POINT('Ctrl Pts',(-16.7192914965339,-12.8707969653127,
115.366034947544)) ;
#163611 = CARTESIAN_POINT('Ctrl Pts',(-16.7398209850698,-12.9086154474282,
115.428564457142)) ;
#163612 = CARTESIAN_POINT('Ctrl Pts',(-16.8136248279612,-12.9086154501767,
115.404333413846)) ;
#163613 = CARTESIAN_POINT('Ctrl Pts',(-16.8874286708526,-12.9086154529253,
115.38010237055)) ;
#163614 = CARTESIAN_POINT('Ctrl Pts',(-16.8668991823167,-12.8707969708098,
115.317572860953)) ;
#163615 = CARTESIAN_POINT('Ctrl Pts',(-16.8463696937809,-12.8329784886943,
115.255043351355)) ;
#163616 = CARTESIAN_POINT('Ctrl Pts',(-16.7725658508895,-12.8329784859458,
115.279274394651)) ;
#163617 = CARTESIAN_POINT('Ctrl Pts',(-16.698762007998,-12.8329784831972,
115.303505437946)) ;
#163618 = CARTESIAN_POINT('Ctrl Pts',(-16.7192914965339,-12.8707969653127,
115.366034947544)) ;
#163619 = CARTESIAN_POINT('Ctrl Pts',(-16.7852951087572,-12.6417711077458,
115.53174600974)) ;
#163620 = CARTESIAN_POINT('Ctrl Pts',(-16.8019769392628,-12.6956372286185,
115.582556173826)) ;
#163621 = CARTESIAN_POINT('Ctrl Pts',(-16.8757807822629,-12.6956372295276,
115.558325130861)) ;
#163622 = CARTESIAN_POINT('Ctrl Pts',(-16.9495846252629,-12.6956372304368,
115.534094087896)) ;
#163623 = CARTESIAN_POINT('Ctrl Pts',(-16.9329027947574,-12.6417711095641,
115.48328392381)) ;
#163624 = CARTESIAN_POINT('Ctrl Pts',(-16.9162209642519,-12.5879049886915,
115.432473759724)) ;
#163625 = CARTESIAN_POINT('Ctrl Pts',(-16.8424171212518,-12.5879049877823,
115.456704802689)) ;
#163626 = CARTESIAN_POINT('Ctrl Pts',(-16.7686132782517,-12.5879049868731,
115.480935845654)) ;
#163627 = CARTESIAN_POINT('Ctrl Pts',(-16.7852951087572,-12.6417711077458,
115.53174600974)) ;
#163628 = CARTESIAN_POINT('Ctrl Pts',(-16.8687385029215,-12.4670674817275,
115.750354845925)) ;
#163629 = CARTESIAN_POINT('Ctrl Pts',(-16.8803538371374,-12.5332118470618,
115.785733279865)) ;
#163630 = CARTESIAN_POINT('Ctrl Pts',(-16.9541576811356,-12.5332118456008,
115.761502239941)) ;
#163631 = CARTESIAN_POINT('Ctrl Pts',(-17.0279615251339,-12.5332118441398,
115.737271200016)) ;
#163632 = CARTESIAN_POINT('Ctrl Pts',(-17.016346190918,-12.4670674788054,
115.701892766076)) ;
#163633 = CARTESIAN_POINT('Ctrl Pts',(-17.0047308567021,-12.4009231134711,
115.666514332135)) ;
#163634 = CARTESIAN_POINT('Ctrl Pts',(-16.9309270127038,-12.4009231149321,
115.69074537206)) ;
#163635 = CARTESIAN_POINT('Ctrl Pts',(-16.8571231687056,-12.4009231163931,
115.714976411984)) ;
#163636 = CARTESIAN_POINT('Ctrl Pts',(-16.8687385029215,-12.4670674817275,
115.750354845925)) ;
#163637 = CARTESIAN_POINT('Ctrl Pts',(-16.9635606886986,-12.3610581795072,
116.003803286491)) ;
#163638 = CARTESIAN_POINT('Ctrl Pts',(-16.9693038547935,-12.434700867629,
116.021296043894)) ;
#163639 = CARTESIAN_POINT('Ctrl Pts',(-17.0431077002693,-12.4347008654183,
115.997065008469)) ;
#163640 = CARTESIAN_POINT('Ctrl Pts',(-17.116911545745,-12.4347008632077,
115.972833973045)) ;
#163641 = CARTESIAN_POINT('Ctrl Pts',(-17.11116837965,-12.3610581750859,115.955341215642)) ;
#163642 = CARTESIAN_POINT('Ctrl Pts',(-17.1054252135551,-12.2874154869641,
115.937848458239)) ;
#163643 = CARTESIAN_POINT('Ctrl Pts',(-17.0316213680793,-12.2874154891748,
115.962079493663)) ;
#163644 = CARTESIAN_POINT('Ctrl Pts',(-16.9578175226036,-12.2874154913854,
115.986310529088)) ;
#163645 = CARTESIAN_POINT('Ctrl Pts',(-16.9635606886986,-12.3610581795072,
116.003803286491)) ;
#163646 = CARTESIAN_POINT('Ctrl Pts',(-17.0649420670116,-12.3304705905987,
116.27693713892)) ;
#163647 = CARTESIAN_POINT('Ctrl Pts',(-17.0643525739706,-12.4063567534876,
116.275141638518)) ;
#163648 = CARTESIAN_POINT('Ctrl Pts',(-17.138156421995,-12.4063567532817,
116.250910610856)) ;
#163649 = CARTESIAN_POINT('Ctrl Pts',(-17.2119602700193,-12.4063567530759,
116.226679583194)) ;
#163650 = CARTESIAN_POINT('Ctrl Pts',(-17.2125497630602,-12.330470590187,
116.228475083596)) ;
#163651 = CARTESIAN_POINT('Ctrl Pts',(-17.2131392561011,-12.2545844272981,
116.230270583998)) ;
#163652 = CARTESIAN_POINT('Ctrl Pts',(-17.1393354080768,-12.254584427504,
116.25450161166)) ;
#163653 = CARTESIAN_POINT('Ctrl Pts',(-17.0655315600525,-12.2545844277098,
116.278732639322)) ;
#163654 = CARTESIAN_POINT('Ctrl Pts',(-17.0649420670116,-12.3304705905987,
116.27693713892)) ;
#163655 = CARTESIAN_POINT('Ctrl Pts',(-17.1648109896159,-12.3780041179342,
116.545751053977)) ;
#163656 = CARTESIAN_POINT('Ctrl Pts',(-17.1579795166612,-12.4506811357788,
116.524943490027)) ;
#163657 = CARTESIAN_POINT('Ctrl Pts',(-17.2317833665539,-12.4506811414498,
116.500712468056)) ;
#163658 = CARTESIAN_POINT('Ctrl Pts',(-17.3055872164466,-12.4506811471207,
116.476481446085)) ;
#163659 = CARTESIAN_POINT('Ctrl Pts',(-17.3124186894012,-12.3780041292761,
116.497289010035)) ;
#163660 = CARTESIAN_POINT('Ctrl Pts',(-17.3192501623558,-12.3053271114316,
116.518096573985)) ;
#163661 = CARTESIAN_POINT('Ctrl Pts',(-17.2454463124632,-12.3053271057606,
116.542327595956)) ;
#163662 = CARTESIAN_POINT('Ctrl Pts',(-17.1716424625705,-12.3053271000897,
116.566558617927)) ;
#163663 = CARTESIAN_POINT('Ctrl Pts',(-17.1648109896159,-12.3780041179342,
116.545751053977)) ;
#163664 = CARTESIAN_POINT('Ctrl Pts',(-17.2579372276331,-12.5002675543906,
116.79387021803)) ;
#163665 = CARTESIAN_POINT('Ctrl Pts',(-17.2453288035709,-12.5645133223993,
116.755466993281)) ;
#163666 = CARTESIAN_POINT('Ctrl Pts',(-17.3191326550243,-12.5645133380227,
116.731235976064)) ;
#163667 = CARTESIAN_POINT('Ctrl Pts',(-17.3929365064777,-12.5645133536461,
116.707004958847)) ;
#163668 = CARTESIAN_POINT('Ctrl Pts',(-17.40554493054,-12.5002675856374,116.745408183595)) ;
#163669 = CARTESIAN_POINT('Ctrl Pts',(-17.4181533546022,-12.4360218176287,
116.783811408344)) ;
#163670 = CARTESIAN_POINT('Ctrl Pts',(-17.3443495031488,-12.4360218020053,
116.808042425561)) ;
#163671 = CARTESIAN_POINT('Ctrl Pts',(-17.2705456516954,-12.4360217863819,
116.832273442779)) ;
#163672 = CARTESIAN_POINT('Ctrl Pts',(-17.2579372276331,-12.5002675543906,
116.79387021803)) ;
#163673 = CARTESIAN_POINT('Ctrl Pts',(-17.3375779201861,-12.6872113223539,
117.001122929289)) ;
#163674 = CARTESIAN_POINT('Ctrl Pts',(-17.3201216848697,-12.7384971666027,
116.947954053789)) ;
#163675 = CARTESIAN_POINT('Ctrl Pts',(-17.3939255362724,-12.7384971937162,
116.923723036417)) ;
#163676 = CARTESIAN_POINT('Ctrl Pts',(-17.4677293876751,-12.7384972208297,
116.899492019045)) ;
#163677 = CARTESIAN_POINT('Ctrl Pts',(-17.4851856229915,-12.6872113765809,
116.952660894545)) ;
#163678 = CARTESIAN_POINT('Ctrl Pts',(-17.5026418583079,-12.635925532332,
117.005829770045)) ;
#163679 = CARTESIAN_POINT('Ctrl Pts',(-17.4288380069052,-12.6359255052185,
117.030060787417)) ;
#163680 = CARTESIAN_POINT('Ctrl Pts',(-17.3550341555026,-12.635925478105,
117.054291804789)) ;
#163681 = CARTESIAN_POINT('Ctrl Pts',(-17.3375779201861,-12.6872113223539,
117.001122929289)) ;
#163682 = CARTESIAN_POINT('Ctrl Pts',(-17.3998316457169,-12.928470822573,
117.155087519117)) ;
#163683 = CARTESIAN_POINT('Ctrl Pts',(-17.3787411946458,-12.9629864518457,
117.09084940901)) ;
#163684 = CARTESIAN_POINT('Ctrl Pts',(-17.4525450450027,-12.9629864941427,
117.066618388453)) ;
#163685 = CARTESIAN_POINT('Ctrl Pts',(-17.5263488953595,-12.9629865364398,
117.042387367896)) ;
#163686 = CARTESIAN_POINT('Ctrl Pts',(-17.5474393464306,-12.9284709071671,
117.106625478002)) ;
#163687 = CARTESIAN_POINT('Ctrl Pts',(-17.5685297975017,-12.8939552778944,
117.170863588109)) ;
#163688 = CARTESIAN_POINT('Ctrl Pts',(-17.4947259471448,-12.8939552355973,
117.195094608666)) ;
#163689 = CARTESIAN_POINT('Ctrl Pts',(-17.420922096788,-12.8939551933003,
117.219325629224)) ;
#163690 = CARTESIAN_POINT('Ctrl Pts',(-17.3998316457169,-12.928470822573,
117.155087519117)) ;
#163691 = CARTESIAN_POINT('Ctrl Pts',(-17.4399174994754,-13.2034657060163,
117.241757837914)) ;
#163692 = CARTESIAN_POINT('Ctrl Pts',(-17.416730872886,-13.2188313176784,
117.171135115555)) ;
#163693 = CARTESIAN_POINT('Ctrl Pts',(-17.4905347199573,-13.2188313725587,
117.146904084991)) ;
#163694 = CARTESIAN_POINT('Ctrl Pts',(-17.5643385670287,-13.218831427439,
117.122673054427)) ;
#163695 = CARTESIAN_POINT('Ctrl Pts',(-17.5875251936181,-13.2034658157769,
117.193295776785)) ;
#163696 = CARTESIAN_POINT('Ctrl Pts',(-17.6107118202076,-13.1881002041148,
117.263918499144)) ;
#163697 = CARTESIAN_POINT('Ctrl Pts',(-17.5369079731363,-13.1881001492345,
117.288149529709)) ;
#163698 = CARTESIAN_POINT('Ctrl Pts',(-17.4631041260649,-13.1881000943542,
117.312380560273)) ;
#163699 = CARTESIAN_POINT('Ctrl Pts',(-17.4399174994754,-13.2034657060163,
117.241757837914)) ;
#163700 = CARTESIAN_POINT('Ctrl Pts',(-17.4562690855038,-13.4939400108665,
117.256107218264)) ;
#163701 = CARTESIAN_POINT('Ctrl Pts',(-17.4326409399332,-13.4890474543543,
117.184139700489)) ;
#163702 = CARTESIAN_POINT('Ctrl Pts',(-17.5064447821528,-13.4890475187126,
117.159908655147)) ;
#163703 = CARTESIAN_POINT('Ctrl Pts',(-17.5802486243724,-13.4890475830709,
117.135677609805)) ;
#163704 = CARTESIAN_POINT('Ctrl Pts',(-17.603876769943,-13.4939401395831,
117.20764512758)) ;
#163705 = CARTESIAN_POINT('Ctrl Pts',(-17.6275049155135,-13.4988326960953,
117.279612645354)) ;
#163706 = CARTESIAN_POINT('Ctrl Pts',(-17.553701073294,-13.498832631737,117.303843690697)) ;
#163707 = CARTESIAN_POINT('Ctrl Pts',(-17.4798972310744,-13.4988325673787,
117.328074736039)) ;
#163708 = CARTESIAN_POINT('Ctrl Pts',(-17.4562690855038,-13.4939400108665,
117.256107218264)) ;
#163709 = CARTESIAN_POINT('Ctrl Pts',(-17.4483972852435,-13.7785749983251,
117.196730556268)) ;
#163710 = CARTESIAN_POINT('Ctrl Pts',(-17.4260170952016,-13.7538028114636,
117.128564109822)) ;
#163711 = CARTESIAN_POINT('Ctrl Pts',(-17.4998209313486,-13.7538028795782,
117.104333045984)) ;
#163712 = CARTESIAN_POINT('Ctrl Pts',(-17.5736247674956,-13.7538029476928,
117.080101982146)) ;
#163713 = CARTESIAN_POINT('Ctrl Pts',(-17.5960049575374,-13.7785751345543,
117.148268428592)) ;
#163714 = CARTESIAN_POINT('Ctrl Pts',(-17.6183851475792,-13.8033473214157,
117.216434875038)) ;
#163715 = CARTESIAN_POINT('Ctrl Pts',(-17.5445813114322,-13.8033472533012,
117.240665938876)) ;
#163716 = CARTESIAN_POINT('Ctrl Pts',(-17.4707774752853,-13.8033471851866,
117.264897002714)) ;
#163717 = CARTESIAN_POINT('Ctrl Pts',(-17.4483972852435,-13.7785749983251,
117.196730556268)) ;
#163718 = CARTESIAN_POINT('Ctrl Pts',(-17.4176717828043,-14.0376123935157,
117.067726587636)) ;
#163719 = CARTESIAN_POINT('Ctrl Pts',(-17.398137247503,-13.9947190826741,
117.008227546524)) ;
#163720 = CARTESIAN_POINT('Ctrl Pts',(-17.4719410769957,-13.9947191481114,
116.983996462419)) ;
#163721 = CARTESIAN_POINT('Ctrl Pts',(-17.5457449064884,-13.9947192135486,
116.959765378313)) ;
#163722 = CARTESIAN_POINT('Ctrl Pts',(-17.5652794417897,-14.0376125243903,
117.019264419424)) ;
#163723 = CARTESIAN_POINT('Ctrl Pts',(-17.584813977091,-14.0805058352319,
117.078763460535)) ;
#163724 = CARTESIAN_POINT('Ctrl Pts',(-17.5110101475983,-14.0805057697947,
117.102994544641)) ;
#163725 = CARTESIAN_POINT('Ctrl Pts',(-17.4372063181056,-14.0805057043574,
117.127225628747)) ;
#163726 = CARTESIAN_POINT('Ctrl Pts',(-17.4176717828043,-14.0376123935157,
117.067726587636)) ;
#163727 = CARTESIAN_POINT('Ctrl Pts',(-17.3669381628985,-14.2526152270872,
116.877737714805)) ;
#163728 = CARTESIAN_POINT('Ctrl Pts',(-17.3516510972301,-14.1946488297789,
116.831175781003)) ;
#163729 = CARTESIAN_POINT('Ctrl Pts',(-17.4254549201375,-14.1946488854693,
116.80694467684)) ;
#163730 = CARTESIAN_POINT('Ctrl Pts',(-17.499258743045,-14.1946489411597,
116.782713572676)) ;
#163731 = CARTESIAN_POINT('Ctrl Pts',(-17.5145458087134,-14.252615338468,
116.829275506478)) ;
#163732 = CARTESIAN_POINT('Ctrl Pts',(-17.5298328743817,-14.3105817357762,
116.87583744028)) ;
#163733 = CARTESIAN_POINT('Ctrl Pts',(-17.4560290514743,-14.3105816800858,
116.900068544444)) ;
#163734 = CARTESIAN_POINT('Ctrl Pts',(-17.3822252285668,-14.3105816243954,
116.924299648607)) ;
#163735 = CARTESIAN_POINT('Ctrl Pts',(-17.3669381628985,-14.2526152270872,
116.877737714805)) ;
#163736 = CARTESIAN_POINT('Ctrl Pts',(-17.300521743148,-14.4080507138092,
116.639938676009)) ;
#163737 = CARTESIAN_POINT('Ctrl Pts',(-17.2905840086684,-14.3391479238767,
116.609669942021)) ;
#163738 = CARTESIAN_POINT('Ctrl Pts',(-17.3643878258509,-14.3391479627699,
116.585438820421)) ;
#163739 = CARTESIAN_POINT('Ctrl Pts',(-17.4381916430334,-14.3391480016631,
116.56120769882)) ;
#163740 = CARTESIAN_POINT('Ctrl Pts',(-17.448129377513,-14.4080507915956,
116.591476432807)) ;
#163741 = CARTESIAN_POINT('Ctrl Pts',(-17.4580671119925,-14.4769535815281,
116.621745166794)) ;
#163742 = CARTESIAN_POINT('Ctrl Pts',(-17.38426329481,-14.4769535426349,116.645976288395)) ;
#163743 = CARTESIAN_POINT('Ctrl Pts',(-17.3104594776275,-14.4769535037417,
116.670207409996)) ;
#163744 = CARTESIAN_POINT('Ctrl Pts',(-17.300521743148,-14.4080507138092,
116.639938676009)) ;
#163745 = CARTESIAN_POINT('Ctrl Pts',(-17.2239015581171,-14.4922598223547,
116.371021974036)) ;
#163746 = CARTESIAN_POINT('Ctrl Pts',(-17.2200340718307,-14.4173770699575,
116.359242236723)) ;
#163747 = CARTESIAN_POINT('Ctrl Pts',(-17.2938378850058,-14.4173770858156,
116.335011102916)) ;
#163748 = CARTESIAN_POINT('Ctrl Pts',(-17.367641698181,-14.4173771016737,
116.31077996911)) ;
#163749 = CARTESIAN_POINT('Ctrl Pts',(-17.3715091844673,-14.4922598540709,
116.322559706423)) ;
#163750 = CARTESIAN_POINT('Ctrl Pts',(-17.3753766707537,-14.5671426064681,
116.334339443736)) ;
#163751 = CARTESIAN_POINT('Ctrl Pts',(-17.3015728575786,-14.56714259061,116.358570577543)) ;
#163752 = CARTESIAN_POINT('Ctrl Pts',(-17.2277690444035,-14.5671425747519,
116.38280171135)) ;
#163753 = CARTESIAN_POINT('Ctrl Pts',(-17.2239015581171,-14.4922598223547,
116.371021974036)) ;
#163754 = CARTESIAN_POINT('Ctrl Pts',(-17.1439517410193,-14.4995566650645,
116.092195902509)) ;
#163755 = CARTESIAN_POINT('Ctrl Pts',(-17.1463910960368,-14.4240553765711,
116.099625786271)) ;
#163756 = CARTESIAN_POINT('Ctrl Pts',(-17.2201949078783,-14.4240553658153,
116.075394648402)) ;
#163757 = CARTESIAN_POINT('Ctrl Pts',(-17.2939987197198,-14.4240553550595,
116.051163510533)) ;
#163758 = CARTESIAN_POINT('Ctrl Pts',(-17.2915593647023,-14.4995566435528,
116.043733626772)) ;
#163759 = CARTESIAN_POINT('Ctrl Pts',(-17.2891200096848,-14.5750579320462,
116.03630374301)) ;
#163760 = CARTESIAN_POINT('Ctrl Pts',(-17.2153161978433,-14.575057942802,
116.060534880879)) ;
#163761 = CARTESIAN_POINT('Ctrl Pts',(-17.1415123860018,-14.5750579535578,
116.084766018747)) ;
#163762 = CARTESIAN_POINT('Ctrl Pts',(-17.1439517410193,-14.4995566650645,
116.092195902509)) ;
#163763 = CARTESIAN_POINT('Ctrl Pts',(-17.0659766810491,-14.4291954268347,
115.819082015723)) ;
#163764 = CARTESIAN_POINT('Ctrl Pts',(-17.0746003967584,-14.3584951723125,
115.845348464383)) ;
#163765 = CARTESIAN_POINT('Ctrl Pts',(-17.1484042095327,-14.3584951335383,
115.821117329355)) ;
#163766 = CARTESIAN_POINT('Ctrl Pts',(-17.2222080223069,-14.358495094764,
115.796886194328)) ;
#163767 = CARTESIAN_POINT('Ctrl Pts',(-17.2135843065975,-14.4291953492863,
115.770619745668)) ;
#163768 = CARTESIAN_POINT('Ctrl Pts',(-17.2049605908881,-14.4998956038086,
115.744353297008)) ;
#163769 = CARTESIAN_POINT('Ctrl Pts',(-17.1311567781139,-14.4998956425828,
115.768584432035)) ;
#163770 = CARTESIAN_POINT('Ctrl Pts',(-17.0573529653397,-14.499895681357,
115.792815567063)) ;
#163771 = CARTESIAN_POINT('Ctrl Pts',(-17.0659766810491,-14.4291954268347,
115.819082015723)) ;
#163772 = CARTESIAN_POINT('Ctrl Pts',(-16.9973489861747,-14.2862746553945,
115.574590132372)) ;
#163773 = CARTESIAN_POINT('Ctrl Pts',(-17.0115105195248,-14.2254484542933,
115.617723880079)) ;
#163774 = CARTESIAN_POINT('Ctrl Pts',(-17.0853143361643,-14.2254483895805,
115.593492756825)) ;
#163775 = CARTESIAN_POINT('Ctrl Pts',(-17.1591181528039,-14.2254483248678,
115.56926163357)) ;
#163776 = CARTESIAN_POINT('Ctrl Pts',(-17.1449566194538,-14.286274525969,
115.526127885863)) ;
#163777 = CARTESIAN_POINT('Ctrl Pts',(-17.1307950861037,-14.3471007270702,
115.482994138157)) ;
#163778 = CARTESIAN_POINT('Ctrl Pts',(-17.0569912694642,-14.347100791783,
115.507225261411)) ;
#163779 = CARTESIAN_POINT('Ctrl Pts',(-16.9831874528246,-14.3471008564957,
115.531456384666)) ;
#163780 = CARTESIAN_POINT('Ctrl Pts',(-16.9973489861747,-14.2862746553945,
115.574590132372)) ;
#163781 = CARTESIAN_POINT('Ctrl Pts',(-16.943507599311,-14.0821782924177,
115.375260361907)) ;
#163782 = CARTESIAN_POINT('Ctrl Pts',(-16.9621801863693,-14.0355118999346,
115.432134051369)) ;
#163783 = CARTESIAN_POINT('Ctrl Pts',(-17.0359840091523,-14.0355118141507,
115.407902946826)) ;
#163784 = CARTESIAN_POINT('Ctrl Pts',(-17.1097878319353,-14.0355117283667,
115.383671842284)) ;
#163785 = CARTESIAN_POINT('Ctrl Pts',(-17.091115244877,-14.0821781208498,
115.326798152822)) ;
#163786 = CARTESIAN_POINT('Ctrl Pts',(-17.0724426578187,-14.1288445133328,
115.26992446336)) ;
#163787 = CARTESIAN_POINT('Ctrl Pts',(-16.9986388350357,-14.1288445991168,
115.294155567902)) ;
#163788 = CARTESIAN_POINT('Ctrl Pts',(-16.9248350122527,-14.1288446849008,
115.318386672445)) ;
#163789 = CARTESIAN_POINT('Ctrl Pts',(-16.943507599311,-14.0821782924177,
115.375260361907)) ;
#163790 = CARTESIAN_POINT('Ctrl Pts',(-16.9086511894243,-13.8298750263426,
115.233624849604)) ;
#163791 = CARTESIAN_POINT('Ctrl Pts',(-16.9305188675121,-13.8007543288235,
115.300230270815)) ;
#163792 = CARTESIAN_POINT('Ctrl Pts',(-17.0043226981659,-13.8007542285384,
115.275999190246)) ;
#163793 = CARTESIAN_POINT('Ctrl Pts',(-17.0781265288196,-13.8007541282534,
115.251768109676)) ;
#163794 = CARTESIAN_POINT('Ctrl Pts',(-17.0562588507318,-13.8298748257726,
115.185162688465)) ;
#163795 = CARTESIAN_POINT('Ctrl Pts',(-17.0343911726441,-13.8589955232917,
115.118557267253)) ;
#163796 = CARTESIAN_POINT('Ctrl Pts',(-16.9605873419903,-13.8589956235767,
115.142788347823)) ;
#163797 = CARTESIAN_POINT('Ctrl Pts',(-16.8867835113365,-13.8589957238618,
115.167019428392)) ;
#163798 = CARTESIAN_POINT('Ctrl Pts',(-16.9086511894243,-13.8298750263426,
115.233624849604)) ;
#163799 = CARTESIAN_POINT('Ctrl Pts',(-16.8963479197035,-13.5470860719876,
115.160572447035)) ;
#163800 = CARTESIAN_POINT('Ctrl Pts',(-16.9198433509072,-13.5376651784076,
115.232135741571)) ;
#163801 = CARTESIAN_POINT('Ctrl Pts',(-16.993647190433,-13.5376650723535,
115.207904688025)) ;
#163802 = CARTESIAN_POINT('Ctrl Pts',(-17.0674510299589,-13.5376649662995,
115.183673634478)) ;
#163803 = CARTESIAN_POINT('Ctrl Pts',(-17.0439555987552,-13.5470858598794,
115.112110339942)) ;
#163804 = CARTESIAN_POINT('Ctrl Pts',(-17.0204601675516,-13.5565067534594,
115.040547045406)) ;
#163805 = CARTESIAN_POINT('Ctrl Pts',(-16.9466563280257,-13.5565068595135,
115.064778098952)) ;
#163806 = CARTESIAN_POINT('Ctrl Pts',(-16.8728524884998,-13.5565069655676,
115.089009152499)) ;
#163807 = CARTESIAN_POINT('Ctrl Pts',(-16.8963479197035,-13.5470860719876,
115.160572447035)) ;
#163808 = CARTESIAN_POINT('Ctrl Pts',(-16.90824578111,-13.2560613841224,115.161364252542)) ;
#163809 = CARTESIAN_POINT('Ctrl Pts',(-16.9316790297655,-13.2669448864172,
115.232738149021)) ;
#163810 = CARTESIAN_POINT('Ctrl Pts',(-17.0054828781172,-13.266944783336,
115.208507122357)) ;
#163811 = CARTESIAN_POINT('Ctrl Pts',(-17.0792867264688,-13.2669446802549,
115.184276095692)) ;
#163812 = CARTESIAN_POINT('Ctrl Pts',(-17.0558534778133,-13.2560611779601,
115.112902199213)) ;
#163813 = CARTESIAN_POINT('Ctrl Pts',(-17.0324202291578,-13.2451776756653,
115.041528302733)) ;
#163814 = CARTESIAN_POINT('Ctrl Pts',(-16.9586163808062,-13.2451777787465,
115.065759329398)) ;
#163815 = CARTESIAN_POINT('Ctrl Pts',(-16.8848125324545,-13.2451778818276,
115.089990356062)) ;
#163816 = CARTESIAN_POINT('Ctrl Pts',(-16.90824578111,-13.2560613841224,115.161364252542)) ;
#163817 = CARTESIAN_POINT('Ctrl Pts',(-16.9442254493305,-12.9762949722028,
115.235455446136)) ;
#163818 = CARTESIAN_POINT('Ctrl Pts',(-16.9659162848826,-13.0067272528639,
115.301522233367)) ;
#163819 = CARTESIAN_POINT('Ctrl Pts',(-17.0397201411344,-13.0067271611354,
115.277291230766)) ;
#163820 = CARTESIAN_POINT('Ctrl Pts',(-17.1135239973862,-13.0067270694068,
115.253060228164)) ;
#163821 = CARTESIAN_POINT('Ctrl Pts',(-17.0918331618342,-12.9762947887458,
115.186993440932)) ;
#163822 = CARTESIAN_POINT('Ctrl Pts',(-17.0701423262821,-12.9458625080848,
115.120926653701)) ;
#163823 = CARTESIAN_POINT('Ctrl Pts',(-16.9963384700303,-12.9458625998133,
115.145157656303)) ;
#163824 = CARTESIAN_POINT('Ctrl Pts',(-16.9225346137784,-12.9458626915418,
115.169388658905)) ;
#163825 = CARTESIAN_POINT('Ctrl Pts',(-16.9442254493305,-12.9762949722028,
115.235455446136)) ;
#163826 = CARTESIAN_POINT('Ctrl Pts',(-17.0022072372073,-12.729021213087,
115.376690040029)) ;
#163827 = CARTESIAN_POINT('Ctrl Pts',(-17.0206142060272,-12.7767631435002,
115.432754698965)) ;
#163828 = CARTESIAN_POINT('Ctrl Pts',(-17.0944180685995,-12.7767630691524,
115.408523715614)) ;
#163829 = CARTESIAN_POINT('Ctrl Pts',(-17.1682219311719,-12.7767629948046,
115.384292732264)) ;
#163830 = CARTESIAN_POINT('Ctrl Pts',(-17.1498149623519,-12.7290210643915,
115.328228073327)) ;
#163831 = CARTESIAN_POINT('Ctrl Pts',(-17.131407993532,-12.6812791339783,
115.272163414391)) ;
#163832 = CARTESIAN_POINT('Ctrl Pts',(-17.0576041309596,-12.6812792083261,
115.296394397742)) ;
#163833 = CARTESIAN_POINT('Ctrl Pts',(-16.9838002683873,-12.6812792826738,
115.320625381093)) ;
#163834 = CARTESIAN_POINT('Ctrl Pts',(-17.0022072372073,-12.729021213087,
115.376690040029)) ;
#163835 = CARTESIAN_POINT('Ctrl Pts',(-17.0792272362676,-12.5300504685621,
115.575764889513)) ;
#163836 = CARTESIAN_POINT('Ctrl Pts',(-17.0930194529222,-12.5917559666324,
115.617773757829)) ;
#163837 = CARTESIAN_POINT('Ctrl Pts',(-17.1668233195247,-12.5917559147477,
115.593542786754)) ;
#163838 = CARTESIAN_POINT('Ctrl Pts',(-17.2406271861272,-12.5917558628629,
115.569311815679)) ;
#163839 = CARTESIAN_POINT('Ctrl Pts',(-17.2268349694727,-12.5300503647925,
115.527302947363)) ;
#163840 = CARTESIAN_POINT('Ctrl Pts',(-17.2130427528181,-12.4683448667222,
115.485294079046)) ;
#163841 = CARTESIAN_POINT('Ctrl Pts',(-17.1392388862155,-12.468344918607,
115.509525050122)) ;
#163842 = CARTESIAN_POINT('Ctrl Pts',(-17.065435019613,-12.4683449704918,
115.533756021197)) ;
#163843 = CARTESIAN_POINT('Ctrl Pts',(-17.0792272362676,-12.5300504685621,
115.575764889513)) ;
#163844 = CARTESIAN_POINT('Ctrl Pts',(-17.1704529515286,-12.3949013412461,
115.818078836631)) ;
#163845 = CARTESIAN_POINT('Ctrl Pts',(-17.1786322750179,-12.4661360013531,
115.842991737866)) ;
#163846 = CARTESIAN_POINT('Ctrl Pts',(-17.2524361430164,-12.4661359735393,
115.818760771042)) ;
#163847 = CARTESIAN_POINT('Ctrl Pts',(-17.3262400110149,-12.4661359457255,
115.794529804219)) ;
#163848 = CARTESIAN_POINT('Ctrl Pts',(-17.3180606875257,-12.3949012856185,
115.769616902984)) ;
#163849 = CARTESIAN_POINT('Ctrl Pts',(-17.3098813640364,-12.3236666255115,
115.744704001749)) ;
#163850 = CARTESIAN_POINT('Ctrl Pts',(-17.2360774960379,-12.3236666533253,
115.768934968573)) ;
#163851 = CARTESIAN_POINT('Ctrl Pts',(-17.1622736280394,-12.3236666811392,
115.793165935396)) ;
#163852 = CARTESIAN_POINT('Ctrl Pts',(-17.1704529515286,-12.3949013412461,
115.818078836631)) ;
#163853 = CARTESIAN_POINT('Ctrl Pts',(-17.2696316491355,-12.3334783627152,
116.084736767084)) ;
#163854 = CARTESIAN_POINT('Ctrl Pts',(-17.2716317461079,-12.4091090544744,
116.090828741229)) ;
#163855 = CARTESIAN_POINT('Ctrl Pts',(-17.3454356133753,-12.4091090490569,
116.066597772179)) ;
#163856 = CARTESIAN_POINT('Ctrl Pts',(-17.4192394806428,-12.4091090436395,
116.042366803129)) ;
#163857 = CARTESIAN_POINT('Ctrl Pts',(-17.4172393836704,-12.3334783518803,
116.036274828984)) ;
#163858 = CARTESIAN_POINT('Ctrl Pts',(-17.415239286698,-12.2578476601211,
116.030182854838)) ;
#163859 = CARTESIAN_POINT('Ctrl Pts',(-17.3414354194305,-12.2578476655386,
116.054413823888)) ;
#163860 = CARTESIAN_POINT('Ctrl Pts',(-17.2676315521631,-12.257847670956,
116.078644792938)) ;
#163861 = CARTESIAN_POINT('Ctrl Pts',(-17.2696316491355,-12.3334783627152,
116.084736767084)) ;
#163862 = CARTESIAN_POINT('Ctrl Pts',(-17.3706199437548,-12.3494129205617,
116.356939612366)) ;
#163863 = CARTESIAN_POINT('Ctrl Pts',(-17.3663044203247,-12.4240452801496,
116.343795225649)) ;
#163864 = CARTESIAN_POINT('Ctrl Pts',(-17.4401082850067,-12.4240452938977,
116.319564248724)) ;
#163865 = CARTESIAN_POINT('Ctrl Pts',(-17.5139121496887,-12.4240453076458,
116.295333271799)) ;
#163866 = CARTESIAN_POINT('Ctrl Pts',(-17.5182276731188,-12.3494129480579,
116.308477658515)) ;
#163867 = CARTESIAN_POINT('Ctrl Pts',(-17.5225431965489,-12.27478058847,116.321622045232)) ;
#163868 = CARTESIAN_POINT('Ctrl Pts',(-17.4487393318669,-12.2747805747219,
116.345853022157)) ;
#163869 = CARTESIAN_POINT('Ctrl Pts',(-17.3749354671849,-12.2747805609737,
116.370083999082)) ;
#163870 = CARTESIAN_POINT('Ctrl Pts',(-17.3706199437548,-12.3494129205617,
116.356939612366)) ;
#163871 = CARTESIAN_POINT('Ctrl Pts',(-17.4673694639669,-12.4418688951199,
116.61612522571)) ;
#163872 = CARTESIAN_POINT('Ctrl Pts',(-17.4570268792605,-12.5101591784945,
116.584623382643)) ;
#163873 = CARTESIAN_POINT('Ctrl Pts',(-17.5308307396141,-12.5101592062549,
116.560392392534)) ;
#163874 = CARTESIAN_POINT('Ctrl Pts',(-17.6046345999678,-12.5101592340153,
116.536161402426)) ;
#163875 = CARTESIAN_POINT('Ctrl Pts',(-17.6149771846741,-12.4418689506407,
116.567663245492)) ;
#163876 = CARTESIAN_POINT('Ctrl Pts',(-17.6253197693805,-12.373578667266,
116.599165088559)) ;
#163877 = CARTESIAN_POINT('Ctrl Pts',(-17.5515159090268,-12.3735786395056,
116.623396078668)) ;
#163878 = CARTESIAN_POINT('Ctrl Pts',(-17.4777120486732,-12.3735786117452,
116.647627068776)) ;
#163879 = CARTESIAN_POINT('Ctrl Pts',(-17.4673694639669,-12.4418688951199,
116.61612522571)) ;
#163880 = CARTESIAN_POINT('Ctrl Pts',(-17.5535183531139,-12.6051421932678,
116.842927305494)) ;
#163881 = CARTESIAN_POINT('Ctrl Pts',(-17.5378815244524,-12.6621364558016,
116.795300049372)) ;
#163882 = CARTESIAN_POINT('Ctrl Pts',(-17.6116853796284,-12.6621364903346,
116.771069043494)) ;
#163883 = CARTESIAN_POINT('Ctrl Pts',(-17.6854892348045,-12.6621365248676,
116.746838037615)) ;
#163884 = CARTESIAN_POINT('Ctrl Pts',(-17.701126063466,-12.6051422623338,
116.794465293737)) ;
#163885 = CARTESIAN_POINT('Ctrl Pts',(-17.7167628921274,-12.5481479998,116.842092549858)) ;
#163886 = CARTESIAN_POINT('Ctrl Pts',(-17.6429590369514,-12.548147965267,
116.866323555737)) ;
#163887 = CARTESIAN_POINT('Ctrl Pts',(-17.5691551817754,-12.548147930734,
116.890554561616)) ;
#163888 = CARTESIAN_POINT('Ctrl Pts',(-17.5535183531139,-12.6051421932678,
116.842927305494)) ;
#163889 = CARTESIAN_POINT('Ctrl Pts',(-17.6228267175663,-12.824581983231,
117.018781891196)) ;
#163890 = CARTESIAN_POINT('Ctrl Pts',(-17.6030564632207,-12.866340572483,
116.958564887239)) ;
#163891 = CARTESIAN_POINT('Ctrl Pts',(-17.6768603140324,-12.8663406101773,
116.934333868067)) ;
#163892 = CARTESIAN_POINT('Ctrl Pts',(-17.7506641648441,-12.8663406478716,
116.910102848895)) ;
#163893 = CARTESIAN_POINT('Ctrl Pts',(-17.7704344191897,-12.8245820586196,
116.970319852852)) ;
#163894 = CARTESIAN_POINT('Ctrl Pts',(-17.7902046735353,-12.7828234693676,
117.030536856809)) ;
#163895 = CARTESIAN_POINT('Ctrl Pts',(-17.7164008227236,-12.7828234316733,
117.054767875981)) ;
#163896 = CARTESIAN_POINT('Ctrl Pts',(-17.6425969719119,-12.782823393979,
117.078998895153)) ;
#163897 = CARTESIAN_POINT('Ctrl Pts',(-17.6228267175663,-12.824581983231,
117.018781891196)) ;
#163898 = CARTESIAN_POINT('Ctrl Pts',(-17.6723197045104,-13.0878606072953,
117.134031445032)) ;
#163899 = CARTESIAN_POINT('Ctrl Pts',(-17.6497982889685,-13.1112998695193,
117.065434847795)) ;
#163900 = CARTESIAN_POINT('Ctrl Pts',(-17.7236021355016,-13.1112999036755,
117.041203815592)) ;
#163901 = CARTESIAN_POINT('Ctrl Pts',(-17.7974059820347,-13.1112999378317,
117.016972783388)) ;
#163902 = CARTESIAN_POINT('Ctrl Pts',(-17.8199273975766,-13.0878606756077,
117.085569380624)) ;
#163903 = CARTESIAN_POINT('Ctrl Pts',(-17.8424488131185,-13.0644214133836,
117.15416597786)) ;
#163904 = CARTESIAN_POINT('Ctrl Pts',(-17.7686449665854,-13.0644213792274,
117.178397010064)) ;
#163905 = CARTESIAN_POINT('Ctrl Pts',(-17.6948411200522,-13.0644213450712,
117.202628042268)) ;
#163906 = CARTESIAN_POINT('Ctrl Pts',(-17.6723197045104,-13.0878606072953,
117.134031445032)) ;
#163907 = CARTESIAN_POINT('Ctrl Pts',(-17.6985731634041,-13.3747557627756,
117.178522404017)) ;
#163908 = CARTESIAN_POINT('Ctrl Pts',(-17.6749185440874,-13.378198596209,
117.10647425076)) ;
#163909 = CARTESIAN_POINT('Ctrl Pts',(-17.7487223875847,-13.3781986232595,
117.082243209309)) ;
#163910 = CARTESIAN_POINT('Ctrl Pts',(-17.822526231082,-13.37819865031,117.058012167859)) ;
#163911 = CARTESIAN_POINT('Ctrl Pts',(-17.8461808503987,-13.3747558168767,
117.130060321116)) ;
#163912 = CARTESIAN_POINT('Ctrl Pts',(-17.8698354697153,-13.3713129834433,
117.202108474372)) ;
#163913 = CARTESIAN_POINT('Ctrl Pts',(-17.796031626218,-13.3713129563928,
117.226339515823)) ;
#163914 = CARTESIAN_POINT('Ctrl Pts',(-17.7222277827207,-13.3713129293423,
117.250570557273)) ;
#163915 = CARTESIAN_POINT('Ctrl Pts',(-17.6985731634041,-13.3747557627756,
117.178522404017)) ;
#163916 = CARTESIAN_POINT('Ctrl Pts',(-17.7004702306017,-13.6654070056361,
117.148736694593)) ;
#163917 = CARTESIAN_POINT('Ctrl Pts',(-17.6773832073947,-13.648560400251,
117.078417347336)) ;
#163918 = CARTESIAN_POINT('Ctrl Pts',(-17.751187049296,-13.6485604179734,
117.054186301025)) ;
#163919 = CARTESIAN_POINT('Ctrl Pts',(-17.8249908911973,-13.6485604356957,
117.029955254713)) ;
#163920 = CARTESIAN_POINT('Ctrl Pts',(-17.8480779144043,-13.6654070410809,
117.10027460197)) ;
#163921 = CARTESIAN_POINT('Ctrl Pts',(-17.8711649376114,-13.682253646466,
117.170593949227)) ;
#163922 = CARTESIAN_POINT('Ctrl Pts',(-17.7973610957101,-13.6822536287436,
117.194824995538)) ;
#163923 = CARTESIAN_POINT('Ctrl Pts',(-17.7235572538088,-13.6822536110213,
117.21905604185)) ;
#163924 = CARTESIAN_POINT('Ctrl Pts',(-17.7004702306017,-13.6654070056361,
117.148736694593)) ;
#163925 = CARTESIAN_POINT('Ctrl Pts',(-17.6787592525954,-13.9370542943595,
117.047221465574)) ;
#163926 = CARTESIAN_POINT('Ctrl Pts',(-17.6578856782785,-13.901214603103,
116.983643926372)) ;
#163927 = CARTESIAN_POINT('Ctrl Pts',(-17.7316895197608,-13.9012146131836,
116.959412878784)) ;
#163928 = CARTESIAN_POINT('Ctrl Pts',(-17.8054933612432,-13.9012146232642,
116.935181831197)) ;
#163929 = CARTESIAN_POINT('Ctrl Pts',(-17.8263669355601,-13.9370543145207,
116.998759370399)) ;
#163930 = CARTESIAN_POINT('Ctrl Pts',(-17.847240509877,-13.9728940057772,
117.062336909601)) ;
#163931 = CARTESIAN_POINT('Ctrl Pts',(-17.7734366683946,-13.9728939956966,
117.086567957188)) ;
#163932 = CARTESIAN_POINT('Ctrl Pts',(-17.6996328269123,-13.972893985616,
117.110799004776)) ;
#163933 = CARTESIAN_POINT('Ctrl Pts',(-17.6787592525954,-13.9370542943595,
117.047221465574)) ;
#163934 = CARTESIAN_POINT('Ctrl Pts',(-17.6354116057115,-14.1729033532404,
116.879576215049)) ;
#163935 = CARTESIAN_POINT('Ctrl Pts',(-17.6182703678625,-14.1205407691761,
116.827366770384)) ;
#163936 = CARTESIAN_POINT('Ctrl Pts',(-17.6920742101075,-14.1205407723559,
116.803135725119)) ;
#163937 = CARTESIAN_POINT('Ctrl Pts',(-17.7658780523526,-14.1205407755357,
116.778904679855)) ;
#163938 = CARTESIAN_POINT('Ctrl Pts',(-17.7830192902016,-14.1729033596,116.83111412452)) ;
#163939 = CARTESIAN_POINT('Ctrl Pts',(-17.8001605280506,-14.2252659436643,
116.883323569186)) ;
#163940 = CARTESIAN_POINT('Ctrl Pts',(-17.7263566858056,-14.2252659404845,
116.90755461445)) ;
#163941 = CARTESIAN_POINT('Ctrl Pts',(-17.6525528435606,-14.2252659373047,
116.931785659715)) ;
#163942 = CARTESIAN_POINT('Ctrl Pts',(-17.6354116057115,-14.1729033532404,
116.879576215049)) ;
#163943 = CARTESIAN_POINT('Ctrl Pts',(-17.5750711191891,-14.3528610645483,
116.660517699246)) ;
#163944 = CARTESIAN_POINT('Ctrl Pts',(-17.5628475105947,-14.2878546501218,
116.623286559762)) ;
#163945 = CARTESIAN_POINT('Ctrl Pts',(-17.6366513536394,-14.2878546504462,
116.599055516933)) ;
#163946 = CARTESIAN_POINT('Ctrl Pts',(-17.7104551966841,-14.2878546507707,
116.574824474105)) ;
#163947 = CARTESIAN_POINT('Ctrl Pts',(-17.7226788052785,-14.3528610651972,
116.612055613588)) ;
#163948 = CARTESIAN_POINT('Ctrl Pts',(-17.7349024138729,-14.4178674796237,
116.649286753072)) ;
#163949 = CARTESIAN_POINT('Ctrl Pts',(-17.6610985708282,-14.4178674792993,
116.673517795901)) ;
#163950 = CARTESIAN_POINT('Ctrl Pts',(-17.5872947277835,-14.4178674789748,
116.69774883873)) ;
#163951 = CARTESIAN_POINT('Ctrl Pts',(-17.5750711191891,-14.3528610645483,
116.660517699246)) ;
#163952 = CARTESIAN_POINT('Ctrl Pts',(-17.5017177853474,-14.4673900074207,
116.401484107417)) ;
#163953 = CARTESIAN_POINT('Ctrl Pts',(-17.4953350224789,-14.3942885636895,
116.382043241526)) ;
#163954 = CARTESIAN_POINT('Ctrl Pts',(-17.5691388666226,-14.39428856281,116.357812202044)) ;
#163955 = CARTESIAN_POINT('Ctrl Pts',(-17.6429427107664,-14.3942885619306,
116.333581162563)) ;
#163956 = CARTESIAN_POINT('Ctrl Pts',(-17.6493254736349,-14.4673900056618,
116.353022028454)) ;
#163957 = CARTESIAN_POINT('Ctrl Pts',(-17.6557082365034,-14.5404914493931,
116.372462894345)) ;
#163958 = CARTESIAN_POINT('Ctrl Pts',(-17.5819043923597,-14.5404914502725,
116.396693933826)) ;
#163959 = CARTESIAN_POINT('Ctrl Pts',(-17.508100548216,-14.540491451152,116.420924973308)) ;
#163960 = CARTESIAN_POINT('Ctrl Pts',(-17.5017177853474,-14.4673900074207,
116.401484107417)) ;
#163961 = CARTESIAN_POINT('Ctrl Pts',(-17.4223560273365,-14.5059091307987,
116.124370136875)) ;
#163962 = CARTESIAN_POINT('Ctrl Pts',(-17.4222379725532,-14.4300095722764,
116.124010560988)) ;
#163963 = CARTESIAN_POINT('Ctrl Pts',(-17.4960418170078,-14.4300095722936,
116.099779522454)) ;
#163964 = CARTESIAN_POINT('Ctrl Pts',(-17.5698456614624,-14.4300095723109,
116.075548483919)) ;
#163965 = CARTESIAN_POINT('Ctrl Pts',(-17.5699637162457,-14.5059091308332,
116.075908059805)) ;
#163966 = CARTESIAN_POINT('Ctrl Pts',(-17.5700817710291,-14.5818086893555,
116.076267635692)) ;
#163967 = CARTESIAN_POINT('Ctrl Pts',(-17.4962779265745,-14.5818086893382,
116.100498674226)) ;
#163968 = CARTESIAN_POINT('Ctrl Pts',(-17.4224740821199,-14.581808689321,
116.124729712761)) ;
#163969 = CARTESIAN_POINT('Ctrl Pts',(-17.4223560273365,-14.5059091307987,
116.124370136875)) ;
#163970 = CARTESIAN_POINT('Ctrl Pts',(-17.3429501969861,-14.467003448986,
115.847090385579)) ;
#163971 = CARTESIAN_POINT('Ctrl Pts',(-17.3491098301786,-14.3937086480908,
115.865851634383)) ;
#163972 = CARTESIAN_POINT('Ctrl Pts',(-17.4229136742994,-14.3937086489183,
115.841620594832)) ;
#163973 = CARTESIAN_POINT('Ctrl Pts',(-17.4967175184202,-14.3937086497458,
115.81738955528)) ;
#163974 = CARTESIAN_POINT('Ctrl Pts',(-17.4905578852277,-14.4670034506409,
115.798628306476)) ;
#163975 = CARTESIAN_POINT('Ctrl Pts',(-17.4843982520352,-14.5402982515361,
115.779867057672)) ;
#163976 = CARTESIAN_POINT('Ctrl Pts',(-17.4105944079144,-14.5402982507086,
115.804098097223)) ;
#163977 = CARTESIAN_POINT('Ctrl Pts',(-17.3367905637937,-14.5402982498811,
115.828329136774)) ;
#163978 = CARTESIAN_POINT('Ctrl Pts',(-17.3429501969861,-14.467003448986,
115.847090385579)) ;
#163979 = CARTESIAN_POINT('Ctrl Pts',(-17.2698268935793,-14.3526296857438,
115.58886231961)) ;
#163980 = CARTESIAN_POINT('Ctrl Pts',(-17.281836401589,-14.2872135873285,
115.625441343297)) ;
#163981 = CARTESIAN_POINT('Ctrl Pts',(-17.3556402447308,-14.2872135872054,
115.601210300764)) ;
#163982 = CARTESIAN_POINT('Ctrl Pts',(-17.4294440878725,-14.2872135870823,
115.57697925823)) ;
#163983 = CARTESIAN_POINT('Ctrl Pts',(-17.4174345798628,-14.3526296854977,
115.540400234544)) ;
#163984 = CARTESIAN_POINT('Ctrl Pts',(-17.4054250718531,-14.418045783913,
115.503821210857)) ;
#163985 = CARTESIAN_POINT('Ctrl Pts',(-17.3316212287113,-14.4180457840361,
115.528052253391)) ;
#163986 = CARTESIAN_POINT('Ctrl Pts',(-17.2578173855695,-14.4180457841592,
115.552283295924)) ;
#163987 = CARTESIAN_POINT('Ctrl Pts',(-17.2698268935793,-14.3526296857438,
115.58886231961)) ;
#163988 = CARTESIAN_POINT('Ctrl Pts',(-17.209359096455,-14.1719531187117,
115.369308707155)) ;
#163989 = CARTESIAN_POINT('Ctrl Pts',(-17.2263404094475,-14.1190573784708,
115.421031046702)) ;
#163990 = CARTESIAN_POINT('Ctrl Pts',(-17.3001442516719,-14.1190573751839,
115.396800001374)) ;
#163991 = CARTESIAN_POINT('Ctrl Pts',(-17.3739480938962,-14.119057371897,
115.372568956047)) ;
#163992 = CARTESIAN_POINT('Ctrl Pts',(-17.3569667809037,-14.1719531121379,
115.3208466165)) ;
#163993 = CARTESIAN_POINT('Ctrl Pts',(-17.3399854679112,-14.2248488523788,
115.269124276952)) ;
#163994 = CARTESIAN_POINT('Ctrl Pts',(-17.2661816256868,-14.2248488556657,
115.29335532228)) ;
#163995 = CARTESIAN_POINT('Ctrl Pts',(-17.1923777834625,-14.2248488589527,
115.317586367608)) ;
#163996 = CARTESIAN_POINT('Ctrl Pts',(-17.209359096455,-14.1719531187117,
115.369308707155)) ;
#163997 = CARTESIAN_POINT('Ctrl Pts',(-17.1661919090706,-13.936583984801,
115.202313468294)) ;
#163998 = CARTESIAN_POINT('Ctrl Pts',(-17.1869470728886,-13.9000456634002,
115.265530348668)) ;
#163999 = CARTESIAN_POINT('Ctrl Pts',(-17.2607509144556,-13.9000456537943,
115.241299301338)) ;
#164000 = CARTESIAN_POINT('Ctrl Pts',(-17.3345547560226,-13.9000456441885,
115.217068254008)) ;
#164001 = CARTESIAN_POINT('Ctrl Pts',(-17.3137995922046,-13.9365839655893,
115.153851373634)) ;
#164002 = CARTESIAN_POINT('Ctrl Pts',(-17.2930444283865,-13.9731222869902,
115.09063449326)) ;
#164003 = CARTESIAN_POINT('Ctrl Pts',(-17.2192405868196,-13.973122296596,
115.11486554059)) ;
#164004 = CARTESIAN_POINT('Ctrl Pts',(-17.1454367452526,-13.9731223062019,
115.13909658792)) ;
#164005 = CARTESIAN_POINT('Ctrl Pts',(-17.1661919090706,-13.936583984801,
115.202313468294)) ;
#164006 = CARTESIAN_POINT('Ctrl Pts',(-17.1445055243567,-13.6642946874373,
115.100795313256)) ;
#164007 = CARTESIAN_POINT('Ctrl Pts',(-17.1675389258918,-13.6467154172206,
115.170951338261)) ;
#164008 = CARTESIAN_POINT('Ctrl Pts',(-17.2413427678139,-13.646715399489,
115.146720292013)) ;
#164009 = CARTESIAN_POINT('Ctrl Pts',(-17.315146609736,-13.6467153817574,
115.122489245764)) ;
#164010 = CARTESIAN_POINT('Ctrl Pts',(-17.2921132082009,-13.664294651974,
115.052333220759)) ;
#164011 = CARTESIAN_POINT('Ctrl Pts',(-17.2690798066658,-13.6818739221906,
114.982177195754)) ;
#164012 = CARTESIAN_POINT('Ctrl Pts',(-17.1952759647437,-13.6818739399222,
115.006408242002)) ;
#164013 = CARTESIAN_POINT('Ctrl Pts',(-17.1214721228216,-13.6818739576539,
115.030639288251)) ;
#164014 = CARTESIAN_POINT('Ctrl Pts',(-17.1445055243567,-13.6642946874373,
115.100795313256)) ;
#164015 = CARTESIAN_POINT('Ctrl Pts',(-17.1464540999734,-13.3747428455626,
115.07130654278)) ;
#164016 = CARTESIAN_POINT('Ctrl Pts',(-17.1701178080888,-13.377355159395,
115.143382380073)) ;
#164017 = CARTESIAN_POINT('Ctrl Pts',(-17.2439216515979,-13.3773551335995,
115.119151338658)) ;
#164018 = CARTESIAN_POINT('Ctrl Pts',(-17.3177254951069,-13.3773551078041,
115.094920297244)) ;
#164019 = CARTESIAN_POINT('Ctrl Pts',(-17.2940617869915,-13.3747427939718,
115.022844459951)) ;
#164020 = CARTESIAN_POINT('Ctrl Pts',(-17.270398078876,-13.3721304801394,
114.950768622658)) ;
#164021 = CARTESIAN_POINT('Ctrl Pts',(-17.196594235367,-13.3721305059348,
114.974999664072)) ;
#164022 = CARTESIAN_POINT('Ctrl Pts',(-17.1227903918579,-13.3721305317302,
114.999230705487)) ;
#164023 = CARTESIAN_POINT('Ctrl Pts',(-17.1464540999734,-13.3747428455626,
115.07130654278)) ;
#164024 = CARTESIAN_POINT('Ctrl Pts',(-17.1727178775642,-13.0876482903165,
115.115799669676)) ;
#164025 = CARTESIAN_POINT('Ctrl Pts',(-17.1953167302795,-13.1103096275797,
115.184632129402)) ;
#164026 = CARTESIAN_POINT('Ctrl Pts',(-17.26912057672,-13.1103095944857,115.160401096916)) ;
#164027 = CARTESIAN_POINT('Ctrl Pts',(-17.3429244231604,-13.1103095613917,
115.136170064429)) ;
#164028 = CARTESIAN_POINT('Ctrl Pts',(-17.320325570445,-13.0876482241285,
115.067337604704)) ;
#164029 = CARTESIAN_POINT('Ctrl Pts',(-17.2977267177297,-13.0649868868653,
114.998505144978)) ;
#164030 = CARTESIAN_POINT('Ctrl Pts',(-17.2239228712894,-13.0649869199593,
115.022736177464)) ;
#164031 = CARTESIAN_POINT('Ctrl Pts',(-17.150119024849,-13.0649869530533,
115.04696720995)) ;
#164032 = CARTESIAN_POINT('Ctrl Pts',(-17.1727178775642,-13.0876482903165,
115.115799669676)) ;
#164033 = CARTESIAN_POINT('Ctrl Pts',(-17.2222028953257,-12.8243385253649,
115.231028671208)) ;
#164034 = CARTESIAN_POINT('Ctrl Pts',(-17.242113859428,-12.8654169528501,
115.291674256081)) ;
#164035 = CARTESIAN_POINT('Ctrl Pts',(-17.3159177100322,-12.8654169160371,
115.267443236277)) ;
#164036 = CARTESIAN_POINT('Ctrl Pts',(-17.3897215606363,-12.8654168792241,
115.243212216473)) ;
#164037 = CARTESIAN_POINT('Ctrl Pts',(-17.369810596534,-12.824338451739,115.1825666316)) ;
#164038 = CARTESIAN_POINT('Ctrl Pts',(-17.3498996324317,-12.7832600242539,
115.121921046727)) ;
#164039 = CARTESIAN_POINT('Ctrl Pts',(-17.2760957818276,-12.7832600610668,
115.146152066531)) ;
#164040 = CARTESIAN_POINT('Ctrl Pts',(-17.2022919312234,-12.7832600978798,
115.170383086335)) ;
#164041 = CARTESIAN_POINT('Ctrl Pts',(-17.2222028953257,-12.8243385253649,
115.231028671208)) ;
#164042 = CARTESIAN_POINT('Ctrl Pts',(-17.2919810291401,-12.6038922563675,
115.408113946603)) ;
#164043 = CARTESIAN_POINT('Ctrl Pts',(-17.3077823918333,-12.6604213844926,
115.456242348831)) ;
#164044 = CARTESIAN_POINT('Ctrl Pts',(-17.3815862472237,-12.6604213494665,
115.432011343605)) ;
#164045 = CARTESIAN_POINT('Ctrl Pts',(-17.4553901026141,-12.6604213144404,
115.407780338379)) ;
#164046 = CARTESIAN_POINT('Ctrl Pts',(-17.4395887399208,-12.6038921863153,
115.359651936151)) ;
#164047 = CARTESIAN_POINT('Ctrl Pts',(-17.4237873772276,-12.5473630581902,
115.311523533924)) ;
#164048 = CARTESIAN_POINT('Ctrl Pts',(-17.3499835218372,-12.5473630932163,
115.33575453915)) ;
#164049 = CARTESIAN_POINT('Ctrl Pts',(-17.2761796664468,-12.5473631282424,
115.359985544376)) ;
#164050 = CARTESIAN_POINT('Ctrl Pts',(-17.2919810291401,-12.6038922563675,
115.408113946603)) ;
#164051 = CARTESIAN_POINT('Ctrl Pts',(-17.3779184788419,-12.4415502102937,
115.634396370926)) ;
#164052 = CARTESIAN_POINT('Ctrl Pts',(-17.3884766007028,-12.5094955214015,
115.666554707739)) ;
#164053 = CARTESIAN_POINT('Ctrl Pts',(-17.4622804609849,-12.5094954939584,
115.642323717413)) ;
#164054 = CARTESIAN_POINT('Ctrl Pts',(-17.5360843212669,-12.5094954665153,
115.618092727086)) ;
#164055 = CARTESIAN_POINT('Ctrl Pts',(-17.5255261994061,-12.4415501554076,
115.585934390273)) ;
#164056 = CARTESIAN_POINT('Ctrl Pts',(-17.5149680775452,-12.3736048442999,
115.553776053459)) ;
#164057 = CARTESIAN_POINT('Ctrl Pts',(-17.4411642172631,-12.3736048717429,
115.578007043786)) ;
#164058 = CARTESIAN_POINT('Ctrl Pts',(-17.3673603569811,-12.373604899186,
115.602238034113)) ;
#164059 = CARTESIAN_POINT('Ctrl Pts',(-17.3779184788419,-12.4415502102937,
115.634396370926)) ;
#164060 = CARTESIAN_POINT('Ctrl Pts',(-17.4746658472938,-12.3493107874977,
115.89357675197)) ;
#164061 = CARTESIAN_POINT('Ctrl Pts',(-17.4792190454332,-12.4237944597024,
115.907445060184)) ;
#164062 = CARTESIAN_POINT('Ctrl Pts',(-17.5530229099982,-12.4237944461757,
115.883214082902)) ;
#164063 = CARTESIAN_POINT('Ctrl Pts',(-17.6268267745631,-12.4237944326489,
115.85898310562)) ;
#164064 = CARTESIAN_POINT('Ctrl Pts',(-17.6222735764238,-12.3493107604442,
115.845114797407)) ;
#164065 = CARTESIAN_POINT('Ctrl Pts',(-17.6177203782844,-12.2748270882395,
115.831246489193)) ;
#164066 = CARTESIAN_POINT('Ctrl Pts',(-17.5439165137194,-12.2748271017662,
115.855477466475)) ;
#164067 = CARTESIAN_POINT('Ctrl Pts',(-17.4701126491544,-12.274827115293,
115.879708443756)) ;
#164068 = CARTESIAN_POINT('Ctrl Pts',(-17.4746658472938,-12.3493107874977,
115.89357675197)) ;
#164069 = CARTESIAN_POINT('Ctrl Pts',(-17.5755185168944,-12.3333698024851,
116.165420915511)) ;
#164070 = CARTESIAN_POINT('Ctrl Pts',(-17.5737682061993,-12.409073916813,
116.160089753013)) ;
#164071 = CARTESIAN_POINT('Ctrl Pts',(-17.6475720732458,-12.409073922124,
116.135858783289)) ;
#164072 = CARTESIAN_POINT('Ctrl Pts',(-17.7213759402922,-12.4090739274351,
116.111627813566)) ;
#164073 = CARTESIAN_POINT('Ctrl Pts',(-17.7231262509873,-12.3333698131071,
116.116958976064)) ;
#164074 = CARTESIAN_POINT('Ctrl Pts',(-17.7248765616823,-12.2576656987791,
116.122290138562)) ;
#164075 = CARTESIAN_POINT('Ctrl Pts',(-17.6510726946359,-12.2576656934681,
116.146521108286)) ;
#164076 = CARTESIAN_POINT('Ctrl Pts',(-17.5772688275895,-12.2576656881571,
116.170752078009)) ;
#164077 = CARTESIAN_POINT('Ctrl Pts',(-17.5755185168944,-12.3333698024851,
116.165420915511)) ;
#164078 = CARTESIAN_POINT('Ctrl Pts',(-17.6754893328123,-12.3958418590805,
116.434192181454)) ;
#164079 = CARTESIAN_POINT('Ctrl Pts',(-17.6674960258275,-12.4672950791635,
116.40984585974)) ;
#164080 = CARTESIAN_POINT('Ctrl Pts',(-17.7412998942639,-12.467295107772,
116.38561489425)) ;
#164081 = CARTESIAN_POINT('Ctrl Pts',(-17.8151037627004,-12.4672951363806,
116.361383928761)) ;
#164082 = CARTESIAN_POINT('Ctrl Pts',(-17.8230970696853,-12.3958419162977,
116.385730250475)) ;
#164083 = CARTESIAN_POINT('Ctrl Pts',(-17.8310903766701,-12.3243886962147,
116.410076572189)) ;
#164084 = CARTESIAN_POINT('Ctrl Pts',(-17.7572865082336,-12.3243886676062,
116.434307537679)) ;
#164085 = CARTESIAN_POINT('Ctrl Pts',(-17.6834826397972,-12.3243886389976,
116.458538503168)) ;
#164086 = CARTESIAN_POINT('Ctrl Pts',(-17.6754893328123,-12.3958418590805,
116.434192181454)) ;
#164087 = CARTESIAN_POINT('Ctrl Pts',(-17.7659177540856,-12.5305465195612,
116.674353272671)) ;
#164088 = CARTESIAN_POINT('Ctrl Pts',(-17.7523292107677,-12.5926984144573,
116.632964763969)) ;
#164089 = CARTESIAN_POINT('Ctrl Pts',(-17.8261330771754,-12.592698466259,
116.6087337923)) ;
#164090 = CARTESIAN_POINT('Ctrl Pts',(-17.8999369435831,-12.5926985180608,
116.584502820631)) ;
#164091 = CARTESIAN_POINT('Ctrl Pts',(-17.913525486901,-12.5305466231647,
116.625891329333)) ;
#164092 = CARTESIAN_POINT('Ctrl Pts',(-17.9271140302189,-12.4683947282686,
116.667279838035)) ;
#164093 = CARTESIAN_POINT('Ctrl Pts',(-17.8533101638112,-12.4683946764668,
116.691510809704)) ;
#164094 = CARTESIAN_POINT('Ctrl Pts',(-17.7795062974035,-12.4683946246651,
116.715741781372)) ;
#164095 = CARTESIAN_POINT('Ctrl Pts',(-17.7659177540856,-12.5305465195612,
116.674353272671)) ;
#164096 = CARTESIAN_POINT('Ctrl Pts',(-17.8428696280429,-12.7291635452138,
116.873260297753)) ;
#164097 = CARTESIAN_POINT('Ctrl Pts',(-17.8246228394944,-12.7775393659294,
116.817683525794)) ;
#164098 = CARTESIAN_POINT('Ctrl Pts',(-17.8984267019353,-12.7775394398199,
116.793452542043)) ;
#164099 = CARTESIAN_POINT('Ctrl Pts',(-17.9722305643762,-12.7775395137104,
116.769221558292)) ;
#164100 = CARTESIAN_POINT('Ctrl Pts',(-17.9904773529247,-12.7291636929948,
116.824798330251)) ;
#164101 = CARTESIAN_POINT('Ctrl Pts',(-18.0087241414732,-12.6807878722793,
116.880375102209)) ;
#164102 = CARTESIAN_POINT('Ctrl Pts',(-17.9349202790323,-12.6807877983888,
116.90460608596)) ;
#164103 = CARTESIAN_POINT('Ctrl Pts',(-17.8611164165914,-12.6807877244983,
116.928837069711)) ;
#164104 = CARTESIAN_POINT('Ctrl Pts',(-17.8428696280429,-12.7291635452138,
116.873260297753)) ;
#164105 = CARTESIAN_POINT('Ctrl Pts',(-17.900952909542,-12.9771312925897,
117.014719731031)) ;
#164106 = CARTESIAN_POINT('Ctrl Pts',(-17.8793578779453,-13.0082656414961,
116.948944751075)) ;
#164107 = CARTESIAN_POINT('Ctrl Pts',(-17.9531617341492,-13.0082657332076,
116.924713748327)) ;
#164108 = CARTESIAN_POINT('Ctrl Pts',(-18.0269655903531,-13.008265824919,
116.900482745579)) ;
#164109 = CARTESIAN_POINT('Ctrl Pts',(-18.0485606219498,-12.9771314760126,
116.966257725535)) ;
#164110 = CARTESIAN_POINT('Ctrl Pts',(-18.0701556535464,-12.9459971271062,
117.032032705491)) ;
#164111 = CARTESIAN_POINT('Ctrl Pts',(-17.9963517973425,-12.9459970353947,
117.056263708239)) ;
#164112 = CARTESIAN_POINT('Ctrl Pts',(-17.9225479411386,-12.9459969436833,
117.080494710987)) ;
#164113 = CARTESIAN_POINT('Ctrl Pts',(-17.900952909542,-12.9771312925897,
117.014719731031)) ;
#164114 = CARTESIAN_POINT('Ctrl Pts',(-17.9368966294271,-13.2574946761857,
117.088639322891)) ;
#164115 = CARTESIAN_POINT('Ctrl Pts',(-17.9134961833614,-13.269101018714,
117.017365341841)) ;
#164116 = CARTESIAN_POINT('Ctrl Pts',(-17.9873000316532,-13.2691011219862,
116.993134314994)) ;
#164117 = CARTESIAN_POINT('Ctrl Pts',(-18.061103879945,-13.2691012252584,
116.968903288147)) ;
#164118 = CARTESIAN_POINT('Ctrl Pts',(-18.0845043260107,-13.2574948827302,
117.040177269197)) ;
#164119 = CARTESIAN_POINT('Ctrl Pts',(-18.1079047720765,-13.2458885402019,
117.111451250246)) ;
#164120 = CARTESIAN_POINT('Ctrl Pts',(-18.0341009237846,-13.2458884369297,
117.135682277093)) ;
#164121 = CARTESIAN_POINT('Ctrl Pts',(-17.9602970754928,-13.2458883336575,
117.15991330394)) ;
#164122 = CARTESIAN_POINT('Ctrl Pts',(-17.9368966294271,-13.2574946761857,
117.088639322891)) ;
#164123 = CARTESIAN_POINT('Ctrl Pts',(-17.9486369502931,-13.5486172877669,
117.088938884935)) ;
#164124 = CARTESIAN_POINT('Ctrl Pts',(-17.9251161316749,-13.5399156323179,
117.017298268559)) ;
#164125 = CARTESIAN_POINT('Ctrl Pts',(-17.9989199711168,-13.5399157383977,
116.993067214757)) ;
#164126 = CARTESIAN_POINT('Ctrl Pts',(-18.0727238105588,-13.5399158444775,
116.968836160955)) ;
#164127 = CARTESIAN_POINT('Ctrl Pts',(-18.096244629177,-13.5486174999264,
117.040476777331)) ;
#164128 = CARTESIAN_POINT('Ctrl Pts',(-18.1197654477952,-13.5573191553753,
117.112117393707)) ;
#164129 = CARTESIAN_POINT('Ctrl Pts',(-18.0459616083532,-13.5573190492956,
117.136348447509)) ;
#164130 = CARTESIAN_POINT('Ctrl Pts',(-17.9721577689113,-13.5573189432158,
117.160579501311)) ;
#164131 = CARTESIAN_POINT('Ctrl Pts',(-17.9486369502931,-13.5486172877669,
117.088938884935)) ;
#164132 = CARTESIAN_POINT('Ctrl Pts',(-17.9363162489277,-13.8299622964239,
117.016005420011)) ;
#164133 = CARTESIAN_POINT('Ctrl Pts',(-17.9143535893981,-13.8016053515907,
116.949110704836)) ;
#164134 = CARTESIAN_POINT('Ctrl Pts',(-17.9881574200438,-13.8016054516698,
116.924879624242)) ;
#164135 = CARTESIAN_POINT('Ctrl Pts',(-18.0619612506894,-13.8016055517489,
116.900648543647)) ;
#164136 = CARTESIAN_POINT('Ctrl Pts',(-18.0839239102189,-13.8299624965821,
116.967543258822)) ;
#164137 = CARTESIAN_POINT('Ctrl Pts',(-18.1058865697484,-13.8583194414153,
117.034437973997)) ;
#164138 = CARTESIAN_POINT('Ctrl Pts',(-18.0320827391028,-13.8583193413362,
117.058669054592)) ;
#164139 = CARTESIAN_POINT('Ctrl Pts',(-17.9582789084571,-13.8583192412571,
117.082900135186)) ;
#164140 = CARTESIAN_POINT('Ctrl Pts',(-17.9363162489277,-13.8299622964239,
117.016005420011)) ;
#164141 = CARTESIAN_POINT('Ctrl Pts',(-17.9015308192628,-14.082140489746,
116.874612226591)) ;
#164142 = CARTESIAN_POINT('Ctrl Pts',(-17.8826976264503,-14.0361354675862,
116.817249362104)) ;
#164143 = CARTESIAN_POINT('Ctrl Pts',(-17.9565014492006,-14.0361355534221,
116.793018257462)) ;
#164144 = CARTESIAN_POINT('Ctrl Pts',(-18.0303052719508,-14.0361356392581,
116.768787152819)) ;
#164145 = CARTESIAN_POINT('Ctrl Pts',(-18.0491384647633,-14.0821406614179,
116.826150017306)) ;
#164146 = CARTESIAN_POINT('Ctrl Pts',(-18.0679716575757,-14.1281456835778,
116.883512881793)) ;
#164147 = CARTESIAN_POINT('Ctrl Pts',(-17.9941678348255,-14.1281455977418,
116.907743986436)) ;
#164148 = CARTESIAN_POINT('Ctrl Pts',(-17.9203640120752,-14.1281455119059,
116.931975091078)) ;
#164149 = CARTESIAN_POINT('Ctrl Pts',(-17.9015308192628,-14.082140489746,
116.874612226591)) ;
#164150 = CARTESIAN_POINT('Ctrl Pts',(-17.8474297188587,-14.2871395255682,
116.67433526165)) ;
#164151 = CARTESIAN_POINT('Ctrl Pts',(-17.8330800933996,-14.2267539066878,
116.630628619884)) ;
#164152 = CARTESIAN_POINT('Ctrl Pts',(-17.906883909967,-14.2267539712464,
116.606397496409)) ;
#164153 = CARTESIAN_POINT('Ctrl Pts',(-17.9806877265344,-14.2267540358049,
116.582166372935)) ;
#164154 = CARTESIAN_POINT('Ctrl Pts',(-17.9950373519935,-14.2871396546853,
116.625873014701)) ;
#164155 = CARTESIAN_POINT('Ctrl Pts',(-18.0093869774526,-14.3475252735657,
116.669579656467)) ;
#164156 = CARTESIAN_POINT('Ctrl Pts',(-17.9355831608852,-14.3475252090071,
116.693810779941)) ;
#164157 = CARTESIAN_POINT('Ctrl Pts',(-17.8617793443178,-14.3475251444486,
116.718041903416)) ;
#164158 = CARTESIAN_POINT('Ctrl Pts',(-17.8474297188587,-14.2871395255682,
116.67433526165)) ;
#164159 = CARTESIAN_POINT('Ctrl Pts',(-17.7784858967829,-14.4298488440199,
116.428771121435)) ;
#164160 = CARTESIAN_POINT('Ctrl Pts',(-17.7696642881067,-14.3594095209829,
116.401901926801)) ;
#164161 = CARTESIAN_POINT('Ctrl Pts',(-17.8434681009777,-14.3594095593736,
116.377670792068)) ;
#164162 = CARTESIAN_POINT('Ctrl Pts',(-17.9172719138486,-14.3594095977643,
116.353439657335)) ;
#164163 = CARTESIAN_POINT('Ctrl Pts',(-17.9260935225248,-14.4298489208013,
116.380308851969)) ;
#164164 = CARTESIAN_POINT('Ctrl Pts',(-17.934915131201,-14.5002882438384,
116.407178046602)) ;
#164165 = CARTESIAN_POINT('Ctrl Pts',(-17.86111131833,-14.5002882054477,116.431409181336)) ;
#164166 = CARTESIAN_POINT('Ctrl Pts',(-17.7873075054591,-14.500288167057,
116.455640316069)) ;
#164167 = CARTESIAN_POINT('Ctrl Pts',(-17.7784858967829,-14.4298488440199,
116.428771121435)) ;
#164168 = CARTESIAN_POINT('Ctrl Pts',(-17.7011619828439,-14.4994383097765,
116.157945215762)) ;
#164169 = CARTESIAN_POINT('Ctrl Pts',(-17.6984564474787,-14.4240356160354,
116.149704593557)) ;
#164170 = CARTESIAN_POINT('Ctrl Pts',(-17.7722602590906,-14.4240356268717,
116.125473454989)) ;
#164171 = CARTESIAN_POINT('Ctrl Pts',(-17.8460640707025,-14.424035637708,
116.101242316421)) ;
#164172 = CARTESIAN_POINT('Ctrl Pts',(-17.8487696060677,-14.4994383314491,
116.109482938626)) ;
#164173 = CARTESIAN_POINT('Ctrl Pts',(-17.8514751414329,-14.5748410251902,
116.11772356083)) ;
#164174 = CARTESIAN_POINT('Ctrl Pts',(-17.777671329821,-14.5748410143539,
116.141954699398)) ;
#164175 = CARTESIAN_POINT('Ctrl Pts',(-17.7038675182091,-14.5748410035177,
116.166185837966)) ;
#164176 = CARTESIAN_POINT('Ctrl Pts',(-17.7011619828439,-14.4994383097765,
116.157945215762)) ;
#164177 = CARTESIAN_POINT('Ctrl Pts',(-17.6208255769599,-14.4922423916848,
115.877768836137)) ;
#164178 = CARTESIAN_POINT('Ctrl Pts',(-17.6244590729136,-14.4172290917828,
115.888835880451)) ;
#164179 = CARTESIAN_POINT('Ctrl Pts',(-17.6982628860497,-14.4172290756449,
115.864604746526)) ;
#164180 = CARTESIAN_POINT('Ctrl Pts',(-17.7720666991857,-14.417229059507,
115.8403736126)) ;
#164181 = CARTESIAN_POINT('Ctrl Pts',(-17.768433203232,-14.492242359409,115.829306568286)) ;
#164182 = CARTESIAN_POINT('Ctrl Pts',(-17.7647997072783,-14.567255659311,
115.818239523972)) ;
#164183 = CARTESIAN_POINT('Ctrl Pts',(-17.6909958941422,-14.5672556754489,
115.842470657898)) ;
#164184 = CARTESIAN_POINT('Ctrl Pts',(-17.6171920810061,-14.5672556915868,
115.866701791824)) ;
#164185 = CARTESIAN_POINT('Ctrl Pts',(-17.6208255769599,-14.4922423916848,
115.877768836137)) ;
#164186 = CARTESIAN_POINT('Ctrl Pts',(-17.5442238721124,-14.4074859363464,
115.60889672167)) ;
#164187 = CARTESIAN_POINT('Ctrl Pts',(-17.5539467158505,-14.3382771247353,
115.638510936711)) ;
#164188 = CARTESIAN_POINT('Ctrl Pts',(-17.6277505330549,-14.3382770857767,
115.614279815176)) ;
#164189 = CARTESIAN_POINT('Ctrl Pts',(-17.7015543502592,-14.3382770468181,
115.590048693642)) ;
#164190 = CARTESIAN_POINT('Ctrl Pts',(-17.6918315065211,-14.4074858584293,
115.560434478601)) ;
#164191 = CARTESIAN_POINT('Ctrl Pts',(-17.6821086627829,-14.4766946700404,
115.53082026356)) ;
#164192 = CARTESIAN_POINT('Ctrl Pts',(-17.6083048455786,-14.476694708999,
115.555051385095)) ;
#164193 = CARTESIAN_POINT('Ctrl Pts',(-17.5345010283743,-14.4766947479576,
115.579282506629)) ;
#164194 = CARTESIAN_POINT('Ctrl Pts',(-17.5442238721124,-14.4074859363464,
115.60889672167)) ;
#164195 = CARTESIAN_POINT('Ctrl Pts',(-17.4781148630412,-14.2527213410347,
115.372193987303)) ;
#164196 = CARTESIAN_POINT('Ctrl Pts',(-17.4931993104765,-14.1942140636659,
115.418138782012)) ;
#164197 = CARTESIAN_POINT('Ctrl Pts',(-17.5670031331039,-14.1942140071928,
115.393907676996)) ;
#164198 = CARTESIAN_POINT('Ctrl Pts',(-17.6408069557314,-14.1942139507198,
115.369676571979)) ;
#164199 = CARTESIAN_POINT('Ctrl Pts',(-17.6257225082961,-14.2527212280886,
115.32373177727)) ;
#164200 = CARTESIAN_POINT('Ctrl Pts',(-17.6106380608608,-14.3112285054574,
115.27778698256)) ;
#164201 = CARTESIAN_POINT('Ctrl Pts',(-17.5368342382334,-14.3112285619304,
115.302018087577)) ;
#164202 = CARTESIAN_POINT('Ctrl Pts',(-17.4630304156059,-14.3112286184035,
115.326249192593)) ;
#164203 = CARTESIAN_POINT('Ctrl Pts',(-17.4781148630412,-14.2527213410347,
115.372193987303)) ;
#164204 = CARTESIAN_POINT('Ctrl Pts',(-17.4272659714627,-14.0372448891262,
115.181771156024)) ;
#164205 = CARTESIAN_POINT('Ctrl Pts',(-17.4466589469468,-13.9936933807782,
115.240839031848)) ;
#164206 = CARTESIAN_POINT('Ctrl Pts',(-17.5204627763427,-13.993693314701,
115.216607947447)) ;
#164207 = CARTESIAN_POINT('Ctrl Pts',(-17.5942666057386,-13.9936932486239,
115.192376863046)) ;
#164208 = CARTESIAN_POINT('Ctrl Pts',(-17.5748736302544,-14.0372447569719,
115.133308987222)) ;
#164209 = CARTESIAN_POINT('Ctrl Pts',(-17.5554806547702,-14.08079626532,115.074241111398)) ;
#164210 = CARTESIAN_POINT('Ctrl Pts',(-17.4816768253743,-14.0807963313971,
115.098472195799)) ;
#164211 = CARTESIAN_POINT('Ctrl Pts',(-17.4078729959785,-14.0807963974743,
115.1227032802)) ;
#164212 = CARTESIAN_POINT('Ctrl Pts',(-17.4272659714627,-14.0372448891262,
115.181771156024)) ;
#164213 = CARTESIAN_POINT('Ctrl Pts',(-17.3965606435217,-13.7782273369584,
115.052841406963)) ;
#164214 = CARTESIAN_POINT('Ctrl Pts',(-17.4188593760479,-13.7526945200312,
115.120759749758)) ;
#164215 = CARTESIAN_POINT('Ctrl Pts',(-17.4926632121621,-13.75269445107,115.09652868582)) ;
#164216 = CARTESIAN_POINT('Ctrl Pts',(-17.5664670482762,-13.7526943821088,
115.072297621882)) ;
#164217 = CARTESIAN_POINT('Ctrl Pts',(-17.5441683157501,-13.778227199036,
115.004379279087)) ;
#164218 = CARTESIAN_POINT('Ctrl Pts',(-17.5218695832239,-13.8037600159632,
114.936460936292)) ;
#164219 = CARTESIAN_POINT('Ctrl Pts',(-17.4480657471097,-13.8037600849244,
114.96069200023)) ;
#164220 = CARTESIAN_POINT('Ctrl Pts',(-17.3742619109955,-13.8037601538856,
114.984923064168)) ;
#164221 = CARTESIAN_POINT('Ctrl Pts',(-17.3965606435217,-13.7782273369584,
115.052841406963)) ;
#164222 = CARTESIAN_POINT('Ctrl Pts',(-17.3887643996198,-13.4921296981973,
114.993517684583)) ;
#164223 = CARTESIAN_POINT('Ctrl Pts',(-17.4123775387182,-13.4865334475081,
115.065439497541)) ;
#164224 = CARTESIAN_POINT('Ctrl Pts',(-17.4861813810062,-13.4865333838988,
115.041208452408)) ;
#164225 = CARTESIAN_POINT('Ctrl Pts',(-17.5599852232941,-13.4865333202894,
115.016977407274)) ;
#164226 = CARTESIAN_POINT('Ctrl Pts',(-17.5363720841956,-13.4921295709785,
114.945055594315)) ;
#164227 = CARTESIAN_POINT('Ctrl Pts',(-17.5127589450972,-13.4977258216677,
114.873133781356)) ;
#164228 = CARTESIAN_POINT('Ctrl Pts',(-17.4389551028092,-13.497725885277,
114.89736482649)) ;
#164229 = CARTESIAN_POINT('Ctrl Pts',(-17.3651512605213,-13.4977259488864,
114.921595871624)) ;
#164230 = CARTESIAN_POINT('Ctrl Pts',(-17.3887643996198,-13.4921296981973,
114.993517684583)) ;
#164231 = CARTESIAN_POINT('Ctrl Pts',(-17.4051724491236,-13.2025980491625,
115.008157982313)) ;
#164232 = CARTESIAN_POINT('Ctrl Pts',(-17.4284068472422,-13.2172086619386,
115.078926211216)) ;
#164233 = CARTESIAN_POINT('Ctrl Pts',(-17.5022106943674,-13.2172086067816,
115.054695180816)) ;
#164234 = CARTESIAN_POINT('Ctrl Pts',(-17.5760145414926,-13.2172085516246,
115.030464150416)) ;
#164235 = CARTESIAN_POINT('Ctrl Pts',(-17.552780143374,-13.2025979388484,
114.959695921512)) ;
#164236 = CARTESIAN_POINT('Ctrl Pts',(-17.5295457452554,-13.1879873260723,
114.888927692608)) ;
#164237 = CARTESIAN_POINT('Ctrl Pts',(-17.4557418981302,-13.1879873812294,
114.913158723009)) ;
#164238 = CARTESIAN_POINT('Ctrl Pts',(-17.3819380510049,-13.1879874363864,
114.937389753409)) ;
#164239 = CARTESIAN_POINT('Ctrl Pts',(-17.4051724491236,-13.2025980491625,
115.008157982313)) ;
#164240 = CARTESIAN_POINT('Ctrl Pts',(-17.4455328120095,-12.9267373644591,
115.095528220572)) ;
#164241 = CARTESIAN_POINT('Ctrl Pts',(-17.4667203967007,-12.960631185249,
115.160062185842)) ;
#164242 = CARTESIAN_POINT('Ctrl Pts',(-17.5405242469435,-12.9606311438607,
115.135831164937)) ;
#164243 = CARTESIAN_POINT('Ctrl Pts',(-17.6143280971863,-12.9606311024724,
115.111600144033)) ;
#164244 = CARTESIAN_POINT('Ctrl Pts',(-17.5931405124951,-12.9267372816824,
115.047066178763)) ;
#164245 = CARTESIAN_POINT('Ctrl Pts',(-17.5719529278039,-12.8928434608925,
114.982532213493)) ;
#164246 = CARTESIAN_POINT('Ctrl Pts',(-17.4981490775612,-12.8928435022808,
115.006763234398)) ;
#164247 = CARTESIAN_POINT('Ctrl Pts',(-17.4243452273184,-12.8928435436691,
115.030994255302)) ;
#164248 = CARTESIAN_POINT('Ctrl Pts',(-17.4455328120095,-12.9267373644591,
115.095528220572)) ;
#164249 = CARTESIAN_POINT('Ctrl Pts',(-17.5074914960105,-12.6871394629104,
115.248815418354)) ;
#164250 = CARTESIAN_POINT('Ctrl Pts',(-17.5251182336107,-12.7378139602179,
115.302503617764)) ;
#164251 = CARTESIAN_POINT('Ctrl Pts',(-17.5989220852435,-12.7378139322017,
115.278272601093)) ;
#164252 = CARTESIAN_POINT('Ctrl Pts',(-17.6727259368762,-12.7378139041855,
115.254041584421)) ;
#164253 = CARTESIAN_POINT('Ctrl Pts',(-17.655099199276,-12.687139406878,115.200353385011)) ;
#164254 = CARTESIAN_POINT('Ctrl Pts',(-17.6374724616758,-12.6364649095704,
115.146665185601)) ;
#164255 = CARTESIAN_POINT('Ctrl Pts',(-17.5636686100431,-12.6364649375867,
115.170896202273)) ;
#164256 = CARTESIAN_POINT('Ctrl Pts',(-17.4898647584103,-12.6364649656029,
115.195127218944)) ;
#164257 = CARTESIAN_POINT('Ctrl Pts',(-17.5074914960105,-12.6871394629104,
115.248815418354)) ;
#164258 = CARTESIAN_POINT('Ctrl Pts',(-17.5873854112055,-12.4995507390681,
115.456720343984)) ;
#164259 = CARTESIAN_POINT('Ctrl Pts',(-17.6001938103164,-12.5633999915825,
115.495732661631)) ;
#164260 = CARTESIAN_POINT('Ctrl Pts',(-17.6739976618083,-12.5633999761432,
115.471501644531)) ;
#164261 = CARTESIAN_POINT('Ctrl Pts',(-17.7478015133002,-12.5633999607039,
115.447270627431)) ;
#164262 = CARTESIAN_POINT('Ctrl Pts',(-17.7349931141894,-12.4995507081895,
115.408258309784)) ;
#164263 = CARTESIAN_POINT('Ctrl Pts',(-17.7221847150785,-12.4357014556752,
115.369245992137)) ;
#164264 = CARTESIAN_POINT('Ctrl Pts',(-17.6483808635866,-12.4357014711144,
115.393477009237)) ;
#164265 = CARTESIAN_POINT('Ctrl Pts',(-17.5745770120946,-12.4357014865537,
115.417708026337)) ;
#164266 = CARTESIAN_POINT('Ctrl Pts',(-17.5873854112055,-12.4995507390681,
115.456720343984)) ;
#164267 = CARTESIAN_POINT('Ctrl Pts',(-17.6808646336861,-12.3773999719713,
115.705811950101)) ;
#164268 = CARTESIAN_POINT('Ctrl Pts',(-17.6879027033359,-12.4498755259628,
115.727248775064)) ;
#164269 = CARTESIAN_POINT('Ctrl Pts',(-17.7617065529551,-12.4498755206207,
115.70301775226)) ;
#164270 = CARTESIAN_POINT('Ctrl Pts',(-17.8355104025744,-12.4498755152786,
115.678786729456)) ;
#164271 = CARTESIAN_POINT('Ctrl Pts',(-17.8284723329247,-12.377399961287,
115.657349904494)) ;
#164272 = CARTESIAN_POINT('Ctrl Pts',(-17.8214342632749,-12.3049244072955,
115.635913079531)) ;
#164273 = CARTESIAN_POINT('Ctrl Pts',(-17.7476304136556,-12.3049244126376,
115.660144102334)) ;
#164274 = CARTESIAN_POINT('Ctrl Pts',(-17.6738265640363,-12.3049244179797,
115.684375125138)) ;
#164275 = CARTESIAN_POINT('Ctrl Pts',(-17.6808646336861,-12.3773999719713,
115.705811950101)) ;
#164276 = CARTESIAN_POINT('Ctrl Pts',(-17.780520996489,-12.3305982965088,
115.974059722386)) ;
#164277 = CARTESIAN_POINT('Ctrl Pts',(-17.7813415036169,-12.4064507655152,
115.976558854994)) ;
#164278 = CARTESIAN_POINT('Ctrl Pts',(-17.8551453516194,-12.4064507656023,
115.952327827266)) ;
#164279 = CARTESIAN_POINT('Ctrl Pts',(-17.9289491996219,-12.4064507656893,
115.928096799537)) ;
#164280 = CARTESIAN_POINT('Ctrl Pts',(-17.928128692494,-12.3305982966829,
115.92559766693)) ;
#164281 = CARTESIAN_POINT('Ctrl Pts',(-17.9273081853662,-12.2547458276765,
115.923098534322)) ;
#164282 = CARTESIAN_POINT('Ctrl Pts',(-17.8535043373637,-12.2547458275895,
115.94732956205)) ;
#164283 = CARTESIAN_POINT('Ctrl Pts',(-17.7797004893612,-12.2547458275024,
115.971560589778)) ;
#164284 = CARTESIAN_POINT('Ctrl Pts',(-17.780520996489,-12.3305982965088,
115.974059722386)) ;
#164285 = CARTESIAN_POINT('Ctrl Pts',(-17.8813348577661,-12.3609522062499,
116.245667417945)) ;
#164286 = CARTESIAN_POINT('Ctrl Pts',(-17.8758509588025,-12.4347996190351,
116.228964346684)) ;
#164287 = CARTESIAN_POINT('Ctrl Pts',(-17.9496548046379,-12.4347996215548,
116.204733312355)) ;
#164288 = CARTESIAN_POINT('Ctrl Pts',(-18.0234586504734,-12.4347996240744,
116.180502278026)) ;
#164289 = CARTESIAN_POINT('Ctrl Pts',(-18.028942549437,-12.3609522112891,
116.197205349288)) ;
#164290 = CARTESIAN_POINT('Ctrl Pts',(-18.0344264484005,-12.2871047985038,
116.21390842055)) ;
#164291 = CARTESIAN_POINT('Ctrl Pts',(-17.9606226025651,-12.2871047959842,
116.238139454878)) ;
#164292 = CARTESIAN_POINT('Ctrl Pts',(-17.8868187567297,-12.2871047934646,
116.262370489207)) ;
#164293 = CARTESIAN_POINT('Ctrl Pts',(-17.8813348577661,-12.3609522062499,
116.245667417945)) ;
#164294 = CARTESIAN_POINT('Ctrl Pts',(-17.9766684026926,-12.4676416333475,
116.500474417848)) ;
#164295 = CARTESIAN_POINT('Ctrl Pts',(-17.9652553121859,-12.5341505224267,
116.465711985703)) ;
#164296 = CARTESIAN_POINT('Ctrl Pts',(-18.0390591561462,-12.5341505238971,
116.441480945663)) ;
#164297 = CARTESIAN_POINT('Ctrl Pts',(-18.1128630001066,-12.5341505253675,
116.417249905623)) ;
#164298 = CARTESIAN_POINT('Ctrl Pts',(-18.1242760906133,-12.4676416362883,
116.452012337768)) ;
#164299 = CARTESIAN_POINT('Ctrl Pts',(-18.1356891811201,-12.4011327472091,
116.486774769912)) ;
#164300 = CARTESIAN_POINT('Ctrl Pts',(-18.0618853371597,-12.4011327457387,
116.511005809952)) ;
#164301 = CARTESIAN_POINT('Ctrl Pts',(-17.9880814931994,-12.4011327442682,
116.535236849992)) ;
#164302 = CARTESIAN_POINT('Ctrl Pts',(-17.9766684026926,-12.4676416333475,
116.500474417848)) ;
#164303 = CARTESIAN_POINT('Ctrl Pts',(-18.0597927746856,-12.6420295507419,
116.718229948439)) ;
#164304 = CARTESIAN_POINT('Ctrl Pts',(-18.0432914214384,-12.6964607838734,
116.667969488908)) ;
#164305 = CARTESIAN_POINT('Ctrl Pts',(-18.1170952645228,-12.6964607831673,
116.6437384462)) ;
#164306 = CARTESIAN_POINT('Ctrl Pts',(-18.1908991076072,-12.6964607824612,
116.619507403492)) ;
#164307 = CARTESIAN_POINT('Ctrl Pts',(-18.2074004608543,-12.6420295493297,
116.669767863023)) ;
#164308 = CARTESIAN_POINT('Ctrl Pts',(-18.2239018141015,-12.5875983161982,
116.720028322554)) ;
#164309 = CARTESIAN_POINT('Ctrl Pts',(-18.1500979710171,-12.5875983169043,
116.744259365262)) ;
#164310 = CARTESIAN_POINT('Ctrl Pts',(-18.0762941279327,-12.5875983176104,
116.76849040797)) ;
#164311 = CARTESIAN_POINT('Ctrl Pts',(-18.0597927746856,-12.6420295507419,
116.718229948439)) ;
#164312 = CARTESIAN_POINT('Ctrl Pts',(-18.1258671840581,-12.8715204701867,
116.884091854367)) ;
#164313 = CARTESIAN_POINT('Ctrl Pts',(-18.1054598564483,-12.9100077875802,
116.821934427118)) ;
#164314 = CARTESIAN_POINT('Ctrl Pts',(-18.1792636993406,-12.9100077849432,
116.797703383825)) ;
#164315 = CARTESIAN_POINT('Ctrl Pts',(-18.253067542233,-12.9100077823063,
116.773472340532)) ;
#164316 = CARTESIAN_POINT('Ctrl Pts',(-18.2734748698428,-12.8715204649127,
116.835629767782)) ;
#164317 = CARTESIAN_POINT('Ctrl Pts',(-18.2938821974526,-12.8330331475192,
116.897787195031)) ;
#164318 = CARTESIAN_POINT('Ctrl Pts',(-18.2200783545602,-12.8330331501562,
116.922018238324)) ;
#164319 = CARTESIAN_POINT('Ctrl Pts',(-18.1462745116679,-12.8330331527932,
116.946249281617)) ;
#164320 = CARTESIAN_POINT('Ctrl Pts',(-18.1258671840581,-12.8715204701867,
116.884091854367)) ;
#164321 = CARTESIAN_POINT('Ctrl Pts',(-18.1711371153448,-13.1406452081899,
116.986504143615)) ;
#164322 = CARTESIAN_POINT('Ctrl Pts',(-18.1482724742896,-13.1603966221908,
116.916862136095)) ;
#164323 = CARTESIAN_POINT('Ctrl Pts',(-18.2220763174873,-13.1603966190533,
116.892631093732)) ;
#164324 = CARTESIAN_POINT('Ctrl Pts',(-18.295880160685,-13.1603966159158,
116.868400051369)) ;
#164325 = CARTESIAN_POINT('Ctrl Pts',(-18.3187448017401,-13.1406452019148,
116.938042058889)) ;
#164326 = CARTESIAN_POINT('Ctrl Pts',(-18.3416094427953,-13.1208937879139,
117.007684066409)) ;
#164327 = CARTESIAN_POINT('Ctrl Pts',(-18.2678055995976,-13.1208937910514,
117.031915108772)) ;
#164328 = CARTESIAN_POINT('Ctrl Pts',(-18.1940017564,-13.1208937941889,117.056146151135)) ;
#164329 = CARTESIAN_POINT('Ctrl Pts',(-18.1711371153448,-13.1406452081899,
116.986504143615)) ;
#164330 = CARTESIAN_POINT('Ctrl Pts',(-18.1928638298168,-13.4310927688211,
117.017038288082)) ;
#164331 = CARTESIAN_POINT('Ctrl Pts',(-18.1691858546894,-13.4305915609801,
116.944918996267)) ;
#164332 = CARTESIAN_POINT('Ctrl Pts',(-18.2429896982003,-13.4305915607747,
116.920687954858)) ;
#164333 = CARTESIAN_POINT('Ctrl Pts',(-18.3167935417111,-13.4305915605693,
116.896456913449)) ;
#164334 = CARTESIAN_POINT('Ctrl Pts',(-18.3404715168385,-13.4310927684104,
116.968576205264)) ;
#164335 = CARTESIAN_POINT('Ctrl Pts',(-18.3641494919659,-13.4315939762514,
117.040695497079)) ;
#164336 = CARTESIAN_POINT('Ctrl Pts',(-18.290345648455,-13.4315939764568,
117.064926538488)) ;
#164337 = CARTESIAN_POINT('Ctrl Pts',(-18.2165418049442,-13.4315939766622,
117.089157579897)) ;
#164338 = CARTESIAN_POINT('Ctrl Pts',(-18.1928638298168,-13.4310927688211,
117.017038288082)) ;
#164339 = CARTESIAN_POINT('Ctrl Pts',(-18.1901471905866,-13.7181744540682,
116.973422879624)) ;
#164340 = CARTESIAN_POINT('Ctrl Pts',(-18.1673557325083,-13.6976269857138,
116.904003775774)) ;
#164341 = CARTESIAN_POINT('Ctrl Pts',(-18.2411595757253,-13.6976269892172,
116.87977273347)) ;
#164342 = CARTESIAN_POINT('Ctrl Pts',(-18.3149634189423,-13.6976269927207,
116.855541691165)) ;
#164343 = CARTESIAN_POINT('Ctrl Pts',(-18.3377548770205,-13.718174461075,
116.924960795015)) ;
#164344 = CARTESIAN_POINT('Ctrl Pts',(-18.3605463350987,-13.7387219294293,
116.994379898865)) ;
#164345 = CARTESIAN_POINT('Ctrl Pts',(-18.2867424918817,-13.7387219259259,
117.018610941169)) ;
#164346 = CARTESIAN_POINT('Ctrl Pts',(-18.2129386486648,-13.7387219224225,
117.042841983473)) ;
#164347 = CARTESIAN_POINT('Ctrl Pts',(-18.1901471905866,-13.7181744540682,
116.973422879624)) ;
#164348 = CARTESIAN_POINT('Ctrl Pts',(-18.1642251375399,-13.9844854804917,
116.85905117826)) ;
#164349 = CARTESIAN_POINT('Ctrl Pts',(-18.1439433958895,-13.9453130684822,
116.797276265807)) ;
#164350 = CARTESIAN_POINT('Ctrl Pts',(-18.2177472380384,-13.9453130761656,
116.77304522025)) ;
#164351 = CARTESIAN_POINT('Ctrl Pts',(-18.2915510801873,-13.945313083849,
116.748814174693)) ;
#164352 = CARTESIAN_POINT('Ctrl Pts',(-18.3118328218377,-13.9844854958585,
116.810589087145)) ;
#164353 = CARTESIAN_POINT('Ctrl Pts',(-18.3321145634881,-14.023657907868,
116.872363999598)) ;
#164354 = CARTESIAN_POINT('Ctrl Pts',(-18.2583107213392,-14.0236579001846,
116.896595045155)) ;
#164355 = CARTESIAN_POINT('Ctrl Pts',(-18.1845068791902,-14.0236578925012,
116.920826090713)) ;
#164356 = CARTESIAN_POINT('Ctrl Pts',(-18.1642251375399,-13.9844854804917,
116.85905117826)) ;
#164357 = CARTESIAN_POINT('Ctrl Pts',(-18.1174211789805,-14.2108138750807,
116.680986260838)) ;
#164358 = CARTESIAN_POINT('Ctrl Pts',(-18.1011127388961,-14.1557813405772,
116.631313384001)) ;
#164359 = CARTESIAN_POINT('Ctrl Pts',(-18.174916578883,-14.1557813517834,
116.607082331859)) ;
#164360 = CARTESIAN_POINT('Ctrl Pts',(-18.24872041887,-14.1557813629896,116.582851279717)) ;
#164361 = CARTESIAN_POINT('Ctrl Pts',(-18.2650288589544,-14.2108138974931,
116.632524156554)) ;
#164362 = CARTESIAN_POINT('Ctrl Pts',(-18.2813372990388,-14.2658464319965,
116.682197033391)) ;
#164363 = CARTESIAN_POINT('Ctrl Pts',(-18.2075334590519,-14.2658464207903,
116.706428085533)) ;
#164364 = CARTESIAN_POINT('Ctrl Pts',(-18.133729619065,-14.2658464095841,
116.730659137676)) ;
#164365 = CARTESIAN_POINT('Ctrl Pts',(-18.1174211789805,-14.2108138750807,
116.680986260838)) ;
#164366 = CARTESIAN_POINT('Ctrl Pts',(-18.0540206588753,-14.3800184665147,
116.452418834705)) ;
#164367 = CARTESIAN_POINT('Ctrl Pts',(-18.0428491294689,-14.313091902712,
116.418392159101)) ;
#164368 = CARTESIAN_POINT('Ctrl Pts',(-18.1166529665764,-14.3130919141767,
116.394161098189)) ;
#164369 = CARTESIAN_POINT('Ctrl Pts',(-18.190456803684,-14.3130919256413,
116.369930037277)) ;
#164370 = CARTESIAN_POINT('Ctrl Pts',(-18.2016283330905,-14.3800184894439,
116.40395671288)) ;
#164371 = CARTESIAN_POINT('Ctrl Pts',(-18.2127998624969,-14.4469450532465,
116.437983388484)) ;
#164372 = CARTESIAN_POINT('Ctrl Pts',(-18.1389960253894,-14.4469450417819,
116.462214449397)) ;
#164373 = CARTESIAN_POINT('Ctrl Pts',(-18.0651921882818,-14.4469450303173,
116.486445510309)) ;
#164374 = CARTESIAN_POINT('Ctrl Pts',(-18.0540206588753,-14.3800184665147,
116.452418834705)) ;
#164375 = CARTESIAN_POINT('Ctrl Pts',(-17.9792474553968,-14.4803359496639,
116.189200422911)) ;
#164376 = CARTESIAN_POINT('Ctrl Pts',(-17.9740145271626,-14.4063082157353,
116.173261768448)) ;
#164377 = CARTESIAN_POINT('Ctrl Pts',(-18.0478183610358,-14.4063082232175,
116.149030697684)) ;
#164378 = CARTESIAN_POINT('Ctrl Pts',(-18.1216221949091,-14.4063082306997,
116.124799626921)) ;
#164379 = CARTESIAN_POINT('Ctrl Pts',(-18.1268551231433,-14.4803359646283,
116.140738281384)) ;
#164380 = CARTESIAN_POINT('Ctrl Pts',(-18.1320880513776,-14.554363698557,
116.156676935847)) ;
#164381 = CARTESIAN_POINT('Ctrl Pts',(-18.0582842175043,-14.5543636910748,
116.180908006611)) ;
#164382 = CARTESIAN_POINT('Ctrl Pts',(-17.9844803836311,-14.5543636835926,
116.205139077375)) ;
#164383 = CARTESIAN_POINT('Ctrl Pts',(-17.9792474553968,-14.4803359496639,
116.189200422911)) ;
#164384 = CARTESIAN_POINT('Ctrl Pts',(-17.8993604815513,-14.5045829128103,
115.910464657861)) ;
#164385 = CARTESIAN_POINT('Ctrl Pts',(-17.9004305121953,-14.4287553960091,
115.913723799318)) ;
#164386 = CARTESIAN_POINT('Ctrl Pts',(-17.9742343432803,-14.4287553947463,
115.889492720062)) ;
#164387 = CARTESIAN_POINT('Ctrl Pts',(-18.0480381743654,-14.4287553934836,
115.865261640806)) ;
#164388 = CARTESIAN_POINT('Ctrl Pts',(-18.0469681437214,-14.5045829102848,
115.862002499349)) ;
#164389 = CARTESIAN_POINT('Ctrl Pts',(-18.0458981130775,-14.580410427086,
115.858743357893)) ;
#164390 = CARTESIAN_POINT('Ctrl Pts',(-17.9720942819924,-14.5804104283487,
115.882974437149)) ;
#164391 = CARTESIAN_POINT('Ctrl Pts',(-17.8982904509073,-14.5804104296115,
115.907205516405)) ;
#164392 = CARTESIAN_POINT('Ctrl Pts',(-17.8993604815513,-14.5045829128103,
115.910464657861)) ;
#164393 = CARTESIAN_POINT('Ctrl Pts',(-17.8204973524233,-14.4510580252238,
115.634757477043)) ;
#164394 = CARTESIAN_POINT('Ctrl Pts',(-17.8278097544475,-14.3788579006376,
115.657029874697)) ;
#164395 = CARTESIAN_POINT('Ctrl Pts',(-17.9016135833738,-14.3788578861591,
115.632798788866)) ;
#164396 = CARTESIAN_POINT('Ctrl Pts',(-17.9754174123,-14.3788578716805,115.608567703034)) ;
#164397 = CARTESIAN_POINT('Ctrl Pts',(-17.9681050102758,-14.4510579962666,
115.58629530538)) ;
#164398 = CARTESIAN_POINT('Ctrl Pts',(-17.9607926082516,-14.5232581208527,
115.564022907727)) ;
#164399 = CARTESIAN_POINT('Ctrl Pts',(-17.8869887793254,-14.5232581353313,
115.588253993558)) ;
#164400 = CARTESIAN_POINT('Ctrl Pts',(-17.8131849503991,-14.5232581498099,
115.612485079389)) ;
#164401 = CARTESIAN_POINT('Ctrl Pts',(-17.8204973524233,-14.4510580252238,
115.634757477043)) ;
#164402 = CARTESIAN_POINT('Ctrl Pts',(-17.7492736539393,-14.3231627979094,
115.382303854319)) ;
#164403 = CARTESIAN_POINT('Ctrl Pts',(-17.7623043373633,-14.2597876685306,
115.421993214653)) ;
#164404 = CARTESIAN_POINT('Ctrl Pts',(-17.8361081656518,-14.2597876370506,
115.397762126879)) ;
#164405 = CARTESIAN_POINT('Ctrl Pts',(-17.9099119939404,-14.2597876055706,
115.373531039106)) ;
#164406 = CARTESIAN_POINT('Ctrl Pts',(-17.8968813105165,-14.3231627349493,
115.333841678772)) ;
#164407 = CARTESIAN_POINT('Ctrl Pts',(-17.8838506270926,-14.386537864328,
115.294152318439)) ;
#164408 = CARTESIAN_POINT('Ctrl Pts',(-17.810046798804,-14.3865378958081,
115.318383406212)) ;
#164409 = CARTESIAN_POINT('Ctrl Pts',(-17.7362429705154,-14.3865379272881,
115.342614493986)) ;
#164410 = CARTESIAN_POINT('Ctrl Pts',(-17.7492736539393,-14.3231627979094,
115.382303854319)) ;
#164411 = CARTESIAN_POINT('Ctrl Pts',(-17.6917549715632,-14.1311846385056,
115.17173247464)) ;
#164412 = CARTESIAN_POINT('Ctrl Pts',(-17.7095523530007,-14.0811216324566,
115.225940428166)) ;
#164413 = CARTESIAN_POINT('Ctrl Pts',(-17.783356182875,-14.0811215835067,
115.201709345222)) ;
#164414 = CARTESIAN_POINT('Ctrl Pts',(-17.8571600127492,-14.0811215345568,
115.177478262278)) ;
#164415 = CARTESIAN_POINT('Ctrl Pts',(-17.8393626313117,-14.1311845406059,
115.123270308753)) ;
#164416 = CARTESIAN_POINT('Ctrl Pts',(-17.8215652498742,-14.181247546655,
115.069062355227)) ;
#164417 = CARTESIAN_POINT('Ctrl Pts',(-17.7477614199999,-14.1812475956048,
115.093293438171)) ;
#164418 = CARTESIAN_POINT('Ctrl Pts',(-17.6739575901257,-14.1812476445547,
115.117524521115)) ;
#164419 = CARTESIAN_POINT('Ctrl Pts',(-17.6917549715632,-14.1311846385056,
115.17173247464)) ;
#164420 = CARTESIAN_POINT('Ctrl Pts',(-17.6523872903775,-13.8873682377616,
115.016307959891)) ;
#164421 = CARTESIAN_POINT('Ctrl Pts',(-17.6736939375746,-13.8542552865156,
115.081204570868)) ;
#164422 = CARTESIAN_POINT('Ctrl Pts',(-17.7474977708464,-13.8542552201397,
115.056973498272)) ;
#164423 = CARTESIAN_POINT('Ctrl Pts',(-17.8213016041181,-13.8542551537638,
115.032742425676)) ;
#164424 = CARTESIAN_POINT('Ctrl Pts',(-17.799994956921,-13.8873681050098,
114.9678458147)) ;
#164425 = CARTESIAN_POINT('Ctrl Pts',(-17.7786883097238,-13.9204810562558,
114.902949203724)) ;
#164426 = CARTESIAN_POINT('Ctrl Pts',(-17.7048844764521,-13.9204811226317,
114.92718027632)) ;
#164427 = CARTESIAN_POINT('Ctrl Pts',(-17.6310806431803,-13.9204811890076,
114.951411348915)) ;
#164428 = CARTESIAN_POINT('Ctrl Pts',(-17.6523872903775,-13.8873682377616,
115.016307959891)) ;
#164429 = CARTESIAN_POINT('Ctrl Pts',(-17.6350445358594,-13.6103444957185,
114.928037639431)) ;
#164430 = CARTESIAN_POINT('Ctrl Pts',(-17.65832634955,-13.5965245493847,114.998950288995)) ;
#164431 = CARTESIAN_POINT('Ctrl Pts',(-17.7321301883026,-13.5965244695658,
114.974719233093)) ;
#164432 = CARTESIAN_POINT('Ctrl Pts',(-17.8059340270552,-13.5965243897469,
114.950488177192)) ;
#164433 = CARTESIAN_POINT('Ctrl Pts',(-17.7826522133646,-13.6103443360808,
114.879575527628)) ;
#164434 = CARTESIAN_POINT('Ctrl Pts',(-17.7593703996741,-13.6241642824146,
114.808662878064)) ;
#164435 = CARTESIAN_POINT('Ctrl Pts',(-17.6855665609215,-13.6241643622335,
114.832893933966)) ;
#164436 = CARTESIAN_POINT('Ctrl Pts',(-17.6117627221689,-13.6241644420523,
114.857124989867)) ;
#164437 = CARTESIAN_POINT('Ctrl Pts',(-17.6350445358594,-13.6103444957185,
114.928037639431)) ;
#164438 = CARTESIAN_POINT('Ctrl Pts',(-17.6416077422069,-13.3193309051749,
114.912549638039)) ;
#164439 = CARTESIAN_POINT('Ctrl Pts',(-17.66519928261,-13.3258084661624,114.984405665328)) ;
#164440 = CARTESIAN_POINT('Ctrl Pts',(-17.7390031283457,-13.3258083784264,
114.960174630696)) ;
#164441 = CARTESIAN_POINT('Ctrl Pts',(-17.8128069740815,-13.3258082906904,
114.935943596063)) ;
#164442 = CARTESIAN_POINT('Ctrl Pts',(-17.7892154336784,-13.3193307297029,
114.864087568775)) ;
#164443 = CARTESIAN_POINT('Ctrl Pts',(-17.7656238932752,-13.3128531687154,
114.792231541486)) ;
#164444 = CARTESIAN_POINT('Ctrl Pts',(-17.6918200475395,-13.3128532564514,
114.816462576118)) ;
#164445 = CARTESIAN_POINT('Ctrl Pts',(-17.6180162018037,-13.3128533441874,
114.84069361075)) ;
#164446 = CARTESIAN_POINT('Ctrl Pts',(-17.6416077422069,-13.3193309051749,
114.912549638039)) ;
#164447 = CARTESIAN_POINT('Ctrl Pts',(-17.6723780315053,-13.0356124679736,
114.970821374696)) ;
#164448 = CARTESIAN_POINT('Ctrl Pts',(-17.6945891508528,-13.0619076839879,
115.038472862292)) ;
#164449 = CARTESIAN_POINT('Ctrl Pts',(-17.7683930044287,-13.061907595961,
115.01424185154)) ;
#164450 = CARTESIAN_POINT('Ctrl Pts',(-17.8421968580047,-13.061907507934,
114.990010840787)) ;
#164451 = CARTESIAN_POINT('Ctrl Pts',(-17.8199857386572,-13.0356122919197,
114.922359353192)) ;
#164452 = CARTESIAN_POINT('Ctrl Pts',(-17.7977746193098,-13.0093170759053,
114.854707865596)) ;
#164453 = CARTESIAN_POINT('Ctrl Pts',(-17.7239707657338,-13.0093171639322,
114.878938876348)) ;
#164454 = CARTESIAN_POINT('Ctrl Pts',(-17.6501669121579,-13.0093172519592,
114.903169887101)) ;
#164455 = CARTESIAN_POINT('Ctrl Pts',(-17.6723780315053,-13.0356124679736,
114.970821374696)) ;
#164456 = CARTESIAN_POINT('Ctrl Pts',(-17.7258605936467,-12.7792808148317,
115.098276186666)) ;
#164457 = CARTESIAN_POINT('Ctrl Pts',(-17.7451035698503,-12.8235105133311,
115.156887189249)) ;
#164458 = CARTESIAN_POINT('Ctrl Pts',(-17.8189074312596,-12.8235104331366,
115.132656202356)) ;
#164459 = CARTESIAN_POINT('Ctrl Pts',(-17.892711292669,-12.8235103529421,
115.108425215463)) ;
#164460 = CARTESIAN_POINT('Ctrl Pts',(-17.8734683164654,-12.7792806544427,
115.04981421288)) ;
#164461 = CARTESIAN_POINT('Ctrl Pts',(-17.8542253402618,-12.7350509559433,
114.991203210297)) ;
#164462 = CARTESIAN_POINT('Ctrl Pts',(-17.7804214788524,-12.7350510361378,
115.01543419719)) ;
#164463 = CARTESIAN_POINT('Ctrl Pts',(-17.706617617443,-12.7350511163323,
115.039665184083)) ;
#164464 = CARTESIAN_POINT('Ctrl Pts',(-17.7258605936467,-12.7792808148317,
115.098276186666)) ;
#164465 = CARTESIAN_POINT('Ctrl Pts',(-17.7991432643167,-12.568318140118,
115.285978414549)) ;
#164466 = CARTESIAN_POINT('Ctrl Pts',(-17.8140327994455,-12.6273412297626,
115.331329538125)) ;
#164467 = CARTESIAN_POINT('Ctrl Pts',(-17.8878366678983,-12.6273411651946,
115.307098572685)) ;
#164468 = CARTESIAN_POINT('Ctrl Pts',(-17.9616405363511,-12.6273411006266,
115.282867607246)) ;
#164469 = CARTESIAN_POINT('Ctrl Pts',(-17.9467510012223,-12.568318010982,
115.23751648367)) ;
#164470 = CARTESIAN_POINT('Ctrl Pts',(-17.9318614660935,-12.5092949213373,
115.192165360094)) ;
#164471 = CARTESIAN_POINT('Ctrl Pts',(-17.8580575976407,-12.5092949859053,
115.216396325534)) ;
#164472 = CARTESIAN_POINT('Ctrl Pts',(-17.7842537291879,-12.5092950504733,
115.240627290974)) ;
#164473 = CARTESIAN_POINT('Ctrl Pts',(-17.7991432643167,-12.568318140118,
115.285978414549)) ;
#164474 = CARTESIAN_POINT('Ctrl Pts',(-17.8875976416786,-12.4185302079718,
115.519914986139)) ;
#164475 = CARTESIAN_POINT('Ctrl Pts',(-17.897067677724,-12.4880976547663,
115.548759189997)) ;
#164476 = CARTESIAN_POINT('Ctrl Pts',(-17.9708715514779,-12.4880976127796,
115.524528240703)) ;
#164477 = CARTESIAN_POINT('Ctrl Pts',(-18.0446754252318,-12.4880975707929,
115.50029729141)) ;
#164478 = CARTESIAN_POINT('Ctrl Pts',(-18.0352053891865,-12.4185301239984,
115.471453087553)) ;
#164479 = CARTESIAN_POINT('Ctrl Pts',(-18.0257353531411,-12.3489626772039,
115.442608883696)) ;
#164480 = CARTESIAN_POINT('Ctrl Pts',(-17.9519314793872,-12.3489627191906,
115.466839832989)) ;
#164481 = CARTESIAN_POINT('Ctrl Pts',(-17.8781276056333,-12.3489627611773,
115.491070782282)) ;
#164482 = CARTESIAN_POINT('Ctrl Pts',(-17.8875976416786,-12.4185302079718,
115.519914986139)) ;
#164483 = CARTESIAN_POINT('Ctrl Pts',(-17.9853421141221,-12.3404555156159,
115.782254580192)) ;
#164484 = CARTESIAN_POINT('Ctrl Pts',(-17.9887338460983,-12.415576081878,
115.792585250618)) ;
#164485 = CARTESIAN_POINT('Ctrl Pts',(-18.0625377227563,-12.415576066971,
115.76835431017)) ;
#164486 = CARTESIAN_POINT('Ctrl Pts',(-18.1363415994144,-12.415576052064,
115.744123369722)) ;
#164487 = CARTESIAN_POINT('Ctrl Pts',(-18.1329498674381,-12.3404554858018,
115.733792699297)) ;
#164488 = CARTESIAN_POINT('Ctrl Pts',(-18.1295581354619,-12.2653349195397,
115.723462028871)) ;
#164489 = CARTESIAN_POINT('Ctrl Pts',(-18.0557542588039,-12.2653349344467,
115.747692969319)) ;
#164490 = CARTESIAN_POINT('Ctrl Pts',(-17.9819503821459,-12.2653349493537,
115.771923909767)) ;
#164491 = CARTESIAN_POINT('Ctrl Pts',(-17.9853421141221,-12.3404555156159,
115.782254580192)) ;
#164492 = CARTESIAN_POINT('Ctrl Pts',(-18.0868118255984,-12.3391866191646,
116.05580631284)) ;
#164493 = CARTESIAN_POINT('Ctrl Pts',(-18.0838591070142,-12.414506911119,
116.046812810549)) ;
#164494 = CARTESIAN_POINT('Ctrl Pts',(-18.1576629839821,-12.4145069252737,
116.022581871045)) ;
#164495 = CARTESIAN_POINT('Ctrl Pts',(-18.2314668609501,-12.4145069394284,
115.998350931541)) ;
#164496 = CARTESIAN_POINT('Ctrl Pts',(-18.2344195795343,-12.339186647474,
116.007344433833)) ;
#164497 = CARTESIAN_POINT('Ctrl Pts',(-18.2373722981186,-12.2638663555197,
116.016337936124)) ;
#164498 = CARTESIAN_POINT('Ctrl Pts',(-18.1635684211506,-12.263866341365,
116.040568875628)) ;
#164499 = CARTESIAN_POINT('Ctrl Pts',(-18.0897645441826,-12.2638663272102,
116.064799815132)) ;
#164500 = CARTESIAN_POINT('Ctrl Pts',(-18.0868118255984,-12.3391866191646,
116.05580631284)) ;
#164501 = CARTESIAN_POINT('Ctrl Pts',(-18.1852509236495,-12.4158174303531,
116.320068764456)) ;
#164502 = CARTESIAN_POINT('Ctrl Pts',(-18.1761571098729,-12.4858997019266,
116.292370477058)) ;
#164503 = CARTESIAN_POINT('Ctrl Pts',(-18.2499609842654,-12.4858997440293,
116.26813952971)) ;
#164504 = CARTESIAN_POINT('Ctrl Pts',(-18.3237648586579,-12.4858997861321,
116.243908582362)) ;
#164505 = CARTESIAN_POINT('Ctrl Pts',(-18.3328586724345,-12.4158175145586,
116.271606869759)) ;
#164506 = CARTESIAN_POINT('Ctrl Pts',(-18.3419524862111,-12.3457352429851,
116.299305157156)) ;
#164507 = CARTESIAN_POINT('Ctrl Pts',(-18.2681486118186,-12.3457352008824,
116.323536104504)) ;
#164508 = CARTESIAN_POINT('Ctrl Pts',(-18.1943447374261,-12.3457351587796,
116.347767051853)) ;
#164509 = CARTESIAN_POINT('Ctrl Pts',(-18.1852509236495,-12.4158174303531,
116.320068764456)) ;
#164510 = CARTESIAN_POINT('Ctrl Pts',(-18.2736690699775,-12.5633739390689,
116.554033969862)) ;
#164511 = CARTESIAN_POINT('Ctrl Pts',(-18.2591199740358,-12.6232581610032,
116.50971977317)) ;
#164512 = CARTESIAN_POINT('Ctrl Pts',(-18.3329238434958,-12.623258227084,
116.485488810798)) ;
#164513 = CARTESIAN_POINT('Ctrl Pts',(-18.4067277129559,-12.6232582931649,
116.461257848426)) ;
#164514 = CARTESIAN_POINT('Ctrl Pts',(-18.4212768088976,-12.5633740712307,
116.505572045118)) ;
#164515 = CARTESIAN_POINT('Ctrl Pts',(-18.4358259048393,-12.5034898492964,
116.549886241811)) ;
#164516 = CARTESIAN_POINT('Ctrl Pts',(-18.3620220353792,-12.5034897832155,
116.574117204182)) ;
#164517 = CARTESIAN_POINT('Ctrl Pts',(-18.2882181659192,-12.5034897171346,
116.598348166554)) ;
#164518 = CARTESIAN_POINT('Ctrl Pts',(-18.2736690699775,-12.5633739390689,
116.554033969862)) ;
#164519 = CARTESIAN_POINT('Ctrl Pts',(-18.34761454464,-12.7732714821549,116.743674390911)) ;
#164520 = CARTESIAN_POINT('Ctrl Pts',(-18.3286173868234,-12.8185910964645,
116.685812115381)) ;
#164521 = CARTESIAN_POINT('Ctrl Pts',(-18.4024212492602,-12.8185911800319,
116.661581131617)) ;
#164522 = CARTESIAN_POINT('Ctrl Pts',(-18.4762251116969,-12.8185912635994,
116.637350147854)) ;
#164523 = CARTESIAN_POINT('Ctrl Pts',(-18.4952222695136,-12.7732716492898,
116.695212423384)) ;
#164524 = CARTESIAN_POINT('Ctrl Pts',(-18.5142194273302,-12.7279520349803,
116.753074698914)) ;
#164525 = CARTESIAN_POINT('Ctrl Pts',(-18.4404155648934,-12.7279519514128,
116.777305682677)) ;
#164526 = CARTESIAN_POINT('Ctrl Pts',(-18.3666117024567,-12.7279518678453,
116.801536666441)) ;
#164527 = CARTESIAN_POINT('Ctrl Pts',(-18.34761454464,-12.7732714821549,116.743674390911)) ;
#164528 = CARTESIAN_POINT('Ctrl Pts',(-18.4016381348897,-13.0290278048664,
116.87274105532)) ;
#164529 = CARTESIAN_POINT('Ctrl Pts',(-18.3795748783009,-13.0565590545988,
116.805539937565)) ;
#164530 = CARTESIAN_POINT('Ctrl Pts',(-18.4533787326858,-13.0565591475459,
116.781308929277)) ;
#164531 = CARTESIAN_POINT('Ctrl Pts',(-18.5271825870708,-13.056559240493,
116.757077920989)) ;
#164532 = CARTESIAN_POINT('Ctrl Pts',(-18.5492458436597,-13.0290279907607,
116.824279038744)) ;
#164533 = CARTESIAN_POINT('Ctrl Pts',(-18.5713091002485,-13.0014967410283,
116.891480156499)) ;
#164534 = CARTESIAN_POINT('Ctrl Pts',(-18.4975052458635,-13.0014966480811,
116.915711164788)) ;
#164535 = CARTESIAN_POINT('Ctrl Pts',(-18.4237013914785,-13.001496555134,
116.939942173076)) ;
#164536 = CARTESIAN_POINT('Ctrl Pts',(-18.4016381348897,-13.0290278048664,
116.87274105532)) ;
#164537 = CARTESIAN_POINT('Ctrl Pts',(-18.4328995250642,-13.311039520292,
116.932661649428)) ;
#164538 = CARTESIAN_POINT('Ctrl Pts',(-18.4093510570389,-13.3189223773524,
116.860936817201)) ;
#164539 = CARTESIAN_POINT('Ctrl Pts',(-18.4831549032372,-13.3189224724508,
116.836705783977)) ;
#164540 = CARTESIAN_POINT('Ctrl Pts',(-18.5569587494355,-13.3189225675491,
116.812474750754)) ;
#164541 = CARTESIAN_POINT('Ctrl Pts',(-18.5805072174607,-13.3110397104886,
116.884199582981)) ;
#164542 = CARTESIAN_POINT('Ctrl Pts',(-18.6040556854859,-13.3031568534281,
116.955924415209)) ;
#164543 = CARTESIAN_POINT('Ctrl Pts',(-18.5302518392876,-13.3031567583298,
116.980155448432)) ;
#164544 = CARTESIAN_POINT('Ctrl Pts',(-18.4564479930894,-13.3031566632315,
117.004386481656)) ;
#164545 = CARTESIAN_POINT('Ctrl Pts',(-18.4328995250642,-13.311039520292,
116.932661649428)) ;
#164546 = CARTESIAN_POINT('Ctrl Pts',(-18.4402061721739,-13.6025944687999,
116.919383947434)) ;
#164547 = CARTESIAN_POINT('Ctrl Pts',(-18.4168473145123,-13.5901335291486,
116.848236637664)) ;
#164548 = CARTESIAN_POINT('Ctrl Pts',(-18.4906511529816,-13.5901336172138,
116.824005580899)) ;
#164549 = CARTESIAN_POINT('Ctrl Pts',(-18.5644549914509,-13.5901337052789,
116.799774524135)) ;
#164550 = CARTESIAN_POINT('Ctrl Pts',(-18.5878138491125,-13.6025946449302,
116.870921833905)) ;
#164551 = CARTESIAN_POINT('Ctrl Pts',(-18.611172706774,-13.6150555845815,
116.942069143675)) ;
#164552 = CARTESIAN_POINT('Ctrl Pts',(-18.5373688683047,-13.6150554965163,
116.96630020044)) ;
#164553 = CARTESIAN_POINT('Ctrl Pts',(-18.4635650298354,-13.6150554084512,
116.990531257205)) ;
#164554 = CARTESIAN_POINT('Ctrl Pts',(-18.4402061721739,-13.6025944687999,
116.919383947434)) ;
#164555 = CARTESIAN_POINT('Ctrl Pts',(-18.4233520704334,-13.8812809383862,
116.83246376881)) ;
#164556 = CARTESIAN_POINT('Ctrl Pts',(-18.4018709139164,-13.8493436684039,
116.767035633613)) ;
#164557 = CARTESIAN_POINT('Ctrl Pts',(-18.475674746248,-13.8493437421996,
116.742804558154)) ;
#164558 = CARTESIAN_POINT('Ctrl Pts',(-18.5494785785796,-13.8493438159953,
116.718573482695)) ;
#164559 = CARTESIAN_POINT('Ctrl Pts',(-18.5709597350966,-13.8812810859776,
116.784001617891)) ;
#164560 = CARTESIAN_POINT('Ctrl Pts',(-18.5924408916136,-13.91321835596,116.849429753088)) ;
#164561 = CARTESIAN_POINT('Ctrl Pts',(-18.518637059282,-13.9132182821642,
116.873660828547)) ;
#164562 = CARTESIAN_POINT('Ctrl Pts',(-18.4448332269504,-13.9132182083685,
116.897891904006)) ;
#164563 = CARTESIAN_POINT('Ctrl Pts',(-18.4233520704334,-13.8812809383862,
116.83246376881)) ;
#164564 = CARTESIAN_POINT('Ctrl Pts',(-18.3845330845332,-14.1255805603194,
116.67878294439)) ;
#164565 = CARTESIAN_POINT('Ctrl Pts',(-18.3664632252227,-14.0765381533461,
116.623745069933)) ;
#164566 = CARTESIAN_POINT('Ctrl Pts',(-18.4402670533431,-14.0765382096367,
116.599513981648)) ;
#164567 = CARTESIAN_POINT('Ctrl Pts',(-18.5140708814636,-14.0765382659272,
116.575282893362)) ;
#164568 = CARTESIAN_POINT('Ctrl Pts',(-18.5321407407742,-14.1255806729005,
116.630320767818)) ;
#164569 = CARTESIAN_POINT('Ctrl Pts',(-18.5502106000847,-14.1746230798738,
116.685358642275)) ;
#164570 = CARTESIAN_POINT('Ctrl Pts',(-18.4764067719642,-14.1746230235832,
116.70958973056)) ;
#164571 = CARTESIAN_POINT('Ctrl Pts',(-18.4026029438438,-14.1746229672927,
116.733820818846)) ;
#164572 = CARTESIAN_POINT('Ctrl Pts',(-18.3845330845332,-14.1255805603194,
116.67878294439)) ;
#164573 = CARTESIAN_POINT('Ctrl Pts',(-18.327532397449,-14.3187775567506,
116.469844757912)) ;
#164574 = CARTESIAN_POINT('Ctrl Pts',(-18.3141460031641,-14.2561721996919,
116.429071962122)) ;
#164575 = CARTESIAN_POINT('Ctrl Pts',(-18.3879498288931,-14.2561722372695,
116.404840866552)) ;
#164576 = CARTESIAN_POINT('Ctrl Pts',(-18.461753654622,-14.256172274847,116.380609770982)) ;
#164577 = CARTESIAN_POINT('Ctrl Pts',(-18.4751400489069,-14.3187776319056,
116.421382566773)) ;
#164578 = CARTESIAN_POINT('Ctrl Pts',(-18.4885264431918,-14.3813829889642,
116.462155362563)) ;
#164579 = CARTESIAN_POINT('Ctrl Pts',(-18.4147226174628,-14.3813829513867,
116.486386458133)) ;
#164580 = CARTESIAN_POINT('Ctrl Pts',(-18.3409187917339,-14.3813829138092,
116.510617553703)) ;
#164581 = CARTESIAN_POINT('Ctrl Pts',(-18.327532397449,-14.3187775567506,
116.469844757912)) ;
#164582 = CARTESIAN_POINT('Ctrl Pts',(-18.2567230506167,-14.4483980300764,
116.218709261403)) ;
#164583 = CARTESIAN_POINT('Ctrl Pts',(-18.2489940958028,-14.3766476693991,
116.195168113257)) ;
#164584 = CARTESIAN_POINT('Ctrl Pts',(-18.3227979214796,-14.3766476878194,
116.170937017528)) ;
#164585 = CARTESIAN_POINT('Ctrl Pts',(-18.3966017471563,-14.3766477062396,
116.146705921799)) ;
#164586 = CARTESIAN_POINT('Ctrl Pts',(-18.4043307019702,-14.4483980669169,
116.170247069945)) ;
#164587 = CARTESIAN_POINT('Ctrl Pts',(-18.4120596567841,-14.5201484275943,
116.193788218092)) ;
#164588 = CARTESIAN_POINT('Ctrl Pts',(-18.3382558311073,-14.520148409174,
116.218019313821)) ;
#164589 = CARTESIAN_POINT('Ctrl Pts',(-18.2644520054306,-14.5201483907537,
116.24225040955)) ;
#164590 = CARTESIAN_POINT('Ctrl Pts',(-18.2567230506167,-14.4483980300764,
116.218709261403)) ;
#164591 = CARTESIAN_POINT('Ctrl Pts',(-18.1778970771393,-14.5042941688686,
115.943075214892)) ;
#164592 = CARTESIAN_POINT('Ctrl Pts',(-18.1763955676776,-14.4285319857966,
115.938501860312)) ;
#164593 = CARTESIAN_POINT('Ctrl Pts',(-18.2501993953997,-14.4285319877587,
115.914270770813)) ;
#164594 = CARTESIAN_POINT('Ctrl Pts',(-18.3240032231218,-14.4285319897207,
115.890039681315)) ;
#164595 = CARTESIAN_POINT('Ctrl Pts',(-18.3255047325835,-14.5042941727927,
115.894613035894)) ;
#164596 = CARTESIAN_POINT('Ctrl Pts',(-18.3270062420453,-14.5800563558646,
115.899186390474)) ;
#164597 = CARTESIAN_POINT('Ctrl Pts',(-18.2532024143231,-14.5800563539026,
115.923417479973)) ;
#164598 = CARTESIAN_POINT('Ctrl Pts',(-18.179398586601,-14.5800563519406,
115.947648569472)) ;
#164599 = CARTESIAN_POINT('Ctrl Pts',(-18.1778970771393,-14.5042941688686,
115.943075214892)) ;
#164600 = CARTESIAN_POINT('Ctrl Pts',(-18.0975716050986,-14.4816544194473,
115.662825279825)) ;
#164601 = CARTESIAN_POINT('Ctrl Pts',(-18.1024128481373,-14.4073576522614,
115.677570925769)) ;
#164602 = CARTESIAN_POINT('Ctrl Pts',(-18.1762166792796,-14.4073576431116,
115.653339846688)) ;
#164603 = CARTESIAN_POINT('Ctrl Pts',(-18.2500205104219,-14.4073576339619,
115.629108767606)) ;
#164604 = CARTESIAN_POINT('Ctrl Pts',(-18.2451792673833,-14.4816544011478,
115.614363121662)) ;
#164605 = CARTESIAN_POINT('Ctrl Pts',(-18.2403380243447,-14.5559511683337,
115.599617475718)) ;
#164606 = CARTESIAN_POINT('Ctrl Pts',(-18.1665341932024,-14.5559511774834,
115.6238485548)) ;
#164607 = CARTESIAN_POINT('Ctrl Pts',(-18.09273036206,-14.5559511866331,115.648079633881)) ;
#164608 = CARTESIAN_POINT('Ctrl Pts',(-18.0975716050986,-14.4816544194473,
115.662825279825)) ;
#164609 = CARTESIAN_POINT('Ctrl Pts',(-18.0231445471785,-14.3839486349316,
115.400927760202)) ;
#164610 = CARTESIAN_POINT('Ctrl Pts',(-18.0339182338649,-14.3163620052717,
115.433742672184)) ;
#164611 = CARTESIAN_POINT('Ctrl Pts',(-18.1077220678756,-14.3163619889056,
115.409511601839)) ;
#164612 = CARTESIAN_POINT('Ctrl Pts',(-18.1815259018863,-14.3163619725394,
115.385280531494)) ;
#164613 = CARTESIAN_POINT('Ctrl Pts',(-18.1707522151998,-14.3839486021993,
115.352465619512)) ;
#164614 = CARTESIAN_POINT('Ctrl Pts',(-18.1599785285133,-14.4515352318592,
115.31965070753)) ;
#164615 = CARTESIAN_POINT('Ctrl Pts',(-18.0861746945026,-14.4515352482253,
115.343881777875)) ;
#164616 = CARTESIAN_POINT('Ctrl Pts',(-18.012370860492,-14.4515352645915,
115.36811284822)) ;
#164617 = CARTESIAN_POINT('Ctrl Pts',(-18.0231445471785,-14.3839486349316,
115.400927760202)) ;
#164618 = CARTESIAN_POINT('Ctrl Pts',(-17.9590787883367,-14.2160711628555,
115.170200653751)) ;
#164619 = CARTESIAN_POINT('Ctrl Pts',(-17.9750787167157,-14.1601035188724,
115.218933854492)) ;
#164620 = CARTESIAN_POINT('Ctrl Pts',(-18.0488825546563,-14.1601035014112,
115.194702796117)) ;
#164621 = CARTESIAN_POINT('Ctrl Pts',(-18.1226863925968,-14.1601034839499,
115.170471737741)) ;
#164622 = CARTESIAN_POINT('Ctrl Pts',(-18.1066864642176,-14.216071127933,
115.121738537)) ;
#164623 = CARTESIAN_POINT('Ctrl Pts',(-18.0906865358385,-14.272038771916,
115.073005336258)) ;
#164624 = CARTESIAN_POINT('Ctrl Pts',(-18.016882697898,-14.2720387893772,
115.097236394634)) ;
#164625 = CARTESIAN_POINT('Ctrl Pts',(-17.9430788599575,-14.2720388068385,
115.121467453009)) ;
#164626 = CARTESIAN_POINT('Ctrl Pts',(-17.9590787883367,-14.2160711628555,
115.170200653751)) ;
#164627 = CARTESIAN_POINT('Ctrl Pts',(-17.9118274735837,-13.9907700541576,
114.990758589762)) ;
#164628 = CARTESIAN_POINT('Ctrl Pts',(-17.9318860793349,-13.9504492968838,
115.051853866757)) ;
#164629 = CARTESIAN_POINT('Ctrl Pts',(-18.0056899201662,-13.950449282471,
115.027622817187)) ;
#164630 = CARTESIAN_POINT('Ctrl Pts',(-18.0794937609976,-13.9504492680581,
115.003391767616)) ;
#164631 = CARTESIAN_POINT('Ctrl Pts',(-18.0594351552463,-13.9907700253318,
114.942296490621)) ;
#164632 = CARTESIAN_POINT('Ctrl Pts',(-18.0393765494951,-14.0310907826056,
114.881201213626)) ;
#164633 = CARTESIAN_POINT('Ctrl Pts',(-17.9655727086638,-14.0310907970185,
114.905432263197)) ;
#164634 = CARTESIAN_POINT('Ctrl Pts',(-17.8917688678324,-14.0310908114314,
114.929663312767)) ;
#164635 = CARTESIAN_POINT('Ctrl Pts',(-17.9118274735837,-13.9907700541576,
114.990758589762)) ;
#164636 = CARTESIAN_POINT('Ctrl Pts',(-17.8853349244506,-13.7263636069236,
114.874779149551)) ;
#164637 = CARTESIAN_POINT('Ctrl Pts',(-17.9080037216021,-13.7044442251976,
114.943824648292)) ;
#164638 = CARTESIAN_POINT('Ctrl Pts',(-17.9818075642068,-13.7044442144499,
114.919593604122)) ;
#164639 = CARTESIAN_POINT('Ctrl Pts',(-18.0556114068114,-13.7044442037021,
114.895362559953)) ;
#164640 = CARTESIAN_POINT('Ctrl Pts',(-18.0329426096599,-13.7263635854281,
114.826317061213)) ;
#164641 = CARTESIAN_POINT('Ctrl Pts',(-18.0102738125084,-13.7482829671541,
114.757271562473)) ;
#164642 = CARTESIAN_POINT('Ctrl Pts',(-17.9364699699037,-13.7482829779018,
114.781502606642)) ;
#164643 = CARTESIAN_POINT('Ctrl Pts',(-17.862666127299,-13.7482829886496,
114.805733650811)) ;
#164644 = CARTESIAN_POINT('Ctrl Pts',(-17.8853349244506,-13.7263636069236,
114.874779149551)) ;
#164645 = CARTESIAN_POINT('Ctrl Pts',(-17.8819867361428,-13.4372481920934,
114.82895312637)) ;
#164646 = CARTESIAN_POINT('Ctrl Pts',(-17.9056609354751,-13.4354837655308,
114.901060917796)) ;
#164647 = CARTESIAN_POINT('Ctrl Pts',(-17.9794647790321,-13.4354837614887,
114.876829876527)) ;
#164648 = CARTESIAN_POINT('Ctrl Pts',(-18.053268622589,-13.4354837574465,
114.852598835258)) ;
#164649 = CARTESIAN_POINT('Ctrl Pts',(-18.0295944232567,-13.4372481840091,
114.780491043832)) ;
#164650 = CARTESIAN_POINT('Ctrl Pts',(-18.0059202239244,-13.4390126105717,
114.708383252406)) ;
#164651 = CARTESIAN_POINT('Ctrl Pts',(-17.9321163803675,-13.4390126146139,
114.732614293675)) ;
#164652 = CARTESIAN_POINT('Ctrl Pts',(-17.8583125368106,-13.4390126186561,
114.756845334944)) ;
#164653 = CARTESIAN_POINT('Ctrl Pts',(-17.8819867361428,-13.4372481920934,
114.82895312637)) ;
#164654 = CARTESIAN_POINT('Ctrl Pts',(-17.9031430677446,-13.1479585724495,
114.857914437922)) ;
#164655 = CARTESIAN_POINT('Ctrl Pts',(-17.926109656016,-13.1663919966203,
114.927866960149)) ;
#164656 = CARTESIAN_POINT('Ctrl Pts',(-17.9999134994939,-13.1663919968395,
114.903635918639)) ;
#164657 = CARTESIAN_POINT('Ctrl Pts',(-18.0737173429717,-13.1663919970587,
114.879404877129)) ;
#164658 = CARTESIAN_POINT('Ctrl Pts',(-18.0507507547003,-13.1479585728878,
114.809452354903)) ;
#164659 = CARTESIAN_POINT('Ctrl Pts',(-18.0277841664289,-13.1295251487169,
114.739499832676)) ;
#164660 = CARTESIAN_POINT('Ctrl Pts',(-17.953980322951,-13.1295251484978,
114.763730874186)) ;
#164661 = CARTESIAN_POINT('Ctrl Pts',(-17.8801764794732,-13.1295251482786,
114.787961915695)) ;
#164662 = CARTESIAN_POINT('Ctrl Pts',(-17.9031430677446,-13.1479585724495,
114.857914437922)) ;
#164663 = CARTESIAN_POINT('Ctrl Pts',(-17.9474975165383,-12.8791408632362,
114.957698840491)) ;
#164664 = CARTESIAN_POINT('Ctrl Pts',(-17.9681319086065,-12.9163723052174,
115.020547869334)) ;
#164665 = CARTESIAN_POINT('Ctrl Pts',(-18.0419357516641,-12.9163723075118,
114.996316826545)) ;
#164666 = CARTESIAN_POINT('Ctrl Pts',(-18.1157395947218,-12.9163723098062,
114.972085783755)) ;
#164667 = CARTESIAN_POINT('Ctrl Pts',(-18.0951052026536,-12.8791408678251,
114.909236754912)) ;
#164668 = CARTESIAN_POINT('Ctrl Pts',(-18.0744708105855,-12.8419094258439,
114.846387726068)) ;
#164669 = CARTESIAN_POINT('Ctrl Pts',(-18.0006669675278,-12.8419094235494,
114.870618768858)) ;
#164670 = CARTESIAN_POINT('Ctrl Pts',(-17.9268631244702,-12.841909421255,
114.894849811647)) ;
#164671 = CARTESIAN_POINT('Ctrl Pts',(-17.9474975165383,-12.8791408632362,
114.957698840491)) ;
#164672 = CARTESIAN_POINT('Ctrl Pts',(-18.0134578929904,-12.6468837882592,
115.122990730371)) ;
#164673 = CARTESIAN_POINT('Ctrl Pts',(-18.0302539814303,-12.7003895422397,
115.174148905655)) ;
#164674 = CARTESIAN_POINT('Ctrl Pts',(-18.1040578240845,-12.7003895445952,
115.149917861637)) ;
#164675 = CARTESIAN_POINT('Ctrl Pts',(-18.1778616667387,-12.7003895469507,
115.125686817618)) ;
#164676 = CARTESIAN_POINT('Ctrl Pts',(-18.1610655782988,-12.6468837929702,
115.074528642334)) ;
#164677 = CARTESIAN_POINT('Ctrl Pts',(-18.1442694898589,-12.5933780389898,
115.02337046705)) ;
#164678 = CARTESIAN_POINT('Ctrl Pts',(-18.0704656472047,-12.5933780366342,
115.047601511069)) ;
#164679 = CARTESIAN_POINT('Ctrl Pts',(-17.9966618045505,-12.5933780342787,
115.071832555087)) ;
#164680 = CARTESIAN_POINT('Ctrl Pts',(-18.0134578929904,-12.6468837882592,
115.122990730371)) ;
#164681 = CARTESIAN_POINT('Ctrl Pts',(-18.0960334426616,-12.471578495706,
115.33917013554)) ;
#164682 = CARTESIAN_POINT('Ctrl Pts',(-18.1078193608246,-12.5374039130151,
115.375068140577)) ;
#164683 = CARTESIAN_POINT('Ctrl Pts',(-18.1816232036953,-12.5374039137778,
115.350837097218)) ;
#164684 = CARTESIAN_POINT('Ctrl Pts',(-18.255427046566,-12.5374039145406,
115.326606053859)) ;
#164685 = CARTESIAN_POINT('Ctrl Pts',(-18.243641128403,-12.4715784972316,
115.290708048822)) ;
#164686 = CARTESIAN_POINT('Ctrl Pts',(-18.23185521024,-12.4057530799226,115.254810043784)) ;
#164687 = CARTESIAN_POINT('Ctrl Pts',(-18.1580513673693,-12.4057530791598,
115.279041087143)) ;
#164688 = CARTESIAN_POINT('Ctrl Pts',(-18.0842475244987,-12.405753078397,
115.303272130502)) ;
#164689 = CARTESIAN_POINT('Ctrl Pts',(-18.0960334426616,-12.471578495706,
115.33917013554)) ;
#164690 = CARTESIAN_POINT('Ctrl Pts',(-18.1907887497896,-12.3629963199509,
115.592326495504)) ;
#164691 = CARTESIAN_POINT('Ctrl Pts',(-18.1967092010793,-12.4365002767228,
115.610359234894)) ;
#164692 = CARTESIAN_POINT('Ctrl Pts',(-18.270513044814,-12.4365002760064,
115.586128194167)) ;
#164693 = CARTESIAN_POINT('Ctrl Pts',(-18.3443168885486,-12.4365002752899,
115.561897153439)) ;
#164694 = CARTESIAN_POINT('Ctrl Pts',(-18.3383964372588,-12.362996318518,
115.543864414049)) ;
#164695 = CARTESIAN_POINT('Ctrl Pts',(-18.332475985969,-12.289492361746,115.525831674658)) ;
#164696 = CARTESIAN_POINT('Ctrl Pts',(-18.2586721422344,-12.2894923624625,
115.550062715386)) ;
#164697 = CARTESIAN_POINT('Ctrl Pts',(-18.1848682984998,-12.289492363179,
115.574293756114)) ;
#164698 = CARTESIAN_POINT('Ctrl Pts',(-18.1907887497896,-12.3629963199509,
115.592326495504)) ;
#164699 = CARTESIAN_POINT('Ctrl Pts',(-18.2921752354518,-12.3302292617424,
115.86545414009)) ;
#164700 = CARTESIAN_POINT('Ctrl Pts',(-18.291763234642,-12.4061292172083,
115.864199252246)) ;
#164701 = CARTESIAN_POINT('Ctrl Pts',(-18.3655670804045,-12.4061292167983,
115.839968217695)) ;
#164702 = CARTESIAN_POINT('Ctrl Pts',(-18.439370926167,-12.4061292163883,
115.815737183144)) ;
#164703 = CARTESIAN_POINT('Ctrl Pts',(-18.4397829269768,-12.3302292609224,
115.816992070988)) ;
#164704 = CARTESIAN_POINT('Ctrl Pts',(-18.4401949277865,-12.2543293054565,
115.818246958833)) ;
#164705 = CARTESIAN_POINT('Ctrl Pts',(-18.366391082024,-12.2543293058665,
115.842477993384)) ;
#164706 = CARTESIAN_POINT('Ctrl Pts',(-18.2925872362615,-12.2543293062765,
115.866709027935)) ;
#164707 = CARTESIAN_POINT('Ctrl Pts',(-18.2921752354518,-12.3302292617424,
115.86545414009)) ;
#164708 = CARTESIAN_POINT('Ctrl Pts',(-18.3922296544393,-12.3757631813199,
116.134800023647)) ;
#164709 = CARTESIAN_POINT('Ctrl Pts',(-18.3855635309461,-12.4485939704729,
116.114496087324)) ;
#164710 = CARTESIAN_POINT('Ctrl Pts',(-18.4593673784764,-12.448593973849,
116.090265058158)) ;
#164711 = CARTESIAN_POINT('Ctrl Pts',(-18.5331712260067,-12.448593977225,
116.066034028991)) ;
#164712 = CARTESIAN_POINT('Ctrl Pts',(-18.5398373495,-12.3757631880721,116.086337965314)) ;
#164713 = CARTESIAN_POINT('Ctrl Pts',(-18.5465034729932,-12.3029323989191,
116.106641901636)) ;
#164714 = CARTESIAN_POINT('Ctrl Pts',(-18.4726996254629,-12.302932395543,
116.130872930802)) ;
#164715 = CARTESIAN_POINT('Ctrl Pts',(-18.3988957779326,-12.302932392167,
116.155103959969)) ;
#164716 = CARTESIAN_POINT('Ctrl Pts',(-18.3922296544393,-12.3757631813199,
116.134800023647)) ;
#164717 = CARTESIAN_POINT('Ctrl Pts',(-18.4853365945326,-12.4955339259777,
116.382983514906)) ;
#164718 = CARTESIAN_POINT('Ctrl Pts',(-18.4728925169486,-12.560107521336,
116.345080862824)) ;
#164719 = CARTESIAN_POINT('Ctrl Pts',(-18.5466963658544,-12.5601075316302,
116.320849837847)) ;
#164720 = CARTESIAN_POINT('Ctrl Pts',(-18.6205002147602,-12.5601075419243,
116.29661881287)) ;
#164721 = CARTESIAN_POINT('Ctrl Pts',(-18.6329442923442,-12.495533946566,
116.334521464952)) ;
#164722 = CARTESIAN_POINT('Ctrl Pts',(-18.6453883699281,-12.4309603512076,
116.372424117033)) ;
#164723 = CARTESIAN_POINT('Ctrl Pts',(-18.5715845210223,-12.4309603409135,
116.39665514201)) ;
#164724 = CARTESIAN_POINT('Ctrl Pts',(-18.4977806721165,-12.4309603306194,
116.420886166987)) ;
#164725 = CARTESIAN_POINT('Ctrl Pts',(-18.4853365945326,-12.4955339259777,
116.382983514906)) ;
#164726 = CARTESIAN_POINT('Ctrl Pts',(-18.5656035304385,-12.6811191445398,
116.592065198689)) ;
#164727 = CARTESIAN_POINT('Ctrl Pts',(-18.5482696175564,-12.7328282545194,
116.539268897404)) ;
#164728 = CARTESIAN_POINT('Ctrl Pts',(-18.622073466999,-12.7328282744618,
116.515037874062)) ;
#164729 = CARTESIAN_POINT('Ctrl Pts',(-18.6958773164415,-12.7328282944042,
116.49080685072)) ;
#164730 = CARTESIAN_POINT('Ctrl Pts',(-18.7132112293236,-12.6811191844247,
116.543603152005)) ;
#164731 = CARTESIAN_POINT('Ctrl Pts',(-18.7305451422058,-12.6294100744451,
116.596399453291)) ;
#164732 = CARTESIAN_POINT('Ctrl Pts',(-18.6567412927632,-12.6294100545027,
116.620630476633)) ;
#164733 = CARTESIAN_POINT('Ctrl Pts',(-18.5829374433206,-12.6294100345603,
116.644861499975)) ;
#164734 = CARTESIAN_POINT('Ctrl Pts',(-18.5656035304385,-12.6811191445398,
116.592065198689)) ;
#164735 = CARTESIAN_POINT('Ctrl Pts',(-18.628225520823,-12.9201897809832,
116.747282894815)) ;
#164736 = CARTESIAN_POINT('Ctrl Pts',(-18.6072291656349,-12.9552816729516,
116.683331385371)) ;
#164737 = CARTESIAN_POINT('Ctrl Pts',(-18.6810330145034,-12.9552817052441,
116.659100360281)) ;
#164738 = CARTESIAN_POINT('Ctrl Pts',(-18.7548368633718,-12.9552817375366,
116.63486933519)) ;
#164739 = CARTESIAN_POINT('Ctrl Pts',(-18.77583321856,-12.9201898455682,116.698820844634)) ;
#164740 = CARTESIAN_POINT('Ctrl Pts',(-18.7968295737481,-12.8850979535998,
116.762772354078)) ;
#164741 = CARTESIAN_POINT('Ctrl Pts',(-18.7230257248796,-12.8850979213072,
116.787003379169)) ;
#164742 = CARTESIAN_POINT('Ctrl Pts',(-18.6492218760112,-12.8850978890147,
116.811234404259)) ;
#164743 = CARTESIAN_POINT('Ctrl Pts',(-18.628225520823,-12.9201897809832,
116.747282894815)) ;
#164744 = CARTESIAN_POINT('Ctrl Pts',(-18.6690904271768,-13.1945616988577,
116.836294766696)) ;
#164745 = CARTESIAN_POINT('Ctrl Pts',(-18.645944233313,-13.2105476900329,
116.765795195688)) ;
#164746 = CARTESIAN_POINT('Ctrl Pts',(-18.7197480798482,-13.2105477342474,
116.741564163491)) ;
#164747 = CARTESIAN_POINT('Ctrl Pts',(-18.7935519263835,-13.2105477784618,
116.717333131293)) ;
#164748 = CARTESIAN_POINT('Ctrl Pts',(-18.8166981202473,-13.1945617872866,
116.787832702302)) ;
#164749 = CARTESIAN_POINT('Ctrl Pts',(-18.8398443141111,-13.1785757961114,
116.85833227331)) ;
#164750 = CARTESIAN_POINT('Ctrl Pts',(-18.7660404675759,-13.178575751897,
116.882563305508)) ;
#164751 = CARTESIAN_POINT('Ctrl Pts',(-18.6922366210406,-13.1785757076825,
116.906794337705)) ;
#164752 = CARTESIAN_POINT('Ctrl Pts',(-18.6690904271768,-13.1945616988577,
116.836294766696)) ;
#164753 = CARTESIAN_POINT('Ctrl Pts',(-18.6862129676211,-13.4849425718836,
116.8529861804)) ;
#164754 = CARTESIAN_POINT('Ctrl Pts',(-18.6625716253769,-13.4806775745737,
116.780978467484)) ;
#164755 = CARTESIAN_POINT('Ctrl Pts',(-18.7363754679992,-13.4806776285265,
116.756747423369)) ;
#164756 = CARTESIAN_POINT('Ctrl Pts',(-18.8101793106214,-13.4806776824793,
116.732516379253)) ;
#164757 = CARTESIAN_POINT('Ctrl Pts',(-18.8338206528657,-13.4849426797892,
116.804524092169)) ;
#164758 = CARTESIAN_POINT('Ctrl Pts',(-18.8574619951098,-13.4892076770991,
116.876531805084)) ;
#164759 = CARTESIAN_POINT('Ctrl Pts',(-18.7836581524876,-13.4892076231463,
116.9007628492)) ;
#164760 = CARTESIAN_POINT('Ctrl Pts',(-18.7098543098653,-13.4892075691935,
116.924993893315)) ;
#164761 = CARTESIAN_POINT('Ctrl Pts',(-18.6862129676211,-13.4849425718836,
116.8529861804)) ;
#164762 = CARTESIAN_POINT('Ctrl Pts',(-18.6790048652342,-13.7714537290315,
116.795457387519)) ;
#164763 = CARTESIAN_POINT('Ctrl Pts',(-18.656568594331,-13.7471788354609,
116.727120127656)) ;
#164764 = CARTESIAN_POINT('Ctrl Pts',(-18.730372431532,-13.7471788958938,
116.702889067029)) ;
#164765 = CARTESIAN_POINT('Ctrl Pts',(-18.8041762687331,-13.7471789563267,
116.678658006401)) ;
#164766 = CARTESIAN_POINT('Ctrl Pts',(-18.8266125396363,-13.7714538498972,
116.746995266264)) ;
#164767 = CARTESIAN_POINT('Ctrl Pts',(-18.8490488105395,-13.7957287434678,
116.815332526127)) ;
#164768 = CARTESIAN_POINT('Ctrl Pts',(-18.7752449733385,-13.7957286830349,
116.839563586755)) ;
#164769 = CARTESIAN_POINT('Ctrl Pts',(-18.7014411361375,-13.7957286226021,
116.863794647382)) ;
#164770 = CARTESIAN_POINT('Ctrl Pts',(-18.6790048652342,-13.7714537290315,
116.795457387519)) ;
#164771 = CARTESIAN_POINT('Ctrl Pts',(-18.6487103937416,-14.0317199143361,
116.667704011276)) ;
#164772 = CARTESIAN_POINT('Ctrl Pts',(-18.6290909043466,-13.9892386384962,
116.60794621356)) ;
#164773 = CARTESIAN_POINT('Ctrl Pts',(-18.7028947352582,-13.9892386981122,
116.583715133776)) ;
#164774 = CARTESIAN_POINT('Ctrl Pts',(-18.7766985661698,-13.9892387577282,
116.559484053992)) ;
#164775 = CARTESIAN_POINT('Ctrl Pts',(-18.7963180555648,-14.0317200335681,
116.619241851708)) ;
#164776 = CARTESIAN_POINT('Ctrl Pts',(-18.8159375449598,-14.074201309408,
116.678999649423)) ;
#164777 = CARTESIAN_POINT('Ctrl Pts',(-18.7421337140482,-14.074201249792,
116.703230729208)) ;
#164778 = CARTESIAN_POINT('Ctrl Pts',(-18.6683298831366,-14.074201190176,
116.727461808992)) ;
#164779 = CARTESIAN_POINT('Ctrl Pts',(-18.6487103937416,-14.0317199143361,
116.667704011276)) ;
#164780 = CARTESIAN_POINT('Ctrl Pts',(-18.5987182341278,-14.2471737495219,
116.480143302008)) ;
#164781 = CARTESIAN_POINT('Ctrl Pts',(-18.5832910387344,-14.1895888186294,
116.433154555517)) ;
#164782 = CARTESIAN_POINT('Ctrl Pts',(-18.6570948637155,-14.1895888696549,
116.408923457669)) ;
#164783 = CARTESIAN_POINT('Ctrl Pts',(-18.7308986886966,-14.1895889206804,
116.384692359822)) ;
#164784 = CARTESIAN_POINT('Ctrl Pts',(-18.74632588409,-14.2471738515729,116.431681106313)) ;
#164785 = CARTESIAN_POINT('Ctrl Pts',(-18.7617530794833,-14.3047587824654,
116.478669852804)) ;
#164786 = CARTESIAN_POINT('Ctrl Pts',(-18.6879492545022,-14.3047587314399,
116.502900950651)) ;
#164787 = CARTESIAN_POINT('Ctrl Pts',(-18.6141454295211,-14.3047586804144,
116.527132048499)) ;
#164788 = CARTESIAN_POINT('Ctrl Pts',(-18.5987182341278,-14.2471737495219,
116.480143302008)) ;
#164789 = CARTESIAN_POINT('Ctrl Pts',(-18.5323754157414,-14.4050269028801,
116.242414711586)) ;
#164790 = CARTESIAN_POINT('Ctrl Pts',(-18.5222953540112,-14.3363371537911,
116.211712471641)) ;
#164791 = CARTESIAN_POINT('Ctrl Pts',(-18.5960991729972,-14.3363371907916,
116.187481355534)) ;
#164792 = CARTESIAN_POINT('Ctrl Pts',(-18.6699029919832,-14.3363372277921,
116.163250239426)) ;
#164793 = CARTESIAN_POINT('Ctrl Pts',(-18.6799830537135,-14.4050269768811,
116.193952479371)) ;
#164794 = CARTESIAN_POINT('Ctrl Pts',(-18.6900631154437,-14.47371672597,116.224654719315)) ;
#164795 = CARTESIAN_POINT('Ctrl Pts',(-18.6162592964577,-14.4737166889695,
116.248885835423)) ;
#164796 = CARTESIAN_POINT('Ctrl Pts',(-18.5424554774717,-14.473716651969,
116.273116951531)) ;
#164797 = CARTESIAN_POINT('Ctrl Pts',(-18.5323754157414,-14.4050269028801,
116.242414711586)) ;
#164798 = CARTESIAN_POINT('Ctrl Pts',(-18.4563272491272,-14.4907853879862,
115.975423526265)) ;
#164799 = CARTESIAN_POINT('Ctrl Pts',(-18.4522736812048,-14.4160085433366,
115.963077014191)) ;
#164800 = CARTESIAN_POINT('Ctrl Pts',(-18.5260774963464,-14.4160085589544,
115.938845886374)) ;
#164801 = CARTESIAN_POINT('Ctrl Pts',(-18.5998813114879,-14.4160085745722,
115.914614758556)) ;
#164802 = CARTESIAN_POINT('Ctrl Pts',(-18.6039348794103,-14.4907854192218,
115.92696127063)) ;
#164803 = CARTESIAN_POINT('Ctrl Pts',(-18.6079884473327,-14.5655622638714,
115.939307782704)) ;
#164804 = CARTESIAN_POINT('Ctrl Pts',(-18.5341846321912,-14.5655622482536,
115.963538910521)) ;
#164805 = CARTESIAN_POINT('Ctrl Pts',(-18.4603808170497,-14.5655622326357,
115.987770038338)) ;
#164806 = CARTESIAN_POINT('Ctrl Pts',(-18.4563272491272,-14.4907853879862,
115.975423526265)) ;
#164807 = CARTESIAN_POINT('Ctrl Pts',(-18.3762354271177,-14.5004458117326,
115.696087954161)) ;
#164808 = CARTESIAN_POINT('Ctrl Pts',(-18.3784999234747,-14.4248856962509,
115.702985246563)) ;
#164809 = CARTESIAN_POINT('Ctrl Pts',(-18.4523037367887,-14.4248856868723,
115.678754113179)) ;
#164810 = CARTESIAN_POINT('Ctrl Pts',(-18.5261075501026,-14.4248856774938,
115.654522979795)) ;
#164811 = CARTESIAN_POINT('Ctrl Pts',(-18.5238430537456,-14.5004457929755,
115.647625687394)) ;
#164812 = CARTESIAN_POINT('Ctrl Pts',(-18.5215785573886,-14.5760059084573,
115.640728394992)) ;
#164813 = CARTESIAN_POINT('Ctrl Pts',(-18.4477747440747,-14.5760059178358,
115.664959528376)) ;
#164814 = CARTESIAN_POINT('Ctrl Pts',(-18.3739709307607,-14.5760059272144,
115.68919066176)) ;
#164815 = CARTESIAN_POINT('Ctrl Pts',(-18.3762354271177,-14.5004458117326,
115.696087954161)) ;
#164816 = CARTESIAN_POINT('Ctrl Pts',(-18.2982431956715,-14.4322721687238,
115.422987302609)) ;
#164817 = CARTESIAN_POINT('Ctrl Pts',(-18.3066916637093,-14.3613608624439,
115.448719975064)) ;
#164818 = CARTESIAN_POINT('Ctrl Pts',(-18.3804954774937,-14.3613608259143,
115.424488843113)) ;
#164819 = CARTESIAN_POINT('Ctrl Pts',(-18.4542992912781,-14.3613607893847,
115.400257711162)) ;
#164820 = CARTESIAN_POINT('Ctrl Pts',(-18.4458508232403,-14.4322720956646,
115.374525038708)) ;
#164821 = CARTESIAN_POINT('Ctrl Pts',(-18.4374023552024,-14.5031834019444,
115.348792366253)) ;
#164822 = CARTESIAN_POINT('Ctrl Pts',(-18.363598541418,-14.5031834384741,
115.373023498204)) ;
#164823 = CARTESIAN_POINT('Ctrl Pts',(-18.2897947276336,-14.5031834750037,
115.397254630155)) ;
#164824 = CARTESIAN_POINT('Ctrl Pts',(-18.2982431956715,-14.4322721687238,
115.422987302609)) ;
#164825 = CARTESIAN_POINT('Ctrl Pts',(-18.2293158225121,-14.2916898608516,
115.177622248156)) ;
#164826 = CARTESIAN_POINT('Ctrl Pts',(-18.2433218842617,-14.2304895577996,
115.220282454403)) ;
#164827 = CARTESIAN_POINT('Ctrl Pts',(-18.3171257013558,-14.2304894954371,
115.196051332533)) ;
#164828 = CARTESIAN_POINT('Ctrl Pts',(-18.3909295184499,-14.2304894330745,
115.171820210663)) ;
#164829 = CARTESIAN_POINT('Ctrl Pts',(-18.3769234567003,-14.2916897361264,
115.129160004416)) ;
#164830 = CARTESIAN_POINT('Ctrl Pts',(-18.3629173949507,-14.3528900391783,
115.086499798169)) ;
#164831 = CARTESIAN_POINT('Ctrl Pts',(-18.2891135778566,-14.3528901015409,
115.110730920039)) ;
#164832 = CARTESIAN_POINT('Ctrl Pts',(-18.2153097607625,-14.3528901639035,
115.134962041909)) ;
#164833 = CARTESIAN_POINT('Ctrl Pts',(-18.2293158225121,-14.2916898608516,
115.177622248156)) ;
#164834 = CARTESIAN_POINT('Ctrl Pts',(-18.174749864149,-14.0883182665925,
114.975935730207)) ;
#164835 = CARTESIAN_POINT('Ctrl Pts',(-18.1933204074683,-14.0412264219864,
115.032498610884)) ;
#164836 = CARTESIAN_POINT('Ctrl Pts',(-18.2671242302435,-14.0412263375894,
115.008267506318)) ;
#164837 = CARTESIAN_POINT('Ctrl Pts',(-18.3409280530187,-14.0412262531924,
114.984036401752)) ;
#164838 = CARTESIAN_POINT('Ctrl Pts',(-18.3223575096994,-14.0883180977985,
114.927473521075)) ;
#164839 = CARTESIAN_POINT('Ctrl Pts',(-18.3037869663801,-14.1354099424045,
114.870910640398)) ;
#164840 = CARTESIAN_POINT('Ctrl Pts',(-18.2299831436049,-14.1354100268015,
114.895141744964)) ;
#164841 = CARTESIAN_POINT('Ctrl Pts',(-18.1561793208297,-14.1354101111986,
114.91937284953)) ;
#164842 = CARTESIAN_POINT('Ctrl Pts',(-18.174749864149,-14.0883182665925,
114.975935730207)) ;
#164843 = CARTESIAN_POINT('Ctrl Pts',(-18.1394221450982,-13.837248063462,
114.832902227183)) ;
#164844 = CARTESIAN_POINT('Ctrl Pts',(-18.1612196540967,-13.8076155637165,
114.89929392467)) ;
#164845 = CARTESIAN_POINT('Ctrl Pts',(-18.2350234844896,-13.8076154638135,
114.875062843306)) ;
#164846 = CARTESIAN_POINT('Ctrl Pts',(-18.3088273148824,-13.8076153639105,
114.850831761941)) ;
#164847 = CARTESIAN_POINT('Ctrl Pts',(-18.2870298058839,-13.837247863656,
114.784440064455)) ;
#164848 = CARTESIAN_POINT('Ctrl Pts',(-18.2652322968854,-13.8668803634015,
114.718048366968)) ;
#164849 = CARTESIAN_POINT('Ctrl Pts',(-18.1914284664925,-13.8668804633045,
114.742279448332)) ;
#164850 = CARTESIAN_POINT('Ctrl Pts',(-18.1176246360997,-13.8668805632075,
114.766510529696)) ;
#164851 = CARTESIAN_POINT('Ctrl Pts',(-18.1394221450982,-13.837248063462,
114.832902227183)) ;
#164852 = CARTESIAN_POINT('Ctrl Pts',(-18.1264317715052,-13.5564419727403,
114.757928115676)) ;
#164853 = CARTESIAN_POINT('Ctrl Pts',(-18.1499010771967,-13.5463705176912,
114.829411836148)) ;
#164854 = CARTESIAN_POINT('Ctrl Pts',(-18.2237049163352,-13.5463704101859,
114.805180781422)) ;
#164855 = CARTESIAN_POINT('Ctrl Pts',(-18.2975087554736,-13.5463703026806,
114.780949726695)) ;
#164856 = CARTESIAN_POINT('Ctrl Pts',(-18.2740394497822,-13.5564417577297,
114.709466006223)) ;
#164857 = CARTESIAN_POINT('Ctrl Pts',(-18.2505701440907,-13.5665132127787,
114.637982285751)) ;
#164858 = CARTESIAN_POINT('Ctrl Pts',(-18.1767663049522,-13.5665133202841,
114.662213340477)) ;
#164859 = CARTESIAN_POINT('Ctrl Pts',(-18.1029624658138,-13.5665134277894,
114.686444395204)) ;
#164860 = CARTESIAN_POINT('Ctrl Pts',(-18.1264317715052,-13.5564419727403,
114.757928115676)) ;
#164861 = CARTESIAN_POINT('Ctrl Pts',(-18.1376262361485,-13.2643191465395,
114.756443371031)) ;
#164862 = CARTESIAN_POINT('Ctrl Pts',(-18.1610852002023,-13.2746275458087,
114.827895592519)) ;
#164863 = CARTESIAN_POINT('Ctrl Pts',(-18.2348890483907,-13.2746274398407,
114.803664565357)) ;
#164864 = CARTESIAN_POINT('Ctrl Pts',(-18.3086928965791,-13.2746273338727,
114.779433538195)) ;
#164865 = CARTESIAN_POINT('Ctrl Pts',(-18.2852339325253,-13.2643189346036,
114.707981316708)) ;
#164866 = CARTESIAN_POINT('Ctrl Pts',(-18.2617749684715,-13.2540105353345,
114.636529095221)) ;
#164867 = CARTESIAN_POINT('Ctrl Pts',(-18.1879711202831,-13.2540106413025,
114.660760122383)) ;
#164868 = CARTESIAN_POINT('Ctrl Pts',(-18.1141672720947,-13.2540107472704,
114.684991149544)) ;
#164869 = CARTESIAN_POINT('Ctrl Pts',(-18.1376262361485,-13.2643191465395,
114.756443371031)) ;
#164870 = CARTESIAN_POINT('Ctrl Pts',(-18.1728174422769,-12.984649033957,
114.828230732684)) ;
#164871 = CARTESIAN_POINT('Ctrl Pts',(-18.1945868419176,-13.0144985177463,
114.894536813537)) ;
#164872 = CARTESIAN_POINT('Ctrl Pts',(-18.2683906984416,-13.0144984216522,
114.870305811764)) ;
#164873 = CARTESIAN_POINT('Ctrl Pts',(-18.3421945549656,-13.0144983255582,
114.846074809991)) ;
#164874 = CARTESIAN_POINT('Ctrl Pts',(-18.3204251553249,-12.9846488417689,
114.779768729138)) ;
#164875 = CARTESIAN_POINT('Ctrl Pts',(-18.2986557556843,-12.9547993579796,
114.713462648285)) ;
#164876 = CARTESIAN_POINT('Ctrl Pts',(-18.2248518991603,-12.9547994540736,
114.737693650058)) ;
#164877 = CARTESIAN_POINT('Ctrl Pts',(-18.1510480426363,-12.9547995501676,
114.761924651831)) ;
#164878 = CARTESIAN_POINT('Ctrl Pts',(-18.1728174422769,-12.984649033957,
114.828230732684)) ;
#164879 = CARTESIAN_POINT('Ctrl Pts',(-18.2303714670288,-12.7352694992048,
114.968035708061)) ;
#164880 = CARTESIAN_POINT('Ctrl Pts',(-18.2488896504848,-12.782574545107,
115.02443910893)) ;
#164881 = CARTESIAN_POINT('Ctrl Pts',(-18.3226935138459,-12.7825744663775,
115.000208127982)) ;
#164882 = CARTESIAN_POINT('Ctrl Pts',(-18.396497377207,-12.782574387648,114.975977147033)) ;
#164883 = CARTESIAN_POINT('Ctrl Pts',(-18.377979193751,-12.7352693417458,
114.919573746164)) ;
#164884 = CARTESIAN_POINT('Ctrl Pts',(-18.3594610102951,-12.6879642958436,
114.863170345295)) ;
#164885 = CARTESIAN_POINT('Ctrl Pts',(-18.285657146934,-12.6879643745731,
114.887401326243)) ;
#164886 = CARTESIAN_POINT('Ctrl Pts',(-18.2118532835729,-12.6879644533026,
114.911632307191)) ;
#164887 = CARTESIAN_POINT('Ctrl Pts',(-18.2303714670288,-12.7352694992048,
114.968035708061)) ;
#164888 = CARTESIAN_POINT('Ctrl Pts',(-18.3068452079196,-12.5350620992742,
115.165496321728)) ;
#164889 = CARTESIAN_POINT('Ctrl Pts',(-18.320785813042,-12.5964160722861,
115.207957157497)) ;
#164890 = CARTESIAN_POINT('Ctrl Pts',(-18.3945896810827,-12.5964160160119,
115.183726190802)) ;
#164891 = CARTESIAN_POINT('Ctrl Pts',(-18.4683935491234,-12.5964159597377,
115.159495224107)) ;
#164892 = CARTESIAN_POINT('Ctrl Pts',(-18.454452944001,-12.5350619867258,
115.117034388338)) ;
#164893 = CARTESIAN_POINT('Ctrl Pts',(-18.4405123388787,-12.4737080137138,
115.07457355257)) ;
#164894 = CARTESIAN_POINT('Ctrl Pts',(-18.366708470838,-12.4737080699881,
115.098804519265)) ;
#164895 = CARTESIAN_POINT('Ctrl Pts',(-18.2929046027973,-12.4737081262623,
115.12303548596)) ;
#164896 = CARTESIAN_POINT('Ctrl Pts',(-18.3068452079196,-12.5350620992742,
115.165496321728)) ;
#164897 = CARTESIAN_POINT('Ctrl Pts',(-18.3974508093172,-12.3981381252086,
115.406021891207)) ;
#164898 = CARTESIAN_POINT('Ctrl Pts',(-18.4058198790453,-12.4691440372206,
115.431512729026)) ;
#164899 = CARTESIAN_POINT('Ctrl Pts',(-18.4796237493277,-12.4691440057978,
115.407281769159)) ;
#164900 = CARTESIAN_POINT('Ctrl Pts',(-18.5534276196102,-12.4691439743751,
115.383050809292)) ;
#164901 = CARTESIAN_POINT('Ctrl Pts',(-18.5450585498822,-12.3981380623631,
115.357559971473)) ;
#164902 = CARTESIAN_POINT('Ctrl Pts',(-18.5366894801541,-12.3271321503511,
115.332069133653)) ;
#164903 = CARTESIAN_POINT('Ctrl Pts',(-18.4628856098716,-12.3271321817739,
115.35630009352)) ;
#164904 = CARTESIAN_POINT('Ctrl Pts',(-18.3890817395891,-12.3271322131966,
115.380531053387)) ;
#164905 = CARTESIAN_POINT('Ctrl Pts',(-18.3974508093172,-12.3981381252086,
115.406021891207)) ;
#164906 = CARTESIAN_POINT('Ctrl Pts',(-18.4965924125013,-12.3341497286325,
115.672519382592)) ;
#164907 = CARTESIAN_POINT('Ctrl Pts',(-18.498786179809,-12.4097302348877,
115.679201245499)) ;
#164908 = CARTESIAN_POINT('Ctrl Pts',(-18.5725900497718,-12.4097302280834,
115.654970284658)) ;
#164909 = CARTESIAN_POINT('Ctrl Pts',(-18.6463939197346,-12.409730221279,
115.630739323818)) ;
#164910 = CARTESIAN_POINT('Ctrl Pts',(-18.644200152427,-12.3341497150238,
115.624057460911)) ;
#164911 = CARTESIAN_POINT('Ctrl Pts',(-18.6420063851193,-12.2585692087685,
115.617375598005)) ;
#164912 = CARTESIAN_POINT('Ctrl Pts',(-18.5682025151565,-12.2585692155729,
115.641606558845)) ;
#164913 = CARTESIAN_POINT('Ctrl Pts',(-18.4943986451936,-12.2585692223772,
115.665837519686)) ;
#164914 = CARTESIAN_POINT('Ctrl Pts',(-18.4965924125013,-12.3341497286325,
115.672519382592)) ;
#164915 = CARTESIAN_POINT('Ctrl Pts',(-18.5978909913726,-12.3478638226298,
115.945574148907)) ;
#164916 = CARTESIAN_POINT('Ctrl Pts',(-18.5937497675865,-12.4226010423524,
115.93296065095)) ;
#164917 = CARTESIAN_POINT('Ctrl Pts',(-18.6675536349436,-12.4226010571477,
115.908729682173)) ;
#164918 = CARTESIAN_POINT('Ctrl Pts',(-18.7413575023006,-12.422601071943,
115.884498713395)) ;
#164919 = CARTESIAN_POINT('Ctrl Pts',(-18.7454987260867,-12.3478638522204,
115.897112211353)) ;
#164920 = CARTESIAN_POINT('Ctrl Pts',(-18.7496399498727,-12.2731266324978,
115.90972570931)) ;
#164921 = CARTESIAN_POINT('Ctrl Pts',(-18.6758360825156,-12.2731266177025,
115.933956678087)) ;
#164922 = CARTESIAN_POINT('Ctrl Pts',(-18.6020322151586,-12.2731266029072,
115.958187646864)) ;
#164923 = CARTESIAN_POINT('Ctrl Pts',(-18.5978909913726,-12.3478638226298,
115.945574148907)) ;
#164924 = CARTESIAN_POINT('Ctrl Pts',(-18.6947567327243,-12.4382992209291,
116.205140753545)) ;
#164925 = CARTESIAN_POINT('Ctrl Pts',(-18.6845800908453,-12.5068353759983,
116.174144345737)) ;
#164926 = CARTESIAN_POINT('Ctrl Pts',(-18.7583839539381,-12.5068354072617,
116.149913363972)) ;
#164927 = CARTESIAN_POINT('Ctrl Pts',(-18.832187817031,-12.5068354385251,
116.125682382207)) ;
#164928 = CARTESIAN_POINT('Ctrl Pts',(-18.84236445891,-12.4382992834559,116.156678790014)) ;
#164929 = CARTESIAN_POINT('Ctrl Pts',(-18.852541100789,-12.3697631283867,
116.187675197822)) ;
#164930 = CARTESIAN_POINT('Ctrl Pts',(-18.7787372376961,-12.3697630971233,
116.211906179587)) ;
#164931 = CARTESIAN_POINT('Ctrl Pts',(-18.7049333746032,-12.3697630658599,
116.236137161352)) ;
#164932 = CARTESIAN_POINT('Ctrl Pts',(-18.6947567327243,-12.4382992209291,
116.205140753545)) ;
#164933 = CARTESIAN_POINT('Ctrl Pts',(-18.7809827309636,-12.5986984925073,
116.432334829973)) ;
#164934 = CARTESIAN_POINT('Ctrl Pts',(-18.7655036399242,-12.6561393028317,
116.385188017416)) ;
#164935 = CARTESIAN_POINT('Ctrl Pts',(-18.8393074978484,-12.65613934453,116.360957019908)) ;
#164936 = CARTESIAN_POINT('Ctrl Pts',(-18.9131113557727,-12.6561393862282,
116.3367260224)) ;
#164937 = CARTESIAN_POINT('Ctrl Pts',(-18.9285904468122,-12.5986985759038,
116.383872834956)) ;
#164938 = CARTESIAN_POINT('Ctrl Pts',(-18.9440695378517,-12.5412577655794,
116.431019647513)) ;
#164939 = CARTESIAN_POINT('Ctrl Pts',(-18.8702656799274,-12.5412577238812,
116.455250645021)) ;
#164940 = CARTESIAN_POINT('Ctrl Pts',(-18.7964618220031,-12.541257682183,
116.479481642529)) ;
#164941 = CARTESIAN_POINT('Ctrl Pts',(-18.7809827309636,-12.5986984925073,
116.432334829973)) ;
#164942 = CARTESIAN_POINT('Ctrl Pts',(-18.851332317076,-12.8181589219149,
116.61110894894)) ;
#164943 = CARTESIAN_POINT('Ctrl Pts',(-18.831652435789,-12.8603639864266,
116.551167206913)) ;
#164944 = CARTESIAN_POINT('Ctrl Pts',(-18.9054562882163,-12.8603640315663,
116.526936192662)) ;
#164945 = CARTESIAN_POINT('Ctrl Pts',(-18.9792601406437,-12.8603640767059,
116.502705178411)) ;
#164946 = CARTESIAN_POINT('Ctrl Pts',(-18.9989400219307,-12.8181590121942,
116.562646920439)) ;
#164947 = CARTESIAN_POINT('Ctrl Pts',(-19.0186199032177,-12.7759539476825,
116.622588662466)) ;
#164948 = CARTESIAN_POINT('Ctrl Pts',(-18.9448160507903,-12.7759539025429,
116.646819676717)) ;
#164949 = CARTESIAN_POINT('Ctrl Pts',(-18.871012198363,-12.7759538574032,
116.671050690968)) ;
#164950 = CARTESIAN_POINT('Ctrl Pts',(-18.851332317076,-12.8181589219149,
116.61110894894)) ;
#164951 = CARTESIAN_POINT('Ctrl Pts',(-18.9012299138603,-13.0797516616193,
116.727706681525)) ;
#164952 = CARTESIAN_POINT('Ctrl Pts',(-18.878768479364,-13.1037557901174,
116.659292777072)) ;
#164953 = CARTESIAN_POINT('Ctrl Pts',(-18.9525723269898,-13.1037558337794,
116.635061748196)) ;
#164954 = CARTESIAN_POINT('Ctrl Pts',(-19.0263761746156,-13.1037558774415,
116.61083071932)) ;
#164955 = CARTESIAN_POINT('Ctrl Pts',(-19.0488376091119,-13.0797517489434,
116.679244623774)) ;
#164956 = CARTESIAN_POINT('Ctrl Pts',(-19.0712990436082,-13.0557476204452,
116.747658528227)) ;
#164957 = CARTESIAN_POINT('Ctrl Pts',(-18.9974951959824,-13.0557475767832,
116.771889557103)) ;
#164958 = CARTESIAN_POINT('Ctrl Pts',(-18.9236913483566,-13.0557475331212,
116.796120585978)) ;
#164959 = CARTESIAN_POINT('Ctrl Pts',(-18.9012299138603,-13.0797516616193,
116.727706681525)) ;
#164960 = CARTESIAN_POINT('Ctrl Pts',(-18.9282094511315,-13.3661182947965,
116.774416487674)) ;
#164961 = CARTESIAN_POINT('Ctrl Pts',(-18.9045640621688,-13.3701640997913,
116.702396448778)) ;
#164962 = CARTESIAN_POINT('Ctrl Pts',(-18.9783679058639,-13.3701641367874,
116.67816540793)) ;
#164963 = CARTESIAN_POINT('Ctrl Pts',(-19.0521717495589,-13.3701641737835,
116.653934367082)) ;
#164964 = CARTESIAN_POINT('Ctrl Pts',(-19.0758171385217,-13.3661183687887,
116.725954405978)) ;
#164965 = CARTESIAN_POINT('Ctrl Pts',(-19.0994625274844,-13.3620725637939,
116.797974444874)) ;
#164966 = CARTESIAN_POINT('Ctrl Pts',(-19.0256586837894,-13.3620725267978,
116.822205485722)) ;
#164967 = CARTESIAN_POINT('Ctrl Pts',(-18.9518548400943,-13.3620724898017,
116.84643652657)) ;
#164968 = CARTESIAN_POINT('Ctrl Pts',(-18.9282094511315,-13.3661182947965,
116.774416487674)) ;
#164969 = CARTESIAN_POINT('Ctrl Pts',(-18.9308376699889,-13.656951267572,
116.746866353868)) ;
#164970 = CARTESIAN_POINT('Ctrl Pts',(-18.9077085946638,-13.6406962235438,
116.676418922825)) ;
#164971 = CARTESIAN_POINT('Ctrl Pts',(-18.9815124359412,-13.6406962503813,
116.652187874613)) ;
#164972 = CARTESIAN_POINT('Ctrl Pts',(-19.0553162772185,-13.6406962772189,
116.627956826401)) ;
#164973 = CARTESIAN_POINT('Ctrl Pts',(-19.0784453525436,-13.6569513212471,
116.698404257444)) ;
#164974 = CARTESIAN_POINT('Ctrl Pts',(-19.1015744278686,-13.6732063652754,
116.768851688486)) ;
#164975 = CARTESIAN_POINT('Ctrl Pts',(-19.0277705865913,-13.6732063384378,
116.793082736698)) ;
#164976 = CARTESIAN_POINT('Ctrl Pts',(-18.953966745314,-13.6732063116003,
116.81731378491)) ;
#164977 = CARTESIAN_POINT('Ctrl Pts',(-18.9308376699889,-13.656951267572,
116.746866353868)) ;
#164978 = CARTESIAN_POINT('Ctrl Pts',(-18.9097356138118,-13.9296721739865,
116.647159993684)) ;
#164979 = CARTESIAN_POINT('Ctrl Pts',(-18.8887782207473,-13.8943500486195,
116.58332715626)) ;
#164980 = CARTESIAN_POINT('Ctrl Pts',(-18.9625820610374,-13.8943500659771,
116.559096105041)) ;
#164981 = CARTESIAN_POINT('Ctrl Pts',(-19.0363859013275,-13.8943500833347,
116.534865053822)) ;
#164982 = CARTESIAN_POINT('Ctrl Pts',(-19.057343294392,-13.9296722087017,
116.598697891246)) ;
#164983 = CARTESIAN_POINT('Ctrl Pts',(-19.0783006874565,-13.9649943340687,
116.662530728671)) ;
#164984 = CARTESIAN_POINT('Ctrl Pts',(-19.0044968471664,-13.9649943167111,
116.68676177989)) ;
#164985 = CARTESIAN_POINT('Ctrl Pts',(-18.9306930068763,-13.9649942993535,
116.710992831109)) ;
#164986 = CARTESIAN_POINT('Ctrl Pts',(-18.9097356138118,-13.9296721739865,
116.647159993684)) ;
#164987 = CARTESIAN_POINT('Ctrl Pts',(-18.867193628718,-14.1660389555352,
116.482117526194)) ;
#164988 = CARTESIAN_POINT('Ctrl Pts',(-18.8499089973715,-14.1141591424512,
116.429471328224)) ;
#164989 = CARTESIAN_POINT('Ctrl Pts',(-18.9237128379045,-14.114159151286,
116.405240277745)) ;
#164990 = CARTESIAN_POINT('Ctrl Pts',(-18.9975166784375,-14.1141591601208,
116.381009227266)) ;
#164991 = CARTESIAN_POINT('Ctrl Pts',(-19.014801309784,-14.1660389732048,
116.433655425236)) ;
#164992 = CARTESIAN_POINT('Ctrl Pts',(-19.0320859411305,-14.2179187862889,
116.486301623206)) ;
#164993 = CARTESIAN_POINT('Ctrl Pts',(-18.9582821005975,-14.2179187774541,
116.510532673685)) ;
#164994 = CARTESIAN_POINT('Ctrl Pts',(-18.8844782600645,-14.2179187686193,
116.534763724164)) ;
#164995 = CARTESIAN_POINT('Ctrl Pts',(-18.867193628718,-14.1660389555352,
116.482117526194)) ;
#164996 = CARTESIAN_POINT('Ctrl Pts',(-18.8069801346924,-14.3487828478669,
116.263249434496)) ;
#164997 = CARTESIAN_POINT('Ctrl Pts',(-18.7946078964765,-14.2840645582721,
116.22556559327)) ;
#164998 = CARTESIAN_POINT('Ctrl Pts',(-18.8684117380704,-14.2840645612063,
116.201334546022)) ;
#164999 = CARTESIAN_POINT('Ctrl Pts',(-18.9422155796643,-14.2840645641405,
116.177103498774)) ;
#165000 = CARTESIAN_POINT('Ctrl Pts',(-18.9545878178802,-14.3487828537354,
116.214787340001)) ;
#165001 = CARTESIAN_POINT('Ctrl Pts',(-18.9669600560961,-14.4135011433302,
116.252471181227)) ;
#165002 = CARTESIAN_POINT('Ctrl Pts',(-18.8931562145022,-14.413501140396,
116.276702228475)) ;
#165003 = CARTESIAN_POINT('Ctrl Pts',(-18.8193523729083,-14.4135011374618,
116.300933275723)) ;
#165004 = CARTESIAN_POINT('Ctrl Pts',(-18.8069801346924,-14.3487828478669,
116.263249434496)) ;
#165005 = CARTESIAN_POINT('Ctrl Pts',(-18.73423883593,-14.4648357931477,116.006250091978)) ;
#165006 = CARTESIAN_POINT('Ctrl Pts',(-18.7276607481248,-14.391916747365,
115.986214297925)) ;
#165007 = CARTESIAN_POINT('Ctrl Pts',(-18.8014645910197,-14.3919167474485,
115.961983254639)) ;
#165008 = CARTESIAN_POINT('Ctrl Pts',(-18.8752684339146,-14.391916747532,
115.937752211354)) ;
#165009 = CARTESIAN_POINT('Ctrl Pts',(-18.8818465217198,-14.4648357933146,
115.957788005407)) ;
#165010 = CARTESIAN_POINT('Ctrl Pts',(-18.8884246095251,-14.5377548390973,
115.97782379946)) ;
#165011 = CARTESIAN_POINT('Ctrl Pts',(-18.8146207666302,-14.5377548390138,
116.002054842746)) ;
#165012 = CARTESIAN_POINT('Ctrl Pts',(-18.7408169237353,-14.5377548389303,
116.026285886031)) ;
#165013 = CARTESIAN_POINT('Ctrl Pts',(-18.73423883593,-14.4648357931477,116.006250091978)) ;
#165014 = CARTESIAN_POINT('Ctrl Pts',(-18.6548178924346,-14.5058959818021,
115.728874128576)) ;
#165015 = CARTESIAN_POINT('Ctrl Pts',(-18.6545098781287,-14.4300007264442,
115.727935966664)) ;
#165016 = CARTESIAN_POINT('Ctrl Pts',(-18.7283137220883,-14.4300007261889,
115.703704926622)) ;
#165017 = CARTESIAN_POINT('Ctrl Pts',(-18.8021175660479,-14.4300007259336,
115.67947388658)) ;
#165018 = CARTESIAN_POINT('Ctrl Pts',(-18.8024255803537,-14.5058959812914,
115.680412048491)) ;
#165019 = CARTESIAN_POINT('Ctrl Pts',(-18.8027335946595,-14.5817912366492,
115.681350210403)) ;
#165020 = CARTESIAN_POINT('Ctrl Pts',(-18.7289297506999,-14.5817912369046,
115.705581250445)) ;
#165021 = CARTESIAN_POINT('Ctrl Pts',(-18.6551259067404,-14.5817912371599,
115.729812290487)) ;
#165022 = CARTESIAN_POINT('Ctrl Pts',(-18.6548178924346,-14.5058959818021,
115.728874128576)) ;
#165023 = CARTESIAN_POINT('Ctrl Pts',(-18.5753873202692,-14.4694242942484,
115.451559578803)) ;
#165024 = CARTESIAN_POINT('Ctrl Pts',(-18.5813575551514,-14.3959630196689,
115.469743950894)) ;
#165025 = CARTESIAN_POINT('Ctrl Pts',(-18.6551613996072,-14.3959630205436,
115.445512912363)) ;
#165026 = CARTESIAN_POINT('Ctrl Pts',(-18.7289652440631,-14.3959630214183,
115.421281873832)) ;
#165027 = CARTESIAN_POINT('Ctrl Pts',(-18.7229950091809,-14.4694242959978,
115.403097501742)) ;
#165028 = CARTESIAN_POINT('Ctrl Pts',(-18.7170247742987,-14.5428855705773,
115.384913129651)) ;
#165029 = CARTESIAN_POINT('Ctrl Pts',(-18.6432209298428,-14.5428855697026,
115.409144168182)) ;
#165030 = CARTESIAN_POINT('Ctrl Pts',(-18.569417085387,-14.542885568828,115.433375206713)) ;
#165031 = CARTESIAN_POINT('Ctrl Pts',(-18.5753873202692,-14.4694242942484,
115.451559578803)) ;
#165032 = CARTESIAN_POINT('Ctrl Pts',(-18.5015763378576,-14.356381751671,
115.191027747652)) ;
#165033 = CARTESIAN_POINT('Ctrl Pts',(-18.5134490185545,-14.2907051755566,
115.227190017359)) ;
#165034 = CARTESIAN_POINT('Ctrl Pts',(-18.5872528625669,-14.2907051768879,
115.202958977478)) ;
#165035 = CARTESIAN_POINT('Ctrl Pts',(-18.6610567065792,-14.2907051782191,
115.178727937596)) ;
#165036 = CARTESIAN_POINT('Ctrl Pts',(-18.6491840258824,-14.3563817543336,
115.142565667889)) ;
#165037 = CARTESIAN_POINT('Ctrl Pts',(-18.6373113451855,-14.422058330448,
115.106403398181)) ;
#165038 = CARTESIAN_POINT('Ctrl Pts',(-18.5635075011732,-14.4220583291168,
115.130634438063)) ;
#165039 = CARTESIAN_POINT('Ctrl Pts',(-18.4897036571608,-14.4220583277855,
115.154865477944)) ;
#165040 = CARTESIAN_POINT('Ctrl Pts',(-18.5015763378576,-14.356381751671,
115.191027747652)) ;
#165041 = CARTESIAN_POINT('Ctrl Pts',(-18.4409491774712,-14.1778422798436,
114.971114813848)) ;
#165042 = CARTESIAN_POINT('Ctrl Pts',(-18.4578020115765,-14.1245364286659,
115.022445827339)) ;
#165043 = CARTESIAN_POINT('Ctrl Pts',(-18.5316058549156,-14.1245364288381,
114.998214785407)) ;
#165044 = CARTESIAN_POINT('Ctrl Pts',(-18.6054096982547,-14.1245364290103,
114.973983743475)) ;
#165045 = CARTESIAN_POINT('Ctrl Pts',(-18.5885568641494,-14.177842280188,
114.922652729984)) ;
#165046 = CARTESIAN_POINT('Ctrl Pts',(-18.5717040300441,-14.2311481313656,
114.871321716493)) ;
#165047 = CARTESIAN_POINT('Ctrl Pts',(-18.497900186705,-14.2311481311934,
114.895552758425)) ;
#165048 = CARTESIAN_POINT('Ctrl Pts',(-18.4240963433659,-14.2311481310212,
114.919783800358)) ;
#165049 = CARTESIAN_POINT('Ctrl Pts',(-18.4409491774712,-14.1778422798436,
114.971114813848)) ;
#165050 = CARTESIAN_POINT('Ctrl Pts',(-18.3972234500987,-13.9441247450056,
114.802451129126)) ;
#165051 = CARTESIAN_POINT('Ctrl Pts',(-18.4178884384501,-13.9070603957443,
114.865393349445)) ;
#165052 = CARTESIAN_POINT('Ctrl Pts',(-18.4916922810686,-13.9070603921811,
114.841162305317)) ;
#165053 = CARTESIAN_POINT('Ctrl Pts',(-18.565496123687,-13.9070603886178,
114.81693126119)) ;
#165054 = CARTESIAN_POINT('Ctrl Pts',(-18.5448311353355,-13.9441247378791,
114.753989040871)) ;
#165055 = CARTESIAN_POINT('Ctrl Pts',(-18.524166146984,-13.9811890871404,
114.691046820552)) ;
#165056 = CARTESIAN_POINT('Ctrl Pts',(-18.4503623043656,-13.9811890907036,
114.71527786468)) ;
#165057 = CARTESIAN_POINT('Ctrl Pts',(-18.3765584617472,-13.9811890942669,
114.739508908807)) ;
#165058 = CARTESIAN_POINT('Ctrl Pts',(-18.3972234500987,-13.9441247450056,
114.802451129126)) ;
#165059 = CARTESIAN_POINT('Ctrl Pts',(-18.374886126082,-13.6724643503177,
114.698927689739)) ;
#165060 = CARTESIAN_POINT('Ctrl Pts',(-18.3978753151959,-13.6543146170461,
114.768949050689)) ;
#165061 = CARTESIAN_POINT('Ctrl Pts',(-18.4716791577005,-13.6543146070783,
114.744718006215)) ;
#165062 = CARTESIAN_POINT('Ctrl Pts',(-18.545483000205,-13.6543145971105,
114.720486961741)) ;
#165063 = CARTESIAN_POINT('Ctrl Pts',(-18.5224938110911,-13.6724643303821,
114.650465600791)) ;
#165064 = CARTESIAN_POINT('Ctrl Pts',(-18.4995046219771,-13.6906140636538,
114.580444239841)) ;
#165065 = CARTESIAN_POINT('Ctrl Pts',(-18.4257007794726,-13.6906140736215,
114.604675284315)) ;
#165066 = CARTESIAN_POINT('Ctrl Pts',(-18.3518969369681,-13.6906140835893,
114.628906328789)) ;
#165067 = CARTESIAN_POINT('Ctrl Pts',(-18.374886126082,-13.6724643503177,
114.698927689739)) ;
#165068 = CARTESIAN_POINT('Ctrl Pts',(-18.3760656718454,-13.3835337156027,
114.66714876584)) ;
#165069 = CARTESIAN_POINT('Ctrl Pts',(-18.3997377752189,-13.3855315872837,
114.739250173553)) ;
#165070 = CARTESIAN_POINT('Ctrl Pts',(-18.4735416185495,-13.3855315707962,
114.715019131595)) ;
#165071 = CARTESIAN_POINT('Ctrl Pts',(-18.54734546188,-13.3855315543086,114.690788089637)) ;
#165072 = CARTESIAN_POINT('Ctrl Pts',(-18.5236733585065,-13.3835336826277,
114.618686681923)) ;
#165073 = CARTESIAN_POINT('Ctrl Pts',(-18.500001255133,-13.3815358109467,
114.546585274209)) ;
#165074 = CARTESIAN_POINT('Ctrl Pts',(-18.4261974118024,-13.3815358274342,
114.570816316167)) ;
#165075 = CARTESIAN_POINT('Ctrl Pts',(-18.3523935684719,-13.3815358439218,
114.595047358126)) ;
#165076 = CARTESIAN_POINT('Ctrl Pts',(-18.3760656718454,-13.3835337156027,
114.66714876584)) ;
#165077 = CARTESIAN_POINT('Ctrl Pts',(-18.401893543203,-13.0942320536069,
114.710077646052)) ;
#165078 = CARTESIAN_POINT('Ctrl Pts',(-18.4245363854837,-13.1164328568091,
114.779044090745)) ;
#165079 = CARTESIAN_POINT('Ctrl Pts',(-18.4983402311482,-13.1164328311838,
114.754813055896)) ;
#165080 = CARTESIAN_POINT('Ctrl Pts',(-18.5721440768125,-13.1164328055585,
114.730582021046)) ;
#165081 = CARTESIAN_POINT('Ctrl Pts',(-18.5495012345318,-13.0942320023563,
114.661615576353)) ;
#165082 = CARTESIAN_POINT('Ctrl Pts',(-18.526858392251,-13.0720311991542,
114.592649131659)) ;
#165083 = CARTESIAN_POINT('Ctrl Pts',(-18.4530545465866,-13.0720312247795,
114.616880166509)) ;
#165084 = CARTESIAN_POINT('Ctrl Pts',(-18.3792507009222,-13.0720312504048,
114.641111201359)) ;
#165085 = CARTESIAN_POINT('Ctrl Pts',(-18.401893543203,-13.0942320536069,
114.710077646052)) ;
#165086 = CARTESIAN_POINT('Ctrl Pts',(-18.4504581445536,-12.8318300831267,
114.822750132505)) ;
#165087 = CARTESIAN_POINT('Ctrl Pts',(-18.4704721032377,-12.8723837829672,
114.883709422054)) ;
#165088 = CARTESIAN_POINT('Ctrl Pts',(-18.544275952011,-12.8723837548031,
114.859478396673)) ;
#165089 = CARTESIAN_POINT('Ctrl Pts',(-18.6180798007842,-12.872383726639,
114.835247371292)) ;
#165090 = CARTESIAN_POINT('Ctrl Pts',(-18.5980658421001,-12.8318300267985,
114.774288081744)) ;
#165091 = CARTESIAN_POINT('Ctrl Pts',(-18.578051883416,-12.791276326958,114.713328792195)) ;
#165092 = CARTESIAN_POINT('Ctrl Pts',(-18.5042480346428,-12.7912763551221,
114.737559817576)) ;
#165093 = CARTESIAN_POINT('Ctrl Pts',(-18.4304441858696,-12.7912763832862,
114.761790842957)) ;
#165094 = CARTESIAN_POINT('Ctrl Pts',(-18.4504581445536,-12.8318300831267,
114.822750132505)) ;
#165095 = CARTESIAN_POINT('Ctrl Pts',(-18.5199862768258,-12.608937228869,
114.9989168848)) ;
#165096 = CARTESIAN_POINT('Ctrl Pts',(-18.5359115586374,-12.6651122393528,
115.047422724493)) ;
#165097 = CARTESIAN_POINT('Ctrl Pts',(-18.6097154118356,-12.6651122100812,
115.02319171259)) ;
#165098 = CARTESIAN_POINT('Ctrl Pts',(-18.6835192650338,-12.6651121808096,
114.998960700687)) ;
#165099 = CARTESIAN_POINT('Ctrl Pts',(-18.6675939832222,-12.6089371703258,
114.950454860994)) ;
#165100 = CARTESIAN_POINT('Ctrl Pts',(-18.6516687014106,-12.5527621598419,
114.901949021301)) ;
#165101 = CARTESIAN_POINT('Ctrl Pts',(-18.5778648482124,-12.5527621891136,
114.926180033204)) ;
#165102 = CARTESIAN_POINT('Ctrl Pts',(-18.5040609950142,-12.5527622183852,
114.950411045107)) ;
#165103 = CARTESIAN_POINT('Ctrl Pts',(-18.5199862768258,-12.608937228869,
114.9989168848)) ;
#165104 = CARTESIAN_POINT('Ctrl Pts',(-18.6052024537699,-12.4456165862493,
115.223155293183)) ;
#165105 = CARTESIAN_POINT('Ctrl Pts',(-18.6159317015771,-12.5132753292444,
115.255834851816)) ;
#165106 = CARTESIAN_POINT('Ctrl Pts',(-18.6897355588925,-12.5132753061601,
115.231603852453)) ;
#165107 = CARTESIAN_POINT('Ctrl Pts',(-18.7635394162079,-12.5132752830759,
115.207372853091)) ;
#165108 = CARTESIAN_POINT('Ctrl Pts',(-18.7528101684007,-12.4456165400809,
115.174693294458)) ;
#165109 = CARTESIAN_POINT('Ctrl Pts',(-18.7420809205935,-12.3779577970859,
115.142013735824)) ;
#165110 = CARTESIAN_POINT('Ctrl Pts',(-18.6682770632781,-12.3779578201701,
115.166244735187)) ;
#165111 = CARTESIAN_POINT('Ctrl Pts',(-18.5944732059627,-12.3779578432543,
115.19047573455)) ;
#165112 = CARTESIAN_POINT('Ctrl Pts',(-18.6052024537699,-12.4456165862493,
115.223155293183)) ;
#165113 = CARTESIAN_POINT('Ctrl Pts',(-18.7017273999509,-12.3507741827119,
115.481643821493)) ;
#165114 = CARTESIAN_POINT('Ctrl Pts',(-18.7064677514607,-12.4251525805178,
115.496082168485)) ;
#165115 = CARTESIAN_POINT('Ctrl Pts',(-18.7802716129605,-12.425152568096,
115.471851181868)) ;
#165116 = CARTESIAN_POINT('Ctrl Pts',(-18.8540754744602,-12.4251525556743,
115.44762019525)) ;
#165117 = CARTESIAN_POINT('Ctrl Pts',(-18.8493351229504,-12.3507741578684,
115.433181848258)) ;
#165118 = CARTESIAN_POINT('Ctrl Pts',(-18.8445947714406,-12.2763957600624,
115.418743501266)) ;
#165119 = CARTESIAN_POINT('Ctrl Pts',(-18.7707909099408,-12.2763957724842,
115.442974487884)) ;
#165120 = CARTESIAN_POINT('Ctrl Pts',(-18.696987048441,-12.276395784906,115.467205474501)) ;
#165121 = CARTESIAN_POINT('Ctrl Pts',(-18.7017273999509,-12.3507741827119,
115.481643821493)) ;
#165122 = CARTESIAN_POINT('Ctrl Pts',(-18.8032672046633,-12.3329811601702,
115.755325050277)) ;
#165123 = CARTESIAN_POINT('Ctrl Pts',(-18.8016616113288,-12.4087098331506,
115.750434673372)) ;
#165124 = CARTESIAN_POINT('Ctrl Pts',(-18.8754654761557,-12.4087098375423,
115.726203696888)) ;
#165125 = CARTESIAN_POINT('Ctrl Pts',(-18.9492693409827,-12.408709841934,
115.701972720404)) ;
#165126 = CARTESIAN_POINT('Ctrl Pts',(-18.9508749343172,-12.3329811689535,
115.70686309731)) ;
#165127 = CARTESIAN_POINT('Ctrl Pts',(-18.9524805276516,-12.2572524959731,
115.711753474215)) ;
#165128 = CARTESIAN_POINT('Ctrl Pts',(-18.8786766628248,-12.2572524915815,
115.735984450699)) ;
#165129 = CARTESIAN_POINT('Ctrl Pts',(-18.8048727979978,-12.2572524871898,
115.760215427183)) ;
#165130 = CARTESIAN_POINT('Ctrl Pts',(-18.8032672046633,-12.3329811601702,
115.755325050277)) ;
#165131 = CARTESIAN_POINT('Ctrl Pts',(-18.9021329558298,-12.3924859215409,
116.021180417224)) ;
#165132 = CARTESIAN_POINT('Ctrl Pts',(-18.8943523561467,-12.4641691937461,
115.997481967433)) ;
#165133 = CARTESIAN_POINT('Ctrl Pts',(-18.9681562216487,-12.4641692182498,
115.973250993006)) ;
#165134 = CARTESIAN_POINT('Ctrl Pts',(-19.0419600871508,-12.4641692427536,
115.949020018578)) ;
#165135 = CARTESIAN_POINT('Ctrl Pts',(-19.0497406868339,-12.3924859705485,
115.97271846837)) ;
#165136 = CARTESIAN_POINT('Ctrl Pts',(-19.057521286517,-12.3208026983433,
115.996416918161)) ;
#165137 = CARTESIAN_POINT('Ctrl Pts',(-18.983717421015,-12.3208026738395,
116.020647892588)) ;
#165138 = CARTESIAN_POINT('Ctrl Pts',(-18.9099135555129,-12.3208026493358,
116.044878867016)) ;
#165139 = CARTESIAN_POINT('Ctrl Pts',(-18.9021329558298,-12.3924859215409,
116.021180417224)) ;
#165140 = CARTESIAN_POINT('Ctrl Pts',(-18.9935434523282,-12.5254680767671,
116.264107206113)) ;
#165141 = CARTESIAN_POINT('Ctrl Pts',(-18.9801040226674,-12.5879710242858,
116.223172873407)) ;
#165142 = CARTESIAN_POINT('Ctrl Pts',(-19.0539078873367,-12.587971070974,
116.198941896443)) ;
#165143 = CARTESIAN_POINT('Ctrl Pts',(-19.127711752006,-12.5879711176621,
116.174710919479)) ;
#165144 = CARTESIAN_POINT('Ctrl Pts',(-19.1411511816667,-12.5254681701434,
116.215645252185)) ;
#165145 = CARTESIAN_POINT('Ctrl Pts',(-19.1545906113275,-12.4629652226247,
116.256579584891)) ;
#165146 = CARTESIAN_POINT('Ctrl Pts',(-19.0807867466582,-12.4629651759366,
116.280810561855)) ;
#165147 = CARTESIAN_POINT('Ctrl Pts',(-19.006982881989,-12.4629651292484,
116.305041538819)) ;
#165148 = CARTESIAN_POINT('Ctrl Pts',(-18.9935434523282,-12.5254680767671,
116.264107206113)) ;
#165149 = CARTESIAN_POINT('Ctrl Pts',(-19.0711087442326,-12.7232333026618,
116.464791322547)) ;
#165150 = CARTESIAN_POINT('Ctrl Pts',(-19.0529703146369,-12.7720201100749,
116.409544594361)) ;
#165151 = CARTESIAN_POINT('Ctrl Pts',(-19.1267741760621,-12.7720201789256,
116.385313607516)) ;
#165152 = CARTESIAN_POINT('Ctrl Pts',(-19.2005780374873,-12.7720202477763,
116.361082620671)) ;
#165153 = CARTESIAN_POINT('Ctrl Pts',(-19.218716467083,-12.7232334403633,
116.416329348858)) ;
#165154 = CARTESIAN_POINT('Ctrl Pts',(-19.2368548966787,-12.6744466329502,
116.471576077045)) ;
#165155 = CARTESIAN_POINT('Ctrl Pts',(-19.1630510352535,-12.6744465640995,
116.49580706389)) ;
#165156 = CARTESIAN_POINT('Ctrl Pts',(-19.0892471738283,-12.6744464952487,
116.520038050734)) ;
#165157 = CARTESIAN_POINT('Ctrl Pts',(-19.0711087442326,-12.7232333026618,
116.464791322547)) ;
#165158 = CARTESIAN_POINT('Ctrl Pts',(-19.1295684502511,-12.9691613747719,
116.607520966914)) ;
#165159 = CARTESIAN_POINT('Ctrl Pts',(-19.1080532454145,-13.0008491150667,
116.541989126278)) ;
#165160 = CARTESIAN_POINT('Ctrl Pts',(-19.1818571011284,-13.0008492011903,
116.517758122037)) ;
#165161 = CARTESIAN_POINT('Ctrl Pts',(-19.2556609568422,-13.0008492873139,
116.493527117796)) ;
#165162 = CARTESIAN_POINT('Ctrl Pts',(-19.2771761616788,-12.9691615470191,
116.559058958432)) ;
#165163 = CARTESIAN_POINT('Ctrl Pts',(-19.2986913665153,-12.9374738067243,
116.624590799068)) ;
#165164 = CARTESIAN_POINT('Ctrl Pts',(-19.2248875108014,-12.9374737206007,
116.648821803309)) ;
#165165 = CARTESIAN_POINT('Ctrl Pts',(-19.1510836550876,-12.937473634477,
116.673052807549)) ;
#165166 = CARTESIAN_POINT('Ctrl Pts',(-19.1295684502511,-12.9691613747719,
116.607520966914)) ;
#165167 = CARTESIAN_POINT('Ctrl Pts',(-19.1662325928152,-13.2488218748192,
116.683635238154)) ;
#165168 = CARTESIAN_POINT('Ctrl Pts',(-19.142861896445,-13.2610313034061,
116.612451869792)) ;
#165169 = CARTESIAN_POINT('Ctrl Pts',(-19.2166657448267,-13.2610314022195,
116.588220843219)) ;
#165170 = CARTESIAN_POINT('Ctrl Pts',(-19.2904695932085,-13.2610315010329,
116.563989816646)) ;
#165171 = CARTESIAN_POINT('Ctrl Pts',(-19.3138402895787,-13.248822072446,
116.635173185008)) ;
#165172 = CARTESIAN_POINT('Ctrl Pts',(-19.337210985949,-13.2366126438591,
116.706356553369)) ;
#165173 = CARTESIAN_POINT('Ctrl Pts',(-19.2634071375672,-13.2366125450457,
116.730587579942)) ;
#165174 = CARTESIAN_POINT('Ctrl Pts',(-19.1896032891855,-13.2366124462323,
116.754818606515)) ;
#165175 = CARTESIAN_POINT('Ctrl Pts',(-19.1662325928152,-13.2488218748192,
116.683635238154)) ;
#165176 = CARTESIAN_POINT('Ctrl Pts',(-19.1787171382524,-13.5399745855604,
116.686196204897)) ;
#165177 = CARTESIAN_POINT('Ctrl Pts',(-19.1551743858641,-13.5318747593251,
116.614488781738)) ;
#165178 = CARTESIAN_POINT('Ctrl Pts',(-19.2289782257133,-13.5318748625201,
116.590257729176)) ;
#165179 = CARTESIAN_POINT('Ctrl Pts',(-19.3027820655625,-13.5318749657152,
116.566026676614)) ;
#165180 = CARTESIAN_POINT('Ctrl Pts',(-19.3263248179508,-13.5399747919505,
116.637734099773)) ;
#165181 = CARTESIAN_POINT('Ctrl Pts',(-19.349867570339,-13.5480746181859,
116.709441522932)) ;
#165182 = CARTESIAN_POINT('Ctrl Pts',(-19.2760637304898,-13.5480745149908,
116.733672575494)) ;
#165183 = CARTESIAN_POINT('Ctrl Pts',(-19.2022598906406,-13.5480744117958,
116.757903628056)) ;
#165184 = CARTESIAN_POINT('Ctrl Pts',(-19.1787171382524,-13.5399745855604,
116.686196204897)) ;
#165185 = CARTESIAN_POINT('Ctrl Pts',(-19.1670328317494,-13.8224630035439,
116.615122093039)) ;
#165186 = CARTESIAN_POINT('Ctrl Pts',(-19.1450054514804,-13.7946290334854,
116.548030248902)) ;
#165187 = CARTESIAN_POINT('Ctrl Pts',(-19.2188092825817,-13.7946291324029,
116.523799169696)) ;
#165188 = CARTESIAN_POINT('Ctrl Pts',(-19.2926131136831,-13.7946292313203,
116.49956809049)) ;
#165189 = CARTESIAN_POINT('Ctrl Pts',(-19.3146404939522,-13.8224632013788,
116.566659934627)) ;
#165190 = CARTESIAN_POINT('Ctrl Pts',(-19.3366678742212,-13.8502971714373,
116.633751778763)) ;
#165191 = CARTESIAN_POINT('Ctrl Pts',(-19.2628640431198,-13.8502970725198,
116.657982857969)) ;
#165192 = CARTESIAN_POINT('Ctrl Pts',(-19.1890602120184,-13.8502969736024,
116.682213937175)) ;
#165193 = CARTESIAN_POINT('Ctrl Pts',(-19.1670328317494,-13.8224630035439,
116.615122093039)) ;
#165194 = CARTESIAN_POINT('Ctrl Pts',(-19.1329061805287,-14.0755037719121,
116.475781142016)) ;
#165195 = CARTESIAN_POINT('Ctrl Pts',(-19.1139613863318,-14.0299625115252,
116.418078357712)) ;
#165196 = CARTESIAN_POINT('Ctrl Pts',(-19.1877652093854,-14.0299625976229,
116.393847253993)) ;
#165197 = CARTESIAN_POINT('Ctrl Pts',(-19.2615690324389,-14.0299626837205,
116.369616150274)) ;
#165198 = CARTESIAN_POINT('Ctrl Pts',(-19.2805138266358,-14.0755039441074,
116.427318934579)) ;
#165199 = CARTESIAN_POINT('Ctrl Pts',(-19.2994586208326,-14.1210452044942,
116.485021718884)) ;
#165200 = CARTESIAN_POINT('Ctrl Pts',(-19.2256547977791,-14.1210451183966,
116.509252822602)) ;
#165201 = CARTESIAN_POINT('Ctrl Pts',(-19.1518509747255,-14.121045032299,
116.533483926321)) ;
#165202 = CARTESIAN_POINT('Ctrl Pts',(-19.1329061805287,-14.0755037719121,
116.475781142016)) ;
#165203 = CARTESIAN_POINT('Ctrl Pts',(-19.0790275217248,-14.2826234653696,
116.276041341228)) ;
#165204 = CARTESIAN_POINT('Ctrl Pts',(-19.0645534585991,-14.2225542775354,
116.231955682423)) ;
#165205 = CARTESIAN_POINT('Ctrl Pts',(-19.1383572751289,-14.2225543432862,
116.207724558834)) ;
#165206 = CARTESIAN_POINT('Ctrl Pts',(-19.2121610916587,-14.222554409037,
116.183493435246)) ;
#165207 = CARTESIAN_POINT('Ctrl Pts',(-19.2266351547843,-14.2826235968712,
116.22757909405)) ;
#165208 = CARTESIAN_POINT('Ctrl Pts',(-19.24110921791,-14.3426927847054,116.271664752854)) ;
#165209 = CARTESIAN_POINT('Ctrl Pts',(-19.1673054013802,-14.3426927189546,
116.295895876443)) ;
#165210 = CARTESIAN_POINT('Ctrl Pts',(-19.0935015848505,-14.3426926532038,
116.320127000032)) ;
#165211 = CARTESIAN_POINT('Ctrl Pts',(-19.0790275217248,-14.2826234653696,
116.276041341228)) ;
#165212 = CARTESIAN_POINT('Ctrl Pts',(-19.0110858794714,-14.4260980932151,
116.033863734951)) ;
#165213 = CARTESIAN_POINT('Ctrl Pts',(-19.0020631113687,-14.3559233104312,
116.006381841212)) ;
#165214 = CARTESIAN_POINT('Ctrl Pts',(-19.0758669235952,-14.3559233508218,
115.982150704516)) ;
#165215 = CARTESIAN_POINT('Ctrl Pts',(-19.1496707358216,-14.3559233912124,
115.95791956782)) ;
#165216 = CARTESIAN_POINT('Ctrl Pts',(-19.1586935039242,-14.4260981739963,
115.985401461558)) ;
#165217 = CARTESIAN_POINT('Ctrl Pts',(-19.1677162720268,-14.4962729567803,
116.012883355297)) ;
#165218 = CARTESIAN_POINT('Ctrl Pts',(-19.0939124598004,-14.4962729163896,
116.037114491993)) ;
#165219 = CARTESIAN_POINT('Ctrl Pts',(-19.020108647574,-14.496272875999,116.061345628689)) ;
#165220 = CARTESIAN_POINT('Ctrl Pts',(-19.0110858794714,-14.4260980932151,
116.033863734951)) ;
#165221 = CARTESIAN_POINT('Ctrl Pts',(-18.9333061628567,-14.4987580687002,
115.761347729046)) ;
#165222 = CARTESIAN_POINT('Ctrl Pts',(-18.9304370258749,-14.4234055963817,
115.752608802777)) ;
#165223 = CARTESIAN_POINT('Ctrl Pts',(-19.0042408365051,-14.423405608344,
115.728377661219)) ;
#165224 = CARTESIAN_POINT('Ctrl Pts',(-19.0780446471354,-14.4234056203062,
115.704146519661)) ;
#165225 = CARTESIAN_POINT('Ctrl Pts',(-19.0809137841172,-14.4987580926247,
115.71288544593)) ;
#165226 = CARTESIAN_POINT('Ctrl Pts',(-19.083782921099,-14.5741105649432,
115.721624372199)) ;
#165227 = CARTESIAN_POINT('Ctrl Pts',(-19.0099791104687,-14.5741105529809,
115.745855513757)) ;
#165228 = CARTESIAN_POINT('Ctrl Pts',(-18.9361752998385,-14.5741105410186,
115.770086655315)) ;
#165229 = CARTESIAN_POINT('Ctrl Pts',(-18.9333061628567,-14.4987580687002,
115.761347729046)) ;
#165230 = CARTESIAN_POINT('Ctrl Pts',(-18.8531245622656,-14.4933400096758,
115.481718981289)) ;
#165231 = CARTESIAN_POINT('Ctrl Pts',(-18.8565818821195,-14.4182534186233,
115.492249421715)) ;
#165232 = CARTESIAN_POINT('Ctrl Pts',(-18.930385693833,-14.4182534027344,
115.468018283457)) ;
#165233 = CARTESIAN_POINT('Ctrl Pts',(-19.0041895055465,-14.4182533868454,
115.443787145198)) ;
#165234 = CARTESIAN_POINT('Ctrl Pts',(-19.0007321856926,-14.493339977898,
115.433256704772)) ;
#165235 = CARTESIAN_POINT('Ctrl Pts',(-18.9972748658387,-14.5684265689505,
115.422726264346)) ;
#165236 = CARTESIAN_POINT('Ctrl Pts',(-18.9234710541252,-14.5684265848394,
115.446957402605)) ;
#165237 = CARTESIAN_POINT('Ctrl Pts',(-18.8496672424117,-14.5684266007284,
115.471188540863)) ;
#165238 = CARTESIAN_POINT('Ctrl Pts',(-18.8531245622656,-14.4933400096758,
115.481718981289)) ;
#165239 = CARTESIAN_POINT('Ctrl Pts',(-18.7765257054284,-14.4113489345642,
115.212967154144)) ;
#165240 = CARTESIAN_POINT('Ctrl Pts',(-18.7860695067199,-14.3418743538158,
115.242036034905)) ;
#165241 = CARTESIAN_POINT('Ctrl Pts',(-18.8598733219957,-14.3418743129385,
115.217804907497)) ;
#165242 = CARTESIAN_POINT('Ctrl Pts',(-18.9336771372715,-14.3418742720612,
115.193573780088)) ;
#165243 = CARTESIAN_POINT('Ctrl Pts',(-18.9241333359799,-14.4113488528096,
115.164504899327)) ;
#165244 = CARTESIAN_POINT('Ctrl Pts',(-18.9145895346884,-14.4808234335579,
115.135436018566)) ;
#165245 = CARTESIAN_POINT('Ctrl Pts',(-18.8407857194126,-14.4808234744352,
115.159667145975)) ;
#165246 = CARTESIAN_POINT('Ctrl Pts',(-18.7669819041369,-14.4808235153125,
115.183898273383)) ;
#165247 = CARTESIAN_POINT('Ctrl Pts',(-18.7765257054284,-14.4113489345642,
115.212967154144)) ;
#165248 = CARTESIAN_POINT('Ctrl Pts',(-18.709586077983,-14.2570982982162,
114.973460633558)) ;
#165249 = CARTESIAN_POINT('Ctrl Pts',(-18.7245548673285,-14.1982882942638,
115.019053152496)) ;
#165250 = CARTESIAN_POINT('Ctrl Pts',(-18.798358688464,-14.1982882346942,
114.994822042935)) ;
#165251 = CARTESIAN_POINT('Ctrl Pts',(-18.8721625095994,-14.1982881751247,
114.970590933375)) ;
#165252 = CARTESIAN_POINT('Ctrl Pts',(-18.8571937202539,-14.2570981790771,
114.924998414437)) ;
#165253 = CARTESIAN_POINT('Ctrl Pts',(-18.8422249309084,-14.3159081830295,
114.879405895499)) ;
#165254 = CARTESIAN_POINT('Ctrl Pts',(-18.768421109773,-14.3159082425991,
114.903637005059)) ;
#165255 = CARTESIAN_POINT('Ctrl Pts',(-18.6946172886376,-14.3159083021687,
114.92786811462)) ;
#165256 = CARTESIAN_POINT('Ctrl Pts',(-18.709586077983,-14.2570982982162,
114.973460633558)) ;
#165257 = CARTESIAN_POINT('Ctrl Pts',(-18.6586281342935,-14.044633200838,
114.782977159409)) ;
#165258 = CARTESIAN_POINT('Ctrl Pts',(-18.6779070569103,-14.000569128791,
114.841697648763)) ;
#165259 = CARTESIAN_POINT('Ctrl Pts',(-18.7517108846106,-14.0005690563028,
114.817466559198)) ;
#165260 = CARTESIAN_POINT('Ctrl Pts',(-18.8255147123109,-14.0005689838146,
114.793235469633)) ;
#165261 = CARTESIAN_POINT('Ctrl Pts',(-18.8062357896941,-14.0446330558616,
114.734514980278)) ;
#165262 = CARTESIAN_POINT('Ctrl Pts',(-18.7869568670774,-14.0886971279086,
114.675794490924)) ;
#165263 = CARTESIAN_POINT('Ctrl Pts',(-18.713153039377,-14.0886972003968,
114.700025580489)) ;
#165264 = CARTESIAN_POINT('Ctrl Pts',(-18.6393492116767,-14.088697272885,
114.724256670054)) ;
#165265 = CARTESIAN_POINT('Ctrl Pts',(-18.6586281342935,-14.044633200838,
114.782977159409)) ;
#165266 = CARTESIAN_POINT('Ctrl Pts',(-18.6271547830504,-13.785410087343,
114.651525939314)) ;
#165267 = CARTESIAN_POINT('Ctrl Pts',(-18.6493967146293,-13.7593778661625,
114.719271275738)) ;
#165268 = CARTESIAN_POINT('Ctrl Pts',(-18.7232005497368,-13.7593777900464,
114.695040208734)) ;
#165269 = CARTESIAN_POINT('Ctrl Pts',(-18.7970043848443,-13.7593777139303,
114.67080914173)) ;
#165270 = CARTESIAN_POINT('Ctrl Pts',(-18.7747624532654,-13.7854099351107,
114.603063805305)) ;
#165271 = CARTESIAN_POINT('Ctrl Pts',(-18.7525205216865,-13.8114421562912,
114.535318468881)) ;
#165272 = CARTESIAN_POINT('Ctrl Pts',(-18.678716686579,-13.8114422324073,
114.559549535885)) ;
#165273 = CARTESIAN_POINT('Ctrl Pts',(-18.6049128514715,-13.8114423085234,
114.583780602889)) ;
#165274 = CARTESIAN_POINT('Ctrl Pts',(-18.6271547830504,-13.785410087343,
114.651525939314)) ;
#165275 = CARTESIAN_POINT('Ctrl Pts',(-18.6186793550776,-13.5013707464361,
114.590343252288)) ;
#165276 = CARTESIAN_POINT('Ctrl Pts',(-18.6422784319961,-13.4951307017579,
114.662222234314)) ;
#165277 = CARTESIAN_POINT('Ctrl Pts',(-18.7160822738892,-13.4951306279953,
114.637991187977)) ;
#165278 = CARTESIAN_POINT('Ctrl Pts',(-18.7898861157823,-13.4951305542326,
114.613760141641)) ;
#165279 = CARTESIAN_POINT('Ctrl Pts',(-18.7662870388639,-13.5013705989108,
114.541881159615)) ;
#165280 = CARTESIAN_POINT('Ctrl Pts',(-18.7426879619454,-13.507610643589,
114.470002177589)) ;
#165281 = CARTESIAN_POINT('Ctrl Pts',(-18.6688841200523,-13.5076107173517,
114.494233223926)) ;
#165282 = CARTESIAN_POINT('Ctrl Pts',(-18.5950802781592,-13.5076107911143,
114.518464270262)) ;
#165283 = CARTESIAN_POINT('Ctrl Pts',(-18.6186793550776,-13.5013707464361,
114.590343252288)) ;
#165284 = CARTESIAN_POINT('Ctrl Pts',(-18.6346005883907,-13.209135818783,
114.60317395719)) ;
#165285 = CARTESIAN_POINT('Ctrl Pts',(-18.657861930824,-13.2232901390273,
114.674024254277)) ;
#165286 = CARTESIAN_POINT('Ctrl Pts',(-18.7316657782842,-13.2232900762476,
114.649793224897)) ;
#165287 = CARTESIAN_POINT('Ctrl Pts',(-18.8054696257443,-13.2232900134679,
114.625562195517)) ;
#165288 = CARTESIAN_POINT('Ctrl Pts',(-18.7822082833109,-13.2091356932237,
114.55471189843)) ;
#165289 = CARTESIAN_POINT('Ctrl Pts',(-18.7589469408775,-13.1949813729794,
114.483861601343)) ;
#165290 = CARTESIAN_POINT('Ctrl Pts',(-18.6851430934174,-13.1949814357591,
114.508092630724)) ;
#165291 = CARTESIAN_POINT('Ctrl Pts',(-18.6113392459573,-13.1949814985388,
114.532323660104)) ;
#165292 = CARTESIAN_POINT('Ctrl Pts',(-18.6346005883907,-13.209135818783,
114.60317395719)) ;
#165293 = CARTESIAN_POINT('Ctrl Pts',(-18.6739150075071,-12.935507537228,
114.68774371454)) ;
#165294 = CARTESIAN_POINT('Ctrl Pts',(-18.6951942663002,-12.9687880563088,
114.752556904557)) ;
#165295 = CARTESIAN_POINT('Ctrl Pts',(-18.7689981179826,-12.9687880043352,
114.728325888037)) ;
#165296 = CARTESIAN_POINT('Ctrl Pts',(-18.842801969665,-12.9687879523617,
114.704094871517)) ;
#165297 = CARTESIAN_POINT('Ctrl Pts',(-18.8215227108719,-12.9355074332809,
114.639281681501)) ;
#165298 = CARTESIAN_POINT('Ctrl Pts',(-18.8002434520789,-12.9022269142001,
114.574468491484)) ;
#165299 = CARTESIAN_POINT('Ctrl Pts',(-18.7264396003964,-12.9022269661736,
114.598699508004)) ;
#165300 = CARTESIAN_POINT('Ctrl Pts',(-18.652635748714,-12.9022270181472,
114.622930524524)) ;
#165301 = CARTESIAN_POINT('Ctrl Pts',(-18.6739150075071,-12.935507537228,
114.68774371454)) ;
#165302 = CARTESIAN_POINT('Ctrl Pts',(-18.7355531362002,-12.6930981261278,
114.839845302761)) ;
#165303 = CARTESIAN_POINT('Ctrl Pts',(-18.7532986257394,-12.7433547054021,
114.893895201602)) ;
#165304 = CARTESIAN_POINT('Ctrl Pts',(-18.8271024793354,-12.7433546700873,
114.869664190911)) ;
#165305 = CARTESIAN_POINT('Ctrl Pts',(-18.9009063329314,-12.7433546347726,
114.845433180219)) ;
#165306 = CARTESIAN_POINT('Ctrl Pts',(-18.8831608433922,-12.6930980554983,
114.791383281379)) ;
#165307 = CARTESIAN_POINT('Ctrl Pts',(-18.865415353853,-12.642841476224,114.737333382538)) ;
#165308 = CARTESIAN_POINT('Ctrl Pts',(-18.791611500257,-12.6428415115388,
114.761564393229)) ;
#165309 = CARTESIAN_POINT('Ctrl Pts',(-18.7178076466611,-12.6428415468535,
114.78579540392)) ;
#165310 = CARTESIAN_POINT('Ctrl Pts',(-18.7355531362002,-12.6930981261278,
114.839845302761)) ;
#165311 = CARTESIAN_POINT('Ctrl Pts',(-18.8147640138156,-12.5044954568888,
115.045790079313)) ;
#165312 = CARTESIAN_POINT('Ctrl Pts',(-18.8277365331886,-12.5679966014652,
115.085302281002)) ;
#165313 = CARTESIAN_POINT('Ctrl Pts',(-18.901540387397,-12.5679965800268,
115.061071272176)) ;
#165314 = CARTESIAN_POINT('Ctrl Pts',(-18.9753442416054,-12.5679965585884,
115.03684026335)) ;
#165315 = CARTESIAN_POINT('Ctrl Pts',(-18.9623717222324,-12.504495414012,
114.997328061661)) ;
#165316 = CARTESIAN_POINT('Ctrl Pts',(-18.9493992028594,-12.4409942694355,
114.957815859971)) ;
#165317 = CARTESIAN_POINT('Ctrl Pts',(-18.875595348651,-12.440994290874,114.982046868797)) ;
#165318 = CARTESIAN_POINT('Ctrl Pts',(-18.8017914944426,-12.4409943123124,
115.006277877623)) ;
#165319 = CARTESIAN_POINT('Ctrl Pts',(-18.8147640138156,-12.5044954568888,
115.045790079313)) ;
#165320 = CARTESIAN_POINT('Ctrl Pts',(-18.9079928918168,-12.3799491141259,
115.294083315744)) ;
#165321 = CARTESIAN_POINT('Ctrl Pts',(-18.9152137115967,-12.4522433406483,
115.316076768303)) ;
#165322 = CARTESIAN_POINT('Ctrl Pts',(-18.9890175640882,-12.4522433323691,
115.291845754247)) ;
#165323 = CARTESIAN_POINT('Ctrl Pts',(-19.0628214165796,-12.4522433240898,
115.267614740191)) ;
#165324 = CARTESIAN_POINT('Ctrl Pts',(-19.0556005967997,-12.3799490975675,
115.245621287633)) ;
#165325 = CARTESIAN_POINT('Ctrl Pts',(-19.0483797770198,-12.3076548710451,
115.223627835074)) ;
#165326 = CARTESIAN_POINT('Ctrl Pts',(-18.9745759245284,-12.3076548793244,
115.247858849129)) ;
#165327 = CARTESIAN_POINT('Ctrl Pts',(-18.9007720720369,-12.3076548876036,
115.272089863185)) ;
#165328 = CARTESIAN_POINT('Ctrl Pts',(-18.9079928918168,-12.3799491141259,
115.294083315744)) ;
#165329 = CARTESIAN_POINT('Ctrl Pts',(-19.0076357668637,-12.3308555788642,
115.562256980437)) ;
#165330 = CARTESIAN_POINT('Ctrl Pts',(-19.0086410153361,-12.4066867963508,
115.56531880554)) ;
#165331 = CARTESIAN_POINT('Ctrl Pts',(-19.0824448660441,-12.4066867960904,
115.541087786052)) ;
#165332 = CARTESIAN_POINT('Ctrl Pts',(-19.1562487167521,-12.4066867958299,
115.516856766564)) ;
#165333 = CARTESIAN_POINT('Ctrl Pts',(-19.1552434682797,-12.3308555783432,
115.513794941461)) ;
#165334 = CARTESIAN_POINT('Ctrl Pts',(-19.1542382198073,-12.2550243608565,
115.510733116358)) ;
#165335 = CARTESIAN_POINT('Ctrl Pts',(-19.0804343690993,-12.255024361117,
115.534964135846)) ;
#165336 = CARTESIAN_POINT('Ctrl Pts',(-19.0066305183913,-12.2550243613775,
115.559195155333)) ;
#165337 = CARTESIAN_POINT('Ctrl Pts',(-19.0076357668637,-12.3308555788642,
115.562256980437)) ;
#165338 = CARTESIAN_POINT('Ctrl Pts',(-19.1085420809616,-12.3590358220882,
115.83413499983)) ;
#165339 = CARTESIAN_POINT('Ctrl Pts',(-19.1032370638223,-12.4330140750954,
115.81797677389)) ;
#165340 = CARTESIAN_POINT('Ctrl Pts',(-19.1770409119809,-12.4330140793916,
115.793745746637)) ;
#165341 = CARTESIAN_POINT('Ctrl Pts',(-19.2508447601395,-12.4330140836878,
115.769514719384)) ;
#165342 = CARTESIAN_POINT('Ctrl Pts',(-19.2561497772788,-12.3590358306806,
115.785672945324)) ;
#165343 = CARTESIAN_POINT('Ctrl Pts',(-19.2614547944181,-12.2850575776733,
115.801831171264)) ;
#165344 = CARTESIAN_POINT('Ctrl Pts',(-19.1876509462595,-12.2850575733772,
115.826062198516)) ;
#165345 = CARTESIAN_POINT('Ctrl Pts',(-19.1138470981009,-12.285057569081,
115.850293225769)) ;
#165346 = CARTESIAN_POINT('Ctrl Pts',(-19.1085420809616,-12.3590358220882,
115.83413499983)) ;
#165347 = CARTESIAN_POINT('Ctrl Pts',(-19.2039631545433,-12.4632787296656,
116.089280063795)) ;
#165348 = CARTESIAN_POINT('Ctrl Pts',(-19.1927217645793,-12.5300899100408,
116.055040603927)) ;
#165349 = CARTESIAN_POINT('Ctrl Pts',(-19.2665256103156,-12.5300899147854,
116.030809569297)) ;
#165350 = CARTESIAN_POINT('Ctrl Pts',(-19.3403294560519,-12.5300899195299,
116.006578534666)) ;
#165351 = CARTESIAN_POINT('Ctrl Pts',(-19.3515708460159,-12.4632787391547,
116.040817994534)) ;
#165352 = CARTESIAN_POINT('Ctrl Pts',(-19.3628122359799,-12.3964675587795,
116.075057454402)) ;
#165353 = CARTESIAN_POINT('Ctrl Pts',(-19.2890083902436,-12.396467554035,
116.099288489033)) ;
#165354 = CARTESIAN_POINT('Ctrl Pts',(-19.2152045445073,-12.3964675492904,
116.123519523663)) ;
#165355 = CARTESIAN_POINT('Ctrl Pts',(-19.2039631545433,-12.4632787296656,
116.089280063795)) ;
#165356 = CARTESIAN_POINT('Ctrl Pts',(-19.2877487102314,-12.6363587431469,
116.308941746476)) ;
#165357 = CARTESIAN_POINT('Ctrl Pts',(-19.2713752688425,-12.6911848598895,
116.259070885909)) ;
#165358 = CARTESIAN_POINT('Ctrl Pts',(-19.3451791128408,-12.6911848623011,
116.234839845984)) ;
#165359 = CARTESIAN_POINT('Ctrl Pts',(-19.4189829568391,-12.6911848647128,
116.21060880606)) ;
#165360 = CARTESIAN_POINT('Ctrl Pts',(-19.435356398228,-12.6363587479702,
116.260479666627)) ;
#165361 = CARTESIAN_POINT('Ctrl Pts',(-19.451729839617,-12.5815326312277,
116.310350527194)) ;
#165362 = CARTESIAN_POINT('Ctrl Pts',(-19.3779259956186,-12.5815326288161,
116.334581567118)) ;
#165363 = CARTESIAN_POINT('Ctrl Pts',(-19.3041221516203,-12.5815326264044,
116.358812607043)) ;
#165364 = CARTESIAN_POINT('Ctrl Pts',(-19.2877487102314,-12.6363587431469,
116.308941746476)) ;
#165365 = CARTESIAN_POINT('Ctrl Pts',(-19.3543294992995,-12.864158222785,
116.476393219925)) ;
#165366 = CARTESIAN_POINT('Ctrl Pts',(-19.3340139079031,-12.9031598637825,
116.414515206428)) ;
#165367 = CARTESIAN_POINT('Ctrl Pts',(-19.4078177511336,-12.9031598633717,
116.390284164164)) ;
#165368 = CARTESIAN_POINT('Ctrl Pts',(-19.481621594364,-12.9031598629608,
116.366053121901)) ;
#165369 = CARTESIAN_POINT('Ctrl Pts',(-19.5019371857604,-12.8641582219634,
116.427931135398)) ;
#165370 = CARTESIAN_POINT('Ctrl Pts',(-19.5222527771567,-12.8251565809659,
116.489809148895)) ;
#165371 = CARTESIAN_POINT('Ctrl Pts',(-19.4484489339263,-12.8251565813767,
116.514040191159)) ;
#165372 = CARTESIAN_POINT('Ctrl Pts',(-19.3746450906959,-12.8251565817875,
116.538271233422)) ;
#165373 = CARTESIAN_POINT('Ctrl Pts',(-19.3543294992995,-12.864158222785,
116.476393219925)) ;
#165374 = CARTESIAN_POINT('Ctrl Pts',(-19.4003945437516,-13.1343225359667,
116.580991063038)) ;
#165375 = CARTESIAN_POINT('Ctrl Pts',(-19.3775707263678,-13.1545167875365,
116.511473397833)) ;
#165376 = CARTESIAN_POINT('Ctrl Pts',(-19.4513745694738,-13.1545167844315,
116.487242355191)) ;
#165377 = CARTESIAN_POINT('Ctrl Pts',(-19.5251784125798,-13.1545167813264,
116.463011312549)) ;
#165378 = CARTESIAN_POINT('Ctrl Pts',(-19.5480022299636,-13.1343225297566,
116.532528977753)) ;
#165379 = CARTESIAN_POINT('Ctrl Pts',(-19.5708260473473,-13.1141282781868,
116.602046642958)) ;
#165380 = CARTESIAN_POINT('Ctrl Pts',(-19.4970222042414,-13.1141282812919,
116.6262776856)) ;
#165381 = CARTESIAN_POINT('Ctrl Pts',(-19.4232183611354,-13.114128284397,
116.650508728242)) ;
#165382 = CARTESIAN_POINT('Ctrl Pts',(-19.4003945437516,-13.1343225359667,
116.580991063038)) ;
#165383 = CARTESIAN_POINT('Ctrl Pts',(-19.4225349879933,-13.4205967944479,
116.613269030922)) ;
#165384 = CARTESIAN_POINT('Ctrl Pts',(-19.3988592410925,-13.4208311388444,
116.541156525867)) ;
#165385 = CARTESIAN_POINT('Ctrl Pts',(-19.4726630845397,-13.4208311356135,
116.516925484264)) ;
#165386 = CARTESIAN_POINT('Ctrl Pts',(-19.5464669279869,-13.4208311323827,
116.492694442662)) ;
#165387 = CARTESIAN_POINT('Ctrl Pts',(-19.5701426748878,-13.4205967879863,
116.564806947716)) ;
#165388 = CARTESIAN_POINT('Ctrl Pts',(-19.5938184217886,-13.4203624435898,
116.636919452771)) ;
#165389 = CARTESIAN_POINT('Ctrl Pts',(-19.5200145783414,-13.4203624468207,
116.661150494374)) ;
#165390 = CARTESIAN_POINT('Ctrl Pts',(-19.4462107348942,-13.4203624500515,
116.685381535977)) ;
#165391 = CARTESIAN_POINT('Ctrl Pts',(-19.4225349879933,-13.4205967944479,
116.613269030922)) ;
#165392 = CARTESIAN_POINT('Ctrl Pts',(-19.4206705194364,-13.7102521447362,
116.57197231337)) ;
#165393 = CARTESIAN_POINT('Ctrl Pts',(-19.3978270561401,-13.6902603542672,
116.502394809927)) ;
#165394 = CARTESIAN_POINT('Ctrl Pts',(-19.4716308997194,-13.6902603532413,
116.478163768727)) ;
#165395 = CARTESIAN_POINT('Ctrl Pts',(-19.5454347432987,-13.6902603522153,
116.453932727526)) ;
#165396 = CARTESIAN_POINT('Ctrl Pts',(-19.568278206595,-13.7102521426842,
116.523510230969)) ;
#165397 = CARTESIAN_POINT('Ctrl Pts',(-19.5911216698912,-13.7302439331532,
116.593087734412)) ;
#165398 = CARTESIAN_POINT('Ctrl Pts',(-19.5173178263119,-13.7302439341791,
116.617318775612)) ;
#165399 = CARTESIAN_POINT('Ctrl Pts',(-19.4435139827326,-13.7302439352051,
116.641549816813)) ;
#165400 = CARTESIAN_POINT('Ctrl Pts',(-19.4206705194364,-13.7102521447362,
116.57197231337)) ;
#165401 = CARTESIAN_POINT('Ctrl Pts',(-19.3953354743405,-13.9772668612757,
116.459412299705)) ;
#165402 = CARTESIAN_POINT('Ctrl Pts',(-19.3749601067379,-13.9386012749513,
116.39735221759)) ;
#165403 = CARTESIAN_POINT('Ctrl Pts',(-19.4487639498612,-13.9386012773307,
116.373121175)) ;
#165404 = CARTESIAN_POINT('Ctrl Pts',(-19.5225677929844,-13.9386012797101,
116.34889013241)) ;
#165405 = CARTESIAN_POINT('Ctrl Pts',(-19.5429431605871,-13.9772668660344,
116.410950214526)) ;
#165406 = CARTESIAN_POINT('Ctrl Pts',(-19.5633185281897,-14.0159324523587,
116.473010296642)) ;
#165407 = CARTESIAN_POINT('Ctrl Pts',(-19.4895146850664,-14.0159324499793,
116.497241339231)) ;
#165408 = CARTESIAN_POINT('Ctrl Pts',(-19.4157108419431,-14.0159324476,116.521472381821)) ;
#165409 = CARTESIAN_POINT('Ctrl Pts',(-19.3953354743405,-13.9772668612757,
116.459412299705)) ;
#165410 = CARTESIAN_POINT('Ctrl Pts',(-19.3490326024128,-14.2052355202481,
116.282832240174)) ;
#165411 = CARTESIAN_POINT('Ctrl Pts',(-19.3325962215449,-14.1505953290783,
116.232769676212)) ;
#165412 = CARTESIAN_POINT('Ctrl Pts',(-19.4064000631929,-14.1505953352011,
116.208538629129)) ;
#165413 = CARTESIAN_POINT('Ctrl Pts',(-19.4802039048408,-14.150595341324,
116.184307582046)) ;
#165414 = CARTESIAN_POINT('Ctrl Pts',(-19.4966402857087,-14.2052355324938,
116.234370146008)) ;
#165415 = CARTESIAN_POINT('Ctrl Pts',(-19.5130766665765,-14.2598757236637,
116.28443270997)) ;
#165416 = CARTESIAN_POINT('Ctrl Pts',(-19.4392728249286,-14.2598757175408,
116.308663757054)) ;
#165417 = CARTESIAN_POINT('Ctrl Pts',(-19.3654689832807,-14.259875711418,
116.332894804137)) ;
#165418 = CARTESIAN_POINT('Ctrl Pts',(-19.3490326024128,-14.2052355202481,
116.282832240174)) ;
#165419 = CARTESIAN_POINT('Ctrl Pts',(-19.2861456806911,-14.3759216033723,
116.055895655754)) ;
#165420 = CARTESIAN_POINT('Ctrl Pts',(-19.2748088376837,-14.3092842663228,
116.021365461424)) ;
#165421 = CARTESIAN_POINT('Ctrl Pts',(-19.3486126772273,-14.309284273676,
115.997134407932)) ;
#165422 = CARTESIAN_POINT('Ctrl Pts',(-19.4224165167709,-14.3092842810292,
115.972903354439)) ;
#165423 = CARTESIAN_POINT('Ctrl Pts',(-19.4337533597783,-14.3759216180787,
116.007433548769)) ;
#165424 = CARTESIAN_POINT('Ctrl Pts',(-19.4450902027857,-14.4425589551282,
116.041963743098)) ;
#165425 = CARTESIAN_POINT('Ctrl Pts',(-19.3712863632421,-14.442558947775,
116.066194796591)) ;
#165426 = CARTESIAN_POINT('Ctrl Pts',(-19.2974825236984,-14.4425589404218,
116.090425850083)) ;
#165427 = CARTESIAN_POINT('Ctrl Pts',(-19.2861456806911,-14.3759216033723,
116.055895655754)) ;
#165428 = CARTESIAN_POINT('Ctrl Pts',(-19.2116524882323,-14.478404639523,
115.793537621104)) ;
#165429 = CARTESIAN_POINT('Ctrl Pts',(-19.2062343723869,-14.404515033937,
115.77703491487)) ;
#165430 = CARTESIAN_POINT('Ctrl Pts',(-19.2800382092211,-14.4045150394246,
115.752803853124)) ;
#165431 = CARTESIAN_POINT('Ctrl Pts',(-19.3538420460552,-14.4045150449122,
115.728572791379)) ;
#165432 = CARTESIAN_POINT('Ctrl Pts',(-19.3592601619006,-14.4784046504982,
115.745075497613)) ;
#165433 = CARTESIAN_POINT('Ctrl Pts',(-19.364678277746,-14.5522942560841,
115.761578203847)) ;
#165434 = CARTESIAN_POINT('Ctrl Pts',(-19.2908744409119,-14.5522942505966,
115.785809265593)) ;
#165435 = CARTESIAN_POINT('Ctrl Pts',(-19.2170706040777,-14.552294245109,
115.810040327338)) ;
#165436 = CARTESIAN_POINT('Ctrl Pts',(-19.2116524882323,-14.478404639523,
115.793537621104)) ;
#165437 = CARTESIAN_POINT('Ctrl Pts',(-19.1318016810032,-14.505089399069,
115.514904636501)) ;
#165438 = CARTESIAN_POINT('Ctrl Pts',(-19.1326839640339,-14.4292297938268,
115.517591928826)) ;
#165439 = CARTESIAN_POINT('Ctrl Pts',(-19.2064877982472,-14.4292297934085,
115.493360859098)) ;
#165440 = CARTESIAN_POINT('Ctrl Pts',(-19.2802916324605,-14.4292297929902,
115.46912978937)) ;
#165441 = CARTESIAN_POINT('Ctrl Pts',(-19.2794093494299,-14.5050893982325,
115.466442497045)) ;
#165442 = CARTESIAN_POINT('Ctrl Pts',(-19.2785270663992,-14.5809490034747,
115.46375520472)) ;
#165443 = CARTESIAN_POINT('Ctrl Pts',(-19.2047232321859,-14.580949003893,
115.487986274448)) ;
#165444 = CARTESIAN_POINT('Ctrl Pts',(-19.1309193979726,-14.5809490043113,
115.512217344176)) ;
#165445 = CARTESIAN_POINT('Ctrl Pts',(-19.1318016810032,-14.505089399069,
115.514904636501)) ;
#165446 = CARTESIAN_POINT('Ctrl Pts',(-19.0524890416985,-14.4533114988155,
115.237672140607)) ;
#165447 = CARTESIAN_POINT('Ctrl Pts',(-19.0596481858551,-14.3809567964235,
115.259477739355)) ;
#165448 = CARTESIAN_POINT('Ctrl Pts',(-19.1334520173609,-14.3809567849074,
115.23524666138)) ;
#165449 = CARTESIAN_POINT('Ctrl Pts',(-19.2072558488666,-14.3809567733913,
115.211015583405)) ;
#165450 = CARTESIAN_POINT('Ctrl Pts',(-19.20009670471,-14.4533114757834,115.189209984658)) ;
#165451 = CARTESIAN_POINT('Ctrl Pts',(-19.1929375605535,-14.5256661781754,
115.16740438591)) ;
#165452 = CARTESIAN_POINT('Ctrl Pts',(-19.1191337290477,-14.5256661896915,
115.191635463884)) ;
#165453 = CARTESIAN_POINT('Ctrl Pts',(-19.045329897542,-14.5256662012075,
115.215866541859)) ;
#165454 = CARTESIAN_POINT('Ctrl Pts',(-19.0524890416985,-14.4533114988155,
115.237672140607)) ;
#165455 = CARTESIAN_POINT('Ctrl Pts',(-18.9813656993656,-14.3281114059052,
114.985728322103)) ;
#165456 = CARTESIAN_POINT('Ctrl Pts',(-18.9942316512457,-14.2643939997168,
115.024915936526)) ;
#165457 = CARTESIAN_POINT('Ctrl Pts',(-19.0680354822422,-14.26439397447,115.000684857001)) ;
#165458 = CARTESIAN_POINT('Ctrl Pts',(-19.1418393132387,-14.2643939492231,
114.976453777475)) ;
#165459 = CARTESIAN_POINT('Ctrl Pts',(-19.1289733613586,-14.3281113554114,
114.937266163052)) ;
#165460 = CARTESIAN_POINT('Ctrl Pts',(-19.1161074094785,-14.3918287615997,
114.898078548628)) ;
#165461 = CARTESIAN_POINT('Ctrl Pts',(-19.042303578482,-14.3918287868466,
114.922309628154)) ;
#165462 = CARTESIAN_POINT('Ctrl Pts',(-18.9684997474855,-14.3918288120935,
114.946540707679)) ;
#165463 = CARTESIAN_POINT('Ctrl Pts',(-18.9813656993656,-14.3281114059052,
114.985728322103)) ;
#165464 = CARTESIAN_POINT('Ctrl Pts',(-18.9231476629716,-14.1371521548342,
114.77288475777)) ;
#165465 = CARTESIAN_POINT('Ctrl Pts',(-18.9408319558963,-14.0866750756418,
114.826748261758)) ;
#165466 = CARTESIAN_POINT('Ctrl Pts',(-19.0146357875153,-14.0866750338847,
114.802517184128)) ;
#165467 = CARTESIAN_POINT('Ctrl Pts',(-19.0884396191342,-14.0866749921275,
114.778286106498)) ;
#165468 = CARTESIAN_POINT('Ctrl Pts',(-19.0707553262095,-14.1371520713199,
114.724422602511)) ;
#165469 = CARTESIAN_POINT('Ctrl Pts',(-19.0530710332848,-14.1876291505123,
114.670559098523)) ;
#165470 = CARTESIAN_POINT('Ctrl Pts',(-18.9792672016658,-14.1876291922694,
114.694790176153)) ;
#165471 = CARTESIAN_POINT('Ctrl Pts',(-18.9054633700469,-14.1876292340265,
114.719021253783)) ;
#165472 = CARTESIAN_POINT('Ctrl Pts',(-18.9231476629716,-14.1371521548342,
114.77288475777)) ;
#165473 = CARTESIAN_POINT('Ctrl Pts',(-18.8833376833502,-13.8952369066383,
114.616222830795)) ;
#165474 = CARTESIAN_POINT('Ctrl Pts',(-18.9045596128905,-13.8615770485299,
114.680861405271)) ;
#165475 = CARTESIAN_POINT('Ctrl Pts',(-18.9783634473156,-13.861576991076,
114.656630336188)) ;
#165476 = CARTESIAN_POINT('Ctrl Pts',(-19.0521672817407,-13.8615769336222,
114.632399267105)) ;
#165477 = CARTESIAN_POINT('Ctrl Pts',(-19.0309453522004,-13.8952367917306,
114.567760692629)) ;
#165478 = CARTESIAN_POINT('Ctrl Pts',(-19.0097234226601,-13.928896649839,
114.503122118153)) ;
#165479 = CARTESIAN_POINT('Ctrl Pts',(-18.935919588235,-13.9288967072929,
114.527353187236)) ;
#165480 = CARTESIAN_POINT('Ctrl Pts',(-18.8621157538098,-13.9288967647467,
114.551584256319)) ;
#165481 = CARTESIAN_POINT('Ctrl Pts',(-18.8833376833502,-13.8952369066383,
114.616222830795)) ;
#165482 = CARTESIAN_POINT('Ctrl Pts',(-18.8652708972368,-13.6186018565224,
114.525698941726)) ;
#165483 = CARTESIAN_POINT('Ctrl Pts',(-18.8885194152068,-13.6042072181223,
114.596510177732)) ;
#165484 = CARTESIAN_POINT('Ctrl Pts',(-18.9623232542295,-13.6042071468649,
114.572279122652)) ;
#165485 = CARTESIAN_POINT('Ctrl Pts',(-19.0361270932522,-13.6042070756075,
114.548048067573)) ;
#165486 = CARTESIAN_POINT('Ctrl Pts',(-19.0128785752822,-13.6186017140076,
114.477236831567)) ;
#165487 = CARTESIAN_POINT('Ctrl Pts',(-18.9896300573122,-13.6329963524077,
114.406425595561)) ;
#165488 = CARTESIAN_POINT('Ctrl Pts',(-18.9158262182895,-13.6329964236651,
114.430656650641)) ;
#165489 = CARTESIAN_POINT('Ctrl Pts',(-18.8420223792668,-13.6329964949225,
114.45488770572)) ;
#165490 = CARTESIAN_POINT('Ctrl Pts',(-18.8652708972368,-13.6186018565224,
114.525698941726)) ;
#165491 = CARTESIAN_POINT('Ctrl Pts',(-18.8711343231666,-13.3278430882069,
114.508099714174)) ;
#165492 = CARTESIAN_POINT('Ctrl Pts',(-18.8947408656178,-13.3337275360589,
114.580001435127)) ;
#165493 = CARTESIAN_POINT('Ctrl Pts',(-18.9685447109095,-13.3337274561623,
114.555770399142)) ;
#165494 = CARTESIAN_POINT('Ctrl Pts',(-19.0423485562011,-13.3337273762658,
114.531539363158)) ;
#165495 = CARTESIAN_POINT('Ctrl Pts',(-19.01874201375,-13.3278429284139,114.459637642204)) ;
#165496 = CARTESIAN_POINT('Ctrl Pts',(-18.9951354712988,-13.3219584805619,
114.387735921251)) ;
#165497 = CARTESIAN_POINT('Ctrl Pts',(-18.9213316260071,-13.3219585604584,
114.411966957236)) ;
#165498 = CARTESIAN_POINT('Ctrl Pts',(-18.8475277807154,-13.3219586403549,
114.436197993221)) ;
#165499 = CARTESIAN_POINT('Ctrl Pts',(-18.8711343231666,-13.3278430882069,
114.508099714174)) ;
#165500 = CARTESIAN_POINT('Ctrl Pts',(-18.9012499909947,-13.0431633993278,
114.564322017916)) ;
#165501 = CARTESIAN_POINT('Ctrl Pts',(-18.9235229473357,-13.0689317715885,
114.632161850889)) ;
#165502 = CARTESIAN_POINT('Ctrl Pts',(-18.9973267999589,-13.0689316894194,
114.607930837235)) ;
#165503 = CARTESIAN_POINT('Ctrl Pts',(-19.0711306525821,-13.0689316072503,
114.583699823581)) ;
#165504 = CARTESIAN_POINT('Ctrl Pts',(-19.0488576962411,-13.0431632349896,
114.515859990607)) ;
#165505 = CARTESIAN_POINT('Ctrl Pts',(-19.0265847399001,-13.0173948627289,
114.448020157633)) ;
#165506 = CARTESIAN_POINT('Ctrl Pts',(-18.9527808872769,-13.017394944898,
114.472251171288)) ;
#165507 = CARTESIAN_POINT('Ctrl Pts',(-18.8789770346537,-13.0173950270671,
114.496482184942)) ;
#165508 = CARTESIAN_POINT('Ctrl Pts',(-18.9012499909947,-13.0431633993278,
114.564322017916)) ;
#165509 = CARTESIAN_POINT('Ctrl Pts',(-18.9542826657054,-12.7854826732307,
114.69034661993)) ;
#165510 = CARTESIAN_POINT('Ctrl Pts',(-18.9736201800411,-12.8292789756885,
114.749245570308)) ;
#165511 = CARTESIAN_POINT('Ctrl Pts',(-19.0474240403087,-12.8292788993553,
114.725014579938)) ;
#165512 = CARTESIAN_POINT('Ctrl Pts',(-19.1212279005763,-12.8292788230221,
114.700783589567)) ;
#165513 = CARTESIAN_POINT('Ctrl Pts',(-19.1018903862406,-12.7854825205643,
114.641884639189)) ;
#165514 = CARTESIAN_POINT('Ctrl Pts',(-19.0825528719048,-12.7416862181065,
114.582985688811)) ;
#165515 = CARTESIAN_POINT('Ctrl Pts',(-19.0087490116372,-12.7416862944397,
114.607216679182)) ;
#165516 = CARTESIAN_POINT('Ctrl Pts',(-18.9349451513697,-12.7416863707729,
114.631447669552)) ;
#165517 = CARTESIAN_POINT('Ctrl Pts',(-18.9542826657054,-12.7854826732307,
114.69034661993)) ;
#165518 = CARTESIAN_POINT('Ctrl Pts',(-19.0266928617708,-12.5740916835464,
114.875572584882)) ;
#165519 = CARTESIAN_POINT('Ctrl Pts',(-19.0417339574054,-12.6327102616695,
114.921385337205)) ;
#165520 = CARTESIAN_POINT('Ctrl Pts',(-19.1155378244281,-12.6327101996491,
114.897154367409)) ;
#165521 = CARTESIAN_POINT('Ctrl Pts',(-19.1893416914507,-12.6327101376288,
114.872923397613)) ;
#165522 = CARTESIAN_POINT('Ctrl Pts',(-19.174300595816,-12.5740915595058,
114.82711064529)) ;
#165523 = CARTESIAN_POINT('Ctrl Pts',(-19.1592595001814,-12.5154729813828,
114.781297892968)) ;
#165524 = CARTESIAN_POINT('Ctrl Pts',(-19.0854556331588,-12.5154730434031,
114.805528862764)) ;
#165525 = CARTESIAN_POINT('Ctrl Pts',(-19.0116517661362,-12.5154731054234,
114.829759832559)) ;
#165526 = CARTESIAN_POINT('Ctrl Pts',(-19.0266928617708,-12.5740916835464,
114.875572584882)) ;
#165527 = CARTESIAN_POINT('Ctrl Pts',(-19.1147735207953,-12.4220262848849,
115.108352144705)) ;
#165528 = CARTESIAN_POINT('Ctrl Pts',(-19.1244217586792,-12.4913473054171,
115.137739122539)) ;
#165529 = CARTESIAN_POINT('Ctrl Pts',(-19.1982256312606,-12.49134726396,115.113508169674)) ;
#165530 = CARTESIAN_POINT('Ctrl Pts',(-19.2720295038421,-12.491347222503,
115.089277216809)) ;
#165531 = CARTESIAN_POINT('Ctrl Pts',(-19.2623812659582,-12.4220262019709,
115.059890238976)) ;
#165532 = CARTESIAN_POINT('Ctrl Pts',(-19.2527330280743,-12.3527051814387,
115.030503261142)) ;
#165533 = CARTESIAN_POINT('Ctrl Pts',(-19.1789291554929,-12.3527052228958,
115.054734214006)) ;
#165534 = CARTESIAN_POINT('Ctrl Pts',(-19.1051252829115,-12.3527052643528,
115.078965166871)) ;
#165535 = CARTESIAN_POINT('Ctrl Pts',(-19.1147735207953,-12.4220262848849,
115.108352144705)) ;
#165536 = CARTESIAN_POINT('Ctrl Pts',(-19.2125943662298,-12.3415697140928,
115.370830458486)) ;
#165537 = CARTESIAN_POINT('Ctrl Pts',(-19.2161611902284,-12.4166096733525,
115.381694430919)) ;
#165538 = CARTESIAN_POINT('Ctrl Pts',(-19.2899650661739,-12.4166096578571,
115.357463488301)) ;
#165539 = CARTESIAN_POINT('Ctrl Pts',(-19.3637689421193,-12.4166096423617,
115.333232545682)) ;
#165540 = CARTESIAN_POINT('Ctrl Pts',(-19.3602021181207,-12.341569683102,
115.32236857325)) ;
#165541 = CARTESIAN_POINT('Ctrl Pts',(-19.356635294122,-12.2665297238424,
115.311504600817)) ;
#165542 = CARTESIAN_POINT('Ctrl Pts',(-19.2828314181766,-12.2665297393378,
115.335735543435)) ;
#165543 = CARTESIAN_POINT('Ctrl Pts',(-19.2090275422311,-12.2665297548332,
115.359966486053)) ;
#165544 = CARTESIAN_POINT('Ctrl Pts',(-19.2125943662298,-12.3415697140928,
115.370830458486)) ;
#165545 = CARTESIAN_POINT('Ctrl Pts',(-19.3139521730816,-12.3382226972324,
115.644076064424)) ;
#165546 = CARTESIAN_POINT('Ctrl Pts',(-19.3111818546697,-12.4136068588393,
115.635638123609)) ;
#165547 = CARTESIAN_POINT('Ctrl Pts',(-19.3849857313629,-12.413606871913,
115.611407183268)) ;
#165548 = CARTESIAN_POINT('Ctrl Pts',(-19.4587896080562,-12.4136068849868,
115.587176242927)) ;
#165549 = CARTESIAN_POINT('Ctrl Pts',(-19.4615599264681,-12.3382227233798,
115.595614183743)) ;
#165550 = CARTESIAN_POINT('Ctrl Pts',(-19.4643302448801,-12.2628385617728,
115.604052124559)) ;
#165551 = CARTESIAN_POINT('Ctrl Pts',(-19.3905263681868,-12.2628385486991,
115.6282830649)) ;
#165552 = CARTESIAN_POINT('Ctrl Pts',(-19.3167224914936,-12.2628385356254,
115.65251400524)) ;
#165553 = CARTESIAN_POINT('Ctrl Pts',(-19.3139521730816,-12.3382226972324,
115.644076064424)) ;
#165554 = CARTESIAN_POINT('Ctrl Pts',(-19.4122471361585,-12.4121411260321,
115.90802651911)) ;
#165555 = CARTESIAN_POINT('Ctrl Pts',(-19.4033434531606,-12.4824758625955,
115.880907339398)) ;
#165556 = CARTESIAN_POINT('Ctrl Pts',(-19.4771473278286,-12.4824759039206,
115.856676392889)) ;
#165557 = CARTESIAN_POINT('Ctrl Pts',(-19.5509512024966,-12.4824759452457,
115.832445446379)) ;
#165558 = CARTESIAN_POINT('Ctrl Pts',(-19.5598548854945,-12.4121412086823,
115.859564626092)) ;
#165559 = CARTESIAN_POINT('Ctrl Pts',(-19.5687585684923,-12.3418064721188,
115.886683805805)) ;
#165560 = CARTESIAN_POINT('Ctrl Pts',(-19.4949546938243,-12.3418064307938,
115.910914752314)) ;
#165561 = CARTESIAN_POINT('Ctrl Pts',(-19.4211508191563,-12.3418063894687,
115.935145698823)) ;
#165562 = CARTESIAN_POINT('Ctrl Pts',(-19.4122471361585,-12.4121411260321,
115.90802651911)) ;
#165563 = CARTESIAN_POINT('Ctrl Pts',(-19.5013836351553,-12.5582147089023,
116.144040613698)) ;
#165564 = CARTESIAN_POINT('Ctrl Pts',(-19.4869777368879,-12.6184554167387,
116.100162574049)) ;
#165565 = CARTESIAN_POINT('Ctrl Pts',(-19.5607816069403,-12.6184554831094,
116.075931613481)) ;
#165566 = CARTESIAN_POINT('Ctrl Pts',(-19.6345854769928,-12.61845554948,116.051700652914)) ;
#165567 = CARTESIAN_POINT('Ctrl Pts',(-19.6489913752602,-12.5582148416436,
116.095578692563)) ;
#165568 = CARTESIAN_POINT('Ctrl Pts',(-19.6633972735277,-12.4979741338071,
116.139456732212)) ;
#165569 = CARTESIAN_POINT('Ctrl Pts',(-19.5895934034752,-12.4979740674365,
116.163687692779)) ;
#165570 = CARTESIAN_POINT('Ctrl Pts',(-19.5157895334227,-12.4979740010659,
116.187918653347)) ;
#165571 = CARTESIAN_POINT('Ctrl Pts',(-19.5013836351553,-12.5582147089023,
116.144040613698)) ;
#165572 = CARTESIAN_POINT('Ctrl Pts',(-19.5755554742575,-12.7657436426172,
116.334505232011)) ;
#165573 = CARTESIAN_POINT('Ctrl Pts',(-19.5566832764055,-12.8115849189124,
116.277023564437)) ;
#165574 = CARTESIAN_POINT('Ctrl Pts',(-19.6304871397366,-12.8115850045316,
116.252792583397)) ;
#165575 = CARTESIAN_POINT('Ctrl Pts',(-19.7042910030678,-12.8115850901508,
116.228561602358)) ;
#165576 = CARTESIAN_POINT('Ctrl Pts',(-19.7231632009198,-12.7657438138556,
116.286043269933)) ;
#165577 = CARTESIAN_POINT('Ctrl Pts',(-19.7420353987717,-12.7199025375603,
116.343524937507)) ;
#165578 = CARTESIAN_POINT('Ctrl Pts',(-19.6682315354406,-12.7199024519411,
116.367755918547)) ;
#165579 = CARTESIAN_POINT('Ctrl Pts',(-19.5944276721094,-12.7199023663219,
116.391986899586)) ;
#165580 = CARTESIAN_POINT('Ctrl Pts',(-19.5755554742575,-12.7657436426172,
116.334505232011)) ;
#165581 = CARTESIAN_POINT('Ctrl Pts',(-19.6303334920016,-13.0202106019441,
116.465864508977)) ;
#165582 = CARTESIAN_POINT('Ctrl Pts',(-19.6083429686133,-13.0483542398271,
116.398884924909)) ;
#165583 = CARTESIAN_POINT('Ctrl Pts',(-19.682146823822,-13.0483543369911,
116.37465391913)) ;
#165584 = CARTESIAN_POINT('Ctrl Pts',(-19.7559506790307,-13.0483544341551,
116.350422913351)) ;
#165585 = CARTESIAN_POINT('Ctrl Pts',(-19.777941202419,-13.0202107962721,
116.417402497419)) ;
#165586 = CARTESIAN_POINT('Ctrl Pts',(-19.7999317258073,-12.992067158389,
116.484382081487)) ;
#165587 = CARTESIAN_POINT('Ctrl Pts',(-19.7261278705986,-12.9920670612251,
116.508613087266)) ;
#165588 = CARTESIAN_POINT('Ctrl Pts',(-19.6523240153899,-12.9920669640611,
116.532844093045)) ;
#165589 = CARTESIAN_POINT('Ctrl Pts',(-19.6303334920016,-13.0202106019441,
116.465864508977)) ;
#165590 = CARTESIAN_POINT('Ctrl Pts',(-19.6624379392262,-13.3031020545658,
116.528178876828)) ;
#165591 = CARTESIAN_POINT('Ctrl Pts',(-19.6389070181145,-13.3115371239571,
116.456507489767)) ;
#165592 = CARTESIAN_POINT('Ctrl Pts',(-19.7127108647141,-13.3115372240585,
116.432276457765)) ;
#165593 = CARTESIAN_POINT('Ctrl Pts',(-19.7865147113136,-13.3115373241599,
116.408045425764)) ;
#165594 = CARTESIAN_POINT('Ctrl Pts',(-19.8100456324252,-13.3031022547687,
116.479716812825)) ;
#165595 = CARTESIAN_POINT('Ctrl Pts',(-19.8335765535369,-13.2946671853774,
116.551388199887)) ;
#165596 = CARTESIAN_POINT('Ctrl Pts',(-19.7597727069374,-13.2946670852759,
116.575619231888)) ;
#165597 = CARTESIAN_POINT('Ctrl Pts',(-19.6859688603378,-13.2946669851745,
116.599850263889)) ;
#165598 = CARTESIAN_POINT('Ctrl Pts',(-19.6624379392262,-13.3031020545658,
116.528178876828)) ;
#165599 = CARTESIAN_POINT('Ctrl Pts',(-19.6703646074423,-13.593918747588,
116.516886330031)) ;
#165600 = CARTESIAN_POINT('Ctrl Pts',(-19.6469782287227,-13.5820623140505,
116.445655195687)) ;
#165601 = CARTESIAN_POINT('Ctrl Pts',(-19.7207820671414,-13.5820624088636,
116.421424138769)) ;
#165602 = CARTESIAN_POINT('Ctrl Pts',(-19.7945859055601,-13.5820625036768,
116.39719308185)) ;
#165603 = CARTESIAN_POINT('Ctrl Pts',(-19.8179722842797,-13.5939189372143,
116.468424216193)) ;
#165604 = CARTESIAN_POINT('Ctrl Pts',(-19.8413586629993,-13.6057753707518,
116.539655350536)) ;
#165605 = CARTESIAN_POINT('Ctrl Pts',(-19.7675548245806,-13.6057752759387,
116.563886407455)) ;
#165606 = CARTESIAN_POINT('Ctrl Pts',(-19.6937509861619,-13.6057751811255,
116.588117464374)) ;
#165607 = CARTESIAN_POINT('Ctrl Pts',(-19.6703646074423,-13.593918747588,
116.516886330031)) ;
#165608 = CARTESIAN_POINT('Ctrl Pts',(-19.654361800593,-13.8723058564386,
116.432695143982)) ;
#165609 = CARTESIAN_POINT('Ctrl Pts',(-19.6327910609281,-13.8409951979867,
116.366994153143)) ;
#165610 = CARTESIAN_POINT('Ctrl Pts',(-19.7065948923452,-13.8409952801853,
116.342763074898)) ;
#165611 = CARTESIAN_POINT('Ctrl Pts',(-19.7803987237623,-13.8409953623839,
116.318531996653)) ;
#165612 = CARTESIAN_POINT('Ctrl Pts',(-19.8019694634272,-13.8723060208357,
116.384232987493)) ;
#165613 = CARTESIAN_POINT('Ctrl Pts',(-19.8235402030921,-13.9036166792876,
116.449933978333)) ;
#165614 = CARTESIAN_POINT('Ctrl Pts',(-19.7497363716751,-13.903616597089,
116.474165056577)) ;
#165615 = CARTESIAN_POINT('Ctrl Pts',(-19.675932540258,-13.9036165148904,
116.498396134822)) ;
#165616 = CARTESIAN_POINT('Ctrl Pts',(-19.654361800593,-13.8723058564386,
116.432695143982)) ;
#165617 = CARTESIAN_POINT('Ctrl Pts',(-19.6160972828307,-14.118869151071,
116.28058076468)) ;
#165618 = CARTESIAN_POINT('Ctrl Pts',(-19.5979014436013,-14.070296502829,
116.225159175889)) ;
#165619 = CARTESIAN_POINT('Ctrl Pts',(-19.6717052700668,-14.0702965663063,
116.200928082563)) ;
#165620 = CARTESIAN_POINT('Ctrl Pts',(-19.7455090965323,-14.0702966297837,
116.176696989237)) ;
#165621 = CARTESIAN_POINT('Ctrl Pts',(-19.7637049357618,-14.1188692780257,
116.232118578027)) ;
#165622 = CARTESIAN_POINT('Ctrl Pts',(-19.7819007749912,-14.1674419262677,
116.287540166818)) ;
#165623 = CARTESIAN_POINT('Ctrl Pts',(-19.7080969485257,-14.1674418627903,
116.311771260144)) ;
#165624 = CARTESIAN_POINT('Ctrl Pts',(-19.6342931220601,-14.167441799313,
116.33600235347)) ;
#165625 = CARTESIAN_POINT('Ctrl Pts',(-19.6160972828307,-14.118869151071,
116.28058076468)) ;
#165626 = CARTESIAN_POINT('Ctrl Pts',(-19.5594235023051,-14.3141618691383,
116.072558650633)) ;
#165627 = CARTESIAN_POINT('Ctrl Pts',(-19.5458897072115,-14.2518807456653,
116.031336895932)) ;
#165628 = CARTESIAN_POINT('Ctrl Pts',(-19.6196935307721,-14.2518807886643,
116.007105793758)) ;
#165629 = CARTESIAN_POINT('Ctrl Pts',(-19.6934973543327,-14.2518808316633,
115.982874691584)) ;
#165630 = CARTESIAN_POINT('Ctrl Pts',(-19.7070311494263,-14.3141619551363,
116.024096446284)) ;
#165631 = CARTESIAN_POINT('Ctrl Pts',(-19.7205649445198,-14.3764430786093,
116.065318200985)) ;
#165632 = CARTESIAN_POINT('Ctrl Pts',(-19.6467611209592,-14.3764430356103,
116.089549303159)) ;
#165633 = CARTESIAN_POINT('Ctrl Pts',(-19.5729572973986,-14.3764429926113,
116.113780405334)) ;
#165634 = CARTESIAN_POINT('Ctrl Pts',(-19.5594235023051,-14.3141618691383,
116.072558650633)) ;
#165635 = CARTESIAN_POINT('Ctrl Pts',(-19.4889283697476,-14.4456574881185,
115.82238678645)) ;
#165636 = CARTESIAN_POINT('Ctrl Pts',(-19.4810297011629,-14.3741011608773,
115.798328717722)) ;
#165637 = CARTESIAN_POINT('Ctrl Pts',(-19.5548335241347,-14.3741011828996,
115.774097613754)) ;
#165638 = CARTESIAN_POINT('Ctrl Pts',(-19.6286373471065,-14.3741012049218,
115.749866509787)) ;
#165639 = CARTESIAN_POINT('Ctrl Pts',(-19.6365360156912,-14.4456575321631,
115.773924578514)) ;
#165640 = CARTESIAN_POINT('Ctrl Pts',(-19.6444346842759,-14.5172138594043,
115.797982647242)) ;
#165641 = CARTESIAN_POINT('Ctrl Pts',(-19.5706308613041,-14.5172138373821,
115.82221375121)) ;
#165642 = CARTESIAN_POINT('Ctrl Pts',(-19.4968270383323,-14.5172138153598,
115.846444855178)) ;
#165643 = CARTESIAN_POINT('Ctrl Pts',(-19.4889283697476,-14.4456574881185,
115.82238678645)) ;
#165644 = CARTESIAN_POINT('Ctrl Pts',(-19.4104748865899,-14.5036635199146,
115.547989903385)) ;
#165645 = CARTESIAN_POINT('Ctrl Pts',(-19.4087752444467,-14.4279488253923,
115.542813068833)) ;
#165646 = CARTESIAN_POINT('Ctrl Pts',(-19.4825790688346,-14.4279488285843,
115.518581969179)) ;
#165647 = CARTESIAN_POINT('Ctrl Pts',(-19.5563828932225,-14.4279488317762,
115.494350869525)) ;
#165648 = CARTESIAN_POINT('Ctrl Pts',(-19.5580825353658,-14.5036635262985,
115.499527704076)) ;
#165649 = CARTESIAN_POINT('Ctrl Pts',(-19.5597821775091,-14.5793782208208,
115.504704538628)) ;
#165650 = CARTESIAN_POINT('Ctrl Pts',(-19.4859783531212,-14.5793782176288,
115.528935638283)) ;
#165651 = CARTESIAN_POINT('Ctrl Pts',(-19.4121745287332,-14.5793782144369,
115.553166737937)) ;
#165652 = CARTESIAN_POINT('Ctrl Pts',(-19.4104748865899,-14.5036635199146,
115.547989903385)) ;
#165653 = CARTESIAN_POINT('Ctrl Pts',(-19.3301101843111,-14.4836080857303,
115.267628373719)) ;
#165654 = CARTESIAN_POINT('Ctrl Pts',(-19.334755451989,-14.409178476904,115.281777110546)) ;
#165655 = CARTESIAN_POINT('Ctrl Pts',(-19.4085592797642,-14.4091784657996,
115.257546021209)) ;
#165656 = CARTESIAN_POINT('Ctrl Pts',(-19.4823631075395,-14.4091784546952,
115.233314931872)) ;
#165657 = CARTESIAN_POINT('Ctrl Pts',(-19.4777178398616,-14.4836080635215,
115.219166195045)) ;
#165658 = CARTESIAN_POINT('Ctrl Pts',(-19.4730725721837,-14.5580376723478,
115.205017458217)) ;
#165659 = CARTESIAN_POINT('Ctrl Pts',(-19.3992687444084,-14.5580376834522,
115.229248547554)) ;
#165660 = CARTESIAN_POINT('Ctrl Pts',(-19.3254649166332,-14.5580376945566,
115.253479636892)) ;
#165661 = CARTESIAN_POINT('Ctrl Pts',(-19.3301101843111,-14.4836080857303,
115.267628373719)) ;
#165662 = CARTESIAN_POINT('Ctrl Pts',(-19.2551325732941,-14.3877127605132,
115.003913883089)) ;
#165663 = CARTESIAN_POINT('Ctrl Pts',(-19.2657513147536,-14.319866136678,
115.036256857093)) ;
#165664 = CARTESIAN_POINT('Ctrl Pts',(-19.3395551461189,-14.3198661161146,
115.01202577869)) ;
#165665 = CARTESIAN_POINT('Ctrl Pts',(-19.4133589774841,-14.3198660955512,
114.987794700287)) ;
#165666 = CARTESIAN_POINT('Ctrl Pts',(-19.4027402360246,-14.3877127193864,
114.955451726283)) ;
#165667 = CARTESIAN_POINT('Ctrl Pts',(-19.392121494565,-14.4555593432216,
114.923108752279)) ;
#165668 = CARTESIAN_POINT('Ctrl Pts',(-19.3183176631998,-14.455559363785,
114.947339830682)) ;
#165669 = CARTESIAN_POINT('Ctrl Pts',(-19.2445138318345,-14.4555593843484,
114.971570909085)) ;
#165670 = CARTESIAN_POINT('Ctrl Pts',(-19.2551325732941,-14.3877127605132,
115.003913883089)) ;
#165671 = CARTESIAN_POINT('Ctrl Pts',(-19.1906766261937,-14.2212524561287,
114.77196540951)) ;
#165672 = CARTESIAN_POINT('Ctrl Pts',(-19.2065492806211,-14.1649252203371,
114.820310954501)) ;
#165673 = CARTESIAN_POINT('Ctrl Pts',(-19.280353116469,-14.1649251971047,
114.796079889752)) ;
#165674 = CARTESIAN_POINT('Ctrl Pts',(-19.3541569523169,-14.1649251738723,
114.771848825002)) ;
#165675 = CARTESIAN_POINT('Ctrl Pts',(-19.3382842978895,-14.2212524096639,
114.723503280012)) ;
#165676 = CARTESIAN_POINT('Ctrl Pts',(-19.3224116434621,-14.2775796454555,
114.675157735021)) ;
#165677 = CARTESIAN_POINT('Ctrl Pts',(-19.2486078076142,-14.2775796686879,
114.69938879977)) ;
#165678 = CARTESIAN_POINT('Ctrl Pts',(-19.1748039717663,-14.2775796919203,
114.723619864519)) ;
#165679 = CARTESIAN_POINT('Ctrl Pts',(-19.1906766261937,-14.2212524561287,
114.77196540951)) ;
#165680 = CARTESIAN_POINT('Ctrl Pts',(-19.1431008734099,-13.9987538981264,
114.591734960995)) ;
#165681 = CARTESIAN_POINT('Ctrl Pts',(-19.1630503294408,-13.9578771653023,
114.652497785746)) ;
#165682 = CARTESIAN_POINT('Ctrl Pts',(-19.2368541686022,-13.9578771425154,
114.628266731089)) ;
#165683 = CARTESIAN_POINT('Ctrl Pts',(-19.3106580077636,-13.9578771197285,
114.604035676433)) ;
#165684 = CARTESIAN_POINT('Ctrl Pts',(-19.2907085517327,-13.9987538525526,
114.543272851682)) ;
#165685 = CARTESIAN_POINT('Ctrl Pts',(-19.2707590957019,-14.0396305853768,
114.482510026931)) ;
#165686 = CARTESIAN_POINT('Ctrl Pts',(-19.1969552565404,-14.0396306081637,
114.506741081588)) ;
#165687 = CARTESIAN_POINT('Ctrl Pts',(-19.123151417379,-14.0396306309506,
114.530972136245)) ;
#165688 = CARTESIAN_POINT('Ctrl Pts',(-19.1431008734099,-13.9987538981264,
114.591734960995)) ;
#165689 = CARTESIAN_POINT('Ctrl Pts',(-19.1158102336092,-13.7338214529053,
114.473123572726)) ;
#165690 = CARTESIAN_POINT('Ctrl Pts',(-19.138429846815,-13.7113815142411,
114.542019265248)) ;
#165691 = CARTESIAN_POINT('Ctrl Pts',(-19.2122336887546,-13.7113814963311,
114.517788219053)) ;
#165692 = CARTESIAN_POINT('Ctrl Pts',(-19.2860375306941,-13.7113814784212,
114.493557172857)) ;
#165693 = CARTESIAN_POINT('Ctrl Pts',(-19.2634179174883,-13.7338214170854,
114.424661480336)) ;
#165694 = CARTESIAN_POINT('Ctrl Pts',(-19.2407983042824,-13.7562613557496,
114.355765787815)) ;
#165695 = CARTESIAN_POINT('Ctrl Pts',(-19.1669944623428,-13.7562613736596,
114.37999683401)) ;
#165696 = CARTESIAN_POINT('Ctrl Pts',(-19.0931906204033,-13.7562613915695,
114.404227880205)) ;
#165697 = CARTESIAN_POINT('Ctrl Pts',(-19.1158102336092,-13.7338214529053,
114.473123572726)) ;
#165698 = CARTESIAN_POINT('Ctrl Pts',(-19.1118129583961,-13.4466916236415,
114.425526047976)) ;
#165699 = CARTESIAN_POINT('Ctrl Pts',(-19.1354788504801,-13.4442666484752,
114.497608537013)) ;
#165700 = CARTESIAN_POINT('Ctrl Pts',(-19.2092826939799,-13.4442666367421,
114.473377495571)) ;
#165701 = CARTESIAN_POINT('Ctrl Pts',(-19.2830865374798,-13.4442666250089,
114.449146454128)) ;
#165702 = CARTESIAN_POINT('Ctrl Pts',(-19.2594206453958,-13.4466916001752,
114.377063965091)) ;
#165703 = CARTESIAN_POINT('Ctrl Pts',(-19.2357547533118,-13.4491165753415,
114.304981476054)) ;
#165704 = CARTESIAN_POINT('Ctrl Pts',(-19.161950909812,-13.4491165870746,
114.329212517497)) ;
#165705 = CARTESIAN_POINT('Ctrl Pts',(-19.0881470663121,-13.4491165988078,
114.353443558939)) ;
#165706 = CARTESIAN_POINT('Ctrl Pts',(-19.1118129583961,-13.4466916236415,
114.425526047976)) ;
#165707 = CARTESIAN_POINT('Ctrl Pts',(-19.1321594034187,-13.1565169960044,
114.451948862421)) ;
#165708 = CARTESIAN_POINT('Ctrl Pts',(-19.1551759820499,-13.1743502694123,
114.522053647319)) ;
#165709 = CARTESIAN_POINT('Ctrl Pts',(-19.2289798260042,-13.1743502645941,
114.49782260726)) ;
#165710 = CARTESIAN_POINT('Ctrl Pts',(-19.3027836699584,-13.174350259776,
114.473591567202)) ;
#165711 = CARTESIAN_POINT('Ctrl Pts',(-19.2797670913271,-13.156516986368,
114.403486782303)) ;
#165712 = CARTESIAN_POINT('Ctrl Pts',(-19.2567505126958,-13.1386837129601,
114.333381997405)) ;
#165713 = CARTESIAN_POINT('Ctrl Pts',(-19.1829466687416,-13.1386837177783,
114.357613037464)) ;
#165714 = CARTESIAN_POINT('Ctrl Pts',(-19.1091428247873,-13.1386837225965,
114.381844077522)) ;
#165715 = CARTESIAN_POINT('Ctrl Pts',(-19.1321594034187,-13.1565169960044,
114.451948862421)) ;
#165716 = CARTESIAN_POINT('Ctrl Pts',(-19.1761811779931,-12.8855146893556,
114.550531779431)) ;
#165717 = CARTESIAN_POINT('Ctrl Pts',(-19.1968930602221,-12.9222982070888,
114.613616830858)) ;
#165718 = CARTESIAN_POINT('Ctrl Pts',(-19.2706969037714,-12.9222982069282,
114.589385789566)) ;
#165719 = CARTESIAN_POINT('Ctrl Pts',(-19.3445007473207,-12.9222982067677,
114.565154748274)) ;
#165720 = CARTESIAN_POINT('Ctrl Pts',(-19.3237888650918,-12.8855146890345,
114.502069696848)) ;
#165721 = CARTESIAN_POINT('Ctrl Pts',(-19.3030769828629,-12.8487311713013,
114.438984645421)) ;
#165722 = CARTESIAN_POINT('Ctrl Pts',(-19.2292731393135,-12.8487311714619,
114.463215686713)) ;
#165723 = CARTESIAN_POINT('Ctrl Pts',(-19.1554692957642,-12.8487311716225,
114.487446728005)) ;
#165724 = CARTESIAN_POINT('Ctrl Pts',(-19.1761811779931,-12.8855146893556,
114.550531779431)) ;
#165725 = CARTESIAN_POINT('Ctrl Pts',(-19.2412304209422,-12.6534167842388,
114.713260927411)) ;
#165726 = CARTESIAN_POINT('Ctrl Pts',(-19.25816354557,-12.7064619703102,114.764836492834)) ;
#165727 = CARTESIAN_POINT('Ctrl Pts',(-19.3319673885266,-12.706461972049,
114.740605449737)) ;
#165728 = CARTESIAN_POINT('Ctrl Pts',(-19.4057712314832,-12.7064619737879,
114.71637440664)) ;
#165729 = CARTESIAN_POINT('Ctrl Pts',(-19.3888381068554,-12.6534167877166,
114.664798841216)) ;
#165730 = CARTESIAN_POINT('Ctrl Pts',(-19.3719049822277,-12.6003716016452,
114.613223275793)) ;
#165731 = CARTESIAN_POINT('Ctrl Pts',(-19.2981011392711,-12.6003715999064,
114.637454318891)) ;
#165732 = CARTESIAN_POINT('Ctrl Pts',(-19.2242972963145,-12.6003715981675,
114.661685361988)) ;
#165733 = CARTESIAN_POINT('Ctrl Pts',(-19.2412304209422,-12.6534167842388,
114.713260927411)) ;
#165734 = CARTESIAN_POINT('Ctrl Pts',(-19.323368321488,-12.475742126735,114.928074488961)) ;
#165735 = CARTESIAN_POINT('Ctrl Pts',(-19.3353229050844,-12.5412726842435,
114.964486221662)) ;
#165736 = CARTESIAN_POINT('Ctrl Pts',(-19.4091267475277,-12.5412726859999,
114.940255177002)) ;
#165737 = CARTESIAN_POINT('Ctrl Pts',(-19.4829305899709,-12.5412726877563,
114.916024132341)) ;
#165738 = CARTESIAN_POINT('Ctrl Pts',(-19.4709760063745,-12.4757421302478,
114.87961239964)) ;
#165739 = CARTESIAN_POINT('Ctrl Pts',(-19.4590214227781,-12.4102115727394,
114.843200666939)) ;
#165740 = CARTESIAN_POINT('Ctrl Pts',(-19.3852175803349,-12.410211570983,
114.8674317116)) ;
#165741 = CARTESIAN_POINT('Ctrl Pts',(-19.3114137378916,-12.4102115692266,
114.89166275626)) ;
#165742 = CARTESIAN_POINT('Ctrl Pts',(-19.323368321488,-12.475742126735,114.928074488961)) ;
#165743 = CARTESIAN_POINT('Ctrl Pts',(-19.4186665635696,-12.3646792210001,
115.18260181179)) ;
#165744 = CARTESIAN_POINT('Ctrl Pts',(-19.4247236549107,-12.438062944576,
115.201050734672)) ;
#165745 = CARTESIAN_POINT('Ctrl Pts',(-19.4985274977625,-12.4380629448186,
115.176819691256)) ;
#165746 = CARTESIAN_POINT('Ctrl Pts',(-19.5723313406143,-12.4380629450611,
115.152588647839)) ;
#165747 = CARTESIAN_POINT('Ctrl Pts',(-19.5662742492732,-12.3646792214852,
115.134139724957)) ;
#165748 = CARTESIAN_POINT('Ctrl Pts',(-19.5602171579321,-12.2912954979092,
115.115690802074)) ;
#165749 = CARTESIAN_POINT('Ctrl Pts',(-19.4864133150803,-12.2912954976667,
115.13992184549)) ;
#165750 = CARTESIAN_POINT('Ctrl Pts',(-19.4126094722285,-12.2912954974242,
115.164152888907)) ;
#165751 = CARTESIAN_POINT('Ctrl Pts',(-19.4186665635696,-12.3646792210001,
115.18260181179)) ;
#165752 = CARTESIAN_POINT('Ctrl Pts',(-19.5188634349595,-12.33019827638,115.452501593325)) ;
#165753 = CARTESIAN_POINT('Ctrl Pts',(-19.518663256346,-12.4060967099992,
115.451891881587)) ;
#165754 = CARTESIAN_POINT('Ctrl Pts',(-19.5924671000764,-12.4060967096592,
115.427660840847)) ;
#165755 = CARTESIAN_POINT('Ctrl Pts',(-19.6662709438068,-12.4060967093193,
115.403429800107)) ;
#165756 = CARTESIAN_POINT('Ctrl Pts',(-19.6664711224204,-12.3301982757,115.404039511845)) ;
#165757 = CARTESIAN_POINT('Ctrl Pts',(-19.6666713010339,-12.2542998420808,
115.404649223583)) ;
#165758 = CARTESIAN_POINT('Ctrl Pts',(-19.5928674573034,-12.2542998424208,
115.428880264323)) ;
#165759 = CARTESIAN_POINT('Ctrl Pts',(-19.519063613573,-12.2542998427607,
115.453111305064)) ;
#165760 = CARTESIAN_POINT('Ctrl Pts',(-19.5188634349595,-12.33019827638,115.452501593325)) ;
#165761 = CARTESIAN_POINT('Ctrl Pts',(-19.6194233101362,-12.3732244526573,
115.723247147594)) ;
#165762 = CARTESIAN_POINT('Ctrl Pts',(-19.6129366875966,-12.4462297114867,
115.703489942071)) ;
#165763 = CARTESIAN_POINT('Ctrl Pts',(-19.6867405329009,-12.4462297127272,
115.679258906124)) ;
#165764 = CARTESIAN_POINT('Ctrl Pts',(-19.7605443782052,-12.4462297139677,
115.655027870178)) ;
#165765 = CARTESIAN_POINT('Ctrl Pts',(-19.7670310007448,-12.3732244551383,
115.674785075701)) ;
#165766 = CARTESIAN_POINT('Ctrl Pts',(-19.7735176232844,-12.300219196309,
115.694542281225)) ;
#165767 = CARTESIAN_POINT('Ctrl Pts',(-19.6997137779801,-12.3002191950685,
115.718773317171)) ;
#165768 = CARTESIAN_POINT('Ctrl Pts',(-19.6259099326758,-12.300219193828,
115.743004353118)) ;
#165769 = CARTESIAN_POINT('Ctrl Pts',(-19.6194233101362,-12.3732244526573,
115.723247147594)) ;
#165770 = CARTESIAN_POINT('Ctrl Pts',(-19.7127947734479,-12.4909980427198,
115.972246654781)) ;
#165771 = CARTESIAN_POINT('Ctrl Pts',(-19.700511630848,-12.5558859351168,
115.93483418453)) ;
#165772 = CARTESIAN_POINT('Ctrl Pts',(-19.7743154775138,-12.555885940904,
115.910603152731)) ;
#165773 = CARTESIAN_POINT('Ctrl Pts',(-19.8481193241796,-12.5558859466913,
115.886372120931)) ;
#165774 = CARTESIAN_POINT('Ctrl Pts',(-19.8604024667795,-12.4909980542943,
115.923784591182)) ;
#165775 = CARTESIAN_POINT('Ctrl Pts',(-19.8726856093794,-12.4261101618973,
115.961197061433)) ;
#165776 = CARTESIAN_POINT('Ctrl Pts',(-19.7988817627136,-12.4261101561101,
115.985428093232)) ;
#165777 = CARTESIAN_POINT('Ctrl Pts',(-19.7250779160477,-12.4261101503228,
116.009659125032)) ;
#165778 = CARTESIAN_POINT('Ctrl Pts',(-19.7127947734479,-12.4909980427198,
115.972246654781)) ;
#165779 = CARTESIAN_POINT('Ctrl Pts',(-19.793610933256,-12.67497986033,116.182961362968)) ;
#165780 = CARTESIAN_POINT('Ctrl Pts',(-19.7764005017003,-12.7271157689749,
116.130541165705)) ;
#165781 = CARTESIAN_POINT('Ctrl Pts',(-19.8502043492699,-12.727115782205,
116.106310136658)) ;
#165782 = CARTESIAN_POINT('Ctrl Pts',(-19.9240081968394,-12.7271157954351,
116.082079107611)) ;
#165783 = CARTESIAN_POINT('Ctrl Pts',(-19.9412186283951,-12.6749798867901,
116.134499304874)) ;
#165784 = CARTESIAN_POINT('Ctrl Pts',(-19.9584290599508,-12.6228439781452,
116.186919502137)) ;
#165785 = CARTESIAN_POINT('Ctrl Pts',(-19.8846252123812,-12.6228439649152,
116.211150531184)) ;
#165786 = CARTESIAN_POINT('Ctrl Pts',(-19.8108213648117,-12.6228439516851,
116.235381560231)) ;
#165787 = CARTESIAN_POINT('Ctrl Pts',(-19.793610933256,-12.67497986033,116.182961362968)) ;
#165788 = CARTESIAN_POINT('Ctrl Pts',(-19.8568164214443,-12.9129719673497,
116.339934873997)) ;
#165789 = CARTESIAN_POINT('Ctrl Pts',(-19.8359033043558,-12.9485664184321,
116.276236894194)) ;
#165790 = CARTESIAN_POINT('Ctrl Pts',(-19.909707151925,-12.9485664423294,
116.252005865145)) ;
#165791 = CARTESIAN_POINT('Ctrl Pts',(-19.9835109994942,-12.9485664662267,
116.227774836097)) ;
#165792 = CARTESIAN_POINT('Ctrl Pts',(-20.0044241165827,-12.9129720151443,
116.291472815901)) ;
#165793 = CARTESIAN_POINT('Ctrl Pts',(-20.0253372336711,-12.8773775640619,
116.355170795705)) ;
#165794 = CARTESIAN_POINT('Ctrl Pts',(-19.951533386102,-12.8773775401646,
116.379401824753)) ;
#165795 = CARTESIAN_POINT('Ctrl Pts',(-19.8777295385328,-12.8773775162673,
116.403632853801)) ;
#165796 = CARTESIAN_POINT('Ctrl Pts',(-19.8568164214443,-12.9129719673497,
116.339934873997)) ;
#165797 = CARTESIAN_POINT('Ctrl Pts',(-19.8982594904765,-13.1860117694584,
116.43078023)) ;
#165798 = CARTESIAN_POINT('Ctrl Pts',(-19.8751548018971,-13.2025937727261,
116.360407077191)) ;
#165799 = CARTESIAN_POINT('Ctrl Pts',(-19.9489586478412,-13.2025938067603,
116.336176043193)) ;
#165800 = CARTESIAN_POINT('Ctrl Pts',(-20.0227624937853,-13.2025938407946,
116.311945009195)) ;
#165801 = CARTESIAN_POINT('Ctrl Pts',(-20.0458671823647,-13.1860118375269,
116.382318162004)) ;
#165802 = CARTESIAN_POINT('Ctrl Pts',(-20.0689718709441,-13.1694298342593,
116.452691314813)) ;
#165803 = CARTESIAN_POINT('Ctrl Pts',(-19.995168025,-13.169429800225,116.476922348811)) ;
#165804 = CARTESIAN_POINT('Ctrl Pts',(-19.9213641790559,-13.1694297661908,
116.501153382809)) ;
#165805 = CARTESIAN_POINT('Ctrl Pts',(-19.8982594904765,-13.1860117694584,
116.43078023)) ;
#165806 = CARTESIAN_POINT('Ctrl Pts',(-19.9161358077784,-13.4763914936473,
116.449746710291)) ;
#165807 = CARTESIAN_POINT('Ctrl Pts',(-19.8924837990799,-13.4727232020181,
116.377706508879)) ;
#165808 = CARTESIAN_POINT('Ctrl Pts',(-19.9662876420239,-13.4727232458184,
116.353475465744)) ;
#165809 = CARTESIAN_POINT('Ctrl Pts',(-20.040091484968,-13.4727232896187,
116.329244422608)) ;
#165810 = CARTESIAN_POINT('Ctrl Pts',(-20.0637434936665,-13.4763915812479,
116.40128462402)) ;
#165811 = CARTESIAN_POINT('Ctrl Pts',(-20.087395502365,-13.4800598728771,
116.473324825431)) ;
#165812 = CARTESIAN_POINT('Ctrl Pts',(-20.0135916594209,-13.4800598290768,
116.497555868567)) ;
#165813 = CARTESIAN_POINT('Ctrl Pts',(-19.9397878164769,-13.4800597852765,
116.521786911702)) ;
#165814 = CARTESIAN_POINT('Ctrl Pts',(-19.9161358077784,-13.4763914936473,
116.449746710291)) ;
#165815 = CARTESIAN_POINT('Ctrl Pts',(-19.9095920128141,-13.7633156829476,
116.394237436287)) ;
#165816 = CARTESIAN_POINT('Ctrl Pts',(-19.887098792294,-13.7396092222064,
116.325726716888)) ;
#165817 = CARTESIAN_POINT('Ctrl Pts',(-19.9609026306121,-13.7396092733025,
116.301495659662)) ;
#165818 = CARTESIAN_POINT('Ctrl Pts',(-20.0347064689303,-13.7396093243987,
116.277264602437)) ;
#165819 = CARTESIAN_POINT('Ctrl Pts',(-20.0571996894504,-13.7633157851398,
116.345775321837)) ;
#165820 = CARTESIAN_POINT('Ctrl Pts',(-20.0796929099706,-13.787022245881,
116.414286041237)) ;
#165821 = CARTESIAN_POINT('Ctrl Pts',(-20.0058890716524,-13.7870221947849,
116.438517098462)) ;
#165822 = CARTESIAN_POINT('Ctrl Pts',(-19.9320852333342,-13.7870221436888,
116.462748155687)) ;
#165823 = CARTESIAN_POINT('Ctrl Pts',(-19.9095920128141,-13.7633156829476,
116.394237436287)) ;
#165824 = CARTESIAN_POINT('Ctrl Pts',(-19.8801111722998,-14.0239605605361,
116.269074441211)) ;
#165825 = CARTESIAN_POINT('Ctrl Pts',(-19.8603756897852,-13.9820221332016,
116.208963346964)) ;
#165826 = CARTESIAN_POINT('Ctrl Pts',(-19.9341795227265,-13.9820221845115,
116.184732273362)) ;
#165827 = CARTESIAN_POINT('Ctrl Pts',(-20.0079833556679,-13.9820222358214,
116.16050119976)) ;
#165828 = CARTESIAN_POINT('Ctrl Pts',(-20.0277188381826,-14.023960663156,
116.220612294007)) ;
#165829 = CARTESIAN_POINT('Ctrl Pts',(-20.0474543206972,-14.0658990904905,
116.280723388254)) ;
#165830 = CARTESIAN_POINT('Ctrl Pts',(-19.9736504877559,-14.0658990391806,
116.304954461856)) ;
#165831 = CARTESIAN_POINT('Ctrl Pts',(-19.8998466548145,-14.0658989878706,
116.329185535458)) ;
#165832 = CARTESIAN_POINT('Ctrl Pts',(-19.8801111722998,-14.0239605605361,
116.269074441211)) ;
#165833 = CARTESIAN_POINT('Ctrl Pts',(-19.8302954553483,-14.2421936446632,
116.081819032021)) ;
#165834 = CARTESIAN_POINT('Ctrl Pts',(-19.8147444706435,-14.1849578741807,
116.034453243106)) ;
#165835 = CARTESIAN_POINT('Ctrl Pts',(-19.8885482976305,-14.1849579203882,
116.010222151368)) ;
#165836 = CARTESIAN_POINT('Ctrl Pts',(-19.9623521246174,-14.1849579665956,
115.98599105963)) ;
#165837 = CARTESIAN_POINT('Ctrl Pts',(-19.9779031093222,-14.2421937370781,
116.033356848544)) ;
#165838 = CARTESIAN_POINT('Ctrl Pts',(-19.9934540940269,-14.2994295075606,
116.080722637459)) ;
#165839 = CARTESIAN_POINT('Ctrl Pts',(-19.91965026704,-14.2994294613532,116.104953729197)) ;
#165840 = CARTESIAN_POINT('Ctrl Pts',(-19.8458464400531,-14.2994294151457,
116.129184820935)) ;
#165841 = CARTESIAN_POINT('Ctrl Pts',(-19.8302954553483,-14.2421936446632,
116.081819032021)) ;
#165842 = CARTESIAN_POINT('Ctrl Pts',(-19.7649637327425,-14.4005934040497,
115.847505400487)) ;
#165843 = CARTESIAN_POINT('Ctrl Pts',(-19.7546825121778,-14.3322159891563,
115.816190462997)) ;
#165844 = CARTESIAN_POINT('Ctrl Pts',(-19.8284863340784,-14.3322160226317,
115.791959355766)) ;
#165845 = CARTESIAN_POINT('Ctrl Pts',(-19.902290155979,-14.332216056107,115.767728248536)) ;
#165846 = CARTESIAN_POINT('Ctrl Pts',(-19.9125713765437,-14.4005934710005,
115.799043186026)) ;
#165847 = CARTESIAN_POINT('Ctrl Pts',(-19.9228525971083,-14.4689708858939,
115.830358123516)) ;
#165848 = CARTESIAN_POINT('Ctrl Pts',(-19.8490487752077,-14.4689708524185,
115.854589230747)) ;
#165849 = CARTESIAN_POINT('Ctrl Pts',(-19.7752449533071,-14.4689708189432,
115.878820337977)) ;
#165850 = CARTESIAN_POINT('Ctrl Pts',(-19.7649637327425,-14.4005934040497,
115.847505400487)) ;
#165851 = CARTESIAN_POINT('Ctrl Pts',(-19.6886669174365,-14.4895021228897,
115.579514611263)) ;
#165852 = CARTESIAN_POINT('Ctrl Pts',(-19.6844341898727,-14.4148177682025,
115.566622407693)) ;
#165853 = CARTESIAN_POINT('Ctrl Pts',(-19.7582380072419,-14.4148177835068,
115.542391286661)) ;
#165854 = CARTESIAN_POINT('Ctrl Pts',(-19.8320418246112,-14.4148177988111,
115.518160165629)) ;
#165855 = CARTESIAN_POINT('Ctrl Pts',(-19.836274552175,-14.4895021534983,
115.531052369199)) ;
#165856 = CARTESIAN_POINT('Ctrl Pts',(-19.8405072797388,-14.5641865081855,
115.54394457277)) ;
#165857 = CARTESIAN_POINT('Ctrl Pts',(-19.7667034623695,-14.5641864928812,
115.568175693802)) ;
#165858 = CARTESIAN_POINT('Ctrl Pts',(-19.6928996450003,-14.5641864775769,
115.592406814834)) ;
#165859 = CARTESIAN_POINT('Ctrl Pts',(-19.6886669174365,-14.4895021228897,
115.579514611263)) ;
#165860 = CARTESIAN_POINT('Ctrl Pts',(-19.6086131782422,-14.5012817728617,
115.300312081332)) ;
#165861 = CARTESIAN_POINT('Ctrl Pts',(-19.6106952959586,-14.425666653241,
115.306653877699)) ;
#165862 = CARTESIAN_POINT('Ctrl Pts',(-19.6844991112022,-14.4256666452889,
115.282422750192)) ;
#165863 = CARTESIAN_POINT('Ctrl Pts',(-19.7583029264457,-14.4256666373369,
115.258191622685)) ;
#165864 = CARTESIAN_POINT('Ctrl Pts',(-19.7562208087292,-14.5012817569575,
115.251849826318)) ;
#165865 = CARTESIAN_POINT('Ctrl Pts',(-19.7541386910127,-14.5768968765781,
115.245508029951)) ;
#165866 = CARTESIAN_POINT('Ctrl Pts',(-19.6803348757692,-14.5768968845302,
115.269739157458)) ;
#165867 = CARTESIAN_POINT('Ctrl Pts',(-19.6065310605257,-14.5768968924823,
115.293970284964)) ;
#165868 = CARTESIAN_POINT('Ctrl Pts',(-19.6086131782422,-14.5012817728617,
115.300312081332)) ;
#165869 = CARTESIAN_POINT('Ctrl Pts',(-19.5302683146018,-14.43501211062,115.026040039372)) ;
#165870 = CARTESIAN_POINT('Ctrl Pts',(-19.5385607693486,-14.363912820796,
115.051297520427)) ;
#165871 = CARTESIAN_POINT('Ctrl Pts',(-19.6123645843789,-14.3639127866614,
115.027066392271)) ;
#165872 = CARTESIAN_POINT('Ctrl Pts',(-19.6861683994091,-14.3639127525269,
115.002835264114)) ;
#165873 = CARTESIAN_POINT('Ctrl Pts',(-19.6778759446623,-14.4350120423509,
114.97757778306)) ;
#165874 = CARTESIAN_POINT('Ctrl Pts',(-19.6695834899155,-14.506111332175,
114.952320302005)) ;
#165875 = CARTESIAN_POINT('Ctrl Pts',(-19.5957796748852,-14.5061113663095,
114.976551430162)) ;
#165876 = CARTESIAN_POINT('Ctrl Pts',(-19.521975859855,-14.5061114004441,
115.000782558318)) ;
#165877 = CARTESIAN_POINT('Ctrl Pts',(-19.5302683146018,-14.43501211062,115.026040039372)) ;
#165878 = CARTESIAN_POINT('Ctrl Pts',(-19.4613020602763,-14.2968843843662,
114.780704827686)) ;
#165879 = CARTESIAN_POINT('Ctrl Pts',(-19.4751514840979,-14.2353253070851,
114.822887939996)) ;
#165880 = CARTESIAN_POINT('Ctrl Pts',(-19.5489553020923,-14.2353252479564,
114.798656820868)) ;
#165881 = CARTESIAN_POINT('Ctrl Pts',(-19.6227591200867,-14.2353251888277,
114.77442570174)) ;
#165882 = CARTESIAN_POINT('Ctrl Pts',(-19.6089096962652,-14.2968842661087,
114.732242589431)) ;
#165883 = CARTESIAN_POINT('Ctrl Pts',(-19.5950602724436,-14.3584433433898,
114.690059477121)) ;
#165884 = CARTESIAN_POINT('Ctrl Pts',(-19.5212564544492,-14.3584434025185,
114.714290596249)) ;
#165885 = CARTESIAN_POINT('Ctrl Pts',(-19.4474526364548,-14.3584434616473,
114.738521715376)) ;
#165886 = CARTESIAN_POINT('Ctrl Pts',(-19.4613020602763,-14.2968843843662,
114.780704827686)) ;
#165887 = CARTESIAN_POINT('Ctrl Pts',(-19.4062019880191,-14.0952651274861,
114.577384783976)) ;
#165888 = CARTESIAN_POINT('Ctrl Pts',(-19.4246530089548,-14.0476919571474,
114.633583618702)) ;
#165889 = CARTESIAN_POINT('Ctrl Pts',(-19.4984568320329,-14.0476918755957,
114.609352515058)) ;
#165890 = CARTESIAN_POINT('Ctrl Pts',(-19.5722606551109,-14.047691794044,
114.585121411415)) ;
#165891 = CARTESIAN_POINT('Ctrl Pts',(-19.5538096341753,-14.0952649643827,
114.528922576688)) ;
#165892 = CARTESIAN_POINT('Ctrl Pts',(-19.5353586132396,-14.1428381347214,
114.472723741961)) ;
#165893 = CARTESIAN_POINT('Ctrl Pts',(-19.4615547901615,-14.1428382162731,
114.496954845605)) ;
#165894 = CARTESIAN_POINT('Ctrl Pts',(-19.3877509670834,-14.1428382978248,
114.521185949249)) ;
#165895 = CARTESIAN_POINT('Ctrl Pts',(-19.4062019880191,-14.0952651274861,
114.577384783976)) ;
#165896 = CARTESIAN_POINT('Ctrl Pts',(-19.3702132925559,-13.8453444760412,
114.432330882525)) ;
#165897 = CARTESIAN_POINT('Ctrl Pts',(-19.3919372890595,-13.8151498849244,
114.498498672785)) ;
#165898 = CARTESIAN_POINT('Ctrl Pts',(-19.4657411193459,-13.8151497867456,
114.474267591096)) ;
#165899 = CARTESIAN_POINT('Ctrl Pts',(-19.5395449496322,-13.8151496885667,
114.450036509408)) ;
#165900 = CARTESIAN_POINT('Ctrl Pts',(-19.5178209531287,-13.8453442796835,
114.383868719148)) ;
#165901 = CARTESIAN_POINT('Ctrl Pts',(-19.4960969566251,-13.8755388708002,
114.317700928887)) ;
#165902 = CARTESIAN_POINT('Ctrl Pts',(-19.4222931263387,-13.8755389689791,
114.341932010576)) ;
#165903 = CARTESIAN_POINT('Ctrl Pts',(-19.3484892960523,-13.8755390671579,
114.366163092264)) ;
#165904 = CARTESIAN_POINT('Ctrl Pts',(-19.3702132925559,-13.8453444760412,
114.432330882525)) ;
#165905 = CARTESIAN_POINT('Ctrl Pts',(-19.356514093291,-13.5639203016943,
114.355047993229)) ;
#165906 = CARTESIAN_POINT('Ctrl Pts',(-19.3799623708669,-13.5533288537195,
114.426467665453)) ;
#165907 = CARTESIAN_POINT('Ctrl Pts',(-19.4537662097389,-13.5533287463832,
114.402236609915)) ;
#165908 = CARTESIAN_POINT('Ctrl Pts',(-19.5275700486109,-13.5533286390469,
114.378005554377)) ;
#165909 = CARTESIAN_POINT('Ctrl Pts',(-19.504121771035,-13.5639200870216,
114.306585882153)) ;
#165910 = CARTESIAN_POINT('Ctrl Pts',(-19.4806734934592,-13.5745115349964,
114.235166209929)) ;
#165911 = CARTESIAN_POINT('Ctrl Pts',(-19.4068696545872,-13.5745116423327,
114.259397265467)) ;
#165912 = CARTESIAN_POINT('Ctrl Pts',(-19.3330658157152,-13.574511749669,
114.283628321005)) ;
#165913 = CARTESIAN_POINT('Ctrl Pts',(-19.356514093291,-13.5639203016943,
114.355047993229)) ;
#165914 = CARTESIAN_POINT('Ctrl Pts',(-19.3670894957072,-13.2722319962961,
114.351731726315)) ;
#165915 = CARTESIAN_POINT('Ctrl Pts',(-19.3905693400295,-13.2819894198182,
114.423247545754)) ;
#165916 = CARTESIAN_POINT('Ctrl Pts',(-19.4643731879902,-13.2819893125246,
114.399016517899)) ;
#165917 = CARTESIAN_POINT('Ctrl Pts',(-19.538177035951,-13.281989205231,114.374785490044)) ;
#165918 = CARTESIAN_POINT('Ctrl Pts',(-19.5146971916288,-13.2722317817088,
114.303269670605)) ;
#165919 = CARTESIAN_POINT('Ctrl Pts',(-19.4912173473065,-13.2624743581867,
114.231753851165)) ;
#165920 = CARTESIAN_POINT('Ctrl Pts',(-19.4174134993458,-13.2624744654803,
114.255984879021)) ;
#165921 = CARTESIAN_POINT('Ctrl Pts',(-19.343609651385,-13.262474572774,114.280215906876)) ;
#165922 = CARTESIAN_POINT('Ctrl Pts',(-19.3670894957072,-13.2722319962961,
114.351731726315)) ;
#165923 = CARTESIAN_POINT('Ctrl Pts',(-19.4014893907637,-12.9927108288244,
114.421205255979)) ;
#165924 = CARTESIAN_POINT('Ctrl Pts',(-19.4233327297624,-13.0219980101555,
114.487736544236)) ;
#165925 = CARTESIAN_POINT('Ctrl Pts',(-19.4971365863264,-13.0219979113137,
114.463505542585)) ;
#165926 = CARTESIAN_POINT('Ctrl Pts',(-19.5709404428904,-13.0219978124719,
114.439274540934)) ;
#165927 = CARTESIAN_POINT('Ctrl Pts',(-19.5490971038917,-12.9927106311408,
114.372743252677)) ;
#165928 = CARTESIAN_POINT('Ctrl Pts',(-19.527253764893,-12.9634234498097,
114.306211964419)) ;
#165929 = CARTESIAN_POINT('Ctrl Pts',(-19.453449908329,-12.9634235486515,
114.330442966071)) ;
#165930 = CARTESIAN_POINT('Ctrl Pts',(-19.379646051765,-12.9634236474933,
114.354673967722)) ;
#165931 = CARTESIAN_POINT('Ctrl Pts',(-19.4014893907637,-12.9927108288244,
114.421205255979)) ;
#165932 = CARTESIAN_POINT('Ctrl Pts',(-19.4584767230081,-12.7419081122581,
114.559249348352)) ;
#165933 = CARTESIAN_POINT('Ctrl Pts',(-19.4771091783895,-12.7887491311702,
114.616000803142)) ;
#165934 = CARTESIAN_POINT('Ctrl Pts',(-19.5509130422714,-12.78874904886,114.591769823781)) ;
#165935 = CARTESIAN_POINT('Ctrl Pts',(-19.6247169061534,-12.7887489665498,
114.567538844419)) ;
#165936 = CARTESIAN_POINT('Ctrl Pts',(-19.606084450772,-12.7419079476376,
114.510787389628)) ;
#165937 = CARTESIAN_POINT('Ctrl Pts',(-19.5874519953906,-12.6950669287254,
114.454035934838)) ;
#165938 = CARTESIAN_POINT('Ctrl Pts',(-19.5136481315087,-12.6950670110357,
114.4782669142)) ;
#165939 = CARTESIAN_POINT('Ctrl Pts',(-19.4398442676267,-12.6950670933459,
114.502497893561)) ;
#165940 = CARTESIAN_POINT('Ctrl Pts',(-19.4584767230081,-12.7419081122581,
114.559249348352)) ;
#165941 = CARTESIAN_POINT('Ctrl Pts',(-19.5343623620457,-12.5402274188012,
114.754960677607)) ;
#165942 = CARTESIAN_POINT('Ctrl Pts',(-19.5484574986284,-12.6012191381552,
114.797892191371)) ;
#165943 = CARTESIAN_POINT('Ctrl Pts',(-19.6222613678262,-12.6012190780927,
114.773661228201)) ;
#165944 = CARTESIAN_POINT('Ctrl Pts',(-19.6960652370241,-12.6012190180302,
114.74943026503)) ;
#165945 = CARTESIAN_POINT('Ctrl Pts',(-19.6819701004414,-12.5402272986761,
114.706498751266)) ;
#165946 = CARTESIAN_POINT('Ctrl Pts',(-19.6678749638587,-12.479235579322,
114.663567237502)) ;
#165947 = CARTESIAN_POINT('Ctrl Pts',(-19.5940710946608,-12.4792356393845,
114.687798200673)) ;
#165948 = CARTESIAN_POINT('Ctrl Pts',(-19.520267225463,-12.4792356994471,
114.712029163843)) ;
#165949 = CARTESIAN_POINT('Ctrl Pts',(-19.5343623620457,-12.5402274188012,
114.754960677607)) ;
#165950 = CARTESIAN_POINT('Ctrl Pts',(-19.624777106285,-12.4011175779625,
114.994845960025)) ;
#165951 = CARTESIAN_POINT('Ctrl Pts',(-19.6333154990108,-12.4719130809355,
115.020852528492)) ;
#165952 = CARTESIAN_POINT('Ctrl Pts',(-19.707119370965,-12.4719130465785,
114.996621573717)) ;
#165953 = CARTESIAN_POINT('Ctrl Pts',(-19.7809232429191,-12.4719130122216,
114.972390618941)) ;
#165954 = CARTESIAN_POINT('Ctrl Pts',(-19.7723848501933,-12.4011175092485,
114.946384050474)) ;
#165955 = CARTESIAN_POINT('Ctrl Pts',(-19.7638464574675,-12.3303220062755,
114.920377482007)) ;
#165956 = CARTESIAN_POINT('Ctrl Pts',(-19.6900425855133,-12.3303220406325,
114.944608436782)) ;
#165957 = CARTESIAN_POINT('Ctrl Pts',(-19.6162387135592,-12.3303220749894,
114.968839391557)) ;
#165958 = CARTESIAN_POINT('Ctrl Pts',(-19.624777106285,-12.4011175779625,
114.994845960025)) ;
#165959 = CARTESIAN_POINT('Ctrl Pts',(-19.7234667624237,-12.3349520470046,
115.260072553625)) ;
#165960 = CARTESIAN_POINT('Ctrl Pts',(-19.7258594391485,-12.4104731774987,
115.267360262672)) ;
#165961 = CARTESIAN_POINT('Ctrl Pts',(-19.7996633114999,-12.4104731691892,
115.243129309107)) ;
#165962 = CARTESIAN_POINT('Ctrl Pts',(-19.8734671838513,-12.4104731608796,
115.218898355542)) ;
#165963 = CARTESIAN_POINT('Ctrl Pts',(-19.8710745071266,-12.3349520303855,
115.211610646495)) ;
#165964 = CARTESIAN_POINT('Ctrl Pts',(-19.8686818304018,-12.2594308998913,
115.204322937447)) ;
#165965 = CARTESIAN_POINT('Ctrl Pts',(-19.7948779580504,-12.2594309082008,
115.228553891012)) ;
#165966 = CARTESIAN_POINT('Ctrl Pts',(-19.7210740856989,-12.2594309165104,
115.252784844578)) ;
#165967 = CARTESIAN_POINT('Ctrl Pts',(-19.7234667624237,-12.3349520470046,
115.260072553625)) ;
#165968 = CARTESIAN_POINT('Ctrl Pts',(-19.8252582804317,-12.346456548631,
115.534462410052)) ;
#165969 = CARTESIAN_POINT('Ctrl Pts',(-19.8212853892728,-12.4212888141347,
115.522361626262)) ;
#165970 = CARTESIAN_POINT('Ctrl Pts',(-19.8950892589879,-12.4212888296186,
115.498130664667)) ;
#165971 = CARTESIAN_POINT('Ctrl Pts',(-19.9688931287029,-12.4212888451025,
115.473899703072)) ;
#165972 = CARTESIAN_POINT('Ctrl Pts',(-19.9728660198618,-12.3464565795988,
115.486000486862)) ;
#165973 = CARTESIAN_POINT('Ctrl Pts',(-19.9768389110207,-12.2716243140951,
115.498101270651)) ;
#165974 = CARTESIAN_POINT('Ctrl Pts',(-19.9030350413057,-12.2716242986112,
115.522332232247)) ;
#165975 = CARTESIAN_POINT('Ctrl Pts',(-19.8292311715906,-12.2716242831273,
115.546563193842)) ;
#165976 = CARTESIAN_POINT('Ctrl Pts',(-19.8252582804317,-12.346456548631,
115.534462410052)) ;
#165977 = CARTESIAN_POINT('Ctrl Pts',(-19.9219904763792,-12.4344867986536,
115.793753215516)) ;
#165978 = CARTESIAN_POINT('Ctrl Pts',(-19.9119891025516,-12.5032854856229,
115.763290646093)) ;
#165979 = CARTESIAN_POINT('Ctrl Pts',(-19.9857929683466,-12.5032855202655,
115.739059672558)) ;
#165980 = CARTESIAN_POINT('Ctrl Pts',(-20.0595968341415,-12.503285554908,
115.714828699023)) ;
#165981 = CARTESIAN_POINT('Ctrl Pts',(-20.0695982079691,-12.4344868679388,
115.745291268445)) ;
#165982 = CARTESIAN_POINT('Ctrl Pts',(-20.0795995817966,-12.3656881809695,
115.775753837868)) ;
#165983 = CARTESIAN_POINT('Ctrl Pts',(-20.0057957160017,-12.365688146327,
115.799984811403)) ;
#165984 = CARTESIAN_POINT('Ctrl Pts',(-19.9319918502067,-12.3656881116844,
115.824215784938)) ;
#165985 = CARTESIAN_POINT('Ctrl Pts',(-19.9219904763792,-12.4344867986536,
115.793753215516)) ;
#165986 = CARTESIAN_POINT('Ctrl Pts',(-20.0087826519236,-12.5932721982848,
116.022595185583)) ;
#165987 = CARTESIAN_POINT('Ctrl Pts',(-19.9934412072172,-12.6510887725529,
115.975867621727)) ;
#165988 = CARTESIAN_POINT('Ctrl Pts',(-20.0672450674469,-12.6510888198682,
115.95163663124)) ;
#165989 = CARTESIAN_POINT('Ctrl Pts',(-20.1410489276766,-12.6510888671835,
115.927405640754)) ;
#165990 = CARTESIAN_POINT('Ctrl Pts',(-20.1563903723829,-12.5932722929155,
115.974133204611)) ;
#165991 = CARTESIAN_POINT('Ctrl Pts',(-20.1717318170893,-12.5354557186474,
116.020860768468)) ;
#165992 = CARTESIAN_POINT('Ctrl Pts',(-20.0979279568596,-12.5354556713321,
116.045091758954)) ;
#165993 = CARTESIAN_POINT('Ctrl Pts',(-20.02412409663,-12.5354556240167,116.06932274944)) ;
#165994 = CARTESIAN_POINT('Ctrl Pts',(-20.0087826519236,-12.5932721982848,
116.022595185583)) ;
#165995 = CARTESIAN_POINT('Ctrl Pts',(-20.0794532739981,-12.8103924299054,
116.202472937064)) ;
#165996 = CARTESIAN_POINT('Ctrl Pts',(-20.0598863895537,-12.8531370145114,
116.142875365397)) ;
#165997 = CARTESIAN_POINT('Ctrl Pts',(-20.1336902439871,-12.8531370683972,
116.118644357256)) ;
#165998 = CARTESIAN_POINT('Ctrl Pts',(-20.2074940984206,-12.8531371222829,
116.094413349116)) ;
#165999 = CARTESIAN_POINT('Ctrl Pts',(-20.2270609828651,-12.810392537677,
116.154010920783)) ;
#166000 = CARTESIAN_POINT('Ctrl Pts',(-20.2466278673096,-12.767647953071,
116.21360849245)) ;
#166001 = CARTESIAN_POINT('Ctrl Pts',(-20.1728240128761,-12.7676478991852,
116.237839500591)) ;
#166002 = CARTESIAN_POINT('Ctrl Pts',(-20.0990201584426,-12.7676478452995,
116.262070508731)) ;
#166003 = CARTESIAN_POINT('Ctrl Pts',(-20.0794532739981,-12.8103924299054,
116.202472937064)) ;
#166004 = CARTESIAN_POINT('Ctrl Pts',(-20.1303453815953,-13.0726323412443,
116.321870495346)) ;
#166005 = CARTESIAN_POINT('Ctrl Pts',(-20.107932288737,-13.0971322435792,
116.253603831893)) ;
#166006 = CARTESIAN_POINT('Ctrl Pts',(-20.1817361372741,-13.0971322955942,
116.229372805793)) ;
#166007 = CARTESIAN_POINT('Ctrl Pts',(-20.2555399858112,-13.0971323476091,
116.205141779694)) ;
#166008 = CARTESIAN_POINT('Ctrl Pts',(-20.2779530786695,-13.0726324452743,
116.273408443147)) ;
#166009 = CARTESIAN_POINT('Ctrl Pts',(-20.3003661715278,-13.0481325429394,
116.3416751066)) ;
#166010 = CARTESIAN_POINT('Ctrl Pts',(-20.2265623229907,-13.0481324909245,
116.3659061327)) ;
#166011 = CARTESIAN_POINT('Ctrl Pts',(-20.1527584744536,-13.0481324389095,
116.3901371588)) ;
#166012 = CARTESIAN_POINT('Ctrl Pts',(-20.1303453815953,-13.0726323412443,
116.321870495346)) ;
#166013 = CARTESIAN_POINT('Ctrl Pts',(-20.1578525019935,-13.3588849654739,
116.370163901629)) ;
#166014 = CARTESIAN_POINT('Ctrl Pts',(-20.1342191538104,-13.3634353466295,
116.298180537171)) ;
#166015 = CARTESIAN_POINT('Ctrl Pts',(-20.2080229977771,-13.3634353921752,
116.27394949715)) ;
#166016 = CARTESIAN_POINT('Ctrl Pts',(-20.2818268417438,-13.3634354377208,
116.24971845713)) ;
#166017 = CARTESIAN_POINT('Ctrl Pts',(-20.3054601899268,-13.3588850565651,
116.321701821588)) ;
#166018 = CARTESIAN_POINT('Ctrl Pts',(-20.3290935381099,-13.3543346754094,
116.393685186046)) ;
#166019 = CARTESIAN_POINT('Ctrl Pts',(-20.2552896941432,-13.3543346298638,
116.417916226066)) ;
#166020 = CARTESIAN_POINT('Ctrl Pts',(-20.1814858501765,-13.3543345843182,
116.442147266087)) ;
#166021 = CARTESIAN_POINT('Ctrl Pts',(-20.1578525019935,-13.3588849654739,
116.370163901629)) ;
#166022 = CARTESIAN_POINT('Ctrl Pts',(-20.1611723681104,-13.6479812710763,
116.344954804695)) ;
#166023 = CARTESIAN_POINT('Ctrl Pts',(-20.1380024070174,-13.6323532637261,
116.274382842406)) ;
#166024 = CARTESIAN_POINT('Ctrl Pts',(-20.2118062476732,-13.6323533009956,
116.250151792301)) ;
#166025 = CARTESIAN_POINT('Ctrl Pts',(-20.285610088329,-13.632353338265,116.225920742195)) ;
#166026 = CARTESIAN_POINT('Ctrl Pts',(-20.308780049422,-13.6479813456151,
116.296492704485)) ;
#166027 = CARTESIAN_POINT('Ctrl Pts',(-20.331950010515,-13.6636093529653,
116.367064666774)) ;
#166028 = CARTESIAN_POINT('Ctrl Pts',(-20.2581461698591,-13.6636093156958,
116.39129571688)) ;
#166029 = CARTESIAN_POINT('Ctrl Pts',(-20.1843423292033,-13.6636092784264,
116.415526766985)) ;
#166030 = CARTESIAN_POINT('Ctrl Pts',(-20.1611723681104,-13.6479812710763,
116.344954804695)) ;
#166031 = CARTESIAN_POINT('Ctrl Pts',(-20.1407285861011,-13.9223253071587,
116.24714907814)) ;
#166032 = CARTESIAN_POINT('Ctrl Pts',(-20.1196862628137,-13.8875179705717,
116.183057557135)) ;
#166033 = CARTESIAN_POINT('Ctrl Pts',(-20.1934901017956,-13.8875179960034,
116.158826501931)) ;
#166034 = CARTESIAN_POINT('Ctrl Pts',(-20.2672939407774,-13.8875180214352,
116.134595446728)) ;
#166035 = CARTESIAN_POINT('Ctrl Pts',(-20.2883362640648,-13.9223253580222,
116.198686967732)) ;
#166036 = CARTESIAN_POINT('Ctrl Pts',(-20.3093785873523,-13.9571326946092,
116.262778488737)) ;
#166037 = CARTESIAN_POINT('Ctrl Pts',(-20.2355747483704,-13.9571326691774,
116.287009543941)) ;
#166038 = CARTESIAN_POINT('Ctrl Pts',(-20.1617709093885,-13.9571326437457,
116.311240599144)) ;
#166039 = CARTESIAN_POINT('Ctrl Pts',(-20.1407285861011,-13.9223253071587,
116.24714907814)) ;
#166040 = CARTESIAN_POINT('Ctrl Pts',(-20.0987741035012,-14.1598247969233,
116.083922230041)) ;
#166041 = CARTESIAN_POINT('Ctrl Pts',(-20.0813627450779,-14.1083816279705,
116.030890042007)) ;
#166042 = CARTESIAN_POINT('Ctrl Pts',(-20.1551665838028,-14.1083816430256,
116.006658986021)) ;
#166043 = CARTESIAN_POINT('Ctrl Pts',(-20.2289704225278,-14.1083816580807,
115.982427930034)) ;
#166044 = CARTESIAN_POINT('Ctrl Pts',(-20.2463817809511,-14.1598248270335,
116.035460118068)) ;
#166045 = CARTESIAN_POINT('Ctrl Pts',(-20.2637931393744,-14.2112679959863,
116.088492306103)) ;
#166046 = CARTESIAN_POINT('Ctrl Pts',(-20.1899893006495,-14.2112679809312,
116.112723362089)) ;
#166047 = CARTESIAN_POINT('Ctrl Pts',(-20.1161854619245,-14.2112679658761,
116.136954418075)) ;
#166048 = CARTESIAN_POINT('Ctrl Pts',(-20.0987741035012,-14.1598247969233,
116.083922230041)) ;
#166049 = CARTESIAN_POINT('Ctrl Pts',(-20.0388440499086,-14.3448019435796,
115.865824123426)) ;
#166050 = CARTESIAN_POINT('Ctrl Pts',(-20.0263268379977,-14.2803646984367,
115.827698715844)) ;
#166051 = CARTESIAN_POINT('Ctrl Pts',(-20.1001306778157,-14.2803647047343,
115.803467663186)) ;
#166052 = CARTESIAN_POINT('Ctrl Pts',(-20.1739345176336,-14.2803647110319,
115.779236610529)) ;
#166053 = CARTESIAN_POINT('Ctrl Pts',(-20.1864517295445,-14.3448019561748,
115.817362018112)) ;
#166054 = CARTESIAN_POINT('Ctrl Pts',(-20.1989689414554,-14.4092392013176,
115.855487425695)) ;
#166055 = CARTESIAN_POINT('Ctrl Pts',(-20.1251651016375,-14.40923919502,115.879718478352)) ;
#166056 = CARTESIAN_POINT('Ctrl Pts',(-20.0513612618195,-14.4092391887224,
115.903949531009)) ;
#166057 = CARTESIAN_POINT('Ctrl Pts',(-20.0388440499086,-14.3448019435796,
115.865824123426)) ;
#166058 = CARTESIAN_POINT('Ctrl Pts',(-19.9663582699684,-14.4625579261475,
115.609608257701)) ;
#166059 = CARTESIAN_POINT('Ctrl Pts',(-19.9596169228226,-14.3898012184393,
115.589075202144)) ;
#166060 = CARTESIAN_POINT('Ctrl Pts',(-20.0334207640732,-14.3898012199962,
115.564844153851)) ;
#166061 = CARTESIAN_POINT('Ctrl Pts',(-20.1072246053238,-14.3898012215531,
115.540613105557)) ;
#166062 = CARTESIAN_POINT('Ctrl Pts',(-20.1139659524696,-14.4625579292612,
115.561146161114)) ;
#166063 = CARTESIAN_POINT('Ctrl Pts',(-20.1207072996154,-14.5353146369693,
115.581679216671)) ;
#166064 = CARTESIAN_POINT('Ctrl Pts',(-20.0469034583648,-14.5353146354125,
115.605910264964)) ;
#166065 = CARTESIAN_POINT('Ctrl Pts',(-19.9730996171142,-14.5353146338556,
115.630141313258)) ;
#166066 = CARTESIAN_POINT('Ctrl Pts',(-19.9663582699684,-14.4625579261475,
115.609608257701)) ;
#166067 = CARTESIAN_POINT('Ctrl Pts',(-19.8873776134028,-14.5058691718866,
115.333726330134)) ;
#166068 = CARTESIAN_POINT('Ctrl Pts',(-19.8868719421637,-14.4299792998369,
115.332186137181)) ;
#166069 = CARTESIAN_POINT('Ctrl Pts',(-19.960675784752,-14.429979299475,115.307955092962)) ;
#166070 = CARTESIAN_POINT('Ctrl Pts',(-20.0344796273404,-14.4299792991131,
115.283724048743)) ;
#166071 = CARTESIAN_POINT('Ctrl Pts',(-20.0349852985795,-14.5058691711628,
115.285264241697)) ;
#166072 = CARTESIAN_POINT('Ctrl Pts',(-20.0354909698187,-14.5817590432124,
115.28680443465)) ;
#166073 = CARTESIAN_POINT('Ctrl Pts',(-19.9616871272303,-14.5817590435743,
115.311035478869)) ;
#166074 = CARTESIAN_POINT('Ctrl Pts',(-19.887883284642,-14.5817590439362,
115.335266523088)) ;
#166075 = CARTESIAN_POINT('Ctrl Pts',(-19.8873776134028,-14.5058691718866,
115.333726330134)) ;
#166076 = CARTESIAN_POINT('Ctrl Pts',(-19.8074081898511,-14.471221053196,
115.054555605598)) ;
#166077 = CARTESIAN_POINT('Ctrl Pts',(-19.8132226145073,-14.3976366078093,
115.072265404916)) ;
#166078 = CARTESIAN_POINT('Ctrl Pts',(-19.8870264584312,-14.397636607939,
115.048034364765)) ;
#166079 = CARTESIAN_POINT('Ctrl Pts',(-19.9608303023551,-14.3976366080687,
115.023803324613)) ;
#166080 = CARTESIAN_POINT('Ctrl Pts',(-19.9550158776989,-14.4712210534553,
115.006093525296)) ;
#166081 = CARTESIAN_POINT('Ctrl Pts',(-19.9492014530427,-14.5448054988419,
114.988383725979)) ;
#166082 = CARTESIAN_POINT('Ctrl Pts',(-19.8753976091188,-14.5448054987123,
115.01261476613)) ;
#166083 = CARTESIAN_POINT('Ctrl Pts',(-19.8015937651949,-14.5448054985826,
115.036845806281)) ;
#166084 = CARTESIAN_POINT('Ctrl Pts',(-19.8074081898511,-14.471221053196,
115.054555605598)) ;
#166085 = CARTESIAN_POINT('Ctrl Pts',(-19.7339488645536,-14.3613267795073,
114.795410318101)) ;
#166086 = CARTESIAN_POINT('Ctrl Pts',(-19.7456340819167,-14.2953066789367,
114.831001604723)) ;
#166087 = CARTESIAN_POINT('Ctrl Pts',(-19.8194379262271,-14.2953066805575,
114.806770565749)) ;
#166088 = CARTESIAN_POINT('Ctrl Pts',(-19.8932417705375,-14.2953066821784,
114.782539526775)) ;
#166089 = CARTESIAN_POINT('Ctrl Pts',(-19.8815565531744,-14.361326782749,
114.746948240154)) ;
#166090 = CARTESIAN_POINT('Ctrl Pts',(-19.8698713358113,-14.4273468833197,
114.711356953532)) ;
#166091 = CARTESIAN_POINT('Ctrl Pts',(-19.7960674915009,-14.4273468816988,
114.735587992506)) ;
#166092 = CARTESIAN_POINT('Ctrl Pts',(-19.7222636471905,-14.4273468800779,
114.75981903148)) ;
#166093 = CARTESIAN_POINT('Ctrl Pts',(-19.7339488645536,-14.3613267795073,
114.795410318101)) ;
#166094 = CARTESIAN_POINT('Ctrl Pts',(-19.6723166521497,-14.1831445066676,
114.572116798133)) ;
#166095 = CARTESIAN_POINT('Ctrl Pts',(-19.6890592182227,-14.1294690686809,
114.623111952935)) ;
#166096 = CARTESIAN_POINT('Ctrl Pts',(-19.7628630622087,-14.1294690707301,
114.598880912973)) ;
#166097 = CARTESIAN_POINT('Ctrl Pts',(-19.8366669061947,-14.1294690727794,
114.574649873011)) ;
#166098 = CARTESIAN_POINT('Ctrl Pts',(-19.8199243401217,-14.1831445107661,
114.523654718209)) ;
#166099 = CARTESIAN_POINT('Ctrl Pts',(-19.8031817740486,-14.2368199487529,
114.472659563407)) ;
#166100 = CARTESIAN_POINT('Ctrl Pts',(-19.7293779300626,-14.2368199467036,
114.496890603369)) ;
#166101 = CARTESIAN_POINT('Ctrl Pts',(-19.6555740860767,-14.2368199446543,
114.521121643331)) ;
#166102 = CARTESIAN_POINT('Ctrl Pts',(-19.6723166521497,-14.1831445066676,
114.572116798133)) ;
#166103 = CARTESIAN_POINT('Ctrl Pts',(-19.6282726005252,-13.9512771233317,
114.40260456507)) ;
#166104 = CARTESIAN_POINT('Ctrl Pts',(-19.6488469329677,-13.9137135164908,
114.465270662026)) ;
#166105 = CARTESIAN_POINT('Ctrl Pts',(-19.7226507763542,-13.9137135169973,
114.441039620238)) ;
#166106 = CARTESIAN_POINT('Ctrl Pts',(-19.7964546197408,-13.9137135175038,
114.41680857845)) ;
#166107 = CARTESIAN_POINT('Ctrl Pts',(-19.7758802872982,-13.9512771243447,
114.354142481495)) ;
#166108 = CARTESIAN_POINT('Ctrl Pts',(-19.7553059548557,-13.9888407311855,
114.291476384539)) ;
#166109 = CARTESIAN_POINT('Ctrl Pts',(-19.6815021114692,-13.988840730679,
114.315707426327)) ;
#166110 = CARTESIAN_POINT('Ctrl Pts',(-19.6076982680827,-13.9888407301726,
114.339938468114)) ;
#166111 = CARTESIAN_POINT('Ctrl Pts',(-19.6282726005252,-13.9512771233317,
114.40260456507)) ;
#166112 = CARTESIAN_POINT('Ctrl Pts',(-19.6052474089062,-13.6804917592119,
114.29698357989)) ;
#166113 = CARTESIAN_POINT('Ctrl Pts',(-19.6281940892339,-13.6617810820817,
114.366875465811)) ;
#166114 = CARTESIAN_POINT('Ctrl Pts',(-19.7019979322277,-13.6617810784038,
114.342644422827)) ;
#166115 = CARTESIAN_POINT('Ctrl Pts',(-19.7758017752214,-13.6617810747259,
114.318413379842)) ;
#166116 = CARTESIAN_POINT('Ctrl Pts',(-19.7528550948936,-13.6804917518562,
114.248521493922)) ;
#166117 = CARTESIAN_POINT('Ctrl Pts',(-19.7299084145659,-13.6992024289864,
114.178629608001)) ;
#166118 = CARTESIAN_POINT('Ctrl Pts',(-19.6561045715721,-13.6992024326643,
114.202860650985)) ;
#166119 = CARTESIAN_POINT('Ctrl Pts',(-19.5823007285784,-13.6992024363421,
114.227091693969)) ;
#166120 = CARTESIAN_POINT('Ctrl Pts',(-19.6052474089062,-13.6804917592119,
114.29698357989)) ;
#166121 = CARTESIAN_POINT('Ctrl Pts',(-19.6057961466648,-13.3916820675785,
114.263270356301)) ;
#166122 = CARTESIAN_POINT('Ctrl Pts',(-19.6294701323659,-13.3931100750182,
114.335377497137)) ;
#166123 = CARTESIAN_POINT('Ctrl Pts',(-19.7032739756634,-13.3931100660094,
114.311146455077)) ;
#166124 = CARTESIAN_POINT('Ctrl Pts',(-19.7770778189608,-13.3931100570005,
114.286915413018)) ;
#166125 = CARTESIAN_POINT('Ctrl Pts',(-19.7534038332597,-13.3916820495608,
114.214808272182)) ;
#166126 = CARTESIAN_POINT('Ctrl Pts',(-19.7297298475586,-13.390254042121,
114.142701131346)) ;
#166127 = CARTESIAN_POINT('Ctrl Pts',(-19.6559260042611,-13.3902540511299,
114.166932173406)) ;
#166128 = CARTESIAN_POINT('Ctrl Pts',(-19.5821221609637,-13.3902540601387,
114.191163215465)) ;
#166129 = CARTESIAN_POINT('Ctrl Pts',(-19.6057961466648,-13.3916820675785,
114.263270356301)) ;
#166130 = CARTESIAN_POINT('Ctrl Pts',(-19.630746144009,-13.10326146677,114.303685809968)) ;
#166131 = CARTESIAN_POINT('Ctrl Pts',(-19.6534487804468,-13.1248302660667,
114.372834377822)) ;
#166132 = CARTESIAN_POINT('Ctrl Pts',(-19.7272526251537,-13.12483024999,114.348603340056)) ;
#166133 = CARTESIAN_POINT('Ctrl Pts',(-19.8010564698606,-13.1248302339134,
114.32437230229)) ;
#166134 = CARTESIAN_POINT('Ctrl Pts',(-19.7783538334228,-13.1032614346168,
114.255223734436)) ;
#166135 = CARTESIAN_POINT('Ctrl Pts',(-19.755651196985,-13.0816926353201,
114.186075166582)) ;
#166136 = CARTESIAN_POINT('Ctrl Pts',(-19.6818473522781,-13.0816926513967,
114.210306204348)) ;
#166137 = CARTESIAN_POINT('Ctrl Pts',(-19.6080435075712,-13.0816926674734,
114.234537242114)) ;
#166138 = CARTESIAN_POINT('Ctrl Pts',(-19.630746144009,-13.10326146677,114.303685809968)) ;
#166139 = CARTESIAN_POINT('Ctrl Pts',(-19.6788883367903,-12.8385043736975,
114.414887005112)) ;
#166140 = CARTESIAN_POINT('Ctrl Pts',(-19.6989956623995,-12.8785902983801,
114.476130675077)) ;
#166141 = CARTESIAN_POINT('Ctrl Pts',(-19.772799509607,-12.8785902776547,
114.451899644927)) ;
#166142 = CARTESIAN_POINT('Ctrl Pts',(-19.8466033568145,-12.8785902569293,
114.427668614778)) ;
#166143 = CARTESIAN_POINT('Ctrl Pts',(-19.8264960312054,-12.8385043322466,
114.366424944813)) ;
#166144 = CARTESIAN_POINT('Ctrl Pts',(-19.8063887055962,-12.7984184075639,
114.305181274849)) ;
#166145 = CARTESIAN_POINT('Ctrl Pts',(-19.7325848583887,-12.7984184282893,
114.329412304998)) ;
#166146 = CARTESIAN_POINT('Ctrl Pts',(-19.6587810111812,-12.7984184490148,
114.353643335148)) ;
#166147 = CARTESIAN_POINT('Ctrl Pts',(-19.6788883367903,-12.8385043736975,
114.414887005112)) ;
#166148 = CARTESIAN_POINT('Ctrl Pts',(-19.7478090515721,-12.6146172171064,
114.589262192695)) ;
#166149 = CARTESIAN_POINT('Ctrl Pts',(-19.7638689510113,-12.6703934014124,
114.63817805577)) ;
#166150 = CARTESIAN_POINT('Ctrl Pts',(-19.8376728018705,-12.6703933786195,
114.613947036742)) ;
#166151 = CARTESIAN_POINT('Ctrl Pts',(-19.9114766527297,-12.6703933558266,
114.589716017715)) ;
#166152 = CARTESIAN_POINT('Ctrl Pts',(-19.8954167532905,-12.6146171715207,
114.54080015464)) ;
#166153 = CARTESIAN_POINT('Ctrl Pts',(-19.8793568538513,-12.5588409872148,
114.491884291566)) ;
#166154 = CARTESIAN_POINT('Ctrl Pts',(-19.8055530029922,-12.5588410100077,
114.516115310593)) ;
#166155 = CARTESIAN_POINT('Ctrl Pts',(-19.731749152133,-12.5588410328005,
114.54034632962)) ;
#166156 = CARTESIAN_POINT('Ctrl Pts',(-19.7478090515721,-12.6146172171064,
114.589262192695)) ;
#166157 = CARTESIAN_POINT('Ctrl Pts',(-19.8327892013851,-12.4490452703409,
114.812711060291)) ;
#166158 = CARTESIAN_POINT('Ctrl Pts',(-19.8436711987224,-12.5164621248353,
114.845855869166)) ;
#166159 = CARTESIAN_POINT('Ctrl Pts',(-19.9174750533839,-12.5164621055273,
114.82162486172)) ;
#166160 = CARTESIAN_POINT('Ctrl Pts',(-19.9912789080454,-12.5164620862193,
114.797393854274)) ;
#166161 = CARTESIAN_POINT('Ctrl Pts',(-19.9803969107081,-12.449045231725,
114.764249045399)) ;
#166162 = CARTESIAN_POINT('Ctrl Pts',(-19.9695149133709,-12.3816283772306,
114.731104236523)) ;
#166163 = CARTESIAN_POINT('Ctrl Pts',(-19.8957110587094,-12.3816283965386,
114.755335243969)) ;
#166164 = CARTESIAN_POINT('Ctrl Pts',(-19.8219072040478,-12.3816284158465,
114.779566251415)) ;
#166165 = CARTESIAN_POINT('Ctrl Pts',(-19.8327892013851,-12.4490452703409,
114.812711060291)) ;
#166166 = CARTESIAN_POINT('Ctrl Pts',(-19.9292782242536,-12.3524023594542,
115.071032776141)) ;
#166167 = CARTESIAN_POINT('Ctrl Pts',(-19.9341751641512,-12.4266644816829,
115.085948065929)) ;
#166168 = CARTESIAN_POINT('Ctrl Pts',(-20.0079790229734,-12.4266644707959,
115.061717071156)) ;
#166169 = CARTESIAN_POINT('Ctrl Pts',(-20.0817828817955,-12.4266644599088,
115.037486076383)) ;
#166170 = CARTESIAN_POINT('Ctrl Pts',(-20.0768859418979,-12.3524023376801,
115.022570786595)) ;
#166171 = CARTESIAN_POINT('Ctrl Pts',(-20.0719890020003,-12.2781402154514,
115.007655496807)) ;
#166172 = CARTESIAN_POINT('Ctrl Pts',(-19.9981851431782,-12.2781402263384,
115.03188649158)) ;
#166173 = CARTESIAN_POINT('Ctrl Pts',(-19.924381284356,-12.2781402372254,
115.056117486353)) ;
#166174 = CARTESIAN_POINT('Ctrl Pts',(-19.9292782242536,-12.3524023594542,
115.071032776141)) ;
#166175 = CARTESIAN_POINT('Ctrl Pts',(-20.02989329958,-12.3322917866331,115.342208218691)) ;
#166176 = CARTESIAN_POINT('Ctrl Pts',(-20.0285025426279,-12.4080647606153,
115.337972198524)) ;
#166177 = CARTESIAN_POINT('Ctrl Pts',(-20.1023064039529,-12.4080647636104,
115.313741211374)) ;
#166178 = CARTESIAN_POINT('Ctrl Pts',(-20.1761102652779,-12.4080647666054,
115.289510224224)) ;
#166179 = CARTESIAN_POINT('Ctrl Pts',(-20.17750102223,-12.3322917926232,115.293746244391)) ;
#166180 = CARTESIAN_POINT('Ctrl Pts',(-20.1788917791821,-12.256518818641,
115.297982264558)) ;
#166181 = CARTESIAN_POINT('Ctrl Pts',(-20.1050879178571,-12.256518815646,
115.322213251708)) ;
#166182 = CARTESIAN_POINT('Ctrl Pts',(-20.0312840565321,-12.2565188126509,
115.346444238858)) ;
#166183 = CARTESIAN_POINT('Ctrl Pts',(-20.02989329958,-12.3322917866331,115.342208218691)) ;
#166184 = CARTESIAN_POINT('Ctrl Pts',(-20.1297073657354,-12.3899082998251,
115.610661574223)) ;
#166185 = CARTESIAN_POINT('Ctrl Pts',(-20.1220816634719,-12.4617684939858,
115.587434916822)) ;
#166186 = CARTESIAN_POINT('Ctrl Pts',(-20.1958855266358,-12.4617685151837,
115.563203935273)) ;
#166187 = CARTESIAN_POINT('Ctrl Pts',(-20.2696893897997,-12.4617685363815,
115.538972953724)) ;
#166188 = CARTESIAN_POINT('Ctrl Pts',(-20.2773150920632,-12.3899083422208,
115.562199611125)) ;
#166189 = CARTESIAN_POINT('Ctrl Pts',(-20.2849407943267,-12.3180481480601,
115.585426268526)) ;
#166190 = CARTESIAN_POINT('Ctrl Pts',(-20.2111369311628,-12.3180481268623,
115.609657250075)) ;
#166191 = CARTESIAN_POINT('Ctrl Pts',(-20.1373330679989,-12.3180481056645,
115.633888231624)) ;
#166192 = CARTESIAN_POINT('Ctrl Pts',(-20.1297073657354,-12.3899082998251,
115.610661574223)) ;
#166193 = CARTESIAN_POINT('Ctrl Pts',(-20.2210035911202,-12.5204817202917,
115.853404760459)) ;
#166194 = CARTESIAN_POINT('Ctrl Pts',(-20.2077238649911,-12.5833292491025,
115.812956858768)) ;
#166195 = CARTESIAN_POINT('Ctrl Pts',(-20.2815277274735,-12.5833292901703,
115.788725875143)) ;
#166196 = CARTESIAN_POINT('Ctrl Pts',(-20.3553315899559,-12.5833293312382,
115.764494891519)) ;
#166197 = CARTESIAN_POINT('Ctrl Pts',(-20.3686113160851,-12.5204818024274,
115.804942793209)) ;
#166198 = CARTESIAN_POINT('Ctrl Pts',(-20.3818910422142,-12.4576342736166,
115.8453906949)) ;
#166199 = CARTESIAN_POINT('Ctrl Pts',(-20.3080871797318,-12.4576342325488,
115.869621678525)) ;
#166200 = CARTESIAN_POINT('Ctrl Pts',(-20.2342833172493,-12.457634191481,
115.893852662149)) ;
#166201 = CARTESIAN_POINT('Ctrl Pts',(-20.2210035911202,-12.5204817202917,
115.853404760459)) ;
#166202 = CARTESIAN_POINT('Ctrl Pts',(-20.2992739009599,-12.7170079033734,
116.056135467332)) ;
#166203 = CARTESIAN_POINT('Ctrl Pts',(-20.2812482485149,-12.7662262828423,
116.00123224001)) ;
#166204 = CARTESIAN_POINT('Ctrl Pts',(-20.3550521086811,-12.7662263456653,
115.977001249331)) ;
#166205 = CARTESIAN_POINT('Ctrl Pts',(-20.4288559688472,-12.7662264084883,
115.952770258651)) ;
#166206 = CARTESIAN_POINT('Ctrl Pts',(-20.4468816212922,-12.7170080290195,
116.007673485972)) ;
#166207 = CARTESIAN_POINT('Ctrl Pts',(-20.4649072737372,-12.6677896495507,
116.062576713293)) ;
#166208 = CARTESIAN_POINT('Ctrl Pts',(-20.391103413571,-12.6677895867277,
116.086807703973)) ;
#166209 = CARTESIAN_POINT('Ctrl Pts',(-20.3172995534049,-12.6677895239046,
116.111038694653)) ;
#166210 = CARTESIAN_POINT('Ctrl Pts',(-20.2992739009599,-12.7170079033734,
116.056135467332)) ;
#166211 = CARTESIAN_POINT('Ctrl Pts',(-20.3582578994183,-12.9615280720901,
116.200502710749)) ;
#166212 = CARTESIAN_POINT('Ctrl Pts',(-20.3368182747409,-12.9937459693296,
116.135201074954)) ;
#166213 = CARTESIAN_POINT('Ctrl Pts',(-20.410622129823,-12.9937460490588,
116.110970068789)) ;
#166214 = CARTESIAN_POINT('Ctrl Pts',(-20.484425984905,-12.9937461287879,
116.086739062624)) ;
#166215 = CARTESIAN_POINT('Ctrl Pts',(-20.5058656095824,-12.9615282315483,
116.152040698419)) ;
#166216 = CARTESIAN_POINT('Ctrl Pts',(-20.5273052342599,-12.9293103343088,
116.217342334215)) ;
#166217 = CARTESIAN_POINT('Ctrl Pts',(-20.4535013791778,-12.9293102545796,
116.241573340379)) ;
#166218 = CARTESIAN_POINT('Ctrl Pts',(-20.3796975240957,-12.9293101748505,
116.265804346544)) ;
#166219 = CARTESIAN_POINT('Ctrl Pts',(-20.3582578994183,-12.9615280720901,
116.200502710749)) ;
#166220 = CARTESIAN_POINT('Ctrl Pts',(-20.3956758286965,-13.241668548695,
116.278772178116)) ;
#166221 = CARTESIAN_POINT('Ctrl Pts',(-20.3723310699443,-13.2543754677215,
116.207667811464)) ;
#166222 = CARTESIAN_POINT('Ctrl Pts',(-20.4461349183247,-13.2543755617733,
116.183436784887)) ;
#166223 = CARTESIAN_POINT('Ctrl Pts',(-20.5199387667051,-13.2543756558251,
116.15920575831)) ;
#166224 = CARTESIAN_POINT('Ctrl Pts',(-20.5432835254574,-13.2416687367986,
116.230310124962)) ;
#166225 = CARTESIAN_POINT('Ctrl Pts',(-20.5666282842096,-13.228961817772,
116.301414491615)) ;
#166226 = CARTESIAN_POINT('Ctrl Pts',(-20.4928244358292,-13.2289617237202,
116.325645518192)) ;
#166227 = CARTESIAN_POINT('Ctrl Pts',(-20.4190205874488,-13.2289616296684,
116.349876544769)) ;
#166228 = CARTESIAN_POINT('Ctrl Pts',(-20.3956758286965,-13.241668548695,
116.278772178116)) ;
#166229 = CARTESIAN_POINT('Ctrl Pts',(-20.4087241002425,-13.5312927388049,
116.283231684985)) ;
#166230 = CARTESIAN_POINT('Ctrl Pts',(-20.3851644865814,-13.5237974675911,
116.21147290502)) ;
#166231 = CARTESIAN_POINT('Ctrl Pts',(-20.4589683268494,-13.5237975662632,
116.187241853734)) ;
#166232 = CARTESIAN_POINT('Ctrl Pts',(-20.5327721671173,-13.5237976649353,
116.163010802447)) ;
#166233 = CARTESIAN_POINT('Ctrl Pts',(-20.5563317807784,-13.5312929361492,
116.234769582413)) ;
#166234 = CARTESIAN_POINT('Ctrl Pts',(-20.5798913944395,-13.538788207363,
116.306528362378)) ;
#166235 = CARTESIAN_POINT('Ctrl Pts',(-20.5060875541715,-13.5387881086909,
116.330759413664)) ;
#166236 = CARTESIAN_POINT('Ctrl Pts',(-20.4322837139035,-13.5387880100187,
116.35499046495)) ;
#166237 = CARTESIAN_POINT('Ctrl Pts',(-20.4087241002425,-13.5312927388049,
116.283231684985)) ;
#166238 = CARTESIAN_POINT('Ctrl Pts',(-20.397812395172,-13.8141856043051,
116.214533598902)) ;
#166239 = CARTESIAN_POINT('Ctrl Pts',(-20.375713872965,-13.7869289146623,
116.147225067836)) ;
#166240 = CARTESIAN_POINT('Ctrl Pts',(-20.4495177047382,-13.7869290108332,
116.122993990676)) ;
#166241 = CARTESIAN_POINT('Ctrl Pts',(-20.5233215365114,-13.7869291070041,
116.098762913516)) ;
#166242 = CARTESIAN_POINT('Ctrl Pts',(-20.5454200587184,-13.8141857966469,
116.166071444582)) ;
#166243 = CARTESIAN_POINT('Ctrl Pts',(-20.5675185809255,-13.8414424862897,
116.233379975647)) ;
#166244 = CARTESIAN_POINT('Ctrl Pts',(-20.4937147491523,-13.8414423901188,
116.257611052807)) ;
#166245 = CARTESIAN_POINT('Ctrl Pts',(-20.4199109173791,-13.8414422939479,
116.281842129967)) ;
#166246 = CARTESIAN_POINT('Ctrl Pts',(-20.397812395172,-13.8141856043051,
116.214533598902)) ;
#166247 = CARTESIAN_POINT('Ctrl Pts',(-20.3642659620429,-14.0686273114668,
116.076918892834)) ;
#166248 = CARTESIAN_POINT('Ctrl Pts',(-20.3452103378789,-14.0235664995227,
116.018878538292)) ;
#166249 = CARTESIAN_POINT('Ctrl Pts',(-20.4190141615538,-14.0235665846011,
115.994647436466)) ;
#166250 = CARTESIAN_POINT('Ctrl Pts',(-20.4928179852287,-14.0235666696795,
115.97041633464)) ;
#166251 = CARTESIAN_POINT('Ctrl Pts',(-20.5118736093927,-14.0686274816236,
116.028456689182)) ;
#166252 = CARTESIAN_POINT('Ctrl Pts',(-20.5309292335566,-14.1136882935678,
116.086497043723)) ;
#166253 = CARTESIAN_POINT('Ctrl Pts',(-20.4571254098818,-14.1136882084894,
116.110728145549)) ;
#166254 = CARTESIAN_POINT('Ctrl Pts',(-20.3833215862069,-14.113688123411,
116.134959247375)) ;
#166255 = CARTESIAN_POINT('Ctrl Pts',(-20.3642659620429,-14.0686273114668,
116.076918892834)) ;
#166256 = CARTESIAN_POINT('Ctrl Pts',(-20.3109843484247,-14.2772225776637,
115.879041201496)) ;
#166257 = CARTESIAN_POINT('Ctrl Pts',(-20.2963568431874,-14.2175318931739,
115.834488182769)) ;
#166258 = CARTESIAN_POINT('Ctrl Pts',(-20.3701606600124,-14.2175319594466,
115.81025706008)) ;
#166259 = CARTESIAN_POINT('Ctrl Pts',(-20.4439644768373,-14.2175320257193,
115.78602593739)) ;
#166260 = CARTESIAN_POINT('Ctrl Pts',(-20.4585919820747,-14.2772227102091,
115.830578956117)) ;
#166261 = CARTESIAN_POINT('Ctrl Pts',(-20.473219487312,-14.3369133946989,
115.875131974844)) ;
#166262 = CARTESIAN_POINT('Ctrl Pts',(-20.399415670487,-14.3369133284262,
115.899363097534)) ;
#166263 = CARTESIAN_POINT('Ctrl Pts',(-20.325611853662,-14.3369132621536,
115.923594220223)) ;
#166264 = CARTESIAN_POINT('Ctrl Pts',(-20.3109843484247,-14.2772225776637,
115.879041201496)) ;
#166265 = CARTESIAN_POINT('Ctrl Pts',(-20.2431888087384,-14.4229662306659,
115.637203831171)) ;
#166266 = CARTESIAN_POINT('Ctrl Pts',(-20.234004322962,-14.3530122150386,
115.609229371502)) ;
#166267 = CARTESIAN_POINT('Ctrl Pts',(-20.3078081351379,-14.3530122565041,
115.584998234652)) ;
#166268 = CARTESIAN_POINT('Ctrl Pts',(-20.3816119473137,-14.3530122979697,
115.560767097802)) ;
#166269 = CARTESIAN_POINT('Ctrl Pts',(-20.3907964330902,-14.4229663135971,
115.588741557471)) ;
#166270 = CARTESIAN_POINT('Ctrl Pts',(-20.3999809188666,-14.4929203292244,
115.61671601714)) ;
#166271 = CARTESIAN_POINT('Ctrl Pts',(-20.3261771066907,-14.4929202877588,
115.640947153991)) ;
#166272 = CARTESIAN_POINT('Ctrl Pts',(-20.2523732945149,-14.4929202462933,
115.665178290841)) ;
#166273 = CARTESIAN_POINT('Ctrl Pts',(-20.2431888087384,-14.4229662306659,
115.637203831171)) ;
#166274 = CARTESIAN_POINT('Ctrl Pts',(-20.165967360864,-14.4976749709137,
115.366562084077)) ;
#166275 = CARTESIAN_POINT('Ctrl Pts',(-20.162893823781,-14.4224014624097,
115.357200588124)) ;
#166276 = CARTESIAN_POINT('Ctrl Pts',(-20.2366976337292,-14.4224014756821,
115.332969444489)) ;
#166277 = CARTESIAN_POINT('Ctrl Pts',(-20.3105014436775,-14.4224014889544,
115.308738300854)) ;
#166278 = CARTESIAN_POINT('Ctrl Pts',(-20.3135749807605,-14.4976749974584,
115.318099796806)) ;
#166279 = CARTESIAN_POINT('Ctrl Pts',(-20.3166485178435,-14.5729485059623,
115.327461292759)) ;
#166280 = CARTESIAN_POINT('Ctrl Pts',(-20.2428447078953,-14.57294849269,115.351692436394)) ;
#166281 = CARTESIAN_POINT('Ctrl Pts',(-20.169040897947,-14.5729484794176,
115.375923580029)) ;
#166282 = CARTESIAN_POINT('Ctrl Pts',(-20.165967360864,-14.4976749709137,
115.366562084077)) ;
#166283 = CARTESIAN_POINT('Ctrl Pts',(-20.0851494998397,-14.4944851703305,
115.084714178899)) ;
#166284 = CARTESIAN_POINT('Ctrl Pts',(-20.0884522101337,-14.4193216059584,
115.094773703609)) ;
#166285 = CARTESIAN_POINT('Ctrl Pts',(-20.1622560208923,-14.4193215903829,
115.070542562443)) ;
#166286 = CARTESIAN_POINT('Ctrl Pts',(-20.2360598316509,-14.4193215748074,
115.046311421276)) ;
#166287 = CARTESIAN_POINT('Ctrl Pts',(-20.232757121357,-14.4944851391795,
115.036251896566)) ;
#166288 = CARTESIAN_POINT('Ctrl Pts',(-20.229454411063,-14.5696487035515,
115.026192371856)) ;
#166289 = CARTESIAN_POINT('Ctrl Pts',(-20.1556506003044,-14.5696487191271,
115.050423513022)) ;
#166290 = CARTESIAN_POINT('Ctrl Pts',(-20.0818467895458,-14.5696487347026,
115.074654654189)) ;
#166291 = CARTESIAN_POINT('Ctrl Pts',(-20.0851494998397,-14.4944851703305,
115.084714178899)) ;
#166292 = CARTESIAN_POINT('Ctrl Pts',(-20.0087955569206,-14.4147277655596,
114.816900333307)) ;
#166293 = CARTESIAN_POINT('Ctrl Pts',(-20.0181634621253,-14.3450211180556,
114.845433463057)) ;
#166294 = CARTESIAN_POINT('Ctrl Pts',(-20.091967275971,-14.3450210762549,
114.821202331292)) ;
#166295 = CARTESIAN_POINT('Ctrl Pts',(-20.1657710898167,-14.3450210344541,
114.796971199528)) ;
#166296 = CARTESIAN_POINT('Ctrl Pts',(-20.156403184612,-14.4147276819581,
114.768438069778)) ;
#166297 = CARTESIAN_POINT('Ctrl Pts',(-20.1470352794072,-14.4844343294621,
114.739904940028)) ;
#166298 = CARTESIAN_POINT('Ctrl Pts',(-20.0732314655615,-14.4844343712628,
114.764136071792)) ;
#166299 = CARTESIAN_POINT('Ctrl Pts',(-19.9994276517158,-14.4844344130636,
114.788367203557)) ;
#166300 = CARTESIAN_POINT('Ctrl Pts',(-20.0087955569206,-14.4147277655596,
114.816900333307)) ;
#166301 = CARTESIAN_POINT('Ctrl Pts',(-19.9415785213677,-14.2631098096402,
114.576628280773)) ;
#166302 = CARTESIAN_POINT('Ctrl Pts',(-19.9563887371762,-14.2038841179929,
114.621737810429)) ;
#166303 = CARTESIAN_POINT('Ctrl Pts',(-20.0301925565596,-14.2038840550099,
114.597506695531)) ;
#166304 = CARTESIAN_POINT('Ctrl Pts',(-20.103996375943,-14.203883992027,114.573275580634)) ;
#166305 = CARTESIAN_POINT('Ctrl Pts',(-20.0891861601345,-14.2631096836743,
114.528166050978)) ;
#166306 = CARTESIAN_POINT('Ctrl Pts',(-20.0743759443261,-14.3223353753216,
114.483056521323)) ;
#166307 = CARTESIAN_POINT('Ctrl Pts',(-20.0005721249426,-14.3223354383045,
114.50728763622)) ;
#166308 = CARTESIAN_POINT('Ctrl Pts',(-19.9267683055592,-14.3223355012875,
114.531518751117)) ;
#166309 = CARTESIAN_POINT('Ctrl Pts',(-19.9415785213677,-14.2631098096402,
114.576628280773)) ;
#166310 = CARTESIAN_POINT('Ctrl Pts',(-19.889902590895,-14.0515534840703,
114.38383900095)) ;
#166311 = CARTESIAN_POINT('Ctrl Pts',(-19.9090752445563,-14.0070094522688,
114.442235812343)) ;
#166312 = CARTESIAN_POINT('Ctrl Pts',(-19.9828790708446,-14.0070093747174,
114.418004718477)) ;
#166313 = CARTESIAN_POINT('Ctrl Pts',(-20.056682897133,-14.007009297166,114.393773624611)) ;
#166314 = CARTESIAN_POINT('Ctrl Pts',(-20.0375102434718,-14.0515533289676,
114.335376813219)) ;
#166315 = CARTESIAN_POINT('Ctrl Pts',(-20.0183375898106,-14.0960973607691,
114.276980001827)) ;
#166316 = CARTESIAN_POINT('Ctrl Pts',(-19.9445337635222,-14.0960974383204,
114.301211095692)) ;
#166317 = CARTESIAN_POINT('Ctrl Pts',(-19.8707299372338,-14.0960975158718,
114.325442189558)) ;
#166318 = CARTESIAN_POINT('Ctrl Pts',(-19.889902590895,-14.0515534840703,
114.38383900095)) ;
#166319 = CARTESIAN_POINT('Ctrl Pts',(-19.8577995917922,-13.793288943793,
114.250462777897)) ;
#166320 = CARTESIAN_POINT('Ctrl Pts',(-19.8799791098395,-13.7667090894671,
114.318018012925)) ;
#166321 = CARTESIAN_POINT('Ctrl Pts',(-19.9537829439215,-13.7667090063188,
114.293786942797)) ;
#166322 = CARTESIAN_POINT('Ctrl Pts',(-20.0275867780035,-13.7667089231704,
114.269555872669)) ;
#166323 = CARTESIAN_POINT('Ctrl Pts',(-20.0054072599561,-13.7932887774963,
114.202000637641)) ;
#166324 = CARTESIAN_POINT('Ctrl Pts',(-19.9832277419088,-13.8198686318222,
114.134445402614)) ;
#166325 = CARTESIAN_POINT('Ctrl Pts',(-19.9094239078268,-13.8198687149705,
114.158676472742)) ;
#166326 = CARTESIAN_POINT('Ctrl Pts',(-19.8356200737448,-13.8198687981189,
114.182907542869)) ;
#166327 = CARTESIAN_POINT('Ctrl Pts',(-19.8577995917922,-13.793288943793,
114.250462777897)) ;
#166328 = CARTESIAN_POINT('Ctrl Pts',(-19.8486859511613,-13.5095097704303,
114.187308101933)) ;
#166329 = CARTESIAN_POINT('Ctrl Pts',(-19.8722676042901,-13.5027030390007,
114.259134014066)) ;
#166330 = CARTESIAN_POINT('Ctrl Pts',(-19.946071445741,-13.5027029571053,
114.234902966383)) ;
#166331 = CARTESIAN_POINT('Ctrl Pts',(-20.0198752871918,-13.50270287521,114.210671918699)) ;
#166332 = CARTESIAN_POINT('Ctrl Pts',(-19.996293634063,-13.5095096066396,
114.138846006567)) ;
#166333 = CARTESIAN_POINT('Ctrl Pts',(-19.9727119809342,-13.5163163380692,
114.067020094434)) ;
#166334 = CARTESIAN_POINT('Ctrl Pts',(-19.8989081394833,-13.5163164199646,
114.091251142118)) ;
#166335 = CARTESIAN_POINT('Ctrl Pts',(-19.8251042980325,-13.5163165018599,
114.115482189801)) ;
#166336 = CARTESIAN_POINT('Ctrl Pts',(-19.8486859511613,-13.5095097704303,
114.187308101933)) ;
#166337 = CARTESIAN_POINT('Ctrl Pts',(-19.8637427605227,-13.218674427129,
114.197696524742)) ;
#166338 = CARTESIAN_POINT('Ctrl Pts',(-19.8870428101562,-13.2321633115492,
114.268664717921)) ;
#166339 = CARTESIAN_POINT('Ctrl Pts',(-19.9608466580392,-13.2321632381837,
114.244433689829)) ;
#166340 = CARTESIAN_POINT('Ctrl Pts',(-20.0346505059221,-13.2321631648182,
114.220202661737)) ;
#166341 = CARTESIAN_POINT('Ctrl Pts',(-20.0113504562886,-13.2186742803981,
114.149234468558)) ;
#166342 = CARTESIAN_POINT('Ctrl Pts',(-19.9880504066551,-13.2051853959779,
114.078266275379)) ;
#166343 = CARTESIAN_POINT('Ctrl Pts',(-19.9142465587722,-13.2051854693434,
114.102497303471)) ;
#166344 = CARTESIAN_POINT('Ctrl Pts',(-19.8404427108892,-13.2051855427089,
114.126728331563)) ;
#166345 = CARTESIAN_POINT('Ctrl Pts',(-19.8637427605227,-13.218674427129,
114.197696524742)) ;
#166346 = CARTESIAN_POINT('Ctrl Pts',(-19.9025785975589,-12.9425272619773,
114.280582549871)) ;
#166347 = CARTESIAN_POINT('Ctrl Pts',(-19.9239349080404,-12.9753170489684,
114.345630427072)) ;
#166348 = CARTESIAN_POINT('Ctrl Pts',(-19.9977387608683,-12.9753169887403,
114.321399414041)) ;
#166349 = CARTESIAN_POINT('Ctrl Pts',(-20.0715426136962,-12.9753169285121,
114.297168401011)) ;
#166350 = CARTESIAN_POINT('Ctrl Pts',(-20.0501863032146,-12.942527141521,
114.232120523809)) ;
#166351 = CARTESIAN_POINT('Ctrl Pts',(-20.0288299927331,-12.9097373545299,
114.167072646608)) ;
#166352 = CARTESIAN_POINT('Ctrl Pts',(-19.9550261399052,-12.9097374147581,
114.191303659639)) ;
#166353 = CARTESIAN_POINT('Ctrl Pts',(-19.8812222870773,-12.9097374749862,
114.21553467267)) ;
#166354 = CARTESIAN_POINT('Ctrl Pts',(-19.9025785975589,-12.9425272619773,
114.280582549871)) ;
#166355 = CARTESIAN_POINT('Ctrl Pts',(-19.9637005352673,-12.6990701230285,
114.431122563372)) ;
#166356 = CARTESIAN_POINT('Ctrl Pts',(-19.9815590200875,-12.7489081846955,
114.485516627788)) ;
#166357 = CARTESIAN_POINT('Ctrl Pts',(-20.0553628755155,-12.748908142065,
114.461285622677)) ;
#166358 = CARTESIAN_POINT('Ctrl Pts',(-20.1291667309434,-12.7489080994345,
114.437054617565)) ;
#166359 = CARTESIAN_POINT('Ctrl Pts',(-20.1113082461232,-12.6990700377675,
114.382660553149)) ;
#166360 = CARTESIAN_POINT('Ctrl Pts',(-20.0934497613029,-12.6492319761005,
114.328266488732)) ;
#166361 = CARTESIAN_POINT('Ctrl Pts',(-20.019645905875,-12.649232018731,114.352497493844)) ;
#166362 = CARTESIAN_POINT('Ctrl Pts',(-19.945842050447,-12.6492320613615,
114.376728498955)) ;
#166363 = CARTESIAN_POINT('Ctrl Pts',(-19.9637005352673,-12.6990701230285,
114.431122563372)) ;
#166364 = CARTESIAN_POINT('Ctrl Pts',(-20.0423283064488,-12.5091750901202,
114.635350522219)) ;
#166365 = CARTESIAN_POINT('Ctrl Pts',(-20.0554534729284,-12.5723470280859,
114.675327662559)) ;
#166366 = CARTESIAN_POINT('Ctrl Pts',(-20.1292573296924,-12.5723470007831,
114.651096661517)) ;
#166367 = CARTESIAN_POINT('Ctrl Pts',(-20.2030611864563,-12.5723469734802,
114.626865660475)) ;
#166368 = CARTESIAN_POINT('Ctrl Pts',(-20.1899360199767,-12.5091750355146,
114.586888520134)) ;
#166369 = CARTESIAN_POINT('Ctrl Pts',(-20.1768108534972,-12.4460030975489,
114.546911379793)) ;
#166370 = CARTESIAN_POINT('Ctrl Pts',(-20.1030069967332,-12.4460031248517,
114.571142380836)) ;
#166371 = CARTESIAN_POINT('Ctrl Pts',(-20.0292031399693,-12.4460031521546,
114.595373381878)) ;
#166372 = CARTESIAN_POINT('Ctrl Pts',(-20.0423283064488,-12.5091750901202,
114.635350522219)) ;
#166373 = CARTESIAN_POINT('Ctrl Pts',(-20.1350384738347,-12.3826566850404,
114.882137699314)) ;
#166374 = CARTESIAN_POINT('Ctrl Pts',(-20.1424469548967,-12.4547585599534,
114.904702738063)) ;
#166375 = CARTESIAN_POINT('Ctrl Pts',(-20.2162508105127,-12.4547585482587,
114.880471733524)) ;
#166376 = CARTESIAN_POINT('Ctrl Pts',(-20.2900546661287,-12.4547585365639,
114.856240728986)) ;
#166377 = CARTESIAN_POINT('Ctrl Pts',(-20.2826461850667,-12.3826566616509,
114.833675690236)) ;
#166378 = CARTESIAN_POINT('Ctrl Pts',(-20.2752377040047,-12.3105547867379,
114.811110651486)) ;
#166379 = CARTESIAN_POINT('Ctrl Pts',(-20.2014338483887,-12.3105547984326,
114.835341656025)) ;
#166380 = CARTESIAN_POINT('Ctrl Pts',(-20.1276299927727,-12.3105548101274,
114.859572660564)) ;
#166381 = CARTESIAN_POINT('Ctrl Pts',(-20.1350384738347,-12.3826566850404,
114.882137699314)) ;
#166382 = CARTESIAN_POINT('Ctrl Pts',(-20.2350090319357,-12.3310754563828,
115.151149980426)) ;
#166383 = CARTESIAN_POINT('Ctrl Pts',(-20.2361827516347,-12.4068883304643,
115.154724941869)) ;
#166384 = CARTESIAN_POINT('Ctrl Pts',(-20.309986605033,-12.406888329813,115.130493930576)) ;
#166385 = CARTESIAN_POINT('Ctrl Pts',(-20.3837904584313,-12.4068883291616,
115.106262919282)) ;
#166386 = CARTESIAN_POINT('Ctrl Pts',(-20.3826167387323,-12.3310754550801,
115.102687957839)) ;
#166387 = CARTESIAN_POINT('Ctrl Pts',(-20.3814430190333,-12.2552625809986,
115.099112996395)) ;
#166388 = CARTESIAN_POINT('Ctrl Pts',(-20.307639165635,-12.25526258165,115.123344007689)) ;
#166389 = CARTESIAN_POINT('Ctrl Pts',(-20.2338353122368,-12.2552625823013,
115.147575018982)) ;
#166390 = CARTESIAN_POINT('Ctrl Pts',(-20.2350090319357,-12.3310754563828,
115.151149980426)) ;
#166391 = CARTESIAN_POINT('Ctrl Pts',(-20.3359195607843,-12.357364074466,
115.42305855361)) ;
#166392 = CARTESIAN_POINT('Ctrl Pts',(-20.3307826681784,-12.4314561765023,
115.40741240803)) ;
#166393 = CARTESIAN_POINT('Ctrl Pts',(-20.4045865188482,-12.4314561824614,
115.383181388426)) ;
#166394 = CARTESIAN_POINT('Ctrl Pts',(-20.4783903695179,-12.4314561884204,
115.358950368822)) ;
#166395 = CARTESIAN_POINT('Ctrl Pts',(-20.4835272621239,-12.3573640863842,
115.374596514401)) ;
#166396 = CARTESIAN_POINT('Ctrl Pts',(-20.4886641547298,-12.2832719843479,
115.39024265998)) ;
#166397 = CARTESIAN_POINT('Ctrl Pts',(-20.4148603040601,-12.2832719783889,
115.414473679585)) ;
#166398 = CARTESIAN_POINT('Ctrl Pts',(-20.3410564533903,-12.2832719724298,
115.438704699189)) ;
#166399 = CARTESIAN_POINT('Ctrl Pts',(-20.3359195607843,-12.357364074466,
115.42305855361)) ;
#166400 = CARTESIAN_POINT('Ctrl Pts',(-20.4312001328524,-12.4589530543375,
115.677923655332)) ;
#166401 = CARTESIAN_POINT('Ctrl Pts',(-20.4201340505478,-12.5260636075349,
115.644218154473)) ;
#166402 = CARTESIAN_POINT('Ctrl Pts',(-20.4939378986042,-12.5260636163209,
115.619987126908)) ;
#166403 = CARTESIAN_POINT('Ctrl Pts',(-20.5677417466605,-12.5260636251069,
115.595756099344)) ;
#166404 = CARTESIAN_POINT('Ctrl Pts',(-20.5788078289651,-12.4589530719095,
115.629461600204)) ;
#166405 = CARTESIAN_POINT('Ctrl Pts',(-20.5898739112697,-12.3918425187121,
115.663167101063)) ;
#166406 = CARTESIAN_POINT('Ctrl Pts',(-20.5160700632133,-12.3918425099261,
115.687398128628)) ;
#166407 = CARTESIAN_POINT('Ctrl Pts',(-20.442266215157,-12.3918425011401,
115.711629156192)) ;
#166408 = CARTESIAN_POINT('Ctrl Pts',(-20.4312001328524,-12.4589530543375,
115.677923655332)) ;
#166409 = CARTESIAN_POINT('Ctrl Pts',(-20.5157214281701,-12.6306888766498,
115.89970465667)) ;
#166410 = CARTESIAN_POINT('Ctrl Pts',(-20.4994746267274,-12.6859095379068,
115.850219521061)) ;
#166411 = CARTESIAN_POINT('Ctrl Pts',(-20.5732784720464,-12.6859095445597,
115.82598848516)) ;
#166412 = CARTESIAN_POINT('Ctrl Pts',(-20.6470823173654,-12.6859095512127,
115.801757449258)) ;
#166413 = CARTESIAN_POINT('Ctrl Pts',(-20.6633291188081,-12.6306888899557,
115.851242584866)) ;
#166414 = CARTESIAN_POINT('Ctrl Pts',(-20.6795759202508,-12.5754682286988,
115.900727720475)) ;
#166415 = CARTESIAN_POINT('Ctrl Pts',(-20.6057720749318,-12.5754682220458,
115.924958756377)) ;
#166416 = CARTESIAN_POINT('Ctrl Pts',(-20.5319682296128,-12.5754682153929,
115.949189792279)) ;
#166417 = CARTESIAN_POINT('Ctrl Pts',(-20.5157214281701,-12.6306888766498,
115.89970465667)) ;
#166418 = CARTESIAN_POINT('Ctrl Pts',(-20.5826648508089,-12.8569331102211,
116.068310974654)) ;
#166419 = CARTESIAN_POINT('Ctrl Pts',(-20.5624497196126,-12.8964388496988,
116.006738946817)) ;
#166420 = CARTESIAN_POINT('Ctrl Pts',(-20.6362535636491,-12.8964388537721,
115.982507907009)) ;
#166421 = CARTESIAN_POINT('Ctrl Pts',(-20.7100574076856,-12.8964388578454,
115.958276867201)) ;
#166422 = CARTESIAN_POINT('Ctrl Pts',(-20.7302725388819,-12.8569331183677,
116.019848895037)) ;
#166423 = CARTESIAN_POINT('Ctrl Pts',(-20.7504876700782,-12.81742737889,116.081420922874)) ;
#166424 = CARTESIAN_POINT('Ctrl Pts',(-20.6766838260417,-12.8174273748167,
116.105651962682)) ;
#166425 = CARTESIAN_POINT('Ctrl Pts',(-20.6028799820052,-12.8174273707434,
116.12988300249)) ;
#166426 = CARTESIAN_POINT('Ctrl Pts',(-20.5826648508089,-12.8569331102211,
116.068310974654)) ;
#166427 = CARTESIAN_POINT('Ctrl Pts',(-20.629281615088,-13.124308622433,116.174814524661)) ;
#166428 = CARTESIAN_POINT('Ctrl Pts',(-20.6065153457123,-13.1452036324507,
116.105472141463)) ;
#166429 = CARTESIAN_POINT('Ctrl Pts',(-20.6803191889954,-13.1452036323883,
116.08124109936)) ;
#166430 = CARTESIAN_POINT('Ctrl Pts',(-20.7541230322785,-13.1452036323259,
116.057010057257)) ;
#166431 = CARTESIAN_POINT('Ctrl Pts',(-20.7768893016542,-13.1243086223082,
116.126352440455)) ;
#166432 = CARTESIAN_POINT('Ctrl Pts',(-20.7996555710298,-13.1034136122904,
116.195694823653)) ;
#166433 = CARTESIAN_POINT('Ctrl Pts',(-20.7258517277467,-13.1034136123528,
116.219925865756)) ;
#166434 = CARTESIAN_POINT('Ctrl Pts',(-20.6520478844636,-13.1034136124152,
116.244156907858)) ;
#166435 = CARTESIAN_POINT('Ctrl Pts',(-20.629281615088,-13.124308622433,116.174814524661)) ;
#166436 = CARTESIAN_POINT('Ctrl Pts',(-20.6523720977963,-13.4140118065031,
116.209521407609)) ;
#166437 = CARTESIAN_POINT('Ctrl Pts',(-20.6286965490956,-13.4147080729357,
116.137409506245)) ;
#166438 = CARTESIAN_POINT('Ctrl Pts',(-20.7025003924587,-13.414708069978,
116.113178464386)) ;
#166439 = CARTESIAN_POINT('Ctrl Pts',(-20.7763042358217,-13.4147080670203,
116.088947422527)) ;
#166440 = CARTESIAN_POINT('Ctrl Pts',(-20.7999797845225,-13.4140118005876,
116.16105932389)) ;
#166441 = CARTESIAN_POINT('Ctrl Pts',(-20.8236553332232,-13.413315534155,
116.233171225254)) ;
#166442 = CARTESIAN_POINT('Ctrl Pts',(-20.7498514898601,-13.4133155371127,
116.257402267113)) ;
#166443 = CARTESIAN_POINT('Ctrl Pts',(-20.676047646497,-13.4133155400704,
116.281633308972)) ;
#166444 = CARTESIAN_POINT('Ctrl Pts',(-20.6523720977963,-13.4140118065031,
116.209521407609)) ;
#166445 = CARTESIAN_POINT('Ctrl Pts',(-20.6511480384506,-13.700942777731,
116.170554445295)) ;
#166446 = CARTESIAN_POINT('Ctrl Pts',(-20.6282523177272,-13.6816044417709,
116.100817774118)) ;
#166447 = CARTESIAN_POINT('Ctrl Pts',(-20.7020561614304,-13.6816044385339,
116.076586733294)) ;
#166448 = CARTESIAN_POINT('Ctrl Pts',(-20.7758600051336,-13.6816044352969,
116.052355692471)) ;
#166449 = CARTESIAN_POINT('Ctrl Pts',(-20.7987557258569,-13.700942771257,
116.122092363648)) ;
#166450 = CARTESIAN_POINT('Ctrl Pts',(-20.8216514465802,-13.7202811072171,
116.191829034826)) ;
#166451 = CARTESIAN_POINT('Ctrl Pts',(-20.747847602877,-13.7202811104541,
116.216060075649)) ;
#166452 = CARTESIAN_POINT('Ctrl Pts',(-20.6740437591738,-13.7202811136911,
116.240291116472)) ;
#166453 = CARTESIAN_POINT('Ctrl Pts',(-20.6511480384506,-13.700942777731,
116.170554445295)) ;
#166454 = CARTESIAN_POINT('Ctrl Pts',(-20.6263783704797,-13.9707477592159,
116.059467822879)) ;
#166455 = CARTESIAN_POINT('Ctrl Pts',(-20.605916023666,-13.9325402407103,
115.997142816043)) ;
#166456 = CARTESIAN_POINT('Ctrl Pts',(-20.6797198673865,-13.9325402395383,
115.972911775272)) ;
#166457 = CARTESIAN_POINT('Ctrl Pts',(-20.753523711107,-13.9325402383663,
115.948680734502)) ;
#166458 = CARTESIAN_POINT('Ctrl Pts',(-20.7739860579206,-13.9707477568719,
116.011005741338)) ;
#166459 = CARTESIAN_POINT('Ctrl Pts',(-20.7944484047343,-14.0089552753775,
116.073330748174)) ;
#166460 = CARTESIAN_POINT('Ctrl Pts',(-20.7206445610138,-14.0089552765495,
116.097561788944)) ;
#166461 = CARTESIAN_POINT('Ctrl Pts',(-20.6468407172933,-14.0089552777215,
116.121792829715)) ;
#166462 = CARTESIAN_POINT('Ctrl Pts',(-20.6263783704797,-13.9707477592159,
116.059467822879)) ;
#166463 = CARTESIAN_POINT('Ctrl Pts',(-20.5806731004674,-14.199353333197,
115.884809057481)) ;
#166464 = CARTESIAN_POINT('Ctrl Pts',(-20.5641058076827,-14.1451271098491,
115.834347756825)) ;
#166465 = CARTESIAN_POINT('Ctrl Pts',(-20.6379096506688,-14.1451271117169,
115.810116713818)) ;
#166466 = CARTESIAN_POINT('Ctrl Pts',(-20.7117134936549,-14.1451271135848,
115.785885670811)) ;
#166467 = CARTESIAN_POINT('Ctrl Pts',(-20.7282807864396,-14.1993533369326,
115.836346971466)) ;
#166468 = CARTESIAN_POINT('Ctrl Pts',(-20.7448480792243,-14.2535795602805,
115.886808272121)) ;
#166469 = CARTESIAN_POINT('Ctrl Pts',(-20.6710442362382,-14.2535795584127,
115.911039315129)) ;
#166470 = CARTESIAN_POINT('Ctrl Pts',(-20.5972403932521,-14.2535795565448,
115.935270358136)) ;
#166471 = CARTESIAN_POINT('Ctrl Pts',(-20.5806731004674,-14.199353333197,
115.884809057481)) ;
#166472 = CARTESIAN_POINT('Ctrl Pts',(-20.5181371616778,-14.3720888987135,
115.6588933938)) ;
#166473 = CARTESIAN_POINT('Ctrl Pts',(-20.5066456971274,-14.3057223139106,
115.623892247061)) ;
#166474 = CARTESIAN_POINT('Ctrl Pts',(-20.5804495386208,-14.3057223178457,
115.599661199507)) ;
#166475 = CARTESIAN_POINT('Ctrl Pts',(-20.6542533801142,-14.3057223217808,
115.575430151953)) ;
#166476 = CARTESIAN_POINT('Ctrl Pts',(-20.6657448446646,-14.3720889065837,
115.610431298692)) ;
#166477 = CARTESIAN_POINT('Ctrl Pts',(-20.677236309215,-14.4384554913866,
115.645432445431)) ;
#166478 = CARTESIAN_POINT('Ctrl Pts',(-20.6034324677216,-14.4384554874515,
115.669663492985)) ;
#166479 = CARTESIAN_POINT('Ctrl Pts',(-20.5296286262282,-14.4384554835164,
115.693894540539)) ;
#166480 = CARTESIAN_POINT('Ctrl Pts',(-20.5181371616778,-14.3720888987135,
115.6588933938)) ;
#166481 = CARTESIAN_POINT('Ctrl Pts',(-20.4439011849796,-14.4765884160959,
115.397333313055)) ;
#166482 = CARTESIAN_POINT('Ctrl Pts',(-20.4383100272348,-14.4028287794428,
115.380303548956)) ;
#166483 = CARTESIAN_POINT('Ctrl Pts',(-20.5121138665716,-14.4028287831727,
115.356072494834)) ;
#166484 = CARTESIAN_POINT('Ctrl Pts',(-20.5859177059085,-14.4028287869026,
115.331841440712)) ;
#166485 = CARTESIAN_POINT('Ctrl Pts',(-20.5915088636533,-14.4765884235558,
115.34887120481)) ;
#166486 = CARTESIAN_POINT('Ctrl Pts',(-20.5971000213981,-14.5503480602089,
115.365900968908)) ;
#166487 = CARTESIAN_POINT('Ctrl Pts',(-20.5232961820612,-14.550348056479,
115.390132023031)) ;
#166488 = CARTESIAN_POINT('Ctrl Pts',(-20.4494923427243,-14.550348052749,
115.414363077153)) ;
#166489 = CARTESIAN_POINT('Ctrl Pts',(-20.4439011849796,-14.4765884160959,
115.397333313055)) ;
#166490 = CARTESIAN_POINT('Ctrl Pts',(-20.3640341320984,-14.5052820126098,
115.118610145838)) ;
#166491 = CARTESIAN_POINT('Ctrl Pts',(-20.364745205464,-14.4294119228674,
115.120775960982)) ;
#166492 = CARTESIAN_POINT('Ctrl Pts',(-20.4385490423595,-14.4294119227756,
115.096544899424)) ;
#166493 = CARTESIAN_POINT('Ctrl Pts',(-20.512352879255,-14.4294119226838,
115.072313837865)) ;
#166494 = CARTESIAN_POINT('Ctrl Pts',(-20.5116418058893,-14.5052820124263,
115.070148022721)) ;
#166495 = CARTESIAN_POINT('Ctrl Pts',(-20.5109307325236,-14.5811521021687,
115.067982207577)) ;
#166496 = CARTESIAN_POINT('Ctrl Pts',(-20.4371268956282,-14.5811521022605,
115.092213269135)) ;
#166497 = CARTESIAN_POINT('Ctrl Pts',(-20.3633230587327,-14.5811521023523,
115.116444330694)) ;
#166498 = CARTESIAN_POINT('Ctrl Pts',(-20.3640341320984,-14.5052820126098,
115.118610145838)) ;
#166499 = CARTESIAN_POINT('Ctrl Pts',(-20.2851290429504,-14.4562719682351,
114.842865677127)) ;
#166500 = CARTESIAN_POINT('Ctrl Pts',(-20.2920831949679,-14.3837141408082,
114.864046902673)) ;
#166501 = CARTESIAN_POINT('Ctrl Pts',(-20.3658870298536,-14.383714132999,
114.839815834993)) ;
#166502 = CARTESIAN_POINT('Ctrl Pts',(-20.4396908647393,-14.3837141251898,
114.815584767313)) ;
#166503 = CARTESIAN_POINT('Ctrl Pts',(-20.4327367127217,-14.4562719526167,
114.794403541767)) ;
#166504 = CARTESIAN_POINT('Ctrl Pts',(-20.4257825607042,-14.5288297800436,
114.77322231622)) ;
#166505 = CARTESIAN_POINT('Ctrl Pts',(-20.3519787258185,-14.5288297878528,
114.7974533839)) ;
#166506 = CARTESIAN_POINT('Ctrl Pts',(-20.2781748909328,-14.528829795662,
114.82168445158)) ;
#166507 = CARTESIAN_POINT('Ctrl Pts',(-20.2851290429504,-14.4562719682351,
114.842865677127)) ;
#166508 = CARTESIAN_POINT('Ctrl Pts',(-20.2133069531199,-14.3327513043896,
114.588610844516)) ;
#166509 = CARTESIAN_POINT('Ctrl Pts',(-20.2260203578033,-14.2687127593662,
114.627333824599)) ;
#166510 = CARTESIAN_POINT('Ctrl Pts',(-20.299824191333,-14.2687127399002,
114.603102752789)) ;
#166511 = CARTESIAN_POINT('Ctrl Pts',(-20.3736280248627,-14.2687127204341,
114.578871680979)) ;
#166512 = CARTESIAN_POINT('Ctrl Pts',(-20.3609146201792,-14.3327512654575,
114.540148700895)) ;
#166513 = CARTESIAN_POINT('Ctrl Pts',(-20.3482012154958,-14.3967898104809,
114.501425720811)) ;
#166514 = CARTESIAN_POINT('Ctrl Pts',(-20.2743973819661,-14.3967898299469,
114.525656792621)) ;
#166515 = CARTESIAN_POINT('Ctrl Pts',(-20.2005935484364,-14.396789849413,
114.549887864432)) ;
#166516 = CARTESIAN_POINT('Ctrl Pts',(-20.2133069531199,-14.3327513043896,
114.588610844516)) ;
#166517 = CARTESIAN_POINT('Ctrl Pts',(-20.1547039197829,-14.1436492001557,
114.37463772925)) ;
#166518 = CARTESIAN_POINT('Ctrl Pts',(-20.1722614774345,-14.0927211498799,
114.428115217844)) ;
#166519 = CARTESIAN_POINT('Ctrl Pts',(-20.2460653110969,-14.0927211161122,
114.403884146439)) ;
#166520 = CARTESIAN_POINT('Ctrl Pts',(-20.3198691447594,-14.0927210823444,
114.379653075033)) ;
#166521 = CARTESIAN_POINT('Ctrl Pts',(-20.3023115871078,-14.1436491326202,
114.326175586438)) ;
#166522 = CARTESIAN_POINT('Ctrl Pts',(-20.2847540294562,-14.194577182896,
114.272698097844)) ;
#166523 = CARTESIAN_POINT('Ctrl Pts',(-20.2109501957937,-14.1945772166637,
114.29692916925)) ;
#166524 = CARTESIAN_POINT('Ctrl Pts',(-20.1371463621312,-14.1945772504315,
114.321160240655)) ;
#166525 = CARTESIAN_POINT('Ctrl Pts',(-20.1547039197829,-14.1436492001557,
114.37463772925)) ;
#166526 = CARTESIAN_POINT('Ctrl Pts',(-20.1142261546022,-13.9025966993027,
114.215876145927)) ;
#166527 = CARTESIAN_POINT('Ctrl Pts',(-20.1353692170321,-13.8684250728151,
114.280274503726)) ;
#166528 = CARTESIAN_POINT('Ctrl Pts',(-20.2091730526184,-13.8684250241037,
114.25604343818)) ;
#166529 = CARTESIAN_POINT('Ctrl Pts',(-20.2829768882046,-13.8684249753923,
114.231812372634)) ;
#166530 = CARTESIAN_POINT('Ctrl Pts',(-20.2618338257748,-13.9025966018799,
114.167414014835)) ;
#166531 = CARTESIAN_POINT('Ctrl Pts',(-20.240690763345,-13.9367682283676,
114.103015657035)) ;
#166532 = CARTESIAN_POINT('Ctrl Pts',(-20.1668869277587,-13.936768277079,
114.127246722581)) ;
#166533 = CARTESIAN_POINT('Ctrl Pts',(-20.0930830921724,-13.9367683257904,
114.151477788127)) ;
#166534 = CARTESIAN_POINT('Ctrl Pts',(-20.1142261546022,-13.9025966993027,
114.215876145927)) ;
#166535 = CARTESIAN_POINT('Ctrl Pts',(-20.095524871316,-13.6267191611602,
114.123431540438)) ;
#166536 = CARTESIAN_POINT('Ctrl Pts',(-20.118738436967,-13.6117593942212,
114.194136317143)) ;
#166537 = CARTESIAN_POINT('Ctrl Pts',(-20.1925422763569,-13.6117593320571,
114.169905263182)) ;
#166538 = CARTESIAN_POINT('Ctrl Pts',(-20.2663461157468,-13.6117592698929,
114.145674209222)) ;
#166539 = CARTESIAN_POINT('Ctrl Pts',(-20.2431325500958,-13.6267190368318,
114.074969432517)) ;
#166540 = CARTESIAN_POINT('Ctrl Pts',(-20.2199189844448,-13.6416788037708,
114.004264655812)) ;
#166541 = CARTESIAN_POINT('Ctrl Pts',(-20.1461151450549,-13.641678865935,
114.028495709773)) ;
#166542 = CARTESIAN_POINT('Ctrl Pts',(-20.072311305665,-13.6416789280991,
114.052726763733)) ;
#166543 = CARTESIAN_POINT('Ctrl Pts',(-20.095524871316,-13.6267191611602,
114.123431540438)) ;
#166544 = CARTESIAN_POINT('Ctrl Pts',(-20.100701888957,-13.3360804435672,
114.103739360305)) ;
#166545 = CARTESIAN_POINT('Ctrl Pts',(-20.1243213452086,-13.3413907563864,
114.175680414446)) ;
#166546 = CARTESIAN_POINT('Ctrl Pts',(-20.1981251900942,-13.3413906849688,
114.151449377224)) ;
#166547 = CARTESIAN_POINT('Ctrl Pts',(-20.2719290349799,-13.3413906135511,
114.127218340003)) ;
#166548 = CARTESIAN_POINT('Ctrl Pts',(-20.2483095787283,-13.3360803007319,
114.055277285862)) ;
#166549 = CARTESIAN_POINT('Ctrl Pts',(-20.2246901224767,-13.3307699879127,
113.983336231722)) ;
#166550 = CARTESIAN_POINT('Ctrl Pts',(-20.1508862775911,-13.3307700593304,
114.007567268943)) ;
#166551 = CARTESIAN_POINT('Ctrl Pts',(-20.0770824327054,-13.330770130748,
114.031798306165)) ;
#166552 = CARTESIAN_POINT('Ctrl Pts',(-20.100701888957,-13.3360804435672,
114.103739360305)) ;
#166553 = CARTESIAN_POINT('Ctrl Pts',(-20.1300970691021,-13.0512189530207,
114.157806062876)) ;
#166554 = CARTESIAN_POINT('Ctrl Pts',(-20.1524323332958,-13.076425168365,
114.22583567536)) ;
#166555 = CARTESIAN_POINT('Ctrl Pts',(-20.2262361848485,-13.0764250935319,
114.201604658445)) ;
#166556 = CARTESIAN_POINT('Ctrl Pts',(-20.3000400364012,-13.0764250186989,
114.17737364153)) ;
#166557 = CARTESIAN_POINT('Ctrl Pts',(-20.2777047722075,-13.0512188033546,
114.109344029046)) ;
#166558 = CARTESIAN_POINT('Ctrl Pts',(-20.2553695080138,-13.0260125880103,
114.041314416562)) ;
#166559 = CARTESIAN_POINT('Ctrl Pts',(-20.1815656564611,-13.0260126628434,
114.065545433477)) ;
#166560 = CARTESIAN_POINT('Ctrl Pts',(-20.1077618049083,-13.0260127376764,
114.089776450392)) ;
#166561 = CARTESIAN_POINT('Ctrl Pts',(-20.1300970691021,-13.0512189530207,
114.157806062876)) ;
#166562 = CARTESIAN_POINT('Ctrl Pts',(-20.1824935961161,-12.7925464774136,
114.281896578911)) ;
#166563 = CARTESIAN_POINT('Ctrl Pts',(-20.2019377404634,-12.835849054134,
114.341120306962)) ;
#166564 = CARTESIAN_POINT('Ctrl Pts',(-20.2757415992436,-12.8358489831972,
114.316889312061)) ;
#166565 = CARTESIAN_POINT('Ctrl Pts',(-20.3495454580238,-12.8358489122603,
114.29265831716)) ;
#166566 = CARTESIAN_POINT('Ctrl Pts',(-20.3301013136765,-12.7925463355399,
114.233434589109)) ;
#166567 = CARTESIAN_POINT('Ctrl Pts',(-20.3106571693291,-12.7492437588195,
114.174210861059)) ;
#166568 = CARTESIAN_POINT('Ctrl Pts',(-20.2368533105489,-12.7492438297564,
114.19844185596)) ;
#166569 = CARTESIAN_POINT('Ctrl Pts',(-20.1630494517688,-12.7492439006932,
114.222672850861)) ;
#166570 = CARTESIAN_POINT('Ctrl Pts',(-20.1824935961161,-12.7925464774136,
114.281896578911)) ;
#166571 = CARTESIAN_POINT('Ctrl Pts',(-20.2543021382623,-12.5795095572681,
114.465309293795)) ;
#166572 = CARTESIAN_POINT('Ctrl Pts',(-20.2694915221364,-12.6377483614764,
114.511573708048)) ;
#166573 = CARTESIAN_POINT('Ctrl Pts',(-20.3432953874626,-12.6377483026741,
114.487342733085)) ;
#166574 = CARTESIAN_POINT('Ctrl Pts',(-20.4170992527888,-12.6377482438719,
114.463111758122)) ;
#166575 = CARTESIAN_POINT('Ctrl Pts',(-20.4019098689147,-12.5795094396635,
114.41684734387)) ;
#166576 = CARTESIAN_POINT('Ctrl Pts',(-20.3867204850407,-12.5212706354552,
114.370582929617)) ;
#166577 = CARTESIAN_POINT('Ctrl Pts',(-20.3129166197145,-12.5212706942575,
114.39481390458)) ;
#166578 = CARTESIAN_POINT('Ctrl Pts',(-20.2391127543883,-12.5212707530598,
114.419044879543)) ;
#166579 = CARTESIAN_POINT('Ctrl Pts',(-20.2543021382623,-12.5795095572681,
114.465309293795)) ;
#166580 = CARTESIAN_POINT('Ctrl Pts',(-20.3427409626681,-12.4247175389401,
114.698907771707)) ;
#166581 = CARTESIAN_POINT('Ctrl Pts',(-20.3525184658105,-12.4938489762306,
114.72868847059)) ;
#166582 = CARTESIAN_POINT('Ctrl Pts',(-20.4263223372475,-12.4938489356481,
114.70445751424)) ;
#166583 = CARTESIAN_POINT('Ctrl Pts',(-20.5001262086845,-12.4938488950656,
114.680226557889)) ;
#166584 = CARTESIAN_POINT('Ctrl Pts',(-20.4903487055421,-12.4247174577751,
114.650445859006)) ;
#166585 = CARTESIAN_POINT('Ctrl Pts',(-20.4805712023998,-12.3555860204846,
114.620665160123)) ;
#166586 = CARTESIAN_POINT('Ctrl Pts',(-20.4067673309628,-12.3555860610671,
114.644896116473)) ;
#166587 = CARTESIAN_POINT('Ctrl Pts',(-20.3329634595258,-12.3555861016496,
114.669127072824)) ;
#166588 = CARTESIAN_POINT('Ctrl Pts',(-20.3427409626681,-12.4247175389401,
114.698907771707)) ;
#166589 = CARTESIAN_POINT('Ctrl Pts',(-20.4394881561563,-12.3430591277612,
114.958446225236)) ;
#166590 = CARTESIAN_POINT('Ctrl Pts',(-20.4432522784755,-12.417991968948,
114.969911136438)) ;
#166591 = CARTESIAN_POINT('Ctrl Pts',(-20.5170561530844,-12.4179919531806,
114.945680189749)) ;
#166592 = CARTESIAN_POINT('Ctrl Pts',(-20.5908600276934,-12.4179919374132,
114.92144924306)) ;
#166593 = CARTESIAN_POINT('Ctrl Pts',(-20.5870959053743,-12.3430590962263,
114.909984331859)) ;
#166594 = CARTESIAN_POINT('Ctrl Pts',(-20.5833317830551,-12.2681262550395,
114.898519420657)) ;
#166595 = CARTESIAN_POINT('Ctrl Pts',(-20.5095279084461,-12.2681262708069,
114.922750367346)) ;
#166596 = CARTESIAN_POINT('Ctrl Pts',(-20.4357240338372,-12.2681262865743,
114.946981314035)) ;
#166597 = CARTESIAN_POINT('Ctrl Pts',(-20.4394881561563,-12.3430591277612,
114.958446225236)) ;
#166598 = CARTESIAN_POINT('Ctrl Pts',(-20.5412299493208,-12.3371678726539,
115.232716171247)) ;
#166599 = CARTESIAN_POINT('Ctrl Pts',(-20.5386334836071,-12.4126223874774,
115.224807757656)) ;
#166600 = CARTESIAN_POINT('Ctrl Pts',(-20.6124373596408,-12.4126223993309,
115.200576815306)) ;
#166601 = CARTESIAN_POINT('Ctrl Pts',(-20.6862412356744,-12.4126224111843,
115.176345872957)) ;
#166602 = CARTESIAN_POINT('Ctrl Pts',(-20.688837701388,-12.3371678963608,
115.184254286548)) ;
#166603 = CARTESIAN_POINT('Ctrl Pts',(-20.6914341671017,-12.2617133815373,
115.192162700139)) ;
#166604 = CARTESIAN_POINT('Ctrl Pts',(-20.6176302910681,-12.2617133696838,
115.216393642489)) ;
#166605 = CARTESIAN_POINT('Ctrl Pts',(-20.5438264150345,-12.2617133578303,
115.240624584839)) ;
#166606 = CARTESIAN_POINT('Ctrl Pts',(-20.5412299493208,-12.3371678726539,
115.232716171247)) ;
#166607 = CARTESIAN_POINT('Ctrl Pts',(-20.6396317245463,-12.4090465693171,
115.497017252412)) ;
#166608 = CARTESIAN_POINT('Ctrl Pts',(-20.630894174844,-12.4795937186109,
115.47040408789)) ;
#166609 = CARTESIAN_POINT('Ctrl Pts',(-20.7046980492917,-12.4795937586664,
115.44617314071)) ;
#166610 = CARTESIAN_POINT('Ctrl Pts',(-20.7785019237393,-12.4795937987218,
115.42194219353)) ;
#166611 = CARTESIAN_POINT('Ctrl Pts',(-20.7872394734417,-12.409046649428,
115.448555358052)) ;
#166612 = CARTESIAN_POINT('Ctrl Pts',(-20.795977023144,-12.3384995001342,
115.475168522574)) ;
#166613 = CARTESIAN_POINT('Ctrl Pts',(-20.7221731486963,-12.3384994600787,
115.499399469754)) ;
#166614 = CARTESIAN_POINT('Ctrl Pts',(-20.6483692742486,-12.3384994200233,
115.523630416934)) ;
#166615 = CARTESIAN_POINT('Ctrl Pts',(-20.6396317245463,-12.4090465693171,
115.497017252412)) ;
#166616 = CARTESIAN_POINT('Ctrl Pts',(-20.7292166921784,-12.5533759332391,
115.734353125795)) ;
#166617 = CARTESIAN_POINT('Ctrl Pts',(-20.7149468386475,-12.6139509456652,
115.690889456467)) ;
#166618 = CARTESIAN_POINT('Ctrl Pts',(-20.788750708927,-12.6139510114575,
115.666658496591)) ;
#166619 = CARTESIAN_POINT('Ctrl Pts',(-20.8625545792065,-12.6139510772497,
115.642427536716)) ;
#166620 = CARTESIAN_POINT('Ctrl Pts',(-20.8768244327374,-12.5533760648236,
115.685891206043)) ;
#166621 = CARTESIAN_POINT('Ctrl Pts',(-20.8910942862683,-12.4928010523974,
115.729354875371)) ;
#166622 = CARTESIAN_POINT('Ctrl Pts',(-20.8172904159888,-12.4928009866052,
115.753585835247)) ;
#166623 = CARTESIAN_POINT('Ctrl Pts',(-20.7434865457093,-12.4928009208129,
115.777816795123)) ;
#166624 = CARTESIAN_POINT('Ctrl Pts',(-20.7292166921784,-12.5533759332391,
115.734353125795)) ;
#166625 = CARTESIAN_POINT('Ctrl Pts',(-20.8038057704106,-12.75934674632,115.926107924776)) ;
#166626 = CARTESIAN_POINT('Ctrl Pts',(-20.7850403755029,-12.8056312692346,
115.868951561764)) ;
#166627 = CARTESIAN_POINT('Ctrl Pts',(-20.8588442393246,-12.8056313554312,
115.844720582219)) ;
#166628 = CARTESIAN_POINT('Ctrl Pts',(-20.9326481031462,-12.8056314416279,
115.820489602673)) ;
#166629 = CARTESIAN_POINT('Ctrl Pts',(-20.9514134980538,-12.7593469187134,
115.877645965685)) ;
#166630 = CARTESIAN_POINT('Ctrl Pts',(-20.9701788929615,-12.7130623957988,
115.934802328697)) ;
#166631 = CARTESIAN_POINT('Ctrl Pts',(-20.8963750291398,-12.7130623096021,
115.959033308242)) ;
#166632 = CARTESIAN_POINT('Ctrl Pts',(-20.8225711653182,-12.7130622234055,
115.983264287788)) ;
#166633 = CARTESIAN_POINT('Ctrl Pts',(-20.8038057704106,-12.75934674632,115.926107924776)) ;
#166634 = CARTESIAN_POINT('Ctrl Pts',(-20.8591055199317,-13.0122957598429,
116.059113603157)) ;
#166635 = CARTESIAN_POINT('Ctrl Pts',(-20.8371845005619,-13.0409889610471,
115.99234571717)) ;
#166636 = CARTESIAN_POINT('Ctrl Pts',(-20.910988356368,-13.0409890604734,
115.968114713211)) ;
#166637 = CARTESIAN_POINT('Ctrl Pts',(-20.9847922121742,-13.0409891598997,
115.943883709251)) ;
#166638 = CARTESIAN_POINT('Ctrl Pts',(-21.006713231544,-13.0122959586955,
116.010651595239)) ;
#166639 = CARTESIAN_POINT('Ctrl Pts',(-21.0286342509138,-12.9836027574913,
116.077419481226)) ;
#166640 = CARTESIAN_POINT('Ctrl Pts',(-20.9548303951076,-12.983602658065,
116.101650485186)) ;
#166641 = CARTESIAN_POINT('Ctrl Pts',(-20.8810265393014,-12.9836025586387,
116.125881489145)) ;
#166642 = CARTESIAN_POINT('Ctrl Pts',(-20.8591055199317,-13.0122957598429,
116.059113603157)) ;
#166643 = CARTESIAN_POINT('Ctrl Pts',(-20.8919173958629,-13.2947806869138,
116.123563569553)) ;
#166644 = CARTESIAN_POINT('Ctrl Pts',(-20.868407196844,-13.3037945330256,
116.051955298721)) ;
#166645 = CARTESIAN_POINT('Ctrl Pts',(-20.9422110438593,-13.303794637043,
116.027724267986)) ;
#166646 = CARTESIAN_POINT('Ctrl Pts',(-21.0160148908745,-13.3037947410603,
116.003493237251)) ;
#166647 = CARTESIAN_POINT('Ctrl Pts',(-21.0395250898934,-13.2947808949484,
116.075101508083)) ;
#166648 = CARTESIAN_POINT('Ctrl Pts',(-21.0630352889123,-13.2857670488366,
116.146709778915)) ;
#166649 = CARTESIAN_POINT('Ctrl Pts',(-20.9892314418971,-13.2857669448193,
116.170940809651)) ;
#166650 = CARTESIAN_POINT('Ctrl Pts',(-20.9154275948818,-13.2857668408019,
116.195171840386)) ;
#166651 = CARTESIAN_POINT('Ctrl Pts',(-20.8919173958629,-13.2947806869138,
116.123563569553)) ;
#166652 = CARTESIAN_POINT('Ctrl Pts',(-20.90055362823,-13.5857642149866,116.114420488259)) ;
#166653 = CARTESIAN_POINT('Ctrl Pts',(-20.8771388082436,-13.5744758994453,
116.043102726506)) ;
#166654 = CARTESIAN_POINT('Ctrl Pts',(-20.9509426466584,-13.574475999467,
116.018871669575)) ;
#166655 = CARTESIAN_POINT('Ctrl Pts',(-21.0247464850732,-13.5744760994887,
115.994640612644)) ;
#166656 = CARTESIAN_POINT('Ctrl Pts',(-21.0481613050596,-13.58576441503,116.065958374398)) ;
#166657 = CARTESIAN_POINT('Ctrl Pts',(-21.0715761250459,-13.5970527305713,
116.137276136152)) ;
#166658 = CARTESIAN_POINT('Ctrl Pts',(-20.9977722866311,-13.5970526305496,
116.161507193082)) ;
#166659 = CARTESIAN_POINT('Ctrl Pts',(-20.9239684482163,-13.5970525305279,
116.185738250013)) ;
#166660 = CARTESIAN_POINT('Ctrl Pts',(-20.90055362823,-13.5857642149866,116.114420488259)) ;
#166661 = CARTESIAN_POINT('Ctrl Pts',(-20.8851305069006,-13.8655802602202,
116.031891050549)) ;
#166662 = CARTESIAN_POINT('Ctrl Pts',(-20.8634929365054,-13.8347390280632,
115.965986504196)) ;
#166663 = CARTESIAN_POINT('Ctrl Pts',(-20.9372967673917,-13.8347391156571,
115.941755424335)) ;
#166664 = CARTESIAN_POINT('Ctrl Pts',(-21.011100598278,-13.834739203251,115.917524344474)) ;
#166665 = CARTESIAN_POINT('Ctrl Pts',(-21.0327381686732,-13.865580435408,
115.983428890826)) ;
#166666 = CARTESIAN_POINT('Ctrl Pts',(-21.0543757390685,-13.8964216675651,
116.049333437179)) ;
#166667 = CARTESIAN_POINT('Ctrl Pts',(-20.9805719081821,-13.8964215799712,
116.07356451704)) ;
#166668 = CARTESIAN_POINT('Ctrl Pts',(-20.9067680772958,-13.8964214923772,
116.097795596901)) ;
#166669 = CARTESIAN_POINT('Ctrl Pts',(-20.8851305069006,-13.8655802602202,
116.031891050549)) ;
#166670 = CARTESIAN_POINT('Ctrl Pts',(-20.8474026723801,-14.1129045177148,
115.881445598306)) ;
#166671 = CARTESIAN_POINT('Ctrl Pts',(-20.8291018150253,-14.0647490921529,
115.825704141381)) ;
#166672 = CARTESIAN_POINT('Ctrl Pts',(-20.9029056403244,-14.0647491613001,
115.801473044502)) ;
#166673 = CARTESIAN_POINT('Ctrl Pts',(-20.9767094656234,-14.0647492304473,
115.777241947622)) ;
#166674 = CARTESIAN_POINT('Ctrl Pts',(-20.9950103229782,-14.1129046560093,
115.832983404548)) ;
#166675 = CARTESIAN_POINT('Ctrl Pts',(-21.0133111803329,-14.1610600815713,
115.888724861473)) ;
#166676 = CARTESIAN_POINT('Ctrl Pts',(-20.9395073550338,-14.161060012424,
115.912955958352)) ;
#166677 = CARTESIAN_POINT('Ctrl Pts',(-20.8657035297348,-14.1610599432768,
115.937187055231)) ;
#166678 = CARTESIAN_POINT('Ctrl Pts',(-20.8474026723801,-14.1129045177148,
115.881445598306)) ;
#166679 = CARTESIAN_POINT('Ctrl Pts',(-20.7913821624318,-14.3092608415155,
115.675523483977)) ;
#166680 = CARTESIAN_POINT('Ctrl Pts',(-20.7776954169706,-14.2473238052157,
115.633835867297)) ;
#166681 = CARTESIAN_POINT('Ctrl Pts',(-20.8514992385119,-14.2473238535572,
115.609604758972)) ;
#166682 = CARTESIAN_POINT('Ctrl Pts',(-20.9253030600531,-14.2473239018987,
115.585373650647)) ;
#166683 = CARTESIAN_POINT('Ctrl Pts',(-20.9389898055142,-14.3092609381985,
115.627061267327)) ;
#166684 = CARTESIAN_POINT('Ctrl Pts',(-20.9526765509754,-14.3711979744983,
115.668748884008)) ;
#166685 = CARTESIAN_POINT('Ctrl Pts',(-20.8788727294342,-14.3711979261568,
115.692979992333)) ;
#166686 = CARTESIAN_POINT('Ctrl Pts',(-20.805068907893,-14.3711978778153,
115.717211100658)) ;
#166687 = CARTESIAN_POINT('Ctrl Pts',(-20.7913821624318,-14.3092608415155,
115.675523483977)) ;
#166688 = CARTESIAN_POINT('Ctrl Pts',(-20.721035507872,-14.4430503329775,
115.425718401597)) ;
#166689 = CARTESIAN_POINT('Ctrl Pts',(-20.7129749835062,-14.3716785302195,
115.401167346437)) ;
#166690 = CARTESIAN_POINT('Ctrl Pts',(-20.786778804069,-14.371678555561,115.376936235132)) ;
#166691 = CARTESIAN_POINT('Ctrl Pts',(-20.8605826246318,-14.3716785809024,
115.352705123826)) ;
#166692 = CARTESIAN_POINT('Ctrl Pts',(-20.8686431489976,-14.4430503836605,
115.377256178986)) ;
#166693 = CARTESIAN_POINT('Ctrl Pts',(-20.8767036733634,-14.5144221864185,
115.401807234146)) ;
#166694 = CARTESIAN_POINT('Ctrl Pts',(-20.8028998528006,-14.5144221610771,
115.426038345451)) ;
#166695 = CARTESIAN_POINT('Ctrl Pts',(-20.7290960322378,-14.5144221357356,
115.450269456757)) ;
#166696 = CARTESIAN_POINT('Ctrl Pts',(-20.721035507872,-14.4430503329775,
115.425718401597)) ;
#166697 = CARTESIAN_POINT('Ctrl Pts',(-20.6429181303812,-14.5029681127336,
115.152436570148)) ;
#166698 = CARTESIAN_POINT('Ctrl Pts',(-20.6410310401035,-14.4273052047568,
115.146688799011)) ;
#166699 = CARTESIAN_POINT('Ctrl Pts',(-20.7148348614875,-14.427305209291,
115.122457690207)) ;
#166700 = CARTESIAN_POINT('Ctrl Pts',(-20.7886386828715,-14.4273052138253,
115.098226581403)) ;
#166701 = CARTESIAN_POINT('Ctrl Pts',(-20.7905257731491,-14.5029681218021,
115.10397435254)) ;
#166702 = CARTESIAN_POINT('Ctrl Pts',(-20.7924128634268,-14.5786310297789,
115.109722123678)) ;
#166703 = CARTESIAN_POINT('Ctrl Pts',(-20.7186090420428,-14.5786310252447,
115.133953232482)) ;
#166704 = CARTESIAN_POINT('Ctrl Pts',(-20.6448052206588,-14.5786310207104,
115.158184341285)) ;
#166705 = CARTESIAN_POINT('Ctrl Pts',(-20.6429181303812,-14.5029681127336,
115.152436570148)) ;
#166706 = CARTESIAN_POINT('Ctrl Pts',(-20.5625765334162,-14.4854361051768,
114.872178149454)) ;
#166707 = CARTESIAN_POINT('Ctrl Pts',(-20.5670316746526,-14.4108823854582,
114.885747792019)) ;
#166708 = CARTESIAN_POINT('Ctrl Pts',(-20.6408354992009,-14.4108823726848,
114.861516692854)) ;
#166709 = CARTESIAN_POINT('Ctrl Pts',(-20.7146393237493,-14.4108823599115,
114.837285593688)) ;
#166710 = CARTESIAN_POINT('Ctrl Pts',(-20.7101841825129,-14.4854360796301,
114.823715951122)) ;
#166711 = CARTESIAN_POINT('Ctrl Pts',(-20.7057290412765,-14.5599897993486,
114.810146308557)) ;
#166712 = CARTESIAN_POINT('Ctrl Pts',(-20.6319252167282,-14.559989812122,
114.834377407723)) ;
#166713 = CARTESIAN_POINT('Ctrl Pts',(-20.5581213921798,-14.5599898248954,
114.858608506888)) ;
#166714 = CARTESIAN_POINT('Ctrl Pts',(-20.5625765334162,-14.4854361051768,
114.872178149454)) ;
#166715 = CARTESIAN_POINT('Ctrl Pts',(-20.487126571455,-14.3912934817558,
114.606906973503)) ;
#166716 = CARTESIAN_POINT('Ctrl Pts',(-20.4975902895172,-14.3231998086573,
114.638777771435)) ;
#166717 = CARTESIAN_POINT('Ctrl Pts',(-20.5713941181967,-14.323199784148,
114.614546684851)) ;
#166718 = CARTESIAN_POINT('Ctrl Pts',(-20.6451979468761,-14.3231997596387,
114.590315598268)) ;
#166719 = CARTESIAN_POINT('Ctrl Pts',(-20.6347342288138,-14.3912934327372,
114.558444800337)) ;
#166720 = CARTESIAN_POINT('Ctrl Pts',(-20.6242705107516,-14.4593871058357,
114.526574002406)) ;
#166721 = CARTESIAN_POINT('Ctrl Pts',(-20.5504666820722,-14.459387130345,
114.550805088989)) ;
#166722 = CARTESIAN_POINT('Ctrl Pts',(-20.4766628533928,-14.4593871548543,
114.575036175572)) ;
#166723 = CARTESIAN_POINT('Ctrl Pts',(-20.487126571455,-14.3912934817558,
114.606906973503)) ;
#166724 = CARTESIAN_POINT('Ctrl Pts',(-20.4224950432622,-14.2271892392871,
114.374541511787)) ;
#166725 = CARTESIAN_POINT('Ctrl Pts',(-20.4382221279366,-14.1704502048887,
114.422443675001)) ;
#166726 = CARTESIAN_POINT('Ctrl Pts',(-20.5120259612717,-14.1704501748707,
114.398212602598)) ;
#166727 = CARTESIAN_POINT('Ctrl Pts',(-20.5858297946069,-14.1704501448526,
114.373981530195)) ;
#166728 = CARTESIAN_POINT('Ctrl Pts',(-20.5701027099325,-14.227189179251,
114.326079366981)) ;
#166729 = CARTESIAN_POINT('Ctrl Pts',(-20.5543756252582,-14.2839282136493,
114.278177203767)) ;
#166730 = CARTESIAN_POINT('Ctrl Pts',(-20.480571791923,-14.2839282436673,
114.30240827617)) ;
#166731 = CARTESIAN_POINT('Ctrl Pts',(-20.4067679585879,-14.2839282736854,
114.326639348572)) ;
#166732 = CARTESIAN_POINT('Ctrl Pts',(-20.4224950432622,-14.2271892392871,
114.374541511787)) ;
#166733 = CARTESIAN_POINT('Ctrl Pts',(-20.3743070729178,-14.0061849375035,
114.192428883395)) ;
#166734 = CARTESIAN_POINT('Ctrl Pts',(-20.3941538224714,-13.9647911087946,
114.252878880981)) ;
#166735 = CARTESIAN_POINT('Ctrl Pts',(-20.4679576599053,-13.9647910776001,
114.228647821063)) ;
#166736 = CARTESIAN_POINT('Ctrl Pts',(-20.5417614973391,-13.9647910464057,
114.204416761144)) ;
#166737 = CARTESIAN_POINT('Ctrl Pts',(-20.5219147477856,-14.0061848751146,
114.143966763558)) ;
#166738 = CARTESIAN_POINT('Ctrl Pts',(-20.502067998232,-14.0475787038235,
114.083516765971)) ;
#166739 = CARTESIAN_POINT('Ctrl Pts',(-20.4282641607982,-14.047578735018,
114.10774782589)) ;
#166740 = CARTESIAN_POINT('Ctrl Pts',(-20.3544603233643,-14.0475787662124,
114.131978885808)) ;
#166741 = CARTESIAN_POINT('Ctrl Pts',(-20.3743070729178,-14.0061849375035,
114.192428883395)) ;
#166742 = CARTESIAN_POINT('Ctrl Pts',(-20.3463468419125,-13.7418695803109,
114.071733618865)) ;
#166743 = CARTESIAN_POINT('Ctrl Pts',(-20.3689113162977,-13.7188682914606,
114.14046136761)) ;
#166744 = CARTESIAN_POINT('Ctrl Pts',(-20.4427151573719,-13.7188682649132,
114.11623031878)) ;
#166745 = CARTESIAN_POINT('Ctrl Pts',(-20.516518998446,-13.7188682383657,
114.091999269949)) ;
#166746 = CARTESIAN_POINT('Ctrl Pts',(-20.4939545240607,-13.741869527216,
114.023271521203)) ;
#166747 = CARTESIAN_POINT('Ctrl Pts',(-20.4713900496754,-13.7648708160662,
113.954543772457)) ;
#166748 = CARTESIAN_POINT('Ctrl Pts',(-20.3975862086013,-13.7648708426137,
113.978774821288)) ;
#166749 = CARTESIAN_POINT('Ctrl Pts',(-20.3237823675271,-13.7648708691611,
114.003005870119)) ;
#166750 = CARTESIAN_POINT('Ctrl Pts',(-20.3463468419125,-13.7418695803109,
114.071733618865)) ;
#166751 = CARTESIAN_POINT('Ctrl Pts',(-20.3416219830562,-13.4550293844737,
114.021913569137)) ;
#166752 = CARTESIAN_POINT('Ctrl Pts',(-20.3652836693087,-13.4520215652615,
114.093983248047)) ;
#166753 = CARTESIAN_POINT('Ctrl Pts',(-20.439087512752,-13.4520215454244,
114.069752206432)) ;
#166754 = CARTESIAN_POINT('Ctrl Pts',(-20.5128913561953,-13.4520215255873,
114.045521164817)) ;
#166755 = CARTESIAN_POINT('Ctrl Pts',(-20.4892296699427,-13.4550293447994,
113.973451485907)) ;
#166756 = CARTESIAN_POINT('Ctrl Pts',(-20.4655679836902,-13.4580371640116,
113.901381806997)) ;
#166757 = CARTESIAN_POINT('Ctrl Pts',(-20.3917641402469,-13.4580371838487,
113.925612848612)) ;
#166758 = CARTESIAN_POINT('Ctrl Pts',(-20.3179602968036,-13.4580372036859,
113.949843890227)) ;
#166759 = CARTESIAN_POINT('Ctrl Pts',(-20.3416219830562,-13.4550293844737,
114.021913569137)) ;
#166760 = CARTESIAN_POINT('Ctrl Pts',(-20.3614601534258,-13.1635845721582,
114.04665004701)) ;
#166761 = CARTESIAN_POINT('Ctrl Pts',(-20.3845110947562,-13.180922781359,
114.11685949526)) ;
#166762 = CARTESIAN_POINT('Ctrl Pts',(-20.4583149391496,-13.1809227707576,
114.092628456539)) ;
#166763 = CARTESIAN_POINT('Ctrl Pts',(-20.532118783543,-13.1809227601562,
114.068397417818)) ;
#166764 = CARTESIAN_POINT('Ctrl Pts',(-20.5090678422126,-13.1635845509553,
113.998187969568)) ;
#166765 = CARTESIAN_POINT('Ctrl Pts',(-20.4860169008822,-13.1462463417545,
113.927978521319)) ;
#166766 = CARTESIAN_POINT('Ctrl Pts',(-20.4122130564889,-13.1462463523559,
113.95220956004)) ;
#166767 = CARTESIAN_POINT('Ctrl Pts',(-20.3384092120955,-13.1462463629573,
113.976440598761)) ;
#166768 = CARTESIAN_POINT('Ctrl Pts',(-20.3614601534258,-13.1635845721582,
114.04665004701)) ;
#166769 = CARTESIAN_POINT('Ctrl Pts',(-20.4044535755017,-12.8938493439813,
114.142385565385)) ;
#166770 = CARTESIAN_POINT('Ctrl Pts',(-20.4252657787376,-12.9300476003649,
114.205776178532)) ;
#166771 = CARTESIAN_POINT('Ctrl Pts',(-20.499069623255,-12.9300475948517,
114.181545140189)) ;
#166772 = CARTESIAN_POINT('Ctrl Pts',(-20.5728734677724,-12.9300475893384,
114.157314101845)) ;
#166773 = CARTESIAN_POINT('Ctrl Pts',(-20.5520612645364,-12.8938493329547,
114.093923488698)) ;
#166774 = CARTESIAN_POINT('Ctrl Pts',(-20.5312490613004,-12.857651076571,
114.030532875551)) ;
#166775 = CARTESIAN_POINT('Ctrl Pts',(-20.4574452167831,-12.8576510820843,
114.054763913894)) ;
#166776 = CARTESIAN_POINT('Ctrl Pts',(-20.3836413722657,-12.8576510875976,
114.078994952238)) ;
#166777 = CARTESIAN_POINT('Ctrl Pts',(-20.4044535755017,-12.8938493439813,
114.142385565385)) ;
#166778 = CARTESIAN_POINT('Ctrl Pts',(-20.4694496412937,-12.658475902558,
114.304658716124)) ;
#166779 = CARTESIAN_POINT('Ctrl Pts',(-20.4864933769325,-12.7111646806542,
114.356571184894)) ;
#166780 = CARTESIAN_POINT('Ctrl Pts',(-20.5602972205623,-12.7111646805121,
114.332340143848)) ;
#166781 = CARTESIAN_POINT('Ctrl Pts',(-20.6341010641921,-12.7111646803699,
114.308109102801)) ;
#166782 = CARTESIAN_POINT('Ctrl Pts',(-20.6170573285533,-12.6584759022737,
114.25619663403)) ;
#166783 = CARTESIAN_POINT('Ctrl Pts',(-20.6000135929145,-12.6057871241775,
114.20428416526)) ;
#166784 = CARTESIAN_POINT('Ctrl Pts',(-20.5262097492847,-12.6057871243196,
114.228515206307)) ;
#166785 = CARTESIAN_POINT('Ctrl Pts',(-20.4524059056549,-12.6057871244618,
114.252746247354)) ;
#166786 = CARTESIAN_POINT('Ctrl Pts',(-20.4694496412937,-12.658475902558,
114.304658716124)) ;
#166787 = CARTESIAN_POINT('Ctrl Pts',(-20.5508406891179,-12.480124052921,
114.517369062638)) ;
#166788 = CARTESIAN_POINT('Ctrl Pts',(-20.5629548634475,-12.545344547809,
114.554266882997)) ;
#166789 = CARTESIAN_POINT('Ctrl Pts',(-20.6367587064007,-12.5453445488469,
114.530035839889)) ;
#166790 = CARTESIAN_POINT('Ctrl Pts',(-20.7105625493539,-12.5453445498848,
114.505804796782)) ;
#166791 = CARTESIAN_POINT('Ctrl Pts',(-20.6984483750243,-12.4801240549968,
114.468906976423)) ;
#166792 = CARTESIAN_POINT('Ctrl Pts',(-20.6863342006947,-12.4149035601088,
114.432009156064)) ;
#166793 = CARTESIAN_POINT('Ctrl Pts',(-20.6125303577415,-12.414903559071,
114.456240199172)) ;
#166794 = CARTESIAN_POINT('Ctrl Pts',(-20.5387265147883,-12.4149035580331,
114.480471242279)) ;
#166795 = CARTESIAN_POINT('Ctrl Pts',(-20.5508406891179,-12.480124052921,
114.517369062638)) ;
#166796 = CARTESIAN_POINT('Ctrl Pts',(-20.6459051268629,-12.366810202119,
114.77115798259)) ;
#166797 = CARTESIAN_POINT('Ctrl Pts',(-20.6521390295966,-12.4400414291151,
114.790145444413)) ;
#166798 = CARTESIAN_POINT('Ctrl Pts',(-20.7259428719618,-12.4400414300861,
114.765914399515)) ;
#166799 = CARTESIAN_POINT('Ctrl Pts',(-20.799746714327,-12.4400414310572,
114.741683354616)) ;
#166800 = CARTESIAN_POINT('Ctrl Pts',(-20.7935128115933,-12.3668102040611,
114.722695892793)) ;
#166801 = CARTESIAN_POINT('Ctrl Pts',(-20.7872789088596,-12.2935789770651,
114.70370843097)) ;
#166802 = CARTESIAN_POINT('Ctrl Pts',(-20.7134750664944,-12.293578976094,
114.727939475869)) ;
#166803 = CARTESIAN_POINT('Ctrl Pts',(-20.6396712241292,-12.293578975123,
114.752170520767)) ;
#166804 = CARTESIAN_POINT('Ctrl Pts',(-20.6459051268629,-12.366810202119,
114.77115798259)) ;
#166805 = CARTESIAN_POINT('Ctrl Pts',(-20.7458815806501,-12.3300613553443,
115.040439167001)) ;
#166806 = CARTESIAN_POINT('Ctrl Pts',(-20.745872671566,-12.4059660659724,
115.040412031318)) ;
#166807 = CARTESIAN_POINT('Ctrl Pts',(-20.8196765141725,-12.4059660657075,
115.016180987155)) ;
#166808 = CARTESIAN_POINT('Ctrl Pts',(-20.8934803567791,-12.4059660654426,
114.991949942991)) ;
#166809 = CARTESIAN_POINT('Ctrl Pts',(-20.8934892658632,-12.3300613548144,
114.991977078674)) ;
#166810 = CARTESIAN_POINT('Ctrl Pts',(-20.8934981749473,-12.2541566441862,
114.992004214356)) ;
#166811 = CARTESIAN_POINT('Ctrl Pts',(-20.8196943323408,-12.2541566444512,
115.01623525852)) ;
#166812 = CARTESIAN_POINT('Ctrl Pts',(-20.7458904897342,-12.2541566447161,
115.040466302683)) ;
#166813 = CARTESIAN_POINT('Ctrl Pts',(-20.7458815806501,-12.3300613553443,
115.040439167001)) ;
#166814 = CARTESIAN_POINT('Ctrl Pts',(-20.8468477493283,-12.3711193571588,
115.312306178945)) ;
#166815 = CARTESIAN_POINT('Ctrl Pts',(-20.8405264551882,-12.4442691147832,
115.293052536951)) ;
#166816 = CARTESIAN_POINT('Ctrl Pts',(-20.9143302989252,-12.4442691147866,
115.268821496231)) ;
#166817 = CARTESIAN_POINT('Ctrl Pts',(-20.9881341426622,-12.44426911479,115.24459045551)) ;
#166818 = CARTESIAN_POINT('Ctrl Pts',(-20.9944554368023,-12.3711193571657,
115.263844097504)) ;
#166819 = CARTESIAN_POINT('Ctrl Pts',(-21.0007767309424,-12.2979695995413,
115.283097739498)) ;
#166820 = CARTESIAN_POINT('Ctrl Pts',(-20.9269728872054,-12.2979695995379,
115.307328780218)) ;
#166821 = CARTESIAN_POINT('Ctrl Pts',(-20.8531690434684,-12.2979695995345,
115.331559820939)) ;
#166822 = CARTESIAN_POINT('Ctrl Pts',(-20.8468477493283,-12.3711193571588,
115.312306178945)) ;
#166823 = CARTESIAN_POINT('Ctrl Pts',(-20.9400118268714,-12.4860834955726,
115.560871243411)) ;
#166824 = CARTESIAN_POINT('Ctrl Pts',(-20.927904670528,-12.5513121633835,
115.523994798755)) ;
#166825 = CARTESIAN_POINT('Ctrl Pts',(-21.0017085151598,-12.5513121652031,
115.49976376076)) ;
#166826 = CARTESIAN_POINT('Ctrl Pts',(-21.0755123597916,-12.5513121670227,
115.475532722765)) ;
#166827 = CARTESIAN_POINT('Ctrl Pts',(-21.087619516135,-12.4860834992117,
115.512409167422)) ;
#166828 = CARTESIAN_POINT('Ctrl Pts',(-21.0997266724784,-12.4208548314008,
115.549285612078)) ;
#166829 = CARTESIAN_POINT('Ctrl Pts',(-21.0259228278466,-12.4208548295812,
115.573516650073)) ;
#166830 = CARTESIAN_POINT('Ctrl Pts',(-20.9521189832147,-12.4208548277616,
115.597747688068)) ;
#166831 = CARTESIAN_POINT('Ctrl Pts',(-20.9400118268714,-12.4860834955726,
115.560871243411)) ;
#166832 = CARTESIAN_POINT('Ctrl Pts',(-21.0218131787759,-12.6694591781323,
115.774349736538)) ;
#166833 = CARTESIAN_POINT('Ctrl Pts',(-21.0047147067805,-12.7219791159764,
115.72227054989)) ;
#166834 = CARTESIAN_POINT('Ctrl Pts',(-21.0785185527964,-12.7219791238396,
115.698039516111)) ;
#166835 = CARTESIAN_POINT('Ctrl Pts',(-21.1523223988123,-12.7219791317028,
115.673808482332)) ;
#166836 = CARTESIAN_POINT('Ctrl Pts',(-21.1694208708077,-12.6694591938587,
115.72588766898)) ;
#166837 = CARTESIAN_POINT('Ctrl Pts',(-21.1865193428031,-12.6169392560146,
115.777966855628)) ;
#166838 = CARTESIAN_POINT('Ctrl Pts',(-21.1127154967872,-12.6169392481514,
115.802197889407)) ;
#166839 = CARTESIAN_POINT('Ctrl Pts',(-21.0389116507713,-12.6169392402883,
115.826428923186)) ;
#166840 = CARTESIAN_POINT('Ctrl Pts',(-21.0218131787759,-12.6694591781323,
115.774349736538)) ;
#166841 = CARTESIAN_POINT('Ctrl Pts',(-21.0853187896977,-12.9054683696908,
115.932363519269)) ;
#166842 = CARTESIAN_POINT('Ctrl Pts',(-21.0644942259678,-12.9415855764778,
115.868935258532)) ;
#166843 = CARTESIAN_POINT('Ctrl Pts',(-21.1382980722319,-12.9415855922766,
115.844704225508)) ;
#166844 = CARTESIAN_POINT('Ctrl Pts',(-21.212101918496,-12.9415856080754,
115.820473192485)) ;
#166845 = CARTESIAN_POINT('Ctrl Pts',(-21.232926482226,-12.9054684012884,
115.883901453223)) ;
#166846 = CARTESIAN_POINT('Ctrl Pts',(-21.2537510459559,-12.8693511945013,
115.947329713961)) ;
#166847 = CARTESIAN_POINT('Ctrl Pts',(-21.1799471996917,-12.8693511787026,
115.971560746984)) ;
#166848 = CARTESIAN_POINT('Ctrl Pts',(-21.1061433534276,-12.8693511629038,
115.995791780007)) ;
#166849 = CARTESIAN_POINT('Ctrl Pts',(-21.0853187896977,-12.9054683696908,
115.932363519269)) ;
#166850 = CARTESIAN_POINT('Ctrl Pts',(-21.1275223807036,-13.1783417993353,
116.025441846581)) ;
#166851 = CARTESIAN_POINT('Ctrl Pts',(-21.1044548326585,-13.1954587831432,
115.955181817674)) ;
#166852 = CARTESIAN_POINT('Ctrl Pts',(-21.1782586780653,-13.1954588083928,
115.93095078204)) ;
#166853 = CARTESIAN_POINT('Ctrl Pts',(-21.252062523472,-13.1954588336424,
115.906719746405)) ;
#166854 = CARTESIAN_POINT('Ctrl Pts',(-21.2751300715171,-13.1783418498345,
115.976979775312)) ;
#166855 = CARTESIAN_POINT('Ctrl Pts',(-21.2981976195622,-13.1612248660266,
116.047239804219)) ;
#166856 = CARTESIAN_POINT('Ctrl Pts',(-21.2243937741555,-13.161224840777,
116.071470839854)) ;
#166857 = CARTESIAN_POINT('Ctrl Pts',(-21.1505899287487,-13.1612248155274,
116.095701875488)) ;
#166858 = CARTESIAN_POINT('Ctrl Pts',(-21.1275223807036,-13.1783417993353,
116.025441846581)) ;
#166859 = CARTESIAN_POINT('Ctrl Pts',(-21.1459730069986,-13.4677014527882,
116.046259246478)) ;
#166860 = CARTESIAN_POINT('Ctrl Pts',(-21.1223160522397,-13.4646398279822,
115.974203979966)) ;
#166861 = CARTESIAN_POINT('Ctrl Pts',(-21.1961198953758,-13.4646398615466,
115.949972937416)) ;
#166862 = CARTESIAN_POINT('Ctrl Pts',(-21.269923738512,-13.464639895111,115.925741894866)) ;
#166863 = CARTESIAN_POINT('Ctrl Pts',(-21.2935806932709,-13.4677015199171,
115.997797161377)) ;
#166864 = CARTESIAN_POINT('Ctrl Pts',(-21.3172376480298,-13.4707631447231,
116.069852427888)) ;
#166865 = CARTESIAN_POINT('Ctrl Pts',(-21.2434338048937,-13.4707631111587,
116.094083470438)) ;
#166866 = CARTESIAN_POINT('Ctrl Pts',(-21.1696299617576,-13.4707630775943,
116.118314512989)) ;
#166867 = CARTESIAN_POINT('Ctrl Pts',(-21.1459730069986,-13.4677014527882,
116.046259246478)) ;
#166868 = CARTESIAN_POINT('Ctrl Pts',(-21.1402886926304,-13.7542094632266,
115.99348562837)) ;
#166869 = CARTESIAN_POINT('Ctrl Pts',(-21.1177281868373,-13.7311394476093,
115.924769968664)) ;
#166870 = CARTESIAN_POINT('Ctrl Pts',(-21.1915320264503,-13.7311394879972,
115.900538915382)) ;
#166871 = CARTESIAN_POINT('Ctrl Pts',(-21.2653358660634,-13.7311395283851,
115.876307862101)) ;
#166872 = CARTESIAN_POINT('Ctrl Pts',(-21.2878963718565,-13.7542095440024,
115.945023521808)) ;
#166873 = CARTESIAN_POINT('Ctrl Pts',(-21.3104568776496,-13.7772795596197,
116.013739181515)) ;
#166874 = CARTESIAN_POINT('Ctrl Pts',(-21.2366530380365,-13.7772795192318,
116.037970234796)) ;
#166875 = CARTESIAN_POINT('Ctrl Pts',(-21.1628491984234,-13.7772794788439,
116.062201288077)) ;
#166876 = CARTESIAN_POINT('Ctrl Pts',(-21.1402886926304,-13.7542094632266,
115.99348562837)) ;
#166877 = CARTESIAN_POINT('Ctrl Pts',(-21.111182052806,-14.0177953901298,
115.869184389673)) ;
#166878 = CARTESIAN_POINT('Ctrl Pts',(-21.091358617658,-13.976288401055,115.808805405729)) ;
#166879 = CARTESIAN_POINT('Ctrl Pts',(-21.1651624521965,-13.9762884453848,
115.784574336992)) ;
#166880 = CARTESIAN_POINT('Ctrl Pts',(-21.238966286735,-13.9762884897146,
115.760343268254)) ;
#166881 = CARTESIAN_POINT('Ctrl Pts',(-21.258789721883,-14.0177954787893,
115.820722252198)) ;
#166882 = CARTESIAN_POINT('Ctrl Pts',(-21.278613157031,-14.0593024678641,
115.881101236141)) ;
#166883 = CARTESIAN_POINT('Ctrl Pts',(-21.2048093224926,-14.0593024235343,
115.905332304878)) ;
#166884 = CARTESIAN_POINT('Ctrl Pts',(-21.131005487954,-14.0593023792045,
115.929563373616)) ;
#166885 = CARTESIAN_POINT('Ctrl Pts',(-21.111182052806,-14.0177953901298,
115.869184389673)) ;
#166886 = CARTESIAN_POINT('Ctrl Pts',(-21.0622744394062,-14.2358411050757,
115.684975992788)) ;
#166887 = CARTESIAN_POINT('Ctrl Pts',(-21.0465664537973,-14.1790508956255,
115.63713200424)) ;
#166888 = CARTESIAN_POINT('Ctrl Pts',(-21.1203702834702,-14.1790509350975,
115.612900920683)) ;
#166889 = CARTESIAN_POINT('Ctrl Pts',(-21.194174113143,-14.1790509745695,
115.588669837125)) ;
#166890 = CARTESIAN_POINT('Ctrl Pts',(-21.2098820987519,-14.2358411840197,
115.636513825673)) ;
#166891 = CARTESIAN_POINT('Ctrl Pts',(-21.2255900843608,-14.2926313934699,
115.684357814221)) ;
#166892 = CARTESIAN_POINT('Ctrl Pts',(-21.1517862546879,-14.2926313539979,
115.708588897779)) ;
#166893 = CARTESIAN_POINT('Ctrl Pts',(-21.077982425015,-14.2926313145259,
115.732819981336)) ;
#166894 = CARTESIAN_POINT('Ctrl Pts',(-21.0622744394062,-14.2358411050757,
115.684975992788)) ;
#166895 = CARTESIAN_POINT('Ctrl Pts',(-20.9969244848175,-14.3973545116793,
115.450360447724)) ;
#166896 = CARTESIAN_POINT('Ctrl Pts',(-20.9864923098944,-14.3292054144305,
115.418585727457)) ;
#166897 = CARTESIAN_POINT('Ctrl Pts',(-21.0602961341888,-14.3292054449857,
115.394354627517)) ;
#166898 = CARTESIAN_POINT('Ctrl Pts',(-21.1340999584832,-14.3292054755409,
115.370123527578)) ;
#166899 = CARTESIAN_POINT('Ctrl Pts',(-21.1445321334063,-14.3973545727897,
115.401898247845)) ;
#166900 = CARTESIAN_POINT('Ctrl Pts',(-21.1549643083294,-14.4655036700385,
115.433672968112)) ;
#166901 = CARTESIAN_POINT('Ctrl Pts',(-21.081160484035,-14.4655036394833,
115.457904068052)) ;
#166902 = CARTESIAN_POINT('Ctrl Pts',(-21.0073566597406,-14.4655036089281,
115.482135167991)) ;
#166903 = CARTESIAN_POINT('Ctrl Pts',(-20.9969244848175,-14.3973545116793,
115.450360447724)) ;
#166904 = CARTESIAN_POINT('Ctrl Pts',(-20.9210657871025,-14.487909543941,
115.183827051948)) ;
#166905 = CARTESIAN_POINT('Ctrl Pts',(-20.9166489046695,-14.4133393487521,
115.170373942196)) ;
#166906 = CARTESIAN_POINT('Ctrl Pts',(-20.9904527246687,-14.4133393631785,
115.146142829174)) ;
#166907 = CARTESIAN_POINT('Ctrl Pts',(-21.0642565446678,-14.413339377605,
115.121911716152)) ;
#166908 = CARTESIAN_POINT('Ctrl Pts',(-21.0686734271008,-14.4879095727939,
115.135364825905)) ;
#166909 = CARTESIAN_POINT('Ctrl Pts',(-21.0730903095338,-14.5624797679828,
115.148817935657)) ;
#166910 = CARTESIAN_POINT('Ctrl Pts',(-20.9992864895347,-14.5624797535563,
115.173049048679)) ;
#166911 = CARTESIAN_POINT('Ctrl Pts',(-20.9254826695355,-14.5624797391299,
115.197280161701)) ;
#166912 = CARTESIAN_POINT('Ctrl Pts',(-20.9210657871025,-14.487909543941,
115.183827051948)) ;
#166913 = CARTESIAN_POINT('Ctrl Pts',(-20.8410002283841,-14.501998059837,
114.904561059631)) ;
#166914 = CARTESIAN_POINT('Ctrl Pts',(-20.842899355212,-14.4263362561648,
114.910345495132)) ;
#166915 = CARTESIAN_POINT('Ctrl Pts',(-20.9167031727645,-14.4263362496198,
114.886114374658)) ;
#166916 = CARTESIAN_POINT('Ctrl Pts',(-20.9905069903171,-14.4263362430748,
114.861883254185)) ;
#166917 = CARTESIAN_POINT('Ctrl Pts',(-20.9886078634892,-14.501998046747,
114.856098818683)) ;
#166918 = CARTESIAN_POINT('Ctrl Pts',(-20.9867087366614,-14.5776598504192,
114.850314383182)) ;
#166919 = CARTESIAN_POINT('Ctrl Pts',(-20.9129049191088,-14.5776598569642,
114.874545503655)) ;
#166920 = CARTESIAN_POINT('Ctrl Pts',(-20.8391011015563,-14.5776598635092,
114.898776624129)) ;
#166921 = CARTESIAN_POINT('Ctrl Pts',(-20.8410002283841,-14.501998059837,
114.904561059631)) ;
#166922 = CARTESIAN_POINT('Ctrl Pts',(-20.7628140637106,-14.4383564825309,
114.63092278003)) ;
#166923 = CARTESIAN_POINT('Ctrl Pts',(-20.7709091130621,-14.3670278101873,
114.65557899596)) ;
#166924 = CARTESIAN_POINT('Ctrl Pts',(-20.8447129301326,-14.3670277794582,
114.631347874018)) ;
#166925 = CARTESIAN_POINT('Ctrl Pts',(-20.918516747203,-14.3670277487292,
114.607116752076)) ;
#166926 = CARTESIAN_POINT('Ctrl Pts',(-20.9104216978515,-14.4383564210728,
114.582460536145)) ;
#166927 = CARTESIAN_POINT('Ctrl Pts',(-20.9023266485,-14.5096850934165,114.557804320215)) ;
#166928 = CARTESIAN_POINT('Ctrl Pts',(-20.8285228314295,-14.5096851241455,
114.582035442157)) ;
#166929 = CARTESIAN_POINT('Ctrl Pts',(-20.7547190143591,-14.5096851548746,
114.606266564099)) ;
#166930 = CARTESIAN_POINT('Ctrl Pts',(-20.7628140637106,-14.4383564825309,
114.63092278003)) ;
#166931 = CARTESIAN_POINT('Ctrl Pts',(-20.6932450307031,-14.3021834028963,
114.383646838591)) ;
#166932 = CARTESIAN_POINT('Ctrl Pts',(-20.706940971323,-14.2402581580985,
114.425362465725)) ;
#166933 = CARTESIAN_POINT('Ctrl Pts',(-20.7807447905397,-14.2402581030473,
114.40113135032)) ;
#166934 = CARTESIAN_POINT('Ctrl Pts',(-20.8545486097562,-14.2402580479961,
114.376900234914)) ;
#166935 = CARTESIAN_POINT('Ctrl Pts',(-20.8408526691363,-14.3021832927938,
114.33518460778)) ;
#166936 = CARTESIAN_POINT('Ctrl Pts',(-20.8271567285164,-14.3641085375916,
114.293468980646)) ;
#166937 = CARTESIAN_POINT('Ctrl Pts',(-20.7533529092998,-14.3641085926428,
114.317700096051)) ;
#166938 = CARTESIAN_POINT('Ctrl Pts',(-20.6795490900832,-14.364108647694,
114.341931211457)) ;
#166939 = CARTESIAN_POINT('Ctrl Pts',(-20.6932450307031,-14.3021834028963,
114.383646838591)) ;
#166940 = CARTESIAN_POINT('Ctrl Pts',(-20.6374385512725,-14.1010124276425,
114.178000289426)) ;
#166941 = CARTESIAN_POINT('Ctrl Pts',(-20.6557888301489,-14.0530410261757,
114.233892280025)) ;
#166942 = CARTESIAN_POINT('Ctrl Pts',(-20.7295926537291,-14.0530409478965,
114.209661177911)) ;
#166943 = CARTESIAN_POINT('Ctrl Pts',(-20.8033964773092,-14.0530408696173,
114.185430075796)) ;
#166944 = CARTESIAN_POINT('Ctrl Pts',(-20.7850461984329,-14.101012271084,
114.129538085197)) ;
#166945 = CARTESIAN_POINT('Ctrl Pts',(-20.7666959195565,-14.1489836725507,
114.073646094597)) ;
#166946 = CARTESIAN_POINT('Ctrl Pts',(-20.6928920959764,-14.14898375083,114.097877196711)) ;
#166947 = CARTESIAN_POINT('Ctrl Pts',(-20.6190882723962,-14.1489838291092,
114.122108298826)) ;
#166948 = CARTESIAN_POINT('Ctrl Pts',(-20.6374385512725,-14.1010124276425,
114.178000289426)) ;
#166949 = CARTESIAN_POINT('Ctrl Pts',(-20.6010815469782,-13.8533300885713,
114.031993487533)) ;
#166950 = CARTESIAN_POINT('Ctrl Pts',(-20.622726691192,-13.822581157602,114.097921106379)) ;
#166951 = CARTESIAN_POINT('Ctrl Pts',(-20.696530521615,-13.8225810627118,
114.073690025107)) ;
#166952 = CARTESIAN_POINT('Ctrl Pts',(-20.770334352038,-13.8225809678216,
114.049458943834)) ;
#166953 = CARTESIAN_POINT('Ctrl Pts',(-20.7486892078241,-13.8533298987908,
113.983531324988)) ;
#166954 = CARTESIAN_POINT('Ctrl Pts',(-20.7270440636103,-13.8840788297601,
113.917603706141)) ;
#166955 = CARTESIAN_POINT('Ctrl Pts',(-20.6532402331873,-13.8840789246503,
113.941834787413)) ;
#166956 = CARTESIAN_POINT('Ctrl Pts',(-20.5794364027644,-13.8840790195405,
113.966065868686)) ;
#166957 = CARTESIAN_POINT('Ctrl Pts',(-20.6010815469782,-13.8533300885713,
114.031993487533)) ;
#166958 = CARTESIAN_POINT('Ctrl Pts',(-20.586642419132,-13.5731370136184,
113.952522413713)) ;
#166959 = CARTESIAN_POINT('Ctrl Pts',(-20.6100618395561,-13.5619047330003,
114.023854191675)) ;
#166960 = CARTESIAN_POINT('Ctrl Pts',(-20.6838656781738,-13.5619046275825,
113.999623135362)) ;
#166961 = CARTESIAN_POINT('Ctrl Pts',(-20.7576695167915,-13.5619045221647,
113.975392079049)) ;
#166962 = CARTESIAN_POINT('Ctrl Pts',(-20.7342500963673,-13.5731368027828,
113.904060301088)) ;
#166963 = CARTESIAN_POINT('Ctrl Pts',(-20.7108306759432,-13.5843690834008,
113.832728523127)) ;
#166964 = CARTESIAN_POINT('Ctrl Pts',(-20.6370268373256,-13.5843691888186,
113.856959579439)) ;
#166965 = CARTESIAN_POINT('Ctrl Pts',(-20.5632229987079,-13.5843692942365,
113.881190635752)) ;
#166966 = CARTESIAN_POINT('Ctrl Pts',(-20.586642419132,-13.5731370136184,
113.952522413713)) ;
#166967 = CARTESIAN_POINT('Ctrl Pts',(-20.5964562900944,-13.2811248351023,
113.946846374768)) ;
#166968 = CARTESIAN_POINT('Ctrl Pts',(-20.6199611334795,-13.2902630338005,
114.018438337316)) ;
#166969 = CARTESIAN_POINT('Ctrl Pts',(-20.6937649811193,-13.2902629265376,
113.994207308483)) ;
#166970 = CARTESIAN_POINT('Ctrl Pts',(-20.767568828759,-13.2902628192747,
113.969976279651)) ;
#166971 = CARTESIAN_POINT('Ctrl Pts',(-20.7440639853739,-13.2811246205765,
113.898384317102)) ;
#166972 = CARTESIAN_POINT('Ctrl Pts',(-20.7205591419887,-13.2719864218783,
113.826792354554)) ;
#166973 = CARTESIAN_POINT('Ctrl Pts',(-20.646755294349,-13.2719865291412,
113.851023383387)) ;
#166974 = CARTESIAN_POINT('Ctrl Pts',(-20.5729514467092,-13.2719866364041,
113.87525441222)) ;
#166975 = CARTESIAN_POINT('Ctrl Pts',(-20.5964562900944,-13.2811248351023,
113.946846374768)) ;
#166976 = CARTESIAN_POINT('Ctrl Pts',(-20.6302134446159,-13.0003515927813,
114.014286748923)) ;
#166977 = CARTESIAN_POINT('Ctrl Pts',(-20.6521282105241,-13.0291058472193,
114.081035592042)) ;
#166978 = CARTESIAN_POINT('Ctrl Pts',(-20.7259320669489,-13.029105747077,
114.056804589967)) ;
#166979 = CARTESIAN_POINT('Ctrl Pts',(-20.7997359233737,-13.0291056469348,
114.032573587892)) ;
#166980 = CARTESIAN_POINT('Ctrl Pts',(-20.7778211574655,-13.0003513924967,
113.965824744773)) ;
#166981 = CARTESIAN_POINT('Ctrl Pts',(-20.7559063915572,-12.9715971380587,
113.899075901654)) ;
#166982 = CARTESIAN_POINT('Ctrl Pts',(-20.6821025351324,-12.971597238201,
113.923306903729)) ;
#166983 = CARTESIAN_POINT('Ctrl Pts',(-20.6082986787076,-12.9715973383433,
113.947537905805)) ;
#166984 = CARTESIAN_POINT('Ctrl Pts',(-20.6302134446159,-13.0003515927813,
114.014286748923)) ;
#166985 = CARTESIAN_POINT('Ctrl Pts',(-20.6868771702669,-12.7476820967297,
114.151219214788)) ;
#166986 = CARTESIAN_POINT('Ctrl Pts',(-20.705606395181,-12.7941196142379,
114.208265414002)) ;
#166987 = CARTESIAN_POINT('Ctrl Pts',(-20.7794102592639,-12.794119529764,
114.184034435252)) ;
#166988 = CARTESIAN_POINT('Ctrl Pts',(-20.8532141233468,-12.7941194452901,
114.159803456503)) ;
#166989 = CARTESIAN_POINT('Ctrl Pts',(-20.8344848984328,-12.7476819277819,
114.102757257289)) ;
#166990 = CARTESIAN_POINT('Ctrl Pts',(-20.8157556735187,-12.7012444102737,
114.045711058075)) ;
#166991 = CARTESIAN_POINT('Ctrl Pts',(-20.7419518094358,-12.7012444947476,
114.069942036824)) ;
#166992 = CARTESIAN_POINT('Ctrl Pts',(-20.6681479453528,-12.7012445792215,
114.094173015574)) ;
#166993 = CARTESIAN_POINT('Ctrl Pts',(-20.6868771702669,-12.7476820967297,
114.151219214788)) ;
#166994 = CARTESIAN_POINT('Ctrl Pts',(-20.7618646026425,-12.5456564605608,
114.344400176223)) ;
#166995 = CARTESIAN_POINT('Ctrl Pts',(-20.7761148264351,-12.6062676271749,
114.387804060677)) ;
#166996 = CARTESIAN_POINT('Ctrl Pts',(-20.8499186963736,-12.6062675641062,
114.363573099762)) ;
#166997 = CARTESIAN_POINT('Ctrl Pts',(-20.9237225663121,-12.6062675010375,
114.339342138848)) ;
#166998 = CARTESIAN_POINT('Ctrl Pts',(-20.9094723425195,-12.5456563344234,
114.295938254394)) ;
#166999 = CARTESIAN_POINT('Ctrl Pts',(-20.8952221187268,-12.4850451678094,
114.25253436994)) ;
#167000 = CARTESIAN_POINT('Ctrl Pts',(-20.8214182487883,-12.4850452308781,
114.276765330855)) ;
#167001 = CARTESIAN_POINT('Ctrl Pts',(-20.7476143788498,-12.4850452939468,
114.300996291769)) ;
#167002 = CARTESIAN_POINT('Ctrl Pts',(-20.7618646026425,-12.5456564605608,
114.344400176223)) ;
#167003 = CARTESIAN_POINT('Ctrl Pts',(-20.851984110481,-12.4041536111177,
114.583349964643)) ;
#167004 = CARTESIAN_POINT('Ctrl Pts',(-20.8606991958322,-12.4747346832578,
114.609894710435)) ;
#167005 = CARTESIAN_POINT('Ctrl Pts',(-20.9345030691503,-12.474734646304,
114.585663759814)) ;
#167006 = CARTESIAN_POINT('Ctrl Pts',(-21.0083069424685,-12.4747346093502,
114.561432809193)) ;
#167007 = CARTESIAN_POINT('Ctrl Pts',(-20.9995918571173,-12.4041535372102,
114.534888063401)) ;
#167008 = CARTESIAN_POINT('Ctrl Pts',(-20.9908767717661,-12.3335724650701,
114.50834331761)) ;
#167009 = CARTESIAN_POINT('Ctrl Pts',(-20.917072898448,-12.3335725020239,
114.532574268231)) ;
#167010 = CARTESIAN_POINT('Ctrl Pts',(-20.8432690251298,-12.3335725389777,
114.556805218851)) ;
#167011 = CARTESIAN_POINT('Ctrl Pts',(-20.851984110481,-12.4041536111177,
114.583349964643)) ;
#167012 = CARTESIAN_POINT('Ctrl Pts',(-20.950708796806,-12.3358248594298,
114.848615416432)) ;
#167013 = CARTESIAN_POINT('Ctrl Pts',(-20.9532774121855,-12.4112821257934,
114.856439006343)) ;
#167014 = CARTESIAN_POINT('Ctrl Pts',(-21.0270812862604,-12.4112821160611,
114.832208058027)) ;
#167015 = CARTESIAN_POINT('Ctrl Pts',(-21.1008851603352,-12.4112821063287,
114.807977109711)) ;
#167016 = CARTESIAN_POINT('Ctrl Pts',(-21.0983165449557,-12.3358248399652,
114.8001535198)) ;
#167017 = CARTESIAN_POINT('Ctrl Pts',(-21.0957479295762,-12.2603675736016,
114.79232992989)) ;
#167018 = CARTESIAN_POINT('Ctrl Pts',(-21.0219440555014,-12.2603675833339,
114.816560878206)) ;
#167019 = CARTESIAN_POINT('Ctrl Pts',(-20.9481401814265,-12.2603675930662,
114.840791826522)) ;
#167020 = CARTESIAN_POINT('Ctrl Pts',(-20.950708796806,-12.3358248594298,
114.848615416432)) ;
#167021 = CARTESIAN_POINT('Ctrl Pts',(-21.0521870092213,-12.3448661715,115.122173404757)) ;
#167022 = CARTESIAN_POINT('Ctrl Pts',(-21.0484096856945,-12.4198057290159,
115.110668288568)) ;
#167023 = CARTESIAN_POINT('Ctrl Pts',(-21.1222135578069,-12.41980574501,115.086437334275)) ;
#167024 = CARTESIAN_POINT('Ctrl Pts',(-21.1960174299193,-12.4198057610042,
115.062206379981)) ;
#167025 = CARTESIAN_POINT('Ctrl Pts',(-21.1997947534461,-12.3448662034884,
115.07371149617)) ;
#167026 = CARTESIAN_POINT('Ctrl Pts',(-21.2035720769729,-12.2699266459725,
115.085216612359)) ;
#167027 = CARTESIAN_POINT('Ctrl Pts',(-21.1297682048605,-12.2699266299783,
115.109447566652)) ;
#167028 = CARTESIAN_POINT('Ctrl Pts',(-21.055964332748,-12.2699266139842,
115.133678520945)) ;
#167029 = CARTESIAN_POINT('Ctrl Pts',(-21.0521870092213,-12.3448661715,115.122173404757)) ;
#167030 = CARTESIAN_POINT('Ctrl Pts',(-21.1496243276175,-12.4312374679016,
115.383425842735)) ;
#167031 = CARTESIAN_POINT('Ctrl Pts',(-21.1397735006215,-12.5002598101882,
115.353421814809)) ;
#167032 = CARTESIAN_POINT('Ctrl Pts',(-21.213577368531,-12.5002598472916,
115.329190847715)) ;
#167033 = CARTESIAN_POINT('Ctrl Pts',(-21.2873812364404,-12.5002598843951,
115.30495988062)) ;
#167034 = CARTESIAN_POINT('Ctrl Pts',(-21.2972320634364,-12.4312375421085,
115.334963908546)) ;
#167035 = CARTESIAN_POINT('Ctrl Pts',(-21.3070828904324,-12.3622151998219,
115.364967936471)) ;
#167036 = CARTESIAN_POINT('Ctrl Pts',(-21.2332790225229,-12.3622151627184,
115.389198903566)) ;
#167037 = CARTESIAN_POINT('Ctrl Pts',(-21.1594751546135,-12.362215125615,
115.413429870661)) ;
#167038 = CARTESIAN_POINT('Ctrl Pts',(-21.1496243276175,-12.4312374679016,
115.383425842735)) ;
#167039 = CARTESIAN_POINT('Ctrl Pts',(-21.2363589987988,-12.5874506151636,
115.612268295527)) ;
#167040 = CARTESIAN_POINT('Ctrl Pts',(-21.2211688298052,-12.6456701044934,
115.566001493264)) ;
#167041 = CARTESIAN_POINT('Ctrl Pts',(-21.2949726923912,-12.6456701572597,
115.541770509954)) ;
#167042 = CARTESIAN_POINT('Ctrl Pts',(-21.3687765549771,-12.6456702100259,
115.517539526645)) ;
#167043 = CARTESIAN_POINT('Ctrl Pts',(-21.3839667239706,-12.5874507206961,
115.563806328909)) ;
#167044 = CARTESIAN_POINT('Ctrl Pts',(-21.3991568929642,-12.5292312313663,
115.610073131172)) ;
#167045 = CARTESIAN_POINT('Ctrl Pts',(-21.3253530303783,-12.5292311786001,
115.634304114482)) ;
#167046 = CARTESIAN_POINT('Ctrl Pts',(-21.2515491677923,-12.5292311258338,
115.658535097791)) ;
#167047 = CARTESIAN_POINT('Ctrl Pts',(-21.2363589987988,-12.5874506151636,
115.612268295527)) ;
#167048 = CARTESIAN_POINT('Ctrl Pts',(-21.3077549923188,-12.8034012905554,
115.794275144926)) ;
#167049 = CARTESIAN_POINT('Ctrl Pts',(-21.2882906825649,-12.8466312900345,
115.734989999395)) ;
#167050 = CARTESIAN_POINT('Ctrl Pts',(-21.3620945387581,-12.8466313512928,
115.710758996614)) ;
#167051 = CARTESIAN_POINT('Ctrl Pts',(-21.4358983949512,-12.8466314125512,
115.686527993833)) ;
#167052 = CARTESIAN_POINT('Ctrl Pts',(-21.455362704705,-12.8034014130721,
115.745813139364)) ;
#167053 = CARTESIAN_POINT('Ctrl Pts',(-21.4748270144589,-12.760171413593,
115.805098284895)) ;
#167054 = CARTESIAN_POINT('Ctrl Pts',(-21.4010231582657,-12.7601713523347,
115.829329287676)) ;
#167055 = CARTESIAN_POINT('Ctrl Pts',(-21.3272193020726,-12.7601712910763,
115.853560290457)) ;
#167056 = CARTESIAN_POINT('Ctrl Pts',(-21.3077549923188,-12.8034012905554,
115.794275144926)) ;
#167057 = CARTESIAN_POINT('Ctrl Pts',(-21.3591929501021,-13.0643708673509,
115.91537665745)) ;
#167058 = CARTESIAN_POINT('Ctrl Pts',(-21.336843717119,-13.0894456413712,
115.847304501069)) ;
#167059 = CARTESIAN_POINT('Ctrl Pts',(-21.4106475668522,-13.0894457028003,
115.823073478613)) ;
#167060 = CARTESIAN_POINT('Ctrl Pts',(-21.4844514165855,-13.0894457642295,
115.798842456156)) ;
#167061 = CARTESIAN_POINT('Ctrl Pts',(-21.5068006495686,-13.0643709902092,
115.866914612537)) ;
#167062 = CARTESIAN_POINT('Ctrl Pts',(-21.5291498825516,-13.0392962161889,
115.934986768918)) ;
#167063 = CARTESIAN_POINT('Ctrl Pts',(-21.4553460328184,-13.0392961547597,
115.959217791375)) ;
#167064 = CARTESIAN_POINT('Ctrl Pts',(-21.3815421830851,-13.0392960933306,
115.983448813831)) ;
#167065 = CARTESIAN_POINT('Ctrl Pts',(-21.3591929501021,-13.0643708673509,
115.91537665745)) ;
#167066 = CARTESIAN_POINT('Ctrl Pts',(-21.3874706338776,-13.3499213722247,
115.966045844109)) ;
#167067 = CARTESIAN_POINT('Ctrl Pts',(-21.3638469150851,-13.355096833582,
115.894091809427)) ;
#167068 = CARTESIAN_POINT('Ctrl Pts',(-21.4376507593288,-13.3550968897529,
115.869860770251)) ;
#167069 = CARTESIAN_POINT('Ctrl Pts',(-21.5114546035725,-13.3550969459238,
115.845629731074)) ;
#167070 = CARTESIAN_POINT('Ctrl Pts',(-21.5350783223649,-13.3499214845666,
115.917583765755)) ;
#167071 = CARTESIAN_POINT('Ctrl Pts',(-21.5587020411574,-13.3447460232093,
115.989537800437)) ;
#167072 = CARTESIAN_POINT('Ctrl Pts',(-21.4848981969137,-13.3447459670383,
116.013768839614)) ;
#167073 = CARTESIAN_POINT('Ctrl Pts',(-21.41109435267,-13.3447459108674,116.037999878791)) ;
#167074 = CARTESIAN_POINT('Ctrl Pts',(-21.3874706338776,-13.3499213722247,
115.966045844109)) ;
#167075 = CARTESIAN_POINT('Ctrl Pts',(-21.391441344453,-13.6410985525755,
115.942581213302)) ;
#167076 = CARTESIAN_POINT('Ctrl Pts',(-21.3682402719706,-13.6259514029626,
115.8719144909)) ;
#167077 = CARTESIAN_POINT('Ctrl Pts',(-21.4420441121637,-13.625951448446,
115.847683439386)) ;
#167078 = CARTESIAN_POINT('Ctrl Pts',(-21.5158479523567,-13.6259514939294,
115.823452387871)) ;
#167079 = CARTESIAN_POINT('Ctrl Pts',(-21.5390490248392,-13.6410986435423,
115.894119110273)) ;
#167080 = CARTESIAN_POINT('Ctrl Pts',(-21.5622500973216,-13.6562457931553,
115.964785832674)) ;
#167081 = CARTESIAN_POINT('Ctrl Pts',(-21.4884462571285,-13.6562457476719,
115.989016884188)) ;
#167082 = CARTESIAN_POINT('Ctrl Pts',(-21.4146424169355,-13.6562457021885,
116.013247935703)) ;
#167083 = CARTESIAN_POINT('Ctrl Pts',(-21.391441344453,-13.6410985525755,
115.942581213302)) ;
#167084 = CARTESIAN_POINT('Ctrl Pts',(-21.3717120179043,-13.9144130152127,
115.847175451564)) ;
#167085 = CARTESIAN_POINT('Ctrl Pts',(-21.3505841798155,-13.8801596021724,
115.782823466471)) ;
#167086 = CARTESIAN_POINT('Ctrl Pts',(-21.4243880174265,-13.8801596369213,
115.758592407092)) ;
#167087 = CARTESIAN_POINT('Ctrl Pts',(-21.4981918550375,-13.8801596716703,
115.734361347713)) ;
#167088 = CARTESIAN_POINT('Ctrl Pts',(-21.5193196931263,-13.9144130847105,
115.798713332805)) ;
#167089 = CARTESIAN_POINT('Ctrl Pts',(-21.5404475312151,-13.9486664977508,
115.863065317898)) ;
#167090 = CARTESIAN_POINT('Ctrl Pts',(-21.4666436936041,-13.9486664630018,
115.887296377277)) ;
#167091 = CARTESIAN_POINT('Ctrl Pts',(-21.3928398559931,-13.9486664282529,
115.911527436656)) ;
#167092 = CARTESIAN_POINT('Ctrl Pts',(-21.3717120179043,-13.9144130152127,
115.847175451564)) ;
#167093 = CARTESIAN_POINT('Ctrl Pts',(-21.3303616828838,-14.1534993419982,
115.685759559863)) ;
#167094 = CARTESIAN_POINT('Ctrl Pts',(-21.3128229753048,-14.1025003039047,
115.632339487033)) ;
#167095 = CARTESIAN_POINT('Ctrl Pts',(-21.3866268120323,-14.1025003260636,
115.608108424963)) ;
#167096 = CARTESIAN_POINT('Ctrl Pts',(-21.4604306487598,-14.1025003482225,
115.583877362893)) ;
#167097 = CARTESIAN_POINT('Ctrl Pts',(-21.4779693563387,-14.153499386316,
115.637297435723)) ;
#167098 = CARTESIAN_POINT('Ctrl Pts',(-21.4955080639176,-14.2044984244094,
115.690717508553)) ;
#167099 = CARTESIAN_POINT('Ctrl Pts',(-21.4217042271901,-14.2044984022505,
115.714948570623)) ;
#167100 = CARTESIAN_POINT('Ctrl Pts',(-21.3479003904626,-14.2044983800916,
115.739179632693)) ;
#167101 = CARTESIAN_POINT('Ctrl Pts',(-21.3303616828838,-14.1534993419982,
115.685759559863)) ;
#167102 = CARTESIAN_POINT('Ctrl Pts',(-21.2710083107908,-14.3398532357648,
115.469490040302)) ;
#167103 = CARTESIAN_POINT('Ctrl Pts',(-21.2583217051769,-14.2757649069183,
115.430848687012)) ;
#167104 = CARTESIAN_POINT('Ctrl Pts',(-21.3321255425352,-14.275764918267,
115.406617626863)) ;
#167105 = CARTESIAN_POINT('Ctrl Pts',(-21.4059293798935,-14.2757649296157,
115.382386566715)) ;
#167106 = CARTESIAN_POINT('Ctrl Pts',(-21.4186159855074,-14.3398532584622,
115.421027920004)) ;
#167107 = CARTESIAN_POINT('Ctrl Pts',(-21.4313025911213,-14.4039415873087,
115.459669273294)) ;
#167108 = CARTESIAN_POINT('Ctrl Pts',(-21.357498753763,-14.4039415759601,
115.483900333442)) ;
#167109 = CARTESIAN_POINT('Ctrl Pts',(-21.2836949164047,-14.4039415646114,
115.508131393591)) ;
#167110 = CARTESIAN_POINT('Ctrl Pts',(-21.2710083107908,-14.3398532357648,
115.469490040302)) ;
#167111 = CARTESIAN_POINT('Ctrl Pts',(-21.1988659886176,-14.4601239905911,
115.214323564159)) ;
#167112 = CARTESIAN_POINT('Ctrl Pts',(-21.1919307384879,-14.3875409587586,
115.193199911556)) ;
#167113 = CARTESIAN_POINT('Ctrl Pts',(-21.2657345773112,-14.3875409624437,
115.168968855869)) ;
#167114 = CARTESIAN_POINT('Ctrl Pts',(-21.3395384161345,-14.3875409661288,
115.144737800182)) ;
#167115 = CARTESIAN_POINT('Ctrl Pts',(-21.3464736662642,-14.4601239979614,
115.165861452786)) ;
#167116 = CARTESIAN_POINT('Ctrl Pts',(-21.3534089163939,-14.532707029794,
115.18698510539)) ;
#167117 = CARTESIAN_POINT('Ctrl Pts',(-21.2796050775706,-14.5327070261088,
115.211216161076)) ;
#167118 = CARTESIAN_POINT('Ctrl Pts',(-21.2058012387473,-14.5327070224237,
115.235447216763)) ;
#167119 = CARTESIAN_POINT('Ctrl Pts',(-21.1988659886176,-14.4601239905911,
115.214323564159)) ;
#167120 = CARTESIAN_POINT('Ctrl Pts',(-21.1193730346472,-14.5056532387337,
114.936603812244)) ;
#167121 = CARTESIAN_POINT('Ctrl Pts',(-21.1187146887639,-14.4297812015044,
114.934598597057)) ;
#167122 = CARTESIAN_POINT('Ctrl Pts',(-21.1925185297582,-14.4297812011716,
114.910367547982)) ;
#167123 = CARTESIAN_POINT('Ctrl Pts',(-21.2663223707524,-14.4297812008388,
114.886136498908)) ;
#167124 = CARTESIAN_POINT('Ctrl Pts',(-21.2669807166357,-14.5056532380682,
114.888141714096)) ;
#167125 = CARTESIAN_POINT('Ctrl Pts',(-21.2676390625191,-14.5815252752975,
114.890146929283)) ;
#167126 = CARTESIAN_POINT('Ctrl Pts',(-21.1938352215248,-14.5815252756303,
114.914377978358)) ;
#167127 = CARTESIAN_POINT('Ctrl Pts',(-21.1200313805306,-14.5815252759631,
114.938609027432)) ;
#167128 = CARTESIAN_POINT('Ctrl Pts',(-21.1193730346472,-14.5056532387337,
114.936603812244)) ;
#167129 = CARTESIAN_POINT('Ctrl Pts',(-21.0400856818068,-14.4736304498916,
114.659861410865)) ;
#167130 = CARTESIAN_POINT('Ctrl Pts',(-21.045691958151,-14.3998809483868,
114.676937224108)) ;
#167131 = CARTESIAN_POINT('Ctrl Pts',(-21.1194958005253,-14.3998809471274,
114.652706179238)) ;
#167132 = CARTESIAN_POINT('Ctrl Pts',(-21.1932996428997,-14.399880945868,
114.628475134367)) ;
#167133 = CARTESIAN_POINT('Ctrl Pts',(-21.1876933665555,-14.4736304473727,
114.611399321123)) ;
#167134 = CARTESIAN_POINT('Ctrl Pts',(-21.1820870902113,-14.5473799488775,
114.59432350788)) ;
#167135 = CARTESIAN_POINT('Ctrl Pts',(-21.108283247837,-14.5473799501369,
114.61855455275)) ;
#167136 = CARTESIAN_POINT('Ctrl Pts',(-21.0344794054626,-14.5473799513963,
114.642785597621)) ;
#167137 = CARTESIAN_POINT('Ctrl Pts',(-21.0400856818068,-14.4736304498916,
114.659861410865)) ;
#167138 = CARTESIAN_POINT('Ctrl Pts',(-20.9656884076386,-14.3649486844788,
114.397529024825)) ;
#167139 = CARTESIAN_POINT('Ctrl Pts',(-20.9772377464687,-14.2986771390851,
114.432706447392)) ;
#167140 = CARTESIAN_POINT('Ctrl Pts',(-21.0510415903523,-14.2986771395707,
114.408475407118)) ;
#167141 = CARTESIAN_POINT('Ctrl Pts',(-21.1248454342359,-14.2986771400562,
114.384244366844)) ;
#167142 = CARTESIAN_POINT('Ctrl Pts',(-21.1132960954058,-14.36494868545,114.349066944277)) ;
#167143 = CARTESIAN_POINT('Ctrl Pts',(-21.1017467565757,-14.4312202308437,
114.31388952171)) ;
#167144 = CARTESIAN_POINT('Ctrl Pts',(-21.0279429126921,-14.4312202303581,
114.338120561984)) ;
#167145 = CARTESIAN_POINT('Ctrl Pts',(-20.9541390688086,-14.4312202298725,
114.362351602257)) ;
#167146 = CARTESIAN_POINT('Ctrl Pts',(-20.9656884076386,-14.3649486844788,
114.397529024825)) ;
#167147 = CARTESIAN_POINT('Ctrl Pts',(-20.9040908794189,-14.1895250687342,
114.174588389894)) ;
#167148 = CARTESIAN_POINT('Ctrl Pts',(-20.9206896003898,-14.1354046364552,
114.225145415719)) ;
#167149 = CARTESIAN_POINT('Ctrl Pts',(-20.9944934444827,-14.1354046385753,
114.200914376082)) ;
#167150 = CARTESIAN_POINT('Ctrl Pts',(-21.0682972885756,-14.1354046406955,
114.176683336446)) ;
#167151 = CARTESIAN_POINT('Ctrl Pts',(-21.0516985676048,-14.1895250729745,
114.126126310621)) ;
#167152 = CARTESIAN_POINT('Ctrl Pts',(-21.0350998466339,-14.2436455052536,
114.075569284796)) ;
#167153 = CARTESIAN_POINT('Ctrl Pts',(-20.9612960025409,-14.2436455031334,
114.099800324432)) ;
#167154 = CARTESIAN_POINT('Ctrl Pts',(-20.887492158448,-14.2436455010133,
114.124031364069)) ;
#167155 = CARTESIAN_POINT('Ctrl Pts',(-20.9040908794189,-14.1895250687342,
114.174588389894)) ;
#167156 = CARTESIAN_POINT('Ctrl Pts',(-20.8593435984038,-13.9587919846541,
114.002862848148)) ;
#167157 = CARTESIAN_POINT('Ctrl Pts',(-20.8798248430018,-13.9207033555361,
114.065245414496)) ;
#167158 = CARTESIAN_POINT('Ctrl Pts',(-20.9536286868818,-13.9207033583064,
114.041014374211)) ;
#167159 = CARTESIAN_POINT('Ctrl Pts',(-21.0274325307618,-13.9207033610767,
114.016783333927)) ;
#167160 = CARTESIAN_POINT('Ctrl Pts',(-21.0069512861638,-13.9587919901947,
113.954400767579)) ;
#167161 = CARTESIAN_POINT('Ctrl Pts',(-20.9864700415659,-13.9968806193127,
113.892018201231)) ;
#167162 = CARTESIAN_POINT('Ctrl Pts',(-20.9126661976859,-13.9968806165424,
113.916249241516)) ;
#167163 = CARTESIAN_POINT('Ctrl Pts',(-20.8388623538059,-13.9968806137721,
113.940480281801)) ;
#167164 = CARTESIAN_POINT('Ctrl Pts',(-20.8593435984038,-13.9587919846541,
114.002862848148)) ;
#167165 = CARTESIAN_POINT('Ctrl Pts',(-20.8356369939423,-13.6889251841896,
113.895181640807)) ;
#167166 = CARTESIAN_POINT('Ctrl Pts',(-20.858537937481,-13.6696247434328,
113.964934219753)) ;
#167167 = CARTESIAN_POINT('Ctrl Pts',(-20.9323417808698,-13.6696247444935,
113.940703177972)) ;
#167168 = CARTESIAN_POINT('Ctrl Pts',(-21.0061456242587,-13.6696247455542,
113.916472136191)) ;
#167169 = CARTESIAN_POINT('Ctrl Pts',(-20.9832446807201,-13.688925186311,
113.846719557246)) ;
#167170 = CARTESIAN_POINT('Ctrl Pts',(-20.9603437371814,-13.7082256270677,
113.7769669783)) ;
#167171 = CARTESIAN_POINT('Ctrl Pts',(-20.8865398937926,-13.708225626007,
113.801198020081)) ;
#167172 = CARTESIAN_POINT('Ctrl Pts',(-20.8127360504037,-13.7082256249463,
113.825429061862)) ;
#167173 = CARTESIAN_POINT('Ctrl Pts',(-20.8356369939423,-13.6889251841896,
113.895181640807)) ;
#167174 = CARTESIAN_POINT('Ctrl Pts',(-20.8355656879003,-13.3992086458092,
113.859432886615)) ;
#167175 = CARTESIAN_POINT('Ctrl Pts',(-20.8592405174172,-13.4001099249718,
113.931542597469)) ;
#167176 = CARTESIAN_POINT('Ctrl Pts',(-20.9330443607297,-13.4001099216027,
113.907311555456)) ;
#167177 = CARTESIAN_POINT('Ctrl Pts',(-21.0068482040421,-13.4001099182335,
113.883080513442)) ;
#167178 = CARTESIAN_POINT('Ctrl Pts',(-20.9831733745252,-13.3992086390708,
113.810970802588)) ;
#167179 = CARTESIAN_POINT('Ctrl Pts',(-20.9594985450083,-13.3983073599082,
113.738861091734)) ;
#167180 = CARTESIAN_POINT('Ctrl Pts',(-20.8856947016959,-13.3983073632774,
113.763092133747)) ;
#167181 = CARTESIAN_POINT('Ctrl Pts',(-20.8118908583834,-13.3983073666465,
113.787323175761)) ;
#167182 = CARTESIAN_POINT('Ctrl Pts',(-20.8355656879003,-13.3992086458092,
113.859432886615)) ;
#167183 = CARTESIAN_POINT('Ctrl Pts',(-20.8596153977637,-13.1124266878776,
113.89736040102)) ;
#167184 = CARTESIAN_POINT('Ctrl Pts',(-20.8823763686297,-13.13335350732,113.966686645961)) ;
#167185 = CARTESIAN_POINT('Ctrl Pts',(-20.9561802125574,-13.1333534995856,
113.942455605822)) ;
#167186 = CARTESIAN_POINT('Ctrl Pts',(-21.029984056485,-13.1333534918511,
113.918224565682)) ;
#167187 = CARTESIAN_POINT('Ctrl Pts',(-21.007223085619,-13.1124266724087,
113.848898320741)) ;
#167188 = CARTESIAN_POINT('Ctrl Pts',(-20.984462114753,-13.0914998529662,
113.7795720758)) ;
#167189 = CARTESIAN_POINT('Ctrl Pts',(-20.9106582708253,-13.0914998607007,
113.803803115939)) ;
#167190 = CARTESIAN_POINT('Ctrl Pts',(-20.8368544268977,-13.0914998684351,
113.828034156079)) ;
#167191 = CARTESIAN_POINT('Ctrl Pts',(-20.8596153977637,-13.1124266878776,
113.89736040102)) ;
#167192 = CARTESIAN_POINT('Ctrl Pts',(-20.9073931832141,-12.8450096600115,
114.007218110877)) ;
#167193 = CARTESIAN_POINT('Ctrl Pts',(-20.9275894252847,-12.8846394195873,
114.068732605881)) ;
#167194 = CARTESIAN_POINT('Ctrl Pts',(-21.0013932711385,-12.8846394056337,
114.044501571608)) ;
#167195 = CARTESIAN_POINT('Ctrl Pts',(-21.0751971169922,-12.8846393916802,
114.020270537335)) ;
#167196 = CARTESIAN_POINT('Ctrl Pts',(-21.0550008749215,-12.8450096321044,
113.95875604233)) ;
#167197 = CARTESIAN_POINT('Ctrl Pts',(-21.0348046328509,-12.8053798725287,
113.897241547326)) ;
#167198 = CARTESIAN_POINT('Ctrl Pts',(-20.9610007869972,-12.8053798864822,
113.921472581599)) ;
#167199 = CARTESIAN_POINT('Ctrl Pts',(-20.8871969411434,-12.8053799004358,
113.945703615872)) ;
#167200 = CARTESIAN_POINT('Ctrl Pts',(-20.9073931832141,-12.8450096600115,
114.007218110877)) ;
#167201 = CARTESIAN_POINT('Ctrl Pts',(-20.9754422866959,-12.6209217910559,
114.179130249146)) ;
#167202 = CARTESIAN_POINT('Ctrl Pts',(-20.9916479840303,-12.6762550632743,
114.228490188886)) ;
#167203 = CARTESIAN_POINT('Ctrl Pts',(-21.0654518325001,-12.6762550473825,
114.204259162581)) ;
#167204 = CARTESIAN_POINT('Ctrl Pts',(-21.1392556809698,-12.6762550314906,
114.180028136276)) ;
#167205 = CARTESIAN_POINT('Ctrl Pts',(-21.1230499836355,-12.6209217592723,
114.130668196536)) ;
#167206 = CARTESIAN_POINT('Ctrl Pts',(-21.1068442863011,-12.5655884870539,
114.081308256797)) ;
#167207 = CARTESIAN_POINT('Ctrl Pts',(-21.0330404378314,-12.5655885029457,
114.105539283102)) ;
#167208 = CARTESIAN_POINT('Ctrl Pts',(-20.9592365893616,-12.5655885188375,
114.129770309407)) ;
#167209 = CARTESIAN_POINT('Ctrl Pts',(-20.9754422866959,-12.6209217910559,
114.179130249146)) ;
#167210 = CARTESIAN_POINT('Ctrl Pts',(-21.060116229982,-12.453038777336,114.401581870571)) ;
#167211 = CARTESIAN_POINT('Ctrl Pts',(-21.0711669360117,-12.520173907181,
114.435240538705)) ;
#167212 = CARTESIAN_POINT('Ctrl Pts',(-21.1449707877985,-12.5201738923226,
114.411009522503)) ;
#167213 = CARTESIAN_POINT('Ctrl Pts',(-21.2187746395854,-12.5201738774643,
114.386778506302)) ;
#167214 = CARTESIAN_POINT('Ctrl Pts',(-21.2077239335557,-12.4530387476193,
114.353119838167)) ;
#167215 = CARTESIAN_POINT('Ctrl Pts',(-21.196673227526,-12.3859036177743,
114.319461170032)) ;
#167216 = CARTESIAN_POINT('Ctrl Pts',(-21.1228693757392,-12.3859036326327,
114.343692186234)) ;
#167217 = CARTESIAN_POINT('Ctrl Pts',(-21.0490655239523,-12.385903647491,
114.367923202436)) ;
#167218 = CARTESIAN_POINT('Ctrl Pts',(-21.060116229982,-12.453038777336,114.401581870571)) ;
#167219 = CARTESIAN_POINT('Ctrl Pts',(-21.1561433073425,-12.3543368017594,
114.658578252509)) ;
#167220 = CARTESIAN_POINT('Ctrl Pts',(-21.1612396516993,-12.4284604690025,
114.67410089589)) ;
#167221 = CARTESIAN_POINT('Ctrl Pts',(-21.23504350709,-12.4284604600379,114.649869890665)) ;
#167222 = CARTESIAN_POINT('Ctrl Pts',(-21.3088473624807,-12.4284604510733,
114.62563888544)) ;
#167223 = CARTESIAN_POINT('Ctrl Pts',(-21.3037510181239,-12.3543367838302,
114.610116242059)) ;
#167224 = CARTESIAN_POINT('Ctrl Pts',(-21.2986546737672,-12.2802131165871,
114.594593598678)) ;
#167225 = CARTESIAN_POINT('Ctrl Pts',(-21.2248508183765,-12.2802131255517,
114.618824603903)) ;
#167226 = CARTESIAN_POINT('Ctrl Pts',(-21.1510469629858,-12.2802131345163,
114.643055609128)) ;
#167227 = CARTESIAN_POINT('Ctrl Pts',(-21.1561433073425,-12.3543368017594,
114.658578252509)) ;
#167228 = CARTESIAN_POINT('Ctrl Pts',(-21.2570400946613,-12.3316786589988,
114.930491348528)) ;
#167229 = CARTESIAN_POINT('Ctrl Pts',(-21.2558318008147,-12.4074912166658,
114.926811081348)) ;
#167230 = CARTESIAN_POINT('Ctrl Pts',(-21.3296356590554,-12.4074912185027,
114.902580084804)) ;
#167231 = CARTESIAN_POINT('Ctrl Pts',(-21.403439517296,-12.4074912203397,
114.878349088259)) ;
#167232 = CARTESIAN_POINT('Ctrl Pts',(-21.4046478111425,-12.3316786626727,
114.882029355439)) ;
#167233 = CARTESIAN_POINT('Ctrl Pts',(-21.4058561049891,-12.2558661050058,
114.885709622619)) ;
#167234 = CARTESIAN_POINT('Ctrl Pts',(-21.3320522467485,-12.2558661031688,
114.909940619164)) ;
#167235 = CARTESIAN_POINT('Ctrl Pts',(-21.2582483885079,-12.2558661013318,
114.934171615708)) ;
#167236 = CARTESIAN_POINT('Ctrl Pts',(-21.2570400946613,-12.3316786589988,
114.930491348528)) ;
#167237 = CARTESIAN_POINT('Ctrl Pts',(-21.3572503237435,-12.3873927929882,
115.200059905244)) ;
#167238 = CARTESIAN_POINT('Ctrl Pts',(-21.3497814966636,-12.4594256106333,
115.177311064172)) ;
#167239 = CARTESIAN_POINT('Ctrl Pts',(-21.4235853573106,-12.4594256285176,
115.153080074957)) ;
#167240 = CARTESIAN_POINT('Ctrl Pts',(-21.4973892179576,-12.4594256464019,
115.128849085742)) ;
#167241 = CARTESIAN_POINT('Ctrl Pts',(-21.5048580450376,-12.3873928287568,
115.151597926814)) ;
#167242 = CARTESIAN_POINT('Ctrl Pts',(-21.5123268721176,-12.3153600111117,
115.174346767886)) ;
#167243 = CARTESIAN_POINT('Ctrl Pts',(-21.4385230114705,-12.3153599932274,
115.198577757101)) ;
#167244 = CARTESIAN_POINT('Ctrl Pts',(-21.3647191508235,-12.3153599753431,
115.222808746316)) ;
#167245 = CARTESIAN_POINT('Ctrl Pts',(-21.3572503237435,-12.3873927929882,
115.200059905244)) ;
#167246 = CARTESIAN_POINT('Ctrl Pts',(-21.4488212057437,-12.5162741275779,
115.443632859608)) ;
#167247 = CARTESIAN_POINT('Ctrl Pts',(-21.4356795074852,-12.5794124829248,
115.40360536838)) ;
#167248 = CARTESIAN_POINT('Ctrl Pts',(-21.5094833678952,-12.5794125189228,
115.379374378443)) ;
#167249 = CARTESIAN_POINT('Ctrl Pts',(-21.5832872283053,-12.5794125549208,
115.355143388506)) ;
#167250 = CARTESIAN_POINT('Ctrl Pts',(-21.5964289265637,-12.5162741995739,
115.395170879734)) ;
#167251 = CARTESIAN_POINT('Ctrl Pts',(-21.6095706248222,-12.453135844227,
115.435198370962)) ;
#167252 = CARTESIAN_POINT('Ctrl Pts',(-21.5357667644122,-12.453135808229,
115.459429360899)) ;
#167253 = CARTESIAN_POINT('Ctrl Pts',(-21.4619629040021,-12.453135772231,
115.483660350836)) ;
#167254 = CARTESIAN_POINT('Ctrl Pts',(-21.4488212057437,-12.5162741275779,
115.443632859608)) ;
#167255 = CARTESIAN_POINT('Ctrl Pts',(-21.5273021746152,-12.7104566542012,
115.647127915526)) ;
#167256 = CARTESIAN_POINT('Ctrl Pts',(-21.5093975650024,-12.7601293026598,
115.592593364974)) ;
#167257 = CARTESIAN_POINT('Ctrl Pts',(-21.5832014235926,-12.7601293584612,
115.568362369495)) ;
#167258 = CARTESIAN_POINT('Ctrl Pts',(-21.6570052821828,-12.7601294142626,
115.544131374015)) ;
#167259 = CARTESIAN_POINT('Ctrl Pts',(-21.6749098917956,-12.7104567658041,
115.598665924566)) ;
#167260 = CARTESIAN_POINT('Ctrl Pts',(-21.6928145014084,-12.6607841173455,
115.653200475117)) ;
#167261 = CARTESIAN_POINT('Ctrl Pts',(-21.6190106428182,-12.6607840615441,
115.677431470597)) ;
#167262 = CARTESIAN_POINT('Ctrl Pts',(-21.5452067842279,-12.6607840057427,
115.701662466077)) ;
#167263 = CARTESIAN_POINT('Ctrl Pts',(-21.5273021746152,-12.7104566542012,
115.647127915526)) ;
#167264 = CARTESIAN_POINT('Ctrl Pts',(-21.5869697508136,-12.9544063196606,
115.793490670685)) ;
#167265 = CARTESIAN_POINT('Ctrl Pts',(-21.5656053858241,-12.9871189134417,
115.728418263615)) ;
#167266 = CARTESIAN_POINT('Ctrl Pts',(-21.6394092401113,-12.9871189862544,
115.704187255029)) ;
#167267 = CARTESIAN_POINT('Ctrl Pts',(-21.7132130943986,-12.987119059067,
115.679956246443)) ;
#167268 = CARTESIAN_POINT('Ctrl Pts',(-21.734577459388,-12.9544064652859,
115.745028653514)) ;
#167269 = CARTESIAN_POINT('Ctrl Pts',(-21.7559418243775,-12.9216938715048,
115.810101060584)) ;
#167270 = CARTESIAN_POINT('Ctrl Pts',(-21.6821379700903,-12.9216937986921,
115.83433206917)) ;
#167271 = CARTESIAN_POINT('Ctrl Pts',(-21.608334115803,-12.9216937258795,
115.858563077756)) ;
#167272 = CARTESIAN_POINT('Ctrl Pts',(-21.5869697508136,-12.9544063196606,
115.793490670685)) ;
#167273 = CARTESIAN_POINT('Ctrl Pts',(-21.6248241880919,-13.2316631461472,
115.873367978984)) ;
#167274 = CARTESIAN_POINT('Ctrl Pts',(-21.6015188760931,-13.2450660236381,
115.802383760619)) ;
#167275 = CARTESIAN_POINT('Ctrl Pts',(-21.6753227243222,-13.2450661094682,
115.778152733581)) ;
#167276 = CARTESIAN_POINT('Ctrl Pts',(-21.7491265725514,-13.2450661952983,
115.753921706544)) ;
#167277 = CARTESIAN_POINT('Ctrl Pts',(-21.7724318845503,-13.2316633178074,
115.824905924908)) ;
#167278 = CARTESIAN_POINT('Ctrl Pts',(-21.7957371965492,-13.2182604403165,
115.895890143273)) ;
#167279 = CARTESIAN_POINT('Ctrl Pts',(-21.72193334832,-13.2182603544864,115.920121170311)) ;
#167280 = CARTESIAN_POINT('Ctrl Pts',(-21.6481295000908,-13.2182602686563,
115.944352197349)) ;
#167281 = CARTESIAN_POINT('Ctrl Pts',(-21.6248241880919,-13.2316631461472,
115.873367978984)) ;
#167282 = CARTESIAN_POINT('Ctrl Pts',(-21.6387981022204,-13.5226486146427,
115.880466253006)) ;
#167283 = CARTESIAN_POINT('Ctrl Pts',(-21.6152170567332,-13.5157554602217,
115.808642195042)) ;
#167284 = CARTESIAN_POINT('Ctrl Pts',(-21.6890208974959,-13.5157555531286,
115.784411145263)) ;
#167285 = CARTESIAN_POINT('Ctrl Pts',(-21.7628247382586,-13.5157556460354,
115.760180095483)) ;
#167286 = CARTESIAN_POINT('Ctrl Pts',(-21.7864057837459,-13.5226488004565,
115.832004153447)) ;
#167287 = CARTESIAN_POINT('Ctrl Pts',(-21.8099868292331,-13.5295419548775,
115.903828211411)) ;
#167288 = CARTESIAN_POINT('Ctrl Pts',(-21.7361829884704,-13.5295418619706,
115.92805926119)) ;
#167289 = CARTESIAN_POINT('Ctrl Pts',(-21.6623791477077,-13.5295417690637,
115.952290310969)) ;
#167290 = CARTESIAN_POINT('Ctrl Pts',(-21.6387981022204,-13.5226486146427,
115.880466253006)) ;
#167291 = CARTESIAN_POINT('Ctrl Pts',(-21.6284861294477,-13.8069296281822,
115.813488458912)) ;
#167292 = CARTESIAN_POINT('Ctrl Pts',(-21.6063264693954,-13.7801790343967,
115.745993711753)) ;
#167293 = CARTESIAN_POINT('Ctrl Pts',(-21.6801303018853,-13.7801791269532,
115.721762636776)) ;
#167294 = CARTESIAN_POINT('Ctrl Pts',(-21.7539341343752,-13.7801792195097,
115.697531561799)) ;
#167295 = CARTESIAN_POINT('Ctrl Pts',(-21.7760937944275,-13.8069298132952,
115.765026308958)) ;
#167296 = CARTESIAN_POINT('Ctrl Pts',(-21.7982534544798,-13.8336804070807,
115.832521056117)) ;
#167297 = CARTESIAN_POINT('Ctrl Pts',(-21.7244496219899,-13.8336803145242,
115.856752131094)) ;
#167298 = CARTESIAN_POINT('Ctrl Pts',(-21.6506457895,-13.8336802219677,115.880983206071)) ;
#167299 = CARTESIAN_POINT('Ctrl Pts',(-21.6284861294477,-13.8069296281822,
115.813488458912)) ;
#167300 = CARTESIAN_POINT('Ctrl Pts',(-21.5954516704821,-14.0625497260425,
115.677400696328)) ;
#167301 = CARTESIAN_POINT('Ctrl Pts',(-21.5762998168345,-14.0179135569207,
115.619067242248)) ;
#167302 = CARTESIAN_POINT('Ctrl Pts',(-21.6501036412778,-14.017913640046,
115.594836142763)) ;
#167303 = CARTESIAN_POINT('Ctrl Pts',(-21.7239074657211,-14.0179137231712,
115.570605043277)) ;
#167304 = CARTESIAN_POINT('Ctrl Pts',(-21.7430593193686,-14.062549892293,
115.628938497357)) ;
#167305 = CARTESIAN_POINT('Ctrl Pts',(-21.7622111730162,-14.1071860614148,
115.687271951437)) ;
#167306 = CARTESIAN_POINT('Ctrl Pts',(-21.6884073485729,-14.1071859782896,
115.711503050923)) ;
#167307 = CARTESIAN_POINT('Ctrl Pts',(-21.6146035241296,-14.1071858951643,
115.735734150408)) ;
#167308 = CARTESIAN_POINT('Ctrl Pts',(-21.5954516704821,-14.0625497260425,
115.677400696328)) ;
#167309 = CARTESIAN_POINT('Ctrl Pts',(-21.5427818566883,-14.2720262448878,
115.481481169144)) ;
#167310 = CARTESIAN_POINT('Ctrl Pts',(-21.528013502307,-14.2126996245835,
115.436499146612)) ;
#167311 = CARTESIAN_POINT('Ctrl Pts',(-21.6018173198018,-14.2126996903488,
115.412268025962)) ;
#167312 = CARTESIAN_POINT('Ctrl Pts',(-21.6756211372967,-14.2126997561141,
115.388036905313)) ;
#167313 = CARTESIAN_POINT('Ctrl Pts',(-21.690389491678,-14.2720263764183,
115.433018927845)) ;
#167314 = CARTESIAN_POINT('Ctrl Pts',(-21.7051578460592,-14.3313529967226,
115.478000950378)) ;
#167315 = CARTESIAN_POINT('Ctrl Pts',(-21.6313540285644,-14.3313529309573,
115.502232071027)) ;
#167316 = CARTESIAN_POINT('Ctrl Pts',(-21.5575502110696,-14.331352865192,
115.526463191677)) ;
#167317 = CARTESIAN_POINT('Ctrl Pts',(-21.5427818566883,-14.2720262448878,
115.481481169144)) ;
#167318 = CARTESIAN_POINT('Ctrl Pts',(-21.4753425478091,-14.4199161330371,
115.240721116631)) ;
#167319 = CARTESIAN_POINT('Ctrl Pts',(-21.4659923355475,-14.3501772641186,
115.212241880814)) ;
#167320 = CARTESIAN_POINT('Ctrl Pts',(-21.5397961480427,-14.3501773061419,
115.188010744936)) ;
#167321 = CARTESIAN_POINT('Ctrl Pts',(-21.613599960538,-14.3501773481651,
115.163779609059)) ;
#167322 = CARTESIAN_POINT('Ctrl Pts',(-21.6229501727996,-14.4199162170836,
115.192258844876)) ;
#167323 = CARTESIAN_POINT('Ctrl Pts',(-21.6323003850611,-14.489655086002,
115.220738080693)) ;
#167324 = CARTESIAN_POINT('Ctrl Pts',(-21.5584965725659,-14.4896550439788,
115.244969216571)) ;
#167325 = CARTESIAN_POINT('Ctrl Pts',(-21.4846927600706,-14.4896550019555,
115.269200352448)) ;
#167326 = CARTESIAN_POINT('Ctrl Pts',(-21.4753425478091,-14.4199161330371,
115.240721116631)) ;
#167327 = CARTESIAN_POINT('Ctrl Pts',(-21.397953128425,-14.496610258064,114.969417382177)) ;
#167328 = CARTESIAN_POINT('Ctrl Pts',(-21.3947284182574,-14.4214134928077,
114.959595437408)) ;
#167329 = CARTESIAN_POINT('Ctrl Pts',(-21.4685322281319,-14.4214135069691,
114.935364293548)) ;
#167330 = CARTESIAN_POINT('Ctrl Pts',(-21.5423360380063,-14.4214135211306,
114.911133149688)) ;
#167331 = CARTESIAN_POINT('Ctrl Pts',(-21.5455607481739,-14.496610286387,
114.920955094457)) ;
#167332 = CARTESIAN_POINT('Ctrl Pts',(-21.5487854583414,-14.5718070516433,
114.930777039227)) ;
#167333 = CARTESIAN_POINT('Ctrl Pts',(-21.474981648467,-14.5718070374819,
114.955008183087)) ;
#167334 = CARTESIAN_POINT('Ctrl Pts',(-21.4011778385925,-14.5718070233204,
114.979239326947)) ;
#167335 = CARTESIAN_POINT('Ctrl Pts',(-21.397953128425,-14.496610258064,114.969417382177)) ;
#167336 = CARTESIAN_POINT('Ctrl Pts',(-21.3180584790138,-14.4958941579837,
114.690798167278)) ;
#167337 = CARTESIAN_POINT('Ctrl Pts',(-21.3211368828269,-14.4206364931476,
114.700174490684)) ;
#167338 = CARTESIAN_POINT('Ctrl Pts',(-21.3949406928266,-14.4206364783751,
114.675943347206)) ;
#167339 = CARTESIAN_POINT('Ctrl Pts',(-21.4687445028263,-14.4206364636026,
114.651712203727)) ;
#167340 = CARTESIAN_POINT('Ctrl Pts',(-21.4656660990133,-14.4958941284387,
114.642335880322)) ;
#167341 = CARTESIAN_POINT('Ctrl Pts',(-21.4625876952002,-14.5711517932748,
114.632959556916)) ;
#167342 = CARTESIAN_POINT('Ctrl Pts',(-21.3887838852004,-14.5711518080473,
114.657190700394)) ;
#167343 = CARTESIAN_POINT('Ctrl Pts',(-21.3149800752007,-14.5711518228198,
114.681421843873)) ;
#167344 = CARTESIAN_POINT('Ctrl Pts',(-21.3180584790138,-14.4958941579837,
114.690798167278)) ;
#167345 = CARTESIAN_POINT('Ctrl Pts',(-21.2408257912765,-14.4180076226564,
114.419996127992)) ;
#167346 = CARTESIAN_POINT('Ctrl Pts',(-21.2500367265787,-14.3480754910907,
114.448051152803)) ;
#167347 = CARTESIAN_POINT('Ctrl Pts',(-21.3238405394614,-14.3480754488814,
114.423820018105)) ;
#167348 = CARTESIAN_POINT('Ctrl Pts',(-21.3976443523441,-14.3480754066721,
114.399588883408)) ;
#167349 = CARTESIAN_POINT('Ctrl Pts',(-21.388433417042,-14.4180075382377,
114.371533858597)) ;
#167350 = CARTESIAN_POINT('Ctrl Pts',(-21.3792224817398,-14.4879396698034,
114.343478833786)) ;
#167351 = CARTESIAN_POINT('Ctrl Pts',(-21.3054186688571,-14.4879397120127,
114.367709968483)) ;
#167352 = CARTESIAN_POINT('Ctrl Pts',(-21.2316148559744,-14.4879397542221,
114.391941103181)) ;
#167353 = CARTESIAN_POINT('Ctrl Pts',(-21.2408257912765,-14.4180076226564,
114.419996127992)) ;
#167354 = CARTESIAN_POINT('Ctrl Pts',(-21.1734230549706,-14.2684543242656,
114.179245557719)) ;
#167355 = CARTESIAN_POINT('Ctrl Pts',(-21.1880871641883,-14.2088592298977,
114.22391007036)) ;
#167356 = CARTESIAN_POINT('Ctrl Pts',(-21.2618909823228,-14.2088591648377,
114.199678951658)) ;
#167357 = CARTESIAN_POINT('Ctrl Pts',(-21.3356948004572,-14.2088590997777,
114.175447832957)) ;
#167358 = CARTESIAN_POINT('Ctrl Pts',(-21.3210306912395,-14.2684541941456,
114.130783320317)) ;
#167359 = CARTESIAN_POINT('Ctrl Pts',(-21.3063665820217,-14.3280492885136,
114.086118807677)) ;
#167360 = CARTESIAN_POINT('Ctrl Pts',(-21.2325627638873,-14.3280493535736,
114.110349926378)) ;
#167361 = CARTESIAN_POINT('Ctrl Pts',(-21.1587589457529,-14.3280494186336,
114.134581045079)) ;
#167362 = CARTESIAN_POINT('Ctrl Pts',(-21.1734230549706,-14.2684543242656,
114.179245557719)) ;
#167363 = CARTESIAN_POINT('Ctrl Pts',(-21.1211403104816,-14.0580103363769,
113.984528831462)) ;
#167364 = CARTESIAN_POINT('Ctrl Pts',(-21.1402105735545,-14.0130186488343,
114.042613777743)) ;
#167365 = CARTESIAN_POINT('Ctrl Pts',(-21.214014398683,-14.0130185675702,
114.018382680344)) ;
#167366 = CARTESIAN_POINT('Ctrl Pts',(-21.2878182238116,-14.013018486306,
113.994151582946)) ;
#167367 = CARTESIAN_POINT('Ctrl Pts',(-21.2687479607386,-14.0580101738486,
113.936066636665)) ;
#167368 = CARTESIAN_POINT('Ctrl Pts',(-21.2496776976657,-14.1030018613912,
113.877981690384)) ;
#167369 = CARTESIAN_POINT('Ctrl Pts',(-21.1758738725372,-14.1030019426553,
113.902212787783)) ;
#167370 = CARTESIAN_POINT('Ctrl Pts',(-21.1020700474087,-14.1030020239195,
113.926443885181)) ;
#167371 = CARTESIAN_POINT('Ctrl Pts',(-21.1211403104816,-14.0580103363769,
113.984528831462)) ;
#167372 = CARTESIAN_POINT('Ctrl Pts',(-21.0885284661435,-13.8017355758307,
113.849734796424)) ;
#167373 = CARTESIAN_POINT('Ctrl Pts',(-21.1106380366097,-13.7745688567898,
113.917076982543)) ;
#167374 = CARTESIAN_POINT('Ctrl Pts',(-21.1844418696645,-13.7745687672832,
113.892845909287)) ;
#167375 = CARTESIAN_POINT('Ctrl Pts',(-21.2582457027194,-13.7745686777767,
113.868614836031)) ;
#167376 = CARTESIAN_POINT('Ctrl Pts',(-21.2361361322532,-13.8017353968177,
113.801272649912)) ;
#167377 = CARTESIAN_POINT('Ctrl Pts',(-21.2140265617871,-13.8289021158586,
113.733930463793)) ;
#167378 = CARTESIAN_POINT('Ctrl Pts',(-21.1402227287323,-13.8289022053652,
113.75816153705)) ;
#167379 = CARTESIAN_POINT('Ctrl Pts',(-21.0664188956774,-13.8289022948717,
113.782392610306)) ;
#167380 = CARTESIAN_POINT('Ctrl Pts',(-21.0885284661435,-13.8017355758307,
113.849734796424)) ;
#167381 = CARTESIAN_POINT('Ctrl Pts',(-21.0786678337561,-13.5177911289146,
113.784214759022)) ;
#167382 = CARTESIAN_POINT('Ctrl Pts',(-21.102233421415,-13.5104079472705,
113.85599173847)) ;
#167383 = CARTESIAN_POINT('Ctrl Pts',(-21.1760372624413,-13.5104078579673,
113.831760689493)) ;
#167384 = CARTESIAN_POINT('Ctrl Pts',(-21.2498411034676,-13.5104077686641,
113.807529640517)) ;
#167385 = CARTESIAN_POINT('Ctrl Pts',(-21.2262755158087,-13.5177909503083,
113.735752661069)) ;
#167386 = CARTESIAN_POINT('Ctrl Pts',(-21.2027099281497,-13.5251741319524,
113.663975681621)) ;
#167387 = CARTESIAN_POINT('Ctrl Pts',(-21.1289060871234,-13.5251742212556,
113.688206730597)) ;
#167388 = CARTESIAN_POINT('Ctrl Pts',(-21.0551022460972,-13.5251743105588,
113.712437779574)) ;
#167389 = CARTESIAN_POINT('Ctrl Pts',(-21.0786678337561,-13.5177911289146,
113.784214759022)) ;
#167390 = CARTESIAN_POINT('Ctrl Pts',(-21.0930193660603,-13.2272027816916,
113.79250094057)) ;
#167391 = CARTESIAN_POINT('Ctrl Pts',(-21.1163514983344,-13.2400970018567,
113.863566852463)) ;
#167392 = CARTESIAN_POINT('Ctrl Pts',(-21.1901553464802,-13.2400969198801,
113.839335825171)) ;
#167393 = CARTESIAN_POINT('Ctrl Pts',(-21.2639591946259,-13.2400968379035,
113.815104797879)) ;
#167394 = CARTESIAN_POINT('Ctrl Pts',(-21.2406270623518,-13.2272026177384,
113.744038885987)) ;
#167395 = CARTESIAN_POINT('Ctrl Pts',(-21.2172949300776,-13.2143083975732,
113.672972974094)) ;
#167396 = CARTESIAN_POINT('Ctrl Pts',(-21.1434910819319,-13.2143084795498,
113.697204001386)) ;
#167397 = CARTESIAN_POINT('Ctrl Pts',(-21.0696872337862,-13.2143085615265,
113.721435028678)) ;
#167398 = CARTESIAN_POINT('Ctrl Pts',(-21.0930193660603,-13.2272027816916,
113.79250094057)) ;
#167399 = CARTESIAN_POINT('Ctrl Pts',(-21.1311631750796,-12.9503466746931,
113.873276997434)) ;
#167400 = CARTESIAN_POINT('Ctrl Pts',(-21.152599925483,-12.9825901613467,
113.938569881838)) ;
#167401 = CARTESIAN_POINT('Ctrl Pts',(-21.2264037793875,-12.9825900924411,
113.914338872086)) ;
#167402 = CARTESIAN_POINT('Ctrl Pts',(-21.3002076332919,-12.9825900235354,
113.890107862335)) ;
#167403 = CARTESIAN_POINT('Ctrl Pts',(-21.2787708828885,-12.9503465368818,
113.82481497793)) ;
#167404 = CARTESIAN_POINT('Ctrl Pts',(-21.257334132485,-12.9181030502282,
113.759522093526)) ;
#167405 = CARTESIAN_POINT('Ctrl Pts',(-21.1835302785805,-12.9181031191338,
113.783753103278)) ;
#167406 = CARTESIAN_POINT('Ctrl Pts',(-21.1097264246761,-12.9181031880395,
113.80798411303)) ;
#167407 = CARTESIAN_POINT('Ctrl Pts',(-21.1311631750796,-12.9503466746931,
113.873276997434)) ;
#167408 = CARTESIAN_POINT('Ctrl Pts',(-21.1916208019657,-12.7057179827167,
114.021818954021)) ;
#167409 = CARTESIAN_POINT('Ctrl Pts',(-21.2096056903535,-12.7550903667589,
114.076598023505)) ;
#167410 = CARTESIAN_POINT('Ctrl Pts',(-21.2834095477442,-12.7550903161595,
114.052367024372)) ;
#167411 = CARTESIAN_POINT('Ctrl Pts',(-21.3572134051349,-12.7550902655601,
114.028136025238)) ;
#167412 = CARTESIAN_POINT('Ctrl Pts',(-21.3392285167472,-12.7057178815179,
113.973356955754)) ;
#167413 = CARTESIAN_POINT('Ctrl Pts',(-21.3212436283594,-12.6563454974757,
113.91857788627)) ;
#167414 = CARTESIAN_POINT('Ctrl Pts',(-21.2474397709687,-12.6563455480751,
113.942808885403)) ;
#167415 = CARTESIAN_POINT('Ctrl Pts',(-21.173635913578,-12.6563455986745,
113.967039884536)) ;
#167416 = CARTESIAN_POINT('Ctrl Pts',(-21.1916208019657,-12.7057179827167,
114.021818954021)) ;
#167417 = CARTESIAN_POINT('Ctrl Pts',(-21.2699420517425,-12.5137879422887,
114.22504280419)) ;
#167418 = CARTESIAN_POINT('Ctrl Pts',(-21.2832167372828,-12.5766355535095,
114.265475355653)) ;
#167419 = CARTESIAN_POINT('Ctrl Pts',(-21.3570205964976,-12.5766355204259,
114.241244362076)) ;
#167420 = CARTESIAN_POINT('Ctrl Pts',(-21.4308244557124,-12.5766354873422,
114.217013368499)) ;
#167421 = CARTESIAN_POINT('Ctrl Pts',(-21.417549770172,-12.5137878761215,
114.176580817036)) ;
#167422 = CARTESIAN_POINT('Ctrl Pts',(-21.4042750846316,-12.4509402649008,
114.136148265573)) ;
#167423 = CARTESIAN_POINT('Ctrl Pts',(-21.3304712254169,-12.4509402979844,
114.16037925915)) ;
#167424 = CARTESIAN_POINT('Ctrl Pts',(-21.2566673662021,-12.450940331068,
114.184610252727)) ;
#167425 = CARTESIAN_POINT('Ctrl Pts',(-21.2699420517425,-12.5137879422887,
114.22504280419)) ;
#167426 = CARTESIAN_POINT('Ctrl Pts',(-21.3620410862087,-12.3855428728414,
114.470083431169)) ;
#167427 = CARTESIAN_POINT('Ctrl Pts',(-21.3696396280776,-12.4574400165938,
114.493227364683)) ;
#167428 = CARTESIAN_POINT('Ctrl Pts',(-21.4434434869082,-12.4574400010847,
114.468996369935)) ;
#167429 = CARTESIAN_POINT('Ctrl Pts',(-21.5172473457389,-12.4574399855756,
114.444765375188)) ;
#167430 = CARTESIAN_POINT('Ctrl Pts',(-21.5096488038699,-12.3855428418231,
114.421621441674)) ;
#167431 = CARTESIAN_POINT('Ctrl Pts',(-21.502050262001,-12.3136456980707,
114.39847750816)) ;
#167432 = CARTESIAN_POINT('Ctrl Pts',(-21.4282464031703,-12.3136457135799,
114.422708502908)) ;
#167433 = CARTESIAN_POINT('Ctrl Pts',(-21.3544425443397,-12.313645729089,
114.446939497655)) ;
#167434 = CARTESIAN_POINT('Ctrl Pts',(-21.3620410862087,-12.3855428728414,
114.470083431169)) ;
#167435 = CARTESIAN_POINT('Ctrl Pts',(-21.4620234613405,-12.3315373856839,
114.739072799255)) ;
#167436 = CARTESIAN_POINT('Ctrl Pts',(-21.4633880246011,-12.4073146251765,
114.743229039594)) ;
#167437 = CARTESIAN_POINT('Ctrl Pts',(-21.5371918812133,-12.4073146237206,
114.718998038089)) ;
#167438 = CARTESIAN_POINT('Ctrl Pts',(-21.6109957378256,-12.4073146222647,
114.694767036585)) ;
#167439 = CARTESIAN_POINT('Ctrl Pts',(-21.609631174565,-12.331537382772,114.690610796247)) ;
#167440 = CARTESIAN_POINT('Ctrl Pts',(-21.6082666113044,-12.2557601432794,
114.686454555908)) ;
#167441 = CARTESIAN_POINT('Ctrl Pts',(-21.5344627546922,-12.2557601447353,
114.710685557413)) ;
#167442 = CARTESIAN_POINT('Ctrl Pts',(-21.4606588980799,-12.2557601461912,
114.734916558917)) ;
#167443 = CARTESIAN_POINT('Ctrl Pts',(-21.4620234613405,-12.3315373856839,
114.739072799255)) ;
#167444 = CARTESIAN_POINT('Ctrl Pts',(-21.5628393644424,-12.3551820249381,
115.010760483268)) ;
#167445 = CARTESIAN_POINT('Ctrl Pts',(-21.557898953099,-12.4294230563163,
114.995712788115)) ;
#167446 = CARTESIAN_POINT('Ctrl Pts',(-21.6317028069505,-12.4294230645316,
114.971481778201)) ;
#167447 = CARTESIAN_POINT('Ctrl Pts',(-21.705506660802,-12.4294230727469,
114.947250768288)) ;
#167448 = CARTESIAN_POINT('Ctrl Pts',(-21.7104470721454,-12.3551820413687,
114.962298463441)) ;
#167449 = CARTESIAN_POINT('Ctrl Pts',(-21.7153874834888,-12.2809410099905,
114.977346158594)) ;
#167450 = CARTESIAN_POINT('Ctrl Pts',(-21.6415836296373,-12.2809410017752,
115.001577168508)) ;
#167451 = CARTESIAN_POINT('Ctrl Pts',(-21.5677797757859,-12.2809409935599,
115.025808178421)) ;
#167452 = CARTESIAN_POINT('Ctrl Pts',(-21.5628393644424,-12.3551820249381,
115.010760483268)) ;
#167453 = CARTESIAN_POINT('Ctrl Pts',(-21.659189028177,-12.4558831035982,
115.268554494791)) ;
#167454 = CARTESIAN_POINT('Ctrl Pts',(-21.6482517146779,-12.5232058909048,
115.23524120307)) ;
#167455 = CARTESIAN_POINT('Ctrl Pts',(-21.7220555646767,-12.52320590289,115.211010181422)) ;
#167456 = CARTESIAN_POINT('Ctrl Pts',(-21.7958594146756,-12.5232059148753,
115.186779159775)) ;
#167457 = CARTESIAN_POINT('Ctrl Pts',(-21.8067967281747,-12.4558831275687,
115.220092451495)) ;
#167458 = CARTESIAN_POINT('Ctrl Pts',(-21.8177340416738,-12.3885603402622,
115.253405743216)) ;
#167459 = CARTESIAN_POINT('Ctrl Pts',(-21.7439301916749,-12.3885603282769,
115.277636764863)) ;
#167460 = CARTESIAN_POINT('Ctrl Pts',(-21.6701263416761,-12.3885603162917,
115.301867786511)) ;
#167461 = CARTESIAN_POINT('Ctrl Pts',(-21.659189028177,-12.4558831035982,
115.268554494791)) ;
#167462 = CARTESIAN_POINT('Ctrl Pts',(-21.743187461739,-12.6240117159259,
115.489136281723)) ;
#167463 = CARTESIAN_POINT('Ctrl Pts',(-21.7270983492204,-12.6796964809936,
115.440131441313)) ;
#167464 = CARTESIAN_POINT('Ctrl Pts',(-21.8009021966587,-12.6796964939069,
115.415900411867)) ;
#167465 = CARTESIAN_POINT('Ctrl Pts',(-21.8747060440971,-12.6796965068202,
115.39166938242)) ;
#167466 = CARTESIAN_POINT('Ctrl Pts',(-21.8907951566158,-12.6240117417526,
115.44067422283)) ;
#167467 = CARTESIAN_POINT('Ctrl Pts',(-21.9068842691344,-12.568326976685,
115.489679063239)) ;
#167468 = CARTESIAN_POINT('Ctrl Pts',(-21.833080421696,-12.5683269637716,
115.513910092686)) ;
#167469 = CARTESIAN_POINT('Ctrl Pts',(-21.7592765742577,-12.5683269508583,
115.538141122132)) ;
#167470 = CARTESIAN_POINT('Ctrl Pts',(-21.743187461739,-12.6240117159259,
115.489136281723)) ;
#167471 = CARTESIAN_POINT('Ctrl Pts',(-21.8112843757368,-12.8504012275685,
115.660972680477)) ;
#167472 = CARTESIAN_POINT('Ctrl Pts',(-21.7911521928067,-12.8903625364955,
115.599653299789)) ;
#167473 = CARTESIAN_POINT('Ctrl Pts',(-21.8649560377389,-12.8903625457094,
115.575422262709)) ;
#167474 = CARTESIAN_POINT('Ctrl Pts',(-21.9387598826711,-12.8903625549234,
115.551191225629)) ;
#167475 = CARTESIAN_POINT('Ctrl Pts',(-21.9588920656012,-12.8504012459964,
115.612510606317)) ;
#167476 = CARTESIAN_POINT('Ctrl Pts',(-21.9790242485314,-12.8104399370694,
115.673829987006)) ;
#167477 = CARTESIAN_POINT('Ctrl Pts',(-21.9052204035992,-12.8104399278554,
115.698061024086)) ;
#167478 = CARTESIAN_POINT('Ctrl Pts',(-21.831416558667,-12.8104399186415,
115.722292061166)) ;
#167479 = CARTESIAN_POINT('Ctrl Pts',(-21.8112843757368,-12.8504012275685,
115.660972680477)) ;
#167480 = CARTESIAN_POINT('Ctrl Pts',(-21.8582977807734,-13.116472804272,
115.768768866899)) ;
#167481 = CARTESIAN_POINT('Ctrl Pts',(-21.8355851398991,-13.1379154690077,
115.699589827564)) ;
#167482 = CARTESIAN_POINT('Ctrl Pts',(-21.9093889836109,-13.1379154738939,
115.675358786767)) ;
#167483 = CARTESIAN_POINT('Ctrl Pts',(-21.9831928273227,-13.13791547878,115.651127745969)) ;
#167484 = CARTESIAN_POINT('Ctrl Pts',(-22.0059054681969,-13.1164728140443,
115.720306785305)) ;
#167485 = CARTESIAN_POINT('Ctrl Pts',(-22.0286181090711,-13.0950301493086,
115.789485824641)) ;
#167486 = CARTESIAN_POINT('Ctrl Pts',(-21.9548142653594,-13.0950301444224,
115.813716865438)) ;
#167487 = CARTESIAN_POINT('Ctrl Pts',(-21.8810104216476,-13.0950301395363,
115.837947906235)) ;
#167488 = CARTESIAN_POINT('Ctrl Pts',(-21.8582977807734,-13.116472804272,
115.768768866899)) ;
#167489 = CARTESIAN_POINT('Ctrl Pts',(-21.8820745506903,-13.4044926459014,
115.805724068696)) ;
#167490 = CARTESIAN_POINT('Ctrl Pts',(-21.8584015173245,-13.4058558527326,
115.733619828702)) ;
#167491 = CARTESIAN_POINT('Ctrl Pts',(-21.9322053606268,-13.4058558531923,
115.709388786657)) ;
#167492 = CARTESIAN_POINT('Ctrl Pts',(-22.0060092039291,-13.405855853652,
115.685157744613)) ;
#167493 = CARTESIAN_POINT('Ctrl Pts',(-22.0296822372949,-13.4044926468209,
115.757261984607)) ;
#167494 = CARTESIAN_POINT('Ctrl Pts',(-22.0533552706608,-13.4031294399897,
115.829366224601)) ;
#167495 = CARTESIAN_POINT('Ctrl Pts',(-21.9795514273585,-13.40312943953,115.853597266645)) ;
#167496 = CARTESIAN_POINT('Ctrl Pts',(-21.9057475840562,-13.4031294390702,
115.877828308689)) ;
#167497 = CARTESIAN_POINT('Ctrl Pts',(-21.8820745506903,-13.4044926459014,
115.805724068696)) ;
#167498 = CARTESIAN_POINT('Ctrl Pts',(-21.8816087919377,-13.6930971947521,
115.768901188639)) ;
#167499 = CARTESIAN_POINT('Ctrl Pts',(-21.8586656358087,-13.6743099521877,
115.699020036887)) ;
#167500 = CARTESIAN_POINT('Ctrl Pts',(-21.9324694793602,-13.6743099497306,
115.674788995601)) ;
#167501 = CARTESIAN_POINT('Ctrl Pts',(-22.0062733229118,-13.6743099472734,
115.650557954316)) ;
#167502 = CARTESIAN_POINT('Ctrl Pts',(-22.0292164790407,-13.6930971898379,
115.720439106068)) ;
#167503 = CARTESIAN_POINT('Ctrl Pts',(-22.0521596351697,-13.7118844324023,
115.79032025782)) ;
#167504 = CARTESIAN_POINT('Ctrl Pts',(-21.9783557916181,-13.7118844348594,
115.814551299106)) ;
#167505 = CARTESIAN_POINT('Ctrl Pts',(-21.9045519480666,-13.7118844373166,
115.838782340391)) ;
#167506 = CARTESIAN_POINT('Ctrl Pts',(-21.8816087919377,-13.6930971947521,
115.768901188639)) ;
#167507 = CARTESIAN_POINT('Ctrl Pts',(-21.8573708161065,-13.9640294815732,
115.659386725099)) ;
#167508 = CARTESIAN_POINT('Ctrl Pts',(-21.8368246163992,-13.9262943650166,
115.596806315842)) ;
#167509 = CARTESIAN_POINT('Ctrl Pts',(-21.9106284603522,-13.9262943620916,
115.572575275779)) ;
#167510 = CARTESIAN_POINT('Ctrl Pts',(-21.9844323043051,-13.9262943591665,
115.548344235717)) ;
#167511 = CARTESIAN_POINT('Ctrl Pts',(-22.0049785040124,-13.9640294757231,
115.610924644974)) ;
#167512 = CARTESIAN_POINT('Ctrl Pts',(-22.0255247037197,-14.0017645922797,
115.673505054231)) ;
#167513 = CARTESIAN_POINT('Ctrl Pts',(-21.9517208597667,-14.0017645952047,
115.697736094293)) ;
#167514 = CARTESIAN_POINT('Ctrl Pts',(-21.8779170158137,-14.0017645981297,
115.721967134356)) ;
#167515 = CARTESIAN_POINT('Ctrl Pts',(-21.8573708161065,-13.9640294815732,
115.659386725099)) ;
#167516 = CARTESIAN_POINT('Ctrl Pts',(-21.8123589552263,-14.1931760928296,
115.486961111576)) ;
#167517 = CARTESIAN_POINT('Ctrl Pts',(-21.7956567301436,-14.1393849019779,
115.436088828833)) ;
#167518 = CARTESIAN_POINT('Ctrl Pts',(-21.8694605740056,-14.1393849008332,
115.411857788494)) ;
#167519 = CARTESIAN_POINT('Ctrl Pts',(-21.9432644178677,-14.1393848996885,
115.387626748154)) ;
#167520 = CARTESIAN_POINT('Ctrl Pts',(-21.9599666429505,-14.1931760905402,
115.438499030898)) ;
#167521 = CARTESIAN_POINT('Ctrl Pts',(-21.9766688680333,-14.2469672813919,
115.489371313641)) ;
#167522 = CARTESIAN_POINT('Ctrl Pts',(-21.9028650241712,-14.2469672825366,
115.513602353981)) ;
#167523 = CARTESIAN_POINT('Ctrl Pts',(-21.8290611803091,-14.2469672836813,
115.53783339432)) ;
#167524 = CARTESIAN_POINT('Ctrl Pts',(-21.8123589552263,-14.1931760928296,
115.486961111576)) ;
#167525 = CARTESIAN_POINT('Ctrl Pts',(-21.7503610168771,-14.3676938142289,
115.262726512895)) ;
#167526 = CARTESIAN_POINT('Ctrl Pts',(-21.7386959620902,-14.3016378950291,
115.227196638184)) ;
#167527 = CARTESIAN_POINT('Ctrl Pts',(-21.8124998052628,-14.3016378958559,
115.202965595744)) ;
#167528 = CARTESIAN_POINT('Ctrl Pts',(-21.8863036484354,-14.3016378966827,
115.178734553305)) ;
#167529 = CARTESIAN_POINT('Ctrl Pts',(-21.8979687032223,-14.3676938158825,
115.214264428016)) ;
#167530 = CARTESIAN_POINT('Ctrl Pts',(-21.9096337580092,-14.4337497350823,
115.249794302726)) ;
#167531 = CARTESIAN_POINT('Ctrl Pts',(-21.8358299148366,-14.4337497342555,
115.274025345166)) ;
#167532 = CARTESIAN_POINT('Ctrl Pts',(-21.762026071664,-14.4337497334287,
115.298256387605)) ;
#167533 = CARTESIAN_POINT('Ctrl Pts',(-21.7503610168771,-14.3676938142289,
115.262726512895)) ;
#167534 = CARTESIAN_POINT('Ctrl Pts',(-21.6763081582206,-14.4745465378171,
115.001681494378)) ;
#167535 = CARTESIAN_POINT('Ctrl Pts',(-21.6705313272715,-14.4009329542059,
114.984086199513)) ;
#167536 = CARTESIAN_POINT('Ctrl Pts',(-21.7443351688861,-14.4009329561401,
114.959855152328)) ;
#167537 = CARTESIAN_POINT('Ctrl Pts',(-21.8181390105007,-14.4009329580743,
114.935624105143)) ;
#167538 = CARTESIAN_POINT('Ctrl Pts',(-21.8239158414498,-14.4745465416855,
114.953219400009)) ;
#167539 = CARTESIAN_POINT('Ctrl Pts',(-21.8296926723988,-14.5481601252968,
114.970814694874)) ;
#167540 = CARTESIAN_POINT('Ctrl Pts',(-21.7558888307842,-14.5481601233625,
114.995045742059)) ;
#167541 = CARTESIAN_POINT('Ctrl Pts',(-21.6820849891696,-14.5481601214283,
115.019276789244)) ;
#167542 = CARTESIAN_POINT('Ctrl Pts',(-21.6763081582206,-14.4745465378171,
115.001681494378)) ;
#167543 = CARTESIAN_POINT('Ctrl Pts',(-21.596449872518,-14.5056303399819,
114.722959733206)) ;
#167544 = CARTESIAN_POINT('Ctrl Pts',(-21.5969750226913,-14.4297391365026,
114.72455925614)) ;
#167545 = CARTESIAN_POINT('Ctrl Pts',(-21.6707788622314,-14.4297391368143,
114.700328202637)) ;
#167546 = CARTESIAN_POINT('Ctrl Pts',(-21.7445827017715,-14.429739137126,
114.676097149134)) ;
#167547 = CARTESIAN_POINT('Ctrl Pts',(-21.7440575515982,-14.5056303406052,
114.674497626199)) ;
#167548 = CARTESIAN_POINT('Ctrl Pts',(-21.7435324014249,-14.5815215440845,
114.672898103265)) ;
#167549 = CARTESIAN_POINT('Ctrl Pts',(-21.6697285618848,-14.5815215437728,
114.697129156768)) ;
#167550 = CARTESIAN_POINT('Ctrl Pts',(-21.5959247223447,-14.5815215434611,
114.721360210271)) ;
#167551 = CARTESIAN_POINT('Ctrl Pts',(-21.596449872518,-14.5056303399819,
114.722959733206)) ;
#167552 = CARTESIAN_POINT('Ctrl Pts',(-21.5172133727287,-14.4584990503317,
114.446100755161)) ;
#167553 = CARTESIAN_POINT('Ctrl Pts',(-21.5240068136617,-14.3857884203973,
114.466792480513)) ;
#167554 = CARTESIAN_POINT('Ctrl Pts',(-21.5978106510323,-14.3857884151158,
114.442561420402)) ;
#167555 = CARTESIAN_POINT('Ctrl Pts',(-21.6716144884028,-14.3857884098344,
114.41833036029)) ;
#167556 = CARTESIAN_POINT('Ctrl Pts',(-21.6648210474699,-14.4584990397688,
114.397638634938)) ;
#167557 = CARTESIAN_POINT('Ctrl Pts',(-21.6580276065369,-14.5312096697032,
114.376946909586)) ;
#167558 = CARTESIAN_POINT('Ctrl Pts',(-21.5842237691663,-14.5312096749846,
114.401177969697)) ;
#167559 = CARTESIAN_POINT('Ctrl Pts',(-21.5104199317957,-14.5312096802661,
114.425409029809)) ;
#167560 = CARTESIAN_POINT('Ctrl Pts',(-21.5172133727287,-14.4584990503317,
114.446100755161)) ;
#167561 = CARTESIAN_POINT('Ctrl Pts',(-21.4454184043166,-14.3375927241235,
114.192092160154)) ;
#167562 = CARTESIAN_POINT('Ctrl Pts',(-21.4579655933527,-14.2732190066455,
114.230308873994)) ;
#167563 = CARTESIAN_POINT('Ctrl Pts',(-21.5317694295724,-14.2732189929484,
114.206077810378)) ;
#167564 = CARTESIAN_POINT('Ctrl Pts',(-21.6055732657922,-14.2732189792513,
114.181846746761)) ;
#167565 = CARTESIAN_POINT('Ctrl Pts',(-21.5930260767561,-14.3375926967294,
114.143630032921)) ;
#167566 = CARTESIAN_POINT('Ctrl Pts',(-21.58047888772,-14.4019664142074,114.105413319081)) ;
#167567 = CARTESIAN_POINT('Ctrl Pts',(-21.5066750515002,-14.4019664279045,
114.129644382697)) ;
#167568 = CARTESIAN_POINT('Ctrl Pts',(-21.4328712152804,-14.4019664416016,
114.153875446314)) ;
#167569 = CARTESIAN_POINT('Ctrl Pts',(-21.4454184043166,-14.3375927241235,
114.192092160154)) ;
#167570 = CARTESIAN_POINT('Ctrl Pts',(-21.3860672106349,-14.1494056626898,
113.975672837523)) ;
#167571 = CARTESIAN_POINT('Ctrl Pts',(-21.4035142179222,-14.0980778114582,
114.02881360737)) ;
#167572 = CARTESIAN_POINT('Ctrl Pts',(-21.4773180533873,-14.0980777847103,
114.004582541455)) ;
#167573 = CARTESIAN_POINT('Ctrl Pts',(-21.5511218888525,-14.0980777579623,
113.98035147554)) ;
#167574 = CARTESIAN_POINT('Ctrl Pts',(-21.5336748815651,-14.1494056091939,
113.927210705693)) ;
#167575 = CARTESIAN_POINT('Ctrl Pts',(-21.5162278742778,-14.2007334604254,
113.874069935846)) ;
#167576 = CARTESIAN_POINT('Ctrl Pts',(-21.4424240388127,-14.2007334871734,
113.898301001761)) ;
#167577 = CARTESIAN_POINT('Ctrl Pts',(-21.3686202033475,-14.2007335139213,
113.922532067676)) ;
#167578 = CARTESIAN_POINT('Ctrl Pts',(-21.3860672106349,-14.1494056626898,
113.975672837523)) ;
#167579 = CARTESIAN_POINT('Ctrl Pts',(-21.345130013158,-13.9095500364901,
113.815534566818)) ;
#167580 = CARTESIAN_POINT('Ctrl Pts',(-21.3661940068873,-13.8748947454948,
113.879692093934)) ;
#167581 = CARTESIAN_POINT('Ctrl Pts',(-21.4399978437013,-13.874894705204,
113.855461032127)) ;
#167582 = CARTESIAN_POINT('Ctrl Pts',(-21.5138016805153,-13.8748946649131,
113.831229970321)) ;
#167583 = CARTESIAN_POINT('Ctrl Pts',(-21.492737686786,-13.9095499559084,
113.767072443205)) ;
#167584 = CARTESIAN_POINT('Ctrl Pts',(-21.4716736930567,-13.9442052469036,
113.702914916089)) ;
#167585 = CARTESIAN_POINT('Ctrl Pts',(-21.3978698562426,-13.9442052871945,
113.727145977895)) ;
#167586 = CARTESIAN_POINT('Ctrl Pts',(-21.3240660194286,-13.9442053274854,
113.751377039702)) ;
#167587 = CARTESIAN_POINT('Ctrl Pts',(-21.345130013158,-13.9095500364901,
113.815534566818)) ;
#167588 = CARTESIAN_POINT('Ctrl Pts',(-21.3258230846178,-13.6354015229083,
113.721370608325)) ;
#167589 = CARTESIAN_POINT('Ctrl Pts',(-21.3489970490078,-13.6198370471349,
113.791954765778)) ;
#167590 = CARTESIAN_POINT('Ctrl Pts',(-21.4228008888894,-13.6198369951942,
113.767723713315)) ;
#167591 = CARTESIAN_POINT('Ctrl Pts',(-21.496604728771,-13.6198369432535,
113.743492660852)) ;
#167592 = CARTESIAN_POINT('Ctrl Pts',(-21.4734307643811,-13.6354014190268,
113.672908503398)) ;
#167593 = CARTESIAN_POINT('Ctrl Pts',(-21.4502567999911,-13.6509658948002,
113.602324345945)) ;
#167594 = CARTESIAN_POINT('Ctrl Pts',(-21.3764529601095,-13.6509659467409,
113.626555398408)) ;
#167595 = CARTESIAN_POINT('Ctrl Pts',(-21.3026491202279,-13.6509659986816,
113.650786450871)) ;
#167596 = CARTESIAN_POINT('Ctrl Pts',(-21.3258230846178,-13.6354015229083,
113.721370608325)) ;
#167597 = CARTESIAN_POINT('Ctrl Pts',(-21.3302591662937,-13.3449945339553,
113.699428650571)) ;
#167598 = CARTESIAN_POINT('Ctrl Pts',(-21.3538905068384,-13.3496833242157,
113.771405902157)) ;
#167599 = CARTESIAN_POINT('Ctrl Pts',(-21.4276943513303,-13.3496832627429,
113.747174863736)) ;
#167600 = CARTESIAN_POINT('Ctrl Pts',(-21.5014981958221,-13.3496832012701,
113.722943825315)) ;
#167601 = CARTESIAN_POINT('Ctrl Pts',(-21.4778668552774,-13.3449944110097,
113.650966573729)) ;
#167602 = CARTESIAN_POINT('Ctrl Pts',(-21.4542355147327,-13.3403056207493,
113.578989322142)) ;
#167603 = CARTESIAN_POINT('Ctrl Pts',(-21.3804316702409,-13.3403056822221,
113.603220360563)) ;
#167604 = CARTESIAN_POINT('Ctrl Pts',(-21.306627825749,-13.3403057436949,
113.627451398984)) ;
#167605 = CARTESIAN_POINT('Ctrl Pts',(-21.3302591662937,-13.3449945339553,
113.699428650571)) ;
#167606 = CARTESIAN_POINT('Ctrl Pts',(-21.3588254375783,-13.0600685836045,
113.75103011028)) ;
#167607 = CARTESIAN_POINT('Ctrl Pts',(-21.3812291127916,-13.0846570049903,
113.8192680915)) ;
#167608 = CARTESIAN_POINT('Ctrl Pts',(-21.4550329630849,-13.0846569392068,
113.795037070749)) ;
#167609 = CARTESIAN_POINT('Ctrl Pts',(-21.5288368133782,-13.0846568734233,
113.770806049999)) ;
#167610 = CARTESIAN_POINT('Ctrl Pts',(-21.5064331381649,-13.0600684520375,
113.702568068778)) ;
#167611 = CARTESIAN_POINT('Ctrl Pts',(-21.4840294629517,-13.0354800306517,
113.634330087558)) ;
#167612 = CARTESIAN_POINT('Ctrl Pts',(-21.4102256126584,-13.0354800964351,
113.658561108309)) ;
#167613 = CARTESIAN_POINT('Ctrl Pts',(-21.3364217623651,-13.0354801622186,
113.68279212906)) ;
#167614 = CARTESIAN_POINT('Ctrl Pts',(-21.3588254375783,-13.0600685836045,
113.75103011028)) ;
#167615 = CARTESIAN_POINT('Ctrl Pts',(-21.4108808833159,-12.7987719757991,
113.873871369962)) ;
#167616 = CARTESIAN_POINT('Ctrl Pts',(-21.4304218220357,-12.8416392533606,
113.933389917914)) ;
#167617 = CARTESIAN_POINT('Ctrl Pts',(-21.5042256793353,-12.8416391878999,
113.909158918504)) ;
#167618 = CARTESIAN_POINT('Ctrl Pts',(-21.5780295366349,-12.8416391224392,
113.884927919093)) ;
#167619 = CARTESIAN_POINT('Ctrl Pts',(-21.5584885979151,-12.7987718448777,
113.825409371141)) ;
#167620 = CARTESIAN_POINT('Ctrl Pts',(-21.5389476591953,-12.7559045673161,
113.765890823189)) ;
#167621 = CARTESIAN_POINT('Ctrl Pts',(-21.4651438018957,-12.7559046327768,
113.790121822599)) ;
#167622 = CARTESIAN_POINT('Ctrl Pts',(-21.3913399445961,-12.7559046982375,
113.81435282201)) ;
#167623 = CARTESIAN_POINT('Ctrl Pts',(-21.4108808833159,-12.7987719757991,
113.873871369962)) ;
#167624 = CARTESIAN_POINT('Ctrl Pts',(-21.4821786810617,-12.5848307790968,
114.055776077785)) ;
#167625 = CARTESIAN_POINT('Ctrl Pts',(-21.4974995321701,-12.6426967262578,
114.102440919885)) ;
#167626 = CARTESIAN_POINT('Ctrl Pts',(-21.571303395686,-12.6426966715405,
114.078209939408)) ;
#167627 = CARTESIAN_POINT('Ctrl Pts',(-21.6451072592018,-12.6426966168232,
114.053978958931)) ;
#167628 = CARTESIAN_POINT('Ctrl Pts',(-21.6297864080934,-12.5848306696622,
114.007314116831)) ;
#167629 = CARTESIAN_POINT('Ctrl Pts',(-21.6144655569851,-12.5269647225012,
113.960649274732)) ;
#167630 = CARTESIAN_POINT('Ctrl Pts',(-21.5406616934692,-12.5269647772185,
113.984880255209)) ;
#167631 = CARTESIAN_POINT('Ctrl Pts',(-21.4668578299534,-12.5269648319358,
114.009111235686)) ;
#167632 = CARTESIAN_POINT('Ctrl Pts',(-21.4821786810617,-12.5848307790968,
114.055776077785)) ;
#167633 = CARTESIAN_POINT('Ctrl Pts',(-21.5695756033995,-12.428840573078,
114.286444660631)) ;
#167634 = CARTESIAN_POINT('Ctrl Pts',(-21.5795521820823,-12.4976814923142,
114.31683171135)) ;
#167635 = CARTESIAN_POINT('Ctrl Pts',(-21.6533560513287,-12.4976814537986,
114.292600748327)) ;
#167636 = CARTESIAN_POINT('Ctrl Pts',(-21.7271599205752,-12.497681415283,
114.268369785305)) ;
#167637 = CARTESIAN_POINT('Ctrl Pts',(-21.7171833418924,-12.4288404960468,
114.237982734586)) ;
#167638 = CARTESIAN_POINT('Ctrl Pts',(-21.7072067632097,-12.3599995768106,
114.207595683868)) ;
#167639 = CARTESIAN_POINT('Ctrl Pts',(-21.6334028939632,-12.3599996153262,
114.23182664689)) ;
#167640 = CARTESIAN_POINT('Ctrl Pts',(-21.5595990247167,-12.3599996538418,
114.256057609913)) ;
#167641 = CARTESIAN_POINT('Ctrl Pts',(-21.5695756033995,-12.428840573078,
114.286444660631)) ;
#167642 = CARTESIAN_POINT('Ctrl Pts',(-21.6669221796403,-12.3440689509793,
114.547509032478)) ;
#167643 = CARTESIAN_POINT('Ctrl Pts',(-21.6708501782994,-12.4189286311326,
114.559473084482)) ;
#167644 = CARTESIAN_POINT('Ctrl Pts',(-21.7446540514633,-12.4189286151795,
114.535242133391)) ;
#167645 = CARTESIAN_POINT('Ctrl Pts',(-21.8184579246271,-12.4189285992263,
114.5110111823)) ;
#167646 = CARTESIAN_POINT('Ctrl Pts',(-21.8145299259679,-12.3440689190729,
114.499047130296)) ;
#167647 = CARTESIAN_POINT('Ctrl Pts',(-21.8106019273088,-12.2692092389195,
114.487083078292)) ;
#167648 = CARTESIAN_POINT('Ctrl Pts',(-21.736798054145,-12.2692092548727,
114.511314029383)) ;
#167649 = CARTESIAN_POINT('Ctrl Pts',(-21.6629941809811,-12.2692092708259,
114.535544980474)) ;
#167650 = CARTESIAN_POINT('Ctrl Pts',(-21.6669221796403,-12.3440689509793,
114.547509032478)) ;
#167651 = CARTESIAN_POINT('Ctrl Pts',(-21.7687094216625,-12.3364316802486,
114.821900463108)) ;
#167652 = CARTESIAN_POINT('Ctrl Pts',(-21.7662742013755,-12.4119346033566,
114.814483177004)) ;
#167653 = CARTESIAN_POINT('Ctrl Pts',(-21.8400780763928,-12.4119346140826,
114.790252231559)) ;
#167654 = CARTESIAN_POINT('Ctrl Pts',(-21.9138819514101,-12.4119346248087,
114.766021286114)) ;
#167655 = CARTESIAN_POINT('Ctrl Pts',(-21.916317171697,-12.3364317017007,
114.773438572217)) ;
#167656 = CARTESIAN_POINT('Ctrl Pts',(-21.918752391984,-12.2609287785927,
114.78085585832)) ;
#167657 = CARTESIAN_POINT('Ctrl Pts',(-21.8449485169667,-12.2609287678666,
114.805086803766)) ;
#167658 = CARTESIAN_POINT('Ctrl Pts',(-21.7711446419494,-12.2609287571406,
114.829317749211)) ;
#167659 = CARTESIAN_POINT('Ctrl Pts',(-21.7687094216625,-12.3364316802486,
114.821900463108)) ;
#167660 = CARTESIAN_POINT('Ctrl Pts',(-21.8668995311495,-12.4059134721985,
115.085690184209)) ;
#167661 = CARTESIAN_POINT('Ctrl Pts',(-21.8583354753262,-12.4766756049436,
115.059605453997)) ;
#167662 = CARTESIAN_POINT('Ctrl Pts',(-21.9321393490943,-12.4766756431297,
115.035374504746)) ;
#167663 = CARTESIAN_POINT('Ctrl Pts',(-22.0059432228623,-12.4766756813157,
115.011143555496)) ;
#167664 = CARTESIAN_POINT('Ctrl Pts',(-22.0145072786857,-12.4059135485707,
115.037228285708)) ;
#167665 = CARTESIAN_POINT('Ctrl Pts',(-22.0230713345091,-12.3351514158256,
115.06331301592)) ;
#167666 = CARTESIAN_POINT('Ctrl Pts',(-21.949267460741,-12.3351513776395,
115.087543965171)) ;
#167667 = CARTESIAN_POINT('Ctrl Pts',(-21.8754635869729,-12.3351513394535,
115.111774914421)) ;
#167668 = CARTESIAN_POINT('Ctrl Pts',(-21.8668995311495,-12.4059134721985,
115.085690184209)) ;
#167669 = CARTESIAN_POINT('Ctrl Pts',(-21.9568607042708,-12.5482447968648,
115.324163533208)) ;
#167670 = CARTESIAN_POINT('Ctrl Pts',(-21.9427385662062,-12.609174259838,
115.281149781333)) ;
#167671 = CARTESIAN_POINT('Ctrl Pts',(-22.0165424363522,-12.6091743240943,
115.25691882105)) ;
#167672 = CARTESIAN_POINT('Ctrl Pts',(-22.0903463064982,-12.6091743883507,
115.232687860767)) ;
#167673 = CARTESIAN_POINT('Ctrl Pts',(-22.1044684445627,-12.5482449253774,
115.275701612643)) ;
#167674 = CARTESIAN_POINT('Ctrl Pts',(-22.1185905826272,-12.4873154624041,
115.318715364518)) ;
#167675 = CARTESIAN_POINT('Ctrl Pts',(-22.0447867124812,-12.4873153981478,
115.342946324801)) ;
#167676 = CARTESIAN_POINT('Ctrl Pts',(-21.9709828423353,-12.4873153338915,
115.367177285083)) ;
#167677 = CARTESIAN_POINT('Ctrl Pts',(-21.9568607042708,-12.5482447968648,
115.324163533208)) ;
#167678 = CARTESIAN_POINT('Ctrl Pts',(-22.0318603212468,-12.7523234032848,
115.517213231457)) ;
#167679 = CARTESIAN_POINT('Ctrl Pts',(-22.0132133823266,-12.7990945462317,
115.460417666269)) ;
#167680 = CARTESIAN_POINT('Ctrl Pts',(-22.0870172463905,-12.7990946317952,
115.436186687461)) ;
#167681 = CARTESIAN_POINT('Ctrl Pts',(-22.1608211104543,-12.7990947173587,
115.411955708654)) ;
#167682 = CARTESIAN_POINT('Ctrl Pts',(-22.1794680493745,-12.7523235744117,
115.468751273841)) ;
#167683 = CARTESIAN_POINT('Ctrl Pts',(-22.1981149882947,-12.7055524314648,
115.525546839029)) ;
#167684 = CARTESIAN_POINT('Ctrl Pts',(-22.1243111242308,-12.7055523459013,
115.549777817836)) ;
#167685 = CARTESIAN_POINT('Ctrl Pts',(-22.050507260167,-12.7055522603379,
115.574008796644)) ;
#167686 = CARTESIAN_POINT('Ctrl Pts',(-22.0318603212468,-12.7523234032848,
115.517213231457)) ;
#167687 = CARTESIAN_POINT('Ctrl Pts',(-22.0879198570419,-13.0044659647124,
115.652477656322)) ;
#167688 = CARTESIAN_POINT('Ctrl Pts',(-22.066065668734,-13.0337028196908,
115.585913326992)) ;
#167689 = CARTESIAN_POINT('Ctrl Pts',(-22.1398695249688,-13.0337029200477,
115.561682324338)) ;
#167690 = CARTESIAN_POINT('Ctrl Pts',(-22.2136733812036,-13.0337030204046,
115.537451321685)) ;
#167691 = CARTESIAN_POINT('Ctrl Pts',(-22.2355275695115,-13.0044661654261,
115.604015651014)) ;
#167692 = CARTESIAN_POINT('Ctrl Pts',(-22.2573817578194,-12.9752293104477,
115.670579980344)) ;
#167693 = CARTESIAN_POINT('Ctrl Pts',(-22.1835779015846,-12.9752292100908,
115.694810982998)) ;
#167694 = CARTESIAN_POINT('Ctrl Pts',(-22.1097740453498,-12.9752291097339,
115.719041985652)) ;
#167695 = CARTESIAN_POINT('Ctrl Pts',(-22.0879198570419,-13.0044659647124,
115.652477656322)) ;
#167696 = CARTESIAN_POINT('Ctrl Pts',(-22.1214488600341,-13.2877069321833,
115.718954843121)) ;
#167697 = CARTESIAN_POINT('Ctrl Pts',(-22.0979587435142,-13.2972126814731,
115.647407740385)) ;
#167698 = CARTESIAN_POINT('Ctrl Pts',(-22.1717625908651,-13.2972127876648,
115.623176710672)) ;
#167699 = CARTESIAN_POINT('Ctrl Pts',(-22.245566438216,-13.2972128938564,
115.598945680959)) ;
#167700 = CARTESIAN_POINT('Ctrl Pts',(-22.269056554736,-13.2877071445666,
115.670492783696)) ;
#167701 = CARTESIAN_POINT('Ctrl Pts',(-22.2925466712559,-13.2782013952768,
115.742039886433)) ;
#167702 = CARTESIAN_POINT('Ctrl Pts',(-22.218742823905,-13.2782012890852,
115.766270916145)) ;
#167703 = CARTESIAN_POINT('Ctrl Pts',(-22.1449389765541,-13.2782011828935,
115.790501945858)) ;
#167704 = CARTESIAN_POINT('Ctrl Pts',(-22.1214488600341,-13.2877069321833,
115.718954843121)) ;
#167705 = CARTESIAN_POINT('Ctrl Pts',(-22.1306963457754,-13.5768962487208,
115.71190010407)) ;
#167706 = CARTESIAN_POINT('Ctrl Pts',(-22.1072546120684,-13.5662255723237,
115.640500367543)) ;
#167707 = CARTESIAN_POINT('Ctrl Pts',(-22.1810584505935,-13.5662256764684,
115.616269310949)) ;
#167708 = CARTESIAN_POINT('Ctrl Pts',(-22.2548622891185,-13.5662257806131,
115.592038254354)) ;
#167709 = CARTESIAN_POINT('Ctrl Pts',(-22.2783040228256,-13.5768964570101,
115.66343799088)) ;
#167710 = CARTESIAN_POINT('Ctrl Pts',(-22.3017457565327,-13.5875671334072,
115.734837727407)) ;
#167711 = CARTESIAN_POINT('Ctrl Pts',(-22.2279419180076,-13.5875670292625,
115.759068784001)) ;
#167712 = CARTESIAN_POINT('Ctrl Pts',(-22.1541380794825,-13.5875669251178,
115.783299840596)) ;
#167713 = CARTESIAN_POINT('Ctrl Pts',(-22.1306963457754,-13.5768962487208,
115.71190010407)) ;
#167714 = CARTESIAN_POINT('Ctrl Pts',(-22.1159420679376,-13.8582071770573,
115.631296548337)) ;
#167715 = CARTESIAN_POINT('Ctrl Pts',(-22.0942331444257,-13.8278804219563,
115.565174672)) ;
#167716 = CARTESIAN_POINT('Ctrl Pts',(-22.1680369749167,-13.8278805144787,
115.540943590935)) ;
#167717 = CARTESIAN_POINT('Ctrl Pts',(-22.2418408054076,-13.8278806070012,
115.516712509869)) ;
#167718 = CARTESIAN_POINT('Ctrl Pts',(-22.2635497289195,-13.8582073621022,
115.582834386206)) ;
#167719 = CARTESIAN_POINT('Ctrl Pts',(-22.2852586524313,-13.8885341172032,
115.648956262542)) ;
#167720 = CARTESIAN_POINT('Ctrl Pts',(-22.2114548219404,-13.8885340246808,
115.673187343608)) ;
#167721 = CARTESIAN_POINT('Ctrl Pts',(-22.1376509914495,-13.8885339321583,
115.697418424673)) ;
#167722 = CARTESIAN_POINT('Ctrl Pts',(-22.1159420679376,-13.8582071770573,
115.631296548337)) ;
#167723 = CARTESIAN_POINT('Ctrl Pts',(-22.0788832137679,-14.1061445299723,
115.482974778229)) ;
#167724 = CARTESIAN_POINT('Ctrl Pts',(-22.0604625649498,-14.0584618505827,
115.426868455962)) ;
#167725 = CARTESIAN_POINT('Ctrl Pts',(-22.134266389145,-14.0584619253186,
115.40263735572)) ;
#167726 = CARTESIAN_POINT('Ctrl Pts',(-22.20807021334,-14.0584620000544,115.378406255479)) ;
#167727 = CARTESIAN_POINT('Ctrl Pts',(-22.2264908621581,-14.106144679444,
115.434512577746)) ;
#167728 = CARTESIAN_POINT('Ctrl Pts',(-22.2449115109762,-14.1538273588336,
115.490618900013)) ;
#167729 = CARTESIAN_POINT('Ctrl Pts',(-22.1711076867811,-14.1538272840978,
115.514850000255)) ;
#167730 = CARTESIAN_POINT('Ctrl Pts',(-22.097303862586,-14.1538272093619,
115.539081100496)) ;
#167731 = CARTESIAN_POINT('Ctrl Pts',(-22.0788832137679,-14.1061445299723,
115.482974778229)) ;
#167732 = CARTESIAN_POINT('Ctrl Pts',(-22.02325368044,-14.3044364274605,115.278182501201)) ;
#167733 = CARTESIAN_POINT('Ctrl Pts',(-22.0094209261797,-14.2428379118998,
115.236050165413)) ;
#167734 = CARTESIAN_POINT('Ctrl Pts',(-22.0832247460729,-14.2428379649648,
115.211819052068)) ;
#167735 = CARTESIAN_POINT('Ctrl Pts',(-22.157028565966,-14.2428380180299,
115.187587938724)) ;
#167736 = CARTESIAN_POINT('Ctrl Pts',(-22.1708613202263,-14.3044365335905,
115.229720274512)) ;
#167737 = CARTESIAN_POINT('Ctrl Pts',(-22.1846940744866,-14.3660350491512,
115.271852610301)) ;
#167738 = CARTESIAN_POINT('Ctrl Pts',(-22.1108902545935,-14.3660349960862,
115.296083723645)) ;
#167739 = CARTESIAN_POINT('Ctrl Pts',(-22.0370864347003,-14.3660349430211,
115.32031483699)) ;
#167740 = CARTESIAN_POINT('Ctrl Pts',(-22.02325368044,-14.3044364274605,115.278182501201)) ;
#167741 = CARTESIAN_POINT('Ctrl Pts',(-21.9534860382684,-14.4399899755949,
115.030260894437)) ;
#167742 = CARTESIAN_POINT('Ctrl Pts',(-21.9452364473927,-14.3688346755136,
115.005133973366)) ;
#167743 = CARTESIAN_POINT('Ctrl Pts',(-22.0190402654135,-14.3688347045207,
114.980902854319)) ;
#167744 = CARTESIAN_POINT('Ctrl Pts',(-22.0928440834343,-14.3688347335278,
114.956671735271)) ;
#167745 = CARTESIAN_POINT('Ctrl Pts',(-22.10109367431,-14.4399900336091,114.981798656342)) ;
#167746 = CARTESIAN_POINT('Ctrl Pts',(-22.1093432651856,-14.5111453336905,
115.006925577413)) ;
#167747 = CARTESIAN_POINT('Ctrl Pts',(-22.0355394471648,-14.5111453046834,
115.03115669646)) ;
#167748 = CARTESIAN_POINT('Ctrl Pts',(-21.961735629144,-14.5111452756763,
115.055387815508)) ;
#167749 = CARTESIAN_POINT('Ctrl Pts',(-21.9534860382684,-14.4399899755949,
115.030260894437)) ;
#167750 = CARTESIAN_POINT('Ctrl Pts',(-21.8748683527051,-14.5025588290042,
114.755160393342)) ;
#167751 = CARTESIAN_POINT('Ctrl Pts',(-21.8728327619573,-14.4269270667857,
114.748960313873)) ;
#167752 = CARTESIAN_POINT('Ctrl Pts',(-21.9466365811031,-14.4269270722705,
114.724729198252)) ;
#167753 = CARTESIAN_POINT('Ctrl Pts',(-22.0204404002489,-14.4269270777552,
114.700498082631)) ;
#167754 = CARTESIAN_POINT('Ctrl Pts',(-22.0224759909966,-14.5025588399736,
114.7066981621)) ;
#167755 = CARTESIAN_POINT('Ctrl Pts',(-22.0245115817444,-14.5781906021921,
114.71289824157)) ;
#167756 = CARTESIAN_POINT('Ctrl Pts',(-21.9507077625986,-14.5781905967074,
114.737129357191)) ;
#167757 = CARTESIAN_POINT('Ctrl Pts',(-21.8769039434528,-14.5781905912227,
114.761360472812)) ;
#167758 = CARTESIAN_POINT('Ctrl Pts',(-21.8748683527051,-14.5025588290042,
114.755160393342)) ;
#167759 = CARTESIAN_POINT('Ctrl Pts',(-21.7947021537826,-14.4867545034676,
114.475532312766)) ;
#167760 = CARTESIAN_POINT('Ctrl Pts',(-21.7989943291188,-14.4121117686934,
114.488605587658)) ;
#167761 = CARTESIAN_POINT('Ctrl Pts',(-21.8727981510333,-14.4121117549338,
114.46437448047)) ;
#167762 = CARTESIAN_POINT('Ctrl Pts',(-21.9466019729478,-14.4121117411741,
114.440143373282)) ;
#167763 = CARTESIAN_POINT('Ctrl Pts',(-21.9423097976117,-14.4867544759483,
114.42707009839)) ;
#167764 = CARTESIAN_POINT('Ctrl Pts',(-21.9380176222755,-14.5613972107224,
114.413996823498)) ;
#167765 = CARTESIAN_POINT('Ctrl Pts',(-21.864213800361,-14.5613972244821,
114.438227930686)) ;
#167766 = CARTESIAN_POINT('Ctrl Pts',(-21.7904099784465,-14.5613972382417,
114.462459037874)) ;
#167767 = CARTESIAN_POINT('Ctrl Pts',(-21.7947021537826,-14.4867545034676,
114.475532312766)) ;
#167768 = CARTESIAN_POINT('Ctrl Pts',(-21.7193075294336,-14.395053842158,
114.210551242128)) ;
#167769 = CARTESIAN_POINT('Ctrl Pts',(-21.7296015565806,-14.3267009786415,
114.241905189105)) ;
#167770 = CARTESIAN_POINT('Ctrl Pts',(-21.8034053823653,-14.3267009501932,
114.217674093705)) ;
#167771 = CARTESIAN_POINT('Ctrl Pts',(-21.8772092081501,-14.3267009217449,
114.193442998305)) ;
#167772 = CARTESIAN_POINT('Ctrl Pts',(-21.866915181003,-14.3950537852614,
114.162089051328)) ;
#167773 = CARTESIAN_POINT('Ctrl Pts',(-21.856621153856,-14.463406648778,114.130735104351)) ;
#167774 = CARTESIAN_POINT('Ctrl Pts',(-21.7828173280713,-14.4634066772262,
114.154966199751)) ;
#167775 = CARTESIAN_POINT('Ctrl Pts',(-21.7090135022865,-14.4634067056745,
114.179197295151)) ;
#167776 = CARTESIAN_POINT('Ctrl Pts',(-21.7193075294336,-14.395053842158,
114.210551242128)) ;
#167777 = CARTESIAN_POINT('Ctrl Pts',(-21.6543128388828,-14.2332235226471,
113.977125631216)) ;
#167778 = CARTESIAN_POINT('Ctrl Pts',(-21.6698942629534,-14.1760661182545,
114.02458413594)) ;
#167779 = CARTESIAN_POINT('Ctrl Pts',(-21.7436980937312,-14.1760660813659,
114.000353055749)) ;
#167780 = CARTESIAN_POINT('Ctrl Pts',(-21.8175019245091,-14.1760660444773,
113.976121975557)) ;
#167781 = CARTESIAN_POINT('Ctrl Pts',(-21.8019205004385,-14.2332234488699,
113.928663470833)) ;
#167782 = CARTESIAN_POINT('Ctrl Pts',(-21.786339076368,-14.2903808532625,
113.881204966109)) ;
#167783 = CARTESIAN_POINT('Ctrl Pts',(-21.7125352455901,-14.2903808901511,
113.905436046301)) ;
#167784 = CARTESIAN_POINT('Ctrl Pts',(-21.6387314148122,-14.2903809270397,
113.929667126492)) ;
#167785 = CARTESIAN_POINT('Ctrl Pts',(-21.6543128388828,-14.2332235226471,
113.977125631216)) ;
#167786 = CARTESIAN_POINT('Ctrl Pts',(-21.605413342524,-14.0127300062097,
113.792696033333)) ;
#167787 = CARTESIAN_POINT('Ctrl Pts',(-21.6251670568667,-13.9708810531426,
113.852862660857)) ;
#167788 = CARTESIAN_POINT('Ctrl Pts',(-21.6989708926631,-13.9708810143348,
113.828631595951)) ;
#167789 = CARTESIAN_POINT('Ctrl Pts',(-21.7727747284595,-13.9708809755269,
113.804400531044)) ;
#167790 = CARTESIAN_POINT('Ctrl Pts',(-21.7530210141168,-14.0127299285939,
113.744233903521)) ;
#167791 = CARTESIAN_POINT('Ctrl Pts',(-21.7332672997741,-14.054578881661,
113.684067275997)) ;
#167792 = CARTESIAN_POINT('Ctrl Pts',(-21.6594634639777,-14.0545789204688,
113.708298340903)) ;
#167793 = CARTESIAN_POINT('Ctrl Pts',(-21.5856596281813,-14.0545789592767,
113.732529405809)) ;
#167794 = CARTESIAN_POINT('Ctrl Pts',(-21.605413342524,-14.0127300062097,
113.792696033333)) ;
#167795 = CARTESIAN_POINT('Ctrl Pts',(-21.5768555726489,-13.7497867225439,
113.670246591571)) ;
#167796 = CARTESIAN_POINT('Ctrl Pts',(-21.5993671606262,-13.7262335262759,
113.738813257035)) ;
#167797 = CARTESIAN_POINT('Ctrl Pts',(-21.6731710007795,-13.7262334907042,
113.7145822054)) ;
#167798 = CARTESIAN_POINT('Ctrl Pts',(-21.7469748409328,-13.7262334551324,
113.690351153764)) ;
#167799 = CARTESIAN_POINT('Ctrl Pts',(-21.7244632529556,-13.7497866514004,
113.6217844883)) ;
#167800 = CARTESIAN_POINT('Ctrl Pts',(-21.7019516649783,-13.7733398476684,
113.553217822836)) ;
#167801 = CARTESIAN_POINT('Ctrl Pts',(-21.628147824825,-13.7733398832402,
113.577448874471)) ;
#167802 = CARTESIAN_POINT('Ctrl Pts',(-21.5543439846717,-13.7733399188119,
113.601679926107)) ;
#167803 = CARTESIAN_POINT('Ctrl Pts',(-21.5768555726489,-13.7497867225439,
113.670246591571)) ;
#167804 = CARTESIAN_POINT('Ctrl Pts',(-21.5715836653068,-13.4618226176213,
113.618571162712)) ;
#167805 = CARTESIAN_POINT('Ctrl Pts',(-21.5952346989203,-13.4583403895165,
113.690608395545)) ;
#167806 = CARTESIAN_POINT('Ctrl Pts',(-21.6690385421918,-13.458340362269,
113.666377353407)) ;
#167807 = CARTESIAN_POINT('Ctrl Pts',(-21.7428423854632,-13.4583403350215,
113.642146311268)) ;
#167808 = CARTESIAN_POINT('Ctrl Pts',(-21.7191913518496,-13.4618225631264,
113.570109078435)) ;
#167809 = CARTESIAN_POINT('Ctrl Pts',(-21.6955403182359,-13.4653047912312,
113.498071845602)) ;
#167810 = CARTESIAN_POINT('Ctrl Pts',(-21.6217364749645,-13.4653048184787,
113.52230288774)) ;
#167811 = CARTESIAN_POINT('Ctrl Pts',(-21.5479326316931,-13.4653048457262,
113.546533929879)) ;
#167812 = CARTESIAN_POINT('Ctrl Pts',(-21.5715836653068,-13.4618226176213,
113.618571162712)) ;
#167813 = CARTESIAN_POINT('Ctrl Pts',(-21.5903574401915,-13.1741720910159,
113.64057286247)) ;
#167814 = CARTESIAN_POINT('Ctrl Pts',(-21.6134611754768,-13.1907692085376,
113.710943112796)) ;
#167815 = CARTESIAN_POINT('Ctrl Pts',(-21.6872650205988,-13.1907691874801,
113.686712076294)) ;
#167816 = CARTESIAN_POINT('Ctrl Pts',(-21.7610688657208,-13.1907691664227,
113.662481039792)) ;
#167817 = CARTESIAN_POINT('Ctrl Pts',(-21.7379651304355,-13.1741720489011,
113.592110789466)) ;
#167818 = CARTESIAN_POINT('Ctrl Pts',(-21.7148613951501,-13.1575749313794,
113.52174053914)) ;
#167819 = CARTESIAN_POINT('Ctrl Pts',(-21.6410575500281,-13.1575749524368,
113.545971575642)) ;
#167820 = CARTESIAN_POINT('Ctrl Pts',(-21.5672537049062,-13.1575749734943,
113.570202612144)) ;
#167821 = CARTESIAN_POINT('Ctrl Pts',(-21.5903574401915,-13.1741720910159,
113.64057286247)) ;
#167822 = CARTESIAN_POINT('Ctrl Pts',(-21.6331211640016,-12.9003777795887,
113.735179592382)) ;
#167823 = CARTESIAN_POINT('Ctrl Pts',(-21.654011633631,-12.9361179634059,
113.798808592458)) ;
#167824 = CARTESIAN_POINT('Ctrl Pts',(-21.7278154791519,-12.9361179523589,
113.774577557172)) ;
#167825 = CARTESIAN_POINT('Ctrl Pts',(-21.8016193246729,-12.9361179413118,
113.750346521885)) ;
#167826 = CARTESIAN_POINT('Ctrl Pts',(-21.7807288550435,-12.9003777574947,
113.686717521809)) ;
#167827 = CARTESIAN_POINT('Ctrl Pts',(-21.759838385414,-12.8646375736775,
113.623088521733)) ;
#167828 = CARTESIAN_POINT('Ctrl Pts',(-21.6860345398931,-12.8646375847245,
113.64731955702)) ;
#167829 = CARTESIAN_POINT('Ctrl Pts',(-21.6122306943722,-12.8646375957715,
113.671550592306)) ;
#167830 = CARTESIAN_POINT('Ctrl Pts',(-21.6331211640016,-12.9003777795887,
113.735179592382)) ;
#167831 = CARTESIAN_POINT('Ctrl Pts',(-21.6969659859909,-12.6657294356323,
113.89428002861)) ;
#167832 = CARTESIAN_POINT('Ctrl Pts',(-21.7141616319594,-12.7179077722526,
113.946655191865)) ;
#167833 = CARTESIAN_POINT('Ctrl Pts',(-21.7879654770538,-12.7179077672934,
113.922424155279)) ;
#167834 = CARTESIAN_POINT('Ctrl Pts',(-21.8617693221483,-12.7179077623343,
113.898193118693)) ;
#167835 = CARTESIAN_POINT('Ctrl Pts',(-21.8445736761798,-12.665729425714,
113.845817955438)) ;
#167836 = CARTESIAN_POINT('Ctrl Pts',(-21.8273780302113,-12.6135510890938,
113.793442792184)) ;
#167837 = CARTESIAN_POINT('Ctrl Pts',(-21.7535741851169,-12.6135510940529,
113.81767382877)) ;
#167838 = CARTESIAN_POINT('Ctrl Pts',(-21.6797703400225,-12.6135510990121,
113.841904865355)) ;
#167839 = CARTESIAN_POINT('Ctrl Pts',(-21.6969659859909,-12.6657294356323,
113.89428002861)) ;
#167840 = CARTESIAN_POINT('Ctrl Pts',(-21.778661308746,-12.4838951882172,
114.107573907655)) ;
#167841 = CARTESIAN_POINT('Ctrl Pts',(-21.7909137057025,-12.5488490680583,
114.144892731903)) ;
#167842 = CARTESIAN_POINT('Ctrl Pts',(-21.8647175496609,-12.5488490674887,
114.120661691857)) ;
#167843 = CARTESIAN_POINT('Ctrl Pts',(-21.9385213936193,-12.5488490669192,
114.096430651811)) ;
#167844 = CARTESIAN_POINT('Ctrl Pts',(-21.9262689966628,-12.4838951870781,
114.059111827563)) ;
#167845 = CARTESIAN_POINT('Ctrl Pts',(-21.9140165997062,-12.418941307237,
114.021793003316)) ;
#167846 = CARTESIAN_POINT('Ctrl Pts',(-21.8402127557478,-12.4189413078066,
114.046024043362)) ;
#167847 = CARTESIAN_POINT('Ctrl Pts',(-21.7664089117894,-12.4189413083761,
114.070255083408)) ;
#167848 = CARTESIAN_POINT('Ctrl Pts',(-21.778661308746,-12.4838951882172,
114.107573907655)) ;
#167849 = CARTESIAN_POINT('Ctrl Pts',(-21.8724459100831,-12.3696269961183,
114.357853657507)) ;
#167850 = CARTESIAN_POINT('Ctrl Pts',(-21.8788999247854,-12.4426568392055,
114.377511544911)) ;
#167851 = CARTESIAN_POINT('Ctrl Pts',(-21.9527037677865,-12.4426568397969,
114.353280501949)) ;
#167852 = CARTESIAN_POINT('Ctrl Pts',(-22.0265076107875,-12.4426568403884,
114.329049458987)) ;
#167853 = CARTESIAN_POINT('Ctrl Pts',(-22.0200535960851,-12.3696269973012,
114.309391571583)) ;
#167854 = CARTESIAN_POINT('Ctrl Pts',(-22.0135995813828,-12.2965971542141,
114.289733684178)) ;
#167855 = CARTESIAN_POINT('Ctrl Pts',(-21.9397957383818,-12.2965971536226,
114.31396472714)) ;
#167856 = CARTESIAN_POINT('Ctrl Pts',(-21.8659918953808,-12.2965971530311,
114.338195770102)) ;
#167857 = CARTESIAN_POINT('Ctrl Pts',(-21.8724459100831,-12.3696269961183,
114.357853657507)) ;
#167858 = CARTESIAN_POINT('Ctrl Pts',(-21.9730577437289,-12.3300023799241,
114.628793507168)) ;
#167859 = CARTESIAN_POINT('Ctrl Pts',(-21.973230577012,-12.4059080645877,
114.629319929397)) ;
#167860 = CARTESIAN_POINT('Ctrl Pts',(-22.0470344193771,-12.4059080646803,
114.605088884498)) ;
#167861 = CARTESIAN_POINT('Ctrl Pts',(-22.1208382617422,-12.4059080647729,
114.580857839599)) ;
#167862 = CARTESIAN_POINT('Ctrl Pts',(-22.1206654284592,-12.3300023801093,
114.58033141737)) ;
#167863 = CARTESIAN_POINT('Ctrl Pts',(-22.120492595176,-12.2540966954457,
114.579804995141)) ;
#167864 = CARTESIAN_POINT('Ctrl Pts',(-22.0466887528109,-12.2540966953531,
114.60403604004)) ;
#167865 = CARTESIAN_POINT('Ctrl Pts',(-21.9728849104458,-12.2540966952605,
114.628267084938)) ;
#167866 = CARTESIAN_POINT('Ctrl Pts',(-21.9730577437289,-12.3300023799241,
114.628793507168)) ;
#167867 = CARTESIAN_POINT('Ctrl Pts',(-22.0736203367957,-12.3684199778557,
114.899625493982)) ;
#167868 = CARTESIAN_POINT('Ctrl Pts',(-22.0675051364082,-12.4417552779972,
114.88099958023)) ;
#167869 = CARTESIAN_POINT('Ctrl Pts',(-22.1413089789616,-12.4417552770606,
114.856768535904)) ;
#167870 = CARTESIAN_POINT('Ctrl Pts',(-22.215112821515,-12.441755276124,114.832537491579)) ;
#167871 = CARTESIAN_POINT('Ctrl Pts',(-22.2212280219025,-12.3684199759825,
114.851163405331)) ;
#167872 = CARTESIAN_POINT('Ctrl Pts',(-22.2273432222899,-12.2950846758409,
114.869789319083)) ;
#167873 = CARTESIAN_POINT('Ctrl Pts',(-22.1535393797365,-12.2950846767775,
114.894020363408)) ;
#167874 = CARTESIAN_POINT('Ctrl Pts',(-22.0797355371831,-12.2950846777141,
114.918251407734)) ;
#167875 = CARTESIAN_POINT('Ctrl Pts',(-22.0736203367957,-12.3684199778557,
114.899625493982)) ;
#167876 = CARTESIAN_POINT('Ctrl Pts',(-22.168037726153,-12.4825669571575,
115.151626856521)) ;
#167877 = CARTESIAN_POINT('Ctrl Pts',(-22.1560567891196,-12.5480396537864,
115.115134855438)) ;
#167878 = CARTESIAN_POINT('Ctrl Pts',(-22.2298606326288,-12.5480396536061,
115.090903814024)) ;
#167879 = CARTESIAN_POINT('Ctrl Pts',(-22.303664476138,-12.5480396534258,
115.06667277261)) ;
#167880 = CARTESIAN_POINT('Ctrl Pts',(-22.3156454131713,-12.4825669567968,
115.103164773693)) ;
#167881 = CARTESIAN_POINT('Ctrl Pts',(-22.3276263502047,-12.4170942601679,
115.139656774775)) ;
#167882 = CARTESIAN_POINT('Ctrl Pts',(-22.2538225066955,-12.4170942603482,
115.163887816189)) ;
#167883 = CARTESIAN_POINT('Ctrl Pts',(-22.1800186631863,-12.4170942605285,
115.188118857604)) ;
#167884 = CARTESIAN_POINT('Ctrl Pts',(-22.168037726153,-12.4825669571575,
115.151626856521)) ;
#167885 = CARTESIAN_POINT('Ctrl Pts',(-22.2495860805879,-12.6630281231511,
115.364618342181)) ;
#167886 = CARTESIAN_POINT('Ctrl Pts',(-22.2326259100458,-12.7159956192618,
115.312960399306)) ;
#167887 = CARTESIAN_POINT('Ctrl Pts',(-22.3064297544898,-12.7159956220205,
115.288729360739)) ;
#167888 = CARTESIAN_POINT('Ctrl Pts',(-22.3802335989338,-12.7159956247792,
115.264498322172)) ;
#167889 = CARTESIAN_POINT('Ctrl Pts',(-22.3971937694758,-12.6630281286685,
115.316156265047)) ;
#167890 = CARTESIAN_POINT('Ctrl Pts',(-22.4141539400179,-12.6100606325577,
115.367814207921)) ;
#167891 = CARTESIAN_POINT('Ctrl Pts',(-22.3403500955739,-12.610060629799,
115.392045246488)) ;
#167892 = CARTESIAN_POINT('Ctrl Pts',(-22.2665462511299,-12.6100606270403,
115.416276285055)) ;
#167893 = CARTESIAN_POINT('Ctrl Pts',(-22.2495860805879,-12.6630281231511,
115.364618342181)) ;
#167894 = CARTESIAN_POINT('Ctrl Pts',(-22.3138854050452,-12.898267035054,
115.524940420666)) ;
#167895 = CARTESIAN_POINT('Ctrl Pts',(-22.293145904255,-12.9348862826856,
115.461771247767)) ;
#167896 = CARTESIAN_POINT('Ctrl Pts',(-22.3669497493675,-12.9348862916205,
115.437540211236)) ;
#167897 = CARTESIAN_POINT('Ctrl Pts',(-22.44075359448,-12.9348863005553,115.413309174706)) ;
#167898 = CARTESIAN_POINT('Ctrl Pts',(-22.4614930952703,-12.8982670529237,
115.476478347604)) ;
#167899 = CARTESIAN_POINT('Ctrl Pts',(-22.4822325960606,-12.8616478052921,
115.539647520503)) ;
#167900 = CARTESIAN_POINT('Ctrl Pts',(-22.4084287509481,-12.8616477963572,
115.563878557034)) ;
#167901 = CARTESIAN_POINT('Ctrl Pts',(-22.3346249058356,-12.8616477874224,
115.588109593565)) ;
#167902 = CARTESIAN_POINT('Ctrl Pts',(-22.3138854050452,-12.898267035054,
115.524940420666)) ;
#167903 = CARTESIAN_POINT('Ctrl Pts',(-22.3565804412161,-13.1692444185093,
115.619663390432)) ;
#167904 = CARTESIAN_POINT('Ctrl Pts',(-22.3335607360355,-13.1869963126333,
115.549549082981)) ;
#167905 = CARTESIAN_POINT('Ctrl Pts',(-22.4073645807767,-13.186996328282,
115.525318045319)) ;
#167906 = CARTESIAN_POINT('Ctrl Pts',(-22.4811684255178,-13.1869963439306,
115.501087007657)) ;
#167907 = CARTESIAN_POINT('Ctrl Pts',(-22.5041881306984,-13.1692444498067,
115.571201315108)) ;
#167908 = CARTESIAN_POINT('Ctrl Pts',(-22.527207835879,-13.1514925556827,
115.641315622559)) ;
#167909 = CARTESIAN_POINT('Ctrl Pts',(-22.4534039911379,-13.1514925400341,
115.665546660221)) ;
#167910 = CARTESIAN_POINT('Ctrl Pts',(-22.3796001463967,-13.1514925243854,
115.689777697883)) ;
#167911 = CARTESIAN_POINT('Ctrl Pts',(-22.3565804412161,-13.1692444185093,
115.619663390432)) ;
#167912 = CARTESIAN_POINT('Ctrl Pts',(-22.3758900582822,-13.4593682561925,
115.642974281355)) ;
#167913 = CARTESIAN_POINT('Ctrl Pts',(-22.3522233784854,-13.4568887930797,
115.570889393765)) ;
#167914 = CARTESIAN_POINT('Ctrl Pts',(-22.4260272218503,-13.4568888172156,
115.546658351912)) ;
#167915 = CARTESIAN_POINT('Ctrl Pts',(-22.4998310652151,-13.4568888413516,
115.522427310058)) ;
#167916 = CARTESIAN_POINT('Ctrl Pts',(-22.5234977450119,-13.4593683044645,
115.594512197648)) ;
#167917 = CARTESIAN_POINT('Ctrl Pts',(-22.5471644248086,-13.4618477675773,
115.666597085238)) ;
#167918 = CARTESIAN_POINT('Ctrl Pts',(-22.4733605814438,-13.4618477434414,
115.690828127091)) ;
#167919 = CARTESIAN_POINT('Ctrl Pts',(-22.399556738079,-13.4618477193054,
115.715059168945)) ;
#167920 = CARTESIAN_POINT('Ctrl Pts',(-22.3758900582822,-13.4593682561925,
115.642974281355)) ;
#167921 = CARTESIAN_POINT('Ctrl Pts',(-22.3707818364666,-13.7466998259824,
115.591894004533)) ;
#167922 = CARTESIAN_POINT('Ctrl Pts',(-22.3481725681148,-13.7241548771273,
115.523029821762)) ;
#167923 = CARTESIAN_POINT('Ctrl Pts',(-22.4219764086385,-13.7241549087659,
115.498798771254)) ;
#167924 = CARTESIAN_POINT('Ctrl Pts',(-22.4957802491622,-13.7241549404046,
115.474567720747)) ;
#167925 = CARTESIAN_POINT('Ctrl Pts',(-22.5183895175141,-13.7466998892598,
115.543431903518)) ;
#167926 = CARTESIAN_POINT('Ctrl Pts',(-22.5409987858659,-13.7692448381149,
115.612296086289)) ;
#167927 = CARTESIAN_POINT('Ctrl Pts',(-22.4671949453422,-13.7692448064763,
115.636527136796)) ;
#167928 = CARTESIAN_POINT('Ctrl Pts',(-22.3933911048185,-13.7692447748376,
115.660758187303)) ;
#167929 = CARTESIAN_POINT('Ctrl Pts',(-22.3707818364666,-13.7466998259824,
115.591894004533)) ;
#167930 = CARTESIAN_POINT('Ctrl Pts',(-22.3425575296485,-14.0096322945866,
115.470512365556)) ;
#167931 = CARTESIAN_POINT('Ctrl Pts',(-22.3226190812992,-13.9686968355008,
115.409783069735)) ;
#167932 = CARTESIAN_POINT('Ctrl Pts',(-22.396422917929,-13.9686968703367,
115.385552007367)) ;
#167933 = CARTESIAN_POINT('Ctrl Pts',(-22.4702267545589,-13.9686969051726,
115.361320945)) ;
#167934 = CARTESIAN_POINT('Ctrl Pts',(-22.4901652029082,-14.0096323642584,
115.422050240821)) ;
#167935 = CARTESIAN_POINT('Ctrl Pts',(-22.5101036512575,-14.0505678233442,
115.482779536643)) ;
#167936 = CARTESIAN_POINT('Ctrl Pts',(-22.4362998146277,-14.0505677885083,
115.50701059901)) ;
#167937 = CARTESIAN_POINT('Ctrl Pts',(-22.3624959779978,-14.0505677536723,
115.531241661378)) ;
#167938 = CARTESIAN_POINT('Ctrl Pts',(-22.3425575296485,-14.0096322945866,
115.470512365556)) ;
#167939 = CARTESIAN_POINT('Ctrl Pts',(-22.2939191122543,-14.2308164989726,
115.286886571348)) ;
#167940 = CARTESIAN_POINT('Ctrl Pts',(-22.2780819245253,-14.1743789457168,
115.238649053812)) ;
#167941 = CARTESIAN_POINT('Ctrl Pts',(-22.3518857564706,-14.1743789796015,
115.214417977176)) ;
#167942 = CARTESIAN_POINT('Ctrl Pts',(-22.4256895884157,-14.1743790134861,
115.19018690054)) ;
#167943 = CARTESIAN_POINT('Ctrl Pts',(-22.4415267761447,-14.2308165667419,
115.238424418076)) ;
#167944 = CARTESIAN_POINT('Ctrl Pts',(-22.4573639638737,-14.2872541199976,
115.286661935612)) ;
#167945 = CARTESIAN_POINT('Ctrl Pts',(-22.3835601319285,-14.287254086113,
115.310893012248)) ;
#167946 = CARTESIAN_POINT('Ctrl Pts',(-22.3097562999833,-14.2872540522283,
115.335124088884)) ;
#167947 = CARTESIAN_POINT('Ctrl Pts',(-22.2939191122543,-14.2308164989726,
115.286886571348)) ;
#167948 = CARTESIAN_POINT('Ctrl Pts',(-22.2288101941412,-14.3939170940553,
115.052972439355)) ;
#167949 = CARTESIAN_POINT('Ctrl Pts',(-22.2182325563075,-14.3260101541607,
115.020754662367)) ;
#167950 = CARTESIAN_POINT('Ctrl Pts',(-22.2920363830491,-14.3260101812409,
114.996523569882)) ;
#167951 = CARTESIAN_POINT('Ctrl Pts',(-22.3658402097907,-14.3260102083211,
114.972292477396)) ;
#167952 = CARTESIAN_POINT('Ctrl Pts',(-22.3764178476244,-14.3939171482158,
115.004510254384)) ;
#167953 = CARTESIAN_POINT('Ctrl Pts',(-22.386995485458,-14.4618240881105,
115.036728031371)) ;
#167954 = CARTESIAN_POINT('Ctrl Pts',(-22.3131916587164,-14.4618240610302,
115.060959123857)) ;
#167955 = CARTESIAN_POINT('Ctrl Pts',(-22.2393878319748,-14.46182403395,115.085190216342)) ;
#167956 = CARTESIAN_POINT('Ctrl Pts',(-22.2288101941412,-14.3939170940553,
115.052972439355)) ;
#167957 = CARTESIAN_POINT('Ctrl Pts',(-22.1536104156,-14.4862563732453,114.788647345672)) ;
#167958 = CARTESIAN_POINT('Ctrl Pts',(-22.1489978393131,-14.411804800515,
114.774598183824)) ;
#167959 = CARTESIAN_POINT('Ctrl Pts',(-22.2228016623764,-14.4118048137988,
114.750367080135)) ;
#167960 = CARTESIAN_POINT('Ctrl Pts',(-22.2966054854396,-14.4118048270827,
114.726135976446)) ;
#167961 = CARTESIAN_POINT('Ctrl Pts',(-22.3012180617265,-14.486256399813,
114.740185138294)) ;
#167962 = CARTESIAN_POINT('Ctrl Pts',(-22.3058306380133,-14.5607079725433,
114.754234300141)) ;
#167963 = CARTESIAN_POINT('Ctrl Pts',(-22.2320268149501,-14.5607079592595,
114.77846540383)) ;
#167964 = CARTESIAN_POINT('Ctrl Pts',(-22.1582229918869,-14.5607079459756,
114.802696507519)) ;
#167965 = CARTESIAN_POINT('Ctrl Pts',(-22.1536104156,-14.4862563732453,114.788647345672)) ;
#167966 = CARTESIAN_POINT('Ctrl Pts',(-22.0731223082853,-14.5025873133897,
114.507882396618)) ;
#167967 = CARTESIAN_POINT('Ctrl Pts',(-22.0748593506673,-14.4268872889833,
114.513173148907)) ;
#167968 = CARTESIAN_POINT('Ctrl Pts',(-22.1486631705148,-14.4268872836565,
114.488942035423)) ;
#167969 = CARTESIAN_POINT('Ctrl Pts',(-22.2224669903623,-14.4268872783298,
114.464710921939)) ;
#167970 = CARTESIAN_POINT('Ctrl Pts',(-22.2207299479803,-14.5025873027362,
114.45942016965)) ;
#167971 = CARTESIAN_POINT('Ctrl Pts',(-22.2189929055983,-14.5782873271426,
114.454129417361)) ;
#167972 = CARTESIAN_POINT('Ctrl Pts',(-22.1451890857508,-14.5782873324694,
114.478360530845)) ;
#167973 = CARTESIAN_POINT('Ctrl Pts',(-22.0713852659033,-14.5782873377961,
114.502591644329)) ;
#167974 = CARTESIAN_POINT('Ctrl Pts',(-22.0731223082853,-14.5025873133897,
114.507882396618)) ;
#167975 = CARTESIAN_POINT('Ctrl Pts',(-21.9952150839896,-14.4415569455837,
114.235304068453)) ;
#167976 = CARTESIAN_POINT('Ctrl Pts',(-22.0031240160095,-14.3700086479268,
114.259393400862)) ;
#167977 = CARTESIAN_POINT('Ctrl Pts',(-22.0769278353894,-14.370008620797,
114.235162285954)) ;
#167978 = CARTESIAN_POINT('Ctrl Pts',(-22.1507316547692,-14.3700085936673,
114.210931171046)) ;
#167979 = CARTESIAN_POINT('Ctrl Pts',(-22.1428227227493,-14.4415568913242,
114.186841838637)) ;
#167980 = CARTESIAN_POINT('Ctrl Pts',(-22.1349137907294,-14.5131051889812,
114.162752506228)) ;
#167981 = CARTESIAN_POINT('Ctrl Pts',(-22.0611099713496,-14.5131052161109,
114.186983621136)) ;
#167982 = CARTESIAN_POINT('Ctrl Pts',(-21.9873061519697,-14.5131052432407,
114.211214736044)) ;
#167983 = CARTESIAN_POINT('Ctrl Pts',(-21.9952150839896,-14.4415569455837,
114.235304068453)) ;
#167984 = CARTESIAN_POINT('Ctrl Pts',(-21.9247229138988,-14.3059463498269,
113.984884763739)) ;
#167985 = CARTESIAN_POINT('Ctrl Pts',(-21.9383038334394,-14.2437611215803,
114.026250055128)) ;
#167986 = CARTESIAN_POINT('Ctrl Pts',(-22.0121076538114,-14.2437610699902,
114.002018943242)) ;
#167987 = CARTESIAN_POINT('Ctrl Pts',(-22.0859114741834,-14.2437610184,113.977787831356)) ;
#167988 = CARTESIAN_POINT('Ctrl Pts',(-22.0723305546428,-14.3059462466466,
113.936422539967)) ;
#167989 = CARTESIAN_POINT('Ctrl Pts',(-22.0587496351021,-14.3681314748932,
113.895057248578)) ;
#167990 = CARTESIAN_POINT('Ctrl Pts',(-21.9849458147301,-14.3681315264833,
113.919288360464)) ;
#167991 = CARTESIAN_POINT('Ctrl Pts',(-21.9111419943582,-14.3681315780735,
113.94351947235)) ;
#167992 = CARTESIAN_POINT('Ctrl Pts',(-21.9247229138988,-14.3059463498269,
113.984884763739)) ;
#167993 = CARTESIAN_POINT('Ctrl Pts',(-21.8690302313287,-14.1081523204692,
113.779936751177)) ;
#167994 = CARTESIAN_POINT('Ctrl Pts',(-21.8872499276746,-14.0596861997997,
113.835431008341)) ;
#167995 = CARTESIAN_POINT('Ctrl Pts',(-21.9610537522494,-14.0596861267513,
113.811199909255)) ;
#167996 = CARTESIAN_POINT('Ctrl Pts',(-22.0348575768242,-14.059686053703,
113.78696881017)) ;
#167997 = CARTESIAN_POINT('Ctrl Pts',(-22.0166378804783,-14.1081521743725,
113.731474553006)) ;
#167998 = CARTESIAN_POINT('Ctrl Pts',(-21.9984181841324,-14.1566182950421,
113.675980295843)) ;
#167999 = CARTESIAN_POINT('Ctrl Pts',(-21.9246143595576,-14.1566183680904,
113.700211394928)) ;
#168000 = CARTESIAN_POINT('Ctrl Pts',(-21.8508105349828,-14.1566184411388,
113.724442494013)) ;
#168001 = CARTESIAN_POINT('Ctrl Pts',(-21.8690302313287,-14.1081523204692,
113.779936751177)) ;
#168002 = CARTESIAN_POINT('Ctrl Pts',(-21.8317929609378,-13.8605107481474,
113.631055122176)) ;
#168003 = CARTESIAN_POINT('Ctrl Pts',(-21.8533727983839,-13.8292631951763,
113.69678382707)) ;
#168004 = CARTESIAN_POINT('Ctrl Pts',(-21.9271766290347,-13.8292631042665,
113.672552746491)) ;
#168005 = CARTESIAN_POINT('Ctrl Pts',(-22.0009804596855,-13.8292630133566,
113.648321665912)) ;
#168006 = CARTESIAN_POINT('Ctrl Pts',(-21.9794006222394,-13.8605105663277,
113.582592961019)) ;
#168007 = CARTESIAN_POINT('Ctrl Pts',(-21.9578207847933,-13.8917581192987,
113.516864256125)) ;
#168008 = CARTESIAN_POINT('Ctrl Pts',(-21.8840169541425,-13.8917582102086,
113.541095336704)) ;
#168009 = CARTESIAN_POINT('Ctrl Pts',(-21.8102131234917,-13.8917583011184,
113.565326417282)) ;
#168010 = CARTESIAN_POINT('Ctrl Pts',(-21.8317929609378,-13.8605107481474,
113.631055122176)) ;
#168011 = CARTESIAN_POINT('Ctrl Pts',(-21.8167817419917,-13.5802159839548,
113.549772204603)) ;
#168012 = CARTESIAN_POINT('Ctrl Pts',(-21.840177115245,-13.5684914929652,
113.621030738711)) ;
#168013 = CARTESIAN_POINT('Ctrl Pts',(-21.9139809537407,-13.5684913902422,
113.596799682027)) ;
#168014 = CARTESIAN_POINT('Ctrl Pts',(-21.9877847922365,-13.5684912875191,
113.572568625343)) ;
#168015 = CARTESIAN_POINT('Ctrl Pts',(-21.9643894189832,-13.5802157785087,
113.501310091235)) ;
#168016 = CARTESIAN_POINT('Ctrl Pts',(-21.94099404573,-13.5919402694983,113.430051557127)) ;
#168017 = CARTESIAN_POINT('Ctrl Pts',(-21.8671902072343,-13.5919403722214,
113.454282613811)) ;
#168018 = CARTESIAN_POINT('Ctrl Pts',(-21.7933863687385,-13.5919404749444,
113.478513670495)) ;
#168019 = CARTESIAN_POINT('Ctrl Pts',(-21.8167817419917,-13.5802159839548,
113.549772204603)) ;
#168020 = CARTESIAN_POINT('Ctrl Pts',(-21.8259670175883,-13.2888355614903,
113.542253086016)) ;
#168021 = CARTESIAN_POINT('Ctrl Pts',(-21.8494900051154,-13.2974368879024,
113.613900312663)) ;
#168022 = CARTESIAN_POINT('Ctrl Pts',(-21.9232938524342,-13.2974367821204,
113.589669282852)) ;
#168023 = CARTESIAN_POINT('Ctrl Pts',(-21.997097699753,-13.2974366763383,
113.565438253042)) ;
#168024 = CARTESIAN_POINT('Ctrl Pts',(-21.973574712226,-13.2888353499262,
113.493791026395)) ;
#168025 = CARTESIAN_POINT('Ctrl Pts',(-21.9500517246989,-13.2802340235141,
113.422143799749)) ;
#168026 = CARTESIAN_POINT('Ctrl Pts',(-21.87624787738,-13.2802341292962,113.446374829559)) ;
#168027 = CARTESIAN_POINT('Ctrl Pts',(-21.8024440300612,-13.2802342350782,
113.47060585937)) ;
#168028 = CARTESIAN_POINT('Ctrl Pts',(-21.8259670175883,-13.2888355614903,
113.542253086016)) ;
#168029 = CARTESIAN_POINT('Ctrl Pts',(-21.8589580647777,-13.0084923611293,
113.607479583454)) ;
#168030 = CARTESIAN_POINT('Ctrl Pts',(-21.8809417628856,-13.0366789477102,
113.674438382918)) ;
#168031 = CARTESIAN_POINT('Ctrl Pts',(-21.9547456189426,-13.0366788478173,
113.650207379723)) ;
#168032 = CARTESIAN_POINT('Ctrl Pts',(-22.0285494749996,-13.0366787479245,
113.625976376527)) ;
#168033 = CARTESIAN_POINT('Ctrl Pts',(-22.0065657768918,-13.0084921613435,
113.559017577064)) ;
#168034 = CARTESIAN_POINT('Ctrl Pts',(-21.9845820787839,-12.9803055747626,
113.4920587776)) ;
#168035 = CARTESIAN_POINT('Ctrl Pts',(-21.9107782227269,-12.9803056746555,
113.516289780796)) ;
#168036 = CARTESIAN_POINT('Ctrl Pts',(-21.8369743666699,-12.9803057745484,
113.540520783991)) ;
#168037 = CARTESIAN_POINT('Ctrl Pts',(-21.8589580647777,-13.0084923611293,
113.607479583454)) ;
#168038 = CARTESIAN_POINT('Ctrl Pts',(-21.9147410221325,-12.7552927085919,
113.741839536219)) ;
#168039 = CARTESIAN_POINT('Ctrl Pts',(-21.9335982548626,-12.8011984065865,
113.799275626608)) ;
#168040 = CARTESIAN_POINT('Ctrl Pts',(-22.0074021188863,-12.8011983205869,
113.775044647678)) ;
#168041 = CARTESIAN_POINT('Ctrl Pts',(-22.0812059829101,-12.8011982345872,
113.750813668748)) ;
#168042 = CARTESIAN_POINT('Ctrl Pts',(-22.06234875018,-12.7552925365926,113.693377578359)) ;
#168043 = CARTESIAN_POINT('Ctrl Pts',(-22.0434915174499,-12.709386838598,
113.635941487971)) ;
#168044 = CARTESIAN_POINT('Ctrl Pts',(-21.9696876534261,-12.7093869245976,
113.660172466901)) ;
#168045 = CARTESIAN_POINT('Ctrl Pts',(-21.8958837894024,-12.7093870105973,
113.68440344583)) ;
#168046 = CARTESIAN_POINT('Ctrl Pts',(-21.9147410221325,-12.7552927085919,
113.741839536219)) ;
#168047 = CARTESIAN_POINT('Ctrl Pts',(-21.9895561849059,-12.5504983058309,
113.934322640531)) ;
#168048 = CARTESIAN_POINT('Ctrl Pts',(-22.0039503096504,-12.6107700146374,
113.978164824106)) ;
#168049 = CARTESIAN_POINT('Ctrl Pts',(-22.0777541799352,-12.6107699496328,
113.953933864246)) ;
#168050 = CARTESIAN_POINT('Ctrl Pts',(-22.1515580502199,-12.6107698846282,
113.929702904386)) ;
#168051 = CARTESIAN_POINT('Ctrl Pts',(-22.1371639254754,-12.5504981758217,
113.885860720812)) ;
#168052 = CARTESIAN_POINT('Ctrl Pts',(-22.1227698007308,-12.4902264670152,
113.842018537237)) ;
#168053 = CARTESIAN_POINT('Ctrl Pts',(-22.048965930446,-12.4902265320198,
113.866249497097)) ;
#168054 = CARTESIAN_POINT('Ctrl Pts',(-21.9751620601613,-12.4902265970244,
113.890480456957)) ;
#168055 = CARTESIAN_POINT('Ctrl Pts',(-21.9895561849059,-12.5504983058309,
113.934322640531)) ;
#168056 = CARTESIAN_POINT('Ctrl Pts',(-22.0795106288401,-12.4070470358761,
114.17271722211)) ;
#168057 = CARTESIAN_POINT('Ctrl Pts',(-22.0883824289903,-12.477423987992,
114.199739295954)) ;
#168058 = CARTESIAN_POINT('Ctrl Pts',(-22.1621863031239,-12.4774239490789,
114.175508347817)) ;
#168059 = CARTESIAN_POINT('Ctrl Pts',(-22.2359901772575,-12.4774239101657,
114.15127739968)) ;
#168060 = CARTESIAN_POINT('Ctrl Pts',(-22.2271183771075,-12.4070469580498,
114.124255325836)) ;
#168061 = CARTESIAN_POINT('Ctrl Pts',(-22.2182465769573,-12.336670005934,
114.097233251992)) ;
#168062 = CARTESIAN_POINT('Ctrl Pts',(-22.1444427028237,-12.3366700448471,
114.121464200129)) ;
#168063 = CARTESIAN_POINT('Ctrl Pts',(-22.07063882869,-12.3366700837602,114.145695148265)) ;
#168064 = CARTESIAN_POINT('Ctrl Pts',(-22.0795106288401,-12.4070470358761,
114.17271722211)) ;
#168065 = CARTESIAN_POINT('Ctrl Pts',(-22.1777882055102,-12.336806735375,
114.436722224739)) ;
#168066 = CARTESIAN_POINT('Ctrl Pts',(-22.180542808377,-12.4121923869935,
114.445112302616)) ;
#168067 = CARTESIAN_POINT('Ctrl Pts',(-22.2543466838533,-12.4121923758419,
114.420881358569)) ;
#168068 = CARTESIAN_POINT('Ctrl Pts',(-22.3281505593297,-12.4121923646903,
114.396650414522)) ;
#168069 = CARTESIAN_POINT('Ctrl Pts',(-22.325395956463,-12.3368067130718,
114.388260336645)) ;
#168070 = CARTESIAN_POINT('Ctrl Pts',(-22.3226413535963,-12.2614210614532,
114.379870258768)) ;
#168071 = CARTESIAN_POINT('Ctrl Pts',(-22.2488374781199,-12.2614210726048,
114.404101202815)) ;
#168072 = CARTESIAN_POINT('Ctrl Pts',(-22.1750336026435,-12.2614210837564,
114.428332146862)) ;
#168073 = CARTESIAN_POINT('Ctrl Pts',(-22.1777882055102,-12.336806735375,
114.436722224739)) ;
#168074 = CARTESIAN_POINT('Ctrl Pts',(-22.2791750260875,-12.343454815208,
114.710038652952)) ;
#168075 = CARTESIAN_POINT('Ctrl Pts',(-22.2755896110811,-12.4184892364302,
114.69911805927)) ;
#168076 = CARTESIAN_POINT('Ctrl Pts',(-22.3493934851188,-12.4184892524871,
114.674887110841)) ;
#168077 = CARTESIAN_POINT('Ctrl Pts',(-22.4231973591565,-12.418489268544,
114.650656162412)) ;
#168078 = CARTESIAN_POINT('Ctrl Pts',(-22.4267827741629,-12.3434548473218,
114.661576756094)) ;
#168079 = CARTESIAN_POINT('Ctrl Pts',(-22.4303681891693,-12.2684204260996,
114.672497349776)) ;
#168080 = CARTESIAN_POINT('Ctrl Pts',(-22.3565643151316,-12.2684204100427,
114.696728298206)) ;
#168081 = CARTESIAN_POINT('Ctrl Pts',(-22.282760441094,-12.2684203939858,
114.720959246635)) ;
#168082 = CARTESIAN_POINT('Ctrl Pts',(-22.2791750260875,-12.343454815208,
114.710038652952)) ;
#168083 = CARTESIAN_POINT('Ctrl Pts',(-22.3767867804856,-12.4274004694333,
114.971842801054)) ;
#168084 = CARTESIAN_POINT('Ctrl Pts',(-22.3671156303644,-12.4966868092395,
114.942386040042)) ;
#168085 = CARTESIAN_POINT('Ctrl Pts',(-22.4409195004905,-12.4966868487172,
114.918155079699)) ;
#168086 = CARTESIAN_POINT('Ctrl Pts',(-22.5147233706166,-12.496686888195,
114.893924119355)) ;
#168087 = CARTESIAN_POINT('Ctrl Pts',(-22.5243945207378,-12.4274005483888,
114.923380880368)) ;
#168088 = CARTESIAN_POINT('Ctrl Pts',(-22.534065670859,-12.3581142085826,
114.95283764138)) ;
#168089 = CARTESIAN_POINT('Ctrl Pts',(-22.460261800733,-12.3581141691049,
114.977068601723)) ;
#168090 = CARTESIAN_POINT('Ctrl Pts',(-22.3864579306068,-12.3581141296271,
115.001299562066)) ;
#168091 = CARTESIAN_POINT('Ctrl Pts',(-22.3767867804856,-12.4274004694333,
114.971842801054)) ;
#168092 = CARTESIAN_POINT('Ctrl Pts',(-22.4641882116034,-12.5821548538746,
115.202603030469)) ;
#168093 = CARTESIAN_POINT('Ctrl Pts',(-22.4491338350531,-12.6407407748519,
115.156749830222)) ;
#168094 = CARTESIAN_POINT('Ctrl Pts',(-22.5229376995646,-12.6407408319528,
115.132518852778)) ;
#168095 = CARTESIAN_POINT('Ctrl Pts',(-22.5967415640761,-12.6407408890538,
115.108287875333)) ;
#168096 = CARTESIAN_POINT('Ctrl Pts',(-22.6117959406265,-12.5821549680765,
115.15414107558)) ;
#168097 = CARTESIAN_POINT('Ctrl Pts',(-22.6268503171768,-12.5235690470992,
115.199994275827)) ;
#168098 = CARTESIAN_POINT('Ctrl Pts',(-22.5530464526653,-12.5235689899983,
115.224225253271)) ;
#168099 = CARTESIAN_POINT('Ctrl Pts',(-22.4792425881538,-12.5235689328973,
115.248456230715)) ;
#168100 = CARTESIAN_POINT('Ctrl Pts',(-22.4641882116034,-12.5821548538746,
115.202603030469)) ;
#168101 = CARTESIAN_POINT('Ctrl Pts',(-22.5360152755925,-12.7965584285917,
115.385946401626)) ;
#168102 = CARTESIAN_POINT('Ctrl Pts',(-22.5166564652332,-12.8402632676504,
115.326982590391)) ;
#168103 = CARTESIAN_POINT('Ctrl Pts',(-22.5904603231125,-12.8402633354297,
115.302751592746)) ;
#168104 = CARTESIAN_POINT('Ctrl Pts',(-22.6642641809918,-12.8402634032089,
115.278520595101)) ;
#168105 = CARTESIAN_POINT('Ctrl Pts',(-22.683622991351,-12.7965585641502,
115.337484406336)) ;
#168106 = CARTESIAN_POINT('Ctrl Pts',(-22.7029818017103,-12.7528537250914,
115.39644821757)) ;
#168107 = CARTESIAN_POINT('Ctrl Pts',(-22.6291779438311,-12.7528536573122,
115.420679215215)) ;
#168108 = CARTESIAN_POINT('Ctrl Pts',(-22.5553740859518,-12.752853589533,
115.444910212861)) ;
#168109 = CARTESIAN_POINT('Ctrl Pts',(-22.5360152755925,-12.7965584285917,
115.385946401626)) ;
#168110 = CARTESIAN_POINT('Ctrl Pts',(-22.587997010465,-13.0557769277784,
115.508794067491)) ;
#168111 = CARTESIAN_POINT('Ctrl Pts',(-22.5657137741848,-13.0814494476449,
115.440922926611)) ;
#168112 = CARTESIAN_POINT('Ctrl Pts',(-22.6395176251257,-13.0814495182785,
115.416691907832)) ;
#168113 = CARTESIAN_POINT('Ctrl Pts',(-22.7133214760666,-13.0814495889122,
115.392460889054)) ;
#168114 = CARTESIAN_POINT('Ctrl Pts',(-22.7356047123469,-13.0557770690457,
115.460332029934)) ;
#168115 = CARTESIAN_POINT('Ctrl Pts',(-22.7578879486272,-13.0301045491793,
115.528203170815)) ;
#168116 = CARTESIAN_POINT('Ctrl Pts',(-22.6840840976862,-13.0301044785456,
115.552434189593)) ;
#168117 = CARTESIAN_POINT('Ctrl Pts',(-22.6102802467453,-13.030104407912,
115.576665208371)) ;
#168118 = CARTESIAN_POINT('Ctrl Pts',(-22.587997010465,-13.0557769277784,
115.508794067491)) ;
#168119 = CARTESIAN_POINT('Ctrl Pts',(-22.6170289999404,-13.3412469909538,
115.561709527004)) ;
#168120 = CARTESIAN_POINT('Ctrl Pts',(-22.593419786976,-13.3470269436932,
115.489799674927)) ;
#168121 = CARTESIAN_POINT('Ctrl Pts',(-22.6672236316055,-13.3470270098198,
115.465568636925)) ;
#168122 = CARTESIAN_POINT('Ctrl Pts',(-22.7410274762349,-13.3470270759464,
115.441337598923)) ;
#168123 = CARTESIAN_POINT('Ctrl Pts',(-22.7646366891993,-13.341247123207,
115.513247451)) ;
#168124 = CARTESIAN_POINT('Ctrl Pts',(-22.7882459021636,-13.3354671704675,
115.585157303077)) ;
#168125 = CARTESIAN_POINT('Ctrl Pts',(-22.7144420575342,-13.335467104341,
115.609388341079)) ;
#168126 = CARTESIAN_POINT('Ctrl Pts',(-22.6406382129048,-13.3354670382144,
115.633619379081)) ;
#168127 = CARTESIAN_POINT('Ctrl Pts',(-22.6170289999404,-13.3412469909538,
115.561709527004)) ;
#168128 = CARTESIAN_POINT('Ctrl Pts',(-22.6217619532277,-13.6316256256215,
115.540686913954)) ;
#168129 = CARTESIAN_POINT('Ctrl Pts',(-22.5985198370732,-13.6171399155478,
115.469895179372)) ;
#168130 = CARTESIAN_POINT('Ctrl Pts',(-22.6723236766946,-13.6171399723523,
115.445664126116)) ;
#168131 = CARTESIAN_POINT('Ctrl Pts',(-22.7461275163159,-13.6171400291567,
115.42143307286)) ;
#168132 = CARTESIAN_POINT('Ctrl Pts',(-22.7693696324704,-13.6316257392305,
115.492224807443)) ;
#168133 = CARTESIAN_POINT('Ctrl Pts',(-22.7926117486249,-13.6461114493042,
115.563016542025)) ;
#168134 = CARTESIAN_POINT('Ctrl Pts',(-22.7188079090035,-13.6461113924997,
115.587247595281)) ;
#168135 = CARTESIAN_POINT('Ctrl Pts',(-22.6450040693822,-13.6461113356952,
115.611478648537)) ;
#168136 = CARTESIAN_POINT('Ctrl Pts',(-22.6217619532277,-13.6316256256215,
115.540686913954)) ;
#168137 = CARTESIAN_POINT('Ctrl Pts',(-22.6026935421642,-13.9070076933881,
115.447135113786)) ;
#168138 = CARTESIAN_POINT('Ctrl Pts',(-22.5814815681784,-13.8732725053054,
115.382526864519)) ;
#168139 = CARTESIAN_POINT('Ctrl Pts',(-22.6552854044309,-13.8732725490148,
115.358295801002)) ;
#168140 = CARTESIAN_POINT('Ctrl Pts',(-22.7290892406833,-13.8732725927241,
115.334064737485)) ;
#168141 = CARTESIAN_POINT('Ctrl Pts',(-22.7503012146691,-13.9070077808067,
115.398672986752)) ;
#168142 = CARTESIAN_POINT('Ctrl Pts',(-22.7715131886548,-13.9407429688894,
115.463281236019)) ;
#168143 = CARTESIAN_POINT('Ctrl Pts',(-22.6977093524024,-13.9407429251801,
115.487512299536)) ;
#168144 = CARTESIAN_POINT('Ctrl Pts',(-22.6239055161499,-13.9407428814708,
115.511743363053)) ;
#168145 = CARTESIAN_POINT('Ctrl Pts',(-22.6026935421642,-13.9070076933881,
115.447135113786)) ;
#168146 = CARTESIAN_POINT('Ctrl Pts',(-22.561780007704,-14.1476875757229,
115.286985040181)) ;
#168147 = CARTESIAN_POINT('Ctrl Pts',(-22.5441277753165,-14.0970962848469,
115.233219189277)) ;
#168148 = CARTESIAN_POINT('Ctrl Pts',(-22.6179316101862,-14.0970963139386,
115.208988121549)) ;
#168149 = CARTESIAN_POINT('Ctrl Pts',(-22.691735445056,-14.0970963430303,
115.18475705382)) ;
#168150 = CARTESIAN_POINT('Ctrl Pts',(-22.7093876774435,-14.1476876339063,
115.238522904724)) ;
#168151 = CARTESIAN_POINT('Ctrl Pts',(-22.7270399098311,-14.1982789247823,
115.292288755627)) ;
#168152 = CARTESIAN_POINT('Ctrl Pts',(-22.6532360749613,-14.1982788956906,
115.316519823355)) ;
#168153 = CARTESIAN_POINT('Ctrl Pts',(-22.5794322400915,-14.1982788665989,
115.340750891084)) ;
#168154 = CARTESIAN_POINT('Ctrl Pts',(-22.561780007704,-14.1476875757229,
115.286985040181)) ;
#168155 = CARTESIAN_POINT('Ctrl Pts',(-22.5030326356716,-14.3351652655006,
115.072661970802)) ;
#168156 = CARTESIAN_POINT('Ctrl Pts',(-22.4901879000911,-14.2714071859544,
115.033538979335)) ;
#168157 = CARTESIAN_POINT('Ctrl Pts',(-22.5639917349384,-14.2714072026928,
115.009307911538)) ;
#168158 = CARTESIAN_POINT('Ctrl Pts',(-22.6377955697856,-14.2714072194312,
114.985076843741)) ;
#168159 = CARTESIAN_POINT('Ctrl Pts',(-22.6506403053661,-14.3351652989775,
115.024199835208)) ;
#168160 = CARTESIAN_POINT('Ctrl Pts',(-22.6634850409466,-14.3989233785238,
115.063322826674)) ;
#168161 = CARTESIAN_POINT('Ctrl Pts',(-22.5896812060994,-14.3989233617854,
115.087553894471)) ;
#168162 = CARTESIAN_POINT('Ctrl Pts',(-22.5158773712521,-14.3989233450469,
115.111784962268)) ;
#168163 = CARTESIAN_POINT('Ctrl Pts',(-22.5030326356716,-14.3351652655006,
115.072661970802)) ;
#168164 = CARTESIAN_POINT('Ctrl Pts',(-22.431285724249,-14.4575099619995,
114.818736284685)) ;
#168165 = CARTESIAN_POINT('Ctrl Pts',(-22.4241636182106,-14.3851129420045,
114.797043499313)) ;
#168166 = CARTESIAN_POINT('Ctrl Pts',(-22.4979674542533,-14.38511294846,114.772812435157)) ;
#168167 = CARTESIAN_POINT('Ctrl Pts',(-22.5717712902961,-14.3851129549154,
114.748581371002)) ;
#168168 = CARTESIAN_POINT('Ctrl Pts',(-22.5788933963345,-14.4575099749105,
114.770274156374)) ;
#168169 = CARTESIAN_POINT('Ctrl Pts',(-22.586015502373,-14.5299069949055,
114.791966941746)) ;
#168170 = CARTESIAN_POINT('Ctrl Pts',(-22.5122116663302,-14.52990698845,114.816198005902)) ;
#168171 = CARTESIAN_POINT('Ctrl Pts',(-22.4384078302875,-14.5299069819946,
114.840429070058)) ;
#168172 = CARTESIAN_POINT('Ctrl Pts',(-22.431285724249,-14.4575099619995,
114.818736284685)) ;
#168173 = CARTESIAN_POINT('Ctrl Pts',(-22.3517910412139,-14.5055206620573,
114.54096052116)) ;
#168174 = CARTESIAN_POINT('Ctrl Pts',(-22.3509465715137,-14.4296611949973,
114.538388403003)) ;
#168175 = CARTESIAN_POINT('Ctrl Pts',(-22.424750410142,-14.4296611947843,
114.514157346723)) ;
#168176 = CARTESIAN_POINT('Ctrl Pts',(-22.4985542487703,-14.4296611945714,
114.489926290442)) ;
#168177 = CARTESIAN_POINT('Ctrl Pts',(-22.4993987184705,-14.5055206616315,
114.492498408599)) ;
#168178 = CARTESIAN_POINT('Ctrl Pts',(-22.5002431881708,-14.5813801286916,
114.495070526755)) ;
#168179 = CARTESIAN_POINT('Ctrl Pts',(-22.4264393495425,-14.5813801289045,
114.519301583036)) ;
#168180 = CARTESIAN_POINT('Ctrl Pts',(-22.3526355109141,-14.5813801291174,
114.543532639316)) ;
#168181 = CARTESIAN_POINT('Ctrl Pts',(-22.3517910412139,-14.5055206620573,
114.54096052116)) ;
#168182 = CARTESIAN_POINT('Ctrl Pts',(-22.2722771348599,-14.4754288487564,
114.263452537845)) ;
#168183 = CARTESIAN_POINT('Ctrl Pts',(-22.2777143862475,-14.4015565166022,
114.280013528463)) ;
#168184 = CARTESIAN_POINT('Ctrl Pts',(-22.3515182267516,-14.4015565138437,
114.255782477895)) ;
#168185 = CARTESIAN_POINT('Ctrl Pts',(-22.4253220672556,-14.4015565110851,
114.231551427328)) ;
#168186 = CARTESIAN_POINT('Ctrl Pts',(-22.419884815868,-14.4754288432393,
114.214990436711)) ;
#168187 = CARTESIAN_POINT('Ctrl Pts',(-22.4144475644804,-14.5493011753935,
114.198429446093)) ;
#168188 = CARTESIAN_POINT('Ctrl Pts',(-22.3406437239764,-14.5493011781521,
114.222660496661)) ;
#168189 = CARTESIAN_POINT('Ctrl Pts',(-22.2668398834723,-14.5493011809106,
114.246891547228)) ;
#168190 = CARTESIAN_POINT('Ctrl Pts',(-22.2722771348599,-14.4754288487564,
114.263452537845)) ;
#168191 = CARTESIAN_POINT('Ctrl Pts',(-22.1980599297582,-14.3696969300058,
114.00189324141)) ;
#168192 = CARTESIAN_POINT('Ctrl Pts',(-22.2094224709354,-14.3030961668257,
114.036501708568)) ;
#168193 = CARTESIAN_POINT('Ctrl Pts',(-22.2832263134077,-14.3030961645972,
114.012270663996)) ;
#168194 = CARTESIAN_POINT('Ctrl Pts',(-22.35703015588,-14.3030961623686,113.988039619424)) ;
#168195 = CARTESIAN_POINT('Ctrl Pts',(-22.3456676147028,-14.3696969255486,
113.953431152266)) ;
#168196 = CARTESIAN_POINT('Ctrl Pts',(-22.3343050735257,-14.4362976887287,
113.918822685108)) ;
#168197 = CARTESIAN_POINT('Ctrl Pts',(-22.2605012310534,-14.4362976909572,
113.94305372968)) ;
#168198 = CARTESIAN_POINT('Ctrl Pts',(-22.1866973885811,-14.4362976931858,
113.967284774253)) ;
#168199 = CARTESIAN_POINT('Ctrl Pts',(-22.1980599297582,-14.3696969300058,
114.00189324141)) ;
#168200 = CARTESIAN_POINT('Ctrl Pts',(-22.1356986945465,-14.1954536297215,
113.776452902693)) ;
#168201 = CARTESIAN_POINT('Ctrl Pts',(-22.1521674655351,-14.1409200386093,
113.826614121888)) ;
#168202 = CARTESIAN_POINT('Ctrl Pts',(-22.2259713091281,-14.1409200387787,
113.802383080729)) ;
#168203 = CARTESIAN_POINT('Ctrl Pts',(-22.2997751527211,-14.1409200389481,
113.77815203957)) ;
#168204 = CARTESIAN_POINT('Ctrl Pts',(-22.2833063817325,-14.1954536300603,
113.727990820375)) ;
#168205 = CARTESIAN_POINT('Ctrl Pts',(-22.266837610744,-14.2499872211724,
113.677829601181)) ;
#168206 = CARTESIAN_POINT('Ctrl Pts',(-22.193033767151,-14.249987221003,113.70206064234)) ;
#168207 = CARTESIAN_POINT('Ctrl Pts',(-22.119229923558,-14.2499872208336,
113.726291683498)) ;
#168208 = CARTESIAN_POINT('Ctrl Pts',(-22.1356986945465,-14.1954536297215,
113.776452902693)) ;
#168209 = CARTESIAN_POINT('Ctrl Pts',(-22.0904372209487,-13.9663067477415,
113.603202833569)) ;
#168210 = CARTESIAN_POINT('Ctrl Pts',(-22.1108234263171,-13.9276927071092,
113.665295925763)) ;
#168211 = CARTESIAN_POINT('Ctrl Pts',(-22.1846272702145,-13.9276927095559,
113.641064885531)) ;
#168212 = CARTESIAN_POINT('Ctrl Pts',(-22.2584311141118,-13.9276927120025,
113.6168338453)) ;
#168213 = CARTESIAN_POINT('Ctrl Pts',(-22.2380449087434,-13.9663067526349,
113.554740753105)) ;
#168214 = CARTESIAN_POINT('Ctrl Pts',(-22.217658703375,-14.0049207932672,
113.492647660911)) ;
#168215 = CARTESIAN_POINT('Ctrl Pts',(-22.1438548594777,-14.0049207908205,
113.516878701143)) ;
#168216 = CARTESIAN_POINT('Ctrl Pts',(-22.0700510155803,-14.0049207883739,
113.541109741375)) ;
#168217 = CARTESIAN_POINT('Ctrl Pts',(-22.0904372209487,-13.9663067477415,
113.603202833569)) ;
#168218 = CARTESIAN_POINT('Ctrl Pts',(-22.0660586940401,-13.6964880977043,
113.493367442293)) ;
#168219 = CARTESIAN_POINT('Ctrl Pts',(-22.088914009386,-13.6766583743927,
113.562981045083)) ;
#168220 = CARTESIAN_POINT('Ctrl Pts',(-22.1627178530358,-13.6766583775101,
113.538750004097)) ;
#168221 = CARTESIAN_POINT('Ctrl Pts',(-22.2365216966856,-13.6766583806274,
113.514518963111)) ;
#168222 = CARTESIAN_POINT('Ctrl Pts',(-22.2136663813398,-13.696488103939,
113.444905360321)) ;
#168223 = CARTESIAN_POINT('Ctrl Pts',(-22.1908110659939,-13.7163178272505,
113.375291757531)) ;
#168224 = CARTESIAN_POINT('Ctrl Pts',(-22.1170072223441,-13.7163178241332,
113.399522798517)) ;
#168225 = CARTESIAN_POINT('Ctrl Pts',(-22.0432033786943,-13.7163178210159,
113.423753839503)) ;
#168226 = CARTESIAN_POINT('Ctrl Pts',(-22.0660586940401,-13.6964880977043,
113.493367442293)) ;
#168227 = CARTESIAN_POINT('Ctrl Pts',(-22.0652380838038,-13.4086720240795,
113.455542704925)) ;
#168228 = CARTESIAN_POINT('Ctrl Pts',(-22.0889152773064,-13.4089104896533,
113.527659616002)) ;
#168229 = CARTESIAN_POINT('Ctrl Pts',(-22.1627191206271,-13.4089104912241,
113.503428574014)) ;
#168230 = CARTESIAN_POINT('Ctrl Pts',(-22.2365229639478,-13.408910492795,
113.479197532026)) ;
#168231 = CARTESIAN_POINT('Ctrl Pts',(-22.2128457704452,-13.4086720272212,
113.407080620949)) ;
#168232 = CARTESIAN_POINT('Ctrl Pts',(-22.1891685769426,-13.4084335616475,
113.334963709871)) ;
#168233 = CARTESIAN_POINT('Ctrl Pts',(-22.1153647336219,-13.4084335600766,
113.359194751859)) ;
#168234 = CARTESIAN_POINT('Ctrl Pts',(-22.0415608903012,-13.4084335585058,
113.383425793848)) ;
#168235 = CARTESIAN_POINT('Ctrl Pts',(-22.0652380838038,-13.4086720240795,
113.455542704925)) ;
#168236 = CARTESIAN_POINT('Ctrl Pts',(-22.0887502249899,-13.1198463580562,
113.49161061441)) ;
#168237 = CARTESIAN_POINT('Ctrl Pts',(-22.11155604208,-13.1402531049797,113.561073453608)) ;
#168238 = CARTESIAN_POINT('Ctrl Pts',(-22.1853598855831,-13.1402531026116,
113.536842412175)) ;
#168239 = CARTESIAN_POINT('Ctrl Pts',(-22.2591637290863,-13.1402531002435,
113.512611370743)) ;
#168240 = CARTESIAN_POINT('Ctrl Pts',(-22.2363579119963,-13.1198463533199,
113.443148531545)) ;
#168241 = CARTESIAN_POINT('Ctrl Pts',(-22.2135520949062,-13.0994396063964,
113.373685692348)) ;
#168242 = CARTESIAN_POINT('Ctrl Pts',(-22.139748251403,-13.0994396087645,
113.39791673378)) ;
#168243 = CARTESIAN_POINT('Ctrl Pts',(-22.0659444078998,-13.0994396111326,
113.422147775213)) ;
#168244 = CARTESIAN_POINT('Ctrl Pts',(-22.0887502249899,-13.1198463580562,
113.49161061441)) ;
#168245 = CARTESIAN_POINT('Ctrl Pts',(-22.1354479268997,-12.8536440540051,
113.598479641973)) ;
#168246 = CARTESIAN_POINT('Ctrl Pts',(-22.1557581310016,-12.8926679376459,
113.660341246762)) ;
#168247 = CARTESIAN_POINT('Ctrl Pts',(-22.2295619753836,-12.8926679313973,
113.636110208007)) ;
#168248 = CARTESIAN_POINT('Ctrl Pts',(-22.3033658197655,-12.8926679251486,
113.611879169251)) ;
#168249 = CARTESIAN_POINT('Ctrl Pts',(-22.2830556156637,-12.8536440415079,
113.550017564462)) ;
#168250 = CARTESIAN_POINT('Ctrl Pts',(-22.2627454115618,-12.8146201578671,
113.488155959672)) ;
#168251 = CARTESIAN_POINT('Ctrl Pts',(-22.1889415671798,-12.8146201641158,
113.512386998428)) ;
#168252 = CARTESIAN_POINT('Ctrl Pts',(-22.1151377227978,-12.8146201703644,
113.536618037184)) ;
#168253 = CARTESIAN_POINT('Ctrl Pts',(-22.1354479268997,-12.8536440540051,
113.598479641973)) ;
#168254 = CARTESIAN_POINT('Ctrl Pts',(-22.2034506138866,-12.6260691585523,
113.769947386255)) ;
#168255 = CARTESIAN_POINT('Ctrl Pts',(-22.2197801294508,-12.6810405314409,
113.819684456192)) ;
#168256 = CARTESIAN_POINT('Ctrl Pts',(-22.2935839760765,-12.6810405208292,
113.79545342427)) ;
#168257 = CARTESIAN_POINT('Ctrl Pts',(-22.3673878227021,-12.6810405102175,
113.771222392348)) ;
#168258 = CARTESIAN_POINT('Ctrl Pts',(-22.3510583071379,-12.6260691373289,
113.721485322411)) ;
#168259 = CARTESIAN_POINT('Ctrl Pts',(-22.3347287915737,-12.5710977644403,
113.671748252474)) ;
#168260 = CARTESIAN_POINT('Ctrl Pts',(-22.2609249449481,-12.571097775052,
113.695979284396)) ;
#168261 = CARTESIAN_POINT('Ctrl Pts',(-22.1871210983224,-12.5710977856637,
113.720210316318)) ;
#168262 = CARTESIAN_POINT('Ctrl Pts',(-22.2034506138866,-12.6260691585523,
113.769947386255)) ;
#168263 = CARTESIAN_POINT('Ctrl Pts',(-22.2875987666924,-12.4569456938658,
113.990878373043)) ;
#168264 = CARTESIAN_POINT('Ctrl Pts',(-22.2988084284199,-12.5238051277268,
114.025021194409)) ;
#168265 = CARTESIAN_POINT('Ctrl Pts',(-22.3726122776629,-12.5238051170314,
114.000790170459)) ;
#168266 = CARTESIAN_POINT('Ctrl Pts',(-22.446416126906,-12.523805106336,113.976559146509)) ;
#168267 = CARTESIAN_POINT('Ctrl Pts',(-22.4352064651785,-12.4569456724751,
113.942416325143)) ;
#168268 = CARTESIAN_POINT('Ctrl Pts',(-22.423996803451,-12.3900862386142,
113.908273503778)) ;
#168269 = CARTESIAN_POINT('Ctrl Pts',(-22.3501929542079,-12.3900862493095,
113.932504527728)) ;
#168270 = CARTESIAN_POINT('Ctrl Pts',(-22.2763891049649,-12.3900862600049,
113.956735551678)) ;
#168271 = CARTESIAN_POINT('Ctrl Pts',(-22.2875987666924,-12.4569456938658,
113.990878373043)) ;
#168272 = CARTESIAN_POINT('Ctrl Pts',(-22.3834860536271,-12.3560371763605,
114.247407246605)) ;
#168273 = CARTESIAN_POINT('Ctrl Pts',(-22.388752146054,-12.4300391766208,
114.263446915039)) ;
#168274 = CARTESIAN_POINT('Ctrl Pts',(-22.4625559985964,-12.43003916942,114.239215901139)) ;
#168275 = CARTESIAN_POINT('Ctrl Pts',(-22.5363598511387,-12.4300391622191,
114.214984887238)) ;
#168276 = CARTESIAN_POINT('Ctrl Pts',(-22.5310937587119,-12.3560371619588,
114.198945218804)) ;
#168277 = CARTESIAN_POINT('Ctrl Pts',(-22.525827666285,-12.2820351616984,
114.182905550369)) ;
#168278 = CARTESIAN_POINT('Ctrl Pts',(-22.4520238137426,-12.2820351688993,
114.20713656427)) ;
#168279 = CARTESIAN_POINT('Ctrl Pts',(-22.3782199612002,-12.2820351761001,
114.23136757817)) ;
#168280 = CARTESIAN_POINT('Ctrl Pts',(-22.3834860536271,-12.3560371763605,
114.247407246605)) ;
#168281 = CARTESIAN_POINT('Ctrl Pts',(-22.4840972968736,-12.3312869891021,
114.51853287169)) ;
#168282 = CARTESIAN_POINT('Ctrl Pts',(-22.4830771493672,-12.407123602134,
114.515425667706)) ;
#168283 = CARTESIAN_POINT('Ctrl Pts',(-22.5568810044093,-12.4071236031691,
114.49119466142)) ;
#168284 = CARTESIAN_POINT('Ctrl Pts',(-22.6306848594514,-12.4071236042042,
114.466963655133)) ;
#168285 = CARTESIAN_POINT('Ctrl Pts',(-22.6317050069579,-12.3312869911723,
114.470070859117)) ;
#168286 = CARTESIAN_POINT('Ctrl Pts',(-22.6327251544643,-12.2554503781403,
114.473178063101)) ;
#168287 = CARTESIAN_POINT('Ctrl Pts',(-22.5589212994222,-12.2554503771052,
114.497409069387)) ;
#168288 = CARTESIAN_POINT('Ctrl Pts',(-22.4851174443801,-12.2554503760701,
114.521640075674)) ;
#168289 = CARTESIAN_POINT('Ctrl Pts',(-22.4840972968736,-12.3312869891021,
114.51853287169)) ;
#168290 = CARTESIAN_POINT('Ctrl Pts',(-22.5844346669737,-12.384579728798,
114.788494098103)) ;
#168291 = CARTESIAN_POINT('Ctrl Pts',(-22.5771451839705,-12.4568056181836,
114.766291509953)) ;
#168292 = CARTESIAN_POINT('Ctrl Pts',(-22.6509490416241,-12.4568056323219,
114.74206051162)) ;
#168293 = CARTESIAN_POINT('Ctrl Pts',(-22.7247528992776,-12.4568056464601,
114.717829513288)) ;
#168294 = CARTESIAN_POINT('Ctrl Pts',(-22.7320423822809,-12.3845797570745,
114.740032101438)) ;
#168295 = CARTESIAN_POINT('Ctrl Pts',(-22.7393318652841,-12.3123538676888,
114.762234689588)) ;
#168296 = CARTESIAN_POINT('Ctrl Pts',(-22.6655280076305,-12.3123538535506,
114.78646568792)) ;
#168297 = CARTESIAN_POINT('Ctrl Pts',(-22.5917241499769,-12.3123538394123,
114.810696686253)) ;
#168298 = CARTESIAN_POINT('Ctrl Pts',(-22.5844346669737,-12.384579728798,
114.788494098103)) ;
#168299 = CARTESIAN_POINT('Ctrl Pts',(-22.6765292835833,-12.5118388251457,
115.033574716962)) ;
#168300 = CARTESIAN_POINT('Ctrl Pts',(-22.6635323516411,-12.5752838792253,
114.993988160397)) ;
#168301 = CARTESIAN_POINT('Ctrl Pts',(-22.7373362097494,-12.5752839097083,
114.96975716345)) ;
#168302 = CARTESIAN_POINT('Ctrl Pts',(-22.8111400678576,-12.5752839401913,
114.945526166502)) ;
#168303 = CARTESIAN_POINT('Ctrl Pts',(-22.8241369997999,-12.5118388861117,
114.985112723066)) ;
#168304 = CARTESIAN_POINT('Ctrl Pts',(-22.8371339317421,-12.448393832032,
115.024699279631)) ;
#168305 = CARTESIAN_POINT('Ctrl Pts',(-22.7633300736338,-12.4483938015491,
115.048930276579)) ;
#168306 = CARTESIAN_POINT('Ctrl Pts',(-22.6895262155256,-12.4483937710661,
115.073161273526)) ;
#168307 = CARTESIAN_POINT('Ctrl Pts',(-22.6765292835833,-12.5118388251457,
115.033574716962)) ;
#168308 = CARTESIAN_POINT('Ctrl Pts',(-22.7552676475542,-12.7038857020727,
115.237944156855)) ;
#168309 = CARTESIAN_POINT('Ctrl Pts',(-22.7374881961524,-12.7540141068732,
115.183790817835)) ;
#168310 = CARTESIAN_POINT('Ctrl Pts',(-22.8112920529231,-12.7540141550584,
115.159559816814)) ;
#168311 = CARTESIAN_POINT('Ctrl Pts',(-22.8850959096938,-12.7540142032436,
115.135328815792)) ;
#168312 = CARTESIAN_POINT('Ctrl Pts',(-22.9028753610955,-12.7038857984431,
115.189482154812)) ;
#168313 = CARTESIAN_POINT('Ctrl Pts',(-22.9206548124973,-12.6537573936426,
115.243635493831)) ;
#168314 = CARTESIAN_POINT('Ctrl Pts',(-22.8468509557266,-12.6537573454574,
115.267866494853)) ;
#168315 = CARTESIAN_POINT('Ctrl Pts',(-22.7730470989559,-12.6537572972722,
115.292097495875)) ;
#168316 = CARTESIAN_POINT('Ctrl Pts',(-22.7552676475542,-12.7038857020727,
115.237944156855)) ;
#168317 = CARTESIAN_POINT('Ctrl Pts',(-22.8155921978644,-12.9467051649881,
115.386282575257)) ;
#168318 = CARTESIAN_POINT('Ctrl Pts',(-22.7943078394483,-12.9799528972862,
115.321453855131)) ;
#168319 = CARTESIAN_POINT('Ctrl Pts',(-22.868111692756,-12.9799529618983,
115.297222843561)) ;
#168320 = CARTESIAN_POINT('Ctrl Pts',(-22.9419155460636,-12.9799530265103,
115.272991831992)) ;
#168321 = CARTESIAN_POINT('Ctrl Pts',(-22.9631999044797,-12.9467052942123,
115.337820552117)) ;
#168322 = CARTESIAN_POINT('Ctrl Pts',(-22.9844842628957,-12.9134575619143,
115.402649272243)) ;
#168323 = CARTESIAN_POINT('Ctrl Pts',(-22.9106804095881,-12.9134574973022,
115.426880283813)) ;
#168324 = CARTESIAN_POINT('Ctrl Pts',(-22.8368765562805,-12.9134574326901,
115.451111295382)) ;
#168325 = CARTESIAN_POINT('Ctrl Pts',(-22.8155921978644,-12.9467051649881,
115.386282575257)) ;
#168326 = CARTESIAN_POINT('Ctrl Pts',(-22.854117195054,-13.2232753780377,
115.468204454967)) ;
#168327 = CARTESIAN_POINT('Ctrl Pts',(-22.8308452016767,-13.237261879662,
115.397321719593)) ;
#168328 = CARTESIAN_POINT('Ctrl Pts',(-22.9046490496905,-13.237261957473,
115.373090691899)) ;
#168329 = CARTESIAN_POINT('Ctrl Pts',(-22.9784528977043,-13.237262035284,
115.348859664205)) ;
#168330 = CARTESIAN_POINT('Ctrl Pts',(-23.0017248910816,-13.2232755336597,
115.419742399579)) ;
#168331 = CARTESIAN_POINT('Ctrl Pts',(-23.0249968844588,-13.2092890320355,
115.490625134953)) ;
#168332 = CARTESIAN_POINT('Ctrl Pts',(-22.9511930364451,-13.2092889542245,
115.514856162647)) ;
#168333 = CARTESIAN_POINT('Ctrl Pts',(-22.8773891884313,-13.2092888764135,
115.539087190341)) ;
#168334 = CARTESIAN_POINT('Ctrl Pts',(-22.854117195054,-13.2232753780377,
115.468204454967)) ;
#168335 = CARTESIAN_POINT('Ctrl Pts',(-22.8687874098863,-13.5141286997517,
115.477425109878)) ;
#168336 = CARTESIAN_POINT('Ctrl Pts',(-22.8451911742884,-13.5078290678433,
115.405554785151)) ;
#168337 = CARTESIAN_POINT('Ctrl Pts',(-22.9189950154969,-13.5078291537003,
115.381323736729)) ;
#168338 = CARTESIAN_POINT('Ctrl Pts',(-22.9927988567055,-13.5078292395572,
115.357092688308)) ;
#168339 = CARTESIAN_POINT('Ctrl Pts',(-23.0163950923034,-13.5141288714655,
115.428963013036)) ;
#168340 = CARTESIAN_POINT('Ctrl Pts',(-23.0399913279013,-13.5204285033738,
115.500833337763)) ;
#168341 = CARTESIAN_POINT('Ctrl Pts',(-22.9661874866927,-13.5204284175169,
115.525064386185)) ;
#168342 = CARTESIAN_POINT('Ctrl Pts',(-22.8923836454841,-13.52042833166,115.549295434606)) ;
#168343 = CARTESIAN_POINT('Ctrl Pts',(-22.8687874098863,-13.5141286997517,
115.477425109878)) ;
#168344 = CARTESIAN_POINT('Ctrl Pts',(-22.8592321322332,-13.7984771926956,
115.412815935399)) ;
#168345 = CARTESIAN_POINT('Ctrl Pts',(-22.8370032864545,-13.7723162248091,
115.345110459558)) ;
#168346 = CARTESIAN_POINT('Ctrl Pts',(-22.9108071199101,-13.7723163117777,
115.320879387523)) ;
#168347 = CARTESIAN_POINT('Ctrl Pts',(-22.9846109533657,-13.7723163987464,
115.296648315487)) ;
#168348 = CARTESIAN_POINT('Ctrl Pts',(-23.0068397991444,-13.7984773666329,
115.364353791328)) ;
#168349 = CARTESIAN_POINT('Ctrl Pts',(-23.0290686449232,-13.8246383345194,
115.432059267169)) ;
#168350 = CARTESIAN_POINT('Ctrl Pts',(-22.9552648114676,-13.8246382475507,
115.456290339205)) ;
#168351 = CARTESIAN_POINT('Ctrl Pts',(-22.881460978012,-13.8246381605821,
115.48052141124)) ;
#168352 = CARTESIAN_POINT('Ctrl Pts',(-22.8592321322332,-13.7984771926956,
115.412815935399)) ;
#168353 = CARTESIAN_POINT('Ctrl Pts',(-22.8267505858683,-14.0556517682192,
115.278338405061)) ;
#168354 = CARTESIAN_POINT('Ctrl Pts',(-22.8074924148263,-14.0114975765456,
115.219681125259)) ;
#168355 = CARTESIAN_POINT('Ctrl Pts',(-22.8812962403663,-14.011497656322,
115.195450029114)) ;
#168356 = CARTESIAN_POINT('Ctrl Pts',(-22.9551000659063,-14.0114977360984,
115.171218932969)) ;
#168357 = CARTESIAN_POINT('Ctrl Pts',(-22.9743582369483,-14.055651927772,
115.22987621277)) ;
#168358 = CARTESIAN_POINT('Ctrl Pts',(-22.9936164079904,-14.0998061194455,
115.288533492572)) ;
#168359 = CARTESIAN_POINT('Ctrl Pts',(-22.9198125824504,-14.0998060396691,
115.312764588717)) ;
#168360 = CARTESIAN_POINT('Ctrl Pts',(-22.8460087569104,-14.0998059598928,
115.336995684862)) ;
#168361 = CARTESIAN_POINT('Ctrl Pts',(-22.8267505858683,-14.0556517682192,
115.278338405061)) ;
#168362 = CARTESIAN_POINT('Ctrl Pts',(-22.7749229736523,-14.2658619034502,
115.085168032102)) ;
#168363 = CARTESIAN_POINT('Ctrl Pts',(-22.7599858265449,-14.206967241119,
115.03967189408)) ;
#168364 = CARTESIAN_POINT('Ctrl Pts',(-22.8337896452694,-14.2069673051098,
115.015440777175)) ;
#168365 = CARTESIAN_POINT('Ctrl Pts',(-22.9075934639938,-14.2069673691006,
114.991209660271)) ;
#168366 = CARTESIAN_POINT('Ctrl Pts',(-22.9225306111012,-14.2658620314317,
115.036705798294)) ;
#168367 = CARTESIAN_POINT('Ctrl Pts',(-22.9374677582085,-14.3247566937629,
115.082201936316)) ;
#168368 = CARTESIAN_POINT('Ctrl Pts',(-22.8636639394841,-14.3247566297721,
115.10643305322)) ;
#168369 = CARTESIAN_POINT('Ctrl Pts',(-22.7898601207596,-14.3247565657813,
115.130664170125)) ;
#168370 = CARTESIAN_POINT('Ctrl Pts',(-22.7749229736523,-14.2658619034502,
115.085168032102)) ;
#168371 = CARTESIAN_POINT('Ctrl Pts',(-22.7073801962301,-14.4169100671748,
114.843829194715)) ;
#168372 = CARTESIAN_POINT('Ctrl Pts',(-22.6978734686817,-14.3473831262014,
114.814873238548)) ;
#168373 = CARTESIAN_POINT('Ctrl Pts',(-22.7716772818824,-14.3473831682741,
114.790642104819)) ;
#168374 = CARTESIAN_POINT('Ctrl Pts',(-22.8454810950831,-14.3473832103469,
114.76641097109)) ;
#168375 = CARTESIAN_POINT('Ctrl Pts',(-22.8549878226315,-14.4169101513204,
114.795366927258)) ;
#168376 = CARTESIAN_POINT('Ctrl Pts',(-22.8644945501799,-14.4864370922939,
114.824322883424)) ;
#168377 = CARTESIAN_POINT('Ctrl Pts',(-22.7906907369792,-14.4864370502211,
114.848554017153)) ;
#168378 = CARTESIAN_POINT('Ctrl Pts',(-22.7168869237785,-14.4864370081483,
114.872785150882)) ;
#168379 = CARTESIAN_POINT('Ctrl Pts',(-22.7073801962301,-14.4169100671748,
114.843829194715)) ;
#168380 = CARTESIAN_POINT('Ctrl Pts',(-22.6304186927666,-14.4953742453793,
114.573953875057)) ;
#168381 = CARTESIAN_POINT('Ctrl Pts',(-22.6270049111093,-14.4202668072197,
114.563556049018)) ;
#168382 = CARTESIAN_POINT('Ctrl Pts',(-22.7008087213179,-14.4202668221935,
114.539324906176)) ;
#168383 = CARTESIAN_POINT('Ctrl Pts',(-22.7746125315266,-14.4202668371673,
114.515093763334)) ;
#168384 = CARTESIAN_POINT('Ctrl Pts',(-22.7780263131839,-14.495374275327,
114.525491589373)) ;
#168385 = CARTESIAN_POINT('Ctrl Pts',(-22.7814400948412,-14.5704817134867,
114.535889415412)) ;
#168386 = CARTESIAN_POINT('Ctrl Pts',(-22.7076362846326,-14.5704816985128,
114.560120558254)) ;
#168387 = CARTESIAN_POINT('Ctrl Pts',(-22.6338324744239,-14.570481683539,
114.584351701096)) ;
#168388 = CARTESIAN_POINT('Ctrl Pts',(-22.6304186927666,-14.4953742453793,
114.573953875057)) ;
#168389 = CARTESIAN_POINT('Ctrl Pts',(-22.550396983414,-14.4969828286805,
114.294883066469)) ;
#168390 = CARTESIAN_POINT('Ctrl Pts',(-22.553296213992,-14.4216525600046,
114.303713657114)) ;
#168391 = CARTESIAN_POINT('Ctrl Pts',(-22.6271000238928,-14.4216525461531,
114.279482513335)) ;
#168392 = CARTESIAN_POINT('Ctrl Pts',(-22.7009038337936,-14.4216525323015,
114.255251369555)) ;
#168393 = CARTESIAN_POINT('Ctrl Pts',(-22.6980046032156,-14.4969828009775,
114.24642077891)) ;
#168394 = CARTESIAN_POINT('Ctrl Pts',(-22.6951053726376,-14.5723130696534,
114.237590188265)) ;
#168395 = CARTESIAN_POINT('Ctrl Pts',(-22.6213015627367,-14.5723130835049,
114.261821332045)) ;
#168396 = CARTESIAN_POINT('Ctrl Pts',(-22.5474977528359,-14.5723130973564,
114.286052475824)) ;
#168397 = CARTESIAN_POINT('Ctrl Pts',(-22.550396983414,-14.4969828286805,
114.294883066469)) ;
#168398 = CARTESIAN_POINT('Ctrl Pts',(-22.4731667198219,-14.421551875411,
114.024183632776)) ;
#168399 = CARTESIAN_POINT('Ctrl Pts',(-22.4821960521994,-14.3513763125925,
114.051685524413)) ;
#168400 = CARTESIAN_POINT('Ctrl Pts',(-22.555999864463,-14.3513762706419,
114.02745438783)) ;
#168401 = CARTESIAN_POINT('Ctrl Pts',(-22.6298036767266,-14.3513762286912,
114.003223251247)) ;
#168402 = CARTESIAN_POINT('Ctrl Pts',(-22.6207743443492,-14.4215517915098,
113.97572135961)) ;
#168403 = CARTESIAN_POINT('Ctrl Pts',(-22.6117450119717,-14.4917273543283,
113.948219467973)) ;
#168404 = CARTESIAN_POINT('Ctrl Pts',(-22.5379411997081,-14.491727396279,
113.972450604555)) ;
#168405 = CARTESIAN_POINT('Ctrl Pts',(-22.4641373874444,-14.4917274382296,
113.996681741138)) ;
#168406 = CARTESIAN_POINT('Ctrl Pts',(-22.4731667198219,-14.421551875411,
114.024183632776)) ;
#168407 = CARTESIAN_POINT('Ctrl Pts',(-22.4051586069589,-14.2735000710325,
113.781463265939)) ;
#168408 = CARTESIAN_POINT('Ctrl Pts',(-22.4196856428359,-14.213556255384,
113.825710275356)) ;
#168409 = CARTESIAN_POINT('Ctrl Pts',(-22.4934894600971,-14.2135561892348,
113.801479153994)) ;
#168410 = CARTESIAN_POINT('Ctrl Pts',(-22.5672932773583,-14.2135561230857,
113.777248032633)) ;
#168411 = CARTESIAN_POINT('Ctrl Pts',(-22.5527662414813,-14.2734999387342,
113.733001023217)) ;
#168412 = CARTESIAN_POINT('Ctrl Pts',(-22.5382392056042,-14.3334437543827,
113.6887540138)) ;
#168413 = CARTESIAN_POINT('Ctrl Pts',(-22.4644353883431,-14.3334438205319,
113.712985135162)) ;
#168414 = CARTESIAN_POINT('Ctrl Pts',(-22.3906315710819,-14.3334438866811,
113.737216256523)) ;
#168415 = CARTESIAN_POINT('Ctrl Pts',(-22.4051586069589,-14.2735000710325,
113.781463265939)) ;
#168416 = CARTESIAN_POINT('Ctrl Pts',(-22.3524264112535,-14.0646532706665,
113.585402345504)) ;
#168417 = CARTESIAN_POINT('Ctrl Pts',(-22.3713901641002,-14.019201123048,
113.643162878901)) ;
#168418 = CARTESIAN_POINT('Ctrl Pts',(-22.4451939882553,-14.0192010389841,
113.618931778537)) ;
#168419 = CARTESIAN_POINT('Ctrl Pts',(-22.5189978124103,-14.0192009549201,
113.594700678174)) ;
#168420 = CARTESIAN_POINT('Ctrl Pts',(-22.5000340595636,-14.0646531025386,
113.536940144777)) ;
#168421 = CARTESIAN_POINT('Ctrl Pts',(-22.4810703067168,-14.110105250157,
113.47917961138)) ;
#168422 = CARTESIAN_POINT('Ctrl Pts',(-22.4072664825617,-14.110105334221,
113.503410711744)) ;
#168423 = CARTESIAN_POINT('Ctrl Pts',(-22.3334626584067,-14.1101054182849,
113.527641812108)) ;
#168424 = CARTESIAN_POINT('Ctrl Pts',(-22.3524264112535,-14.0646532706665,
113.585402345504)) ;
#168425 = CARTESIAN_POINT('Ctrl Pts',(-22.3192033937915,-13.8091818841456,
113.448713324322)) ;
#168426 = CARTESIAN_POINT('Ctrl Pts',(-22.3412495726263,-13.7814979528365,
113.515862429858)) ;
#168427 = CARTESIAN_POINT('Ctrl Pts',(-22.4150534048702,-13.7814978588796,
113.491631354132)) ;
#168428 = CARTESIAN_POINT('Ctrl Pts',(-22.4888572371141,-13.7814977649226,
113.467400278406)) ;
#168429 = CARTESIAN_POINT('Ctrl Pts',(-22.4668110582793,-13.8091816962316,
113.400251172869)) ;
#168430 = CARTESIAN_POINT('Ctrl Pts',(-22.4447648794445,-13.8368656275406,
113.333102067333)) ;
#168431 = CARTESIAN_POINT('Ctrl Pts',(-22.3709610472006,-13.8368657214976,
113.357333143059)) ;
#168432 = CARTESIAN_POINT('Ctrl Pts',(-22.2971572149566,-13.8368658154546,
113.381564218785)) ;
#168433 = CARTESIAN_POINT('Ctrl Pts',(-22.3192033937915,-13.8091818841456,
113.448713324322)) ;
#168434 = CARTESIAN_POINT('Ctrl Pts',(-22.3086900686666,-13.5266904596517,
113.381322855657)) ;
#168435 = CARTESIAN_POINT('Ctrl Pts',(-22.3322350932624,-13.5186880514058,
113.453037203464)) ;
#168436 = CARTESIAN_POINT('Ctrl Pts',(-22.406038933809,-13.5186879553988,
113.428806153027)) ;
#168437 = CARTESIAN_POINT('Ctrl Pts',(-22.4798427743556,-13.5186878593918,
113.404575102589)) ;
#168438 = CARTESIAN_POINT('Ctrl Pts',(-22.4562977497598,-13.5266902676377,
113.332860754782)) ;
#168439 = CARTESIAN_POINT('Ctrl Pts',(-22.432752725164,-13.5346926758837,
113.261146406975)) ;
#168440 = CARTESIAN_POINT('Ctrl Pts',(-22.3589488846175,-13.5346927718906,
113.285377457413)) ;
#168441 = CARTESIAN_POINT('Ctrl Pts',(-22.2851450440709,-13.5346928678976,
113.30960850785)) ;
#168442 = CARTESIAN_POINT('Ctrl Pts',(-22.3086900686666,-13.5266904596517,
113.381322855657)) ;
#168443 = CARTESIAN_POINT('Ctrl Pts',(-22.3223045121506,-13.2352604395114,
113.387274613305)) ;
#168444 = CARTESIAN_POINT('Ctrl Pts',(-22.3456693500622,-13.2475929455495,
113.458440141433)) ;
#168445 = CARTESIAN_POINT('Ctrl Pts',(-22.4194731984143,-13.2475928562787,
113.434209114769)) ;
#168446 = CARTESIAN_POINT('Ctrl Pts',(-22.4932770467663,-13.2475927670079,
113.409978088106)) ;
#168447 = CARTESIAN_POINT('Ctrl Pts',(-22.4699122088548,-13.2352602609698,
113.338812559978)) ;
#168448 = CARTESIAN_POINT('Ctrl Pts',(-22.4465473709432,-13.2229277549316,
113.26764703185)) ;
#168449 = CARTESIAN_POINT('Ctrl Pts',(-22.3727435225911,-13.2229278442025,
113.291878058513)) ;
#168450 = CARTESIAN_POINT('Ctrl Pts',(-22.2989396742391,-13.2229279334733,
113.316109085177)) ;
#168451 = CARTESIAN_POINT('Ctrl Pts',(-22.3223045121506,-13.2352604395114,
113.387274613305)) ;
#168452 = CARTESIAN_POINT('Ctrl Pts',(-22.360045558316,-12.9567404114365,
113.466682888076)) ;
#168453 = CARTESIAN_POINT('Ctrl Pts',(-22.3815461871748,-12.9885373907524,
113.532170336082)) ;
#168454 = CARTESIAN_POINT('Ctrl Pts',(-22.4553500418253,-12.9885373153284,
113.507939328603)) ;
#168455 = CARTESIAN_POINT('Ctrl Pts',(-22.5291538964759,-12.9885372399044,
113.483708321124)) ;
#168456 = CARTESIAN_POINT('Ctrl Pts',(-22.5076532676171,-12.9567402605885,
113.418220873118)) ;
#168457 = CARTESIAN_POINT('Ctrl Pts',(-22.4861526387583,-12.9249432812726,
113.352733425112)) ;
#168458 = CARTESIAN_POINT('Ctrl Pts',(-22.4123487841078,-12.9249433566966,
113.376964432591)) ;
#168459 = CARTESIAN_POINT('Ctrl Pts',(-22.3385449294572,-12.9249434321206,
113.401195440071)) ;
#168460 = CARTESIAN_POINT('Ctrl Pts',(-22.360045558316,-12.9567404114365,
113.466682888076)) ;
#168461 = CARTESIAN_POINT('Ctrl Pts',(-22.4196665993384,-12.7122106250869,
113.612854579177)) ;
#168462 = CARTESIAN_POINT('Ctrl Pts',(-22.437769996859,-12.7611284974195,
113.667994608535)) ;
#168463 = CARTESIAN_POINT('Ctrl Pts',(-22.5115738559352,-12.7611284394827,
113.643763614535)) ;
#168464 = CARTESIAN_POINT('Ctrl Pts',(-22.5853777150113,-12.7611283815459,
113.619532620536)) ;
#168465 = CARTESIAN_POINT('Ctrl Pts',(-22.5672743174907,-12.7122105092134,
113.564392591178)) ;
#168466 = CARTESIAN_POINT('Ctrl Pts',(-22.5491709199701,-12.6632926368809,
113.509252561821)) ;
#168467 = CARTESIAN_POINT('Ctrl Pts',(-22.4753670608939,-12.6632926948177,
113.533483555821)) ;
#168468 = CARTESIAN_POINT('Ctrl Pts',(-22.4015632018178,-12.6632927527544,
113.55771454982)) ;
#168469 = CARTESIAN_POINT('Ctrl Pts',(-22.4196665993384,-12.7122106250869,
113.612854579177)) ;
#168470 = CARTESIAN_POINT('Ctrl Pts',(-22.4976345852883,-12.5182289407429,
113.814941278565)) ;
#168471 = CARTESIAN_POINT('Ctrl Pts',(-22.5110539521442,-12.5807644314872,
113.855814506146)) ;
#168472 = CARTESIAN_POINT('Ctrl Pts',(-22.5848578136224,-12.5807643929597,
113.831583519462)) ;
#168473 = CARTESIAN_POINT('Ctrl Pts',(-22.6586616751006,-12.5807643544323,
113.807352532779)) ;
#168474 = CARTESIAN_POINT('Ctrl Pts',(-22.6452423082446,-12.518228863688,
113.766479305198)) ;
#168475 = CARTESIAN_POINT('Ctrl Pts',(-22.6318229413887,-12.4556933729437,
113.725606077618)) ;
#168476 = CARTESIAN_POINT('Ctrl Pts',(-22.5580190799105,-12.4556934114712,
113.749837064301)) ;
#168477 = CARTESIAN_POINT('Ctrl Pts',(-22.4842152184323,-12.4556934499986,
113.774068050984)) ;
#168478 = CARTESIAN_POINT('Ctrl Pts',(-22.4976345852883,-12.5182289407429,
113.814941278565)) ;
#168479 = CARTESIAN_POINT('Ctrl Pts',(-22.5895023142545,-12.3880154836096,
114.059257743448)) ;
#168480 = CARTESIAN_POINT('Ctrl Pts',(-22.5972623678869,-12.4597373427525,
114.082893615912)) ;
#168481 = CARTESIAN_POINT('Ctrl Pts',(-22.6710662293981,-12.4597373239449,
114.058662629329)) ;
#168482 = CARTESIAN_POINT('Ctrl Pts',(-22.7448700909092,-12.4597373051373,
114.034431642746)) ;
#168483 = CARTESIAN_POINT('Ctrl Pts',(-22.7371100372769,-12.3880154459944,
114.010795770283)) ;
#168484 = CARTESIAN_POINT('Ctrl Pts',(-22.7293499836445,-12.3162935868514,
113.987159897819)) ;
#168485 = CARTESIAN_POINT('Ctrl Pts',(-22.6555461221333,-12.316293605659,
114.011390884402)) ;
#168486 = CARTESIAN_POINT('Ctrl Pts',(-22.5817422606221,-12.3162936244666,
114.035621870985)) ;
#168487 = CARTESIAN_POINT('Ctrl Pts',(-22.5895023142545,-12.3880154836096,
114.059257743448)) ;
#168488 = CARTESIAN_POINT('Ctrl Pts',(-22.6895136884931,-12.3319594983171,
114.328282716118)) ;
#168489 = CARTESIAN_POINT('Ctrl Pts',(-22.6910391558902,-12.4077044418995,
114.332929044665)) ;
#168490 = CARTESIAN_POINT('Ctrl Pts',(-22.7648430152365,-12.407704439621,
114.308698051488)) ;
#168491 = CARTESIAN_POINT('Ctrl Pts',(-22.8386468745828,-12.4077044373425,
114.284467058311)) ;
#168492 = CARTESIAN_POINT('Ctrl Pts',(-22.8371214071857,-12.33195949376,114.279820729764)) ;
#168493 = CARTESIAN_POINT('Ctrl Pts',(-22.8355959397885,-12.2562145501775,
114.275174401218)) ;
#168494 = CARTESIAN_POINT('Ctrl Pts',(-22.7617920804422,-12.2562145524561,
114.299405394395)) ;
#168495 = CARTESIAN_POINT('Ctrl Pts',(-22.6879882210959,-12.2562145547346,
114.323636387572)) ;
#168496 = CARTESIAN_POINT('Ctrl Pts',(-22.6895136884931,-12.3319594983171,
114.328282716118)) ;
#168497 = CARTESIAN_POINT('Ctrl Pts',(-22.7899870488057,-12.3535606969818,
114.599060850757)) ;
#168498 = CARTESIAN_POINT('Ctrl Pts',(-22.7852289860199,-12.4279116529158,
114.584568560083)) ;
#168499 = CARTESIAN_POINT('Ctrl Pts',(-22.8590328429792,-12.4279116627694,
114.560337559636)) ;
#168500 = CARTESIAN_POINT('Ctrl Pts',(-22.9328366999386,-12.427911672623,
114.536106559189)) ;
#168501 = CARTESIAN_POINT('Ctrl Pts',(-22.9375947627244,-12.3535607166891,
114.550598849862)) ;
#168502 = CARTESIAN_POINT('Ctrl Pts',(-22.9423528255101,-12.2792097607552,
114.565091140536)) ;
#168503 = CARTESIAN_POINT('Ctrl Pts',(-22.8685489685508,-12.2792097509015,
114.589322140983)) ;
#168504 = CARTESIAN_POINT('Ctrl Pts',(-22.7947451115915,-12.2792097410479,
114.61355314143)) ;
#168505 = CARTESIAN_POINT('Ctrl Pts',(-22.7899870488057,-12.3535606969818,
114.599060850757)) ;
#168506 = CARTESIAN_POINT('Ctrl Pts',(-22.8861512888301,-12.451253883518,
114.856463511096)) ;
#168507 = CARTESIAN_POINT('Ctrl Pts',(-22.8754061618611,-12.5188965599117,
114.823735588756)) ;
#168508 = CARTESIAN_POINT('Ctrl Pts',(-22.9492100150156,-12.5188965769681,
114.79950457672)) ;
#168509 = CARTESIAN_POINT('Ctrl Pts',(-23.0230138681702,-12.5188965940245,
114.775273564684)) ;
#168510 = CARTESIAN_POINT('Ctrl Pts',(-23.0337589951393,-12.4512539176309,
114.808001487025)) ;
#168511 = CARTESIAN_POINT('Ctrl Pts',(-23.0445041221084,-12.3836112412372,
114.840729409365)) ;
#168512 = CARTESIAN_POINT('Ctrl Pts',(-22.9707002689538,-12.3836112241808,
114.864960421401)) ;
#168513 = CARTESIAN_POINT('Ctrl Pts',(-22.8968964157992,-12.3836112071243,
114.889191433437)) ;
#168514 = CARTESIAN_POINT('Ctrl Pts',(-22.8861512888301,-12.451253883518,
114.856463511096)) ;
#168515 = CARTESIAN_POINT('Ctrl Pts',(-22.9710997816442,-12.618326669095,
115.079730072994)) ;
#168516 = CARTESIAN_POINT('Ctrl Pts',(-22.9551410288214,-12.6744063613934,
115.031122287354)) ;
#168517 = CARTESIAN_POINT('Ctrl Pts',(-23.0289448782623,-12.6744063803127,
115.006891264007)) ;
#168518 = CARTESIAN_POINT('Ctrl Pts',(-23.1027487277032,-12.6744063992319,
114.98266024066)) ;
#168519 = CARTESIAN_POINT('Ctrl Pts',(-23.118707480526,-12.6183267069335,
115.0312680263)) ;
#168520 = CARTESIAN_POINT('Ctrl Pts',(-23.1346662333488,-12.5622470146351,
115.07987581194)) ;
#168521 = CARTESIAN_POINT('Ctrl Pts',(-23.0608623839079,-12.5622469957158,
115.104106835287)) ;
#168522 = CARTESIAN_POINT('Ctrl Pts',(-22.987058534467,-12.5622469767965,
115.128337858634)) ;
#168523 = CARTESIAN_POINT('Ctrl Pts',(-22.9710997816442,-12.618326669095,
115.079730072994)) ;
#168524 = CARTESIAN_POINT('Ctrl Pts',(-23.0396705642867,-12.8433532834822,
115.253021743051)) ;
#168525 = CARTESIAN_POINT('Ctrl Pts',(-23.0196356089412,-12.883805650216,
115.191998502051)) ;
#168526 = CARTESIAN_POINT('Ctrl Pts',(-23.0934394551956,-12.8838056661619,
115.167767468999)) ;
#168527 = CARTESIAN_POINT('Ctrl Pts',(-23.16724330145,-12.8838056821078,115.143536435946)) ;
#168528 = CARTESIAN_POINT('Ctrl Pts',(-23.1872782567955,-12.843353315374,
115.204559676946)) ;
#168529 = CARTESIAN_POINT('Ctrl Pts',(-23.207313212141,-12.8029009486403,
115.265582917945)) ;
#168530 = CARTESIAN_POINT('Ctrl Pts',(-23.1335093658866,-12.8029009326944,
115.289813950998)) ;
#168531 = CARTESIAN_POINT('Ctrl Pts',(-23.0597055196322,-12.8029009167485,
115.314044984051)) ;
#168532 = CARTESIAN_POINT('Ctrl Pts',(-23.0396705642867,-12.8433532834822,
115.253021743051)) ;
#168533 = CARTESIAN_POINT('Ctrl Pts',(-23.0873467114543,-13.1083703127966,
115.362848501741)) ;
#168534 = CARTESIAN_POINT('Ctrl Pts',(-23.0646848738263,-13.1303789495469,
115.293824201028)) ;
#168535 = CARTESIAN_POINT('Ctrl Pts',(-23.1384887180983,-13.1303789610419,
115.269593161937)) ;
#168536 = CARTESIAN_POINT('Ctrl Pts',(-23.2122925623702,-13.130378972537,
115.245362122846)) ;
#168537 = CARTESIAN_POINT('Ctrl Pts',(-23.2349543999982,-13.1083703357867,
115.314386423559)) ;
#168538 = CARTESIAN_POINT('Ctrl Pts',(-23.2576162376261,-13.0863616990364,
115.383410724271)) ;
#168539 = CARTESIAN_POINT('Ctrl Pts',(-23.1838123933542,-13.0863616875414,
115.407641763362)) ;
#168540 = CARTESIAN_POINT('Ctrl Pts',(-23.1100085490823,-13.0863616760463,
115.431872802453)) ;
#168541 = CARTESIAN_POINT('Ctrl Pts',(-23.0873467114543,-13.1083703127966,
115.362848501741)) ;
#168542 = CARTESIAN_POINT('Ctrl Pts',(-23.1118506671336,-13.3973093025061,
115.401868284808)) ;
#168543 = CARTESIAN_POINT('Ctrl Pts',(-23.0881805683991,-13.3991753907739,
115.329772983313)) ;
#168544 = CARTESIAN_POINT('Ctrl Pts',(-23.1619844116872,-13.399175395662,
115.305541941225)) ;
#168545 = CARTESIAN_POINT('Ctrl Pts',(-23.2357882549754,-13.39917540055,115.281310899138)) ;
#168546 = CARTESIAN_POINT('Ctrl Pts',(-23.2594583537099,-13.3973093122823,
115.353406200633)) ;
#168547 = CARTESIAN_POINT('Ctrl Pts',(-23.2831284524444,-13.3954432240146,
115.425501502128)) ;
#168548 = CARTESIAN_POINT('Ctrl Pts',(-23.2093246091562,-13.3954432191265,
115.449732544215)) ;
#168549 = CARTESIAN_POINT('Ctrl Pts',(-23.1355207658681,-13.3954432142384,
115.473963586303)) ;
#168550 = CARTESIAN_POINT('Ctrl Pts',(-23.1118506671336,-13.3973093025061,
115.401868284808)) ;
#168551 = CARTESIAN_POINT('Ctrl Pts',(-23.1119807889645,-13.685052446536,
115.366993485152)) ;
#168552 = CARTESIAN_POINT('Ctrl Pts',(-23.0889961755581,-13.666829482395,
115.296986061293)) ;
#168553 = CARTESIAN_POINT('Ctrl Pts',(-23.1628000187813,-13.6668294834514,
115.272755019008)) ;
#168554 = CARTESIAN_POINT('Ctrl Pts',(-23.2366038620046,-13.6668294845077,
115.248523976722)) ;
#168555 = CARTESIAN_POINT('Ctrl Pts',(-23.2595884754109,-13.6850524486487,
115.318531400582)) ;
#168556 = CARTESIAN_POINT('Ctrl Pts',(-23.2825730888173,-13.7032754127896,
115.388538824441)) ;
#168557 = CARTESIAN_POINT('Ctrl Pts',(-23.2087692455941,-13.7032754117333,
115.412769866726)) ;
#168558 = CARTESIAN_POINT('Ctrl Pts',(-23.1349654023708,-13.7032754106769,
115.437000909011)) ;
#168559 = CARTESIAN_POINT('Ctrl Pts',(-23.1119807889645,-13.685052446536,
115.366993485152)) ;
#168560 = CARTESIAN_POINT('Ctrl Pts',(-23.0885048309624,-13.9562925901238,
115.259878332445)) ;
#168561 = CARTESIAN_POINT('Ctrl Pts',(-23.0678620146304,-13.9191017880253,
115.197003644556)) ;
#168562 = CARTESIAN_POINT('Ctrl Pts',(-23.1416658583648,-13.9191017857383,
115.172772603827)) ;
#168563 = CARTESIAN_POINT('Ctrl Pts',(-23.2154697020991,-13.9191017834513,
115.148541563099)) ;
#168564 = CARTESIAN_POINT('Ctrl Pts',(-23.236112518431,-13.9562925855498,
115.211416250988)) ;
#168565 = CARTESIAN_POINT('Ctrl Pts',(-23.2567553347629,-13.9934833876483,
115.274290938878)) ;
#168566 = CARTESIAN_POINT('Ctrl Pts',(-23.1829514910286,-13.9934833899353,
115.298521979606)) ;
#168567 = CARTESIAN_POINT('Ctrl Pts',(-23.1091476472943,-13.9934833922223,
115.322753020334)) ;
#168568 = CARTESIAN_POINT('Ctrl Pts',(-23.0885048309624,-13.9562925901238,
115.259878332445)) ;
#168569 = CARTESIAN_POINT('Ctrl Pts',(-23.0439896792581,-14.1872893194723,
115.088901502234)) ;
#168570 = CARTESIAN_POINT('Ctrl Pts',(-23.0271571303233,-14.1339131286007,
115.037632274036)) ;
#168571 = CARTESIAN_POINT('Ctrl Pts',(-23.1009609744752,-14.1339131262424,
115.013401234579)) ;
#168572 = CARTESIAN_POINT('Ctrl Pts',(-23.1747648186271,-14.1339131238842,
114.989170195123)) ;
#168573 = CARTESIAN_POINT('Ctrl Pts',(-23.1915973675619,-14.1872893147558,
115.040439423321)) ;
#168574 = CARTESIAN_POINT('Ctrl Pts',(-23.2084299164967,-14.2406655056274,
115.091708651519)) ;
#168575 = CARTESIAN_POINT('Ctrl Pts',(-23.1346260723448,-14.2406655079856,
115.115939690975)) ;
#168576 = CARTESIAN_POINT('Ctrl Pts',(-23.0608222281929,-14.2406655103439,
115.140170730432)) ;
#168577 = CARTESIAN_POINT('Ctrl Pts',(-23.0439896792581,-14.1872893194723,
115.088901502234)) ;
#168578 = CARTESIAN_POINT('Ctrl Pts',(-22.9823604254838,-14.3636852679792,
114.865766334949)) ;
#168579 = CARTESIAN_POINT('Ctrl Pts',(-22.9705395949471,-14.2979128675593,
114.829761992371)) ;
#168580 = CARTESIAN_POINT('Ctrl Pts',(-23.0443434390419,-14.2979128665308,
114.805530952741)) ;
#168581 = CARTESIAN_POINT('Ctrl Pts',(-23.1181472831367,-14.2979128655022,
114.78129991311)) ;
#168582 = CARTESIAN_POINT('Ctrl Pts',(-23.1299681136734,-14.3636852659222,
114.817304255688)) ;
#168583 = CARTESIAN_POINT('Ctrl Pts',(-23.1417889442101,-14.4294576663421,
114.853308598265)) ;
#168584 = CARTESIAN_POINT('Ctrl Pts',(-23.0679851001154,-14.4294576673706,
114.877539637896)) ;
#168585 = CARTESIAN_POINT('Ctrl Pts',(-22.9941812560206,-14.4294576683991,
114.901770677526)) ;
#168586 = CARTESIAN_POINT('Ctrl Pts',(-22.9823604254838,-14.3636852679792,
114.865766334949)) ;
#168587 = CARTESIAN_POINT('Ctrl Pts',(-22.908524900711,-14.4725504618335,
114.605368957616)) ;
#168588 = CARTESIAN_POINT('Ctrl Pts',(-22.9025772469157,-14.3990795841732,
114.587253363822)) ;
#168589 = CARTESIAN_POINT('Ctrl Pts',(-22.9763810901088,-14.3990795846932,
114.563022321445)) ;
#168590 = CARTESIAN_POINT('Ctrl Pts',(-23.0501849333019,-14.3990795852131,
114.538791279068)) ;
#168591 = CARTESIAN_POINT('Ctrl Pts',(-23.0561325870972,-14.4725504628734,
114.556906872862)) ;
#168592 = CARTESIAN_POINT('Ctrl Pts',(-23.0620802408925,-14.5460213405337,
114.575022466657)) ;
#168593 = CARTESIAN_POINT('Ctrl Pts',(-22.9882763976994,-14.5460213400138,
114.599253509034)) ;
#168594 = CARTESIAN_POINT('Ctrl Pts',(-22.9144725545063,-14.5460213394938,
114.623484551411)) ;
#168595 = CARTESIAN_POINT('Ctrl Pts',(-22.908524900711,-14.4725504618335,
114.605368957616)) ;
#168596 = CARTESIAN_POINT('Ctrl Pts',(-22.8289915160444,-14.505767100085,
114.327744641728)) ;
#168597 = CARTESIAN_POINT('Ctrl Pts',(-22.8293207368645,-14.4298697296846,
114.328747395323)) ;
#168598 = CARTESIAN_POINT('Ctrl Pts',(-22.903124578711,-14.429869730049,114.304516348845)) ;
#168599 = CARTESIAN_POINT('Ctrl Pts',(-22.9769284205575,-14.4298697304134,
114.280285302366)) ;
#168600 = CARTESIAN_POINT('Ctrl Pts',(-22.9765991997374,-14.5057671008138,
114.279282548771)) ;
#168601 = CARTESIAN_POINT('Ctrl Pts',(-22.9762699789173,-14.5816644712143,
114.278279795176)) ;
#168602 = CARTESIAN_POINT('Ctrl Pts',(-22.9024661370708,-14.5816644708498,
114.302510841654)) ;
#168603 = CARTESIAN_POINT('Ctrl Pts',(-22.8286622952243,-14.5816644704854,
114.326741888133)) ;
#168604 = CARTESIAN_POINT('Ctrl Pts',(-22.8289915160444,-14.505767100085,
114.327744641728)) ;
#168605 = CARTESIAN_POINT('Ctrl Pts',(-22.7496283707013,-14.461184023194,
114.050502355121)) ;
#168606 = CARTESIAN_POINT('Ctrl Pts',(-22.7562345239439,-14.388288943336,
114.070623632217)) ;
#168607 = CARTESIAN_POINT('Ctrl Pts',(-22.8300383639314,-14.3882889407252,
114.046392580076)) ;
#168608 = CARTESIAN_POINT('Ctrl Pts',(-22.9038422039188,-14.3882889381144,
114.022161527935)) ;
#168609 = CARTESIAN_POINT('Ctrl Pts',(-22.8972360506762,-14.4611840179724,
114.002040250839)) ;
#168610 = CARTESIAN_POINT('Ctrl Pts',(-22.8906298974336,-14.5340790978304,
113.981918973743)) ;
#168611 = CARTESIAN_POINT('Ctrl Pts',(-22.8168260574461,-14.5340791004412,
114.006150025884)) ;
#168612 = CARTESIAN_POINT('Ctrl Pts',(-22.7430222174587,-14.534079103052,
114.030381078025)) ;
#168613 = CARTESIAN_POINT('Ctrl Pts',(-22.7496283707013,-14.461184023194,
114.050502355121)) ;
#168614 = CARTESIAN_POINT('Ctrl Pts',(-22.6772956319986,-14.3417566878776,
113.794723577592)) ;
#168615 = CARTESIAN_POINT('Ctrl Pts',(-22.6896957697514,-14.2770945733709,
113.832492396787)) ;
#168616 = CARTESIAN_POINT('Ctrl Pts',(-22.7634996081967,-14.2770945642116,
113.808261339949)) ;
#168617 = CARTESIAN_POINT('Ctrl Pts',(-22.837303446642,-14.2770945550524,
113.784030283111)) ;
#168618 = CARTESIAN_POINT('Ctrl Pts',(-22.8249033088892,-14.3417566695591,
113.746261463916)) ;
#168619 = CARTESIAN_POINT('Ctrl Pts',(-22.8125031711365,-14.4064187840659,
113.708492644721)) ;
#168620 = CARTESIAN_POINT('Ctrl Pts',(-22.7386993326912,-14.4064187932251,
113.732723701559)) ;
#168621 = CARTESIAN_POINT('Ctrl Pts',(-22.6648954942459,-14.4064188023844,
113.756954758397)) ;
#168622 = CARTESIAN_POINT('Ctrl Pts',(-22.6772956319986,-14.3417566878776,
113.794723577592)) ;
#168623 = CARTESIAN_POINT('Ctrl Pts',(-22.6178545187857,-14.1564991842471,
113.578251720131)) ;
#168624 = CARTESIAN_POINT('Ctrl Pts',(-22.6351559129392,-14.104678506832,
113.630948975651)) ;
#168625 = CARTESIAN_POINT('Ctrl Pts',(-22.7089597507266,-14.1046784883743,
113.60671791681)) ;
#168626 = CARTESIAN_POINT('Ctrl Pts',(-22.7827635885141,-14.1046784699167,
113.582486857968)) ;
#168627 = CARTESIAN_POINT('Ctrl Pts',(-22.7654621943605,-14.1564991473318,
113.529789602448)) ;
#168628 = CARTESIAN_POINT('Ctrl Pts',(-22.748160800207,-14.208319824747,113.477092346927)) ;
#168629 = CARTESIAN_POINT('Ctrl Pts',(-22.6743569624196,-14.2083198432046,
113.501323405769)) ;
#168630 = CARTESIAN_POINT('Ctrl Pts',(-22.6005531246321,-14.2083198616622,
113.52555446461)) ;
#168631 = CARTESIAN_POINT('Ctrl Pts',(-22.6178545187857,-14.1564991842471,
113.578251720131)) ;
#168632 = CARTESIAN_POINT('Ctrl Pts',(-22.5761478520901,-13.9178865274089,
113.415717840721)) ;
#168633 = CARTESIAN_POINT('Ctrl Pts',(-22.5971209446297,-13.8826509917796,
113.479598497267)) ;
#168634 = CARTESIAN_POINT('Ctrl Pts',(-22.6709247828783,-13.8826509615156,
113.45536743983)) ;
#168635 = CARTESIAN_POINT('Ctrl Pts',(-22.744728621127,-13.8826509312515,
113.431136382393)) ;
#168636 = CARTESIAN_POINT('Ctrl Pts',(-22.7237555285874,-13.9178864668808,
113.367255725847)) ;
#168637 = CARTESIAN_POINT('Ctrl Pts',(-22.7027824360478,-13.9531220025101,
113.303375069301)) ;
#168638 = CARTESIAN_POINT('Ctrl Pts',(-22.6289785977992,-13.9531220327742,
113.327606126738)) ;
#168639 = CARTESIAN_POINT('Ctrl Pts',(-22.5551747595505,-13.9531220630382,
113.351837184175)) ;
#168640 = CARTESIAN_POINT('Ctrl Pts',(-22.5761478520901,-13.9178865274089,
113.415717840721)) ;
#168641 = CARTESIAN_POINT('Ctrl Pts',(-22.5561014124412,-13.643415658276,
113.31916524184)) ;
#168642 = CARTESIAN_POINT('Ctrl Pts',(-22.579238957361,-13.6272927364366,
113.389638471276)) ;
#168643 = CARTESIAN_POINT('Ctrl Pts',(-22.6530427977317,-13.627292694101,
113.365407420303)) ;
#168644 = CARTESIAN_POINT('Ctrl Pts',(-22.7268466381025,-13.6272926517654,
113.34117636933)) ;
#168645 = CARTESIAN_POINT('Ctrl Pts',(-22.7037090931827,-13.6434155736048,
113.270703139894)) ;
#168646 = CARTESIAN_POINT('Ctrl Pts',(-22.6805715482629,-13.6595384954442,
113.200229910458)) ;
#168647 = CARTESIAN_POINT('Ctrl Pts',(-22.6067677078921,-13.6595385377798,
113.224460961431)) ;
#168648 = CARTESIAN_POINT('Ctrl Pts',(-22.5329638675213,-13.6595385801154,
113.248692012404)) ;
#168649 = CARTESIAN_POINT('Ctrl Pts',(-22.5561014124412,-13.643415658276,
113.31916524184)) ;
#168650 = CARTESIAN_POINT('Ctrl Pts',(-22.5598524729045,-13.3531854263633,
113.295142705237)) ;
#168651 = CARTESIAN_POINT('Ctrl Pts',(-22.5834950317507,-13.3573028544331,
113.367154125775)) ;
#168652 = CARTESIAN_POINT('Ctrl Pts',(-22.6572988758986,-13.3573028025058,
113.342923086306)) ;
#168653 = CARTESIAN_POINT('Ctrl Pts',(-22.7311027200465,-13.3573027505784,
113.318692046837)) ;
#168654 = CARTESIAN_POINT('Ctrl Pts',(-22.7074601612002,-13.3531853225086,
113.2466806263)) ;
#168655 = CARTESIAN_POINT('Ctrl Pts',(-22.683817602354,-13.3490678944388,
113.174669205762)) ;
#168656 = CARTESIAN_POINT('Ctrl Pts',(-22.6100137582061,-13.3490679463661,
113.198900245231)) ;
#168657 = CARTESIAN_POINT('Ctrl Pts',(-22.5362099140582,-13.3490679982935,
113.2231312847)) ;
#168658 = CARTESIAN_POINT('Ctrl Pts',(-22.5598524729045,-13.3531854263633,
113.295142705237)) ;
#168659 = CARTESIAN_POINT('Ctrl Pts',(-22.5878485384446,-13.0673885224611,
113.344945022211)) ;
#168660 = CARTESIAN_POINT('Ctrl Pts',(-22.6103045670656,-13.0914657876093,
113.413342463295)) ;
#168661 = CARTESIAN_POINT('Ctrl Pts',(-22.6841084163441,-13.0914657299476,
113.389111439454)) ;
#168662 = CARTESIAN_POINT('Ctrl Pts',(-22.7579122656227,-13.0914656722859,
113.364880415613)) ;
#168663 = CARTESIAN_POINT('Ctrl Pts',(-22.7354562370017,-13.0673884071377,
113.296482974528)) ;
#168664 = CARTESIAN_POINT('Ctrl Pts',(-22.7130002083808,-13.0433111419895,
113.228085533443)) ;
#168665 = CARTESIAN_POINT('Ctrl Pts',(-22.6391963591022,-13.0433111996512,
113.252316557285)) ;
#168666 = CARTESIAN_POINT('Ctrl Pts',(-22.5653925098236,-13.0433112573129,
113.276547581126)) ;
#168667 = CARTESIAN_POINT('Ctrl Pts',(-22.5878485384446,-13.0673885224611,
113.344945022211)) ;
#168668 = CARTESIAN_POINT('Ctrl Pts',(-22.6389570341485,-12.8066409255768,
113.465116760669)) ;
#168669 = CARTESIAN_POINT('Ctrl Pts',(-22.6586117821665,-12.8489579270799,
113.524981953187)) ;
#168670 = CARTESIAN_POINT('Ctrl Pts',(-22.7324156375432,-12.8489578695406,
113.50075094792)) ;
#168671 = CARTESIAN_POINT('Ctrl Pts',(-22.8062194929197,-12.8489578120014,
113.476519942652)) ;
#168672 = CARTESIAN_POINT('Ctrl Pts',(-22.7865647449017,-12.8066408104982,
113.416654750134)) ;
#168673 = CARTESIAN_POINT('Ctrl Pts',(-22.7669099968836,-12.7643238089951,
113.356789557615)) ;
#168674 = CARTESIAN_POINT('Ctrl Pts',(-22.693106141507,-12.7643238665344,
113.381020562883)) ;
#168675 = CARTESIAN_POINT('Ctrl Pts',(-22.6193022861304,-12.7643239240736,
113.405251568151)) ;
#168676 = CARTESIAN_POINT('Ctrl Pts',(-22.6389570341485,-12.8066409255768,
113.465116760669)) ;
#168677 = CARTESIAN_POINT('Ctrl Pts',(-22.7097903100766,-12.5904014103484,
113.645526694695)) ;
#168678 = CARTESIAN_POINT('Ctrl Pts',(-22.7252592148691,-12.6478767369269,
113.692642484262)) ;
#168679 = CARTESIAN_POINT('Ctrl Pts',(-22.7990630761565,-12.6478766870741,
113.668411496998)) ;
#168680 = CARTESIAN_POINT('Ctrl Pts',(-22.872866937444,-12.6478766372212,
113.644180509733)) ;
#168681 = CARTESIAN_POINT('Ctrl Pts',(-22.8573980326515,-12.5904013106426,
113.597064720167)) ;
#168682 = CARTESIAN_POINT('Ctrl Pts',(-22.8419291278591,-12.5329259840641,
113.5499489306)) ;
#168683 = CARTESIAN_POINT('Ctrl Pts',(-22.7681252665716,-12.5329260339169,
113.574179917864)) ;
#168684 = CARTESIAN_POINT('Ctrl Pts',(-22.6943214052842,-12.5329260837698,
113.598410905129)) ;
#168685 = CARTESIAN_POINT('Ctrl Pts',(-22.7097903100766,-12.5904014103484,
113.645526694695)) ;
#168686 = CARTESIAN_POINT('Ctrl Pts',(-22.7973377104979,-12.4318423089519,
113.876458241546)) ;
#168687 = CARTESIAN_POINT('Ctrl Pts',(-22.807456155429,-12.500471718984,113.907277393848)) ;
#168688 = CARTESIAN_POINT('Ctrl Pts',(-22.8812600228401,-12.5004716824447,
113.883046425235)) ;
#168689 = CARTESIAN_POINT('Ctrl Pts',(-22.9550638902512,-12.5004716459054,
113.858815456623)) ;
#168690 = CARTESIAN_POINT('Ctrl Pts',(-22.94494544532,-12.4318422358733,113.827996304321)) ;
#168691 = CARTESIAN_POINT('Ctrl Pts',(-22.9348270003888,-12.3632128258413,
113.797177152019)) ;
#168692 = CARTESIAN_POINT('Ctrl Pts',(-22.8610231329778,-12.3632128623805,
113.821408120632)) ;
#168693 = CARTESIAN_POINT('Ctrl Pts',(-22.7872192655667,-12.3632128989198,
113.845639089245)) ;
#168694 = CARTESIAN_POINT('Ctrl Pts',(-22.7973377104979,-12.4318423089519,
113.876458241546)) ;
#168695 = CARTESIAN_POINT('Ctrl Pts',(-22.8940411989731,-12.3456712150683,
114.135732174982)) ;
#168696 = CARTESIAN_POINT('Ctrl Pts',(-22.8981525025119,-12.4204161323536,
114.148254543946)) ;
#168697 = CARTESIAN_POINT('Ctrl Pts',(-22.9719563736072,-12.4204161168077,
114.124023586555)) ;
#168698 = CARTESIAN_POINT('Ctrl Pts',(-23.0457602447025,-12.4204161012619,
114.099792629164)) ;
#168699 = CARTESIAN_POINT('Ctrl Pts',(-23.0416489411638,-12.3456711839767,
114.0872702602)) ;
#168700 = CARTESIAN_POINT('Ctrl Pts',(-23.037537637625,-12.2709262666914,
114.074747891236)) ;
#168701 = CARTESIAN_POINT('Ctrl Pts',(-22.9637337665296,-12.2709262822373,
114.098978848627)) ;
#168702 = CARTESIAN_POINT('Ctrl Pts',(-22.8899298954343,-12.2709262977831,
114.123209806018)) ;
#168703 = CARTESIAN_POINT('Ctrl Pts',(-22.8940411989731,-12.3456712150683,
114.135732174982)) ;
#168704 = CARTESIAN_POINT('Ctrl Pts',(-22.9953415992751,-12.3353742164119,
114.408800882689)) ;
#168705 = CARTESIAN_POINT('Ctrl Pts',(-22.9931205397198,-12.4109469942247,
114.402035895503)) ;
#168706 = CARTESIAN_POINT('Ctrl Pts',(-23.0669244128859,-12.4109470032869,
114.377804944419)) ;
#168707 = CARTESIAN_POINT('Ctrl Pts',(-23.1407282860521,-12.410947012349,
114.353573993335)) ;
#168708 = CARTESIAN_POINT('Ctrl Pts',(-23.1429493456074,-12.3353742345363,
114.360338980522)) ;
#168709 = CARTESIAN_POINT('Ctrl Pts',(-23.1451704051626,-12.2598014567236,
114.367103967708)) ;
#168710 = CARTESIAN_POINT('Ctrl Pts',(-23.0713665319965,-12.2598014476614,
114.391334918792)) ;
#168711 = CARTESIAN_POINT('Ctrl Pts',(-22.9975626588303,-12.2598014385992,
114.415565869876)) ;
#168712 = CARTESIAN_POINT('Ctrl Pts',(-22.9953415992751,-12.3353742164119,
114.408800882689)) ;
#168713 = CARTESIAN_POINT('Ctrl Pts',(-23.0941945934012,-12.402733699683,
114.674438282461)) ;
#168714 = CARTESIAN_POINT('Ctrl Pts',(-23.0858023223332,-12.473714122898,
114.648876780817)) ;
#168715 = CARTESIAN_POINT('Ctrl Pts',(-23.1596061950238,-12.4737141587005,
114.624645828285)) ;
#168716 = CARTESIAN_POINT('Ctrl Pts',(-23.2334100677144,-12.473714194503,
114.600414875753)) ;
#168717 = CARTESIAN_POINT('Ctrl Pts',(-23.2418023387824,-12.402733771288,
114.625976377397)) ;
#168718 = CARTESIAN_POINT('Ctrl Pts',(-23.2501946098504,-12.331753348073,
114.651537879041)) ;
#168719 = CARTESIAN_POINT('Ctrl Pts',(-23.1763907371598,-12.3317533122705,
114.675768831573)) ;
#168720 = CARTESIAN_POINT('Ctrl Pts',(-23.1025868644692,-12.331753276468,
114.699999784105)) ;
#168721 = CARTESIAN_POINT('Ctrl Pts',(-23.0941945934012,-12.402733699683,
114.674438282461)) ;
#168722 = CARTESIAN_POINT('Ctrl Pts',(-23.1845580290586,-12.5432714498278,
114.914111547974)) ;
#168723 = CARTESIAN_POINT('Ctrl Pts',(-23.1705803992153,-12.6045444668254,
114.871537944772)) ;
#168724 = CARTESIAN_POINT('Ctrl Pts',(-23.244384268865,-12.6045445287426,
114.847306982978)) ;
#168725 = CARTESIAN_POINT('Ctrl Pts',(-23.3181881385147,-12.6045445906598,
114.823076021184)) ;
#168726 = CARTESIAN_POINT('Ctrl Pts',(-23.332165768358,-12.5432715736621,
114.865649624386)) ;
#168727 = CARTESIAN_POINT('Ctrl Pts',(-23.3461433982013,-12.4819985566645,
114.908223227588)) ;
#168728 = CARTESIAN_POINT('Ctrl Pts',(-23.2723395285516,-12.4819984947474,
114.932454189382)) ;
#168729 = CARTESIAN_POINT('Ctrl Pts',(-23.1985356589018,-12.4819984328302,
114.956685151176)) ;
#168730 = CARTESIAN_POINT('Ctrl Pts',(-23.1845580290586,-12.5432714498278,
114.914111547974)) ;
#168731 = CARTESIAN_POINT('Ctrl Pts',(-23.2601807339086,-12.7462375607508,
115.108986544249)) ;
#168732 = CARTESIAN_POINT('Ctrl Pts',(-23.2416365667801,-12.7934303811122,
115.052504005331)) ;
#168733 = CARTESIAN_POINT('Ctrl Pts',(-23.3154404307945,-12.7934304650843,
115.028273026373)) ;
#168734 = CARTESIAN_POINT('Ctrl Pts',(-23.3892442948089,-12.7934305490564,
115.004042047414)) ;
#168735 = CARTESIAN_POINT('Ctrl Pts',(-23.4077884619374,-12.746237728695,
115.060524586332)) ;
#168736 = CARTESIAN_POINT('Ctrl Pts',(-23.4263326290658,-12.6990449083337,
115.11700712525)) ;
#168737 = CARTESIAN_POINT('Ctrl Pts',(-23.3525287650514,-12.6990448243616,
115.141238104209)) ;
#168738 = CARTESIAN_POINT('Ctrl Pts',(-23.278724901037,-12.6990447403895,
115.165469083167)) ;
#168739 = CARTESIAN_POINT('Ctrl Pts',(-23.2601807339086,-12.7462375607508,
115.108986544249)) ;
#168740 = CARTESIAN_POINT('Ctrl Pts',(-23.3166354321301,-12.9968255702811,
115.245531849597)) ;
#168741 = CARTESIAN_POINT('Ctrl Pts',(-23.2948551085598,-13.0265927652578,
115.179192500334)) ;
#168742 = CARTESIAN_POINT('Ctrl Pts',(-23.368658965033,-13.0265928649381,
115.154961498407)) ;
#168743 = CARTESIAN_POINT('Ctrl Pts',(-23.4424628215062,-13.0265929646183,
115.130730496479)) ;
#168744 = CARTESIAN_POINT('Ctrl Pts',(-23.4642431450764,-12.9968257696416,
115.197069845742)) ;
#168745 = CARTESIAN_POINT('Ctrl Pts',(-23.4860234686466,-12.9670585746648,
115.263409195005)) ;
#168746 = CARTESIAN_POINT('Ctrl Pts',(-23.4122196121735,-12.9670584749846,
115.287640196933)) ;
#168747 = CARTESIAN_POINT('Ctrl Pts',(-23.3384157557003,-12.9670583753043,
115.31187119886)) ;
#168748 = CARTESIAN_POINT('Ctrl Pts',(-23.3166354321301,-12.9968255702811,
115.245531849597)) ;
#168749 = CARTESIAN_POINT('Ctrl Pts',(-23.3507793496113,-13.2777710794654,
115.314086325876)) ;
#168750 = CARTESIAN_POINT('Ctrl Pts',(-23.3273163717843,-13.2879677234676,
115.242621883247)) ;
#168751 = CARTESIAN_POINT('Ctrl Pts',(-23.4011202195342,-13.2879678309871,
115.21839085475)) ;
#168752 = CARTESIAN_POINT('Ctrl Pts',(-23.474924067284,-13.2879679385065,
115.194159826252)) ;
#168753 = CARTESIAN_POINT('Ctrl Pts',(-23.498387045111,-13.2777712945044,
115.26562426888)) ;
#168754 = CARTESIAN_POINT('Ctrl Pts',(-23.521850022938,-13.2675746505022,
115.337088711509)) ;
#168755 = CARTESIAN_POINT('Ctrl Pts',(-23.4480461751882,-13.2675745429828,
115.361319740006)) ;
#168756 = CARTESIAN_POINT('Ctrl Pts',(-23.3742423274384,-13.2675744354633,
115.385550768504)) ;
#168757 = CARTESIAN_POINT('Ctrl Pts',(-23.3507793496113,-13.2777710794654,
115.314086325876)) ;
#168758 = CARTESIAN_POINT('Ctrl Pts',(-23.3608646469754,-13.5692121151867,
115.309310772099)) ;
#168759 = CARTESIAN_POINT('Ctrl Pts',(-23.3373971099136,-13.5590766136152,
115.23783244276)) ;
#168760 = CARTESIAN_POINT('Ctrl Pts',(-23.4112009485982,-13.5590767201184,
115.213601386652)) ;
#168761 = CARTESIAN_POINT('Ctrl Pts',(-23.4850047872827,-13.5590768266217,
115.189370330543)) ;
#168762 = CARTESIAN_POINT('Ctrl Pts',(-23.5084723243445,-13.5692123281932,
115.260848659881)) ;
#168763 = CARTESIAN_POINT('Ctrl Pts',(-23.5319398614064,-13.5793478297647,
115.332326989219)) ;
#168764 = CARTESIAN_POINT('Ctrl Pts',(-23.4581360227218,-13.5793477232615,
115.356558045328)) ;
#168765 = CARTESIAN_POINT('Ctrl Pts',(-23.3843321840373,-13.5793476167582,
115.380789101437)) ;
#168766 = CARTESIAN_POINT('Ctrl Pts',(-23.3608646469754,-13.5692121151867,
115.309310772099)) ;
#168767 = CARTESIAN_POINT('Ctrl Pts',(-23.3467205470048,-13.8503430324929,
115.230657743514)) ;
#168768 = CARTESIAN_POINT('Ctrl Pts',(-23.3249414773231,-13.8205648157971,
115.164322213335)) ;
#168769 = CARTESIAN_POINT('Ctrl Pts',(-23.3987453076205,-13.8205649121888,
115.140091131681)) ;
#168770 = CARTESIAN_POINT('Ctrl Pts',(-23.4725491379179,-13.8205650085804,
115.115860050026)) ;
#168771 = CARTESIAN_POINT('Ctrl Pts',(-23.4943282075997,-13.8503432252762,
115.182195580204)) ;
#168772 = CARTESIAN_POINT('Ctrl Pts',(-23.5161072772814,-13.880121441972,
115.248531110382)) ;
#168773 = CARTESIAN_POINT('Ctrl Pts',(-23.442303446984,-13.8801213455804,
115.272762192037)) ;
#168774 = CARTESIAN_POINT('Ctrl Pts',(-23.3684996166866,-13.8801212491888,
115.296993273692)) ;
#168775 = CARTESIAN_POINT('Ctrl Pts',(-23.3467205470048,-13.8503430324929,
115.230657743514)) ;
#168776 = CARTESIAN_POINT('Ctrl Pts',(-23.3104950812117,-14.0986233529731,
115.085011079683)) ;
#168777 = CARTESIAN_POINT('Ctrl Pts',(-23.2919434103993,-14.0514664875456,
115.028505685671)) ;
#168778 = CARTESIAN_POINT('Ctrl Pts',(-23.3657472337263,-14.0514665673178,
115.004274582785)) ;
#168779 = CARTESIAN_POINT('Ctrl Pts',(-23.4395510570533,-14.05146664709,114.9800434799)) ;
#168780 = CARTESIAN_POINT('Ctrl Pts',(-23.4581027278657,-14.0986235125175,
115.036548873912)) ;
#168781 = CARTESIAN_POINT('Ctrl Pts',(-23.4766543986781,-14.145780377945,
115.093054267924)) ;
#168782 = CARTESIAN_POINT('Ctrl Pts',(-23.4028505753511,-14.1457802981728,
115.11728537081)) ;
#168783 = CARTESIAN_POINT('Ctrl Pts',(-23.3290467520241,-14.1457802184006,
115.141516473695)) ;
#168784 = CARTESIAN_POINT('Ctrl Pts',(-23.3104950812117,-14.0986233529731,
115.085011079683)) ;
#168785 = CARTESIAN_POINT('Ctrl Pts',(-23.2552110709686,-14.2995832696182,
114.881140254992)) ;
#168786 = CARTESIAN_POINT('Ctrl Pts',(-23.2412255998243,-14.2383253097085,
114.838542768335)) ;
#168787 = CARTESIAN_POINT('Ctrl Pts',(-23.315029418276,-14.2383253669594,
114.8143116506)) ;
#168788 = CARTESIAN_POINT('Ctrl Pts',(-23.3888332367278,-14.2383254242103,
114.790080532865)) ;
#168789 = CARTESIAN_POINT('Ctrl Pts',(-23.402818707872,-14.29958338412,114.832678019522)) ;
#168790 = CARTESIAN_POINT('Ctrl Pts',(-23.4168041790163,-14.3608413440297,
114.875275506179)) ;
#168791 = CARTESIAN_POINT('Ctrl Pts',(-23.3430003605645,-14.3608412867788,
114.899506623914)) ;
#168792 = CARTESIAN_POINT('Ctrl Pts',(-23.2691965421128,-14.3608412295279,
114.923737741649)) ;
#168793 = CARTESIAN_POINT('Ctrl Pts',(-23.2552110709686,-14.2995832696182,
114.881140254992)) ;
#168794 = CARTESIAN_POINT('Ctrl Pts',(-23.1854571810787,-14.4373031232107,
114.633125479994)) ;
#168795 = CARTESIAN_POINT('Ctrl Pts',(-23.1770564137006,-14.3663375815008,
114.607538099809)) ;
#168796 = CARTESIAN_POINT('Ctrl Pts',(-23.2508602299918,-14.3663376133963,
114.583306975493)) ;
#168797 = CARTESIAN_POINT('Ctrl Pts',(-23.3246640462829,-14.3663376452917,
114.559075851177)) ;
#168798 = CARTESIAN_POINT('Ctrl Pts',(-23.3330648136609,-14.4373031870016,
114.584663231363)) ;
#168799 = CARTESIAN_POINT('Ctrl Pts',(-23.341465581039,-14.5082687287115,
114.610250611548)) ;
#168800 = CARTESIAN_POINT('Ctrl Pts',(-23.2676617647479,-14.5082686968161,
114.634481735864)) ;
#168801 = CARTESIAN_POINT('Ctrl Pts',(-23.1938579484568,-14.5082686649206,
114.65871286018)) ;
#168802 = CARTESIAN_POINT('Ctrl Pts',(-23.1854571810787,-14.4373031232107,
114.633125479994)) ;
#168803 = CARTESIAN_POINT('Ctrl Pts',(-23.1076519671601,-14.5016051754735,
114.360797992838)) ;
#168804 = CARTESIAN_POINT('Ctrl Pts',(-23.1054022061001,-14.4260436157556,
114.353945585335)) ;
#168805 = CARTESIAN_POINT('Ctrl Pts',(-23.1792060223591,-14.4260436229732,
114.329714460921)) ;
#168806 = CARTESIAN_POINT('Ctrl Pts',(-23.2530098386182,-14.4260436301907,
114.305483336507)) ;
#168807 = CARTESIAN_POINT('Ctrl Pts',(-23.2552595996782,-14.5016051899087,
114.31233574401)) ;
#168808 = CARTESIAN_POINT('Ctrl Pts',(-23.2575093607382,-14.5771667496267,
114.319188151513)) ;
#168809 = CARTESIAN_POINT('Ctrl Pts',(-23.1837055444792,-14.5771667424091,
114.343419275927)) ;
#168810 = CARTESIAN_POINT('Ctrl Pts',(-23.1099017282202,-14.5771667351915,
114.367650400341)) ;
#168811 = CARTESIAN_POINT('Ctrl Pts',(-23.1076519671601,-14.5016051754735,
114.360797992838)) ;
#168812 = CARTESIAN_POINT('Ctrl Pts',(-23.0272520332699,-14.4885235205326,
114.080367454721)) ;
#168813 = CARTESIAN_POINT('Ctrl Pts',(-23.031347792647,-14.4137610040608,
114.092842478479)) ;
#168814 = CARTESIAN_POINT('Ctrl Pts',(-23.1051516115704,-14.4137609891403,
114.06861136218)) ;
#168815 = CARTESIAN_POINT('Ctrl Pts',(-23.1789554304938,-14.4137609742198,
114.044380245882)) ;
#168816 = CARTESIAN_POINT('Ctrl Pts',(-23.1748596711167,-14.4885234906916,
114.031905222124)) ;
#168817 = CARTESIAN_POINT('Ctrl Pts',(-23.1707639117397,-14.5632860071634,
114.019430198366)) ;
#168818 = CARTESIAN_POINT('Ctrl Pts',(-23.0969600928162,-14.5632860220839,
114.043661314664)) ;
#168819 = CARTESIAN_POINT('Ctrl Pts',(-23.0231562738928,-14.5632860370044,
114.067892430963)) ;
#168820 = CARTESIAN_POINT('Ctrl Pts',(-23.0272520332699,-14.4885235205326,
114.080367454721)) ;
#168821 = CARTESIAN_POINT('Ctrl Pts',(-22.9514685700045,-14.3988909925641,
113.814136978792)) ;
#168822 = CARTESIAN_POINT('Ctrl Pts',(-22.9615943154396,-14.3302736656516,
113.844978367012)) ;
#168823 = CARTESIAN_POINT('Ctrl Pts',(-23.0353981384749,-14.3302736334562,
113.820747263238)) ;
#168824 = CARTESIAN_POINT('Ctrl Pts',(-23.1092019615102,-14.3302736012609,
113.796516159463)) ;
#168825 = CARTESIAN_POINT('Ctrl Pts',(-23.0990762160752,-14.3988909281734,
113.765674771244)) ;
#168826 = CARTESIAN_POINT('Ctrl Pts',(-23.0889504706401,-14.4675082550859,
113.734833383024)) ;
#168827 = CARTESIAN_POINT('Ctrl Pts',(-23.0151466476048,-14.4675082872812,
113.759064486798)) ;
#168828 = CARTESIAN_POINT('Ctrl Pts',(-22.9413428245695,-14.4675083194766,
113.783295590572)) ;
#168829 = CARTESIAN_POINT('Ctrl Pts',(-22.9514685700045,-14.3988909925641,
113.814136978792)) ;
#168830 = CARTESIAN_POINT('Ctrl Pts',(-22.8859156809784,-14.2382785177405,
113.578895834363)) ;
#168831 = CARTESIAN_POINT('Ctrl Pts',(-22.9013699117956,-14.1807709154062,
113.625966929132)) ;
#168832 = CARTESIAN_POINT('Ctrl Pts',(-22.9751737403754,-14.180770872992,
113.601735842246)) ;
#168833 = CARTESIAN_POINT('Ctrl Pts',(-23.0489775689551,-14.1807708305777,
113.577504755359)) ;
#168834 = CARTESIAN_POINT('Ctrl Pts',(-23.0335233381379,-14.2382784329119,
113.53043366059)) ;
#168835 = CARTESIAN_POINT('Ctrl Pts',(-23.0180691073207,-14.2957860352462,
113.483362565821)) ;
#168836 = CARTESIAN_POINT('Ctrl Pts',(-22.9442652787409,-14.2957860776604,
113.507593652707)) ;
#168837 = CARTESIAN_POINT('Ctrl Pts',(-22.8704614501611,-14.2957861200747,
113.531824739594)) ;
#168838 = CARTESIAN_POINT('Ctrl Pts',(-22.8859156809784,-14.2382785177405,
113.578895834363)) ;
#168839 = CARTESIAN_POINT('Ctrl Pts',(-22.8366909878539,-14.0201835577284,
113.393629387852)) ;
#168840 = CARTESIAN_POINT('Ctrl Pts',(-22.8563366770582,-13.9778166138277,
113.453466988439)) ;
#168841 = CARTESIAN_POINT('Ctrl Pts',(-22.9301405109221,-13.9778165664169,
113.429235917646)) ;
#168842 = CARTESIAN_POINT('Ctrl Pts',(-23.003944344786,-13.9778165190061,
113.405004846854)) ;
#168843 = CARTESIAN_POINT('Ctrl Pts',(-22.9842986555816,-14.0201834629068,
113.345167246267)) ;
#168844 = CARTESIAN_POINT('Ctrl Pts',(-22.9646529663773,-14.0625504068075,
113.28532964568)) ;
#168845 = CARTESIAN_POINT('Ctrl Pts',(-22.8908491325134,-14.0625504542183,
113.309560716472)) ;
#168846 = CARTESIAN_POINT('Ctrl Pts',(-22.8170452986496,-14.0625505016291,
113.333791787265)) ;
#168847 = CARTESIAN_POINT('Ctrl Pts',(-22.8366909878539,-14.0201835577284,
113.393629387852)) ;
#168848 = CARTESIAN_POINT('Ctrl Pts',(-22.8074315802463,-13.7575805640437,
113.268949038296)) ;
#168849 = CARTESIAN_POINT('Ctrl Pts',(-22.829885948188,-13.7334844884055,
113.337341420952)) ;
#168850 = CARTESIAN_POINT('Ctrl Pts',(-22.9036897872937,-13.7334844436557,
113.313110366126)) ;
#168851 = CARTESIAN_POINT('Ctrl Pts',(-22.9774936263994,-13.7334843989059,
113.288879311299)) ;
#168852 = CARTESIAN_POINT('Ctrl Pts',(-22.9550392584577,-13.7575804745442,
113.220486928643)) ;
#168853 = CARTESIAN_POINT('Ctrl Pts',(-22.9325848905159,-13.7816765501825,
113.152094545987)) ;
#168854 = CARTESIAN_POINT('Ctrl Pts',(-22.8587810514102,-13.7816765949322,
113.176325600813)) ;
#168855 = CARTESIAN_POINT('Ctrl Pts',(-22.7849772123045,-13.781676639682,
113.20055665564)) ;
#168856 = CARTESIAN_POINT('Ctrl Pts',(-22.8074315802463,-13.7575805640437,
113.268949038296)) ;
#168857 = CARTESIAN_POINT('Ctrl Pts',(-22.8014281414069,-13.4715356144856,
113.215234575554)) ;
#168858 = CARTESIAN_POINT('Ctrl Pts',(-22.8250688612617,-13.467375361388,
113.287240394559)) ;
#168859 = CARTESIAN_POINT('Ctrl Pts',(-22.8988727043007,-13.4673753229371,
113.263009351712)) ;
#168860 = CARTESIAN_POINT('Ctrl Pts',(-22.9726765473396,-13.4673752844861,
113.238778308866)) ;
#168861 = CARTESIAN_POINT('Ctrl Pts',(-22.9490358274848,-13.4715355375837,
113.166772489861)) ;
#168862 = CARTESIAN_POINT('Ctrl Pts',(-22.92539510763,-13.4756957906813,113.094766670856)) ;
#168863 = CARTESIAN_POINT('Ctrl Pts',(-22.8515912645911,-13.4756958291323,
113.118997713702)) ;
#168864 = CARTESIAN_POINT('Ctrl Pts',(-22.7777874215521,-13.4756958675833,
113.143228756549)) ;
#168865 = CARTESIAN_POINT('Ctrl Pts',(-22.8014281414069,-13.4715356144856,
113.215234575554)) ;
#168866 = CARTESIAN_POINT('Ctrl Pts',(-22.8195788653586,-13.1815808813972,
113.235079702884)) ;
#168867 = CARTESIAN_POINT('Ctrl Pts',(-22.8427214378284,-13.1976597435624,
113.30556824517)) ;
#168868 = CARTESIAN_POINT('Ctrl Pts',(-22.9165252835433,-13.1976597143198,
113.281337210474)) ;
#168869 = CARTESIAN_POINT('Ctrl Pts',(-22.9903291292582,-13.1976596850772,
113.257106175778)) ;
#168870 = CARTESIAN_POINT('Ctrl Pts',(-22.9671865567883,-13.1815808229121,
113.186617633492)) ;
#168871 = CARTESIAN_POINT('Ctrl Pts',(-22.9440439843185,-13.1655019607469,
113.116129091206)) ;
#168872 = CARTESIAN_POINT('Ctrl Pts',(-22.8702401386036,-13.1655019899895,
113.140360125902)) ;
#168873 = CARTESIAN_POINT('Ctrl Pts',(-22.7964362928887,-13.1655020192321,
113.164591160598)) ;
#168874 = CARTESIAN_POINT('Ctrl Pts',(-22.8195788653586,-13.1815808813972,
113.235079702884)) ;
#168875 = CARTESIAN_POINT('Ctrl Pts',(-22.8617885311853,-12.9071949482228,
113.328012511746)) ;
#168876 = CARTESIAN_POINT('Ctrl Pts',(-22.8827563840684,-12.9424572144763,
113.391877208875)) ;
#168877 = CARTESIAN_POINT('Ctrl Pts',(-22.9565602306879,-12.9424571966172,
113.367646176935)) ;
#168878 = CARTESIAN_POINT('Ctrl Pts',(-23.0303640773074,-12.9424571787581,
113.343415144994)) ;
#168879 = CARTESIAN_POINT('Ctrl Pts',(-23.0093962244244,-12.9071949125046,
113.279550447865)) ;
#168880 = CARTESIAN_POINT('Ctrl Pts',(-22.9884283715413,-12.8719326462511,
113.215685750736)) ;
#168881 = CARTESIAN_POINT('Ctrl Pts',(-22.9146245249218,-12.8719326641102,
113.239916782676)) ;
#168882 = CARTESIAN_POINT('Ctrl Pts',(-22.8408206783023,-12.8719326819694,
113.264147814617)) ;
#168883 = CARTESIAN_POINT('Ctrl Pts',(-22.8617885311853,-12.9071949482228,
113.328012511746)) ;
#168884 = CARTESIAN_POINT('Ctrl Pts',(-22.9249619978587,-12.6718251326146,
113.485139268914)) ;
#168885 = CARTESIAN_POINT('Ctrl Pts',(-22.9422806312259,-12.723574947821,
113.537889032084)) ;
#168886 = CARTESIAN_POINT('Ctrl Pts',(-23.0160844779008,-12.7235749374657,
113.513658000312)) ;
#168887 = CARTESIAN_POINT('Ctrl Pts',(-23.0898883245757,-12.7235749271105,
113.48942696854)) ;
#168888 = CARTESIAN_POINT('Ctrl Pts',(-23.0725696912085,-12.6718251119041,
113.43667720537)) ;
#168889 = CARTESIAN_POINT('Ctrl Pts',(-23.0552510578412,-12.6200752966978,
113.3839274422)) ;
#168890 = CARTESIAN_POINT('Ctrl Pts',(-22.9814472111664,-12.620075307053,
113.408158473972)) ;
#168891 = CARTESIAN_POINT('Ctrl Pts',(-22.9076433644914,-12.6200753174082,
113.432389505744)) ;
#168892 = CARTESIAN_POINT('Ctrl Pts',(-22.9249619978587,-12.6718251326146,
113.485139268914)) ;
#168893 = CARTESIAN_POINT('Ctrl Pts',(-23.0059942336063,-12.4884732056212,
113.696495324864)) ;
#168894 = CARTESIAN_POINT('Ctrl Pts',(-23.0184146037982,-12.553103678643,
113.734325768607)) ;
#168895 = CARTESIAN_POINT('Ctrl Pts',(-23.0922184494783,-12.5531036749217,
113.710094733805)) ;
#168896 = CARTESIAN_POINT('Ctrl Pts',(-23.1660222951584,-12.5531036712005,
113.685863699003)) ;
#168897 = CARTESIAN_POINT('Ctrl Pts',(-23.1536019249665,-12.4884731981787,
113.64803325526)) ;
#168898 = CARTESIAN_POINT('Ctrl Pts',(-23.1411815547745,-12.4238427251569,
113.610202811517)) ;
#168899 = CARTESIAN_POINT('Ctrl Pts',(-23.0673777090945,-12.4238427288782,
113.634433846319)) ;
#168900 = CARTESIAN_POINT('Ctrl Pts',(-22.9935738634144,-12.4238427325995,
113.658664881121)) ;
#168901 = CARTESIAN_POINT('Ctrl Pts',(-23.0059942336063,-12.4884732056212,
113.696495324864)) ;
#168902 = CARTESIAN_POINT('Ctrl Pts',(-23.1000078654876,-12.3715751089405,
113.947282082598)) ;
#168903 = CARTESIAN_POINT('Ctrl Pts',(-23.1066182036233,-12.4444657268571,
113.967416106029)) ;
#168904 = CARTESIAN_POINT('Ctrl Pts',(-23.1804220477466,-12.4444657266469,
113.943185066485)) ;
#168905 = CARTESIAN_POINT('Ctrl Pts',(-23.2542258918699,-12.4444657264366,
113.918954026941)) ;
#168906 = CARTESIAN_POINT('Ctrl Pts',(-23.2476155537342,-12.3715751085199,
113.89882000351)) ;
#168907 = CARTESIAN_POINT('Ctrl Pts',(-23.2410052155985,-12.2986844906033,
113.878685980079)) ;
#168908 = CARTESIAN_POINT('Ctrl Pts',(-23.1672013714752,-12.2986844908136,
113.902917019623)) ;
#168909 = CARTESIAN_POINT('Ctrl Pts',(-23.0933975273519,-12.2986844910239,
113.927148059167)) ;
#168910 = CARTESIAN_POINT('Ctrl Pts',(-23.1000078654876,-12.3715751089405,
113.947282082598)) ;
#168911 = CARTESIAN_POINT('Ctrl Pts',(-23.2003199061484,-12.3301226383043,
114.217388478731)) ;
#168912 = CARTESIAN_POINT('Ctrl Pts',(-23.2006687533814,-12.4060167548224,
114.218451011093)) ;
#168913 = CARTESIAN_POINT('Ctrl Pts',(-23.2744725964053,-12.4060167550604,
114.1942199682)) ;
#168914 = CARTESIAN_POINT('Ctrl Pts',(-23.3482764394292,-12.4060167552985,
114.169988925308)) ;
#168915 = CARTESIAN_POINT('Ctrl Pts',(-23.3479275921962,-12.3301226387804,
114.168926392946)) ;
#168916 = CARTESIAN_POINT('Ctrl Pts',(-23.3475787449632,-12.2542285222622,
114.167863860585)) ;
#168917 = CARTESIAN_POINT('Ctrl Pts',(-23.2737749019393,-12.2542285220242,
114.192094903477)) ;
#168918 = CARTESIAN_POINT('Ctrl Pts',(-23.1999710589154,-12.2542285217862,
114.216325946369)) ;
#168919 = CARTESIAN_POINT('Ctrl Pts',(-23.2003199061484,-12.3301226383043,
114.217388478731)) ;
#168920 = CARTESIAN_POINT('Ctrl Pts',(-23.3007380070665,-12.3662578527564,
114.487855727773)) ;
#168921 = CARTESIAN_POINT('Ctrl Pts',(-23.2948077898911,-12.4397415757967,
114.469793243034)) ;
#168922 = CARTESIAN_POINT('Ctrl Pts',(-23.3686116323531,-12.4397415751055,
114.44556219843)) ;
#168923 = CARTESIAN_POINT('Ctrl Pts',(-23.4424154748152,-12.4397415744144,
114.421331153827)) ;
#168924 = CARTESIAN_POINT('Ctrl Pts',(-23.4483456919906,-12.366257851374,
114.439393638566)) ;
#168925 = CARTESIAN_POINT('Ctrl Pts',(-23.454275909166,-12.2927741283337,
114.457456123305)) ;
#168926 = CARTESIAN_POINT('Ctrl Pts',(-23.3804720667039,-12.2927741290249,
114.481687167909)) ;
#168927 = CARTESIAN_POINT('Ctrl Pts',(-23.3066682242419,-12.2927741297161,
114.505918212512)) ;
#168928 = CARTESIAN_POINT('Ctrl Pts',(-23.3007380070665,-12.3662578527564,
114.487855727773)) ;
#168929 = CARTESIAN_POINT('Ctrl Pts',(-23.3952053708607,-12.4776432814408,
114.740115458462)) ;
#168930 = CARTESIAN_POINT('Ctrl Pts',(-23.3834038459423,-12.5434578807603,
114.704169917668)) ;
#168931 = CARTESIAN_POINT('Ctrl Pts',(-23.4572076885097,-12.5434578790229,
114.679938873385)) ;
#168932 = CARTESIAN_POINT('Ctrl Pts',(-23.5310115310771,-12.5434578772856,
114.655707829103)) ;
#168933 = CARTESIAN_POINT('Ctrl Pts',(-23.5428130559955,-12.477643277966,
114.691653369897)) ;
#168934 = CARTESIAN_POINT('Ctrl Pts',(-23.5546145809139,-12.4118286786465,
114.727598910691)) ;
#168935 = CARTESIAN_POINT('Ctrl Pts',(-23.4808107383465,-12.4118286803839,
114.751829954974)) ;
#168936 = CARTESIAN_POINT('Ctrl Pts',(-23.4070068957792,-12.4118286821212,
114.776060999257)) ;
#168937 = CARTESIAN_POINT('Ctrl Pts',(-23.3952053708607,-12.4776432814408,
114.740115458462)) ;
#168938 = CARTESIAN_POINT('Ctrl Pts',(-23.4777530924333,-12.6576066827307,
114.955900577125)) ;
#168939 = CARTESIAN_POINT('Ctrl Pts',(-23.460907482304,-12.71095179343,114.904591566696)) ;
#168940 = CARTESIAN_POINT('Ctrl Pts',(-23.5347113257398,-12.7109517930547,
114.880360525058)) ;
#168941 = CARTESIAN_POINT('Ctrl Pts',(-23.6085151691756,-12.7109517926794,
114.856129483421)) ;
#168942 = CARTESIAN_POINT('Ctrl Pts',(-23.6253607793049,-12.6576066819802,
114.907438493849)) ;
#168943 = CARTESIAN_POINT('Ctrl Pts',(-23.6422063894341,-12.604261571281,
114.958747504278)) ;
#168944 = CARTESIAN_POINT('Ctrl Pts',(-23.5684025459984,-12.6042615716562,
114.982978545915)) ;
#168945 = CARTESIAN_POINT('Ctrl Pts',(-23.4945987025626,-12.6042615720315,
115.007209587553)) ;
#168946 = CARTESIAN_POINT('Ctrl Pts',(-23.4777530924333,-12.6576066827307,
114.955900577125)) ;
#168947 = CARTESIAN_POINT('Ctrl Pts',(-23.5422559394209,-12.8904240369604,
115.117024877862)) ;
#168948 = CARTESIAN_POINT('Ctrl Pts',(-23.5216131954621,-12.9275904125638,
115.054150410526)) ;
#168949 = CARTESIAN_POINT('Ctrl Pts',(-23.5954170395086,-12.9275904154763,
115.029919370748)) ;
#168950 = CARTESIAN_POINT('Ctrl Pts',(-23.6692208835552,-12.9275904183888,
115.005688330971)) ;
#168951 = CARTESIAN_POINT('Ctrl Pts',(-23.689863627514,-12.8904240427854,
115.068562798306)) ;
#168952 = CARTESIAN_POINT('Ctrl Pts',(-23.7105063714728,-12.853257667182,
115.131437265642)) ;
#168953 = CARTESIAN_POINT('Ctrl Pts',(-23.6367025274263,-12.8532576642695,
115.15566830542)) ;
#168954 = CARTESIAN_POINT('Ctrl Pts',(-23.5628986833797,-12.853257661357,
115.179899345197)) ;
#168955 = CARTESIAN_POINT('Ctrl Pts',(-23.5422559394209,-12.8904240369604,
115.117024877862)) ;
#168956 = CARTESIAN_POINT('Ctrl Pts',(-23.5857808510703,-13.1612401483887,
115.214177425736)) ;
#168957 = CARTESIAN_POINT('Ctrl Pts',(-23.5628018590313,-13.1795510816038,
115.144187123799)) ;
#168958 = CARTESIAN_POINT('Ctrl Pts',(-23.6366057032453,-13.1795510898929,
115.119956084532)) ;
#168959 = CARTESIAN_POINT('Ctrl Pts',(-23.7104095474593,-13.1795510981819,
115.095725045265)) ;
#168960 = CARTESIAN_POINT('Ctrl Pts',(-23.7333885394984,-13.1612401649668,
115.165715347201)) ;
#168961 = CARTESIAN_POINT('Ctrl Pts',(-23.7563675315375,-13.1429292317516,
115.235705649138)) ;
#168962 = CARTESIAN_POINT('Ctrl Pts',(-23.6825636873234,-13.1429292234626,
115.259936688406)) ;
#168963 = CARTESIAN_POINT('Ctrl Pts',(-23.6087598431094,-13.1429292151735,
115.284167727673)) ;
#168964 = CARTESIAN_POINT('Ctrl Pts',(-23.5857808510703,-13.1612401483887,
115.214177425736)) ;
#168965 = CARTESIAN_POINT('Ctrl Pts',(-23.6057316422003,-13.4512163582634,
115.239436705029)) ;
#168966 = CARTESIAN_POINT('Ctrl Pts',(-23.5820609538197,-13.4493066869731,
115.167339607776)) ;
#168967 = CARTESIAN_POINT('Ctrl Pts',(-23.6558647972831,-13.4493067026551,
115.143108566222)) ;
#168968 = CARTESIAN_POINT('Ctrl Pts',(-23.7296686407465,-13.4493067183372,
115.118877524669)) ;
#168969 = CARTESIAN_POINT('Ctrl Pts',(-23.7533393291271,-13.4512163896275,
115.190974621922)) ;
#168970 = CARTESIAN_POINT('Ctrl Pts',(-23.7770100175077,-13.4531260609178,
115.263071719175)) ;
#168971 = CARTESIAN_POINT('Ctrl Pts',(-23.7032061740443,-13.4531260452357,
115.287302760728)) ;
#168972 = CARTESIAN_POINT('Ctrl Pts',(-23.6294023305809,-13.4531260295536,
115.311533802282)) ;
#168973 = CARTESIAN_POINT('Ctrl Pts',(-23.6057316422003,-13.4512163582634,
115.239436705029)) ;
#168974 = CARTESIAN_POINT('Ctrl Pts',(-23.6013424516955,-13.7384260494091,
115.190608267416)) ;
#168975 = CARTESIAN_POINT('Ctrl Pts',(-23.5786776934113,-13.7164599573725,
115.121575071076)) ;
#168976 = CARTESIAN_POINT('Ctrl Pts',(-23.6524815348966,-13.7164599797673,
115.097344023498)) ;
#168977 = CARTESIAN_POINT('Ctrl Pts',(-23.726285376382,-13.7164600021621,
115.073112975919)) ;
#168978 = CARTESIAN_POINT('Ctrl Pts',(-23.7489501346663,-13.7384260941987,
115.142146172259)) ;
#168979 = CARTESIAN_POINT('Ctrl Pts',(-23.7716148929505,-13.7603921862353,
115.211179368599)) ;
#168980 = CARTESIAN_POINT('Ctrl Pts',(-23.6978110514652,-13.7603921638405,
115.235410416177)) ;
#168981 = CARTESIAN_POINT('Ctrl Pts',(-23.6240072099798,-13.7603921414456,
115.259641463756)) ;
#168982 = CARTESIAN_POINT('Ctrl Pts',(-23.6013424516955,-13.7384260494091,
115.190608267416)) ;
#168983 = CARTESIAN_POINT('Ctrl Pts',(-23.5737147002099,-14.0027479972631,
115.070987295502)) ;
#168984 = CARTESIAN_POINT('Ctrl Pts',(-23.5536801496635,-13.9622948022858,
115.009965287708)) ;
#168985 = CARTESIAN_POINT('Ctrl Pts',(-23.6274839879841,-13.962294829201,
114.985734230491)) ;
#168986 = CARTESIAN_POINT('Ctrl Pts',(-23.7012878263047,-13.9622948561163,
114.961503173273)) ;
#168987 = CARTESIAN_POINT('Ctrl Pts',(-23.7213223768512,-14.0027480510937,
115.022525181066)) ;
#168988 = CARTESIAN_POINT('Ctrl Pts',(-23.7413569273976,-14.0432012460711,
115.08354718886)) ;
#168989 = CARTESIAN_POINT('Ctrl Pts',(-23.667553089077,-14.0432012191558,
115.107778246078)) ;
#168990 = CARTESIAN_POINT('Ctrl Pts',(-23.5937492507564,-14.0432011922405,
115.132009303295)) ;
#168991 = CARTESIAN_POINT('Ctrl Pts',(-23.5737147002099,-14.0027479972631,
115.070987295502)) ;
#168992 = CARTESIAN_POINT('Ctrl Pts',(-23.5256807526921,-14.2248634912547,
114.889270709179)) ;
#168993 = CARTESIAN_POINT('Ctrl Pts',(-23.5097038108168,-14.1688437545673,
114.840607522861)) ;
#168994 = CARTESIAN_POINT('Ctrl Pts',(-23.583507645237,-14.1688437816251,
114.816376453763)) ;
#168995 = CARTESIAN_POINT('Ctrl Pts',(-23.6573114796572,-14.168843808683,
114.792145384665)) ;
#168996 = CARTESIAN_POINT('Ctrl Pts',(-23.6732884215325,-14.2248635453705,
114.840808570983)) ;
#168997 = CARTESIAN_POINT('Ctrl Pts',(-23.6892653634078,-14.2808832820579,
114.889471757302)) ;
#168998 = CARTESIAN_POINT('Ctrl Pts',(-23.6154615289876,-14.2808832550001,
114.913702826399)) ;
#168999 = CARTESIAN_POINT('Ctrl Pts',(-23.5416576945674,-14.2808832279422,
114.937933895497)) ;
#169000 = CARTESIAN_POINT('Ctrl Pts',(-23.5256807526921,-14.2248634912547,
114.889270709179)) ;
#169001 = CARTESIAN_POINT('Ctrl Pts',(-23.461215966023,-14.3897502001773,
114.657418556327)) ;
#169002 = CARTESIAN_POINT('Ctrl Pts',(-23.4504514511971,-14.3221371212432,
114.624631581955)) ;
#169003 = CARTESIAN_POINT('Ctrl Pts',(-23.5242552811751,-14.3221371438564,
114.600400499327)) ;
#169004 = CARTESIAN_POINT('Ctrl Pts',(-23.5980591111531,-14.3221371664696,
114.576169416699)) ;
#169005 = CARTESIAN_POINT('Ctrl Pts',(-23.6088236259791,-14.3897502454037,
114.608956391071)) ;
#169006 = CARTESIAN_POINT('Ctrl Pts',(-23.619588140805,-14.4573633243378,
114.641743365443)) ;
#169007 = CARTESIAN_POINT('Ctrl Pts',(-23.545784310827,-14.4573633017246,
114.665974448071)) ;
#169008 = CARTESIAN_POINT('Ctrl Pts',(-23.471980480849,-14.4573632791114,
114.690205530699)) ;
#169009 = CARTESIAN_POINT('Ctrl Pts',(-23.461215966023,-14.3897502001773,
114.657418556327)) ;
#169010 = CARTESIAN_POINT('Ctrl Pts',(-23.3857401849695,-14.4847583322739,
114.392013776167)) ;
#169011 = CARTESIAN_POINT('Ctrl Pts',(-23.3809646627516,-14.4104140333925,
114.377468307136)) ;
#169012 = CARTESIAN_POINT('Ctrl Pts',(-23.4547684885272,-14.4104140454356,
114.353237211708)) ;
#169013 = CARTESIAN_POINT('Ctrl Pts',(-23.5285723143027,-14.4104140574787,
114.32900611628)) ;
#169014 = CARTESIAN_POINT('Ctrl Pts',(-23.5333478365205,-14.4847583563601,
114.343551585311)) ;
#169015 = CARTESIAN_POINT('Ctrl Pts',(-23.5381233587383,-14.5591026552415,
114.358097054342)) ;
#169016 = CARTESIAN_POINT('Ctrl Pts',(-23.4643195329628,-14.5591026431984,
114.38232814977)) ;
#169017 = CARTESIAN_POINT('Ctrl Pts',(-23.3905157071873,-14.5591026311553,
114.406559245198)) ;
#169018 = CARTESIAN_POINT('Ctrl Pts',(-23.3857401849695,-14.4847583322739,
114.392013776167)) ;
#169019 = CARTESIAN_POINT('Ctrl Pts',(-23.3057972119039,-14.5032991769,114.113141625194)) ;
#169020 = CARTESIAN_POINT('Ctrl Pts',(-23.3073283222928,-14.4275531479525,
114.117805141659)) ;
#169021 = CARTESIAN_POINT('Ctrl Pts',(-23.3811321453339,-14.4275531440522,
114.093574037902)) ;
#169022 = CARTESIAN_POINT('Ctrl Pts',(-23.454935968375,-14.427553140152,114.069342934146)) ;
#169023 = CARTESIAN_POINT('Ctrl Pts',(-23.4534048579861,-14.5032991690996,
114.064679417681)) ;
#169024 = CARTESIAN_POINT('Ctrl Pts',(-23.4518737475972,-14.5790451980471,
114.060015901216)) ;
#169025 = CARTESIAN_POINT('Ctrl Pts',(-23.3780699245561,-14.5790452019473,
114.084247004972)) ;
#169026 = CARTESIAN_POINT('Ctrl Pts',(-23.304266101515,-14.5790452058476,
114.108478108729)) ;
#169027 = CARTESIAN_POINT('Ctrl Pts',(-23.3057972119039,-14.5032991769,114.113141625194)) ;
#169028 = CARTESIAN_POINT('Ctrl Pts',(-23.2272555357364,-14.4441301859155,
113.838399442431)) ;
#169029 = CARTESIAN_POINT('Ctrl Pts',(-23.2350073561252,-14.3724053611762,
113.862010238012)) ;
#169030 = CARTESIAN_POINT('Ctrl Pts',(-23.3088111777221,-14.3724053372545,
113.837779129857)) ;
#169031 = CARTESIAN_POINT('Ctrl Pts',(-23.382614999319,-14.3724053133327,
113.813548021702)) ;
#169032 = CARTESIAN_POINT('Ctrl Pts',(-23.3748631789302,-14.444130138072,
113.789937226121)) ;
#169033 = CARTESIAN_POINT('Ctrl Pts',(-23.3671113585414,-14.5158549628113,
113.76632643054)) ;
#169034 = CARTESIAN_POINT('Ctrl Pts',(-23.2933075369445,-14.5158549867331,
113.790557538695)) ;
#169035 = CARTESIAN_POINT('Ctrl Pts',(-23.2195037153477,-14.5158550106548,
113.81478864685)) ;
#169036 = CARTESIAN_POINT('Ctrl Pts',(-23.2272555357364,-14.4441301859155,
113.838399442431)) ;
#169037 = CARTESIAN_POINT('Ctrl Pts',(-23.1569464450254,-14.3114937407021,
113.588802208014)) ;
#169038 = CARTESIAN_POINT('Ctrl Pts',(-23.1703517418229,-14.2489252476856,
113.629632580692)) ;
#169039 = CARTESIAN_POINT('Ctrl Pts',(-23.2441555643269,-14.2489252018326,
113.6054014753)) ;
#169040 = CARTESIAN_POINT('Ctrl Pts',(-23.317959386831,-14.2489251559797,
113.581170369907)) ;
#169041 = CARTESIAN_POINT('Ctrl Pts',(-23.3045540900335,-14.3114936489961,
113.54033999723)) ;
#169042 = CARTESIAN_POINT('Ctrl Pts',(-23.2911487932361,-14.3740621420126,
113.499509624552)) ;
#169043 = CARTESIAN_POINT('Ctrl Pts',(-23.217344970732,-14.3740621878656,
113.523740729944)) ;
#169044 = CARTESIAN_POINT('Ctrl Pts',(-23.143541148228,-14.3740622337185,
113.547971835337)) ;
#169045 = CARTESIAN_POINT('Ctrl Pts',(-23.1569464450254,-14.3114937407021,
113.588802208014)) ;
#169046 = CARTESIAN_POINT('Ctrl Pts',(-23.1004490169695,-14.114774307687,
113.381241689025)) ;
#169047 = CARTESIAN_POINT('Ctrl Pts',(-23.118552366844,-14.0658491597741,
113.43638157348)) ;
#169048 = CARTESIAN_POINT('Ctrl Pts',(-23.1923561925365,-14.0658490924885,
113.412150477799)) ;
#169049 = CARTESIAN_POINT('Ctrl Pts',(-23.2661600182289,-14.0658490252028,
113.387919382118)) ;
#169050 = CARTESIAN_POINT('Ctrl Pts',(-23.2480566683545,-14.1147741731156,
113.332779497664)) ;
#169051 = CARTESIAN_POINT('Ctrl Pts',(-23.22995331848,-14.1636993210285,113.277639613209)) ;
#169052 = CARTESIAN_POINT('Ctrl Pts',(-23.1561494927875,-14.1636993883142,
113.30187070889)) ;
#169053 = CARTESIAN_POINT('Ctrl Pts',(-23.082345667095,-14.1636994555999,
113.326101804571)) ;
#169054 = CARTESIAN_POINT('Ctrl Pts',(-23.1004490169695,-14.114774307687,
113.381241689025)) ;
#169055 = CARTESIAN_POINT('Ctrl Pts',(-23.062667902268,-13.8682921869894,
113.230716909827)) ;
#169056 = CARTESIAN_POINT('Ctrl Pts',(-23.0841688593971,-13.8365043277557,
113.296205357889)) ;
#169057 = CARTESIAN_POINT('Ctrl Pts',(-23.1579726905666,-13.8365042424835,
113.271974278891)) ;
#169058 = CARTESIAN_POINT('Ctrl Pts',(-23.2317765217361,-13.8365041572113,
113.247743199892)) ;
#169059 = CARTESIAN_POINT('Ctrl Pts',(-23.210275564607,-13.868292016445,113.182254751829)) ;
#169060 = CARTESIAN_POINT('Ctrl Pts',(-23.1887746074778,-13.9000798756787,
113.116766303766)) ;
#169061 = CARTESIAN_POINT('Ctrl Pts',(-23.1149707763083,-13.9000799609509,
113.140997382765)) ;
#169062 = CARTESIAN_POINT('Ctrl Pts',(-23.0411669451388,-13.9000800462231,
113.165228461764)) ;
#169063 = CARTESIAN_POINT('Ctrl Pts',(-23.062667902268,-13.8682921869894,
113.230716909827)) ;
#169064 = CARTESIAN_POINT('Ctrl Pts',(-23.046982381011,-13.5896536678714,
113.147496899994)) ;
#169065 = CARTESIAN_POINT('Ctrl Pts',(-23.0703432142598,-13.5772729173919,
113.218650230723)) ;
#169066 = CARTESIAN_POINT('Ctrl Pts',(-23.1441470526942,-13.5772728198901,
113.194419173852)) ;
#169067 = CARTESIAN_POINT('Ctrl Pts',(-23.2179508911286,-13.5772727223883,
113.170188116981)) ;
#169068 = CARTESIAN_POINT('Ctrl Pts',(-23.1945900578798,-13.5896534728677,
113.099034786252)) ;
#169069 = CARTESIAN_POINT('Ctrl Pts',(-23.1712292246311,-13.6020342233472,
113.027881455524)) ;
#169070 = CARTESIAN_POINT('Ctrl Pts',(-23.0974253861966,-13.6020343208491,
113.052112512395)) ;
#169071 = CARTESIAN_POINT('Ctrl Pts',(-23.0236215477622,-13.6020344183509,
113.076343569266)) ;
#169072 = CARTESIAN_POINT('Ctrl Pts',(-23.046982381011,-13.5896536678714,
113.147496899994)) ;
#169073 = CARTESIAN_POINT('Ctrl Pts',(-23.0553081301007,-13.2982167701219,
113.137350825504)) ;
#169074 = CARTESIAN_POINT('Ctrl Pts',(-23.0788565858859,-13.3061648042617,
113.209075624288)) ;
#169075 = CARTESIAN_POINT('Ctrl Pts',(-23.1526604327469,-13.3061647018305,
113.184844593083)) ;
#169076 = CARTESIAN_POINT('Ctrl Pts',(-23.2264642796078,-13.3061645993992,
113.160613561877)) ;
#169077 = CARTESIAN_POINT('Ctrl Pts',(-23.2029158238225,-13.2982165652594,
113.088888763094)) ;
#169078 = CARTESIAN_POINT('Ctrl Pts',(-23.1793673680372,-13.2902685311196,
113.01716396431)) ;
#169079 = CARTESIAN_POINT('Ctrl Pts',(-23.1055635211763,-13.2902686335509,
113.041394995515)) ;
#169080 = CARTESIAN_POINT('Ctrl Pts',(-23.0317596743153,-13.2902687359821,
113.06562602672)) ;
#169081 = CARTESIAN_POINT('Ctrl Pts',(-23.0553081301007,-13.2982167701219,
113.137350825504)) ;
#169082 = CARTESIAN_POINT('Ctrl Pts',(-23.0878545163832,-13.0155927262678,
113.201000676988)) ;
#169083 = CARTESIAN_POINT('Ctrl Pts',(-23.1098994771013,-13.0432841492844,
113.268146072441)) ;
#169084 = CARTESIAN_POINT('Ctrl Pts',(-23.183703332692,-13.0432840507906,
113.243915067826)) ;
#169085 = CARTESIAN_POINT('Ctrl Pts',(-23.2575071882827,-13.0432839522968,
113.21968406321)) ;
#169086 = CARTESIAN_POINT('Ctrl Pts',(-23.2354622275647,-13.0155925292803,
113.152538667757)) ;
#169087 = CARTESIAN_POINT('Ctrl Pts',(-23.2134172668467,-12.9879011062637,
113.085393272303)) ;
#169088 = CARTESIAN_POINT('Ctrl Pts',(-23.1396134112559,-12.9879012047575,
113.109624276918)) ;
#169089 = CARTESIAN_POINT('Ctrl Pts',(-23.0658095556652,-12.9879013032513,
113.133855281534)) ;
#169090 = CARTESIAN_POINT('Ctrl Pts',(-23.0878545163832,-13.0155927262678,
113.201000676988)) ;
#169091 = CARTESIAN_POINT('Ctrl Pts',(-23.1427829186928,-12.7625129426041,
113.33292942976)) ;
#169092 = CARTESIAN_POINT('Ctrl Pts',(-23.1617573175269,-12.8079141772025,
113.390722389181)) ;
#169093 = CARTESIAN_POINT('Ctrl Pts',(-23.235561181146,-12.8079140912617,
113.366491409019)) ;
#169094 = CARTESIAN_POINT('Ctrl Pts',(-23.3093650447651,-12.8079140053209,
113.342260428856)) ;
#169095 = CARTESIAN_POINT('Ctrl Pts',(-23.290390645931,-12.7625127707225,
113.284467469435)) ;
#169096 = CARTESIAN_POINT('Ctrl Pts',(-23.2714162470969,-12.7171115361241,
113.226674510015)) ;
#169097 = CARTESIAN_POINT('Ctrl Pts',(-23.1976123834778,-12.7171116220649,
113.250905490177)) ;
#169098 = CARTESIAN_POINT('Ctrl Pts',(-23.1238085198587,-12.7171117080057,
113.275136470339)) ;
#169099 = CARTESIAN_POINT('Ctrl Pts',(-23.1427829186928,-12.7625129426041,
113.33292942976)) ;
#169100 = CARTESIAN_POINT('Ctrl Pts',(-23.2173049964885,-12.5553594059935,
113.524403018202)) ;
#169101 = CARTESIAN_POINT('Ctrl Pts',(-23.231839369238,-12.6152904005215,
113.568672374581)) ;
#169102 = CARTESIAN_POINT('Ctrl Pts',(-23.3056432394893,-12.6152903344179,
113.54444141462)) ;
#169103 = CARTESIAN_POINT('Ctrl Pts',(-23.3794471097407,-12.6152902683143,
113.520210454658)) ;
#169104 = CARTESIAN_POINT('Ctrl Pts',(-23.3649127369912,-12.5553592737864,
113.475941098278)) ;
#169105 = CARTESIAN_POINT('Ctrl Pts',(-23.3503783642417,-12.4954282792585,
113.431671741899)) ;
#169106 = CARTESIAN_POINT('Ctrl Pts',(-23.2765744939903,-12.4954283453621,
113.45590270186)) ;
#169107 = CARTESIAN_POINT('Ctrl Pts',(-23.202770623739,-12.4954284114656,
113.480133661822)) ;
#169108 = CARTESIAN_POINT('Ctrl Pts',(-23.2173049964885,-12.5553594059935,
113.524403018202)) ;
#169109 = CARTESIAN_POINT('Ctrl Pts',(-23.3068806905073,-12.4101759250027,
113.761668971239)) ;
#169110 = CARTESIAN_POINT('Ctrl Pts',(-23.3159187908398,-12.4803322250042,
113.789197568645)) ;
#169111 = CARTESIAN_POINT('Ctrl Pts',(-23.3897226654383,-12.4803321844946,
113.764966621924)) ;
#169112 = CARTESIAN_POINT('Ctrl Pts',(-23.4635265400367,-12.4803321439849,
113.740735675203)) ;
#169113 = CARTESIAN_POINT('Ctrl Pts',(-23.4544884397042,-12.4101758439834,
113.713207077797)) ;
#169114 = CARTESIAN_POINT('Ctrl Pts',(-23.4454503393718,-12.3400195439819,
113.685678480392)) ;
#169115 = CARTESIAN_POINT('Ctrl Pts',(-23.3716464647733,-12.3400195844916,
113.709909427113)) ;
#169116 = CARTESIAN_POINT('Ctrl Pts',(-23.2978425901748,-12.3400196250012,
113.734140373834)) ;
#169117 = CARTESIAN_POINT('Ctrl Pts',(-23.3068806905073,-12.4101759250027,
113.761668971239)) ;
#169118 = CARTESIAN_POINT('Ctrl Pts',(-23.405005780283,-12.3376963152453,
114.025199960178)) ;
#169119 = CARTESIAN_POINT('Ctrl Pts',(-23.4079377709915,-12.4130169374688,
114.034130332859)) ;
#169120 = CARTESIAN_POINT('Ctrl Pts',(-23.4817416473952,-12.4130169250925,
114.009899391637)) ;
#169121 = CARTESIAN_POINT('Ctrl Pts',(-23.5555455237989,-12.4130169127163,
113.985668450414)) ;
#169122 = CARTESIAN_POINT('Ctrl Pts',(-23.5526135330904,-12.3376962904928,
113.976738077733)) ;
#169123 = CARTESIAN_POINT('Ctrl Pts',(-23.5496815423819,-12.2623756682694,
113.967807705051)) ;
#169124 = CARTESIAN_POINT('Ctrl Pts',(-23.4758776659782,-12.2623756806456,
113.992038646274)) ;
#169125 = CARTESIAN_POINT('Ctrl Pts',(-23.4020737895745,-12.2623756930219,
114.016269587496)) ;
#169126 = CARTESIAN_POINT('Ctrl Pts',(-23.405005780283,-12.3376963152453,
114.025199960178)) ;
#169127 = CARTESIAN_POINT('Ctrl Pts',(-23.5066801809222,-12.3422639933637,
114.299298215706)) ;
#169128 = CARTESIAN_POINT('Ctrl Pts',(-23.5032543515753,-12.4173784848516,
114.28886369427)) ;
#169129 = CARTESIAN_POINT('Ctrl Pts',(-23.577058226874,-12.4173785007626,
114.264632749682)) ;
#169130 = CARTESIAN_POINT('Ctrl Pts',(-23.6508621021727,-12.4173785166736,
114.240401805094)) ;
#169131 = CARTESIAN_POINT('Ctrl Pts',(-23.6542879315196,-12.3422640251856,
114.25083632653)) ;
#169132 = CARTESIAN_POINT('Ctrl Pts',(-23.6577137608664,-12.2671495336977,
114.261270847965)) ;
#169133 = CARTESIAN_POINT('Ctrl Pts',(-23.5839098855678,-12.2671495177867,
114.285501792553)) ;
#169134 = CARTESIAN_POINT('Ctrl Pts',(-23.5101060102691,-12.2671495018757,
114.309732737142)) ;
#169135 = CARTESIAN_POINT('Ctrl Pts',(-23.5066801809222,-12.3422639933637,
114.299298215706)) ;
#169136 = CARTESIAN_POINT('Ctrl Pts',(-23.6043850261139,-12.4243537888734,
114.561410934724)) ;
#169137 = CARTESIAN_POINT('Ctrl Pts',(-23.5948667124673,-12.4938495197523,
114.532419689052)) ;
#169138 = CARTESIAN_POINT('Ctrl Pts',(-23.6686705841451,-12.4938495605533,
114.508188733435)) ;
#169139 = CARTESIAN_POINT('Ctrl Pts',(-23.7424744558228,-12.4938496013543,
114.483957777818)) ;
#169140 = CARTESIAN_POINT('Ctrl Pts',(-23.7519927694694,-12.4243538704754,
114.51294902349)) ;
#169141 = CARTESIAN_POINT('Ctrl Pts',(-23.761511083116,-12.3548581395965,
114.541940269163)) ;
#169142 = CARTESIAN_POINT('Ctrl Pts',(-23.6877072114382,-12.3548580987955,
114.56617122478)) ;
#169143 = CARTESIAN_POINT('Ctrl Pts',(-23.6139033397605,-12.3548580579945,
114.590402180397)) ;
#169144 = CARTESIAN_POINT('Ctrl Pts',(-23.6043850261139,-12.4243537888734,
114.561410934724)) ;
#169145 = CARTESIAN_POINT('Ctrl Pts',(-23.6917800294508,-12.5764990896273,
114.7923054574)) ;
#169146 = CARTESIAN_POINT('Ctrl Pts',(-23.6768761024066,-12.6354761389067,
114.746910502209)) ;
#169147 = CARTESIAN_POINT('Ctrl Pts',(-23.7506799687729,-12.6354761997948,
114.722679530414)) ;
#169148 = CARTESIAN_POINT('Ctrl Pts',(-23.8244838351391,-12.6354762606829,
114.698448558619)) ;
#169149 = CARTESIAN_POINT('Ctrl Pts',(-23.8393877621834,-12.5764992114035,
114.74384351381)) ;
#169150 = CARTESIAN_POINT('Ctrl Pts',(-23.8542916892276,-12.5175221621241,
114.789238469001)) ;
#169151 = CARTESIAN_POINT('Ctrl Pts',(-23.7804878228613,-12.517522101236,
114.813469440796)) ;
#169152 = CARTESIAN_POINT('Ctrl Pts',(-23.7066839564951,-12.5175220403479,
114.837700412591)) ;
#169153 = CARTESIAN_POINT('Ctrl Pts',(-23.6917800294508,-12.5764990896273,
114.7923054574)) ;
#169154 = CARTESIAN_POINT('Ctrl Pts',(-23.7643708740628,-12.7898749801387,
114.977872887432)) ;
#169155 = CARTESIAN_POINT('Ctrl Pts',(-23.7451115981193,-12.8340435200322,
114.91921224211)) ;
#169156 = CARTESIAN_POINT('Ctrl Pts',(-23.8189154574709,-12.834043593478,
114.894981248949)) ;
#169157 = CARTESIAN_POINT('Ctrl Pts',(-23.8927193168225,-12.8340436669238,
114.870750255788)) ;
#169158 = CARTESIAN_POINT('Ctrl Pts',(-23.9119785927659,-12.7898751270303,
114.92941090111)) ;
#169159 = CARTESIAN_POINT('Ctrl Pts',(-23.9312378687094,-12.7457065871368,
114.988071546433)) ;
#169160 = CARTESIAN_POINT('Ctrl Pts',(-23.8574340093578,-12.745706513691,
115.012302539593)) ;
#169161 = CARTESIAN_POINT('Ctrl Pts',(-23.7836301500062,-12.7457064402452,
115.036533532754)) ;
#169162 = CARTESIAN_POINT('Ctrl Pts',(-23.7643708740628,-12.7898749801387,
114.977872887432)) ;
#169163 = CARTESIAN_POINT('Ctrl Pts',(-23.8170503352041,-13.0489854290901,
115.102740722146)) ;
#169164 = CARTESIAN_POINT('Ctrl Pts',(-23.7948202389745,-13.0751301371368,
115.035031437426)) ;
#169165 = CARTESIAN_POINT('Ctrl Pts',(-23.8686240908392,-13.0751302144171,
115.010800421462)) ;
#169166 = CARTESIAN_POINT('Ctrl Pts',(-23.942427942704,-13.0751302916973,
114.986569405497)) ;
#169167 = CARTESIAN_POINT('Ctrl Pts',(-23.9646580389336,-13.0489855836505,
115.054278690217)) ;
#169168 = CARTESIAN_POINT('Ctrl Pts',(-23.9868881351632,-13.0228408756037,
115.121987974937)) ;
#169169 = CARTESIAN_POINT('Ctrl Pts',(-23.9130842832985,-13.0228407983235,
115.146218990902)) ;
#169170 = CARTESIAN_POINT('Ctrl Pts',(-23.8392804314337,-13.0228407210433,
115.170450006866)) ;
#169171 = CARTESIAN_POINT('Ctrl Pts',(-23.8170503352041,-13.0489854290901,
115.102740722146)) ;
#169172 = CARTESIAN_POINT('Ctrl Pts',(-23.8466050136932,-13.3335116646803,
115.157315047406)) ;
#169173 = CARTESIAN_POINT('Ctrl Pts',(-23.8230112672121,-13.3398303944034,
115.085452303904)) ;
#169174 = CARTESIAN_POINT('Ctrl Pts',(-23.8968151122376,-13.3398304688619,
115.061221267108)) ;
#169175 = CARTESIAN_POINT('Ctrl Pts',(-23.970618957263,-13.3398305433204,
115.036990230313)) ;
#169176 = CARTESIAN_POINT('Ctrl Pts',(-23.994212703744,-13.3335118135973,
115.108852973814)) ;
#169177 = CARTESIAN_POINT('Ctrl Pts',(-24.0178064502251,-13.3271930838743,
115.180715717316)) ;
#169178 = CARTESIAN_POINT('Ctrl Pts',(-23.9440026051996,-13.3271930094158,
115.204946754112)) ;
#169179 = CARTESIAN_POINT('Ctrl Pts',(-23.8701987601742,-13.3271929349573,
115.229177790907)) ;
#169180 = CARTESIAN_POINT('Ctrl Pts',(-23.8466050136932,-13.3335116646803,
115.157315047406)) ;
#169181 = CARTESIAN_POINT('Ctrl Pts',(-23.8520217309769,-13.6230727255243,
115.138490203622)) ;
#169182 = CARTESIAN_POINT('Ctrl Pts',(-23.8287451419027,-13.6091838535946,
115.06759347028)) ;
#169183 = CARTESIAN_POINT('Ctrl Pts',(-23.9025489811084,-13.6091839202508,
115.043362415759)) ;
#169184 = CARTESIAN_POINT('Ctrl Pts',(-23.9763528203141,-13.6091839869071,
115.019131361237)) ;
#169185 = CARTESIAN_POINT('Ctrl Pts',(-23.9996294093884,-13.6230728588367,
115.090028094579)) ;
#169186 = CARTESIAN_POINT('Ctrl Pts',(-24.0229059984626,-13.6369617307664,
115.160924827921)) ;
#169187 = CARTESIAN_POINT('Ctrl Pts',(-23.9491021592569,-13.6369616641102,
115.185155882443)) ;
#169188 = CARTESIAN_POINT('Ctrl Pts',(-23.8752983200512,-13.6369615974539,
115.209386936964)) ;
#169189 = CARTESIAN_POINT('Ctrl Pts',(-23.8520217309769,-13.6230727255243,
115.138490203622)) ;
#169190 = CARTESIAN_POINT('Ctrl Pts',(-23.8336611247372,-13.8991091738745,
115.047105108385)) ;
#169191 = CARTESIAN_POINT('Ctrl Pts',(-23.8123650030025,-13.8659263158171,
114.982240558852)) ;
#169192 = CARTESIAN_POINT('Ctrl Pts',(-23.8861688379437,-13.8659263690519,
114.958009491342)) ;
#169193 = CARTESIAN_POINT('Ctrl Pts',(-23.959972672885,-13.8659264222868,
114.933778423831)) ;
#169194 = CARTESIAN_POINT('Ctrl Pts',(-23.9812687946197,-13.8991092803442,
114.998642973364)) ;
#169195 = CARTESIAN_POINT('Ctrl Pts',(-24.0025649163544,-13.9322921384017,
115.063507522897)) ;
#169196 = CARTESIAN_POINT('Ctrl Pts',(-23.9287610814131,-13.9322920851668,
115.087738590407)) ;
#169197 = CARTESIAN_POINT('Ctrl Pts',(-23.8549572464718,-13.9322920319319,
115.111969657918)) ;
#169198 = CARTESIAN_POINT('Ctrl Pts',(-23.8336611247372,-13.8991091738745,
115.047105108385)) ;
#169199 = CARTESIAN_POINT('Ctrl Pts',(-23.7933725279164,-14.1412745978093,
114.888849693188)) ;
#169200 = CARTESIAN_POINT('Ctrl Pts',(-23.7755925026804,-14.0911330408888,
114.834694606088)) ;
#169201 = CARTESIAN_POINT('Ctrl Pts',(-23.8493963354353,-14.0911330778526,
114.810463531918)) ;
#169202 = CARTESIAN_POINT('Ctrl Pts',(-23.9232001681903,-14.0911331148164,
114.786232457749)) ;
#169203 = CARTESIAN_POINT('Ctrl Pts',(-23.9409801934264,-14.141274671737,
114.840387544848)) ;
#169204 = CARTESIAN_POINT('Ctrl Pts',(-23.9587602186625,-14.1914162286575,
114.894542631948)) ;
#169205 = CARTESIAN_POINT('Ctrl Pts',(-23.8849563859075,-14.1914161916937,
114.918773706118)) ;
#169206 = CARTESIAN_POINT('Ctrl Pts',(-23.8111525531525,-14.1914161547299,
114.943004780288)) ;
#169207 = CARTESIAN_POINT('Ctrl Pts',(-23.7933725279164,-14.1412745978093,
114.888849693188)) ;
#169208 = CARTESIAN_POINT('Ctrl Pts',(-23.7346974692278,-14.3313662237517,
114.67454342391)) ;
#169209 = CARTESIAN_POINT('Ctrl Pts',(-23.7217237245287,-14.2678756388728,
114.635027491642)) ;
#169210 = CARTESIAN_POINT('Ctrl Pts',(-23.7955275572489,-14.2678756602265,
114.610796417367)) ;
#169211 = CARTESIAN_POINT('Ctrl Pts',(-23.8693313899692,-14.2678756815801,
114.586565343091)) ;
#169212 = CARTESIAN_POINT('Ctrl Pts',(-23.8823051346683,-14.331366266459,
114.626081275358)) ;
#169213 = CARTESIAN_POINT('Ctrl Pts',(-23.8952788793673,-14.3948568513378,
114.665597207626)) ;
#169214 = CARTESIAN_POINT('Ctrl Pts',(-23.8214750466471,-14.3948568299842,
114.689828281901)) ;
#169215 = CARTESIAN_POINT('Ctrl Pts',(-23.7476712139269,-14.3948568086305,
114.714059356177)) ;
#169216 = CARTESIAN_POINT('Ctrl Pts',(-23.7346974692278,-14.3313662237517,
114.67454342391)) ;
#169217 = CARTESIAN_POINT('Ctrl Pts',(-23.6635924763443,-14.4547660222928,
114.422764378375)) ;
#169218 = CARTESIAN_POINT('Ctrl Pts',(-23.6562923933097,-14.3825637894308,
114.400529503979)) ;
#169219 = CARTESIAN_POINT('Ctrl Pts',(-23.7300962264647,-14.3825637991791,
114.376298431027)) ;
#169220 = CARTESIAN_POINT('Ctrl Pts',(-23.8039000596197,-14.3825638089273,
114.352067358076)) ;
#169221 = CARTESIAN_POINT('Ctrl Pts',(-23.8112001426543,-14.4547660417892,
114.374302232472)) ;
#169222 = CARTESIAN_POINT('Ctrl Pts',(-23.8185002256888,-14.5269682746512,
114.396537106869)) ;
#169223 = CARTESIAN_POINT('Ctrl Pts',(-23.7446963925338,-14.526968264903,
114.42076817982)) ;
#169224 = CARTESIAN_POINT('Ctrl Pts',(-23.6708925593788,-14.5269682551548,
114.444999252771)) ;
#169225 = CARTESIAN_POINT('Ctrl Pts',(-23.6635924763443,-14.4547660222928,
114.422764378375)) ;
#169226 = CARTESIAN_POINT('Ctrl Pts',(-23.5843592342863,-14.5053328691454,
114.145839565311)) ;
#169227 = CARTESIAN_POINT('Ctrl Pts',(-23.5833169453667,-14.4294900381805,
114.142664921913)) ;
#169228 = CARTESIAN_POINT('Ctrl Pts',(-23.6571207810576,-14.4294900382422,
114.118433856685)) ;
#169229 = CARTESIAN_POINT('Ctrl Pts',(-23.7309246167484,-14.4294900383039,
114.094202791458)) ;
#169230 = CARTESIAN_POINT('Ctrl Pts',(-23.731966905668,-14.5053328692688,
114.097377434856)) ;
#169231 = CARTESIAN_POINT('Ctrl Pts',(-23.7330091945875,-14.5811757002337,
114.100552078255)) ;
#169232 = CARTESIAN_POINT('Ctrl Pts',(-23.6592053588967,-14.581175700172,
114.124783143482)) ;
#169233 = CARTESIAN_POINT('Ctrl Pts',(-23.5854015232058,-14.5811757001103,
114.14901420871)) ;
#169234 = CARTESIAN_POINT('Ctrl Pts',(-23.5843592342863,-14.5053328691454,
114.145839565311)) ;
#169235 = CARTESIAN_POINT('Ctrl Pts',(-23.5043319156258,-14.4771328889757,
113.866567081809)) ;
#169236 = CARTESIAN_POINT('Ctrl Pts',(-23.5096110710499,-14.4031442032382,
113.882646537764)) ;
#169237 = CARTESIAN_POINT('Ctrl Pts',(-23.5834149094567,-14.4031441988983,
113.858415480808)) ;
#169238 = CARTESIAN_POINT('Ctrl Pts',(-23.6572187478634,-14.4031441945584,
113.834184423853)) ;
#169239 = CARTESIAN_POINT('Ctrl Pts',(-23.6519395924393,-14.4771328802959,
113.818104967899)) ;
#169240 = CARTESIAN_POINT('Ctrl Pts',(-23.6466604370152,-14.5511215660333,
113.802025511944)) ;
#169241 = CARTESIAN_POINT('Ctrl Pts',(-23.5728565986085,-14.5511215703732,
113.8262565689)) ;
#169242 = CARTESIAN_POINT('Ctrl Pts',(-23.4990527602017,-14.5511215747131,
113.850487625855)) ;
#169243 = CARTESIAN_POINT('Ctrl Pts',(-23.5043319156258,-14.4771328889757,
113.866567081809)) ;
#169244 = CARTESIAN_POINT('Ctrl Pts',(-23.4303264176823,-14.3740575561619,
113.605870865708)) ;
#169245 = CARTESIAN_POINT('Ctrl Pts',(-23.4415111093854,-14.3071548458452,
113.639937632206)) ;
#169246 = CARTESIAN_POINT('Ctrl Pts',(-23.5153149498543,-14.307154840074,
113.615706581531)) ;
#169247 = CARTESIAN_POINT('Ctrl Pts',(-23.5891187903231,-14.3071548343027,
113.591475530857)) ;
#169248 = CARTESIAN_POINT('Ctrl Pts',(-23.5779340986201,-14.3740575446194,
113.557408764359)) ;
#169249 = CARTESIAN_POINT('Ctrl Pts',(-23.5667494069171,-14.4409602549361,
113.523341997861)) ;
#169250 = CARTESIAN_POINT('Ctrl Pts',(-23.4929455664482,-14.4409602607073,
113.547573048536)) ;
#169251 = CARTESIAN_POINT('Ctrl Pts',(-23.4191417259793,-14.4409602664786,
113.57180409921)) ;
#169252 = CARTESIAN_POINT('Ctrl Pts',(-23.4303264176823,-14.3740575561619,
113.605870865708)) ;
#169253 = CARTESIAN_POINT('Ctrl Pts',(-23.367255733875,-14.2012582823737,
113.378139757424)) ;
#169254 = CARTESIAN_POINT('Ctrl Pts',(-23.3835987072137,-14.1463204404916,
113.427917817362)) ;
#169255 = CARTESIAN_POINT('Ctrl Pts',(-23.4574025498353,-14.1463204373001,
113.403686773245)) ;
#169256 = CARTESIAN_POINT('Ctrl Pts',(-23.531206392457,-14.1463204341086,
113.379455729128)) ;
#169257 = CARTESIAN_POINT('Ctrl Pts',(-23.5148634191183,-14.2012582759907,
113.329677669189)) ;
#169258 = CARTESIAN_POINT('Ctrl Pts',(-23.4985204457796,-14.2561961178728,
113.27989960925)) ;
#169259 = CARTESIAN_POINT('Ctrl Pts',(-23.4247166031579,-14.2561961210643,
113.304130653368)) ;
#169260 = CARTESIAN_POINT('Ctrl Pts',(-23.3509127605363,-14.2561961242558,
113.328361697485)) ;
#169261 = CARTESIAN_POINT('Ctrl Pts',(-23.367255733875,-14.2012582823737,
113.378139757424)) ;
#169262 = CARTESIAN_POINT('Ctrl Pts',(-23.3214527143622,-13.9726608385018,
113.203153689332)) ;
#169263 = CARTESIAN_POINT('Ctrl Pts',(-23.341752719975,-13.9336031304971,
113.264984231032)) ;
#169264 = CARTESIAN_POINT('Ctrl Pts',(-23.4155565634811,-13.9336031304968,
113.240753189609)) ;
#169265 = CARTESIAN_POINT('Ctrl Pts',(-23.4893604069873,-13.9336031304964,
113.216522148185)) ;
#169266 = CARTESIAN_POINT('Ctrl Pts',(-23.4690604013745,-13.9726608385011,
113.154691606486)) ;
#169267 = CARTESIAN_POINT('Ctrl Pts',(-23.4487603957618,-14.0117185465058,
113.092861064786)) ;
#169268 = CARTESIAN_POINT('Ctrl Pts',(-23.3749565522556,-14.0117185465062,
113.117092106209)) ;
#169269 = CARTESIAN_POINT('Ctrl Pts',(-23.3011527087495,-14.0117185465065,
113.141323147633)) ;
#169270 = CARTESIAN_POINT('Ctrl Pts',(-23.3214527143622,-13.9726608385018,
113.203153689332)) ;
#169271 = CARTESIAN_POINT('Ctrl Pts',(-23.2965488105759,-13.7058102020006,
113.091988324737)) ;
#169272 = CARTESIAN_POINT('Ctrl Pts',(-23.3193487242451,-13.6853276622156,
113.161433182971)) ;
#169273 = CARTESIAN_POINT('Ctrl Pts',(-23.3931525679122,-13.685327664635,
113.137202142038)) ;
#169274 = CARTESIAN_POINT('Ctrl Pts',(-23.4669564115793,-13.6853276670543,
113.112971101105)) ;
#169275 = CARTESIAN_POINT('Ctrl Pts',(-23.4441564979102,-13.7058102068394,
113.04352624287)) ;
#169276 = CARTESIAN_POINT('Ctrl Pts',(-23.421356584241,-13.7262927466244,
112.974081384636)) ;
#169277 = CARTESIAN_POINT('Ctrl Pts',(-23.3475527405739,-13.726292744205,
112.998312425569)) ;
#169278 = CARTESIAN_POINT('Ctrl Pts',(-23.2737488969068,-13.7262927417856,
113.022543466502)) ;
#169279 = CARTESIAN_POINT('Ctrl Pts',(-23.2965488105759,-13.7058102020006,
113.091988324737)) ;
#169280 = CARTESIAN_POINT('Ctrl Pts',(-23.2950095776943,-13.4160016672544,
113.051687295608)) ;
#169281 = CARTESIAN_POINT('Ctrl Pts',(-23.318688002029,-13.4157263085417,
113.123807955567)) ;
#169282 = CARTESIAN_POINT('Ctrl Pts',(-23.3924918454245,-13.4157263119192,
113.099576913806)) ;
#169283 = CARTESIAN_POINT('Ctrl Pts',(-23.4662956888199,-13.4157263152968,
113.075345872045)) ;
#169284 = CARTESIAN_POINT('Ctrl Pts',(-23.4426172644851,-13.4160016740095,
113.003225212087)) ;
#169285 = CARTESIAN_POINT('Ctrl Pts',(-23.4189388401504,-13.4162770327222,
112.931104552128)) ;
#169286 = CARTESIAN_POINT('Ctrl Pts',(-23.345134996755,-13.4162770293446,
112.955335593889)) ;
#169287 = CARTESIAN_POINT('Ctrl Pts',(-23.2713311533596,-13.4162770259671,
112.979566635649)) ;
#169288 = CARTESIAN_POINT('Ctrl Pts',(-23.2950095776943,-13.4160016672544,
113.051687295608)) ;
#169289 = CARTESIAN_POINT('Ctrl Pts',(-23.3177569881887,-13.1285751860039,
113.085639842079)) ;
#169290 = CARTESIAN_POINT('Ctrl Pts',(-23.3406129860406,-13.1483696405658,
113.155255523698)) ;
#169291 = CARTESIAN_POINT('Ctrl Pts',(-23.4144168292376,-13.1483696423267,
113.131024481333)) ;
#169292 = CARTESIAN_POINT('Ctrl Pts',(-23.4882206724346,-13.1483696440876,
113.106793438967)) ;
#169293 = CARTESIAN_POINT('Ctrl Pts',(-23.4653646745826,-13.1285751895257,
113.037177757348)) ;
#169294 = CARTESIAN_POINT('Ctrl Pts',(-23.4425086767307,-13.1087807349637,
112.967562075729)) ;
#169295 = CARTESIAN_POINT('Ctrl Pts',(-23.3687048335338,-13.1087807332029,
112.991793118094)) ;
#169296 = CARTESIAN_POINT('Ctrl Pts',(-23.2949009903368,-13.108780731442,
113.016024160459)) ;
#169297 = CARTESIAN_POINT('Ctrl Pts',(-23.3177569881887,-13.1285751860039,
113.085639842079)) ;
#169298 = CARTESIAN_POINT('Ctrl Pts',(-23.3638473343004,-12.8607655160009,
113.19057058285)) ;
#169299 = CARTESIAN_POINT('Ctrl Pts',(-23.3842522246996,-12.8992892822013,
113.252720586712)) ;
#169300 = CARTESIAN_POINT('Ctrl Pts',(-23.4580560681807,-12.8992892809573,
113.228489545212)) ;
#169301 = CARTESIAN_POINT('Ctrl Pts',(-23.5318599116619,-12.8992892797133,
113.204258503713)) ;
#169302 = CARTESIAN_POINT('Ctrl Pts',(-23.5114550212627,-12.8607655135129,
113.14210849985)) ;
#169303 = CARTESIAN_POINT('Ctrl Pts',(-23.4910501308634,-12.8222417473126,
113.079958495988)) ;
#169304 = CARTESIAN_POINT('Ctrl Pts',(-23.4172462873823,-12.8222417485565,
113.104189537488)) ;
#169305 = CARTESIAN_POINT('Ctrl Pts',(-23.3434424439011,-12.8222417498005,
113.128420578987)) ;
#169306 = CARTESIAN_POINT('Ctrl Pts',(-23.3638473343004,-12.8607655160009,
113.19057058285)) ;
#169307 = CARTESIAN_POINT('Ctrl Pts',(-23.4313745687069,-12.6316532711116,
113.360568411281)) ;
#169308 = CARTESIAN_POINT('Ctrl Pts',(-23.4478325750678,-12.686231857174,
113.410696843313)) ;
#169309 = CARTESIAN_POINT('Ctrl Pts',(-23.5216364200498,-12.6862318515475,
113.386465806385)) ;
#169310 = CARTESIAN_POINT('Ctrl Pts',(-23.5954402650319,-12.6862318459211,
113.362234769457)) ;
#169311 = CARTESIAN_POINT('Ctrl Pts',(-23.5789822586709,-12.6316532598588,
113.312106337425)) ;
#169312 = CARTESIAN_POINT('Ctrl Pts',(-23.56252425231,-12.5770746737964,113.261977905393)) ;
#169313 = CARTESIAN_POINT('Ctrl Pts',(-23.488720407328,-12.5770746794228,
113.286208942321)) ;
#169314 = CARTESIAN_POINT('Ctrl Pts',(-23.4149165623459,-12.5770746850493,
113.310439979249)) ;
#169315 = CARTESIAN_POINT('Ctrl Pts',(-23.4313745687069,-12.6316532711116,
113.360568411281)) ;
#169316 = CARTESIAN_POINT('Ctrl Pts',(-23.5152154328115,-12.460718041819,
113.580530422711)) ;
#169317 = CARTESIAN_POINT('Ctrl Pts',(-23.5265758928896,-12.5273111609863,
113.615132551369)) ;
#169318 = CARTESIAN_POINT('Ctrl Pts',(-23.6003797399565,-12.5273111540266,
113.590901520791)) ;
#169319 = CARTESIAN_POINT('Ctrl Pts',(-23.6741835870235,-12.5273111470668,
113.566670490213)) ;
#169320 = CARTESIAN_POINT('Ctrl Pts',(-23.6628231269454,-12.4607180278995,
113.532068361556)) ;
#169321 = CARTESIAN_POINT('Ctrl Pts',(-23.6514626668674,-12.3941249087322,
113.497466232898)) ;
#169322 = CARTESIAN_POINT('Ctrl Pts',(-23.5776588198004,-12.394124915692,
113.521697263476)) ;
#169323 = CARTESIAN_POINT('Ctrl Pts',(-23.5038549727334,-12.3941249226517,
113.545928294054)) ;
#169324 = CARTESIAN_POINT('Ctrl Pts',(-23.5152154328115,-12.460718041819,
113.580530422711)) ;
#169325 = CARTESIAN_POINT('Ctrl Pts',(-23.6105283082249,-12.3580087732105,
113.83543283703)) ;
#169326 = CARTESIAN_POINT('Ctrl Pts',(-23.6159828998831,-12.4318697519678,
113.85204664352)) ;
#169327 = CARTESIAN_POINT('Ctrl Pts',(-23.6897867494488,-12.4318697467782,
113.827815620553)) ;
#169328 = CARTESIAN_POINT('Ctrl Pts',(-23.7635905990146,-12.4318697415885,
113.803584597586)) ;
#169329 = CARTESIAN_POINT('Ctrl Pts',(-23.7581360073565,-12.3580087628311,
113.786970791096)) ;
#169330 = CARTESIAN_POINT('Ctrl Pts',(-23.7526814156984,-12.2841477840738,
113.770356984606)) ;
#169331 = CARTESIAN_POINT('Ctrl Pts',(-23.6788775661326,-12.2841477892635,
113.794588007573)) ;
#169332 = CARTESIAN_POINT('Ctrl Pts',(-23.6050737165668,-12.2841477944531,
113.81881903054)) ;
#169333 = CARTESIAN_POINT('Ctrl Pts',(-23.6105283082249,-12.3580087732105,
113.83543283703)) ;
#169334 = CARTESIAN_POINT('Ctrl Pts',(-23.711289186048,-12.3309308762199,
114.106935761208)) ;
#169335 = CARTESIAN_POINT('Ctrl Pts',(-23.7104488970533,-12.4067892276866,
114.104376377047)) ;
#169336 = CARTESIAN_POINT('Ctrl Pts',(-23.7842527491276,-12.4067892280987,
114.08014536172)) ;
#169337 = CARTESIAN_POINT('Ctrl Pts',(-23.8580566012019,-12.4067892285108,
114.055914346394)) ;
#169338 = CARTESIAN_POINT('Ctrl Pts',(-23.8588968901966,-12.330930877044,
114.058473730555)) ;
#169339 = CARTESIAN_POINT('Ctrl Pts',(-23.8597371791913,-12.2550725255773,
114.061033114716)) ;
#169340 = CARTESIAN_POINT('Ctrl Pts',(-23.7859333271171,-12.2550725251652,
114.085264130043)) ;
#169341 = CARTESIAN_POINT('Ctrl Pts',(-23.7121294750428,-12.2550725247531,
114.109495145369)) ;
#169342 = CARTESIAN_POINT('Ctrl Pts',(-23.711289186048,-12.3309308762199,
114.106935761208)) ;
#169343 = CARTESIAN_POINT('Ctrl Pts',(-23.811392388045,-12.3817530522947,
114.376315180334)) ;
#169344 = CARTESIAN_POINT('Ctrl Pts',(-23.8042965762851,-12.4541728296822,
114.354702483328)) ;
#169345 = CARTESIAN_POINT('Ctrl Pts',(-23.878100430679,-12.454172840125,114.330471475067)) ;
#169346 = CARTESIAN_POINT('Ctrl Pts',(-23.9519042850728,-12.4541728505679,
114.306240466806)) ;
#169347 = CARTESIAN_POINT('Ctrl Pts',(-23.9590000968328,-12.3817530731804,
114.327853163812)) ;
#169348 = CARTESIAN_POINT('Ctrl Pts',(-23.9660959085927,-12.3093332957928,
114.349465860818)) ;
#169349 = CARTESIAN_POINT('Ctrl Pts',(-23.8922920541988,-12.30933328535,114.373696869079)) ;
#169350 = CARTESIAN_POINT('Ctrl Pts',(-23.818488199805,-12.3093332749072,
114.39792787734)) ;
#169351 = CARTESIAN_POINT('Ctrl Pts',(-23.811392388045,-12.3817530522947,
114.376315180334)) ;
#169352 = CARTESIAN_POINT('Ctrl Pts',(-23.9039028684115,-12.506826084586,
114.622631137675)) ;
#169353 = CARTESIAN_POINT('Ctrl Pts',(-23.8910714153864,-12.5706179101752,
114.583548602984)) ;
#169354 = CARTESIAN_POINT('Ctrl Pts',(-23.9648752707621,-12.5706179343356,
114.559317597713)) ;
#169355 = CARTESIAN_POINT('Ctrl Pts',(-24.0386791261378,-12.5706179584961,
114.535086592443)) ;
#169356 = CARTESIAN_POINT('Ctrl Pts',(-24.0515105791629,-12.5068261329069,
114.574169127134)) ;
#169357 = CARTESIAN_POINT('Ctrl Pts',(-24.0643420321881,-12.4430343073178,
114.613251661825)) ;
#169358 = CARTESIAN_POINT('Ctrl Pts',(-23.9905381768124,-12.4430342831573,
114.637482667096)) ;
#169359 = CARTESIAN_POINT('Ctrl Pts',(-23.9167343214367,-12.4430342589969,
114.661713672366)) ;
#169360 = CARTESIAN_POINT('Ctrl Pts',(-23.9039028684115,-12.506826084586,
114.622631137675)) ;
#169361 = CARTESIAN_POINT('Ctrl Pts',(-23.9831660419676,-12.6970626230436,
114.828592893483)) ;
#169362 = CARTESIAN_POINT('Ctrl Pts',(-23.9655157499272,-12.7476645000542,
114.774832952836)) ;
#169363 = CARTESIAN_POINT('Ctrl Pts',(-24.0393196046863,-12.7476645399719,
114.750601945687)) ;
#169364 = CARTESIAN_POINT('Ctrl Pts',(-24.1131234594454,-12.7476645798895,
114.726370938538)) ;
#169365 = CARTESIAN_POINT('Ctrl Pts',(-24.1307737514858,-12.6970627028788,
114.780130879185)) ;
#169366 = CARTESIAN_POINT('Ctrl Pts',(-24.1484240435262,-12.6464608258682,
114.833890819833)) ;
#169367 = CARTESIAN_POINT('Ctrl Pts',(-24.0746201887671,-12.6464607859506,
114.858121826981)) ;
#169368 = CARTESIAN_POINT('Ctrl Pts',(-24.000816334008,-12.646460746033,114.88235283413)) ;
#169369 = CARTESIAN_POINT('Ctrl Pts',(-23.9831660419676,-12.6970626230436,
114.828592893483)) ;
#169370 = CARTESIAN_POINT('Ctrl Pts',(-24.0443887911562,-12.9398196291384,
114.979493433224)) ;
#169371 = CARTESIAN_POINT('Ctrl Pts',(-24.0231745362282,-12.9735460220805,
114.91487823685)) ;
#169372 = CARTESIAN_POINT('Ctrl Pts',(-24.0969783885857,-12.9735460788729,
114.890647222387)) ;
#169373 = CARTESIAN_POINT('Ctrl Pts',(-24.1707822409432,-12.9735461356652,
114.866416207923)) ;
#169374 = CARTESIAN_POINT('Ctrl Pts',(-24.1919964958711,-12.9398197427232,
114.931031404297)) ;
#169375 = CARTESIAN_POINT('Ctrl Pts',(-24.2132107507992,-12.9060933497811,
114.995646600671)) ;
#169376 = CARTESIAN_POINT('Ctrl Pts',(-24.1394068984417,-12.9060932929888,
115.019877615135)) ;
#169377 = CARTESIAN_POINT('Ctrl Pts',(-24.0656030460843,-12.9060932361964,
115.044108629598)) ;
#169378 = CARTESIAN_POINT('Ctrl Pts',(-24.0443887911562,-12.9398196291384,
114.979493433224)) ;
#169379 = CARTESIAN_POINT('Ctrl Pts',(-24.0834950036509,-13.2163226304817,
115.063123342648)) ;
#169380 = CARTESIAN_POINT('Ctrl Pts',(-24.060253892529,-13.2307930159817,
114.992334669498)) ;
#169381 = CARTESIAN_POINT('Ctrl Pts',(-24.134057740261,-13.2307930864604,
114.968103640946)) ;
#169382 = CARTESIAN_POINT('Ctrl Pts',(-24.207861587993,-13.2307931569392,
114.943872612394)) ;
#169383 = CARTESIAN_POINT('Ctrl Pts',(-24.2311026991149,-13.2163227714392,
115.014661285543)) ;
#169384 = CARTESIAN_POINT('Ctrl Pts',(-24.2543438102368,-13.2018523859393,
115.085449958693)) ;
#169385 = CARTESIAN_POINT('Ctrl Pts',(-24.1805399625048,-13.2018523154605,
115.109680987245)) ;
#169386 = CARTESIAN_POINT('Ctrl Pts',(-24.1067361147728,-13.2018522449817,
115.133912015797)) ;
#169387 = CARTESIAN_POINT('Ctrl Pts',(-24.0834950036509,-13.2163226304817,
115.063123342648)) ;
#169388 = CARTESIAN_POINT('Ctrl Pts',(-24.0987740331511,-13.5056990228868,
115.074368143953)) ;
#169389 = CARTESIAN_POINT('Ctrl Pts',(-24.0751629373277,-13.4999868027269,
115.00245255722)) ;
#169390 = CARTESIAN_POINT('Ctrl Pts',(-24.1489667789724,-13.4999868805839,
114.978221510127)) ;
#169391 = CARTESIAN_POINT('Ctrl Pts',(-24.2227706206172,-13.499986958441,
114.953990463034)) ;
#169392 = CARTESIAN_POINT('Ctrl Pts',(-24.2463817164407,-13.5056991786008,
115.025906049768)) ;
#169393 = CARTESIAN_POINT('Ctrl Pts',(-24.2699928122642,-13.5114113987607,
115.097821636502)) ;
#169394 = CARTESIAN_POINT('Ctrl Pts',(-24.1961889706194,-13.5114113209037,
115.122052683594)) ;
#169395 = CARTESIAN_POINT('Ctrl Pts',(-24.1223851289746,-13.5114112430466,
115.146283730687)) ;
#169396 = CARTESIAN_POINT('Ctrl Pts',(-24.0987740331511,-13.5056990228868,
115.074368143953)) ;
#169397 = CARTESIAN_POINT('Ctrl Pts',(-24.0898176525087,-13.7916926696265,
115.011429383632)) ;
#169398 = CARTESIAN_POINT('Ctrl Pts',(-24.067535226085,-13.7660050582146,
114.943560709675)) ;
#169399 = CARTESIAN_POINT('Ctrl Pts',(-24.1413390603976,-13.7660051397553,
114.91932964025)) ;
#169400 = CARTESIAN_POINT('Ctrl Pts',(-24.2151428947103,-13.766005221296,
114.895098570825)) ;
#169401 = CARTESIAN_POINT('Ctrl Pts',(-24.2374253211339,-13.791692832708,
114.962967244781)) ;
#169402 = CARTESIAN_POINT('Ctrl Pts',(-24.2597077475576,-13.81738044412,115.030835918738)) ;
#169403 = CARTESIAN_POINT('Ctrl Pts',(-24.185903913245,-13.8173803625793,
115.055066988163)) ;
#169404 = CARTESIAN_POINT('Ctrl Pts',(-24.1121000789324,-13.8173802810385,
115.079298057588)) ;
#169405 = CARTESIAN_POINT('Ctrl Pts',(-24.0898176525087,-13.7916926696265,
115.011429383632)) ;
#169406 = CARTESIAN_POINT('Ctrl Pts',(-24.0580663785572,-14.0485418604028,
114.879359386084)) ;
#169407 = CARTESIAN_POINT('Ctrl Pts',(-24.0387000607933,-14.0048845368929,
114.820372708696)) ;
#169408 = CARTESIAN_POINT('Ctrl Pts',(-24.1125038876702,-14.0048846120398,
114.796141616622)) ;
#169409 = CARTESIAN_POINT('Ctrl Pts',(-24.1863077145469,-14.0048846871867,
114.771910524549)) ;
#169410 = CARTESIAN_POINT('Ctrl Pts',(-24.2056740323108,-14.0485420106967,
114.830897201937)) ;
#169411 = CARTESIAN_POINT('Ctrl Pts',(-24.2250403500747,-14.0921993342066,
114.889883879324)) ;
#169412 = CARTESIAN_POINT('Ctrl Pts',(-24.1512365231979,-14.0921992590597,
114.914114971398)) ;
#169413 = CARTESIAN_POINT('Ctrl Pts',(-24.0774326963211,-14.0921991839128,
114.938346063471)) ;
#169414 = CARTESIAN_POINT('Ctrl Pts',(-24.0580663785572,-14.0485418604028,
114.879359386084)) ;
#169415 = CARTESIAN_POINT('Ctrl Pts',(-24.0066666727784,-14.2607963084926,
114.687415370563)) ;
#169416 = CARTESIAN_POINT('Ctrl Pts',(-23.9915929582829,-14.2022566312554,
114.641503270218)) ;
#169417 = CARTESIAN_POINT('Ctrl Pts',(-24.0653967783519,-14.2022566928803,
114.617272157409)) ;
#169418 = CARTESIAN_POINT('Ctrl Pts',(-24.1392005984209,-14.2022567545052,
114.5930410446)) ;
#169419 = CARTESIAN_POINT('Ctrl Pts',(-24.1542743129165,-14.2607964317425,
114.638953144946)) ;
#169420 = CARTESIAN_POINT('Ctrl Pts',(-24.169348027412,-14.3193361089797,
114.684865245291)) ;
#169421 = CARTESIAN_POINT('Ctrl Pts',(-24.095544207343,-14.3193360473548,
114.7090963581)) ;
#169422 = CARTESIAN_POINT('Ctrl Pts',(-24.021740387274,-14.3193359857299,
114.733327470909)) ;
#169423 = CARTESIAN_POINT('Ctrl Pts',(-24.0066666727784,-14.2607963084926,
114.687415370563)) ;
#169424 = CARTESIAN_POINT('Ctrl Pts',(-23.9395888105032,-14.4133855037132,
114.447558126479)) ;
#169425 = CARTESIAN_POINT('Ctrl Pts',(-23.9299116484695,-14.3441068413642,
114.418083054295)) ;
#169426 = CARTESIAN_POINT('Ctrl Pts',(-24.0037154628795,-14.3441068827324,
114.39385192425)) ;
#169427 = CARTESIAN_POINT('Ctrl Pts',(-24.0775192772894,-14.3441069241007,
114.369620794205)) ;
#169428 = CARTESIAN_POINT('Ctrl Pts',(-24.0871964393232,-14.4133855864497,
114.399095866389)) ;
#169429 = CARTESIAN_POINT('Ctrl Pts',(-24.096873601357,-14.4826642487988,
114.428570938573)) ;
#169430 = CARTESIAN_POINT('Ctrl Pts',(-24.023069786947,-14.4826642074306,
114.452802068618)) ;
#169431 = CARTESIAN_POINT('Ctrl Pts',(-23.949265972537,-14.4826641660623,
114.477033198663)) ;
#169432 = CARTESIAN_POINT('Ctrl Pts',(-23.9395888105032,-14.4133855037132,
114.447558126479)) ;
#169433 = CARTESIAN_POINT('Ctrl Pts',(-23.8629281001325,-14.4941554742073,
114.178638574649)) ;
#169434 = CARTESIAN_POINT('Ctrl Pts',(-23.8593218801757,-14.4191362246067,
114.16765461255)) ;
#169435 = CARTESIAN_POINT('Ctrl Pts',(-23.9331256912243,-14.4191362402107,
114.143423472266)) ;
#169436 = CARTESIAN_POINT('Ctrl Pts',(-24.0069295022728,-14.4191362558146,
114.119192331982)) ;
#169437 = CARTESIAN_POINT('Ctrl Pts',(-24.0105357222296,-14.4941555054153,
114.130176294082)) ;
#169438 = CARTESIAN_POINT('Ctrl Pts',(-24.0141419421864,-14.5691747550159,
114.141160256181)) ;
#169439 = CARTESIAN_POINT('Ctrl Pts',(-23.9403381311378,-14.5691747394119,
114.165391396465)) ;
#169440 = CARTESIAN_POINT('Ctrl Pts',(-23.8665343200893,-14.5691747238079,
114.189622536749)) ;
#169441 = CARTESIAN_POINT('Ctrl Pts',(-23.8629281001325,-14.4941554742073,
114.178638574649)) ;
#169442 = CARTESIAN_POINT('Ctrl Pts',(-23.7825672394954,-14.4980202636657,
113.898384946366)) ;
#169443 = CARTESIAN_POINT('Ctrl Pts',(-23.7853004615776,-14.4226207212898,
113.906709901897)) ;
#169444 = CARTESIAN_POINT('Ctrl Pts',(-23.859104271779,-14.4226207084362,
113.882478759033)) ;
#169445 = CARTESIAN_POINT('Ctrl Pts',(-23.9329080819803,-14.4226206955826,
113.858247616169)) ;
#169446 = CARTESIAN_POINT('Ctrl Pts',(-23.9301748598981,-14.4980202379585,
113.849922660638)) ;
#169447 = CARTESIAN_POINT('Ctrl Pts',(-23.9274416378159,-14.5734197803344,
113.841597705107)) ;
#169448 = CARTESIAN_POINT('Ctrl Pts',(-23.8536378276146,-14.573419793188,
113.865828847971)) ;
#169449 = CARTESIAN_POINT('Ctrl Pts',(-23.7798340174132,-14.5734198060416,
113.890059990835)) ;
#169450 = CARTESIAN_POINT('Ctrl Pts',(-23.7825672394954,-14.4980202636657,
113.898384946366)) ;
#169451 = CARTESIAN_POINT('Ctrl Pts',(-23.7052727096048,-14.4245044594768,
113.627527308844)) ;
#169452 = CARTESIAN_POINT('Ctrl Pts',(-23.7141395064161,-14.3541263042152,
113.654534143371)) ;
#169453 = CARTESIAN_POINT('Ctrl Pts',(-23.7879433185797,-14.3541262631264,
113.630303006484)) ;
#169454 = CARTESIAN_POINT('Ctrl Pts',(-23.8617471307432,-14.3541262220375,
113.606071869596)) ;
#169455 = CARTESIAN_POINT('Ctrl Pts',(-23.8528803339319,-14.4245043772991,
113.579065035068)) ;
#169456 = CARTESIAN_POINT('Ctrl Pts',(-23.8440135371206,-14.4948825325607,
113.552058200541)) ;
#169457 = CARTESIAN_POINT('Ctrl Pts',(-23.770209724957,-14.4948825736496,
113.576289337429)) ;
#169458 = CARTESIAN_POINT('Ctrl Pts',(-23.6964059127935,-14.4948826147384,
113.600520474317)) ;
#169459 = CARTESIAN_POINT('Ctrl Pts',(-23.7052727096048,-14.4245044594768,
113.627527308844)) ;
#169460 = CARTESIAN_POINT('Ctrl Pts',(-23.6372016675347,-14.279297376843,
113.384786368389)) ;
#169461 = CARTESIAN_POINT('Ctrl Pts',(-23.6515666761006,-14.2189530105724,
113.428539868789)) ;
#169462 = CARTESIAN_POINT('Ctrl Pts',(-23.7253704927677,-14.2189529442762,
113.404308745619)) ;
#169463 = CARTESIAN_POINT('Ctrl Pts',(-23.7991743094348,-14.2189528779799,
113.380077622448)) ;
#169464 = CARTESIAN_POINT('Ctrl Pts',(-23.7848093008689,-14.2792972442505,
113.336324122048)) ;
#169465 = CARTESIAN_POINT('Ctrl Pts',(-23.770444292303,-14.3396416105211,
113.292570621647)) ;
#169466 = CARTESIAN_POINT('Ctrl Pts',(-23.696640475636,-14.3396416768173,
113.316801744818)) ;
#169467 = CARTESIAN_POINT('Ctrl Pts',(-23.6228366589689,-14.3396417431136,
113.341032867988)) ;
#169468 = CARTESIAN_POINT('Ctrl Pts',(-23.6372016675347,-14.279297376843,
113.384786368389)) ;
#169469 = CARTESIAN_POINT('Ctrl Pts',(-23.583741652297,-14.0713598205673,
113.186374509989)) ;
#169470 = CARTESIAN_POINT('Ctrl Pts',(-23.6025966694698,-14.0254428843111,
113.24380385212)) ;
#169471 = CARTESIAN_POINT('Ctrl Pts',(-23.6764004928724,-14.0254427985769,
113.219572749465)) ;
#169472 = CARTESIAN_POINT('Ctrl Pts',(-23.750204316275,-14.0254427128428,
113.19534164681)) ;
#169473 = CARTESIAN_POINT('Ctrl Pts',(-23.7313492991022,-14.0713596490991,
113.137912304678)) ;
#169474 = CARTESIAN_POINT('Ctrl Pts',(-23.7124942819294,-14.1172765853553,
113.080482962546)) ;
#169475 = CARTESIAN_POINT('Ctrl Pts',(-23.6386904585268,-14.1172766710895,
113.104714065202)) ;
#169476 = CARTESIAN_POINT('Ctrl Pts',(-23.5648866351242,-14.1172767568236,
113.128945167857)) ;
#169477 = CARTESIAN_POINT('Ctrl Pts',(-23.583741652297,-14.0713598205673,
113.186374509989)) ;
#169478 = CARTESIAN_POINT('Ctrl Pts',(-23.5499741300626,-13.8176789860274,
113.048124711497)) ;
#169479 = CARTESIAN_POINT('Ctrl Pts',(-23.5719472275288,-13.7894049725344,
113.115051223061)) ;
#169480 = CARTESIAN_POINT('Ctrl Pts',(-23.6457510590017,-13.7894048748747,
113.090820144986)) ;
#169481 = CARTESIAN_POINT('Ctrl Pts',(-23.7195548904747,-13.789404777215,
113.066589066912)) ;
#169482 = CARTESIAN_POINT('Ctrl Pts',(-23.6975817930084,-13.8176787907079,
112.999662555348)) ;
#169483 = CARTESIAN_POINT('Ctrl Pts',(-23.6756086955422,-13.8459528042009,
112.932736043785)) ;
#169484 = CARTESIAN_POINT('Ctrl Pts',(-23.6018048640693,-13.8459529018606,
112.95696712186)) ;
#169485 = CARTESIAN_POINT('Ctrl Pts',(-23.5280010325963,-13.8459529995203,
112.981198199934)) ;
#169486 = CARTESIAN_POINT('Ctrl Pts',(-23.5499741300626,-13.8176789860274,
113.048124711497)) ;
#169487 = CARTESIAN_POINT('Ctrl Pts',(-23.5387047936549,-13.5347545509982,
112.97830483339)) ;
#169488 = CARTESIAN_POINT('Ctrl Pts',(-23.5622320126425,-13.526191139526,
113.049964948284)) ;
#169489 = CARTESIAN_POINT('Ctrl Pts',(-23.6360358527796,-13.5261910386332,
113.0257338966)) ;
#169490 = CARTESIAN_POINT('Ctrl Pts',(-23.7098396929168,-13.5261909377405,
113.001502844915)) ;
#169491 = CARTESIAN_POINT('Ctrl Pts',(-23.6863124739292,-13.5347543492127,
112.929842730021)) ;
#169492 = CARTESIAN_POINT('Ctrl Pts',(-23.6627852549415,-13.5433177606849,
112.858182615127)) ;
#169493 = CARTESIAN_POINT('Ctrl Pts',(-23.5889814148044,-13.5433178615776,
112.882413666812)) ;
#169494 = CARTESIAN_POINT('Ctrl Pts',(-23.5151775746673,-13.5433179624704,
112.906644718497)) ;
#169495 = CARTESIAN_POINT('Ctrl Pts',(-23.5387047936549,-13.5347545509982,
112.97830483339)) ;
#169496 = CARTESIAN_POINT('Ctrl Pts',(-23.5516559483396,-13.2436560304018,
112.982285898806)) ;
#169497 = CARTESIAN_POINT('Ctrl Pts',(-23.575048090854,-13.2554035564965,
113.05353459247)) ;
#169498 = CARTESIAN_POINT('Ctrl Pts',(-23.6488519392539,-13.2554034608617,
113.029303565953)) ;
#169499 = CARTESIAN_POINT('Ctrl Pts',(-23.7226557876538,-13.2554033652269,
113.005072539435)) ;
#169500 = CARTESIAN_POINT('Ctrl Pts',(-23.6992636451394,-13.2436558391322,
112.93382384577)) ;
#169501 = CARTESIAN_POINT('Ctrl Pts',(-23.675871502625,-13.2319083130375,
112.862575152106)) ;
#169502 = CARTESIAN_POINT('Ctrl Pts',(-23.6020676542251,-13.2319084086723,
112.886806178624)) ;
#169503 = CARTESIAN_POINT('Ctrl Pts',(-23.5282638058252,-13.2319085043071,
112.911037205141)) ;
#169504 = CARTESIAN_POINT('Ctrl Pts',(-23.5516559483396,-13.2436560304018,
112.982285898806)) ;
#169505 = CARTESIAN_POINT('Ctrl Pts',(-23.5885583255177,-12.9652204672347,
113.059240112295)) ;
#169506 = CARTESIAN_POINT('Ctrl Pts',(-23.6101425833914,-12.9964254468849,
113.124982280943)) ;
#169507 = CARTESIAN_POINT('Ctrl Pts',(-23.6839464388598,-12.9964253637305,
113.100751275955)) ;
#169508 = CARTESIAN_POINT('Ctrl Pts',(-23.7577502943282,-12.996425280576,
113.076520270967)) ;
#169509 = CARTESIAN_POINT('Ctrl Pts',(-23.7361660364545,-12.9652203009257,
113.010778102319)) ;
#169510 = CARTESIAN_POINT('Ctrl Pts',(-23.7145817785808,-12.9340153212755,
112.94503593367)) ;
#169511 = CARTESIAN_POINT('Ctrl Pts',(-23.6407779231125,-12.93401540443,112.969266938659)) ;
#169512 = CARTESIAN_POINT('Ctrl Pts',(-23.5669740676441,-12.9340154875845,
112.993497943647)) ;
#169513 = CARTESIAN_POINT('Ctrl Pts',(-23.5885583255177,-12.9652204672347,
113.059240112295)) ;
#169514 = CARTESIAN_POINT('Ctrl Pts',(-23.6475911503442,-12.7189935301929,
113.203572736331)) ;
#169515 = CARTESIAN_POINT('Ctrl Pts',(-23.6658203545754,-12.7674367069974,
113.259095952798)) ;
#169516 = CARTESIAN_POINT('Ctrl Pts',(-23.7396242152506,-12.7674366419676,
113.234864963669)) ;
#169517 = CARTESIAN_POINT('Ctrl Pts',(-23.8134280759257,-12.7674365769377,
113.210633974539)) ;
#169518 = CARTESIAN_POINT('Ctrl Pts',(-23.7951988716945,-12.7189934001331,
113.155110758072)) ;
#169519 = CARTESIAN_POINT('Ctrl Pts',(-23.7769696674633,-12.6705502233285,
113.099587541605)) ;
#169520 = CARTESIAN_POINT('Ctrl Pts',(-23.7031658067881,-12.6705502883584,
113.123818530734)) ;
#169521 = CARTESIAN_POINT('Ctrl Pts',(-23.629361946113,-12.6705503533883,
113.148049519863)) ;
#169522 = CARTESIAN_POINT('Ctrl Pts',(-23.6475911503442,-12.7189935301929,
113.203572736331)) ;
#169523 = CARTESIAN_POINT('Ctrl Pts',(-23.7252965328095,-12.5228013953796,
113.404766433141)) ;
#169524 = CARTESIAN_POINT('Ctrl Pts',(-23.738862230298,-12.585015703863,113.446085360385)) ;
#169525 = CARTESIAN_POINT('Ctrl Pts',(-23.812666093898,-12.5850156600089,
113.421854380164)) ;
#169526 = CARTESIAN_POINT('Ctrl Pts',(-23.8864699574979,-12.5850156161548,
113.397623399943)) ;
#169527 = CARTESIAN_POINT('Ctrl Pts',(-23.8729042600094,-12.5228013076713,
113.356304472699)) ;
#169528 = CARTESIAN_POINT('Ctrl Pts',(-23.8593385625208,-12.4605869991879,
113.314985545455)) ;
#169529 = CARTESIAN_POINT('Ctrl Pts',(-23.7855346989208,-12.460587043042,
113.339216525676)) ;
#169530 = CARTESIAN_POINT('Ctrl Pts',(-23.7117308353209,-12.4605870868961,
113.363447505897)) ;
#169531 = CARTESIAN_POINT('Ctrl Pts',(-23.7252965328095,-12.5228013953796,
113.404766433141)) ;
#169532 = CARTESIAN_POINT('Ctrl Pts',(-23.8167981675552,-12.3908781186536,
113.647994834552)) ;
#169533 = CARTESIAN_POINT('Ctrl Pts',(-23.8247297631087,-12.462397411453,
113.672153196211)) ;
#169534 = CARTESIAN_POINT('Ctrl Pts',(-23.8985336273289,-12.4623973889088,
113.647922217879)) ;
#169535 = CARTESIAN_POINT('Ctrl Pts',(-23.9723374915491,-12.4623973663647,
113.623691239548)) ;
#169536 = CARTESIAN_POINT('Ctrl Pts',(-23.9644058959957,-12.3908780735653,
113.599532877889)) ;
#169537 = CARTESIAN_POINT('Ctrl Pts',(-23.9564743004422,-12.3193587807659,
113.575374516231)) ;
#169538 = CARTESIAN_POINT('Ctrl Pts',(-23.882670436222,-12.3193588033101,
113.599605494562)) ;
#169539 = CARTESIAN_POINT('Ctrl Pts',(-23.8088665720018,-12.3193588258542,
113.623836472894)) ;
#169540 = CARTESIAN_POINT('Ctrl Pts',(-23.8167981675552,-12.3908781186536,
113.647994834552)) ;
#169541 = CARTESIAN_POINT('Ctrl Pts',(-23.9162161601881,-12.3325103501403,
113.915369597383)) ;
#169542 = CARTESIAN_POINT('Ctrl Pts',(-23.9179516544004,-12.4082131688575,
113.92065563394)) ;
#169543 = CARTESIAN_POINT('Ctrl Pts',(-23.9917555172703,-12.4082131654103,
113.896424651495)) ;
#169544 = CARTESIAN_POINT('Ctrl Pts',(-24.0655593801402,-12.4082131619632,
113.872193669051)) ;
#169545 = CARTESIAN_POINT('Ctrl Pts',(-24.0638238859279,-12.332510343246,
113.866907632493)) ;
#169546 = CARTESIAN_POINT('Ctrl Pts',(-24.0620883917157,-12.2568075245288,
113.861621595936)) ;
#169547 = CARTESIAN_POINT('Ctrl Pts',(-23.9882845288458,-12.2568075279759,
113.885852578381)) ;
#169548 = CARTESIAN_POINT('Ctrl Pts',(-23.9144806659759,-12.2568075314231,
113.910083560825)) ;
#169549 = CARTESIAN_POINT('Ctrl Pts',(-23.9162161601881,-12.3325103501403,
113.915369597383)) ;
#169550 = CARTESIAN_POINT('Ctrl Pts',(-24.017451872201,-12.3519340314614,
114.188217872385)) ;
#169551 = CARTESIAN_POINT('Ctrl Pts',(-24.0128562086239,-12.4263955875959,
114.174220223673)) ;
#169552 = CARTESIAN_POINT('Ctrl Pts',(-24.0866600683682,-12.4263955990476,
114.149989231708)) ;
#169553 = CARTESIAN_POINT('Ctrl Pts',(-24.1604639281124,-12.4263956104993,
114.125758239743)) ;
#169554 = CARTESIAN_POINT('Ctrl Pts',(-24.1650595916895,-12.3519340543648,
114.139755888456)) ;
#169555 = CARTESIAN_POINT('Ctrl Pts',(-24.1696552552667,-12.2774724982303,
114.153753537168)) ;
#169556 = CARTESIAN_POINT('Ctrl Pts',(-24.0958513955224,-12.2774724867786,
114.177984529133)) ;
#169557 = CARTESIAN_POINT('Ctrl Pts',(-24.0220475357782,-12.2774724753269,
114.202215521098)) ;
#169558 = CARTESIAN_POINT('Ctrl Pts',(-24.017451872201,-12.3519340314614,
114.188217872385)) ;
#169559 = CARTESIAN_POINT('Ctrl Pts',(-24.113519984847,-12.4474402254027,
114.445443546699)) ;
#169560 = CARTESIAN_POINT('Ctrl Pts',(-24.1029419026619,-12.5153461039576,
114.413224416014)) ;
#169561 = CARTESIAN_POINT('Ctrl Pts',(-24.1767457586865,-12.5153461252544,
114.38899341272)) ;
#169562 = CARTESIAN_POINT('Ctrl Pts',(-24.250549614711,-12.5153461465513,
114.364762409425)) ;
#169563 = CARTESIAN_POINT('Ctrl Pts',(-24.2611276968961,-12.4474402679963,
114.39698154011)) ;
#169564 = CARTESIAN_POINT('Ctrl Pts',(-24.2717057790811,-12.3795343894413,
114.429200670795)) ;
#169565 = CARTESIAN_POINT('Ctrl Pts',(-24.1979019230565,-12.3795343681445,
114.45343167409)) ;
#169566 = CARTESIAN_POINT('Ctrl Pts',(-24.124098067032,-12.3795343468477,
114.477662677384)) ;
#169567 = CARTESIAN_POINT('Ctrl Pts',(-24.113519984847,-12.4474402254027,
114.445443546699)) ;
#169568 = CARTESIAN_POINT('Ctrl Pts',(-24.1988643834179,-12.6124878626438,
114.669923303231)) ;
#169569 = CARTESIAN_POINT('Ctrl Pts',(-24.1830452149199,-12.6689727866278,
114.621740669115)) ;
#169570 = CARTESIAN_POINT('Ctrl Pts',(-24.2568490666953,-12.6689728121277,
114.597509652878)) ;
#169571 = CARTESIAN_POINT('Ctrl Pts',(-24.3306529184707,-12.6689728376277,
114.573278636642)) ;
#169572 = CARTESIAN_POINT('Ctrl Pts',(-24.3464720869687,-12.6124879136438,
114.621461270758)) ;
#169573 = CARTESIAN_POINT('Ctrl Pts',(-24.3622912554668,-12.5560029896598,
114.669643904875)) ;
#169574 = CARTESIAN_POINT('Ctrl Pts',(-24.2884874036914,-12.5560029641598,
114.693874921111)) ;
#169575 = CARTESIAN_POINT('Ctrl Pts',(-24.214683551916,-12.5560029386599,
114.718105937348)) ;
#169576 = CARTESIAN_POINT('Ctrl Pts',(-24.1988643834179,-12.6124878626438,
114.669923303231)) ;
#169577 = CARTESIAN_POINT('Ctrl Pts',(-24.2679912812749,-12.8359789539693,
114.844917416136)) ;
#169578 = CARTESIAN_POINT('Ctrl Pts',(-24.2480571471312,-12.8769447916209,
114.78420126043)) ;
#169579 = CARTESIAN_POINT('Ctrl Pts',(-24.3218609949561,-12.8769448154243,
114.759970232161)) ;
#169580 = CARTESIAN_POINT('Ctrl Pts',(-24.395664842781,-12.8769448392277,
114.735739203891)) ;
#169581 = CARTESIAN_POINT('Ctrl Pts',(-24.4155989769246,-12.8359790015761,
114.796455359597)) ;
#169582 = CARTESIAN_POINT('Ctrl Pts',(-24.4355331110683,-12.7950131639245,
114.857171515303)) ;
#169583 = CARTESIAN_POINT('Ctrl Pts',(-24.3617292632435,-12.7950131401211,
114.881402543573)) ;
#169584 = CARTESIAN_POINT('Ctrl Pts',(-24.2879254154186,-12.7950131163177,
114.905633571842)) ;
#169585 = CARTESIAN_POINT('Ctrl Pts',(-24.2679912812749,-12.8359789539693,
114.844917416136)) ;
#169586 = CARTESIAN_POINT('Ctrl Pts',(-24.3163387004766,-13.1004046039055,
114.956742952325)) ;
#169587 = CARTESIAN_POINT('Ctrl Pts',(-24.2937318355072,-13.1229691360916,
114.887886089619)) ;
#169588 = CARTESIAN_POINT('Ctrl Pts',(-24.3675356805423,-13.1229691554338,
114.863655052853)) ;
#169589 = CARTESIAN_POINT('Ctrl Pts',(-24.4413395255774,-13.1229691747759,
114.839424016087)) ;
#169590 = CARTESIAN_POINT('Ctrl Pts',(-24.4639463905468,-13.1004046425898,
114.908280878792)) ;
#169591 = CARTESIAN_POINT('Ctrl Pts',(-24.4865532555163,-13.0778401104037,
114.977137741498)) ;
#169592 = CARTESIAN_POINT('Ctrl Pts',(-24.4127494104811,-13.0778400910615,
115.001368778264)) ;
#169593 = CARTESIAN_POINT('Ctrl Pts',(-24.338945565446,-13.0778400717194,
115.02559981503)) ;
#169594 = CARTESIAN_POINT('Ctrl Pts',(-24.3163387004766,-13.1004046039055,
114.956742952325)) ;
#169595 = CARTESIAN_POINT('Ctrl Pts',(-24.3415133892028,-13.3877822848103,
114.997954547246)) ;
#169596 = CARTESIAN_POINT('Ctrl Pts',(-24.3178484788146,-13.3903147860949,
114.925875048769)) ;
#169597 = CARTESIAN_POINT('Ctrl Pts',(-24.3916523221406,-13.3903147988625,
114.901644006797)) ;
#169598 = CARTESIAN_POINT('Ctrl Pts',(-24.4654561654666,-13.3903148116302,
114.877412964825)) ;
#169599 = CARTESIAN_POINT('Ctrl Pts',(-24.4891210758549,-13.3877823103455,
114.949492463302)) ;
#169600 = CARTESIAN_POINT('Ctrl Pts',(-24.5127859862431,-13.3852498090609,
115.021571961778)) ;
#169601 = CARTESIAN_POINT('Ctrl Pts',(-24.438982142917,-13.3852497962932,
115.04580300375)) ;
#169602 = CARTESIAN_POINT('Ctrl Pts',(-24.365178299591,-13.3852497835256,
115.070034045722)) ;
#169603 = CARTESIAN_POINT('Ctrl Pts',(-24.3415133892028,-13.3877822848103,
114.997954547246)) ;
#169604 = CARTESIAN_POINT('Ctrl Pts',(-24.3423651713577,-13.6773386169807,
114.965081433948)) ;
#169605 = CARTESIAN_POINT('Ctrl Pts',(-24.3193390920628,-13.6596563698358,
114.894947711785)) ;
#169606 = CARTESIAN_POINT('Ctrl Pts',(-24.3931429348365,-13.659656376027,
114.870716668131)) ;
#169607 = CARTESIAN_POINT('Ctrl Pts',(-24.4669467776103,-13.6596563822181,
114.846485624477)) ;
#169608 = CARTESIAN_POINT('Ctrl Pts',(-24.4899728569052,-13.6773386293631,
114.916619346639)) ;
#169609 = CARTESIAN_POINT('Ctrl Pts',(-24.5129989362001,-13.695020876508,
114.986753068802)) ;
#169610 = CARTESIAN_POINT('Ctrl Pts',(-24.4391950934264,-13.6950208703168,
115.010984112456)) ;
#169611 = CARTESIAN_POINT('Ctrl Pts',(-24.3653912506526,-13.6950208641256,
115.03521515611)) ;
#169612 = CARTESIAN_POINT('Ctrl Pts',(-24.3423651713577,-13.6773386169807,
114.965081433948)) ;
#169613 = CARTESIAN_POINT('Ctrl Pts',(-24.3196433120407,-13.9481535278235,
114.860433233373)) ;
#169614 = CARTESIAN_POINT('Ctrl Pts',(-24.2989026954842,-13.9115346180425,
114.797260661859)) ;
#169615 = CARTESIAN_POINT('Ctrl Pts',(-24.3727065385483,-13.9115346192683,
114.773029619089)) ;
#169616 = CARTESIAN_POINT('Ctrl Pts',(-24.4465103816125,-13.9115346204941,
114.74879857632)) ;
#169617 = CARTESIAN_POINT('Ctrl Pts',(-24.467250998169,-13.948153530275,114.811971147834)) ;
#169618 = CARTESIAN_POINT('Ctrl Pts',(-24.4879916147256,-13.984772440056,
114.875143719347)) ;
#169619 = CARTESIAN_POINT('Ctrl Pts',(-24.4141877716614,-13.9847724388302,
114.899374762117)) ;
#169620 = CARTESIAN_POINT('Ctrl Pts',(-24.3403839285972,-13.9847724376044,
114.923605804887)) ;
#169621 = CARTESIAN_POINT('Ctrl Pts',(-24.3196433120407,-13.9481535278235,
114.860433233373)) ;
#169622 = CARTESIAN_POINT('Ctrl Pts',(-24.2756541802911,-14.1811353756388,
114.690976851647)) ;
#169623 = CARTESIAN_POINT('Ctrl Pts',(-24.2586883222684,-14.1281930358969,
114.639301585507)) ;
#169624 = CARTESIAN_POINT('Ctrl Pts',(-24.3324921660103,-14.1281930344687,
114.615070544802)) ;
#169625 = CARTESIAN_POINT('Ctrl Pts',(-24.4062960097522,-14.1281930330404,
114.590839504097)) ;
#169626 = CARTESIAN_POINT('Ctrl Pts',(-24.4232618677749,-14.1811353727823,
114.642514770237)) ;
#169627 = CARTESIAN_POINT('Ctrl Pts',(-24.4402277257976,-14.2340777125242,
114.694190036376)) ;
#169628 = CARTESIAN_POINT('Ctrl Pts',(-24.3664238820557,-14.2340777139524,
114.718421077082)) ;
#169629 = CARTESIAN_POINT('Ctrl Pts',(-24.2926200383138,-14.2340777153806,
114.742652117787)) ;
#169630 = CARTESIAN_POINT('Ctrl Pts',(-24.2756541802911,-14.1811353756388,
114.690976851647)) ;
#169631 = CARTESIAN_POINT('Ctrl Pts',(-24.21454103563,-14.3592804603128,114.469454230547)) ;
#169632 = CARTESIAN_POINT('Ctrl Pts',(-24.2025496065343,-14.2938199374356,
114.432930272264)) ;
#169633 = CARTESIAN_POINT('Ctrl Pts',(-24.2763534508764,-14.2938199356805,
114.408699233387)) ;
#169634 = CARTESIAN_POINT('Ctrl Pts',(-24.3501572952184,-14.2938199339254,
114.384468194509)) ;
#169635 = CARTESIAN_POINT('Ctrl Pts',(-24.362148724314,-14.3592804568026,
114.420992152792)) ;
#169636 = CARTESIAN_POINT('Ctrl Pts',(-24.3741401534097,-14.4247409796798,
114.457516111074)) ;
#169637 = CARTESIAN_POINT('Ctrl Pts',(-24.3003363090677,-14.4247409814349,
114.481747149952)) ;
#169638 = CARTESIAN_POINT('Ctrl Pts',(-24.2265324647257,-14.4247409831899,
114.505978188829)) ;
#169639 = CARTESIAN_POINT('Ctrl Pts',(-24.21454103563,-14.3592804603128,114.469454230547)) ;
#169640 = CARTESIAN_POINT('Ctrl Pts',(-24.1405314237191,-14.4707867328028,
114.208317405989)) ;
#169641 = CARTESIAN_POINT('Ctrl Pts',(-24.1344295829411,-14.3974420670784,
114.189732183463)) ;
#169642 = CARTESIAN_POINT('Ctrl Pts',(-24.2082334270705,-14.3974420666518,
114.165501143937)) ;
#169643 = CARTESIAN_POINT('Ctrl Pts',(-24.2820372711998,-14.3974420662252,
114.141270104412)) ;
#169644 = CARTESIAN_POINT('Ctrl Pts',(-24.2881391119777,-14.4707867319496,
114.159855326938)) ;
#169645 = CARTESIAN_POINT('Ctrl Pts',(-24.2942409527556,-14.5441313976739,
114.178440549464)) ;
#169646 = CARTESIAN_POINT('Ctrl Pts',(-24.2204371086263,-14.5441313981005,
114.20267158899)) ;
#169647 = CARTESIAN_POINT('Ctrl Pts',(-24.146633264497,-14.5441313985271,
114.226902628515)) ;
#169648 = CARTESIAN_POINT('Ctrl Pts',(-24.1405314237191,-14.4707867328028,
114.208317405989)) ;
#169649 = CARTESIAN_POINT('Ctrl Pts',(-24.0613460516658,-14.5057904984994,
113.931879153805)) ;
#169650 = CARTESIAN_POINT('Ctrl Pts',(-24.0614939657,-14.429894649573,113.932329676088)) ;
#169651 = CARTESIAN_POINT('Ctrl Pts',(-24.1352978090977,-14.4298946498541,
113.908098634334)) ;
#169652 = CARTESIAN_POINT('Ctrl Pts',(-24.2091016524954,-14.4298946501351,
113.88386759258)) ;
#169653 = CARTESIAN_POINT('Ctrl Pts',(-24.2089537384612,-14.5057904990616,
113.883417070297)) ;
#169654 = CARTESIAN_POINT('Ctrl Pts',(-24.208805824427,-14.581686347988,113.882966548014)) ;
#169655 = CARTESIAN_POINT('Ctrl Pts',(-24.1350019810292,-14.5816863477069,
113.907197589767)) ;
#169656 = CARTESIAN_POINT('Ctrl Pts',(-24.0611981376315,-14.5816863474258,
113.931428631521)) ;
#169657 = CARTESIAN_POINT('Ctrl Pts',(-24.0613460516658,-14.5057904984994,
113.931879153805)) ;
#169658 = CARTESIAN_POINT('Ctrl Pts',(-23.981949761782,-14.4636194148643,
113.654568691097)) ;
#169659 = CARTESIAN_POINT('Ctrl Pts',(-23.9883761002209,-14.3905570608512,
113.67414228118)) ;
#169660 = CARTESIAN_POINT('Ctrl Pts',(-24.062179942285,-14.3905570601267,
113.649911235364)) ;
#169661 = CARTESIAN_POINT('Ctrl Pts',(-24.135983784349,-14.3905570594022,
113.625680189548)) ;
#169662 = CARTESIAN_POINT('Ctrl Pts',(-24.1295574459101,-14.4636194134152,
113.606106599465)) ;
#169663 = CARTESIAN_POINT('Ctrl Pts',(-24.1231311074711,-14.5366817674283,
113.586533009382)) ;
#169664 = CARTESIAN_POINT('Ctrl Pts',(-24.0493272654071,-14.5366817681528,
113.610764055198)) ;
#169665 = CARTESIAN_POINT('Ctrl Pts',(-23.9755234233431,-14.5366817688773,
113.634995101014)) ;
#169666 = CARTESIAN_POINT('Ctrl Pts',(-23.981949761782,-14.4636194148643,
113.654568691097)) ;
#169667 = CARTESIAN_POINT('Ctrl Pts',(-23.9092977046696,-14.3461280489561,
113.397794692953)) ;
#169668 = CARTESIAN_POINT('Ctrl Pts',(-23.9215407074399,-14.2811630148822,
113.435084904191)) ;
#169669 = CARTESIAN_POINT('Ctrl Pts',(-23.9953445480101,-14.2811630098894,
113.410853853825)) ;
#169670 = CARTESIAN_POINT('Ctrl Pts',(-24.0691483885803,-14.2811630048965,
113.386622803459)) ;
#169671 = CARTESIAN_POINT('Ctrl Pts',(-24.05690538581,-14.3461280389704,113.349332592221)) ;
#169672 = CARTESIAN_POINT('Ctrl Pts',(-24.0446623830397,-14.4110930730442,
113.312042380983)) ;
#169673 = CARTESIAN_POINT('Ctrl Pts',(-23.9708585424695,-14.4110930780371,
113.336273431349)) ;
#169674 = CARTESIAN_POINT('Ctrl Pts',(-23.8970547018993,-14.41109308303,113.360504481715)) ;
#169675 = CARTESIAN_POINT('Ctrl Pts',(-23.9092977046696,-14.3461280489561,
113.397794692953)) ;
#169676 = CARTESIAN_POINT('Ctrl Pts',(-23.8494456096459,-14.1630186070769,
113.180123238634)) ;
#169677 = CARTESIAN_POINT('Ctrl Pts',(-23.8666173455508,-14.1107446176607,
113.232425575869)) ;
#169678 = CARTESIAN_POINT('Ctrl Pts',(-23.940421185266,-14.1107446061865,
113.208194522899)) ;
#169679 = CARTESIAN_POINT('Ctrl Pts',(-24.0142250249813,-14.1107445947124,
113.183963469929)) ;
#169680 = CARTESIAN_POINT('Ctrl Pts',(-23.9970532890764,-14.1630185841287,
113.131661132695)) ;
#169681 = CARTESIAN_POINT('Ctrl Pts',(-23.9798815531715,-14.215292573545,
113.07935879546)) ;
#169682 = CARTESIAN_POINT('Ctrl Pts',(-23.9060777134563,-14.2152925850191,
113.10358984843)) ;
#169683 = CARTESIAN_POINT('Ctrl Pts',(-23.832273873741,-14.2152925964932,
113.1278209014)) ;
#169684 = CARTESIAN_POINT('Ctrl Pts',(-23.8494456096459,-14.1630186070769,
113.180123238634)) ;
#169685 = CARTESIAN_POINT('Ctrl Pts',(-23.8069643592986,-13.9239936072657,
113.01499355577)) ;
#169686 = CARTESIAN_POINT('Ctrl Pts',(-23.8278669143801,-13.8883328136029,
113.078659366449)) ;
#169687 = CARTESIAN_POINT('Ctrl Pts',(-23.9016707537285,-13.8883327903774,
113.054428312361)) ;
#169688 = CARTESIAN_POINT('Ctrl Pts',(-23.9754745930768,-13.8883327671519,
113.030197258274)) ;
#169689 = CARTESIAN_POINT('Ctrl Pts',(-23.9545720379952,-13.9239935608147,
112.966531447595)) ;
#169690 = CARTESIAN_POINT('Ctrl Pts',(-23.9336694829136,-13.9596543544774,
112.902865636916)) ;
#169691 = CARTESIAN_POINT('Ctrl Pts',(-23.8598656435653,-13.9596543777029,
112.927096691003)) ;
#169692 = CARTESIAN_POINT('Ctrl Pts',(-23.7860618042169,-13.9596544009284,
112.951327745091)) ;
#169693 = CARTESIAN_POINT('Ctrl Pts',(-23.8069643592986,-13.9239936072657,
113.01499355577)) ;
#169694 = CARTESIAN_POINT('Ctrl Pts',(-23.7864462608402,-13.6520857920573,
112.917251285057)) ;
#169695 = CARTESIAN_POINT('Ctrl Pts',(-23.8095408056918,-13.6353584241277,
112.987593543021)) ;
#169696 = CARTESIAN_POINT('Ctrl Pts',(-23.8833446466771,-13.6353583920573,
112.96336249392)) ;
#169697 = CARTESIAN_POINT('Ctrl Pts',(-23.9571484876624,-13.635358359987,
112.939131444818)) ;
#169698 = CARTESIAN_POINT('Ctrl Pts',(-23.9340539428108,-13.6520857279166,
112.868789186854)) ;
#169699 = CARTESIAN_POINT('Ctrl Pts',(-23.9109593979592,-13.6688130958462,
112.79844692889)) ;
#169700 = CARTESIAN_POINT('Ctrl Pts',(-23.8371555569739,-13.6688131279166,
112.822677977992)) ;
#169701 = CARTESIAN_POINT('Ctrl Pts',(-23.7633517159886,-13.668813159987,
112.846909027093)) ;
#169702 = CARTESIAN_POINT('Ctrl Pts',(-23.7864462608402,-13.6520857920573,
112.917251285057)) ;
#169703 = CARTESIAN_POINT('Ctrl Pts',(-23.7894943758897,-13.3607989189298,
112.890930631403)) ;
#169704 = CARTESIAN_POINT('Ctrl Pts',(-23.8131463729172,-13.3643850289944,
112.962970798943)) ;
#169705 = CARTESIAN_POINT('Ctrl Pts',(-23.8869502167856,-13.3643849861059,
112.938739758623)) ;
#169706 = CARTESIAN_POINT('Ctrl Pts',(-23.9607540606539,-13.3643849432174,
112.914508718302)) ;
#169707 = CARTESIAN_POINT('Ctrl Pts',(-23.9371020636264,-13.3607988331528,
112.842468550762)) ;
#169708 = CARTESIAN_POINT('Ctrl Pts',(-23.9134500665988,-13.3572127230881,
112.770428383222)) ;
#169709 = CARTESIAN_POINT('Ctrl Pts',(-23.8396462227305,-13.3572127659766,
112.794659423543)) ;
#169710 = CARTESIAN_POINT('Ctrl Pts',(-23.7658423788621,-13.3572128088652,
112.818890463863)) ;
#169711 = CARTESIAN_POINT('Ctrl Pts',(-23.7894943758897,-13.3607989189298,
112.890930631403)) ;
#169712 = CARTESIAN_POINT('Ctrl Pts',(-23.8167514278251,-13.0758433976518,
112.938634896679)) ;
#169713 = CARTESIAN_POINT('Ctrl Pts',(-23.8392651657168,-13.0993300266372,
113.007208110689)) ;
#169714 = CARTESIAN_POINT('Ctrl Pts',(-23.9130690138605,-13.0993299787843,
112.982977083391)) ;
#169715 = CARTESIAN_POINT('Ctrl Pts',(-23.9868728620042,-13.0993299309314,
112.958746056093)) ;
#169716 = CARTESIAN_POINT('Ctrl Pts',(-23.9643591241125,-13.075843301946,
112.890172842083)) ;
#169717 = CARTESIAN_POINT('Ctrl Pts',(-23.9418453862208,-13.0523566729605,
112.821599628073)) ;
#169718 = CARTESIAN_POINT('Ctrl Pts',(-23.8680415380771,-13.0523567208134,
112.845830655371)) ;
#169719 = CARTESIAN_POINT('Ctrl Pts',(-23.7942376899334,-13.0523567686663,
112.870061682669)) ;
#169720 = CARTESIAN_POINT('Ctrl Pts',(-23.8167514278251,-13.0758433976518,
112.938634896679)) ;
#169721 = CARTESIAN_POINT('Ctrl Pts',(-23.8671295596071,-12.8137701829539,
113.056567674092)) ;
#169722 = CARTESIAN_POINT('Ctrl Pts',(-23.8868933516135,-12.8555883335488,
113.116764996813)) ;
#169723 = CARTESIAN_POINT('Ctrl Pts',(-23.9606972050676,-12.8555882837421,
113.092533985689)) ;
#169724 = CARTESIAN_POINT('Ctrl Pts',(-24.0345010585216,-12.8555882339354,
113.068302974566)) ;
#169725 = CARTESIAN_POINT('Ctrl Pts',(-24.0147372665152,-12.8137700833405,
113.008105651844)) ;
#169726 = CARTESIAN_POINT('Ctrl Pts',(-23.9949734745088,-12.7719519327456,
112.947908329123)) ;
#169727 = CARTESIAN_POINT('Ctrl Pts',(-23.9211696210548,-12.7719519825523,
112.972139340247)) ;
#169728 = CARTESIAN_POINT('Ctrl Pts',(-23.8473657676007,-12.771952032359,
112.99637035137)) ;
#169729 = CARTESIAN_POINT('Ctrl Pts',(-23.8671295596071,-12.8137701829539,
113.056567674092)) ;
#169730 = CARTESIAN_POINT('Ctrl Pts',(-23.9380620209041,-12.5948352961054,
113.237023873309)) ;
#169731 = CARTESIAN_POINT('Ctrl Pts',(-23.9536386278267,-12.6519997752805,
113.284467706048)) ;
#169732 = CARTESIAN_POINT('Ctrl Pts',(-24.0274424873426,-12.6519997298115,
113.260236713388)) ;
#169733 = CARTESIAN_POINT('Ctrl Pts',(-24.1012463468584,-12.6519996843424,
113.236005720728)) ;
#169734 = CARTESIAN_POINT('Ctrl Pts',(-24.0856697399359,-12.5948352051674,
113.188561887988)) ;
#169735 = CARTESIAN_POINT('Ctrl Pts',(-24.0700931330132,-12.5376707259923,
113.141118055248)) ;
#169736 = CARTESIAN_POINT('Ctrl Pts',(-23.9962892734974,-12.5376707714613,
113.165349047909)) ;
#169737 = CARTESIAN_POINT('Ctrl Pts',(-23.9224854139815,-12.5376708169303,
113.189580040569)) ;
#169738 = CARTESIAN_POINT('Ctrl Pts',(-23.9380620209041,-12.5948352961054,
113.237023873309)) ;
#169739 = CARTESIAN_POINT('Ctrl Pts',(-24.0241344799407,-12.4363827345609,
113.463912936618)) ;
#169740 = CARTESIAN_POINT('Ctrl Pts',(-24.034454027819,-12.5046923403289,
113.495344615851)) ;
#169741 = CARTESIAN_POINT('Ctrl Pts',(-24.1082578922502,-12.5046923075435,
113.471113638162)) ;
#169742 = CARTESIAN_POINT('Ctrl Pts',(-24.1820617566815,-12.5046922747581,
113.446882660473)) ;
#169743 = CARTESIAN_POINT('Ctrl Pts',(-24.1717422088033,-12.4363826689901,
113.415450981241)) ;
#169744 = CARTESIAN_POINT('Ctrl Pts',(-24.1614226609251,-12.368073063222,
113.384019302008)) ;
#169745 = CARTESIAN_POINT('Ctrl Pts',(-24.0876187964938,-12.3680730960074,
113.408250279697)) ;
#169746 = CARTESIAN_POINT('Ctrl Pts',(-24.0138149320625,-12.3680731287928,
113.432481257386)) ;
#169747 = CARTESIAN_POINT('Ctrl Pts',(-24.0241344799407,-12.4363827345609,
113.463912936618)) ;
#169748 = CARTESIAN_POINT('Ctrl Pts',(-24.1211715621355,-12.3469185629382,
113.723977397692)) ;
#169749 = CARTESIAN_POINT('Ctrl Pts',(-24.1254657239507,-12.4215734203002,
113.737056723317)) ;
#169750 = CARTESIAN_POINT('Ctrl Pts',(-24.1992695926889,-12.4215734050828,
113.712825758746)) ;
#169751 = CARTESIAN_POINT('Ctrl Pts',(-24.2730734614271,-12.4215733898654,
113.688594794176)) ;
#169752 = CARTESIAN_POINT('Ctrl Pts',(-24.2687792996119,-12.3469185325034,
113.675515468551)) ;
#169753 = CARTESIAN_POINT('Ctrl Pts',(-24.2644851377967,-12.2722636751415,
113.662436142925)) ;
#169754 = CARTESIAN_POINT('Ctrl Pts',(-24.1906812690584,-12.2722636903589,
113.686667107496)) ;
#169755 = CARTESIAN_POINT('Ctrl Pts',(-24.1168774003202,-12.2722637055763,
113.710898072066)) ;
#169756 = CARTESIAN_POINT('Ctrl Pts',(-24.1211715621355,-12.3469185629382,
113.723977397692)) ;
#169757 = CARTESIAN_POINT('Ctrl Pts',(-24.2227254729925,-12.3346897142696,
113.997726976907)) ;
#169758 = CARTESIAN_POINT('Ctrl Pts',(-24.2206716932284,-12.410307219777,
113.991471496858)) ;
#169759 = CARTESIAN_POINT('Ctrl Pts',(-24.2944755645646,-12.4103072275808,
113.967240540201)) ;
#169760 = CARTESIAN_POINT('Ctrl Pts',(-24.3682794359007,-12.4103072353845,
113.943009583543)) ;
#169761 = CARTESIAN_POINT('Ctrl Pts',(-24.3703332156647,-12.3346897298771,
113.949265063591)) ;
#169762 = CARTESIAN_POINT('Ctrl Pts',(-24.3723869954288,-12.2590722243697,
113.95552054364)) ;
#169763 = CARTESIAN_POINT('Ctrl Pts',(-24.2985831240927,-12.259072216566,
113.979751500297)) ;
#169764 = CARTESIAN_POINT('Ctrl Pts',(-24.2247792527566,-12.2590722087622,
114.003982456955)) ;
#169765 = CARTESIAN_POINT('Ctrl Pts',(-24.2227254729925,-12.3346897142696,
113.997726976907)) ;
#169766 = CARTESIAN_POINT('Ctrl Pts',(-24.3213836615378,-12.3996707792268,
114.262894713048)) ;
#169767 = CARTESIAN_POINT('Ctrl Pts',(-24.3131699295231,-12.470861286488,
114.237877012443)) ;
#169768 = CARTESIAN_POINT('Ctrl Pts',(-24.3869738006343,-12.4708613194526,
114.2136460551)) ;
#169769 = CARTESIAN_POINT('Ctrl Pts',(-24.4607776717455,-12.4708613524172,
114.189415097757)) ;
#169770 = CARTESIAN_POINT('Ctrl Pts',(-24.4689914037601,-12.3996708451561,
114.214432798363)) ;
#169771 = CARTESIAN_POINT('Ctrl Pts',(-24.4772051357748,-12.3284803378949,
114.239450498968)) ;
#169772 = CARTESIAN_POINT('Ctrl Pts',(-24.4034012646637,-12.3284803049303,
114.263681456311)) ;
#169773 = CARTESIAN_POINT('Ctrl Pts',(-24.3295973935525,-12.3284802719657,
114.287912413654)) ;
#169774 = CARTESIAN_POINT('Ctrl Pts',(-24.3213836615378,-12.3996707792268,
114.262894713048)) ;
#169775 = CARTESIAN_POINT('Ctrl Pts',(-24.4121011317654,-12.5380776390174,
114.503646698879)) ;
#169776 = CARTESIAN_POINT('Ctrl Pts',(-24.3982776140999,-12.5997094329327,
114.461542496421)) ;
#169777 = CARTESIAN_POINT('Ctrl Pts',(-24.4720814828292,-12.5997094914945,
114.437311531823)) ;
#169778 = CARTESIAN_POINT('Ctrl Pts',(-24.5458853515585,-12.5997095500564,
114.413080567226)) ;
#169779 = CARTESIAN_POINT('Ctrl Pts',(-24.559708869224,-12.5380777561411,
114.455184769684)) ;
#169780 = CARTESIAN_POINT('Ctrl Pts',(-24.5735323868896,-12.4764459622258,
114.497288972142)) ;
#169781 = CARTESIAN_POINT('Ctrl Pts',(-24.4997285181602,-12.476445903664,
114.52151993674)) ;
#169782 = CARTESIAN_POINT('Ctrl Pts',(-24.4259246494309,-12.4764458451021,
114.545750901337)) ;
#169783 = CARTESIAN_POINT('Ctrl Pts',(-24.4121011317654,-12.5380776390174,
114.503646698879)) ;
#169784 = CARTESIAN_POINT('Ctrl Pts',(-24.488256946051,-12.739380812412,114.700140077213)) ;
#169785 = CARTESIAN_POINT('Ctrl Pts',(-24.4698300851511,-12.7870487344557,
114.644014834082)) ;
#169786 = CARTESIAN_POINT('Ctrl Pts',(-24.5436339488168,-12.7870488154654,
114.619783854061)) ;
#169787 = CARTESIAN_POINT('Ctrl Pts',(-24.6174378124824,-12.7870488964751,
114.59555287404)) ;
#169788 = CARTESIAN_POINT('Ctrl Pts',(-24.6358646733823,-12.7393809744314,
114.651678117172)) ;
#169789 = CARTESIAN_POINT('Ctrl Pts',(-24.6542915342823,-12.6917130523877,
114.707803360304)) ;
#169790 = CARTESIAN_POINT('Ctrl Pts',(-24.5804876706166,-12.691712971378,
114.732034340324)) ;
#169791 = CARTESIAN_POINT('Ctrl Pts',(-24.506683806951,-12.6917128903682,
114.756265320345)) ;
#169792 = CARTESIAN_POINT('Ctrl Pts',(-24.488256946051,-12.739380812412,114.700140077213)) ;
#169793 = CARTESIAN_POINT('Ctrl Pts',(-24.5454206194932,-12.9893867745162,
114.838765803688)) ;
#169794 = CARTESIAN_POINT('Ctrl Pts',(-24.5237099602011,-13.0196703754918,
114.772638640544)) ;
#169795 = CARTESIAN_POINT('Ctrl Pts',(-24.59751381674,-13.0196704733174,114.748407638817)) ;
#169796 = CARTESIAN_POINT('Ctrl Pts',(-24.671317673279,-13.019670571143,114.724176637089)) ;
#169797 = CARTESIAN_POINT('Ctrl Pts',(-24.6930283325711,-12.9893869701674,
114.790303800233)) ;
#169798 = CARTESIAN_POINT('Ctrl Pts',(-24.7147389918632,-12.9591033691919,
114.856430963377)) ;
#169799 = CARTESIAN_POINT('Ctrl Pts',(-24.6409351353243,-12.9591032713663,
114.880661965104)) ;
#169800 = CARTESIAN_POINT('Ctrl Pts',(-24.5671312787853,-12.9591031735407,
114.904892966831)) ;
#169801 = CARTESIAN_POINT('Ctrl Pts',(-24.5454206194932,-12.9893867745162,
114.838765803688)) ;
#169802 = CARTESIAN_POINT('Ctrl Pts',(-24.5802165214264,-13.2694171615401,
114.909351828959)) ;
#169803 = CARTESIAN_POINT('Ctrl Pts',(-24.5567770069868,-13.2801946819997,
114.837958852016)) ;
#169804 = CARTESIAN_POINT('Ctrl Pts',(-24.6305808550088,-13.2801947890163,
114.813727824347)) ;
#169805 = CARTESIAN_POINT('Ctrl Pts',(-24.7043847030307,-13.2801948960329,
114.789496796678)) ;
#169806 = CARTESIAN_POINT('Ctrl Pts',(-24.7278242174703,-13.2694173755733,
114.860889773621)) ;
#169807 = CARTESIAN_POINT('Ctrl Pts',(-24.7512637319099,-13.2586398551137,
114.932282750565)) ;
#169808 = CARTESIAN_POINT('Ctrl Pts',(-24.677459883888,-13.2586397480971,
114.956513778234)) ;
#169809 = CARTESIAN_POINT('Ctrl Pts',(-24.603656035866,-13.2586396410806,
114.980744805903)) ;
#169810 = CARTESIAN_POINT('Ctrl Pts',(-24.5802165214264,-13.2694171615401,
114.909351828959)) ;
#169811 = CARTESIAN_POINT('Ctrl Pts',(-24.5909392079198,-13.5619468890867,
114.906377302558)) ;
#169812 = CARTESIAN_POINT('Ctrl Pts',(-24.5674535497162,-13.5523172456924,
114.834843779161)) ;
#169813 = CARTESIAN_POINT('Ctrl Pts',(-24.6412573886373,-13.5523173531236,
114.810612723773)) ;
#169814 = CARTESIAN_POINT('Ctrl Pts',(-24.7150612275583,-13.5523174605549,
114.786381668384)) ;
#169815 = CARTESIAN_POINT('Ctrl Pts',(-24.7385468857619,-13.5619471039492,
114.85791519178)) ;
#169816 = CARTESIAN_POINT('Ctrl Pts',(-24.7620325439655,-13.5715767473435,
114.929448715177)) ;
#169817 = CARTESIAN_POINT('Ctrl Pts',(-24.6882287050445,-13.5715766399123,
114.953679770565)) ;
#169818 = CARTESIAN_POINT('Ctrl Pts',(-24.6144248661234,-13.5715765324811,
114.977910825954)) ;
#169819 = CARTESIAN_POINT('Ctrl Pts',(-24.5909392079198,-13.5619468890867,
114.906377302558)) ;
#169820 = CARTESIAN_POINT('Ctrl Pts',(-24.5776432777125,-13.8411213292838,
114.83064171812)) ;
#169821 = CARTESIAN_POINT('Ctrl Pts',(-24.5557804108624,-13.8119862931275,
114.764050955339)) ;
#169822 = CARTESIAN_POINT('Ctrl Pts',(-24.6295842411457,-13.8119863923944,
114.739819873641)) ;
#169823 = CARTESIAN_POINT('Ctrl Pts',(-24.7033880714288,-13.8119864916613,
114.715588791943)) ;
#169824 = CARTESIAN_POINT('Ctrl Pts',(-24.7252509382789,-13.8411215278176,
114.782179554724)) ;
#169825 = CARTESIAN_POINT('Ctrl Pts',(-24.7471138051289,-13.870256563974,
114.848770317504)) ;
#169826 = CARTESIAN_POINT('Ctrl Pts',(-24.6733099748457,-13.8702564647071,
114.873001399203)) ;
#169827 = CARTESIAN_POINT('Ctrl Pts',(-24.5995061445625,-13.8702563654402,
114.897232480901)) ;
#169828 = CARTESIAN_POINT('Ctrl Pts',(-24.5776432777125,-13.8411213292838,
114.83064171812)) ;
#169829 = CARTESIAN_POINT('Ctrl Pts',(-24.5417994729014,-14.0928083771544,
114.685855733235)) ;
#169830 = CARTESIAN_POINT('Ctrl Pts',(-24.5231432551102,-14.0460580395473,
114.629031906056)) ;
#169831 = CARTESIAN_POINT('Ctrl Pts',(-24.5969470779918,-14.0460581223417,
114.604800801814)) ;
#169832 = CARTESIAN_POINT('Ctrl Pts',(-24.6707509008735,-14.0460582051361,
114.580569697572)) ;
#169833 = CARTESIAN_POINT('Ctrl Pts',(-24.6894071186647,-14.0928085427432,
114.637393524751)) ;
#169834 = CARTESIAN_POINT('Ctrl Pts',(-24.7080633364559,-14.1395588803503,
114.694217351929)) ;
#169835 = CARTESIAN_POINT('Ctrl Pts',(-24.6342595135742,-14.1395587975559,
114.718448456171)) ;
#169836 = CARTESIAN_POINT('Ctrl Pts',(-24.5604556906926,-14.1395587147615,
114.742679560413)) ;
#169837 = CARTESIAN_POINT('Ctrl Pts',(-24.5417994729014,-14.0928083771544,
114.685855733235)) ;
#169838 = CARTESIAN_POINT('Ctrl Pts',(-24.4870105886222,-14.2946225939457,
114.483569102264)) ;
#169839 = CARTESIAN_POINT('Ctrl Pts',(-24.4728844270664,-14.2337123839225,
114.4405430954)) ;
#169840 = CARTESIAN_POINT('Ctrl Pts',(-24.5466882445676,-14.2337124445756,
114.41631197477)) ;
#169841 = CARTESIAN_POINT('Ctrl Pts',(-24.6204920620688,-14.2337125052288,
114.39208085414)) ;
#169842 = CARTESIAN_POINT('Ctrl Pts',(-24.6346182236247,-14.2946227152521,
114.435106861004)) ;
#169843 = CARTESIAN_POINT('Ctrl Pts',(-24.6487443851805,-14.3555329252753,
114.478132867868)) ;
#169844 = CARTESIAN_POINT('Ctrl Pts',(-24.5749405676793,-14.3555328646222,
114.502363988498)) ;
#169845 = CARTESIAN_POINT('Ctrl Pts',(-24.5011367501781,-14.355532803969,
114.526595109128)) ;
#169846 = CARTESIAN_POINT('Ctrl Pts',(-24.4870105886222,-14.2946225939457,
114.483569102264)) ;
#169847 = CARTESIAN_POINT('Ctrl Pts',(-24.4178592615303,-14.4342154714355,
114.237501249069)) ;
#169848 = CARTESIAN_POINT('Ctrl Pts',(-24.4092733028564,-14.3634681415102,
114.211349806201)) ;
#169849 = CARTESIAN_POINT('Ctrl Pts',(-24.483077117361,-14.3634681764234,
114.187118676444)) ;
#169850 = CARTESIAN_POINT('Ctrl Pts',(-24.5568809318657,-14.3634682113365,
114.162887546687)) ;
#169851 = CARTESIAN_POINT('Ctrl Pts',(-24.5654668905395,-14.4342155412618,
114.189038989554)) ;
#169852 = CARTESIAN_POINT('Ctrl Pts',(-24.5740528492134,-14.5049628711871,
114.215190432422)) ;
#169853 = CARTESIAN_POINT('Ctrl Pts',(-24.5002490347088,-14.5049628362739,
114.239421562179)) ;
#169854 = CARTESIAN_POINT('Ctrl Pts',(-24.4264452202042,-14.5049628013607,
114.263652691936)) ;
#169855 = CARTESIAN_POINT('Ctrl Pts',(-24.4178592615303,-14.4342154714355,
114.237501249069)) ;
#169856 = CARTESIAN_POINT('Ctrl Pts',(-24.3396042038614,-14.5009486089819,
113.96352975376)) ;
#169857 = CARTESIAN_POINT('Ctrl Pts',(-24.3372058944274,-14.4254353908754,
113.956224891987)) ;
#169858 = CARTESIAN_POINT('Ctrl Pts',(-24.4110097089487,-14.4254353992881,
113.93199376228)) ;
#169859 = CARTESIAN_POINT('Ctrl Pts',(-24.4848135234698,-14.4254354077009,
113.907762632573)) ;
#169860 = CARTESIAN_POINT('Ctrl Pts',(-24.4872118329038,-14.5009486258073,
113.915067494347)) ;
#169861 = CARTESIAN_POINT('Ctrl Pts',(-24.4896101423378,-14.5764618439138,
113.92237235612)) ;
#169862 = CARTESIAN_POINT('Ctrl Pts',(-24.4158063278166,-14.5764618355011,
113.946603485826)) ;
#169863 = CARTESIAN_POINT('Ctrl Pts',(-24.3420025132954,-14.5764618270883,
113.970834615533)) ;
#169864 = CARTESIAN_POINT('Ctrl Pts',(-24.3396042038614,-14.5009486089819,
113.96352975376)) ;
#169865 = CARTESIAN_POINT('Ctrl Pts',(-24.2597681290623,-14.4900601303297,
113.68508815172)) ;
#169866 = CARTESIAN_POINT('Ctrl Pts',(-24.2636701688541,-14.4151940072696,
113.69697313704)) ;
#169867 = CARTESIAN_POINT('Ctrl Pts',(-24.3374739851644,-14.4151939916633,
113.672742012783)) ;
#169868 = CARTESIAN_POINT('Ctrl Pts',(-24.4112778014747,-14.4151939760569,
113.648510888525)) ;
#169869 = CARTESIAN_POINT('Ctrl Pts',(-24.4073757616829,-14.490060099117,
113.636625903205)) ;
#169870 = CARTESIAN_POINT('Ctrl Pts',(-24.4034737218912,-14.564926222177,
113.624740917885)) ;
#169871 = CARTESIAN_POINT('Ctrl Pts',(-24.3296699055809,-14.5649262377834,
113.648972042142)) ;
#169872 = CARTESIAN_POINT('Ctrl Pts',(-24.2558660892706,-14.5649262533898,
113.6732031664)) ;
#169873 = CARTESIAN_POINT('Ctrl Pts',(-24.2597681290623,-14.4900601303297,
113.68508815172)) ;
#169874 = CARTESIAN_POINT('Ctrl Pts',(-24.1834123171793,-14.4021465802023,
113.416932198274)) ;
#169875 = CARTESIAN_POINT('Ctrl Pts',(-24.1933877112254,-14.3333051056759,
113.447315640572)) ;
#169876 = CARTESIAN_POINT('Ctrl Pts',(-24.2671915319703,-14.3333050707066,
113.423084529822)) ;
#169877 = CARTESIAN_POINT('Ctrl Pts',(-24.3409953527152,-14.3333050357374,
113.398853419072)) ;
#169878 = CARTESIAN_POINT('Ctrl Pts',(-24.3310199586691,-14.4021465102638,
113.368469976773)) ;
#169879 = CARTESIAN_POINT('Ctrl Pts',(-24.321044564623,-14.4709879847903,
113.338086534475)) ;
#169880 = CARTESIAN_POINT('Ctrl Pts',(-24.2472407438781,-14.4709880197595,
113.362317645225)) ;
#169881 = CARTESIAN_POINT('Ctrl Pts',(-24.1734369231332,-14.4709880547288,
113.386548755976)) ;
#169882 = CARTESIAN_POINT('Ctrl Pts',(-24.1834123171793,-14.4021465802023,
113.416932198274)) ;
#169883 = CARTESIAN_POINT('Ctrl Pts',(-24.1178153865265,-14.2443882215466,
113.181766630605)) ;
#169884 = CARTESIAN_POINT('Ctrl Pts',(-24.1331176094938,-14.1864574930971,
113.228374734188)) ;
#169885 = CARTESIAN_POINT('Ctrl Pts',(-24.206921435554,-14.1864574444021,
113.204143639628)) ;
#169886 = CARTESIAN_POINT('Ctrl Pts',(-24.2807252616142,-14.1864573957072,
113.179912545067)) ;
#169887 = CARTESIAN_POINT('Ctrl Pts',(-24.2654230386468,-14.2443881241568,
113.133304441483)) ;
#169888 = CARTESIAN_POINT('Ctrl Pts',(-24.2501208156794,-14.3023188526063,
113.0866963379)) ;
#169889 = CARTESIAN_POINT('Ctrl Pts',(-24.1763169896193,-14.3023189013012,
113.110927432461)) ;
#169890 = CARTESIAN_POINT('Ctrl Pts',(-24.1025131635591,-14.3023189499961,
113.135158527022)) ;
#169891 = CARTESIAN_POINT('Ctrl Pts',(-24.1178153865265,-14.2443882215466,
113.181766630605)) ;
#169892 = CARTESIAN_POINT('Ctrl Pts',(-24.0676784811312,-14.0257063779415,
112.993394903444)) ;
#169893 = CARTESIAN_POINT('Ctrl Pts',(-24.0872425216887,-13.9829558305902,
113.052983815574)) ;
#169894 = CARTESIAN_POINT('Ctrl Pts',(-24.1610463541072,-13.9829557770323,
113.028752740379)) ;
#169895 = CARTESIAN_POINT('Ctrl Pts',(-24.2348501865257,-13.9829557234744,
113.004521665184)) ;
#169896 = CARTESIAN_POINT('Ctrl Pts',(-24.2152861459681,-14.0257062708258,
112.944932753054)) ;
#169897 = CARTESIAN_POINT('Ctrl Pts',(-24.1957221054106,-14.0684568181771,
112.885343840924)) ;
#169898 = CARTESIAN_POINT('Ctrl Pts',(-24.1219182729921,-14.068456871735,
112.909574916119)) ;
#169899 = CARTESIAN_POINT('Ctrl Pts',(-24.0481144405737,-14.0684569252929,
112.933805991313)) ;
#169900 = CARTESIAN_POINT('Ctrl Pts',(-24.0676784811312,-14.0257063779415,
112.993394903444)) ;
#169901 = CARTESIAN_POINT('Ctrl Pts',(-24.0381389778697,-13.7667943185538,
112.86824672277)) ;
#169902 = CARTESIAN_POINT('Ctrl Pts',(-24.0605227986181,-13.7420568683352,
112.936424230282)) ;
#169903 = CARTESIAN_POINT('Ctrl Pts',(-24.1343266364055,-13.7420568128391,
112.91219317144)) ;
#169904 = CARTESIAN_POINT('Ctrl Pts',(-24.2081304741928,-13.7420567573429,
112.887962112598)) ;
#169905 = CARTESIAN_POINT('Ctrl Pts',(-24.1857466534444,-13.7667942075616,
112.819784605086)) ;
#169906 = CARTESIAN_POINT('Ctrl Pts',(-24.1633628326959,-13.7915316577803,
112.751607097573)) ;
#169907 = CARTESIAN_POINT('Ctrl Pts',(-24.0895589949086,-13.7915317132764,
112.775838156415)) ;
#169908 = CARTESIAN_POINT('Ctrl Pts',(-24.0157551571213,-13.7915317687725,
112.800069215258)) ;
#169909 = CARTESIAN_POINT('Ctrl Pts',(-24.0381389778697,-13.7667943185538,
112.86824672277)) ;
#169910 = CARTESIAN_POINT('Ctrl Pts',(-24.0313067339811,-13.4796298971122,
112.81179860376)) ;
#169911 = CARTESIAN_POINT('Ctrl Pts',(-24.0549391608204,-13.4749049518927,
112.883779163764)) ;
#169912 = CARTESIAN_POINT('Ctrl Pts',(-24.1287430036364,-13.4749049038309,
112.859548120238)) ;
#169913 = CARTESIAN_POINT('Ctrl Pts',(-24.2025468464523,-13.474904855769,
112.835317076712)) ;
#169914 = CARTESIAN_POINT('Ctrl Pts',(-24.178914419613,-13.4796298009885,
112.763336516709)) ;
#169915 = CARTESIAN_POINT('Ctrl Pts',(-24.1552819927736,-13.4843547462079,
112.691355956706)) ;
#169916 = CARTESIAN_POINT('Ctrl Pts',(-24.0814781499577,-13.4843547942698,
112.715587000231)) ;
#169917 = CARTESIAN_POINT('Ctrl Pts',(-24.0076743071417,-13.4843548423316,
112.739818043757)) ;
#169918 = CARTESIAN_POINT('Ctrl Pts',(-24.0313067339811,-13.4796298971122,
112.81179860376)) ;
#169919 = CARTESIAN_POINT('Ctrl Pts',(-24.0487404996973,-13.1904267551927,
112.829580265168)) ;
#169920 = CARTESIAN_POINT('Ctrl Pts',(-24.0719222496774,-13.2058873743104,
112.900188136033)) ;
#169921 = CARTESIAN_POINT('Ctrl Pts',(-24.1457260959883,-13.2058873346672,
112.875957103152)) ;
#169922 = CARTESIAN_POINT('Ctrl Pts',(-24.2195299422992,-13.205887295024,
112.851726070272)) ;
#169923 = CARTESIAN_POINT('Ctrl Pts',(-24.1963481923192,-13.1904266759062,
112.781118199406)) ;
#169924 = CARTESIAN_POINT('Ctrl Pts',(-24.1731664423392,-13.1749660567885,
112.710510328541)) ;
#169925 = CARTESIAN_POINT('Ctrl Pts',(-24.0993625960283,-13.1749660964317,
112.734741361422)) ;
#169926 = CARTESIAN_POINT('Ctrl Pts',(-24.0255587497174,-13.1749661360749,
112.758972394302)) ;
#169927 = CARTESIAN_POINT('Ctrl Pts',(-24.0487404996973,-13.1904267551927,
112.829580265168)) ;
#169928 = CARTESIAN_POINT('Ctrl Pts',(-24.0902477017721,-12.9149395489465,
112.920337621988)) ;
#169929 = CARTESIAN_POINT('Ctrl Pts',(-24.1113047035226,-12.9496591977343,
112.98447385237)) ;
#169930 = CARTESIAN_POINT('Ctrl Pts',(-24.1851085515239,-12.9496591712855,
112.960242824638)) ;
#169931 = CARTESIAN_POINT('Ctrl Pts',(-24.2589123995253,-12.9496591448368,
112.936011796906)) ;
#169932 = CARTESIAN_POINT('Ctrl Pts',(-24.2378553977748,-12.914939496049,
112.871875566525)) ;
#169933 = CARTESIAN_POINT('Ctrl Pts',(-24.2167983960244,-12.8802198472613,
112.807739336143)) ;
#169934 = CARTESIAN_POINT('Ctrl Pts',(-24.142994548023,-12.88021987371,112.831970363875)) ;
#169935 = CARTESIAN_POINT('Ctrl Pts',(-24.0691907000217,-12.8802199001588,
112.856201391607)) ;
#169936 = CARTESIAN_POINT('Ctrl Pts',(-24.0902477017721,-12.9149395489465,
112.920337621988)) ;
#169937 = CARTESIAN_POINT('Ctrl Pts',(-24.1529087502765,-12.6780026906519,
113.075870610028)) ;
#169938 = CARTESIAN_POINT('Ctrl Pts',(-24.1703532645626,-12.7293185102392,
113.129003786334)) ;
#169939 = CARTESIAN_POINT('Ctrl Pts',(-24.2441571130729,-12.7293184935026,
113.104772760153)) ;
#169940 = CARTESIAN_POINT('Ctrl Pts',(-24.3179609615833,-12.729318476766,
113.080541733971)) ;
#169941 = CARTESIAN_POINT('Ctrl Pts',(-24.3005164472972,-12.6780026571787,
113.027408557665)) ;
#169942 = CARTESIAN_POINT('Ctrl Pts',(-24.2830719330111,-12.6266868375913,
112.974275381359)) ;
#169943 = CARTESIAN_POINT('Ctrl Pts',(-24.2092680845008,-12.6266868543279,
112.998506407541)) ;
#169944 = CARTESIAN_POINT('Ctrl Pts',(-24.1354642359904,-12.6266868710645,
113.022737433722)) ;
#169945 = CARTESIAN_POINT('Ctrl Pts',(-24.1529087502765,-12.6780026906519,
113.075870610028)) ;
#169946 = CARTESIAN_POINT('Ctrl Pts',(-24.2335276358452,-12.492912372698,
113.285956395486)) ;
#169947 = CARTESIAN_POINT('Ctrl Pts',(-24.2461033083903,-12.5572296336134,
113.324259865286)) ;
#169948 = CARTESIAN_POINT('Ctrl Pts',(-24.3199071561044,-12.5572296258791,
113.300028836679)) ;
#169949 = CARTESIAN_POINT('Ctrl Pts',(-24.3937110038185,-12.5572296181447,
113.275797808072)) ;
#169950 = CARTESIAN_POINT('Ctrl Pts',(-24.3811353312734,-12.4929123572293,
113.237494338272)) ;
#169951 = CARTESIAN_POINT('Ctrl Pts',(-24.3685596587283,-12.4285950963139,
113.199190868472)) ;
#169952 = CARTESIAN_POINT('Ctrl Pts',(-24.2947558110142,-12.4285951040482,
113.223421897078)) ;
#169953 = CARTESIAN_POINT('Ctrl Pts',(-24.2209519633001,-12.4285951117825,
113.247652925685)) ;
#169954 = CARTESIAN_POINT('Ctrl Pts',(-24.2335276358452,-12.492912372698,
113.285956395486)) ;
#169955 = CARTESIAN_POINT('Ctrl Pts',(-24.3270570352882,-12.3740385950698,
113.535339725245)) ;
#169956 = CARTESIAN_POINT('Ctrl Pts',(-24.3338554351378,-12.446753464716,
113.55604655444)) ;
#169957 = CARTESIAN_POINT('Ctrl Pts',(-24.4076592812388,-12.4467534627922,
113.53181552092)) ;
#169958 = CARTESIAN_POINT('Ctrl Pts',(-24.4814631273398,-12.4467534608683,
113.5075844874)) ;
#169959 = CARTESIAN_POINT('Ctrl Pts',(-24.4746647274902,-12.374038591222,
113.486877658205)) ;
#169960 = CARTESIAN_POINT('Ctrl Pts',(-24.4678663276405,-12.3013237215758,
113.46617082901)) ;
#169961 = CARTESIAN_POINT('Ctrl Pts',(-24.3940624815395,-12.3013237234996,
113.49040186253)) ;
#169962 = CARTESIAN_POINT('Ctrl Pts',(-24.3202586354385,-12.3013237254235,
113.51463289605)) ;
#169963 = CARTESIAN_POINT('Ctrl Pts',(-24.3270570352882,-12.3740385950698,
113.535339725245)) ;
#169964 = CARTESIAN_POINT('Ctrl Pts',(-24.4275571229869,-12.3302346237977,
113.80591117555)) ;
#169965 = CARTESIAN_POINT('Ctrl Pts',(-24.4280835159596,-12.406117742521,
113.807514483671)) ;
#169966 = CARTESIAN_POINT('Ctrl Pts',(-24.5018873603174,-12.4061177428899,
113.783283444841)) ;
#169967 = CARTESIAN_POINT('Ctrl Pts',(-24.5756912046753,-12.4061177432587,
113.759052406012)) ;
#169968 = CARTESIAN_POINT('Ctrl Pts',(-24.5751648117025,-12.3302346245354,
113.757449097891)) ;
#169969 = CARTESIAN_POINT('Ctrl Pts',(-24.5746384187298,-12.2543515058121,
113.755845789771)) ;
#169970 = CARTESIAN_POINT('Ctrl Pts',(-24.5008345743719,-12.2543515054432,
113.7800768286)) ;
#169971 = CARTESIAN_POINT('Ctrl Pts',(-24.4270307300141,-12.2543515050743,
113.80430786743)) ;
#169972 = CARTESIAN_POINT('Ctrl Pts',(-24.4275571229869,-12.3302346237977,
113.80591117555)) ;
#169973 = CARTESIAN_POINT('Ctrl Pts',(-24.5279557593141,-12.3639942142519,
114.076366355261)) ;
#169974 = CARTESIAN_POINT('Ctrl Pts',(-24.5222038772141,-12.4376333996041,
114.058847050435)) ;
#169975 = CARTESIAN_POINT('Ctrl Pts',(-24.5960077204063,-12.4376333997196,
114.034616008055)) ;
#169976 = CARTESIAN_POINT('Ctrl Pts',(-24.6698115635986,-12.4376333998351,
114.010384965676)) ;
#169977 = CARTESIAN_POINT('Ctrl Pts',(-24.6755634456986,-12.3639942144829,
114.027904270502)) ;
#169978 = CARTESIAN_POINT('Ctrl Pts',(-24.6813153277986,-12.2903550291307,
114.045423575328)) ;
#169979 = CARTESIAN_POINT('Ctrl Pts',(-24.6075114846064,-12.2903550290152,
114.069654617708)) ;
#169980 = CARTESIAN_POINT('Ctrl Pts',(-24.5337076414141,-12.2903550288997,
114.093885660087)) ;
#169981 = CARTESIAN_POINT('Ctrl Pts',(-24.5279557593141,-12.3639942142519,
114.076366355261)) ;
#169982 = CARTESIAN_POINT('Ctrl Pts',(-24.6232350266706,-12.4744699305646,
114.330862780655)) ;
#169983 = CARTESIAN_POINT('Ctrl Pts',(-24.6115600779504,-12.5405049323792,
114.295302770537)) ;
#169984 = CARTESIAN_POINT('Ctrl Pts',(-24.6853639204602,-12.5405049308727,
114.271071726079)) ;
#169985 = CARTESIAN_POINT('Ctrl Pts',(-24.7591677629699,-12.5405049293662,
114.24684068162)) ;
#169986 = CARTESIAN_POINT('Ctrl Pts',(-24.7708427116901,-12.4744699275516,
114.282400691739)) ;
#169987 = CARTESIAN_POINT('Ctrl Pts',(-24.7825176604102,-12.408434925737,
114.317960701857)) ;
#169988 = CARTESIAN_POINT('Ctrl Pts',(-24.7087138179005,-12.4084349272435,
114.342191746315)) ;
#169989 = CARTESIAN_POINT('Ctrl Pts',(-24.6349099753908,-12.40843492875,114.366422790774)) ;
#169990 = CARTESIAN_POINT('Ctrl Pts',(-24.6232350266706,-12.4744699305646,
114.330862780655)) ;
#169991 = CARTESIAN_POINT('Ctrl Pts',(-24.7051121876909,-12.6502203530517,
114.545089149363)) ;
#169992 = CARTESIAN_POINT('Ctrl Pts',(-24.6884304701762,-12.7040802804882,
114.494279329336)) ;
#169993 = CARTESIAN_POINT('Ctrl Pts',(-24.7622343128994,-12.7040802781189,
114.470048285528)) ;
#169994 = CARTESIAN_POINT('Ctrl Pts',(-24.8360381556225,-12.7040802757496,
114.44581724172)) ;
#169995 = CARTESIAN_POINT('Ctrl Pts',(-24.8527198731372,-12.6502203483131,
114.496627061747)) ;
#169996 = CARTESIAN_POINT('Ctrl Pts',(-24.8694015906519,-12.5963604208767,
114.547436881774)) ;
#169997 = CARTESIAN_POINT('Ctrl Pts',(-24.7955977479287,-12.596360423246,
114.571667925582)) ;
#169998 = CARTESIAN_POINT('Ctrl Pts',(-24.7217939052056,-12.5963604256153,
114.59589896939)) ;
#169999 = CARTESIAN_POINT('Ctrl Pts',(-24.7051121876909,-12.6502203530517,
114.545089149363)) ;
#170000 = CARTESIAN_POINT('Ctrl Pts',(-24.7708093325559,-12.8831101738135,
114.709574205269)) ;
#170001 = CARTESIAN_POINT('Ctrl Pts',(-24.7502524566444,-12.9207872316337,
114.64696127806)) ;
#170002 = CARTESIAN_POINT('Ctrl Pts',(-24.8240562999475,-12.9207872305233,
114.622730236018)) ;
#170003 = CARTESIAN_POINT('Ctrl Pts',(-24.8978601432505,-12.9207872294128,
114.598499193976)) ;
#170004 = CARTESIAN_POINT('Ctrl Pts',(-24.9184170191621,-12.8831101715926,
114.661112121185)) ;
#170005 = CARTESIAN_POINT('Ctrl Pts',(-24.9389738950736,-12.8454331137723,
114.723725048394)) ;
#170006 = CARTESIAN_POINT('Ctrl Pts',(-24.8651700517706,-12.8454331148828,
114.747956090436)) ;
#170007 = CARTESIAN_POINT('Ctrl Pts',(-24.7913662084675,-12.8454331159932,
114.772187132478)) ;
#170008 = CARTESIAN_POINT('Ctrl Pts',(-24.7708093325559,-12.8831101738135,
114.709574205269)) ;
#170009 = CARTESIAN_POINT('Ctrl Pts',(-24.8149023489856,-13.1530763913863,
114.808480864834)) ;
#170010 = CARTESIAN_POINT('Ctrl Pts',(-24.7919690280488,-13.1719578711027,
114.738629669587)) ;
#170011 = CARTESIAN_POINT('Ctrl Pts',(-24.865772871781,-13.1719578734333,
114.714398628852)) ;
#170012 = CARTESIAN_POINT('Ctrl Pts',(-24.9395767155132,-13.1719578757638,
114.690167588117)) ;
#170013 = CARTESIAN_POINT('Ctrl Pts',(-24.96251003645,-13.1530763960474,114.760018783364)) ;
#170014 = CARTESIAN_POINT('Ctrl Pts',(-24.9854433573868,-13.134194916331,
114.829869978612)) ;
#170015 = CARTESIAN_POINT('Ctrl Pts',(-24.9116395136546,-13.1341949140004,
114.854101019347)) ;
#170016 = CARTESIAN_POINT('Ctrl Pts',(-24.8378356699223,-13.1341949116699,
114.878332060081)) ;
#170017 = CARTESIAN_POINT('Ctrl Pts',(-24.8149023489856,-13.1530763913863,
114.808480864834)) ;
#170018 = CARTESIAN_POINT('Ctrl Pts',(-24.8355728558331,-13.4431032907692,
114.835890910938)) ;
#170019 = CARTESIAN_POINT('Ctrl Pts',(-24.8118983223279,-13.4417610754161,
114.763782101914)) ;
#170020 = CARTESIAN_POINT('Ctrl Pts',(-24.8857021658435,-13.4417610837383,
114.73955106052)) ;
#170021 = CARTESIAN_POINT('Ctrl Pts',(-24.9595060093591,-13.4417610920606,
114.715320019125)) ;
#170022 = CARTESIAN_POINT('Ctrl Pts',(-24.9831805428643,-13.4431033074138,
114.787428828149)) ;
#170023 = CARTESIAN_POINT('Ctrl Pts',(-25.0068550763695,-13.4444455227669,
114.859537637173)) ;
#170024 = CARTESIAN_POINT('Ctrl Pts',(-24.9330512328539,-13.4444455144446,
114.883768678568)) ;
#170025 = CARTESIAN_POINT('Ctrl Pts',(-24.8592473893383,-13.4444455061224,
114.907999719962)) ;
#170026 = CARTESIAN_POINT('Ctrl Pts',(-24.8355728558331,-13.4431032907692,
114.835890910938)) ;
#170027 = CARTESIAN_POINT('Ctrl Pts',(-24.8318678122467,-13.7301505723016,
114.789212778357)) ;
#170028 = CARTESIAN_POINT('Ctrl Pts',(-24.8091500394405,-13.7087638139034,
114.720018108166)) ;
#170029 = CARTESIAN_POINT('Ctrl Pts',(-24.8829538817403,-13.7087638278677,
114.695787063069)) ;
#170030 = CARTESIAN_POINT('Ctrl Pts',(-24.9567577240401,-13.7087638418319,
114.671556017971)) ;
#170031 = CARTESIAN_POINT('Ctrl Pts',(-24.9794754968464,-13.7301506002301,
114.740750688162)) ;
#170032 = CARTESIAN_POINT('Ctrl Pts',(-25.0021932696526,-13.7515373586284,
114.809945358352)) ;
#170033 = CARTESIAN_POINT('Ctrl Pts',(-24.9283894273528,-13.7515373446641,
114.83417640345)) ;
#170034 = CARTESIAN_POINT('Ctrl Pts',(-24.854585585053,-13.7515373306999,
114.858407448548)) ;
#170035 = CARTESIAN_POINT('Ctrl Pts',(-24.8318678122467,-13.7301505723016,
114.789212778357)) ;
#170036 = CARTESIAN_POINT('Ctrl Pts',(-24.8049151957928,-13.9953629945928,
114.671655667574)) ;
#170037 = CARTESIAN_POINT('Ctrl Pts',(-24.7847802406744,-13.9554274129798,
114.610327843468)) ;
#170038 = CARTESIAN_POINT('Ctrl Pts',(-24.8585840806476,-13.9554274317702,
114.586096791283)) ;
#170039 = CARTESIAN_POINT('Ctrl Pts',(-24.9323879206208,-13.9554274505607,
114.561865739099)) ;
#170040 = CARTESIAN_POINT('Ctrl Pts',(-24.9525228757392,-13.9953630321736,
114.623193563205)) ;
#170041 = CARTESIAN_POINT('Ctrl Pts',(-24.9726578308576,-14.0352986137866,
114.684521387312)) ;
#170042 = CARTESIAN_POINT('Ctrl Pts',(-24.8988539908844,-14.0352985949962,
114.708752439496)) ;
#170043 = CARTESIAN_POINT('Ctrl Pts',(-24.8250501509112,-14.0352985762058,
114.732983491681)) ;
#170044 = CARTESIAN_POINT('Ctrl Pts',(-24.8049151957928,-13.9953629945928,
114.671655667574)) ;
#170045 = CARTESIAN_POINT('Ctrl Pts',(-24.7574454109872,-14.2191243988368,
114.491650052615)) ;
#170046 = CARTESIAN_POINT('Ctrl Pts',(-24.7413286926604,-14.1635077763497,
114.442561129583)) ;
#170047 = CARTESIAN_POINT('Ctrl Pts',(-24.8151325294779,-14.1635077969098,
114.418330067787)) ;
#170048 = CARTESIAN_POINT('Ctrl Pts',(-24.8889363662954,-14.16350781747,114.394099005991)) ;
#170049 = CARTESIAN_POINT('Ctrl Pts',(-24.9050530846223,-14.2191244399571,
114.443187929023)) ;
#170050 = CARTESIAN_POINT('Ctrl Pts',(-24.9211698029491,-14.2747410624442,
114.492276852054)) ;
#170051 = CARTESIAN_POINT('Ctrl Pts',(-24.8473659661316,-14.2747410418841,
114.51650791385)) ;
#170052 = CARTESIAN_POINT('Ctrl Pts',(-24.7735621293141,-14.2747410213239,
114.540738975646)) ;
#170053 = CARTESIAN_POINT('Ctrl Pts',(-24.7574454109872,-14.2191243988368,
114.491650052615)) ;
#170054 = CARTESIAN_POINT('Ctrl Pts',(-24.6930620100319,-14.3863702551061,
114.259889607909)) ;
#170055 = CARTESIAN_POINT('Ctrl Pts',(-24.6821550649487,-14.318995498507,
114.226668813785)) ;
#170056 = CARTESIAN_POINT('Ctrl Pts',(-24.7559588974035,-14.3189955173641,
114.202437738701)) ;
#170057 = CARTESIAN_POINT('Ctrl Pts',(-24.8297627298584,-14.3189955362211,
114.178206663618)) ;
#170058 = CARTESIAN_POINT('Ctrl Pts',(-24.8406696749416,-14.3863702928201,
114.211427457741)) ;
#170059 = CARTESIAN_POINT('Ctrl Pts',(-24.8515766200249,-14.4537450494192,
114.244648251865)) ;
#170060 = CARTESIAN_POINT('Ctrl Pts',(-24.77777278757,-14.4537450305621,114.268879326949)) ;
#170061 = CARTESIAN_POINT('Ctrl Pts',(-24.7039689551151,-14.4537450117051,
114.293110402033)) ;
#170062 = CARTESIAN_POINT('Ctrl Pts',(-24.6930620100319,-14.3863702551061,
114.259889607909)) ;
#170063 = CARTESIAN_POINT('Ctrl Pts',(-24.6182341661136,-14.4829184358348,
113.996662475295)) ;
#170064 = CARTESIAN_POINT('Ctrl Pts',(-24.6132666839143,-14.408705819493,
113.981532326927)) ;
#170065 = CARTESIAN_POINT('Ctrl Pts',(-24.6870705129792,-14.4087058298003,
113.957301241518)) ;
#170066 = CARTESIAN_POINT('Ctrl Pts',(-24.7608743420441,-14.4087058401076,
113.933070156109)) ;
#170067 = CARTESIAN_POINT('Ctrl Pts',(-24.7658418242435,-14.4829184564494,
113.948200304477)) ;
#170068 = CARTESIAN_POINT('Ctrl Pts',(-24.7708093064428,-14.5571310727912,
113.963330452846)) ;
#170069 = CARTESIAN_POINT('Ctrl Pts',(-24.6970054773779,-14.5571310624839,
113.987561538255)) ;
#170070 = CARTESIAN_POINT('Ctrl Pts',(-24.623201648313,-14.5571310521766,
114.011792623664)) ;
#170071 = CARTESIAN_POINT('Ctrl Pts',(-24.6182341661136,-14.4829184358348,
113.996662475295)) ;
#170072 = CARTESIAN_POINT('Ctrl Pts',(-24.5380341001339,-14.5038609743369,
113.716865195632)) ;
#170073 = CARTESIAN_POINT('Ctrl Pts',(-24.5393939069206,-14.4280787626501,
113.721006948789)) ;
#170074 = CARTESIAN_POINT('Ctrl Pts',(-24.613197732782,-14.4280787598768,
113.696775853622)) ;
#170075 = CARTESIAN_POINT('Ctrl Pts',(-24.6870015586434,-14.4280787571034,
113.672544758456)) ;
#170076 = CARTESIAN_POINT('Ctrl Pts',(-24.6856417518568,-14.5038609687901,
113.668403005299)) ;
#170077 = CARTESIAN_POINT('Ctrl Pts',(-24.6842819450701,-14.5796431804768,
113.664261252142)) ;
#170078 = CARTESIAN_POINT('Ctrl Pts',(-24.6104781192086,-14.5796431832502,
113.688492347308)) ;
#170079 = CARTESIAN_POINT('Ctrl Pts',(-24.5366742933472,-14.5796431860236,
113.712723442475)) ;
#170080 = CARTESIAN_POINT('Ctrl Pts',(-24.5380341001339,-14.5038609743369,
113.716865195632)) ;
#170081 = CARTESIAN_POINT('Ctrl Pts',(-24.4595898163493,-14.4469649885374,
113.442529411797)) ;
#170082 = CARTESIAN_POINT('Ctrl Pts',(-24.4671610719166,-14.3750457551338,
113.465590235879)) ;
#170083 = CARTESIAN_POINT('Ctrl Pts',(-24.5409648962975,-14.3750457349022,
113.441359136204)) ;
#170084 = CARTESIAN_POINT('Ctrl Pts',(-24.6147687206784,-14.3750457146707,
113.417128036528)) ;
#170085 = CARTESIAN_POINT('Ctrl Pts',(-24.6071974651112,-14.4469649480743,
113.394067212446)) ;
#170086 = CARTESIAN_POINT('Ctrl Pts',(-24.5996262095439,-14.5188841814779,
113.371006388363)) ;
#170087 = CARTESIAN_POINT('Ctrl Pts',(-24.525822385163,-14.5188842017095,
113.395237488039)) ;
#170088 = CARTESIAN_POINT('Ctrl Pts',(-24.452018560782,-14.518884221941,113.419468587715)) ;
#170089 = CARTESIAN_POINT('Ctrl Pts',(-24.4595898163493,-14.4469649885374,
113.442529411797)) ;
#170090 = CARTESIAN_POINT('Ctrl Pts',(-24.3888589686452,-14.3162777489947,
113.191599288438)) ;
#170091 = CARTESIAN_POINT('Ctrl Pts',(-24.4021139128791,-14.2533785894399,
113.231971711301)) ;
#170092 = CARTESIAN_POINT('Ctrl Pts',(-24.4759177374634,-14.2533785490254,
113.207740612244)) ;
#170093 = CARTESIAN_POINT('Ctrl Pts',(-24.5497215620477,-14.253378508611,
113.183509513188)) ;
#170094 = CARTESIAN_POINT('Ctrl Pts',(-24.5364666178138,-14.3162776681657,
113.143137090325)) ;
#170095 = CARTESIAN_POINT('Ctrl Pts',(-24.5232116735799,-14.3791768277205,
113.102764667462)) ;
#170096 = CARTESIAN_POINT('Ctrl Pts',(-24.4494078489956,-14.379176868135,
113.126995766519)) ;
#170097 = CARTESIAN_POINT('Ctrl Pts',(-24.3756040244114,-14.3791769085495,
113.151226865575)) ;
#170098 = CARTESIAN_POINT('Ctrl Pts',(-24.3888589686452,-14.3162777489947,
113.191599288438)) ;
#170099 = CARTESIAN_POINT('Ctrl Pts',(-24.3319214311833,-14.1213118802641,
112.982718459293)) ;
#170100 = CARTESIAN_POINT('Ctrl Pts',(-24.3499044990959,-14.0719335115926,
113.037491984146)) ;
#170101 = CARTESIAN_POINT('Ctrl Pts',(-24.4237083262045,-14.0719334508548,
113.013260892779)) ;
#170102 = CARTESIAN_POINT('Ctrl Pts',(-24.4975121533131,-14.0719333901169,
112.989029801411)) ;
#170103 = CARTESIAN_POINT('Ctrl Pts',(-24.4795290854005,-14.1213117587884,
112.934256276558)) ;
#170104 = CARTESIAN_POINT('Ctrl Pts',(-24.4615460174878,-14.1706901274599,
112.879482751705)) ;
#170105 = CARTESIAN_POINT('Ctrl Pts',(-24.3877421903792,-14.1706901881977,
112.903713843072)) ;
#170106 = CARTESIAN_POINT('Ctrl Pts',(-24.3139383632706,-14.1706902489356,
112.92794493444)) ;
#170107 = CARTESIAN_POINT('Ctrl Pts',(-24.3319214311833,-14.1213118802641,
112.982718459293)) ;
#170108 = CARTESIAN_POINT('Ctrl Pts',(-24.2934703508109,-13.8756723338256,
112.83009751122)) ;
#170109 = CARTESIAN_POINT('Ctrl Pts',(-24.3148987517297,-13.8433718742573,
112.895364964646)) ;
#170110 = CARTESIAN_POINT('Ctrl Pts',(-24.3887025835186,-13.8433717952861,
112.871133887534)) ;
#170111 = CARTESIAN_POINT('Ctrl Pts',(-24.4625064153074,-13.8433717163149,
112.846902810421)) ;
#170112 = CARTESIAN_POINT('Ctrl Pts',(-24.4410780143885,-13.8756721758832,
112.781635356995)) ;
#170113 = CARTESIAN_POINT('Ctrl Pts',(-24.4196496134697,-13.9079726354515,
112.716367903568)) ;
#170114 = CARTESIAN_POINT('Ctrl Pts',(-24.3458457816808,-13.9079727144228,
112.740598980681)) ;
#170115 = CARTESIAN_POINT('Ctrl Pts',(-24.272041949892,-13.907972793394,112.764830057793)) ;
#170116 = CARTESIAN_POINT('Ctrl Pts',(-24.2934703508109,-13.8756723338256,
112.83009751122)) ;
#170117 = CARTESIAN_POINT('Ctrl Pts',(-24.2771743617304,-13.597140902686,
112.744958189465)) ;
#170118 = CARTESIAN_POINT('Ctrl Pts',(-24.3005063726652,-13.584239435371,
112.816023731974)) ;
#170119 = CARTESIAN_POINT('Ctrl Pts',(-24.3743102111448,-13.5842393431877,
112.791792675241)) ;
#170120 = CARTESIAN_POINT('Ctrl Pts',(-24.4481140496243,-13.5842392510044,
112.767561618507)) ;
#170121 = CARTESIAN_POINT('Ctrl Pts',(-24.4247820386894,-13.5971407183194,
112.696496075998)) ;
#170122 = CARTESIAN_POINT('Ctrl Pts',(-24.4014500277545,-13.6100421856345,
112.625430533489)) ;
#170123 = CARTESIAN_POINT('Ctrl Pts',(-24.327646189275,-13.6100422778178,
112.649661590222)) ;
#170124 = CARTESIAN_POINT('Ctrl Pts',(-24.2538423507955,-13.6100423700011,
112.673892646956)) ;
#170125 = CARTESIAN_POINT('Ctrl Pts',(-24.2771743617304,-13.597140902686,
112.744958189465)) ;
#170126 = CARTESIAN_POINT('Ctrl Pts',(-24.2847732062642,-13.3072582096283,
112.732779234924)) ;
#170127 = CARTESIAN_POINT('Ctrl Pts',(-24.3083395158188,-13.3145766205793,
112.804558413309)) ;
#170128 = CARTESIAN_POINT('Ctrl Pts',(-24.3821433622311,-13.3145765231922,
112.780327380737)) ;
#170129 = CARTESIAN_POINT('Ctrl Pts',(-24.4559472086434,-13.3145764258051,
112.756096348166)) ;
#170130 = CARTESIAN_POINT('Ctrl Pts',(-24.4323808990888,-13.3072580148542,
112.684317169781)) ;
#170131 = CARTESIAN_POINT('Ctrl Pts',(-24.4088145895342,-13.2999396039032,
112.612537991397)) ;
#170132 = CARTESIAN_POINT('Ctrl Pts',(-24.335010743122,-13.2999397012903,
112.636769023968)) ;
#170133 = CARTESIAN_POINT('Ctrl Pts',(-24.2612068967096,-13.2999397986774,
112.66100005654)) ;
#170134 = CARTESIAN_POINT('Ctrl Pts',(-24.2847732062642,-13.3072582096283,
112.732779234924)) ;
#170135 = CARTESIAN_POINT('Ctrl Pts',(-24.3165545058404,-13.023884652308,
112.794080029736)) ;
#170136 = CARTESIAN_POINT('Ctrl Pts',(-24.3386710351731,-13.0509977629016,
112.861443411571)) ;
#170137 = CARTESIAN_POINT('Ctrl Pts',(-24.412474890052,-13.0509976674412,
112.837212404788)) ;
#170138 = CARTESIAN_POINT('Ctrl Pts',(-24.486278744931,-13.0509975719808,
112.812981398004)) ;
#170139 = CARTESIAN_POINT('Ctrl Pts',(-24.4641622155983,-13.0238844613873,
112.745618016169)) ;
#170140 = CARTESIAN_POINT('Ctrl Pts',(-24.4420456862657,-12.9967713507938,
112.678254634333)) ;
#170141 = CARTESIAN_POINT('Ctrl Pts',(-24.3682418313867,-12.9967714462542,
112.702485641117)) ;
#170142 = CARTESIAN_POINT('Ctrl Pts',(-24.2944379765078,-12.9967715417145,
112.7267166479)) ;
#170143 = CARTESIAN_POINT('Ctrl Pts',(-24.3165545058404,-13.023884652308,
112.794080029736)) ;
#170144 = CARTESIAN_POINT('Ctrl Pts',(-24.3710194266415,-12.7690113233817,
112.924503192536)) ;
#170145 = CARTESIAN_POINT('Ctrl Pts',(-24.3900997882587,-12.8139584952445,
112.982618897456)) ;
#170146 = CARTESIAN_POINT('Ctrl Pts',(-24.4639036512443,-12.813958410504,
112.958387915364)) ;
#170147 = CARTESIAN_POINT('Ctrl Pts',(-24.5377075142299,-12.8139583257634,
112.934156933272)) ;
#170148 = CARTESIAN_POINT('Ctrl Pts',(-24.5186271526127,-12.7690111539007,
112.876041228353)) ;
#170149 = CARTESIAN_POINT('Ctrl Pts',(-24.4995467909954,-12.7240639820379,
112.817925523433)) ;
#170150 = CARTESIAN_POINT('Ctrl Pts',(-24.4257429280098,-12.7240640667784,
112.842156505525)) ;
#170151 = CARTESIAN_POINT('Ctrl Pts',(-24.3519390650242,-12.724064151519,
112.866387487617)) ;
#170152 = CARTESIAN_POINT('Ctrl Pts',(-24.3710194266415,-12.7690113233817,
112.924503192536)) ;
#170153 = CARTESIAN_POINT('Ctrl Pts',(-24.4450008074729,-12.5606194771078,
113.114364621987)) ;
#170154 = CARTESIAN_POINT('Ctrl Pts',(-24.4596781905624,-12.6201819472302,
113.159069564768)) ;
#170155 = CARTESIAN_POINT('Ctrl Pts',(-24.533482060381,-12.6201818809856,
113.134838603488)) ;
#170156 = CARTESIAN_POINT('Ctrl Pts',(-24.6072859301996,-12.620181814741,
113.110607642208)) ;
#170157 = CARTESIAN_POINT('Ctrl Pts',(-24.5926085471101,-12.5606193446187,
113.065902699427)) ;
#170158 = CARTESIAN_POINT('Ctrl Pts',(-24.5779311640206,-12.5010568744963,
113.021197756646)) ;
#170159 = CARTESIAN_POINT('Ctrl Pts',(-24.504127294202,-12.5010569407409,
113.045428717926)) ;
#170160 = CARTESIAN_POINT('Ctrl Pts',(-24.4303234243834,-12.5010570069855,
113.069659679205)) ;
#170161 = CARTESIAN_POINT('Ctrl Pts',(-24.4450008074729,-12.5606194771078,
113.114364621987)) ;
#170162 = CARTESIAN_POINT('Ctrl Pts',(-24.5338650383482,-12.413760463827,
113.349590588029)) ;
#170163 = CARTESIAN_POINT('Ctrl Pts',(-24.5430932310349,-12.4836640016496,
113.377698176085)) ;
#170164 = CARTESIAN_POINT('Ctrl Pts',(-24.6168971056564,-12.4836639599655,
113.353467229434)) ;
#170165 = CARTESIAN_POINT('Ctrl Pts',(-24.690700980278,-12.4836639182814,
113.329236282783)) ;
#170166 = CARTESIAN_POINT('Ctrl Pts',(-24.6814727875913,-12.4137603804588,
113.301128694728)) ;
#170167 = CARTESIAN_POINT('Ctrl Pts',(-24.6722445949046,-12.3438568426362,
113.273021106673)) ;
#170168 = CARTESIAN_POINT('Ctrl Pts',(-24.5984407202831,-12.3438568843203,
113.297252053324)) ;
#170169 = CARTESIAN_POINT('Ctrl Pts',(-24.5246368456615,-12.3438569260044,
113.321482999974)) ;
#170170 = CARTESIAN_POINT('Ctrl Pts',(-24.5338650383482,-12.413760463827,
113.349590588029)) ;
#170171 = CARTESIAN_POINT('Ctrl Pts',(-24.6321826857904,-12.3386970972896,
113.613568979409)) ;
#170172 = CARTESIAN_POINT('Ctrl Pts',(-24.6352945524771,-12.4139449164538,
113.623047225329)) ;
#170173 = CARTESIAN_POINT('Ctrl Pts',(-24.7090984293634,-12.4139449029389,
113.598816285577)) ;
#170174 = CARTESIAN_POINT('Ctrl Pts',(-24.7829023062498,-12.4139448894239,
113.574585345824)) ;
#170175 = CARTESIAN_POINT('Ctrl Pts',(-24.7797904395631,-12.3386970702597,
113.565107099904)) ;
#170176 = CARTESIAN_POINT('Ctrl Pts',(-24.7766785728765,-12.2634492510955,
113.555628853984)) ;
#170177 = CARTESIAN_POINT('Ctrl Pts',(-24.7028746959902,-12.2634492646105,
113.579859793736)) ;
#170178 = CARTESIAN_POINT('Ctrl Pts',(-24.6290708191038,-12.2634492781254,
113.604090733489)) ;
#170179 = CARTESIAN_POINT('Ctrl Pts',(-24.6321826857904,-12.3386970972896,
113.613568979409)) ;
#170180 = CARTESIAN_POINT('Ctrl Pts',(-24.7334826748307,-12.3409867725706,
113.886661565323)) ;
#170181 = CARTESIAN_POINT('Ctrl Pts',(-24.730260281677,-12.4161865646984,
113.876846677773)) ;
#170182 = CARTESIAN_POINT('Ctrl Pts',(-24.8040641580606,-12.4161865800311,
113.852615736489)) ;
#170183 = CARTESIAN_POINT('Ctrl Pts',(-24.8778680344442,-12.4161865953639,
113.828384795205)) ;
#170184 = CARTESIAN_POINT('Ctrl Pts',(-24.8810904275978,-12.3409868032361,
113.838199682755)) ;
#170185 = CARTESIAN_POINT('Ctrl Pts',(-24.8843128207515,-12.2657870111083,
113.848014570306)) ;
#170186 = CARTESIAN_POINT('Ctrl Pts',(-24.8105089443679,-12.2657869957756,
113.87224551159)) ;
#170187 = CARTESIAN_POINT('Ctrl Pts',(-24.7367050679843,-12.2657869804429,
113.896476452874)) ;
#170188 = CARTESIAN_POINT('Ctrl Pts',(-24.7334826748307,-12.3409867725706,
113.886661565323)) ;
#170189 = CARTESIAN_POINT('Ctrl Pts',(-24.8314366572385,-12.4204578395528,
114.149527864238)) ;
#170190 = CARTESIAN_POINT('Ctrl Pts',(-24.8221048881669,-12.4902214392955,
114.121104803336)) ;
#170191 = CARTESIAN_POINT('Ctrl Pts',(-24.8959087613574,-12.4902214812087,
114.096873852327)) ;
#170192 = CARTESIAN_POINT('Ctrl Pts',(-24.9697126345479,-12.4902215231219,
114.072642901317)) ;
#170193 = CARTESIAN_POINT('Ctrl Pts',(-24.9790444036195,-12.4204579233792,
114.101065962219)) ;
#170194 = CARTESIAN_POINT('Ctrl Pts',(-24.9883761726911,-12.3506943236366,
114.129489023121)) ;
#170195 = CARTESIAN_POINT('Ctrl Pts',(-24.9145722995006,-12.3506942817234,
114.15371997413)) ;
#170196 = CARTESIAN_POINT('Ctrl Pts',(-24.8407684263101,-12.3506942398102,
114.17795092514)) ;
#170197 = CARTESIAN_POINT('Ctrl Pts',(-24.8314366572385,-12.4204578395528,
114.149527864238)) ;
#170198 = CARTESIAN_POINT('Ctrl Pts',(-24.9196367729375,-12.5714299256093,
114.382700587259)) ;
#170199 = CARTESIAN_POINT('Ctrl Pts',(-24.9048671068876,-12.6307574701192,
114.337714569493)) ;
#170200 = CARTESIAN_POINT('Ctrl Pts',(-24.9786709746415,-12.6307575336333,
114.313483601925)) ;
#170201 = CARTESIAN_POINT('Ctrl Pts',(-25.0524748423954,-12.6307575971475,
114.289252634356)) ;
#170202 = CARTESIAN_POINT('Ctrl Pts',(-25.0672445084453,-12.5714300526376,
114.334238652123)) ;
#170203 = CARTESIAN_POINT('Ctrl Pts',(-25.0820141744952,-12.5121025081277,
114.379224669889)) ;
#170204 = CARTESIAN_POINT('Ctrl Pts',(-25.0082103067413,-12.5121024446135,
114.403455637457)) ;
#170205 = CARTESIAN_POINT('Ctrl Pts',(-24.9344064389874,-12.5121023810993,
114.427686605026)) ;
#170206 = CARTESIAN_POINT('Ctrl Pts',(-24.9196367729375,-12.5714299256093,
114.382700587259)) ;
#170207 = CARTESIAN_POINT('Ctrl Pts',(-24.9924945178044,-12.7828129113163,
114.56917762335)) ;
#170208 = CARTESIAN_POINT('Ctrl Pts',(-24.9733491898405,-12.8274711161602,
114.510864045317)) ;
#170209 = CARTESIAN_POINT('Ctrl Pts',(-25.0471530506454,-12.82747119449,114.486633056583)) ;
#170210 = CARTESIAN_POINT('Ctrl Pts',(-25.1209569114504,-12.8274712728199,
114.46240206785)) ;
#170211 = CARTESIAN_POINT('Ctrl Pts',(-25.1401022394143,-12.782813067976,
114.520715645882)) ;
#170212 = CARTESIAN_POINT('Ctrl Pts',(-25.1592475673782,-12.7381548631321,
114.579029223915)) ;
#170213 = CARTESIAN_POINT('Ctrl Pts',(-25.0854437065732,-12.7381547848022,
114.603260212648)) ;
#170214 = CARTESIAN_POINT('Ctrl Pts',(-25.0116398457683,-12.7381547064724,
114.627491201382)) ;
#170215 = CARTESIAN_POINT('Ctrl Pts',(-24.9924945178044,-12.7828129113163,
114.56917762335)) ;
#170216 = CARTESIAN_POINT('Ctrl Pts',(-25.0456977654746,-13.0396896566704,
114.695776913012)) ;
#170217 = CARTESIAN_POINT('Ctrl Pts',(-25.023542631379,-13.0664804040034,
114.628295951028)) ;
#170218 = CARTESIAN_POINT('Ctrl Pts',(-25.0973464844517,-13.0664804892966,
114.604064938743)) ;
#170219 = CARTESIAN_POINT('Ctrl Pts',(-25.1711503375243,-13.0664805745898,
114.579833926458)) ;
#170220 = CARTESIAN_POINT('Ctrl Pts',(-25.1933054716199,-13.0396898272568,
114.647314888442)) ;
#170221 = CARTESIAN_POINT('Ctrl Pts',(-25.2154606057155,-13.0128990799238,
114.714795850425)) ;
#170222 = CARTESIAN_POINT('Ctrl Pts',(-25.1416567526428,-13.0128989946306,
114.739026862711)) ;
#170223 = CARTESIAN_POINT('Ctrl Pts',(-25.0678528995702,-13.0128989093375,
114.763257874996)) ;
#170224 = CARTESIAN_POINT('Ctrl Pts',(-25.0456977654746,-13.0396896566704,
114.695776913012)) ;
#170225 = CARTESIAN_POINT('Ctrl Pts',(-25.0761544983611,-13.3246405733811,
114.752976375053)) ;
#170226 = CARTESIAN_POINT('Ctrl Pts',(-25.0525753762368,-13.3315770270648,
114.681158175154)) ;
#170227 = CARTESIAN_POINT('Ctrl Pts',(-25.1263792216785,-13.331577110356,
114.656927139626)) ;
#170228 = CARTESIAN_POINT('Ctrl Pts',(-25.2001830671202,-13.3315771936471,
114.632696104099)) ;
#170229 = CARTESIAN_POINT('Ctrl Pts',(-25.2237621892446,-13.3246407399634,
114.704514303997)) ;
#170230 = CARTESIAN_POINT('Ctrl Pts',(-25.2473413113689,-13.3177042862798,
114.776332503896)) ;
#170231 = CARTESIAN_POINT('Ctrl Pts',(-25.1735374659272,-13.3177042029886,
114.800563539424)) ;
#170232 = CARTESIAN_POINT('Ctrl Pts',(-25.0997336204854,-13.3177041196975,
114.824794574952)) ;
#170233 = CARTESIAN_POINT('Ctrl Pts',(-25.0761544983611,-13.3246405733811,
114.752976375053)) ;
#170234 = CARTESIAN_POINT('Ctrl Pts',(-25.0822716580922,-13.6149949699245,
114.736205333748)) ;
#170235 = CARTESIAN_POINT('Ctrl Pts',(-25.0589624399057,-13.6016695488901,
114.665209217564)) ;
#170236 = CARTESIAN_POINT('Ctrl Pts',(-25.1327662787753,-13.6016696242958,
114.640978162019)) ;
#170237 = CARTESIAN_POINT('Ctrl Pts',(-25.2065701176448,-13.6016696997014,
114.616747106473)) ;
#170238 = CARTESIAN_POINT('Ctrl Pts',(-25.2298793358313,-13.6149951207358,
114.687743222656)) ;
#170239 = CARTESIAN_POINT('Ctrl Pts',(-25.2531885540178,-13.6283205417703,
114.758739338839)) ;
#170240 = CARTESIAN_POINT('Ctrl Pts',(-25.1793847151483,-13.6283204663646,
114.782970394385)) ;
#170241 = CARTESIAN_POINT('Ctrl Pts',(-25.1055808762787,-13.6283203909589,
114.807201449931)) ;
#170242 = CARTESIAN_POINT('Ctrl Pts',(-25.0822716580922,-13.6149949699245,
114.736205333748)) ;
#170243 = CARTESIAN_POINT('Ctrl Pts',(-25.06454635551,-13.8916396903177,114.646761857288)) ;
#170244 = CARTESIAN_POINT('Ctrl Pts',(-25.043173102537,-13.8589788645426,
114.58166237863)) ;
#170245 = CARTESIAN_POINT('Ctrl Pts',(-25.1169769363613,-13.8589789264578,
114.557431307717)) ;
#170246 = CARTESIAN_POINT('Ctrl Pts',(-25.1907807701857,-13.858978988373,
114.533200236805)) ;
#170247 = CARTESIAN_POINT('Ctrl Pts',(-25.2121540231587,-13.891639814148,
114.598299715463)) ;
#170248 = CARTESIAN_POINT('Ctrl Pts',(-25.2335272761317,-13.9243006399231,
114.663399194122)) ;
#170249 = CARTESIAN_POINT('Ctrl Pts',(-25.1597234423074,-13.9243005780079,
114.687630265035)) ;
#170250 = CARTESIAN_POINT('Ctrl Pts',(-25.085919608483,-13.9243005160927,
114.711861335947)) ;
#170251 = CARTESIAN_POINT('Ctrl Pts',(-25.06454635551,-13.8916396903177,114.646761857288)) ;
#170252 = CARTESIAN_POINT('Ctrl Pts',(-25.0249777077505,-14.1343825887975,
114.490801908801)) ;
#170253 = CARTESIAN_POINT('Ctrl Pts',(-25.0070681267458,-14.0847239411806,
114.436252215942)) ;
#170254 = CARTESIAN_POINT('Ctrl Pts',(-25.0808719574157,-14.0847239865753,
114.412021135421)) ;
#170255 = CARTESIAN_POINT('Ctrl Pts',(-25.1546757880855,-14.0847240319701,
114.387790054901)) ;
#170256 = CARTESIAN_POINT('Ctrl Pts',(-25.1725853690902,-14.134382679587,
114.44233974776)) ;
#170257 = CARTESIAN_POINT('Ctrl Pts',(-25.1904949500949,-14.1840413272039,
114.49688944062)) ;
#170258 = CARTESIAN_POINT('Ctrl Pts',(-25.116691119425,-14.1840412818091,
114.521120521141)) ;
#170259 = CARTESIAN_POINT('Ctrl Pts',(-25.0428872887551,-14.1840412364144,
114.545351601661)) ;
#170260 = CARTESIAN_POINT('Ctrl Pts',(-25.0249777077505,-14.1343825887975,
114.490801908801)) ;
#170261 = CARTESIAN_POINT('Ctrl Pts',(-24.9668445289914,-14.3263844089833,
114.278154012734)) ;
#170262 = CARTESIAN_POINT('Ctrl Pts',(-24.9537029589574,-14.2632443878997,
114.238126911786)) ;
#170263 = CARTESIAN_POINT('Ctrl Pts',(-25.0275067888665,-14.263244415508,
114.213895828948)) ;
#170264 = CARTESIAN_POINT('Ctrl Pts',(-25.1013106187757,-14.2632444431164,
114.189664746111)) ;
#170265 = CARTESIAN_POINT('Ctrl Pts',(-25.1144521888096,-14.3263844642,114.229691847058)) ;
#170266 = CARTESIAN_POINT('Ctrl Pts',(-25.1275937588436,-14.3895244852836,
114.269718948005)) ;
#170267 = CARTESIAN_POINT('Ctrl Pts',(-25.0537899289344,-14.3895244576753,
114.293950030843)) ;
#170268 = CARTESIAN_POINT('Ctrl Pts',(-24.9799860990254,-14.3895244300669,
114.318181113681)) ;
#170269 = CARTESIAN_POINT('Ctrl Pts',(-24.9668445289914,-14.3263844089833,
114.278154012734)) ;
#170270 = CARTESIAN_POINT('Ctrl Pts',(-24.8957621143126,-14.4524065463604,
114.026303661662)) ;
#170271 = CARTESIAN_POINT('Ctrl Pts',(-24.8882951456828,-14.3803719566858,
114.003560480852)) ;
#170272 = CARTESIAN_POINT('Ctrl Pts',(-24.9620989760419,-14.3803719694669,
113.979329399385)) ;
#170273 = CARTESIAN_POINT('Ctrl Pts',(-25.035902806401,-14.3803719822481,
113.955098317918)) ;
#170274 = CARTESIAN_POINT('Ctrl Pts',(-25.0433697750307,-14.4524065719227,
113.977841498727)) ;
#170275 = CARTESIAN_POINT('Ctrl Pts',(-25.0508367436604,-14.5244411615974,
114.000584679537)) ;
#170276 = CARTESIAN_POINT('Ctrl Pts',(-24.9770329133014,-14.5244411488162,
114.024815761004)) ;
#170277 = CARTESIAN_POINT('Ctrl Pts',(-24.9032290829423,-14.5244411360351,
114.049046842471)) ;
#170278 = CARTESIAN_POINT('Ctrl Pts',(-24.8957621143126,-14.4524065463604,
114.026303661662)) ;
#170279 = CARTESIAN_POINT('Ctrl Pts',(-24.8165686904461,-14.5048820459499,
113.749467211737)) ;
#170280 = CARTESIAN_POINT('Ctrl Pts',(-24.8153570946285,-14.4290737092712,
113.745776887015)) ;
#170281 = CARTESIAN_POINT('Ctrl Pts',(-24.8891609275668,-14.4290737099999,
113.721545813404)) ;
#170282 = CARTESIAN_POINT('Ctrl Pts',(-24.9629647605052,-14.4290737107285,
113.697314739792)) ;
#170283 = CARTESIAN_POINT('Ctrl Pts',(-24.9641763563227,-14.5048820474072,
113.701005064514)) ;
#170284 = CARTESIAN_POINT('Ctrl Pts',(-24.9653879521404,-14.5806903840858,
113.704695389236)) ;
#170285 = CARTESIAN_POINT('Ctrl Pts',(-24.891584119202,-14.5806903833572,
113.728926462847)) ;
#170286 = CARTESIAN_POINT('Ctrl Pts',(-24.8177802862637,-14.5806903826285,
113.753157536459)) ;
#170287 = CARTESIAN_POINT('Ctrl Pts',(-24.8165686904461,-14.5048820459499,
113.749467211737)) ;
#170288 = CARTESIAN_POINT('Ctrl Pts',(-24.7369131556287,-14.4792643387988,
113.471526923201)) ;
#170289 = CARTESIAN_POINT('Ctrl Pts',(-24.7419924769914,-14.4051302441696,
113.48699771704)) ;
#170290 = CARTESIAN_POINT('Ctrl Pts',(-24.8157963123699,-14.4051302376983,
113.462766650861)) ;
#170291 = CARTESIAN_POINT('Ctrl Pts',(-24.8896001477485,-14.405130231227,
113.438535584683)) ;
#170292 = CARTESIAN_POINT('Ctrl Pts',(-24.8845208263858,-14.4792643258562,
113.423064790844)) ;
#170293 = CARTESIAN_POINT('Ctrl Pts',(-24.8794415050231,-14.5533984204853,
113.407593997005)) ;
#170294 = CARTESIAN_POINT('Ctrl Pts',(-24.8056376696446,-14.5533984269566,
113.431825063184)) ;
#170295 = CARTESIAN_POINT('Ctrl Pts',(-24.731833834266,-14.5533984334279,
113.456056129363)) ;
#170296 = CARTESIAN_POINT('Ctrl Pts',(-24.7369131556287,-14.4792643387988,
113.471526923201)) ;
#170297 = CARTESIAN_POINT('Ctrl Pts',(-24.6622449881226,-14.3777623982077,
113.208611229877)) ;
#170298 = CARTESIAN_POINT('Ctrl Pts',(-24.6732800440833,-14.3106033154662,
113.242222230191)) ;
#170299 = CARTESIAN_POINT('Ctrl Pts',(-24.7470838825016,-14.3106033061414,
113.217991173271)) ;
#170300 = CARTESIAN_POINT('Ctrl Pts',(-24.8208877209198,-14.3106032968165,
113.193760116351)) ;
#170301 = CARTESIAN_POINT('Ctrl Pts',(-24.8098526649591,-14.377762379558,
113.160149116037)) ;
#170302 = CARTESIAN_POINT('Ctrl Pts',(-24.7988176089984,-14.4449214622994,
113.126538115723)) ;
#170303 = CARTESIAN_POINT('Ctrl Pts',(-24.7250137705801,-14.4449214716243,
113.150769172643)) ;
#170304 = CARTESIAN_POINT('Ctrl Pts',(-24.6512099321618,-14.4449214809491,
113.175000229563)) ;
#170305 = CARTESIAN_POINT('Ctrl Pts',(-24.6622449881226,-14.3777623982077,
113.208611229877)) ;
#170306 = CARTESIAN_POINT('Ctrl Pts',(-24.59913585455,-14.2077004202751,112.980968522228)) ;
#170307 = CARTESIAN_POINT('Ctrl Pts',(-24.6153271901671,-14.1523145589373,
113.030284718282)) ;
#170308 = CARTESIAN_POINT('Ctrl Pts',(-24.6891310310512,-14.1523145504394,
113.006053668872)) ;
#170309 = CARTESIAN_POINT('Ctrl Pts',(-24.7629348719354,-14.1523145419415,
112.981822619462)) ;
#170310 = CARTESIAN_POINT('Ctrl Pts',(-24.7467435363182,-14.2077004032793,
112.932506423408)) ;
#170311 = CARTESIAN_POINT('Ctrl Pts',(-24.7305522007011,-14.2630862646171,
112.883190227354)) ;
#170312 = CARTESIAN_POINT('Ctrl Pts',(-24.656748359817,-14.2630862731151,
112.907421276764)) ;
#170313 = CARTESIAN_POINT('Ctrl Pts',(-24.5829445189329,-14.263086281613,
112.931652326173)) ;
#170314 = CARTESIAN_POINT('Ctrl Pts',(-24.59913585455,-14.2077004202751,112.980968522228)) ;
#170315 = CARTESIAN_POINT('Ctrl Pts',(-24.5525713605202,-13.980362420234,
112.803591412359)) ;
#170316 = CARTESIAN_POINT('Ctrl Pts',(-24.5727742599949,-13.9407671671798,
112.865126184531)) ;
#170317 = CARTESIAN_POINT('Ctrl Pts',(-24.6465781027262,-13.9407671625387,
112.840895140748)) ;
#170318 = CARTESIAN_POINT('Ctrl Pts',(-24.7203819454574,-13.9407671578977,
112.816664096964)) ;
#170319 = CARTESIAN_POINT('Ctrl Pts',(-24.7001790459827,-13.980362410952,
112.755129324791)) ;
#170320 = CARTESIAN_POINT('Ctrl Pts',(-24.679976146508,-14.0199576640062,
112.693594552618)) ;
#170321 = CARTESIAN_POINT('Ctrl Pts',(-24.6061723037767,-14.0199576686472,
112.717825596402)) ;
#170322 = CARTESIAN_POINT('Ctrl Pts',(-24.5323684610455,-14.0199576732883,
112.742056640186)) ;
#170323 = CARTESIAN_POINT('Ctrl Pts',(-24.5525713605202,-13.980362420234,
112.803591412359)) ;
#170324 = CARTESIAN_POINT('Ctrl Pts',(-24.5269666018519,-13.7128487430244,
112.690103143311)) ;
#170325 = CARTESIAN_POINT('Ctrl Pts',(-24.5497224381023,-13.6918738812675,
112.759413748897)) ;
#170326 = CARTESIAN_POINT('Ctrl Pts',(-24.6235262815752,-13.6918738808366,
112.735182707372)) ;
#170327 = CARTESIAN_POINT('Ctrl Pts',(-24.697330125048,-13.6918738804057,
112.710951665847)) ;
#170328 = CARTESIAN_POINT('Ctrl Pts',(-24.6745742887976,-13.7128487421626,
112.641641060262)) ;
#170329 = CARTESIAN_POINT('Ctrl Pts',(-24.6518184525471,-13.7338236039195,
112.572330454676)) ;
#170330 = CARTESIAN_POINT('Ctrl Pts',(-24.5780146090743,-13.7338236043504,
112.596561496201)) ;
#170331 = CARTESIAN_POINT('Ctrl Pts',(-24.5042107656014,-13.7338236047813,
112.620792537726)) ;
#170332 = CARTESIAN_POINT('Ctrl Pts',(-24.5269666018519,-13.7128487430244,
112.690103143311)) ;
#170333 = CARTESIAN_POINT('Ctrl Pts',(-24.5248000668453,-13.4250762896625,
112.648103876864)) ;
#170334 = CARTESIAN_POINT('Ctrl Pts',(-24.5484737092852,-13.4241646281582,
112.720209971964)) ;
#170335 = CARTESIAN_POINT('Ctrl Pts',(-24.6222775527583,-13.424164630414,
112.69597893044)) ;
#170336 = CARTESIAN_POINT('Ctrl Pts',(-24.6960813962314,-13.4241646326699,
112.671747888916)) ;
#170337 = CARTESIAN_POINT('Ctrl Pts',(-24.6724077537915,-13.4250762941742,
112.599641793815)) ;
#170338 = CARTESIAN_POINT('Ctrl Pts',(-24.6487341113515,-13.4259879556785,
112.527535698715)) ;
#170339 = CARTESIAN_POINT('Ctrl Pts',(-24.5749302678784,-13.4259879534226,
112.551766740239)) ;
#170340 = CARTESIAN_POINT('Ctrl Pts',(-24.5011264244053,-13.4259879511667,
112.575997781763)) ;
#170341 = CARTESIAN_POINT('Ctrl Pts',(-24.5248000668453,-13.4250762896625,
112.648103876864)) ;
#170342 = CARTESIAN_POINT('Ctrl Pts',(-24.5467181523936,-13.1369898154444,
112.679497598363)) ;
#170343 = CARTESIAN_POINT('Ctrl Pts',(-24.5696282907065,-13.1561933535751,
112.749278183058)) ;
#170344 = CARTESIAN_POINT('Ctrl Pts',(-24.6434321338206,-13.1561933570076,
112.725047140441)) ;
#170345 = CARTESIAN_POINT('Ctrl Pts',(-24.7172359769348,-13.15619336044,112.700816097823)) ;
#170346 = CARTESIAN_POINT('Ctrl Pts',(-24.6943258386219,-13.1369898223093,
112.631035513128)) ;
#170347 = CARTESIAN_POINT('Ctrl Pts',(-24.6714157003091,-13.1177862841786,
112.561254928433)) ;
#170348 = CARTESIAN_POINT('Ctrl Pts',(-24.597611857195,-13.1177862807461,
112.585485971051)) ;
#170349 = CARTESIAN_POINT('Ctrl Pts',(-24.5238080140808,-13.1177862773137,
112.609717013668)) ;
#170350 = CARTESIAN_POINT('Ctrl Pts',(-24.5467181523936,-13.1369898154444,
112.679497598363)) ;
#170351 = CARTESIAN_POINT('Ctrl Pts',(-24.5926693672663,-12.8663855366991,
112.783721838426)) ;
#170352 = CARTESIAN_POINT('Ctrl Pts',(-24.6131442990518,-12.9045144387046,
112.846085176993)) ;
#170353 = CARTESIAN_POINT('Ctrl Pts',(-24.6869481421206,-12.9045144401406,
112.821854134237)) ;
#170354 = CARTESIAN_POINT('Ctrl Pts',(-24.7607519851895,-12.9045144415766,
112.797623091482)) ;
#170355 = CARTESIAN_POINT('Ctrl Pts',(-24.7402770534039,-12.8663855395711,
112.735259752915)) ;
#170356 = CARTESIAN_POINT('Ctrl Pts',(-24.7198021216184,-12.8282566375656,
112.672896414349)) ;
#170357 = CARTESIAN_POINT('Ctrl Pts',(-24.6459982785496,-12.8282566361296,
112.697127457104)) ;
#170358 = CARTESIAN_POINT('Ctrl Pts',(-24.5721944354807,-12.8282566346936,
112.72135849986)) ;
#170359 = CARTESIAN_POINT('Ctrl Pts',(-24.5926693672663,-12.8663855366991,
112.783721838426)) ;
#170360 = CARTESIAN_POINT('Ctrl Pts',(-24.6589432293647,-12.6384940512534,
112.950297607118)) ;
#170361 = CARTESIAN_POINT('Ctrl Pts',(-24.6755506105844,-12.6925911695923,
113.000881010742)) ;
#170362 = CARTESIAN_POINT('Ctrl Pts',(-24.7493544541457,-12.6925911686239,
112.976649969486)) ;
#170363 = CARTESIAN_POINT('Ctrl Pts',(-24.823158297707,-12.6925911676555,
112.952418928231)) ;
#170364 = CARTESIAN_POINT('Ctrl Pts',(-24.8065509164873,-12.6384940493165,
112.901835524607)) ;
#170365 = CARTESIAN_POINT('Ctrl Pts',(-24.7899435352676,-12.5843969309776,
112.851252120983)) ;
#170366 = CARTESIAN_POINT('Ctrl Pts',(-24.7161396917063,-12.584396931946,
112.875483162238)) ;
#170367 = CARTESIAN_POINT('Ctrl Pts',(-24.642335848145,-12.5843969329144,
112.899714203494)) ;
#170368 = CARTESIAN_POINT('Ctrl Pts',(-24.6589432293647,-12.6384940512534,
112.950297607118)) ;
#170369 = CARTESIAN_POINT('Ctrl Pts',(-24.7426000968426,-12.4647340958094,
113.169559327226)) ;
#170370 = CARTESIAN_POINT('Ctrl Pts',(-24.7541259248004,-12.5310434351584,
113.20466513962)) ;
#170371 = CARTESIAN_POINT('Ctrl Pts',(-24.8279297698228,-12.5310434317377,
113.180434102815)) ;
#170372 = CARTESIAN_POINT('Ctrl Pts',(-24.9017336148452,-12.5310434283171,
113.156203066009)) ;
#170373 = CARTESIAN_POINT('Ctrl Pts',(-24.8902077868874,-12.4647340889681,
113.121097253616)) ;
#170374 = CARTESIAN_POINT('Ctrl Pts',(-24.8786819589297,-12.3984247496191,
113.085991441223)) ;
#170375 = CARTESIAN_POINT('Ctrl Pts',(-24.8048781139073,-12.3984247530398,
113.110222478028)) ;
#170376 = CARTESIAN_POINT('Ctrl Pts',(-24.7310742688849,-12.3984247564605,
113.134453514833)) ;
#170377 = CARTESIAN_POINT('Ctrl Pts',(-24.7426000968426,-12.4647340958094,
113.169559327226)) ;
#170378 = CARTESIAN_POINT('Ctrl Pts',(-24.8376583123465,-12.3600064377204,
113.423696409434)) ;
#170379 = CARTESIAN_POINT('Ctrl Pts',(-24.8432960062769,-12.4337245690079,
113.440867915738)) ;
#170380 = CARTESIAN_POINT('Ctrl Pts',(-24.917099853265,-12.4337245657129,
113.41663688492)) ;
#170381 = CARTESIAN_POINT('Ctrl Pts',(-24.9909037002531,-12.4337245624179,
113.392405854102)) ;
#170382 = CARTESIAN_POINT('Ctrl Pts',(-24.9852660063225,-12.3600064311304,
113.375234347797)) ;
#170383 = CARTESIAN_POINT('Ctrl Pts',(-24.979628312392,-12.286288299843,113.358062841493)) ;
#170384 = CARTESIAN_POINT('Ctrl Pts',(-24.905824465404,-12.286288303138,113.382293872311)) ;
#170385 = CARTESIAN_POINT('Ctrl Pts',(-24.8320206184159,-12.286288306433,
113.406524903129)) ;
#170386 = CARTESIAN_POINT('Ctrl Pts',(-24.8376583123465,-12.3600064377204,
113.423696409434)) ;
#170387 = CARTESIAN_POINT('Ctrl Pts',(-24.9384569987699,-12.3305764766961,
113.695274669522)) ;
#170388 = CARTESIAN_POINT('Ctrl Pts',(-24.9377981669915,-12.4064564353267,
113.69326797459)) ;
#170389 = CARTESIAN_POINT('Ctrl Pts',(-25.0116020162607,-12.4064564352426,
113.66903695072)) ;
#170390 = CARTESIAN_POINT('Ctrl Pts',(-25.08540586553,-12.4064564351584,113.64480592685)) ;
#170391 = CARTESIAN_POINT('Ctrl Pts',(-25.0860646973084,-12.3305764765278,
113.646812621782)) ;
#170392 = CARTESIAN_POINT('Ctrl Pts',(-25.0867235290868,-12.2546965178971,
113.648819316715)) ;
#170393 = CARTESIAN_POINT('Ctrl Pts',(-25.0129196798176,-12.2546965179813,
113.673050340585)) ;
#170394 = CARTESIAN_POINT('Ctrl Pts',(-24.9391158305484,-12.2546965180655,
113.697281364455)) ;
#170395 = CARTESIAN_POINT('Ctrl Pts',(-24.9384569987699,-12.3305764766961,
113.695274669522)) ;
#170396 = CARTESIAN_POINT('Ctrl Pts',(-25.0387364603478,-12.3793274592069,
113.965169521633)) ;
#170397 = CARTESIAN_POINT('Ctrl Pts',(-25.0318103813017,-12.4519136571081,
113.944073802906)) ;
#170398 = CARTESIAN_POINT('Ctrl Pts',(-25.1056142329247,-12.4519136645641,
113.919842786205)) ;
#170399 = CARTESIAN_POINT('Ctrl Pts',(-25.1794180845476,-12.4519136720201,
113.895611769504)) ;
#170400 = CARTESIAN_POINT('Ctrl Pts',(-25.1863441635937,-12.379327474119,
113.916707488231)) ;
#170401 = CARTESIAN_POINT('Ctrl Pts',(-25.1932702426397,-12.3067412762178,
113.937803206958)) ;
#170402 = CARTESIAN_POINT('Ctrl Pts',(-25.1194663910168,-12.3067412687618,
113.962034223658)) ;
#170403 = CARTESIAN_POINT('Ctrl Pts',(-25.0456625393938,-12.3067412613058,
113.986265240359)) ;
#170404 = CARTESIAN_POINT('Ctrl Pts',(-25.0387364603478,-12.3793274592069,
113.965169521633)) ;
#170405 = CARTESIAN_POINT('Ctrl Pts',(-25.1313553076052,-12.5020990421703,
114.211888040928)) ;
#170406 = CARTESIAN_POINT('Ctrl Pts',(-25.1186847142816,-12.5662179845147,
114.173295458733)) ;
#170407 = CARTESIAN_POINT('Ctrl Pts',(-25.192488566993,-12.5662180028208,
114.149064445347)) ;
#170408 = CARTESIAN_POINT('Ctrl Pts',(-25.2662924197043,-12.5662180211268,
114.124833431961)) ;
#170409 = CARTESIAN_POINT('Ctrl Pts',(-25.2789630130279,-12.5020990787824,
114.163426014156)) ;
#170410 = CARTESIAN_POINT('Ctrl Pts',(-25.2916336063514,-12.4379801364379,
114.20201859635)) ;
#170411 = CARTESIAN_POINT('Ctrl Pts',(-25.21782975364,-12.4379801181319,114.226249609736)) ;
#170412 = CARTESIAN_POINT('Ctrl Pts',(-25.1440259009287,-12.4379800998258,
114.250480623122)) ;
#170413 = CARTESIAN_POINT('Ctrl Pts',(-25.1313553076052,-12.5020990421703,
114.211888040928)) ;
#170414 = CARTESIAN_POINT('Ctrl Pts',(-25.2111527874365,-12.6906392671464,
114.419456391341)) ;
#170415 = CARTESIAN_POINT('Ctrl Pts',(-25.1936266344623,-12.7416870715668,
114.366074558063)) ;
#170416 = CARTESIAN_POINT('Ctrl Pts',(-25.2674304872085,-12.7416871035792,
114.341843544783)) ;
#170417 = CARTESIAN_POINT('Ctrl Pts',(-25.3412343399546,-12.7416871355915,
114.317612531503)) ;
#170418 = CARTESIAN_POINT('Ctrl Pts',(-25.3587604929287,-12.6906393311711,
114.370994364781)) ;
#170419 = CARTESIAN_POINT('Ctrl Pts',(-25.3762866459028,-12.6395915267507,
114.424376198059)) ;
#170420 = CARTESIAN_POINT('Ctrl Pts',(-25.3024827931567,-12.6395914947383,
114.448607211339)) ;
#170421 = CARTESIAN_POINT('Ctrl Pts',(-25.2286789404106,-12.639591462726,
114.472838224619)) ;
#170422 = CARTESIAN_POINT('Ctrl Pts',(-25.2111527874365,-12.6906392671464,
114.419456391341)) ;
#170423 = CARTESIAN_POINT('Ctrl Pts',(-25.2729365333473,-12.9321841999642,
114.572061782235)) ;
#170424 = CARTESIAN_POINT('Ctrl Pts',(-25.25180746659,-12.9664415034876,114.507706055091)) ;
#170425 = CARTESIAN_POINT('Ctrl Pts',(-25.3256113176767,-12.9664415511475,
114.483475036757)) ;
#170426 = CARTESIAN_POINT('Ctrl Pts',(-25.3994151687633,-12.9664415988073,
114.459244018423)) ;
#170427 = CARTESIAN_POINT('Ctrl Pts',(-25.4205442355206,-12.9321842952839,
114.523599745566)) ;
#170428 = CARTESIAN_POINT('Ctrl Pts',(-25.4416733022779,-12.8979269917605,
114.58795547271)) ;
#170429 = CARTESIAN_POINT('Ctrl Pts',(-25.3678694511913,-12.8979269441006,
114.612186491044)) ;
#170430 = CARTESIAN_POINT('Ctrl Pts',(-25.2940656001046,-12.8979268964408,
114.636417509379)) ;
#170431 = CARTESIAN_POINT('Ctrl Pts',(-25.2729365333473,-12.9321841999642,
114.572061782235)) ;
#170432 = CARTESIAN_POINT('Ctrl Pts',(-25.3126916179783,-13.2070342064579,
114.657780243976)) ;
#170433 = CARTESIAN_POINT('Ctrl Pts',(-25.2894883187306,-13.2221513251204,
114.58710673949)) ;
#170434 = CARTESIAN_POINT('Ctrl Pts',(-25.3632921660642,-13.2221513851254,
114.562875709725)) ;
#170435 = CARTESIAN_POINT('Ctrl Pts',(-25.4370960133978,-13.2221514451304,
114.538644679959)) ;
#170436 = CARTESIAN_POINT('Ctrl Pts',(-25.4602993126456,-13.2070343264679,
114.609318184445)) ;
#170437 = CARTESIAN_POINT('Ctrl Pts',(-25.4835026118934,-13.1919172078054,
114.679991688931)) ;
#170438 = CARTESIAN_POINT('Ctrl Pts',(-25.4096987645597,-13.1919171478004,
114.704222718696)) ;
#170439 = CARTESIAN_POINT('Ctrl Pts',(-25.3358949172261,-13.1919170877954,
114.728453748462)) ;
#170440 = CARTESIAN_POINT('Ctrl Pts',(-25.3126916179783,-13.2070342064579,
114.657780243976)) ;
#170441 = CARTESIAN_POINT('Ctrl Pts',(-25.3287288342473,-13.4981307625057,
114.671102244044)) ;
#170442 = CARTESIAN_POINT('Ctrl Pts',(-25.30510729808,-13.4929460625343,114.599154857553)) ;
#170443 = CARTESIAN_POINT('Ctrl Pts',(-25.3789111400793,-13.492946132437,
114.57492381154)) ;
#170444 = CARTESIAN_POINT('Ctrl Pts',(-25.4527149820785,-13.4929462023397,
114.550692765527)) ;
#170445 = CARTESIAN_POINT('Ctrl Pts',(-25.4763365182457,-13.4981309023111,
114.622640152017)) ;
#170446 = CARTESIAN_POINT('Ctrl Pts',(-25.499958054413,-13.5033156022825,
114.694587538508)) ;
#170447 = CARTESIAN_POINT('Ctrl Pts',(-25.4261542124138,-13.5033155323798,
114.718818584521)) ;
#170448 = CARTESIAN_POINT('Ctrl Pts',(-25.3523503704145,-13.5033154624771,
114.743049630534)) ;
#170449 = CARTESIAN_POINT('Ctrl Pts',(-25.3287288342473,-13.4981307625057,
114.671102244044)) ;
#170450 = CARTESIAN_POINT('Ctrl Pts',(-25.3205785524251,-13.7819922849582,
114.610954054946)) ;
#170451 = CARTESIAN_POINT('Ctrl Pts',(-25.2982228761858,-13.7569816324817,
114.542862273677)) ;
#170452 = CARTESIAN_POINT('Ctrl Pts',(-25.3720267117804,-13.7569817049211,
114.518631208156)) ;
#170453 = CARTESIAN_POINT('Ctrl Pts',(-25.4458305473751,-13.7569817773604,
114.494400142636)) ;
#170454 = CARTESIAN_POINT('Ctrl Pts',(-25.4681862236144,-13.7819924298369,
114.562491923905)) ;
#170455 = CARTESIAN_POINT('Ctrl Pts',(-25.4905418998538,-13.8070030823134,
114.630583705174)) ;
#170456 = CARTESIAN_POINT('Ctrl Pts',(-25.4167380642591,-13.807003009874,
114.654814770694)) ;
#170457 = CARTESIAN_POINT('Ctrl Pts',(-25.3429342286645,-13.8070029374347,
114.679045836215)) ;
#170458 = CARTESIAN_POINT('Ctrl Pts',(-25.3205785524251,-13.7819922849582,
114.610954054946)) ;
#170459 = CARTESIAN_POINT('Ctrl Pts',(-25.2893677697261,-14.041794726603,
114.480288046438)) ;
#170460 = CARTESIAN_POINT('Ctrl Pts',(-25.2698952365706,-13.9986090894959,
114.420977853969)) ;
#170461 = CARTESIAN_POINT('Ctrl Pts',(-25.3436990649528,-13.998609159369,
114.39674676648)) ;
#170462 = CARTESIAN_POINT('Ctrl Pts',(-25.4175028933349,-13.998609229242,
114.372515678992)) ;
#170463 = CARTESIAN_POINT('Ctrl Pts',(-25.4369754264904,-14.0417948663491,
114.431825871461)) ;
#170464 = CARTESIAN_POINT('Ctrl Pts',(-25.4564479596458,-14.0849805034562,
114.49113606393)) ;
#170465 = CARTESIAN_POINT('Ctrl Pts',(-25.3826441312637,-14.0849804335832,
114.515367151419)) ;
#170466 = CARTESIAN_POINT('Ctrl Pts',(-25.3088403028815,-14.0849803637101,
114.539598238908)) ;
#170467 = CARTESIAN_POINT('Ctrl Pts',(-25.2893677697261,-14.041794726603,
114.480288046438)) ;
#170468 = CARTESIAN_POINT('Ctrl Pts',(-25.2384611579753,-14.255449164482,
114.289862963828)) ;
#170469 = CARTESIAN_POINT('Ctrl Pts',(-25.2232464047646,-14.197284228839,
114.243521282191)) ;
#170470 = CARTESIAN_POINT('Ctrl Pts',(-25.2970502265122,-14.197284287096,
114.219290174495)) ;
#170471 = CARTESIAN_POINT('Ctrl Pts',(-25.3708540482598,-14.197284345353,
114.195059066798)) ;
#170472 = CARTESIAN_POINT('Ctrl Pts',(-25.3860688014705,-14.2554492809961,
114.241400748435)) ;
#170473 = CARTESIAN_POINT('Ctrl Pts',(-25.4012835546813,-14.3136142166391,
114.287742430073)) ;
#170474 = CARTESIAN_POINT('Ctrl Pts',(-25.3274797329337,-14.3136141583821,
114.311973537769)) ;
#170475 = CARTESIAN_POINT('Ctrl Pts',(-25.2536759111861,-14.313614100125,
114.336204645465)) ;
#170476 = CARTESIAN_POINT('Ctrl Pts',(-25.2384611579753,-14.255449164482,
114.289862963828)) ;
#170477 = CARTESIAN_POINT('Ctrl Pts',(-25.1715626825997,-14.4102492008634,
114.050454773655)) ;
#170478 = CARTESIAN_POINT('Ctrl Pts',(-25.161733771036,-14.3411914994799,
114.0205174968)) ;
#170479 = CARTESIAN_POINT('Ctrl Pts',(-25.2355375868551,-14.3411915397154,
113.996286371046)) ;
#170480 = CARTESIAN_POINT('Ctrl Pts',(-25.3093414026742,-14.3411915799509,
113.972055245292)) ;
#170481 = CARTESIAN_POINT('Ctrl Pts',(-25.3191703142378,-14.4102492813345,
114.001992522148)) ;
#170482 = CARTESIAN_POINT('Ctrl Pts',(-25.3289992258014,-14.4793069827181,
114.031929799003)) ;
#170483 = CARTESIAN_POINT('Ctrl Pts',(-25.2551954099824,-14.4793069424825,
114.056160924757)) ;
#170484 = CARTESIAN_POINT('Ctrl Pts',(-25.1813915941633,-14.479306902247,
114.080392050511)) ;
#170485 = CARTESIAN_POINT('Ctrl Pts',(-25.1715626825997,-14.4102492008634,
114.050454773655)) ;
#170486 = CARTESIAN_POINT('Ctrl Pts',(-25.0954032709923,-14.4927425304254,
113.7832103655)) ;
#170487 = CARTESIAN_POINT('Ctrl Pts',(-25.0916071708474,-14.4178249477771,
113.771648058903)) ;
#170488 = CARTESIAN_POINT('Ctrl Pts',(-25.1654109832459,-14.4178249636249,
113.747416922731)) ;
#170489 = CARTESIAN_POINT('Ctrl Pts',(-25.2392147956444,-14.4178249794727,
113.723185786558)) ;
#170490 = CARTESIAN_POINT('Ctrl Pts',(-25.2430108957893,-14.4927425621209,
113.734748093156)) ;
#170491 = CARTESIAN_POINT('Ctrl Pts',(-25.2468069959341,-14.5676601447692,
113.746310399753)) ;
#170492 = CARTESIAN_POINT('Ctrl Pts',(-25.1730031835356,-14.5676601289214,
113.770541535925)) ;
#170493 = CARTESIAN_POINT('Ctrl Pts',(-25.0991993711371,-14.5676601130736,
113.794772672097)) ;
#170494 = CARTESIAN_POINT('Ctrl Pts',(-25.0954032709923,-14.4927425304254,
113.7832103655)) ;
#170495 = CARTESIAN_POINT('Ctrl Pts',(-25.0150521907154,-14.4990616510816,
113.502979825597)) ;
#170496 = CARTESIAN_POINT('Ctrl Pts',(-25.0175947209408,-14.4235929848165,
113.510723964445)) ;
#170497 = CARTESIAN_POINT('Ctrl Pts',(-25.0913985319841,-14.4235929732871,
113.486492824145)) ;
#170498 = CARTESIAN_POINT('Ctrl Pts',(-25.1652023430274,-14.4235929617576,
113.462261683846)) ;
#170499 = CARTESIAN_POINT('Ctrl Pts',(-25.162659812802,-14.4990616280226,
113.454517544997)) ;
#170500 = CARTESIAN_POINT('Ctrl Pts',(-25.1601172825766,-14.5745302942877,
113.446773406148)) ;
#170501 = CARTESIAN_POINT('Ctrl Pts',(-25.0863134715333,-14.5745303058172,
113.471004546448)) ;
#170502 = CARTESIAN_POINT('Ctrl Pts',(-25.01250966049,-14.5745303173466,113.495235686748)) ;
#170503 = CARTESIAN_POINT('Ctrl Pts',(-25.0150521907154,-14.4990616510816,
113.502979825597)) ;
#170504 = CARTESIAN_POINT('Ctrl Pts',(-24.9375447991963,-14.4278621718276,
113.231466674976)) ;
#170505 = CARTESIAN_POINT('Ctrl Pts',(-24.9462355998666,-14.3572534635398,
113.257937453626)) ;
#170506 = CARTESIAN_POINT('Ctrl Pts',(-25.0200394123353,-14.357253423911,
113.233706317668)) ;
#170507 = CARTESIAN_POINT('Ctrl Pts',(-25.0938432248041,-14.3572533842822,
113.20947518171)) ;
#170508 = CARTESIAN_POINT('Ctrl Pts',(-25.0851524241338,-14.4278620925699,
113.18300440306)) ;
#170509 = CARTESIAN_POINT('Ctrl Pts',(-25.0764616234635,-14.4984708008576,
113.15653362441)) ;
#170510 = CARTESIAN_POINT('Ctrl Pts',(-25.0026578109947,-14.4984708404865,
113.180764760368)) ;
#170511 = CARTESIAN_POINT('Ctrl Pts',(-24.928853998526,-14.4984708801153,
113.204995896326)) ;
#170512 = CARTESIAN_POINT('Ctrl Pts',(-24.9375447991963,-14.4278621718276,
113.231466674976)) ;
#170513 = CARTESIAN_POINT('Ctrl Pts',(-24.8688494001846,-14.2839264835508,
112.986674234856)) ;
#170514 = CARTESIAN_POINT('Ctrl Pts',(-24.8830847973271,-14.2232622888904,
113.030032959772)) ;
#170515 = CARTESIAN_POINT('Ctrl Pts',(-24.9568886138432,-14.2232622233179,
113.005801836142)) ;
#170516 = CARTESIAN_POINT('Ctrl Pts',(-25.0306924303592,-14.2232621577455,
112.981570712511)) ;
#170517 = CARTESIAN_POINT('Ctrl Pts',(-25.0164570332166,-14.2839263524059,
112.938211987594)) ;
#170518 = CARTESIAN_POINT('Ctrl Pts',(-25.0022216360741,-14.3445905470663,
112.894853262678)) ;
#170519 = CARTESIAN_POINT('Ctrl Pts',(-24.928417819558,-14.3445906126388,
112.919084386308)) ;
#170520 = CARTESIAN_POINT('Ctrl Pts',(-24.854614003042,-14.3445906782112,
112.943315509939)) ;
#170521 = CARTESIAN_POINT('Ctrl Pts',(-24.8688494001846,-14.2839264835508,
112.986674234856)) ;
#170522 = CARTESIAN_POINT('Ctrl Pts',(-24.815043038472,-14.0776636855761,
112.787261502365)) ;
#170523 = CARTESIAN_POINT('Ctrl Pts',(-24.8337912269029,-14.0313099788708,
112.844365461409)) ;
#170524 = CARTESIAN_POINT('Ctrl Pts',(-24.9075950498521,-14.0313098927161,
112.820134357373)) ;
#170525 = CARTESIAN_POINT('Ctrl Pts',(-24.9813988728013,-14.0313098065613,
112.795903253336)) ;
#170526 = CARTESIAN_POINT('Ctrl Pts',(-24.9626506843704,-14.0776635132666,
112.738799294292)) ;
#170527 = CARTESIAN_POINT('Ctrl Pts',(-24.9439024959395,-14.1240172199719,
112.681695335248)) ;
#170528 = CARTESIAN_POINT('Ctrl Pts',(-24.8700986729903,-14.1240173061266,
112.705926439284)) ;
#170529 = CARTESIAN_POINT('Ctrl Pts',(-24.7962948500411,-14.1240173922814,
112.730157543321)) ;
#170530 = CARTESIAN_POINT('Ctrl Pts',(-24.815043038472,-14.0776636855761,
112.787261502365)) ;
#170531 = CARTESIAN_POINT('Ctrl Pts',(-24.7807407303966,-13.825817961869,
112.647479206348)) ;
#170532 = CARTESIAN_POINT('Ctrl Pts',(-24.8026420004503,-13.7969788395993,
112.714186943252)) ;
#170533 = CARTESIAN_POINT('Ctrl Pts',(-24.8764458313452,-13.7969787399069,
112.689955863417)) ;
#170534 = CARTESIAN_POINT('Ctrl Pts',(-24.95024966224,-13.7969786402144,112.665724783582)) ;
#170535 = CARTESIAN_POINT('Ctrl Pts',(-24.9283483921862,-13.8258177624841,
112.599017046678)) ;
#170536 = CARTESIAN_POINT('Ctrl Pts',(-24.9064471221324,-13.8546568847537,
112.532309309774)) ;
#170537 = CARTESIAN_POINT('Ctrl Pts',(-24.8326432912376,-13.8546569844462,
112.556540389609)) ;
#170538 = CARTESIAN_POINT('Ctrl Pts',(-24.7588394603428,-13.8546570841386,
112.580771469444)) ;
#170539 = CARTESIAN_POINT('Ctrl Pts',(-24.7807407303966,-13.825817961869,
112.647479206348)) ;
#170540 = CARTESIAN_POINT('Ctrl Pts',(-24.7687598363281,-13.5431962708422,
112.575457209354)) ;
#170541 = CARTESIAN_POINT('Ctrl Pts',(-24.7922654208681,-13.5340457388908,
112.647051429285)) ;
#170542 = CARTESIAN_POINT('Ctrl Pts',(-24.8660692605831,-13.5340456342861,
112.622820376315)) ;
#170543 = CARTESIAN_POINT('Ctrl Pts',(-24.9398731002982,-13.5340455296813,
112.598589323345)) ;
#170544 = CARTESIAN_POINT('Ctrl Pts',(-24.9163675157582,-13.5431960616327,
112.526995103414)) ;
#170545 = CARTESIAN_POINT('Ctrl Pts',(-24.8928619312182,-13.5523465935841,
112.455400883483)) ;
#170546 = CARTESIAN_POINT('Ctrl Pts',(-24.8190580915032,-13.5523466981889,
112.479631936453)) ;
#170547 = CARTESIAN_POINT('Ctrl Pts',(-24.7452542517881,-13.5523468027936,
112.503862989423)) ;
#170548 = CARTESIAN_POINT('Ctrl Pts',(-24.7687598363281,-13.5431962708422,
112.575457209354)) ;
#170549 = CARTESIAN_POINT('Ctrl Pts',(-24.7809665685125,-13.2523620051609,
112.577212862889)) ;
#170550 = CARTESIAN_POINT('Ctrl Pts',(-24.8043879898163,-13.2635030369063,
112.648550735123)) ;
#170551 = CARTESIAN_POINT('Ctrl Pts',(-24.878191838198,-13.2635029359697,
112.62431970855)) ;
#170552 = CARTESIAN_POINT('Ctrl Pts',(-24.9519956865798,-13.2635028350331,
112.600088681977)) ;
#170553 = CARTESIAN_POINT('Ctrl Pts',(-24.9285742652759,-13.2523618032878,
112.528750809743)) ;
#170554 = CARTESIAN_POINT('Ctrl Pts',(-24.9051528439722,-13.2412207715424,
112.457412937509)) ;
#170555 = CARTESIAN_POINT('Ctrl Pts',(-24.8313489955904,-13.241220872479,
112.481643964082)) ;
#170556 = CARTESIAN_POINT('Ctrl Pts',(-24.7575451472087,-13.2412209734156,
112.505874990655)) ;
#170557 = CARTESIAN_POINT('Ctrl Pts',(-24.7809665685125,-13.2523620051609,
112.577212862889)) ;
#170558 = CARTESIAN_POINT('Ctrl Pts',(-24.8172568115443,-12.972854005055,
112.652243647584)) ;
#170559 = CARTESIAN_POINT('Ctrl Pts',(-24.8389143107608,-13.0035262645876,
112.718208897662)) ;
#170560 = CARTESIAN_POINT('Ctrl Pts',(-24.9127181667632,-13.0035261755681,
112.6939778943)) ;
#170561 = CARTESIAN_POINT('Ctrl Pts',(-24.9865220227656,-13.0035260865486,
112.669746890938)) ;
#170562 = CARTESIAN_POINT('Ctrl Pts',(-24.9648645235491,-12.9728538270159,
112.603781640861)) ;
#170563 = CARTESIAN_POINT('Ctrl Pts',(-24.9432070243326,-12.9421815674833,
112.537816390783)) ;
#170564 = CARTESIAN_POINT('Ctrl Pts',(-24.8694031683302,-12.9421816565028,
112.562047394144)) ;
#170565 = CARTESIAN_POINT('Ctrl Pts',(-24.7955993123278,-12.9421817455224,
112.586278397506)) ;
#170566 = CARTESIAN_POINT('Ctrl Pts',(-24.8172568115443,-12.972854005055,
112.652243647584)) ;
#170567 = CARTESIAN_POINT('Ctrl Pts',(-24.8754805907761,-12.7260422771964,
112.794217709271)) ;
#170568 = CARTESIAN_POINT('Ctrl Pts',(-24.8938372765157,-12.7739923813095,
112.850129213994)) ;
#170569 = CARTESIAN_POINT('Ctrl Pts',(-24.9676411385468,-12.7739923097986,
112.825898228995)) ;
#170570 = CARTESIAN_POINT('Ctrl Pts',(-25.041445000578,-12.7739922382878,
112.801667243996)) ;
#170571 = CARTESIAN_POINT('Ctrl Pts',(-25.0230883148385,-12.7260421341746,
112.745755739273)) ;
#170572 = CARTESIAN_POINT('Ctrl Pts',(-25.0047316290989,-12.6780920300614,
112.68984423455)) ;
#170573 = CARTESIAN_POINT('Ctrl Pts',(-24.9309277670678,-12.6780921015723,
112.714075219549)) ;
#170574 = CARTESIAN_POINT('Ctrl Pts',(-24.8571239050366,-12.6780921730832,
112.738306204548)) ;
#170575 = CARTESIAN_POINT('Ctrl Pts',(-24.8754805907761,-12.7260422771964,
112.794217709271)) ;
#170576 = CARTESIAN_POINT('Ctrl Pts',(-24.9530612233143,-12.5272823112894,
112.994865114969)) ;
#170577 = CARTESIAN_POINT('Ctrl Pts',(-24.9667668683183,-12.5891820336003,
113.03661029991)) ;
#170578 = CARTESIAN_POINT('Ctrl Pts',(-25.0405707337368,-12.5891819848851,
113.012379325228)) ;
#170579 = CARTESIAN_POINT('Ctrl Pts',(-25.1143745991552,-12.58918193617,112.988148350546)) ;
#170580 = CARTESIAN_POINT('Ctrl Pts',(-25.1006689541512,-12.5272822138591,
112.946403165605)) ;
#170581 = CARTESIAN_POINT('Ctrl Pts',(-25.0869633091472,-12.4653824915483,
112.904657980664)) ;
#170582 = CARTESIAN_POINT('Ctrl Pts',(-25.0131594437287,-12.4653825402634,
112.928888955346)) ;
#170583 = CARTESIAN_POINT('Ctrl Pts',(-24.9393555783103,-12.4653825889786,
112.953119930028)) ;
#170584 = CARTESIAN_POINT('Ctrl Pts',(-24.9530612233143,-12.5272823112894,
112.994865114969)) ;
#170585 = CARTESIAN_POINT('Ctrl Pts',(-25.043926335439,-12.3938739809445,
113.23628572976)) ;
#170586 = CARTESIAN_POINT('Ctrl Pts',(-25.0520397402365,-12.4651813337181,
113.26099785322)) ;
#170587 = CARTESIAN_POINT('Ctrl Pts',(-25.1258436071122,-12.4651813074342,
113.236766882977)) ;
#170588 = CARTESIAN_POINT('Ctrl Pts',(-25.1996474739879,-12.4651812811503,
113.212535912733)) ;
#170589 = CARTESIAN_POINT('Ctrl Pts',(-25.1915340691904,-12.3938739283766,
113.187823789273)) ;
#170590 = CARTESIAN_POINT('Ctrl Pts',(-25.1834206643929,-12.322566575603,
113.163111665812)) ;
#170591 = CARTESIAN_POINT('Ctrl Pts',(-25.1096167975172,-12.3225666018869,
113.187342636056)) ;
#170592 = CARTESIAN_POINT('Ctrl Pts',(-25.0358129306415,-12.3225666281708,
113.211573606299)) ;
#170593 = CARTESIAN_POINT('Ctrl Pts',(-25.043926335439,-12.3938739809445,
113.23628572976)) ;
#170594 = CARTESIAN_POINT('Ctrl Pts',(-25.1433950034912,-12.3331330123649,
113.503738250658)) ;
#170595 = CARTESIAN_POINT('Ctrl Pts',(-25.1453107042945,-12.4087892430706,
113.509573167594)) ;
#170596 = CARTESIAN_POINT('Ctrl Pts',(-25.2191145700333,-12.408789238365,
113.485342193888)) ;
#170597 = CARTESIAN_POINT('Ctrl Pts',(-25.2929184357722,-12.4087892336594,
113.461111220182)) ;
#170598 = CARTESIAN_POINT('Ctrl Pts',(-25.2910027349689,-12.3331330029537,
113.455276303246)) ;
#170599 = CARTESIAN_POINT('Ctrl Pts',(-25.2890870341656,-12.257476772248,
113.44944138631)) ;
#170600 = CARTESIAN_POINT('Ctrl Pts',(-25.2152831684267,-12.2574767769536,
113.473672360017)) ;
#170601 = CARTESIAN_POINT('Ctrl Pts',(-25.1414793026879,-12.2574767816592,
113.497903333723)) ;
#170602 = CARTESIAN_POINT('Ctrl Pts',(-25.1433950034912,-12.3331330123649,
113.503738250658)) ;
#170603 = CARTESIAN_POINT('Ctrl Pts',(-25.2443302602174,-12.3500900604043,
113.775797196118)) ;
#170604 = CARTESIAN_POINT('Ctrl Pts',(-25.2399335184134,-12.4246766699504,
113.76240543124)) ;
#170605 = CARTESIAN_POINT('Ctrl Pts',(-25.3137373815055,-12.4246766830339,
113.738174449473)) ;
#170606 = CARTESIAN_POINT('Ctrl Pts',(-25.3875412445977,-12.4246766961173,
113.713943467705)) ;
#170607 = CARTESIAN_POINT('Ctrl Pts',(-25.3919379864017,-12.3500900865712,
113.727335232583)) ;
#170608 = CARTESIAN_POINT('Ctrl Pts',(-25.3963347282057,-12.2755034770251,
113.740726997461)) ;
#170609 = CARTESIAN_POINT('Ctrl Pts',(-25.3225308651136,-12.2755034639416,
113.764957979228)) ;
#170610 = CARTESIAN_POINT('Ctrl Pts',(-25.2487270020214,-12.2755034508582,
113.789188960996)) ;
#170611 = CARTESIAN_POINT('Ctrl Pts',(-25.2443302602174,-12.3500900604043,
113.775797196118)) ;
#170612 = CARTESIAN_POINT('Ctrl Pts',(-25.3412640091243,-12.4439523224458,
114.035430164998)) ;
#170613 = CARTESIAN_POINT('Ctrl Pts',(-25.3308294983348,-12.5120989674076,
114.003648329789)) ;
#170614 = CARTESIAN_POINT('Ctrl Pts',(-25.4046333568467,-12.5120989925412,
113.979417334071)) ;
#170615 = CARTESIAN_POINT('Ctrl Pts',(-25.4784372153586,-12.5120990176749,
113.955186338353)) ;
#170616 = CARTESIAN_POINT('Ctrl Pts',(-25.4888717261481,-12.4439523727131,
113.986968173562)) ;
#170617 = CARTESIAN_POINT('Ctrl Pts',(-25.4993062369376,-12.3758057277512,
114.01875000877)) ;
#170618 = CARTESIAN_POINT('Ctrl Pts',(-25.4255023784257,-12.3758057026176,
114.042981004488)) ;
#170619 = CARTESIAN_POINT('Ctrl Pts',(-25.3516985199137,-12.3758056774839,
114.067212000207)) ;
#170620 = CARTESIAN_POINT('Ctrl Pts',(-25.3412640091243,-12.4439523224458,
114.035430164998)) ;
#170621 = CARTESIAN_POINT('Ctrl Pts',(-25.4269581595394,-12.607738556858,
114.260951876422)) ;
#170622 = CARTESIAN_POINT('Ctrl Pts',(-25.411258848313,-12.6645527953263,
114.213134308381)) ;
#170623 = CARTESIAN_POINT('Ctrl Pts',(-25.485062702167,-12.6645528262529,
114.188903298476)) ;
#170624 = CARTESIAN_POINT('Ctrl Pts',(-25.558866556021,-12.6645528571796,
114.16467228857)) ;
#170625 = CARTESIAN_POINT('Ctrl Pts',(-25.5745658672475,-12.6077386187113,
114.212489856611)) ;
#170626 = CARTESIAN_POINT('Ctrl Pts',(-25.5902651784739,-12.5509243802431,
114.260307424651)) ;
#170627 = CARTESIAN_POINT('Ctrl Pts',(-25.5164613246199,-12.5509243493165,
114.284538434557)) ;
#170628 = CARTESIAN_POINT('Ctrl Pts',(-25.4426574707659,-12.5509243183898,
114.308769444462)) ;
#170629 = CARTESIAN_POINT('Ctrl Pts',(-25.4269581595394,-12.607738556858,
114.260951876422)) ;
#170630 = CARTESIAN_POINT('Ctrl Pts',(-25.4961702874896,-12.8282760815645,
114.436439976788)) ;
#170631 = CARTESIAN_POINT('Ctrl Pts',(-25.4763456274778,-12.8697778180786,
114.376057261829)) ;
#170632 = CARTESIAN_POINT('Ctrl Pts',(-25.5501494771654,-12.8697778506645,
114.351826239234)) ;
#170633 = CARTESIAN_POINT('Ctrl Pts',(-25.6239533268531,-12.8697778832504,
114.327595216638)) ;
#170634 = CARTESIAN_POINT('Ctrl Pts',(-25.6437779868649,-12.8282761467363,
114.387977931597)) ;
#170635 = CARTESIAN_POINT('Ctrl Pts',(-25.6636026468767,-12.7867744102223,
114.448360646555)) ;
#170636 = CARTESIAN_POINT('Ctrl Pts',(-25.589798797189,-12.7867743776364,
114.472591669151)) ;
#170637 = CARTESIAN_POINT('Ctrl Pts',(-25.5159949475014,-12.7867743450505,
114.496822691746)) ;
#170638 = CARTESIAN_POINT('Ctrl Pts',(-25.4961702874896,-12.8282760815645,
114.436439976788)) ;
#170639 = CARTESIAN_POINT('Ctrl Pts',(-25.5453502164331,-13.0924261676405,
114.550696842166)) ;
#170640 = CARTESIAN_POINT('Ctrl Pts',(-25.5227969254224,-13.1155471529824,
114.48200315727)) ;
#170641 = CARTESIAN_POINT('Ctrl Pts',(-25.5966007713147,-13.1155471809982,
114.457772123114)) ;
#170642 = CARTESIAN_POINT('Ctrl Pts',(-25.6704046172069,-13.1155472090139,
114.433541088958)) ;
#170643 = CARTESIAN_POINT('Ctrl Pts',(-25.6929579082176,-13.092426223672,
114.502234773854)) ;
#170644 = CARTESIAN_POINT('Ctrl Pts',(-25.7155111992283,-13.06930523833,114.57092845875)) ;
#170645 = CARTESIAN_POINT('Ctrl Pts',(-25.641707353336,-13.0693052103143,
114.595159492906)) ;
#170646 = CARTESIAN_POINT('Ctrl Pts',(-25.5679035074438,-13.0693051822985,
114.619390527062)) ;
#170647 = CARTESIAN_POINT('Ctrl Pts',(-25.5453502164331,-13.0924261676405,
114.550696842166)) ;
#170648 = CARTESIAN_POINT('Ctrl Pts',(-25.5711878044013,-13.3792544087802,
114.593953694912)) ;
#170649 = CARTESIAN_POINT('Ctrl Pts',(-25.5475296838539,-13.3823829246599,
114.52189487736)) ;
#170650 = CARTESIAN_POINT('Ctrl Pts',(-25.6213335272747,-13.3823829459244,
114.497663835676)) ;
#170651 = CARTESIAN_POINT('Ctrl Pts',(-25.6951373706955,-13.3823829671888,
114.473432793993)) ;
#170652 = CARTESIAN_POINT('Ctrl Pts',(-25.7187954912429,-13.3792544513091,
114.545491611545)) ;
#170653 = CARTESIAN_POINT('Ctrl Pts',(-25.7424536117902,-13.3761259354293,
114.617550429098)) ;
#170654 = CARTESIAN_POINT('Ctrl Pts',(-25.6686497683694,-13.3761259141649,
114.641781470781)) ;
#170655 = CARTESIAN_POINT('Ctrl Pts',(-25.5948459249486,-13.3761258929005,
114.666012512465)) ;
#170656 = CARTESIAN_POINT('Ctrl Pts',(-25.5711878044013,-13.3792544087802,
114.593953694912)) ;
#170657 = CARTESIAN_POINT('Ctrl Pts',(-25.572740914633,-13.6698091146606,
114.563123414499)) ;
#170658 = CARTESIAN_POINT('Ctrl Pts',(-25.5496743867624,-13.6526542862593,
114.492866492629)) ;
#170659 = CARTESIAN_POINT('Ctrl Pts',(-25.6234782290232,-13.6526542988554,
114.468635447412)) ;
#170660 = CARTESIAN_POINT('Ctrl Pts',(-25.697282071284,-13.6526543114514,
114.444404402195)) ;
#170661 = CARTESIAN_POINT('Ctrl Pts',(-25.7203485991545,-13.6698091398527,
114.514661324065)) ;
#170662 = CARTESIAN_POINT('Ctrl Pts',(-25.7434151270251,-13.686963968254,
114.584918245935)) ;
#170663 = CARTESIAN_POINT('Ctrl Pts',(-25.6696112847643,-13.686963955658,
114.609149291152)) ;
#170664 = CARTESIAN_POINT('Ctrl Pts',(-25.5958074425035,-13.6869639430619,
114.633380336369)) ;
#170665 = CARTESIAN_POINT('Ctrl Pts',(-25.572740914633,-13.6698091146606,
114.563123414499)) ;
#170666 = CARTESIAN_POINT('Ctrl Pts',(-25.5505747674364,-13.9412445098837,
114.460172921106)) ;
#170667 = CARTESIAN_POINT('Ctrl Pts',(-25.5297546025764,-13.9051106030385,
114.396758058401)) ;
#170668 = CARTESIAN_POINT('Ctrl Pts',(-25.6035584448034,-13.9051106090347,
114.372527013081)) ;
#170669 = CARTESIAN_POINT('Ctrl Pts',(-25.6773622870305,-13.905110615031,
114.348295967762)) ;
#170670 = CARTESIAN_POINT('Ctrl Pts',(-25.6981824518905,-13.9412445218762,
114.411710830467)) ;
#170671 = CARTESIAN_POINT('Ctrl Pts',(-25.7190026167506,-13.9773784287214,
114.475125693173)) ;
#170672 = CARTESIAN_POINT('Ctrl Pts',(-25.6451987745235,-13.9773784227252,
114.499356738492)) ;
#170673 = CARTESIAN_POINT('Ctrl Pts',(-25.5713949322964,-13.9773784167289,
114.523587783811)) ;
#170674 = CARTESIAN_POINT('Ctrl Pts',(-25.5505747674364,-13.9412445098837,
114.460172921106)) ;
#170675 = CARTESIAN_POINT('Ctrl Pts',(-25.5073811967448,-14.1747166899893,
114.293293093269)) ;
#170676 = CARTESIAN_POINT('Ctrl Pts',(-25.4902767699507,-14.1222263839683,
114.241195769094)) ;
#170677 = CARTESIAN_POINT('Ctrl Pts',(-25.5640806127003,-14.1222263855747,
114.216964725366)) ;
#170678 = CARTESIAN_POINT('Ctrl Pts',(-25.6378844554499,-14.122226387181,
114.192733681639)) ;
#170679 = CARTESIAN_POINT('Ctrl Pts',(-25.654988882244,-14.1747166932021,
114.244831005813)) ;
#170680 = CARTESIAN_POINT('Ctrl Pts',(-25.672093309038,-14.2272069992232,
114.296928329988)) ;
#170681 = CARTESIAN_POINT('Ctrl Pts',(-25.5982894662884,-14.2272069976168,
114.321159373716)) ;
#170682 = CARTESIAN_POINT('Ctrl Pts',(-25.5244856235388,-14.2272069960104,
114.345390417444)) ;
#170683 = CARTESIAN_POINT('Ctrl Pts',(-25.5073811967448,-14.1747166899893,
114.293293093269)) ;
#170684 = CARTESIAN_POINT('Ctrl Pts',(-25.4463048591916,-14.355514528968,
114.071666128729)) ;
#170685 = CARTESIAN_POINT('Ctrl Pts',(-25.4341763419453,-14.2903204554486,
114.034724622094)) ;
#170686 = CARTESIAN_POINT('Ctrl Pts',(-25.5079801857457,-14.2903204543728,
114.010493581567)) ;
#170687 = CARTESIAN_POINT('Ctrl Pts',(-25.581784029546,-14.290320453297,113.98626254104)) ;
#170688 = CARTESIAN_POINT('Ctrl Pts',(-25.5939125467923,-14.3555145268165,
114.023204047674)) ;
#170689 = CARTESIAN_POINT('Ctrl Pts',(-25.6060410640385,-14.4207086003359,
114.060145554309)) ;
#170690 = CARTESIAN_POINT('Ctrl Pts',(-25.5322372202382,-14.4207086014117,
114.084376594836)) ;
#170691 = CARTESIAN_POINT('Ctrl Pts',(-25.4584333764379,-14.4207086024875,
114.108607635363)) ;
#170692 = CARTESIAN_POINT('Ctrl Pts',(-25.4463048591916,-14.355514528968,
114.071666128729)) ;
#170693 = CARTESIAN_POINT('Ctrl Pts',(-25.3732239530328,-14.4682461385157,
113.813679160758)) ;
#170694 = CARTESIAN_POINT('Ctrl Pts',(-25.3669130070119,-14.3950833007867,
113.794457037381)) ;
#170695 = CARTESIAN_POINT('Ctrl Pts',(-25.4407168514207,-14.3950832998909,
113.770225998707)) ;
#170696 = CARTESIAN_POINT('Ctrl Pts',(-25.5145206958295,-14.395083298995,
113.745994960033)) ;
#170697 = CARTESIAN_POINT('Ctrl Pts',(-25.5208316418504,-14.468246136724,
113.76521708341)) ;
#170698 = CARTESIAN_POINT('Ctrl Pts',(-25.5271425878713,-14.5414089744529,
113.784439206786)) ;
#170699 = CARTESIAN_POINT('Ctrl Pts',(-25.4533387434625,-14.5414089753487,
113.80867024546)) ;
#170700 = CARTESIAN_POINT('Ctrl Pts',(-25.3795348990537,-14.5414089762446,
113.832901284134)) ;
#170701 = CARTESIAN_POINT('Ctrl Pts',(-25.3732239530328,-14.4682461385157,
113.813679160758)) ;
#170702 = CARTESIAN_POINT('Ctrl Pts',(-25.2933869167422,-14.5059599121584,
113.534915352588)) ;
#170703 = CARTESIAN_POINT('Ctrl Pts',(-25.2933783368985,-14.4300548891346,
113.534889219716)) ;
#170704 = CARTESIAN_POINT('Ctrl Pts',(-25.3671821811493,-14.4300548892677,
113.510658180561)) ;
#170705 = CARTESIAN_POINT('Ctrl Pts',(-25.4409860254001,-14.4300548894008,
113.486427141406)) ;
#170706 = CARTESIAN_POINT('Ctrl Pts',(-25.4409946052437,-14.5059599124246,
113.486453274277)) ;
#170707 = CARTESIAN_POINT('Ctrl Pts',(-25.4410031850873,-14.5818649354484,
113.486479407148)) ;
#170708 = CARTESIAN_POINT('Ctrl Pts',(-25.3671993408365,-14.5818649353153,
113.510710446304)) ;
#170709 = CARTESIAN_POINT('Ctrl Pts',(-25.2933954965857,-14.5818649351822,
113.534941485459)) ;
#170710 = CARTESIAN_POINT('Ctrl Pts',(-25.2933869167422,-14.5059599121584,
113.534915352588)) ;
#170711 = CARTESIAN_POINT('Ctrl Pts',(-25.2143421603494,-14.4658731530402,
113.258876232179)) ;
#170712 = CARTESIAN_POINT('Ctrl Pts',(-25.2205830584677,-14.3926562072765,
113.27788500087)) ;
#170713 = CARTESIAN_POINT('Ctrl Pts',(-25.2943869020412,-14.3926562077147,
113.253653959652)) ;
#170714 = CARTESIAN_POINT('Ctrl Pts',(-25.3681907456146,-14.3926562081529,
113.229422918433)) ;
#170715 = CARTESIAN_POINT('Ctrl Pts',(-25.3619498474963,-14.4658731539167,
113.210414149742)) ;
#170716 = CARTESIAN_POINT('Ctrl Pts',(-25.355708949378,-14.5390900996804,
113.191405381051)) ;
#170717 = CARTESIAN_POINT('Ctrl Pts',(-25.2819051058046,-14.5390900992422,
113.215636422269)) ;
#170718 = CARTESIAN_POINT('Ctrl Pts',(-25.2081012622311,-14.539090098804,
113.239867463488)) ;
#170719 = CARTESIAN_POINT('Ctrl Pts',(-25.2143421603494,-14.4658731530402,
113.258876232179)) ;
#170720 = CARTESIAN_POINT('Ctrl Pts',(-25.1412442200855,-14.3505784504634,
113.000683869835)) ;
#170721 = CARTESIAN_POINT('Ctrl Pts',(-25.153334124402,-14.2853046871927,
113.037507767757)) ;
#170722 = CARTESIAN_POINT('Ctrl Pts',(-25.2271379667205,-14.2853046856717,
113.013276722716)) ;
#170723 = CARTESIAN_POINT('Ctrl Pts',(-25.300941809039,-14.2853046841507,
112.989045677675)) ;
#170724 = CARTESIAN_POINT('Ctrl Pts',(-25.2888519047224,-14.3505784474213,
112.952221779753)) ;
#170725 = CARTESIAN_POINT('Ctrl Pts',(-25.2767620004059,-14.4158522106919,
112.915397881831)) ;
#170726 = CARTESIAN_POINT('Ctrl Pts',(-25.2029581580874,-14.4158522122129,
112.939628926871)) ;
#170727 = CARTESIAN_POINT('Ctrl Pts',(-25.129154315769,-14.415852213734,112.963859971912)) ;
#170728 = CARTESIAN_POINT('Ctrl Pts',(-25.1412442200855,-14.3505784504634,
113.000683869835)) ;
#170729 = CARTESIAN_POINT('Ctrl Pts',(-25.0807965149899,-14.1680509006919,
112.781046396121)) ;
#170730 = CARTESIAN_POINT('Ctrl Pts',(-25.0978599658701,-14.1154268840112,
112.833018914517)) ;
#170731 = CARTESIAN_POINT('Ctrl Pts',(-25.1716638070098,-14.1154268771774,
112.808787865886)) ;
#170732 = CARTESIAN_POINT('Ctrl Pts',(-25.2454676481495,-14.1154268703437,
112.784556817255)) ;
#170733 = CARTESIAN_POINT('Ctrl Pts',(-25.2284041972694,-14.1680508870244,
112.732584298859)) ;
#170734 = CARTESIAN_POINT('Ctrl Pts',(-25.2113407463893,-14.220674903705,
112.680611780463)) ;
#170735 = CARTESIAN_POINT('Ctrl Pts',(-25.1375369052496,-14.2206749105388,
112.704842829094)) ;
#170736 = CARTESIAN_POINT('Ctrl Pts',(-25.0637330641098,-14.2206749173726,
112.729073877726)) ;
#170737 = CARTESIAN_POINT('Ctrl Pts',(-25.0807965149899,-14.1680509006919,
112.781046396121)) ;
#170738 = CARTESIAN_POINT('Ctrl Pts',(-25.0381542588277,-13.9327426687889,
112.615783480832)) ;
#170739 = CARTESIAN_POINT('Ctrl Pts',(-25.0589520128571,-13.8964722980425,
112.679130084212)) ;
#170740 = CARTESIAN_POINT('Ctrl Pts',(-25.1327558537343,-13.8964722840852,
112.654899034782)) ;
#170741 = CARTESIAN_POINT('Ctrl Pts',(-25.2065596946115,-13.896472270128,
112.630667985351)) ;
#170742 = CARTESIAN_POINT('Ctrl Pts',(-25.1857619405821,-13.9327426408744,
112.56732138197)) ;
#170743 = CARTESIAN_POINT('Ctrl Pts',(-25.1649641865527,-13.9690130116207,
112.50397477859)) ;
#170744 = CARTESIAN_POINT('Ctrl Pts',(-25.0911603456755,-13.969013025578,
112.528205828021)) ;
#170745 = CARTESIAN_POINT('Ctrl Pts',(-25.0173565047983,-13.9690130395352,
112.552436877452)) ;
#170746 = CARTESIAN_POINT('Ctrl Pts',(-25.0381542588277,-13.9327426687889,
112.615783480832)) ;
#170747 = CARTESIAN_POINT('Ctrl Pts',(-25.01675443207,-13.660519783253,112.515187651297)) ;
#170748 = CARTESIAN_POINT('Ctrl Pts',(-25.0398093319936,-13.6432040400609,
112.58540915702)) ;
#170749 = CARTESIAN_POINT('Ctrl Pts',(-25.1136131735509,-13.6432040175434,
112.56117810966)) ;
#170750 = CARTESIAN_POINT('Ctrl Pts',(-25.1874170151081,-13.643203995026,
112.536947062301)) ;
#170751 = CARTESIAN_POINT('Ctrl Pts',(-25.1643621151845,-13.6605197382181,
112.466725556578)) ;
#170752 = CARTESIAN_POINT('Ctrl Pts',(-25.1413072152608,-13.6778354814103,
112.396504050855)) ;
#170753 = CARTESIAN_POINT('Ctrl Pts',(-25.0675033737036,-13.6778355039277,
112.420735098215)) ;
#170754 = CARTESIAN_POINT('Ctrl Pts',(-24.9936995321464,-13.6778355264452,
112.444966145574)) ;
#170755 = CARTESIAN_POINT('Ctrl Pts',(-25.01675443207,-13.660519783253,112.515187651297)) ;
#170756 = CARTESIAN_POINT('Ctrl Pts',(-25.0191170090691,-13.3693405601706,
112.486775760889)) ;
#170757 = CARTESIAN_POINT('Ctrl Pts',(-25.0427772853919,-13.3723302960764,
112.558841145632)) ;
#170758 = CARTESIAN_POINT('Ctrl Pts',(-25.1165811290148,-13.3723302632285,
112.534610104564)) ;
#170759 = CARTESIAN_POINT('Ctrl Pts',(-25.1903849726377,-13.3723302303806,
112.510379063496)) ;
#170760 = CARTESIAN_POINT('Ctrl Pts',(-25.1667246963149,-13.3693404944748,
112.438313678754)) ;
#170761 = CARTESIAN_POINT('Ctrl Pts',(-25.143064419992,-13.3663507585691,
112.366248294011)) ;
#170762 = CARTESIAN_POINT('Ctrl Pts',(-25.0692605763692,-13.366350791417,
112.390479335079)) ;
#170763 = CARTESIAN_POINT('Ctrl Pts',(-24.9954567327463,-13.3663508242649,
112.414710376146)) ;
#170764 = CARTESIAN_POINT('Ctrl Pts',(-25.0191170090691,-13.3693405601706,
112.486775760889)) ;
#170765 = CARTESIAN_POINT('Ctrl Pts',(-25.0457464324794,-13.0834454323783,
112.532499973071)) ;
#170766 = CARTESIAN_POINT('Ctrl Pts',(-25.0683137612795,-13.1064007088209,
112.601236416157)) ;
#170767 = CARTESIAN_POINT('Ctrl Pts',(-25.1421176083962,-13.1064006698969,
112.577005385731)) ;
#170768 = CARTESIAN_POINT('Ctrl Pts',(-25.2159214555129,-13.1064006309729,
112.552774355305)) ;
#170769 = CARTESIAN_POINT('Ctrl Pts',(-25.1933541267128,-13.0834453545303,
112.484037912218)) ;
#170770 = CARTESIAN_POINT('Ctrl Pts',(-25.1707867979127,-13.0604900780877,
112.415301469132)) ;
#170771 = CARTESIAN_POINT('Ctrl Pts',(-25.096982950796,-13.0604901170117,
112.439532499558)) ;
#170772 = CARTESIAN_POINT('Ctrl Pts',(-25.0231791036793,-13.0604901559357,
112.463763529984)) ;
#170773 = CARTESIAN_POINT('Ctrl Pts',(-25.0457464324794,-13.0834454323783,
112.532499973071)) ;
#170774 = CARTESIAN_POINT('Ctrl Pts',(-25.0953927384069,-12.8212149019315,
112.648303528621)) ;
#170775 = CARTESIAN_POINT('Ctrl Pts',(-25.1152590939034,-12.8625120463937,
112.708813242983)) ;
#170776 = CARTESIAN_POINT('Ctrl Pts',(-25.1890629454817,-12.8625120051449,
112.684582226146)) ;
#170777 = CARTESIAN_POINT('Ctrl Pts',(-25.26286679706,-12.8625119638961,112.660351209309)) ;
#170778 = CARTESIAN_POINT('Ctrl Pts',(-25.2430004415635,-12.8212148194339,
112.599841494947)) ;
#170779 = CARTESIAN_POINT('Ctrl Pts',(-25.223134086067,-12.7799176749718,
112.539331780585)) ;
#170780 = CARTESIAN_POINT('Ctrl Pts',(-25.1493302344887,-12.7799177162206,
112.563562797422)) ;
#170781 = CARTESIAN_POINT('Ctrl Pts',(-25.0755263829104,-12.7799177574694,
112.587793814259)) ;
#170782 = CARTESIAN_POINT('Ctrl Pts',(-25.0953927384069,-12.8212149019315,
112.648303528621)) ;
#170783 = CARTESIAN_POINT('Ctrl Pts',(-25.1654351503245,-12.6012650290221,
112.826176017049)) ;
#170784 = CARTESIAN_POINT('Ctrl Pts',(-25.1811738053442,-12.6579784616352,
112.874113421929)) ;
#170785 = CARTESIAN_POINT('Ctrl Pts',(-25.2549776620693,-12.6579784230308,
112.849882420768)) ;
#170786 = CARTESIAN_POINT('Ctrl Pts',(-25.3287815187944,-12.6579783844264,
112.825651419607)) ;
#170787 = CARTESIAN_POINT('Ctrl Pts',(-25.3130428637748,-12.6012649518134,
112.777714014728)) ;
#170788 = CARTESIAN_POINT('Ctrl Pts',(-25.2973042087551,-12.5445515192003,
112.729776609848)) ;
#170789 = CARTESIAN_POINT('Ctrl Pts',(-25.22350035203,-12.5445515578047,112.754007611009)) ;
#170790 = CARTESIAN_POINT('Ctrl Pts',(-25.1496964953049,-12.5445515964091,
112.77823861217)) ;
#170791 = CARTESIAN_POINT('Ctrl Pts',(-25.1654351503245,-12.6012650290221,
112.826176017049)) ;
#170792 = CARTESIAN_POINT('Ctrl Pts',(-25.2517211384274,-12.4396335453714,
113.053457862825)) ;
#170793 = CARTESIAN_POINT('Ctrl Pts',(-25.2621934935828,-12.5077139487023,
113.085354968207)) ;
#170794 = CARTESIAN_POINT('Ctrl Pts',(-25.3359973555674,-12.5077139189152,
113.061123983066)) ;
#170795 = CARTESIAN_POINT('Ctrl Pts',(-25.4098012175519,-12.5077138891282,
113.036892997925)) ;
#170796 = CARTESIAN_POINT('Ctrl Pts',(-25.3993288623965,-12.4396334857973,
113.004995892543)) ;
#170797 = CARTESIAN_POINT('Ctrl Pts',(-25.3888565072411,-12.3715530824664,
112.973098787161)) ;
#170798 = CARTESIAN_POINT('Ctrl Pts',(-25.3150526452566,-12.3715531122535,
112.997329772302)) ;
#170799 = CARTESIAN_POINT('Ctrl Pts',(-25.241248783272,-12.3715531420405,
113.021560757443)) ;
#170800 = CARTESIAN_POINT('Ctrl Pts',(-25.2517211384274,-12.4396335453714,
113.053457862825)) ;
#170801 = CARTESIAN_POINT('Ctrl Pts',(-25.3485498372979,-12.3483868402897,
113.31290023935)) ;
#170802 = CARTESIAN_POINT('Ctrl Pts',(-25.3530112255867,-12.4229364888091,
113.32648890968)) ;
#170803 = CARTESIAN_POINT('Ctrl Pts',(-25.4268150918738,-12.4229364744478,
113.302257937644)) ;
#170804 = CARTESIAN_POINT('Ctrl Pts',(-25.5006189581609,-12.4229364600866,
113.278026965608)) ;
#170805 = CARTESIAN_POINT('Ctrl Pts',(-25.4961575698721,-12.3483868115671,
113.264438295278)) ;
#170806 = CARTESIAN_POINT('Ctrl Pts',(-25.4916961815832,-12.2738371630477,
113.250849624949)) ;
#170807 = CARTESIAN_POINT('Ctrl Pts',(-25.4178923152961,-12.2738371774089,
113.275080596985)) ;
#170808 = CARTESIAN_POINT('Ctrl Pts',(-25.344088449009,-12.2738371917702,
113.299311569021)) ;
#170809 = CARTESIAN_POINT('Ctrl Pts',(-25.3485498372979,-12.3483868402897,
113.31290023935)) ;
#170810 = CARTESIAN_POINT('Ctrl Pts',(-25.4498951527532,-12.3339887574785,
113.58607265207)) ;
#170811 = CARTESIAN_POINT('Ctrl Pts',(-25.4480221295144,-12.4096519181944,
113.580367727088)) ;
#170812 = CARTESIAN_POINT('Ctrl Pts',(-25.5218259985408,-12.4096519246285,
113.556136763396)) ;
#170813 = CARTESIAN_POINT('Ctrl Pts',(-25.5956298675672,-12.4096519310626,
113.531905799703)) ;
#170814 = CARTESIAN_POINT('Ctrl Pts',(-25.597502890806,-12.3339887703467,
113.537610724685)) ;
#170815 = CARTESIAN_POINT('Ctrl Pts',(-25.5993759140449,-12.2583256096307,
113.543315649667)) ;
#170816 = CARTESIAN_POINT('Ctrl Pts',(-25.5255720450185,-12.2583256031966,
113.56754661336)) ;
#170817 = CARTESIAN_POINT('Ctrl Pts',(-25.4517681759921,-12.2583255967626,
113.591777577052)) ;
#170818 = CARTESIAN_POINT('Ctrl Pts',(-25.4498951527532,-12.3339887574785,
113.58607265207)) ;
#170819 = CARTESIAN_POINT('Ctrl Pts',(-25.5487281653842,-12.3966946761742,
113.851770969332)) ;
#170820 = CARTESIAN_POINT('Ctrl Pts',(-25.5406832866208,-12.4680894419109,
113.827267568358)) ;
#170821 = CARTESIAN_POINT('Ctrl Pts',(-25.6144871558984,-12.4680894717794,
113.80303660543)) ;
#170822 = CARTESIAN_POINT('Ctrl Pts',(-25.6882910251759,-12.4680895016479,
113.778805642503)) ;
#170823 = CARTESIAN_POINT('Ctrl Pts',(-25.6963359039393,-12.3966947359113,
113.803309043476)) ;
#170824 = CARTESIAN_POINT('Ctrl Pts',(-25.7043807827027,-12.3252999701746,
113.82781244445)) ;
#170825 = CARTESIAN_POINT('Ctrl Pts',(-25.6305769134251,-12.3252999403061,
113.852043407378)) ;
#170826 = CARTESIAN_POINT('Ctrl Pts',(-25.5567730441475,-12.3252999104375,
113.876274370305)) ;
#170827 = CARTESIAN_POINT('Ctrl Pts',(-25.5487281653842,-12.3966946761742,
113.851770969332)) ;
#170828 = CARTESIAN_POINT('Ctrl Pts',(-25.6400647909922,-12.5338429010278,
114.094279498921)) ;
#170829 = CARTESIAN_POINT('Ctrl Pts',(-25.6263698061829,-12.5957672263305,
114.052566786713)) ;
#170830 = CARTESIAN_POINT('Ctrl Pts',(-25.7001736738541,-12.5957672815326,
114.028335818893)) ;
#170831 = CARTESIAN_POINT('Ctrl Pts',(-25.7739775415252,-12.5957673367347,
114.004104851072)) ;
#170832 = CARTESIAN_POINT('Ctrl Pts',(-25.7876725263345,-12.533843011432,
114.04581756328)) ;
#170833 = CARTESIAN_POINT('Ctrl Pts',(-25.8013675111438,-12.4719186861293,
114.087530275488)) ;
#170834 = CARTESIAN_POINT('Ctrl Pts',(-25.7275636434727,-12.4719186309272,
114.111761243309)) ;
#170835 = CARTESIAN_POINT('Ctrl Pts',(-25.6537597758015,-12.4719185757251,
114.135992211129)) ;
#170836 = CARTESIAN_POINT('Ctrl Pts',(-25.6400647909922,-12.5338429010278,
114.094279498921)) ;
#170837 = CARTESIAN_POINT('Ctrl Pts',(-25.7162744596763,-12.7326606979156,
114.291115372328)) ;
#170838 = CARTESIAN_POINT('Ctrl Pts',(-25.6979689798409,-12.780794213553,
114.235359836244)) ;
#170839 = CARTESIAN_POINT('Ctrl Pts',(-25.7717728428061,-12.7807942904156,
114.21112885409)) ;
#170840 = CARTESIAN_POINT('Ctrl Pts',(-25.8455767057714,-12.7807943672782,
114.186897871936)) ;
#170841 = CARTESIAN_POINT('Ctrl Pts',(-25.8638821856068,-12.7326608516408,
114.24265340802)) ;
#170842 = CARTESIAN_POINT('Ctrl Pts',(-25.8821876654422,-12.6845273360034,
114.298408944103)) ;
#170843 = CARTESIAN_POINT('Ctrl Pts',(-25.8083838024769,-12.6845272591408,
114.322639926257)) ;
#170844 = CARTESIAN_POINT('Ctrl Pts',(-25.7345799395117,-12.6845271822782,
114.346870908411)) ;
#170845 = CARTESIAN_POINT('Ctrl Pts',(-25.7162744596763,-12.7326606979156,
114.291115372328)) ;
#170846 = CARTESIAN_POINT('Ctrl Pts',(-25.774069178511,-12.9811862243396,
114.431686787132)) ;
#170847 = CARTESIAN_POINT('Ctrl Pts',(-25.7524356589921,-13.0120391573078,
114.365794579227)) ;
#170848 = CARTESIAN_POINT('Ctrl Pts',(-25.8262395153994,-13.0120392516688,
114.341563577098)) ;
#170849 = CARTESIAN_POINT('Ctrl Pts',(-25.9000433718066,-13.0120393460298,
114.31733257497)) ;
#170850 = CARTESIAN_POINT('Ctrl Pts',(-25.9216768913254,-12.9811864130616,
114.383224782875)) ;
#170851 = CARTESIAN_POINT('Ctrl Pts',(-25.9433104108443,-12.9503334800935,
114.44911699078)) ;
#170852 = CARTESIAN_POINT('Ctrl Pts',(-25.8695065544371,-12.9503333857324,
114.473347992909)) ;
#170853 = CARTESIAN_POINT('Ctrl Pts',(-25.7957026980299,-12.9503332913714,
114.497578995037)) ;
#170854 = CARTESIAN_POINT('Ctrl Pts',(-25.774069178511,-12.9811862243396,
114.431686787132)) ;
#170855 = CARTESIAN_POINT('Ctrl Pts',(-25.8095884902637,-13.260918115125,
114.504434976696)) ;
#170856 = CARTESIAN_POINT('Ctrl Pts',(-25.7861766587316,-13.2722865612631,
114.433126317383)) ;
#170857 = CARTESIAN_POINT('Ctrl Pts',(-25.8599805069678,-13.2722866661501,
114.408895290367)) ;
#170858 = CARTESIAN_POINT('Ctrl Pts',(-25.9337843552041,-13.2722867710372,
114.384664263351)) ;
#170859 = CARTESIAN_POINT('Ctrl Pts',(-25.9571961867363,-13.2609183248991,
114.455972922664)) ;
#170860 = CARTESIAN_POINT('Ctrl Pts',(-25.9806080182684,-13.249549878761,
114.527281581977)) ;
#170861 = CARTESIAN_POINT('Ctrl Pts',(-25.9068041700321,-13.249549773874,
114.551512608993)) ;
#170862 = CARTESIAN_POINT('Ctrl Pts',(-25.8330003217958,-13.249549668987,
114.575743636009)) ;
#170863 = CARTESIAN_POINT('Ctrl Pts',(-25.8095884902637,-13.260918115125,
114.504434976696)) ;
#170864 = CARTESIAN_POINT('Ctrl Pts',(-25.8210548218699,-13.5531074788782,
114.503769138301)) ;
#170865 = CARTESIAN_POINT('Ctrl Pts',(-25.7975442428386,-13.5440933427765,
114.432159710076)) ;
#170866 = CARTESIAN_POINT('Ctrl Pts',(-25.8713480820835,-13.5440934499071,
114.407928655674)) ;
#170867 = CARTESIAN_POINT('Ctrl Pts',(-25.9451519213283,-13.5440935570377,
114.383697601272)) ;
#170868 = CARTESIAN_POINT('Ctrl Pts',(-25.9686625003595,-13.5531076931393,
114.455307029496)) ;
#170869 = CARTESIAN_POINT('Ctrl Pts',(-25.9921730793908,-13.5621218292409,
114.526916457721)) ;
#170870 = CARTESIAN_POINT('Ctrl Pts',(-25.9183692401459,-13.5621217221104,
114.551147512123)) ;
#170871 = CARTESIAN_POINT('Ctrl Pts',(-25.8445654009011,-13.5621216149798,
114.575378566526)) ;
#170872 = CARTESIAN_POINT('Ctrl Pts',(-25.8210548218699,-13.5531074788782,
114.503769138301)) ;
#170873 = CARTESIAN_POINT('Ctrl Pts',(-25.808372018338,-13.8336246591284,
114.429796254132)) ;
#170874 = CARTESIAN_POINT('Ctrl Pts',(-25.7864435705866,-13.8050124160848,
114.363005742518)) ;
#170875 = CARTESIAN_POINT('Ctrl Pts',(-25.8602474010713,-13.805012516226,
114.338774661433)) ;
#170876 = CARTESIAN_POINT('Ctrl Pts',(-25.934051231556,-13.8050126163672,
114.314543580349)) ;
#170877 = CARTESIAN_POINT('Ctrl Pts',(-25.9559796793074,-13.8336248594109,
114.381334091963)) ;
#170878 = CARTESIAN_POINT('Ctrl Pts',(-25.9779081270588,-13.8622371024545,
114.448124603577)) ;
#170879 = CARTESIAN_POINT('Ctrl Pts',(-25.9041042965741,-13.8622370023133,
114.472355684662)) ;
#170880 = CARTESIAN_POINT('Ctrl Pts',(-25.8303004660894,-13.8622369021721,
114.496586765746)) ;
#170881 = CARTESIAN_POINT('Ctrl Pts',(-25.808372018338,-13.8336246591284,
114.429796254132)) ;
#170882 = CARTESIAN_POINT('Ctrl Pts',(-25.7733597736157,-14.0853767704005,
114.287716933633)) ;
#170883 = CARTESIAN_POINT('Ctrl Pts',(-25.7545765163614,-14.0391458019482,
114.230506164792)) ;
#170884 = CARTESIAN_POINT('Ctrl Pts',(-25.8283803390502,-14.0391458872152,
114.206275059963)) ;
#170885 = CARTESIAN_POINT('Ctrl Pts',(-25.9021841617389,-14.0391459724823,
114.182043955133)) ;
#170886 = CARTESIAN_POINT('Ctrl Pts',(-25.9209674189931,-14.0853769409346,
114.239254723973)) ;
#170887 = CARTESIAN_POINT('Ctrl Pts',(-25.9397506762473,-14.131607909387,
114.296465492813)) ;
#170888 = CARTESIAN_POINT('Ctrl Pts',(-25.8659468535586,-14.1316078241199,
114.320696597643)) ;
#170889 = CARTESIAN_POINT('Ctrl Pts',(-25.7921430308699,-14.1316077388528,
114.344927702473)) ;
#170890 = CARTESIAN_POINT('Ctrl Pts',(-25.7733597736157,-14.0853767704005,
114.287716933633)) ;
#170891 = CARTESIAN_POINT('Ctrl Pts',(-25.7186373576974,-14.2903978532202,
114.085351542632)) ;
#170892 = CARTESIAN_POINT('Ctrl Pts',(-25.7043849358257,-14.2297838798409,
114.041940967275)) ;
#170893 = CARTESIAN_POINT('Ctrl Pts',(-25.7781887527212,-14.2297839428811,
114.0177098448)) ;
#170894 = CARTESIAN_POINT('Ctrl Pts',(-25.8519925696167,-14.2297840059213,
113.993478722325)) ;
#170895 = CARTESIAN_POINT('Ctrl Pts',(-25.8662449914884,-14.2903979793006,
114.036889297682)) ;
#170896 = CARTESIAN_POINT('Ctrl Pts',(-25.8804974133601,-14.3510119526798,
114.080299873038)) ;
#170897 = CARTESIAN_POINT('Ctrl Pts',(-25.8066935964646,-14.3510118896396,
114.104530995513)) ;
#170898 = CARTESIAN_POINT('Ctrl Pts',(-25.7328897795691,-14.3510118265994,
114.128762117988)) ;
#170899 = CARTESIAN_POINT('Ctrl Pts',(-25.7186373576974,-14.2903978532202,
114.085351542632)) ;
#170900 = CARTESIAN_POINT('Ctrl Pts',(-25.6501353567778,-14.430884933304,
113.841453445767)) ;
#170901 = CARTESIAN_POINT('Ctrl Pts',(-25.6413738678537,-14.36037249955,113.814767366167)) ;
#170902 = CARTESIAN_POINT('Ctrl Pts',(-25.7151776811438,-14.3603725370538,
113.790536232711)) ;
#170903 = CARTESIAN_POINT('Ctrl Pts',(-25.7889814944339,-14.3603725745575,
113.766305099254)) ;
#170904 = CARTESIAN_POINT('Ctrl Pts',(-25.797742983358,-14.4308850083114,
113.792991178854)) ;
#170905 = CARTESIAN_POINT('Ctrl Pts',(-25.8065044722821,-14.5013974420654,
113.819677258453)) ;
#170906 = CARTESIAN_POINT('Ctrl Pts',(-25.732700658992,-14.5013974045617,
113.84390839191)) ;
#170907 = CARTESIAN_POINT('Ctrl Pts',(-25.6588968457018,-14.501397367058,
113.868139525366)) ;
#170908 = CARTESIAN_POINT('Ctrl Pts',(-25.6501353567778,-14.430884933304,
113.841453445767)) ;
#170909 = CARTESIAN_POINT('Ctrl Pts',(-25.5722582992266,-14.5000545452193,
113.568712686133)) ;
#170910 = CARTESIAN_POINT('Ctrl Pts',(-25.5696561821823,-14.4246071586731,
113.560787059388)) ;
#170911 = CARTESIAN_POINT('Ctrl Pts',(-25.643459994712,-14.4246071686467,
113.536555923616)) ;
#170912 = CARTESIAN_POINT('Ctrl Pts',(-25.7172638072416,-14.4246071786203,
113.512324787843)) ;
#170913 = CARTESIAN_POINT('Ctrl Pts',(-25.7198659242859,-14.5000545651665,
113.520250414587)) ;
#170914 = CARTESIAN_POINT('Ctrl Pts',(-25.7224680413302,-14.5755019517128,
113.528176041332)) ;
#170915 = CARTESIAN_POINT('Ctrl Pts',(-25.6486642288005,-14.5755019417391,
113.552407177104)) ;
#170916 = CARTESIAN_POINT('Ctrl Pts',(-25.5748604162709,-14.5755019317655,
113.576638312877)) ;
#170917 = CARTESIAN_POINT('Ctrl Pts',(-25.5722582992266,-14.5000545452193,
113.568712686133)) ;
#170918 = CARTESIAN_POINT('Ctrl Pts',(-25.492125647743,-14.4915166284975,
113.289248825608)) ;
#170919 = CARTESIAN_POINT('Ctrl Pts',(-25.4958466642941,-14.4165522893736,
113.300582443476)) ;
#170920 = CARTESIAN_POINT('Ctrl Pts',(-25.5696504784892,-14.4165522733908,
113.276351312775)) ;
#170921 = CARTESIAN_POINT('Ctrl Pts',(-25.6434542926842,-14.4165522574081,
113.252120182075)) ;
#170922 = CARTESIAN_POINT('Ctrl Pts',(-25.6397332761331,-14.491516596532,
113.240786564208)) ;
#170923 = CARTESIAN_POINT('Ctrl Pts',(-25.636012259582,-14.566480935656,113.229452946341)) ;
#170924 = CARTESIAN_POINT('Ctrl Pts',(-25.5622084453869,-14.5664809516387,
113.253684077041)) ;
#170925 = CARTESIAN_POINT('Ctrl Pts',(-25.4884046311919,-14.5664809676215,
113.277915207741)) ;
#170926 = CARTESIAN_POINT('Ctrl Pts',(-25.492125647743,-14.4915166284975,
113.289248825608)) ;
#170927 = CARTESIAN_POINT('Ctrl Pts',(-25.4155369746647,-14.4057133919849,
113.020376417355)) ;
#170928 = CARTESIAN_POINT('Ctrl Pts',(-25.4253474075907,-14.3366264116548,
113.050257414847)) ;
#170929 = CARTESIAN_POINT('Ctrl Pts',(-25.499151226059,-14.3366263740412,
113.026026297163)) ;
#170930 = CARTESIAN_POINT('Ctrl Pts',(-25.5729550445272,-14.3366263364276,
113.001795179478)) ;
#170931 = CARTESIAN_POINT('Ctrl Pts',(-25.5631446116012,-14.4057133167577,
112.971914181986)) ;
#170932 = CARTESIAN_POINT('Ctrl Pts',(-25.5533341786752,-14.4748002970877,
112.942033184493)) ;
#170933 = CARTESIAN_POINT('Ctrl Pts',(-25.479530360207,-14.4748003347014,
112.966264302178)) ;
#170934 = CARTESIAN_POINT('Ctrl Pts',(-25.4057265417387,-14.474800372315,
112.990495419862)) ;
#170935 = CARTESIAN_POINT('Ctrl Pts',(-25.4155369746647,-14.4057133919849,
113.020376417355)) ;
#170936 = CARTESIAN_POINT('Ctrl Pts',(-25.3495488251331,-14.2496052022137,
112.783991163958)) ;
#170937 = CARTESIAN_POINT('Ctrl Pts',(-25.3647136799672,-14.1913134689692,
112.83018086653)) ;
#170938 = CARTESIAN_POINT('Ctrl Pts',(-25.4385175039201,-14.1913134155293,
112.805949765551)) ;
#170939 = CARTESIAN_POINT('Ctrl Pts',(-25.512321327873,-14.1913133620894,
112.781718664571)) ;
#170940 = CARTESIAN_POINT('Ctrl Pts',(-25.4971564730389,-14.2496050953339,
112.735528961999)) ;
#170941 = CARTESIAN_POINT('Ctrl Pts',(-25.4819916182047,-14.3078968285784,
112.689339259427)) ;
#170942 = CARTESIAN_POINT('Ctrl Pts',(-25.4081877942518,-14.3078968820183,
112.713570360406)) ;
#170943 = CARTESIAN_POINT('Ctrl Pts',(-25.3343839702989,-14.3078969354582,
112.737801461386)) ;
#170944 = CARTESIAN_POINT('Ctrl Pts',(-25.3495488251331,-14.2496052022137,
112.783991163958)) ;
#170945 = CARTESIAN_POINT('Ctrl Pts',(-25.2990932542373,-14.0337448610519,
112.594839446854)) ;
#170946 = CARTESIAN_POINT('Ctrl Pts',(-25.3185378072279,-13.9904362158164,
112.654064419341)) ;
#170947 = CARTESIAN_POINT('Ctrl Pts',(-25.3923416376092,-13.9904361538178,
112.629833337941)) ;
#170948 = CARTESIAN_POINT('Ctrl Pts',(-25.4661454679905,-13.9904360918192,
112.605602256542)) ;
#170949 = CARTESIAN_POINT('Ctrl Pts',(-25.4467009149999,-14.0337447370547,
112.546377284055)) ;
#170950 = CARTESIAN_POINT('Ctrl Pts',(-25.4272563620092,-14.0770533822902,
112.487152311568)) ;
#170951 = CARTESIAN_POINT('Ctrl Pts',(-25.353452531628,-14.0770534442888,
112.511383392968)) ;
#170952 = CARTESIAN_POINT('Ctrl Pts',(-25.2796487012467,-14.0770535062874,
112.535614474367)) ;
#170953 = CARTESIAN_POINT('Ctrl Pts',(-25.2990932542373,-14.0337448610519,
112.594839446854)) ;
#170954 = CARTESIAN_POINT('Ctrl Pts',(-25.2686792913389,-13.774289830103,
112.466801754916)) ;
#170955 = CARTESIAN_POINT('Ctrl Pts',(-25.2910092781579,-13.7490307967716,
112.534815293139)) ;
#170956 = CARTESIAN_POINT('Ctrl Pts',(-25.3648131149332,-13.7490307328435,
112.510584231214)) ;
#170957 = CARTESIAN_POINT('Ctrl Pts',(-25.4386169517085,-13.7490306689154,
112.48635316929)) ;
#170958 = CARTESIAN_POINT('Ctrl Pts',(-25.4162869648896,-13.7742897022469,
112.418339631067)) ;
#170959 = CARTESIAN_POINT('Ctrl Pts',(-25.3939569780706,-13.7995487355784,
112.350326092844)) ;
#170960 = CARTESIAN_POINT('Ctrl Pts',(-25.3201531412953,-13.7995487995064,
112.374557154769)) ;
#170961 = CARTESIAN_POINT('Ctrl Pts',(-25.24634930452,-13.7995488634345,112.398788216693)) ;
#170962 = CARTESIAN_POINT('Ctrl Pts',(-25.2686792913389,-13.774289830103,
112.466801754916)) ;
#170963 = CARTESIAN_POINT('Ctrl Pts',(-25.2612500837139,-13.4875484100679,
112.408546039972)) ;
#170964 = CARTESIAN_POINT('Ctrl Pts',(-25.284870016536,-13.4822714043299,
112.480488545396)) ;
#170965 = CARTESIAN_POINT('Ctrl Pts',(-25.3586738590323,-13.4822713469427,
112.456257500897)) ;
#170966 = CARTESIAN_POINT('Ctrl Pts',(-25.4324777015287,-13.4822712895556,
112.432026456398)) ;
#170967 = CARTESIAN_POINT('Ctrl Pts',(-25.4088577687066,-13.4875482952936,
112.360083950974)) ;
#170968 = CARTESIAN_POINT('Ctrl Pts',(-25.3852378358846,-13.4928253010316,
112.28814144555)) ;
#170969 = CARTESIAN_POINT('Ctrl Pts',(-25.3114339933882,-13.4928253584187,
112.312372490049)) ;
#170970 = CARTESIAN_POINT('Ctrl Pts',(-25.2376301508919,-13.4928254158059,
112.336603534548)) ;
#170971 = CARTESIAN_POINT('Ctrl Pts',(-25.2612500837139,-13.4875484100679,
112.408546039972)) ;
#170972 = CARTESIAN_POINT('Ctrl Pts',(-25.2779813826279,-13.1987144632943,
112.424247332912)) ;
#170973 = CARTESIAN_POINT('Ctrl Pts',(-25.3011983723262,-13.2135962190273,
112.494962538468)) ;
#170974 = CARTESIAN_POINT('Ctrl Pts',(-25.3750022191492,-13.2135961694435,
112.470731507147)) ;
#170975 = CARTESIAN_POINT('Ctrl Pts',(-25.4488060659722,-13.2135961198597,
112.446500475826)) ;
#170976 = CARTESIAN_POINT('Ctrl Pts',(-25.4255890762739,-13.1987143641267,
112.375785270271)) ;
#170977 = CARTESIAN_POINT('Ctrl Pts',(-25.4023720865755,-13.1838326083937,
112.305070064715)) ;
#170978 = CARTESIAN_POINT('Ctrl Pts',(-25.3285682397525,-13.1838326579775,
112.329301096036)) ;
#170979 = CARTESIAN_POINT('Ctrl Pts',(-25.2547643929295,-13.1838327075613,
112.353532127357)) ;
#170980 = CARTESIAN_POINT('Ctrl Pts',(-25.2779813826279,-13.1987144632943,
112.424247332912)) ;
#170981 = CARTESIAN_POINT('Ctrl Pts',(-25.3186803797673,-12.9229602452279,
112.512616871207)) ;
#170982 = CARTESIAN_POINT('Ctrl Pts',(-25.3398275683234,-12.9571183444642,
112.577027796252)) ;
#170983 = CARTESIAN_POINT('Ctrl Pts',(-25.4136314177794,-12.9571183085152,
112.552796772951)) ;
#170984 = CARTESIAN_POINT('Ctrl Pts',(-25.4874352672354,-12.9571182725662,
112.528565749649)) ;
#170985 = CARTESIAN_POINT('Ctrl Pts',(-25.4662880786793,-12.9229601733299,
112.464154824605)) ;
#170986 = CARTESIAN_POINT('Ctrl Pts',(-25.4451408901232,-12.8888020740936,
112.399743899561)) ;
#170987 = CARTESIAN_POINT('Ctrl Pts',(-25.3713370406672,-12.8888021100426,
112.423974922862)) ;
#170988 = CARTESIAN_POINT('Ctrl Pts',(-25.2975331912112,-12.8888021459916,
112.448205946163)) ;
#170989 = CARTESIAN_POINT('Ctrl Pts',(-25.3186803797673,-12.9229602452279,
112.512616871207)) ;
#170990 = CARTESIAN_POINT('Ctrl Pts',(-25.3810378795507,-12.6836290013039,
112.667065868669)) ;
#170991 = CARTESIAN_POINT('Ctrl Pts',(-25.3985974186503,-12.7345497889164,
112.720549392164)) ;
#170992 = CARTESIAN_POINT('Ctrl Pts',(-25.4724012689758,-12.7345497658022,
112.696318371512)) ;
#170993 = CARTESIAN_POINT('Ctrl Pts',(-25.5462051193014,-12.734549742688,
112.672087350859)) ;
#170994 = CARTESIAN_POINT('Ctrl Pts',(-25.5286455802018,-12.6836289550754,
112.618603827363)) ;
#170995 = CARTESIAN_POINT('Ctrl Pts',(-25.5110860411021,-12.6327081674629,
112.565120303868)) ;
#170996 = CARTESIAN_POINT('Ctrl Pts',(-25.4372821907766,-12.6327081905771,
112.58935132452)) ;
#170997 = CARTESIAN_POINT('Ctrl Pts',(-25.3634783404511,-12.6327082136913,
112.613582345173)) ;
#170998 = CARTESIAN_POINT('Ctrl Pts',(-25.3810378795507,-12.6836290013039,
112.667065868669)) ;
#170999 = CARTESIAN_POINT('Ctrl Pts',(-25.4612408939245,-12.4971808863818,
112.875902607548)) ;
#171000 = CARTESIAN_POINT('Ctrl Pts',(-25.4739605108467,-12.5611972883497,
112.914644508854)) ;
#171001 = CARTESIAN_POINT('Ctrl Pts',(-25.5477643607026,-12.5611972760957,
112.890413486771)) ;
#171002 = CARTESIAN_POINT('Ctrl Pts',(-25.6215682105584,-12.5611972638417,
112.866182464688)) ;
#171003 = CARTESIAN_POINT('Ctrl Pts',(-25.6088485936362,-12.4971808618738,
112.827440563381)) ;
#171004 = CARTESIAN_POINT('Ctrl Pts',(-25.596128976714,-12.4331644599059,
112.788698662075)) ;
#171005 = CARTESIAN_POINT('Ctrl Pts',(-25.5223251268581,-12.4331644721599,
112.812929684158)) ;
#171006 = CARTESIAN_POINT('Ctrl Pts',(-25.4485212770022,-12.4331644844139,
112.837160706241)) ;
#171007 = CARTESIAN_POINT('Ctrl Pts',(-25.4612408939245,-12.4971808863818,
112.875902607548)) ;
#171008 = CARTESIAN_POINT('Ctrl Pts',(-25.5540720154026,-12.3766482309411,
113.123307400288)) ;
#171009 = CARTESIAN_POINT('Ctrl Pts',(-25.5610604027361,-12.4491772372763,
113.144592900868)) ;
#171010 = CARTESIAN_POINT('Ctrl Pts',(-25.6348642513686,-12.4491772329469,
113.120361875059)) ;
#171011 = CARTESIAN_POINT('Ctrl Pts',(-25.7086681000012,-12.4491772286174,
113.09613084925)) ;
#171012 = CARTESIAN_POINT('Ctrl Pts',(-25.7016797126678,-12.3766482222823,
113.07484534867)) ;
#171013 = CARTESIAN_POINT('Ctrl Pts',(-25.6946913253343,-12.3041192159472,
113.05355984809)) ;
#171014 = CARTESIAN_POINT('Ctrl Pts',(-25.6208874767018,-12.3041192202766,
113.077790873899)) ;
#171015 = CARTESIAN_POINT('Ctrl Pts',(-25.5470836280692,-12.304119224606,
113.102021899709)) ;
#171016 = CARTESIAN_POINT('Ctrl Pts',(-25.5540720154026,-12.3766482309411,
113.123307400288)) ;
#171017 = CARTESIAN_POINT('Ctrl Pts',(-25.6548077636956,-12.3303160635296,
113.394473806366)) ;
#171018 = CARTESIAN_POINT('Ctrl Pts',(-25.6555106525389,-12.406190350598,
113.396614692547)) ;
#171019 = CARTESIAN_POINT('Ctrl Pts',(-25.7293144987663,-12.4061903509704,
113.372383659411)) ;
#171020 = CARTESIAN_POINT('Ctrl Pts',(-25.8031183449935,-12.4061903513427,
113.348152626276)) ;
#171021 = CARTESIAN_POINT('Ctrl Pts',(-25.8024154561502,-12.3303160642744,
113.346011740096)) ;
#171022 = CARTESIAN_POINT('Ctrl Pts',(-25.8017125673069,-12.254441777206,
113.343870853916)) ;
#171023 = CARTESIAN_POINT('Ctrl Pts',(-25.7279087210796,-12.2544417768337,
113.368101887051)) ;
#171024 = CARTESIAN_POINT('Ctrl Pts',(-25.6541048748523,-12.2544417764613,
113.392332920186)) ;
#171025 = CARTESIAN_POINT('Ctrl Pts',(-25.6548077636956,-12.3303160635296,
113.394473806366)) ;
#171026 = CARTESIAN_POINT('Ctrl Pts',(-25.7551087146694,-12.3620878034078,
113.664686262464)) ;
#171027 = CARTESIAN_POINT('Ctrl Pts',(-25.7495393610477,-12.4358572257211,
113.647722910032)) ;
#171028 = CARTESIAN_POINT('Ctrl Pts',(-25.8233432057987,-12.435857227174,
113.6234918724)) ;
#171029 = CARTESIAN_POINT('Ctrl Pts',(-25.8971470505497,-12.4358572286269,
113.599260834769)) ;
#171030 = CARTESIAN_POINT('Ctrl Pts',(-25.9027164041715,-12.3620878063136,
113.616224187201)) ;
#171031 = CARTESIAN_POINT('Ctrl Pts',(-25.9082857577932,-12.2883183840004,
113.633187539633)) ;
#171032 = CARTESIAN_POINT('Ctrl Pts',(-25.8344819130422,-12.2883183825475,
113.657418577265)) ;
#171033 = CARTESIAN_POINT('Ctrl Pts',(-25.7606780682912,-12.2883183810946,
113.681649614896)) ;
#171034 = CARTESIAN_POINT('Ctrl Pts',(-25.7551087146694,-12.3620878034078,
113.664686262464)) ;
#171035 = CARTESIAN_POINT('Ctrl Pts',(-25.8501668503569,-12.4693107333451,
113.918717660534)) ;
#171036 = CARTESIAN_POINT('Ctrl Pts',(-25.8386861551213,-12.5357038324563,
113.883749315246)) ;
#171037 = CARTESIAN_POINT('Ctrl Pts',(-25.9124899984294,-12.5357038327128,
113.859518273219)) ;
#171038 = CARTESIAN_POINT('Ctrl Pts',(-25.9862938417375,-12.5357038329694,
113.835287231193)) ;
#171039 = CARTESIAN_POINT('Ctrl Pts',(-25.9977745369731,-12.4693107338582,
113.87025557648)) ;
#171040 = CARTESIAN_POINT('Ctrl Pts',(-26.0092552322087,-12.402917634747,
113.905223921768)) ;
#171041 = CARTESIAN_POINT('Ctrl Pts',(-25.9354513889006,-12.4029176344904,
113.929454963794)) ;
#171042 = CARTESIAN_POINT('Ctrl Pts',(-25.8616475455925,-12.4029176342339,
113.953686005821)) ;
#171043 = CARTESIAN_POINT('Ctrl Pts',(-25.8501668503569,-12.4693107333451,
113.918717660534)) ;
#171044 = CARTESIAN_POINT('Ctrl Pts',(-25.9334232704776,-12.645191135036,
114.136742805122)) ;
#171045 = CARTESIAN_POINT('Ctrl Pts',(-25.9168475822572,-12.6994019736038,
114.086255933222)) ;
#171046 = CARTESIAN_POINT('Ctrl Pts',(-25.9906514249747,-12.6994019715653,
114.062024889397)) ;
#171047 = CARTESIAN_POINT('Ctrl Pts',(-26.0644552676921,-12.6994019695268,
114.037793845571)) ;
#171048 = CARTESIAN_POINT('Ctrl Pts',(-26.0810309559125,-12.6451911309591,
114.088280717471)) ;
#171049 = CARTESIAN_POINT('Ctrl Pts',(-26.0976066441328,-12.5909802923914,
114.138767589371)) ;
#171050 = CARTESIAN_POINT('Ctrl Pts',(-26.0238028014154,-12.5909802944298,
114.162998633196)) ;
#171051 = CARTESIAN_POINT('Ctrl Pts',(-25.9499989586979,-12.5909802964683,
114.187229677022)) ;
#171052 = CARTESIAN_POINT('Ctrl Pts',(-25.9334232704776,-12.645191135036,
114.136742805122)) ;
#171053 = CARTESIAN_POINT('Ctrl Pts',(-25.999272047211,-12.8761323945115,
114.301835536524)) ;
#171054 = CARTESIAN_POINT('Ctrl Pts',(-25.9788076787168,-12.9142969383445,
114.239504371944)) ;
#171055 = CARTESIAN_POINT('Ctrl Pts',(-26.0526115216438,-12.9142969355883,
114.215273328757)) ;
#171056 = CARTESIAN_POINT('Ctrl Pts',(-26.1264153645708,-12.9142969328321,
114.191042285569)) ;
#171057 = CARTESIAN_POINT('Ctrl Pts',(-26.1468797330649,-12.8761323889991,
114.253373450149)) ;
#171058 = CARTESIAN_POINT('Ctrl Pts',(-26.1673441015591,-12.8379678451661,
114.31570461473)) ;
#171059 = CARTESIAN_POINT('Ctrl Pts',(-26.0935402586321,-12.8379678479223,
114.339935657917)) ;
#171060 = CARTESIAN_POINT('Ctrl Pts',(-26.0197364157051,-12.8379678506785,
114.364166701105)) ;
#171061 = CARTESIAN_POINT('Ctrl Pts',(-25.999272047211,-12.8761323945115,
114.301835536524)) ;
#171062 = CARTESIAN_POINT('Ctrl Pts',(-26.0439639830932,-13.1443073603244,
114.40267311779)) ;
#171063 = CARTESIAN_POINT('Ctrl Pts',(-26.0210791556646,-13.1638021990363,
114.332969625858)) ;
#171064 = CARTESIAN_POINT('Ctrl Pts',(-26.0948829990038,-13.16380219707,114.308738583926)) ;
#171065 = CARTESIAN_POINT('Ctrl Pts',(-26.1686868423429,-13.1638021951038,
114.284507541994)) ;
#171066 = CARTESIAN_POINT('Ctrl Pts',(-26.1915716697714,-13.1443073563919,
114.354211033926)) ;
#171067 = CARTESIAN_POINT('Ctrl Pts',(-26.2144564971999,-13.12481251768,114.423914525858)) ;
#171068 = CARTESIAN_POINT('Ctrl Pts',(-26.1406526538608,-13.1248125196462,
114.44814556779)) ;
#171069 = CARTESIAN_POINT('Ctrl Pts',(-26.0668488105217,-13.1248125216125,
114.472376609722)) ;
#171070 = CARTESIAN_POINT('Ctrl Pts',(-26.0439639830932,-13.1443073603244,
114.40267311779)) ;
#171071 = CARTESIAN_POINT('Ctrl Pts',(-26.0654214447628,-13.4354170804365,
114.432316659204)) ;
#171072 = CARTESIAN_POINT('Ctrl Pts',(-26.0417435519583,-13.4346128293488,
114.360197618186)) ;
#171073 = CARTESIAN_POINT('Ctrl Pts',(-26.1155473954861,-13.4346128319822,
114.335966576829)) ;
#171074 = CARTESIAN_POINT('Ctrl Pts',(-26.189351239014,-13.4346128346157,
114.311735535472)) ;
#171075 = CARTESIAN_POINT('Ctrl Pts',(-26.2130291318185,-13.4354170857033,
114.383854576489)) ;
#171076 = CARTESIAN_POINT('Ctrl Pts',(-26.2367070246231,-13.436221336791,
114.455973617507)) ;
#171077 = CARTESIAN_POINT('Ctrl Pts',(-26.1629031810952,-13.4362213341576,
114.480204658864)) ;
#171078 = CARTESIAN_POINT('Ctrl Pts',(-26.0890993375674,-13.4362213315242,
114.504435700221)) ;
#171079 = CARTESIAN_POINT('Ctrl Pts',(-26.0654214447628,-13.4354170804365,
114.432316659204)) ;
#171080 = CARTESIAN_POINT('Ctrl Pts',(-26.0623510035417,-13.7221366616439,
114.38765243736)) ;
#171081 = CARTESIAN_POINT('Ctrl Pts',(-26.0395838511607,-13.7013113003572,
114.318307364811)) ;
#171082 = CARTESIAN_POINT('Ctrl Pts',(-26.1133876940889,-13.7013113073341,
114.294076321627)) ;
#171083 = CARTESIAN_POINT('Ctrl Pts',(-26.1871915370171,-13.7013113143109,
114.269845278443)) ;
#171084 = CARTESIAN_POINT('Ctrl Pts',(-26.2099586893981,-13.7221366755976,
114.339190350992)) ;
#171085 = CARTESIAN_POINT('Ctrl Pts',(-26.2327258417792,-13.7429620368844,
114.408535423541)) ;
#171086 = CARTESIAN_POINT('Ctrl Pts',(-26.158921998851,-13.7429620299075,
114.432766466724)) ;
#171087 = CARTESIAN_POINT('Ctrl Pts',(-26.0851181559228,-13.7429620229307,
114.456997509908)) ;
#171088 = CARTESIAN_POINT('Ctrl Pts',(-26.0623510035417,-13.7221366616439,
114.38765243736)) ;
#171089 = CARTESIAN_POINT('Ctrl Pts',(-26.0360612678888,-13.9882040306806,
114.272122330666)) ;
#171090 = CARTESIAN_POINT('Ctrl Pts',(-26.0158303614321,-13.948770536174,
114.210502254101)) ;
#171091 = CARTESIAN_POINT('Ctrl Pts',(-26.0896342028091,-13.9487705477941,
114.186271206193)) ;
#171092 = CARTESIAN_POINT('Ctrl Pts',(-26.1634380441861,-13.9487705594142,
114.162040158284)) ;
#171093 = CARTESIAN_POINT('Ctrl Pts',(-26.1836689506428,-13.9882040539209,
114.223660234849)) ;
#171094 = CARTESIAN_POINT('Ctrl Pts',(-26.2038998570996,-14.0276375484275,
114.285280311414)) ;
#171095 = CARTESIAN_POINT('Ctrl Pts',(-26.1300960157226,-14.0276375368073,
114.309511359322)) ;
#171096 = CARTESIAN_POINT('Ctrl Pts',(-26.0562921743456,-14.0276375251872,
114.333742407231)) ;
#171097 = CARTESIAN_POINT('Ctrl Pts',(-26.0360612678888,-13.9882040306806,
114.272122330666)) ;
#171098 = CARTESIAN_POINT('Ctrl Pts',(-25.9891697623435,-14.2132831582582,
114.093901493958)) ;
#171099 = CARTESIAN_POINT('Ctrl Pts',(-25.9729161073915,-14.1580769970448,
114.044395483879)) ;
#171100 = CARTESIAN_POINT('Ctrl Pts',(-26.0467199463987,-14.1580770113055,
114.020164428752)) ;
#171101 = CARTESIAN_POINT('Ctrl Pts',(-26.1205237854058,-14.1580770255661,
113.995933373626)) ;
#171102 = CARTESIAN_POINT('Ctrl Pts',(-26.1367774403579,-14.2132831867795,
114.045439383705)) ;
#171103 = CARTESIAN_POINT('Ctrl Pts',(-26.1530310953099,-14.2684893479928,
114.094945393784)) ;
#171104 = CARTESIAN_POINT('Ctrl Pts',(-26.0792272563027,-14.2684893337322,
114.119176448911)) ;
#171105 = CARTESIAN_POINT('Ctrl Pts',(-26.0054234172956,-14.2684893194715,
114.143407504037)) ;
#171106 = CARTESIAN_POINT('Ctrl Pts',(-25.9891697623435,-14.2132831582582,
114.093901493958)) ;
#171107 = CARTESIAN_POINT('Ctrl Pts',(-25.9251466069735,-14.3825130038358,
113.863210711069)) ;
#171108 = CARTESIAN_POINT('Ctrl Pts',(-25.9140780038205,-14.3154103550948,
113.829497532359)) ;
#171109 = CARTESIAN_POINT('Ctrl Pts',(-25.9878818390175,-14.3154103696642,
113.805266465627)) ;
#171110 = CARTESIAN_POINT('Ctrl Pts',(-26.0616856742145,-14.3154103842335,
113.781035398895)) ;
#171111 = CARTESIAN_POINT('Ctrl Pts',(-26.0727542773675,-14.3825130329745,
113.814748577605)) ;
#171112 = CARTESIAN_POINT('Ctrl Pts',(-26.0838228805205,-14.4496156817154,
113.848461756315)) ;
#171113 = CARTESIAN_POINT('Ctrl Pts',(-26.0100190453235,-14.4496156671461,
113.872692823047)) ;
#171114 = CARTESIAN_POINT('Ctrl Pts',(-25.9362152101265,-14.4496156525767,
113.896923889778)) ;
#171115 = CARTESIAN_POINT('Ctrl Pts',(-25.9251466069735,-14.3825130038358,
113.863210711069)) ;
#171116 = CARTESIAN_POINT('Ctrl Pts',(-25.8506582051535,-14.4810713491466,
113.601065674823)) ;
#171117 = CARTESIAN_POINT('Ctrl Pts',(-25.8455042079974,-14.4069908889082,
113.585367431789)) ;
#171118 = CARTESIAN_POINT('Ctrl Pts',(-25.9193080402583,-14.4069908973545,
113.561136356115)) ;
#171119 = CARTESIAN_POINT('Ctrl Pts',(-25.9931118725193,-14.4069909058008,
113.53690528044)) ;
#171120 = CARTESIAN_POINT('Ctrl Pts',(-25.9982658696754,-14.4810713660392,
113.552603523474)) ;
#171121 = CARTESIAN_POINT('Ctrl Pts',(-26.0034198668315,-14.5551518262776,
113.568301766508)) ;
#171122 = CARTESIAN_POINT('Ctrl Pts',(-25.9296160345705,-14.5551518178313,
113.592532842183)) ;
#171123 = CARTESIAN_POINT('Ctrl Pts',(-25.8558122023096,-14.555151809385,
113.616763917857)) ;
#171124 = CARTESIAN_POINT('Ctrl Pts',(-25.8506582051535,-14.4810713491466,
113.601065674823)) ;
#171125 = CARTESIAN_POINT('Ctrl Pts',(-25.770453573245,-14.5044054817918,
113.321227426534)) ;
#171126 = CARTESIAN_POINT('Ctrl Pts',(-25.7716275560046,-14.4285885279282,
113.324803189491)) ;
#171127 = CARTESIAN_POINT('Ctrl Pts',(-25.8454313850184,-14.4285885262166,
113.300572103926)) ;
#171128 = CARTESIAN_POINT('Ctrl Pts',(-25.9192352140321,-14.4285885245051,
113.276341018362)) ;
#171129 = CARTESIAN_POINT('Ctrl Pts',(-25.9180612312726,-14.5044054783686,
113.272765255405)) ;
#171130 = CARTESIAN_POINT('Ctrl Pts',(-25.9168872485131,-14.5802224322322,
113.269189492448)) ;
#171131 = CARTESIAN_POINT('Ctrl Pts',(-25.8430834194993,-14.5802224339438,
113.293420578013)) ;
#171132 = CARTESIAN_POINT('Ctrl Pts',(-25.7692795904855,-14.5802224356554,
113.317651663578)) ;
#171133 = CARTESIAN_POINT('Ctrl Pts',(-25.770453573245,-14.5044054817918,
113.321227426534)) ;
#171134 = CARTESIAN_POINT('Ctrl Pts',(-25.6917906589482,-14.4496129795719,
113.046187296342)) ;
#171135 = CARTESIAN_POINT('Ctrl Pts',(-25.6991919532336,-14.377512086332,
113.068730445599)) ;
#171136 = CARTESIAN_POINT('Ctrl Pts',(-25.7729957803867,-14.3775120696296,
113.044499354366)) ;
#171137 = CARTESIAN_POINT('Ctrl Pts',(-25.8467996075397,-14.3775120529272,
113.020268263134)) ;
#171138 = CARTESIAN_POINT('Ctrl Pts',(-25.8393983132543,-14.449612946167,
112.997725113878)) ;
#171139 = CARTESIAN_POINT('Ctrl Pts',(-25.8319970189689,-14.5217138394069,
112.975181964621)) ;
#171140 = CARTESIAN_POINT('Ctrl Pts',(-25.7581931918158,-14.5217138561093,
112.999413055854)) ;
#171141 = CARTESIAN_POINT('Ctrl Pts',(-25.6843893646628,-14.5217138728117,
113.023644147086)) ;
#171142 = CARTESIAN_POINT('Ctrl Pts',(-25.6917906589482,-14.4496129795719,
113.046187296342)) ;
#171143 = CARTESIAN_POINT('Ctrl Pts',(-25.6207924323353,-14.3209948065222,
112.79446435437)) ;
#171144 = CARTESIAN_POINT('Ctrl Pts',(-25.6338954260901,-14.2577695417982,
112.83437396041)) ;
#171145 = CARTESIAN_POINT('Ctrl Pts',(-25.7076992529809,-14.257769507085,
112.810142868379)) ;
#171146 = CARTESIAN_POINT('Ctrl Pts',(-25.7815030798717,-14.2577694723718,
112.785911776348)) ;
#171147 = CARTESIAN_POINT('Ctrl Pts',(-25.7684000861169,-14.3209947370958,
112.746002170308)) ;
#171148 = CARTESIAN_POINT('Ctrl Pts',(-25.7552970923621,-14.3842200018198,
112.706092564267)) ;
#171149 = CARTESIAN_POINT('Ctrl Pts',(-25.6814932654713,-14.384220036533,
112.730323656298)) ;
#171150 = CARTESIAN_POINT('Ctrl Pts',(-25.6076894385805,-14.3842200712462,
112.754554748329)) ;
#171151 = CARTESIAN_POINT('Ctrl Pts',(-25.6207924323353,-14.3209948065222,
112.79446435437)) ;
#171152 = CARTESIAN_POINT('Ctrl Pts',(-25.5633709290415,-14.1276267553148,
112.584095959637)) ;
#171153 = CARTESIAN_POINT('Ctrl Pts',(-25.5812359055684,-14.0778104825488,
112.638509797017)) ;
#171154 = CARTESIAN_POINT('Ctrl Pts',(-25.6550397342676,-14.077810428769,
112.614278710494)) ;
#171155 = CARTESIAN_POINT('Ctrl Pts',(-25.7288435629669,-14.0778103749893,
112.590047623971)) ;
#171156 = CARTESIAN_POINT('Ctrl Pts',(-25.71097858644,-14.1276266477552,112.535633786592)) ;
#171157 = CARTESIAN_POINT('Ctrl Pts',(-25.6931136099132,-14.1774429205212,
112.481219949212)) ;
#171158 = CARTESIAN_POINT('Ctrl Pts',(-25.6193097812139,-14.177442974301,
112.505451035735)) ;
#171159 = CARTESIAN_POINT('Ctrl Pts',(-25.5455059525147,-14.1774430280807,
112.529682122257)) ;
#171160 = CARTESIAN_POINT('Ctrl Pts',(-25.5633709290415,-14.1276267553148,
112.584095959637)) ;
#171161 = CARTESIAN_POINT('Ctrl Pts',(-25.5243599004901,-13.88341485216,112.429801042865)) ;
#171162 = CARTESIAN_POINT('Ctrl Pts',(-25.5457084250049,-13.8505765249219,
112.494825205497)) ;
#171163 = CARTESIAN_POINT('Ctrl Pts',(-25.6195122576543,-13.8505764535514,
112.470594131005)) ;
#171164 = CARTESIAN_POINT('Ctrl Pts',(-25.6933160903036,-13.850576382181,
112.446363056514)) ;
#171165 = CARTESIAN_POINT('Ctrl Pts',(-25.6719675657889,-13.8834147094192,
112.381338893882)) ;
#171166 = CARTESIAN_POINT('Ctrl Pts',(-25.6506190412741,-13.9162530366573,
112.31631473125)) ;
#171167 = CARTESIAN_POINT('Ctrl Pts',(-25.5768152086248,-13.9162531080278,
112.340545805741)) ;
#171168 = CARTESIAN_POINT('Ctrl Pts',(-25.5030113759754,-13.9162531793982,
112.364776880233)) ;
#171169 = CARTESIAN_POINT('Ctrl Pts',(-25.5243599004901,-13.88341485216,112.429801042865)) ;
#171170 = CARTESIAN_POINT('Ctrl Pts',(-25.5073970747293,-13.605636693064,
112.342636129513)) ;
#171171 = CARTESIAN_POINT('Ctrl Pts',(-25.5306954589167,-13.5921442428259,
112.413599250237)) ;
#171172 = CARTESIAN_POINT('Ctrl Pts',(-25.6044992975363,-13.5921441578331,
112.38936819393)) ;
#171173 = CARTESIAN_POINT('Ctrl Pts',(-25.6783031361559,-13.5921440728403,
112.365137137623)) ;
#171174 = CARTESIAN_POINT('Ctrl Pts',(-25.6550047519685,-13.6056365230784,
112.294174016899)) ;
#171175 = CARTESIAN_POINT('Ctrl Pts',(-25.631706367781,-13.6191289733166,
112.223210896175)) ;
#171176 = CARTESIAN_POINT('Ctrl Pts',(-25.5579025291614,-13.6191290583094,
112.247441952482)) ;
#171177 = CARTESIAN_POINT('Ctrl Pts',(-25.4840986905419,-13.6191291433021,
112.271673008789)) ;
#171178 = CARTESIAN_POINT('Ctrl Pts',(-25.5073970747293,-13.605636693064,
112.342636129513)) ;
#171179 = CARTESIAN_POINT('Ctrl Pts',(-25.5142052747166,-13.3159385103922,
112.328067762604)) ;
#171180 = CARTESIAN_POINT('Ctrl Pts',(-25.5377925942813,-13.3226522577716,
112.399910933968)) ;
#171181 = CARTESIAN_POINT('Ctrl Pts',(-25.6115964402047,-13.3226521665054,
112.375679899907)) ;
#171182 = CARTESIAN_POINT('Ctrl Pts',(-25.685400286128,-13.3226520752392,
112.351448865846)) ;
#171183 = CARTESIAN_POINT('Ctrl Pts',(-25.6618129665633,-13.3159383278597,
112.279605694482)) ;
#171184 = CARTESIAN_POINT('Ctrl Pts',(-25.6382256469986,-13.3092245804803,
112.207762523118)) ;
#171185 = CARTESIAN_POINT('Ctrl Pts',(-25.5644218010753,-13.3092246717465,
112.231993557178)) ;
#171186 = CARTESIAN_POINT('Ctrl Pts',(-25.4906179551519,-13.3092247630127,
112.256224591239)) ;
#171187 = CARTESIAN_POINT('Ctrl Pts',(-25.5142052747166,-13.3159385103922,
112.328067762604)) ;
#171188 = CARTESIAN_POINT('Ctrl Pts',(-25.5456617971205,-13.0300093756574,
112.388107483979)) ;
#171189 = CARTESIAN_POINT('Ctrl Pts',(-25.5678278490325,-13.0566953178852,
112.45562170353)) ;
#171190 = CARTESIAN_POINT('Ctrl Pts',(-25.6416317032956,-13.0566952256386,
112.43139069487)) ;
#171191 = CARTESIAN_POINT('Ctrl Pts',(-25.7154355575587,-13.0566951333921,
112.407159686211)) ;
#171192 = CARTESIAN_POINT('Ctrl Pts',(-25.6932695056467,-13.0300091911643,
112.33964546666)) ;
#171193 = CARTESIAN_POINT('Ctrl Pts',(-25.6711034537346,-13.0033232489365,
112.27213124711)) ;
#171194 = CARTESIAN_POINT('Ctrl Pts',(-25.5972995994715,-13.003323341183,
112.296362255769)) ;
#171195 = CARTESIAN_POINT('Ctrl Pts',(-25.5234957452084,-13.0033234334296,
112.320593264428)) ;
#171196 = CARTESIAN_POINT('Ctrl Pts',(-25.5456617971205,-13.0300093756574,
112.388107483979)) ;
#171197 = CARTESIAN_POINT('Ctrl Pts',(-25.5990739293158,-12.7764992730081,
112.515654295035)) ;
#171198 = CARTESIAN_POINT('Ctrl Pts',(-25.6182700989793,-12.820923286975,
112.574122732496)) ;
#171199 = CARTESIAN_POINT('Ctrl Pts',(-25.6920739609603,-12.8209232050731,
112.549891747345)) ;
#171200 = CARTESIAN_POINT('Ctrl Pts',(-25.7658778229413,-12.8209231231712,
112.525660762193)) ;
#171201 = CARTESIAN_POINT('Ctrl Pts',(-25.7466816532778,-12.7764991092043,
112.467192324731)) ;
#171202 = CARTESIAN_POINT('Ctrl Pts',(-25.7274854836142,-12.7320750952375,
112.40872388727)) ;
#171203 = CARTESIAN_POINT('Ctrl Pts',(-25.6536816216332,-12.7320751771394,
112.432954872422)) ;
#171204 = CARTESIAN_POINT('Ctrl Pts',(-25.5798777596522,-12.7320752590413,
112.457185857574)) ;
#171205 = CARTESIAN_POINT('Ctrl Pts',(-25.5990739293158,-12.7764992730081,
112.515654295035)) ;
#171206 = CARTESIAN_POINT('Ctrl Pts',(-25.6727778832843,-12.5655360581605,
112.704525516889)) ;
#171207 = CARTESIAN_POINT('Ctrl Pts',(-25.6875936661384,-12.6247539701097,
112.749652002979)) ;
#171208 = CARTESIAN_POINT('Ctrl Pts',(-25.7613975352215,-12.6247539044987,
112.725421039459)) ;
#171209 = CARTESIAN_POINT('Ctrl Pts',(-25.8352014043047,-12.6247538388877,
112.701190075939)) ;
#171210 = CARTESIAN_POINT('Ctrl Pts',(-25.8203856214506,-12.5655359269385,
112.656063589849)) ;
#171211 = CARTESIAN_POINT('Ctrl Pts',(-25.8055698385965,-12.5063180149893,
112.610937103759)) ;
#171212 = CARTESIAN_POINT('Ctrl Pts',(-25.7317659695133,-12.5063180806004,
112.635168067279)) ;
#171213 = CARTESIAN_POINT('Ctrl Pts',(-25.6579621004302,-12.5063181462114,
112.659399030798)) ;
#171214 = CARTESIAN_POINT('Ctrl Pts',(-25.6727778832843,-12.5655360581605,
112.704525516889)) ;
#171215 = CARTESIAN_POINT('Ctrl Pts',(-25.7612652883096,-12.4169761529621,
112.938629023383)) ;
#171216 = CARTESIAN_POINT('Ctrl Pts',(-25.7706577740588,-12.4866530449287,
112.967237021576)) ;
#171217 = CARTESIAN_POINT('Ctrl Pts',(-25.8444616482445,-12.4866530028469,
112.943006073598)) ;
#171218 = CARTESIAN_POINT('Ctrl Pts',(-25.9182655224302,-12.4866529607651,
112.91877512562)) ;
#171219 = CARTESIAN_POINT('Ctrl Pts',(-25.908873036681,-12.4169760687985,
112.890167127427)) ;
#171220 = CARTESIAN_POINT('Ctrl Pts',(-25.8994805509318,-12.3472991768318,
112.861559129234)) ;
#171221 = CARTESIAN_POINT('Ctrl Pts',(-25.8256766767461,-12.3472992189136,
112.885790077212)) ;
#171222 = CARTESIAN_POINT('Ctrl Pts',(-25.7518728025604,-12.3472992609954,
112.91002102519)) ;
#171223 = CARTESIAN_POINT('Ctrl Pts',(-25.7612652883096,-12.4169761529621,
112.938629023383)) ;
#171224 = CARTESIAN_POINT('Ctrl Pts',(-25.8595188377888,-12.339692635442,
113.20236799913)) ;
#171225 = CARTESIAN_POINT('Ctrl Pts',(-25.8628006300689,-12.4148681964576,
113.212363810995)) ;
#171226 = CARTESIAN_POINT('Ctrl Pts',(-25.9366045069881,-12.4148681820189,
113.188132871343)) ;
#171227 = CARTESIAN_POINT('Ctrl Pts',(-26.0104083839073,-12.4148681675802,
113.16390193169)) ;
#171228 = CARTESIAN_POINT('Ctrl Pts',(-26.0071265916272,-12.3396926065646,
113.153906119825)) ;
#171229 = CARTESIAN_POINT('Ctrl Pts',(-26.0038447993471,-12.264517045549,
113.14391030796)) ;
#171230 = CARTESIAN_POINT('Ctrl Pts',(-25.9300409224279,-12.2645170599877,
113.168141247613)) ;
#171231 = CARTESIAN_POINT('Ctrl Pts',(-25.8562370455087,-12.2645170744263,
113.192372187265)) ;
#171232 = CARTESIAN_POINT('Ctrl Pts',(-25.8595188377888,-12.339692635442,
113.20236799913)) ;
#171233 = CARTESIAN_POINT('Ctrl Pts',(-25.9607682026483,-12.3399218128255,
113.475325729361)) ;
#171234 = CARTESIAN_POINT('Ctrl Pts',(-25.9577191084769,-12.4151926619622,
113.466038682576)) ;
#171235 = CARTESIAN_POINT('Ctrl Pts',(-26.0315229853345,-12.4151926765907,
113.441807742736)) ;
#171236 = CARTESIAN_POINT('Ctrl Pts',(-26.1053268621922,-12.4151926912192,
113.417576802896)) ;
#171237 = CARTESIAN_POINT('Ctrl Pts',(-26.1083759563636,-12.3399218420826,
113.426863849681)) ;
#171238 = CARTESIAN_POINT('Ctrl Pts',(-26.1114250505351,-12.2646509929459,
113.436150896466)) ;
#171239 = CARTESIAN_POINT('Ctrl Pts',(-26.0376211736774,-12.2646509783174,
113.460381836306)) ;
#171240 = CARTESIAN_POINT('Ctrl Pts',(-25.9638172968198,-12.2646509636889,
113.484612776146)) ;
#171241 = CARTESIAN_POINT('Ctrl Pts',(-25.9607682026483,-12.3399218128255,
113.475325729361)) ;
#171242 = CARTESIAN_POINT('Ctrl Pts',(-26.0587509812645,-12.4170982893213,
113.738337027537)) ;
#171243 = CARTESIAN_POINT('Ctrl Pts',(-26.0495896106153,-12.4870926783877,
113.710432972791)) ;
#171244 = CARTESIAN_POINT('Ctrl Pts',(-26.1233934847273,-12.4870927205449,
113.686202024588)) ;
#171245 = CARTESIAN_POINT('Ctrl Pts',(-26.1971973588393,-12.4870927627021,
113.661971076385)) ;
#171246 = CARTESIAN_POINT('Ctrl Pts',(-26.2063587294884,-12.4170983736357,
113.689875131132)) ;
#171247 = CARTESIAN_POINT('Ctrl Pts',(-26.2155201001376,-12.3471039845693,
113.717779185878)) ;
#171248 = CARTESIAN_POINT('Ctrl Pts',(-26.1417162260256,-12.3471039424121,
113.742010134081)) ;
#171249 = CARTESIAN_POINT('Ctrl Pts',(-26.0679123519136,-12.3471039002549,
113.766241082284)) ;
#171250 = CARTESIAN_POINT('Ctrl Pts',(-26.0587509812645,-12.4170982893213,
113.738337027537)) ;
#171251 = CARTESIAN_POINT('Ctrl Pts',(-26.1473630413061,-12.5661915214183,
113.972745351393)) ;
#171252 = CARTESIAN_POINT('Ctrl Pts',(-26.1327357424787,-12.6258811352282,
113.928192961293)) ;
#171253 = CARTESIAN_POINT('Ctrl Pts',(-26.2065396113906,-12.6258812005672,
113.903961997252)) ;
#171254 = CARTESIAN_POINT('Ctrl Pts',(-26.2803434803025,-12.6258812659061,
113.879731033211)) ;
#171255 = CARTESIAN_POINT('Ctrl Pts',(-26.2949707791298,-12.5661916520963,
113.92428342331)) ;
#171256 = CARTESIAN_POINT('Ctrl Pts',(-26.3095980779572,-12.5065020382865,
113.968835813409)) ;
#171257 = CARTESIAN_POINT('Ctrl Pts',(-26.2357942090453,-12.5065019729475,
113.993066777451)) ;
#171258 = CARTESIAN_POINT('Ctrl Pts',(-26.1619903401334,-12.5065019076085,
114.017297741492)) ;
#171259 = CARTESIAN_POINT('Ctrl Pts',(-26.1473630413061,-12.5661915214183,
113.972745351393)) ;
#171260 = CARTESIAN_POINT('Ctrl Pts',(-26.2207601261338,-12.7760910985915,
114.160853377573)) ;
#171261 = CARTESIAN_POINT('Ctrl Pts',(-26.2017200658351,-12.8212153371298,
114.102860427963)) ;
#171262 = CARTESIAN_POINT('Ctrl Pts',(-26.2755239277867,-12.8212154191497,
114.078629442721)) ;
#171263 = CARTESIAN_POINT('Ctrl Pts',(-26.3493277897383,-12.8212155011696,
114.05439845748)) ;
#171264 = CARTESIAN_POINT('Ctrl Pts',(-26.368367850037,-12.7760912626314,
114.11239140709)) ;
#171265 = CARTESIAN_POINT('Ctrl Pts',(-26.3874079103356,-12.7309670240931,
114.1703843567)) ;
#171266 = CARTESIAN_POINT('Ctrl Pts',(-26.3136040483841,-12.7309669420732,
114.194615341941)) ;
#171267 = CARTESIAN_POINT('Ctrl Pts',(-26.2398001864325,-12.7309668600532,
114.218846327183)) ;
#171268 = CARTESIAN_POINT('Ctrl Pts',(-26.2207601261338,-12.7760910985915,
114.160853377573)) ;
#171269 = CARTESIAN_POINT('Ctrl Pts',(-26.274697438766,-13.0327329322163,
114.289584630443)) ;
#171270 = CARTESIAN_POINT('Ctrl Pts',(-26.2525986608536,-13.0600070239695,
114.222275320409)) ;
#171271 = CARTESIAN_POINT('Ctrl Pts',(-26.3264025147417,-13.0600071142797,
114.198044310608)) ;
#171272 = CARTESIAN_POINT('Ctrl Pts',(-26.4002063686298,-13.0600072045899,
114.173813300806)) ;
#171273 = CARTESIAN_POINT('Ctrl Pts',(-26.4223051465423,-13.0327331128366,
114.241122610841)) ;
#171274 = CARTESIAN_POINT('Ctrl Pts',(-26.4444039244547,-13.0054590210833,
114.308431920875)) ;
#171275 = CARTESIAN_POINT('Ctrl Pts',(-26.3706000705666,-13.0054589307732,
114.332662930677)) ;
#171276 = CARTESIAN_POINT('Ctrl Pts',(-26.2967962166784,-13.005458840463,
114.356893940478)) ;
#171277 = CARTESIAN_POINT('Ctrl Pts',(-26.274697438766,-13.0327329322163,
114.289584630443)) ;
#171278 = CARTESIAN_POINT('Ctrl Pts',(-26.3056984325726,-13.3169814944794,
114.34847609993)) ;
#171279 = CARTESIAN_POINT('Ctrl Pts',(-26.2821371567087,-13.3244510016564,
114.276712256991)) ;
#171280 = CARTESIAN_POINT('Ctrl Pts',(-26.3559410025772,-13.3244510916003,
114.252481222763)) ;
#171281 = CARTESIAN_POINT('Ctrl Pts',(-26.4297448484457,-13.3244511815443,
114.228250188535)) ;
#171282 = CARTESIAN_POINT('Ctrl Pts',(-26.4533061243096,-13.3169816743673,
114.300014031474)) ;
#171283 = CARTESIAN_POINT('Ctrl Pts',(-26.4768674001734,-13.3095121671903,
114.371777874413)) ;
#171284 = CARTESIAN_POINT('Ctrl Pts',(-26.4030635543049,-13.3095120772463,
114.396008908641)) ;
#171285 = CARTESIAN_POINT('Ctrl Pts',(-26.3292597084365,-13.3095119873024,
114.420239942869)) ;
#171286 = CARTESIAN_POINT('Ctrl Pts',(-26.3056984325726,-13.3169814944794,
114.34847609993)) ;
#171287 = CARTESIAN_POINT('Ctrl Pts',(-26.3125024381578,-13.6065319682423,
114.333907323218)) ;
#171288 = CARTESIAN_POINT('Ctrl Pts',(-26.2891610497531,-13.593796615994,
114.262813221903)) ;
#171289 = CARTESIAN_POINT('Ctrl Pts',(-26.3629648883744,-13.5937966997554,
114.238582165601)) ;
#171290 = CARTESIAN_POINT('Ctrl Pts',(-26.4367687269956,-13.5937967835168,
114.214351109299)) ;
#171291 = CARTESIAN_POINT('Ctrl Pts',(-26.4601101154003,-13.6065321357651,
114.285445210614)) ;
#171292 = CARTESIAN_POINT('Ctrl Pts',(-26.483451503805,-13.6192674880133,
114.35653931193)) ;
#171293 = CARTESIAN_POINT('Ctrl Pts',(-26.4096476651838,-13.6192674042519,
114.380770368232)) ;
#171294 = CARTESIAN_POINT('Ctrl Pts',(-26.3358438265625,-13.6192673204905,
114.405001424534)) ;
#171295 = CARTESIAN_POINT('Ctrl Pts',(-26.3125024381578,-13.6065319682423,
114.333907323218)) ;
#171296 = CARTESIAN_POINT('Ctrl Pts',(-26.2953957023122,-13.8845186470045,
114.246262443011)) ;
#171297 = CARTESIAN_POINT('Ctrl Pts',(-26.2739487735497,-13.8523553116745,
114.180938559947)) ;
#171298 = CARTESIAN_POINT('Ctrl Pts',(-26.3477526064039,-13.852355381399,
114.156707486079)) ;
#171299 = CARTESIAN_POINT('Ctrl Pts',(-26.4215564392581,-13.8523554511235,
114.132476412212)) ;
#171300 = CARTESIAN_POINT('Ctrl Pts',(-26.4430033680206,-13.8845187864536,
114.197800295276)) ;
#171301 = CARTESIAN_POINT('Ctrl Pts',(-26.464450296783,-13.9166821217837,
114.263124178339)) ;
#171302 = CARTESIAN_POINT('Ctrl Pts',(-26.3906464639288,-13.9166820520591,
114.287355252207)) ;
#171303 = CARTESIAN_POINT('Ctrl Pts',(-26.3168426310747,-13.9166819823346,
114.311586326074)) ;
#171304 = CARTESIAN_POINT('Ctrl Pts',(-26.2953957023122,-13.8845186470045,
114.246262443011)) ;
#171305 = CARTESIAN_POINT('Ctrl Pts',(-26.2564785433818,-14.1277890814299,
114.092378152371)) ;
#171306 = CARTESIAN_POINT('Ctrl Pts',(-26.2384479066427,-14.0785921493268,
114.037459743464)) ;
#171307 = CARTESIAN_POINT('Ctrl Pts',(-26.3122517354857,-14.0785922024829,
114.013228657379)) ;
#171308 = CARTESIAN_POINT('Ctrl Pts',(-26.3860555643286,-14.0785922556391,
113.988997571294)) ;
#171309 = CARTESIAN_POINT('Ctrl Pts',(-26.4040862010677,-14.1277891877422,
114.043915980201)) ;
#171310 = CARTESIAN_POINT('Ctrl Pts',(-26.4221168378068,-14.1769861198453,
114.098834389108)) ;
#171311 = CARTESIAN_POINT('Ctrl Pts',(-26.3483130089639,-14.1769860666892,
114.123065475193)) ;
#171312 = CARTESIAN_POINT('Ctrl Pts',(-26.2745091801209,-14.1769860135331,
114.147296561278)) ;
#171313 = CARTESIAN_POINT('Ctrl Pts',(-26.2564785433818,-14.1277890814299,
114.092378152371)) ;
#171314 = CARTESIAN_POINT('Ctrl Pts',(-26.1989157065957,-14.3214999944636,
113.88150015982)) ;
#171315 = CARTESIAN_POINT('Ctrl Pts',(-26.1856123717527,-14.2587034430882,
113.840980349568)) ;
#171316 = CARTESIAN_POINT('Ctrl Pts',(-26.2594161990129,-14.2587034768352,
113.816749258662)) ;
#171317 = CARTESIAN_POINT('Ctrl Pts',(-26.3332200262729,-14.2587035105822,
113.792518167755)) ;
#171318 = CARTESIAN_POINT('Ctrl Pts',(-26.3465233611159,-14.3215000619577,
113.833037978008)) ;
#171319 = CARTESIAN_POINT('Ctrl Pts',(-26.3598266959589,-14.3842966133332,
113.873557788261)) ;
#171320 = CARTESIAN_POINT('Ctrl Pts',(-26.2860228686988,-14.3842965795861,
113.897788879167)) ;
#171321 = CARTESIAN_POINT('Ctrl Pts',(-26.2122190414387,-14.3842965458391,
113.922019970073)) ;
#171322 = CARTESIAN_POINT('Ctrl Pts',(-26.1989157065957,-14.3214999944636,
113.88150015982)) ;
#171323 = CARTESIAN_POINT('Ctrl Pts',(-26.1278964756566,-14.4499114443817,
113.629724275749)) ;
#171324 = CARTESIAN_POINT('Ctrl Pts',(-26.1202654228016,-14.3780538242765,
113.606481321047)) ;
#171325 = CARTESIAN_POINT('Ctrl Pts',(-26.1940692503916,-14.37805384036,113.582250231146)) ;
#171326 = CARTESIAN_POINT('Ctrl Pts',(-26.2678730779816,-14.3780538564435,
113.558019141244)) ;
#171327 = CARTESIAN_POINT('Ctrl Pts',(-26.2755041308367,-14.4499114765488,
113.581262095946)) ;
#171328 = CARTESIAN_POINT('Ctrl Pts',(-26.2831351836917,-14.521769096654,
113.604505050649)) ;
#171329 = CARTESIAN_POINT('Ctrl Pts',(-26.2093313561017,-14.5217690805705,
113.62873614055)) ;
#171330 = CARTESIAN_POINT('Ctrl Pts',(-26.1355275285117,-14.521769064487,
113.652967230451)) ;
#171331 = CARTESIAN_POINT('Ctrl Pts',(-26.1278964756566,-14.4499114443817,
113.629724275749)) ;
#171332 = CARTESIAN_POINT('Ctrl Pts',(-26.0490886415224,-14.5043711676863,
113.354180073168)) ;
#171333 = CARTESIAN_POINT('Ctrl Pts',(-26.0476832870499,-14.4286019200682,
113.34989959105)) ;
#171334 = CARTESIAN_POINT('Ctrl Pts',(-26.1214871167149,-14.4286019216996,
113.325668507468)) ;
#171335 = CARTESIAN_POINT('Ctrl Pts',(-26.1952909463798,-14.4286019233309,
113.301437423887)) ;
#171336 = CARTESIAN_POINT('Ctrl Pts',(-26.1966963008522,-14.504371170949,
113.305717906005)) ;
#171337 = CARTESIAN_POINT('Ctrl Pts',(-26.1981016553247,-14.5801404185671,
113.309998388123)) ;
#171338 = CARTESIAN_POINT('Ctrl Pts',(-26.1242978256598,-14.5801404169357,
113.334229471704)) ;
#171339 = CARTESIAN_POINT('Ctrl Pts',(-26.0504939959948,-14.5801404153043,
113.358460555286)) ;
#171340 = CARTESIAN_POINT('Ctrl Pts',(-26.0490886415224,-14.5043711676863,
113.354180073168)) ;
#171341 = CARTESIAN_POINT('Ctrl Pts',(-25.9693316672278,-14.481209763182,
113.075913353523)) ;
#171342 = CARTESIAN_POINT('Ctrl Pts',(-25.9742242882722,-14.4069431255803,
113.090815488511)) ;
#171343 = CARTESIAN_POINT('Ctrl Pts',(-26.0480281205744,-14.4069431170847,
113.066584412962)) ;
#171344 = CARTESIAN_POINT('Ctrl Pts',(-26.1218319528766,-14.4069431085892,
113.042353337413)) ;
#171345 = CARTESIAN_POINT('Ctrl Pts',(-26.1169393318322,-14.4812097461908,
113.027451202425)) ;
#171346 = CARTESIAN_POINT('Ctrl Pts',(-26.1120467107878,-14.5554763837924,
113.012549067438)) ;
#171347 = CARTESIAN_POINT('Ctrl Pts',(-26.0382428784855,-14.555476392288,
113.036780142987)) ;
#171348 = CARTESIAN_POINT('Ctrl Pts',(-25.9644390461833,-14.5554764007836,
113.061011218535)) ;
#171349 = CARTESIAN_POINT('Ctrl Pts',(-25.9693316672278,-14.481209763182,
113.075913353523)) ;
#171350 = CARTESIAN_POINT('Ctrl Pts',(-25.8943302897143,-14.3816923411007,
112.811938342538)) ;
#171351 = CARTESIAN_POINT('Ctrl Pts',(-25.9052024989069,-14.3142615616255,
112.845053338047)) ;
#171352 = CARTESIAN_POINT('Ctrl Pts',(-25.9790063348074,-14.3142615481585,
112.820822273458)) ;
#171353 = CARTESIAN_POINT('Ctrl Pts',(-26.052810170708,-14.3142615346915,
112.796591208869)) ;
#171354 = CARTESIAN_POINT('Ctrl Pts',(-26.0419379615153,-14.3816923141668,
112.76347621336)) ;
#171355 = CARTESIAN_POINT('Ctrl Pts',(-26.0310657523227,-14.449123093642,
112.730361217852)) ;
#171356 = CARTESIAN_POINT('Ctrl Pts',(-25.9572619164222,-14.449123107109,
112.754592282441)) ;
#171357 = CARTESIAN_POINT('Ctrl Pts',(-25.8834580805216,-14.4491231205759,
112.778823347029)) ;
#171358 = CARTESIAN_POINT('Ctrl Pts',(-25.8943302897143,-14.3816923411007,
112.811938342538)) ;
#171359 = CARTESIAN_POINT('Ctrl Pts',(-25.8307713706495,-14.2134896291755,
112.582919254125)) ;
#171360 = CARTESIAN_POINT('Ctrl Pts',(-25.8468311156039,-14.1577013578714,
112.63183464641)) ;
#171361 = CARTESIAN_POINT('Ctrl Pts',(-25.9206349546597,-14.1577013437741,
112.607603591431)) ;
#171362 = CARTESIAN_POINT('Ctrl Pts',(-25.9944387937155,-14.1577013296769,
112.583372536453)) ;
#171363 = CARTESIAN_POINT('Ctrl Pts',(-25.9783790487612,-14.2134896009809,
112.534457144168)) ;
#171364 = CARTESIAN_POINT('Ctrl Pts',(-25.9623193038068,-14.269277872285,
112.485541751884)) ;
#171365 = CARTESIAN_POINT('Ctrl Pts',(-25.888515464751,-14.2692778863823,
112.509772806863)) ;
#171366 = CARTESIAN_POINT('Ctrl Pts',(-25.8147116256952,-14.2692779004795,
112.534003861841)) ;
#171367 = CARTESIAN_POINT('Ctrl Pts',(-25.8307713706495,-14.2134896291755,
112.582919254125)) ;
#171368 = CARTESIAN_POINT('Ctrl Pts',(-25.7835794301014,-13.9864989351748,
112.403492770186)) ;
#171369 = CARTESIAN_POINT('Ctrl Pts',(-25.8036973649584,-13.9464758835493,
112.464768753956)) ;
#171370 = CARTESIAN_POINT('Ctrl Pts',(-25.8775012067237,-13.9464758738248,
112.440537707231)) ;
#171371 = CARTESIAN_POINT('Ctrl Pts',(-25.9513050484891,-13.9464758641003,
112.416306660505)) ;
#171372 = CARTESIAN_POINT('Ctrl Pts',(-25.9311871136321,-13.9864989157259,
112.355030676735)) ;
#171373 = CARTESIAN_POINT('Ctrl Pts',(-25.9110691787752,-14.0265219673515,
112.293754692964)) ;
#171374 = CARTESIAN_POINT('Ctrl Pts',(-25.8372653370098,-14.0265219770759,
112.31798573969)) ;
#171375 = CARTESIAN_POINT('Ctrl Pts',(-25.7634614952445,-14.0265219868004,
112.342216786415)) ;
#171376 = CARTESIAN_POINT('Ctrl Pts',(-25.7835794301014,-13.9864989351748,
112.403492770186)) ;
#171377 = CARTESIAN_POINT('Ctrl Pts',(-25.7575024369132,-13.7220237261921,
112.288851169171)) ;
#171378 = CARTESIAN_POINT('Ctrl Pts',(-25.780200037052,-13.7004075787871,
112.357984397076)) ;
#171379 = CARTESIAN_POINT('Ctrl Pts',(-25.8540038800281,-13.7004075723778,
112.333753354038)) ;
#171380 = CARTESIAN_POINT('Ctrl Pts',(-25.9278077230041,-13.7004075659685,
112.309522311)) ;
#171381 = CARTESIAN_POINT('Ctrl Pts',(-25.9051101228652,-13.7220237133736,
112.240389083094)) ;
#171382 = CARTESIAN_POINT('Ctrl Pts',(-25.8824125227264,-13.7436398607786,
112.171255855189)) ;
#171383 = CARTESIAN_POINT('Ctrl Pts',(-25.8086086797504,-13.7436398671878,
112.195486898227)) ;
#171384 = CARTESIAN_POINT('Ctrl Pts',(-25.7348048367744,-13.7436398735971,
112.219717941265)) ;
#171385 = CARTESIAN_POINT('Ctrl Pts',(-25.7575024369132,-13.7220237261921,
112.288851169171)) ;
#171386 = CARTESIAN_POINT('Ctrl Pts',(-25.7546020971339,-13.4322464163541,
112.244321998672)) ;
#171387 = CARTESIAN_POINT('Ctrl Pts',(-25.7782752222252,-13.4308324436495,
112.316426518066)) ;
#171388 = CARTESIAN_POINT('Ctrl Pts',(-25.8520790657583,-13.4308324430486,
112.292195476725)) ;
#171389 = CARTESIAN_POINT('Ctrl Pts',(-25.9258829092914,-13.4308324424476,
112.267964435384)) ;
#171390 = CARTESIAN_POINT('Ctrl Pts',(-25.9022097842002,-13.4322464151522,
112.195859915989)) ;
#171391 = CARTESIAN_POINT('Ctrl Pts',(-25.878536659109,-13.4336603878567,
112.123755396595)) ;
#171392 = CARTESIAN_POINT('Ctrl Pts',(-25.8047328155758,-13.4336603884577,
112.147986437936)) ;
#171393 = CARTESIAN_POINT('Ctrl Pts',(-25.7309289720427,-13.4336603890586,
112.172217479278)) ;
#171394 = CARTESIAN_POINT('Ctrl Pts',(-25.7546020971339,-13.4322464163541,
112.244321998672)) ;
#171395 = CARTESIAN_POINT('Ctrl Pts',(-25.7758240368022,-13.1452897052538,
112.273770028607)) ;
#171396 = CARTESIAN_POINT('Ctrl Pts',(-25.7987787120654,-13.1639105046461,
112.343686265702)) ;
#171397 = CARTESIAN_POINT('Ctrl Pts',(-25.8725825553839,-13.1639105064164,
112.319455223707)) ;
#171398 = CARTESIAN_POINT('Ctrl Pts',(-25.9463863987024,-13.1639105081867,
112.295224181712)) ;
#171399 = CARTESIAN_POINT('Ctrl Pts',(-25.9234317234392,-13.1452897087944,
112.225307944617)) ;
#171400 = CARTESIAN_POINT('Ctrl Pts',(-25.900477048176,-13.1266689094021,
112.155391707523)) ;
#171401 = CARTESIAN_POINT('Ctrl Pts',(-25.8266732048575,-13.1266689076317,
112.179622749518)) ;
#171402 = CARTESIAN_POINT('Ctrl Pts',(-25.752869361539,-13.1266689058614,
112.203853791513)) ;
#171403 = CARTESIAN_POINT('Ctrl Pts',(-25.7758240368022,-13.1452897052538,
112.273770028607)) ;
#171404 = CARTESIAN_POINT('Ctrl Pts',(-25.821130261938,-12.8735307541799,
112.375991971865)) ;
#171405 = CARTESIAN_POINT('Ctrl Pts',(-25.8416958911711,-12.9111570713961,
112.438631560189)) ;
#171406 = CARTESIAN_POINT('Ctrl Pts',(-25.9154997340476,-12.9111570744422,
112.414400516848)) ;
#171407 = CARTESIAN_POINT('Ctrl Pts',(-25.989303576924,-12.9111570774884,
112.390169473506)) ;
#171408 = CARTESIAN_POINT('Ctrl Pts',(-25.9687379476908,-12.8735307602723,
112.327529885182)) ;
#171409 = CARTESIAN_POINT('Ctrl Pts',(-25.9481723184577,-12.8359044430562,
112.264890296858)) ;
#171410 = CARTESIAN_POINT('Ctrl Pts',(-25.8743684755813,-12.83590444001,112.289121340199)) ;
#171411 = CARTESIAN_POINT('Ctrl Pts',(-25.8005646327049,-12.8359044369638,
112.31335238354)) ;
#171412 = CARTESIAN_POINT('Ctrl Pts',(-25.821130261938,-12.8735307541799,
112.375991971865)) ;
#171413 = CARTESIAN_POINT('Ctrl Pts',(-25.8866884207212,-12.6449175335016,
112.54048346263)) ;
#171414 = CARTESIAN_POINT('Ctrl Pts',(-25.9034346718771,-12.6985622170396,
112.591489841605)) ;
#171415 = CARTESIAN_POINT('Ctrl Pts',(-25.9772385146951,-12.698562218704,
112.567258798085)) ;
#171416 = CARTESIAN_POINT('Ctrl Pts',(-26.0510423575131,-12.6985622203683,
112.543027754566)) ;
#171417 = CARTESIAN_POINT('Ctrl Pts',(-26.0342961063572,-12.6449175368303,
112.492021375591)) ;
#171418 = CARTESIAN_POINT('Ctrl Pts',(-26.0175498552012,-12.5912728532923,
112.441014996616)) ;
#171419 = CARTESIAN_POINT('Ctrl Pts',(-25.9437460123832,-12.5912728516279,
112.465246040135)) ;
#171420 = CARTESIAN_POINT('Ctrl Pts',(-25.8699421695653,-12.5912728499636,
112.489477083655)) ;
#171421 = CARTESIAN_POINT('Ctrl Pts',(-25.8866884207212,-12.6449175335016,
112.54048346263)) ;
#171422 = CARTESIAN_POINT('Ctrl Pts',(-25.9697390448969,-12.4692026417619,
112.757943207403)) ;
#171423 = CARTESIAN_POINT('Ctrl Pts',(-25.9814453819459,-12.5351960145383,
112.793598821244)) ;
#171424 = CARTESIAN_POINT('Ctrl Pts',(-26.0552492253081,-12.5351960141678,
112.769367779382)) ;
#171425 = CARTESIAN_POINT('Ctrl Pts',(-26.1290530686703,-12.5351960137972,
112.74513673752)) ;
#171426 = CARTESIAN_POINT('Ctrl Pts',(-26.1173467316213,-12.4692026410208,
112.709481123679)) ;
#171427 = CARTESIAN_POINT('Ctrl Pts',(-26.1056403945723,-12.4032092682444,
112.673825509837)) ;
#171428 = CARTESIAN_POINT('Ctrl Pts',(-26.0318365512101,-12.4032092686149,
112.698056551699)) ;
#171429 = CARTESIAN_POINT('Ctrl Pts',(-25.9580327078479,-12.4032092689855,
112.722287593561)) ;
#171430 = CARTESIAN_POINT('Ctrl Pts',(-25.9697390448969,-12.4692026417619,
112.757943207403)) ;
#171431 = CARTESIAN_POINT('Ctrl Pts',(-26.0651797901007,-12.3617390442732,
113.013009958698)) ;
#171432 = CARTESIAN_POINT('Ctrl Pts',(-26.0709763080344,-12.4353332114667,
113.030665217169)) ;
#171433 = CARTESIAN_POINT('Ctrl Pts',(-26.1447801531298,-12.4353332096564,
113.006434180586)) ;
#171434 = CARTESIAN_POINT('Ctrl Pts',(-26.2185839982252,-12.4353332078462,
112.982203144004)) ;
#171435 = CARTESIAN_POINT('Ctrl Pts',(-26.2127874802915,-12.3617390406526,
112.964547885532)) ;
#171436 = CARTESIAN_POINT('Ctrl Pts',(-26.2069909623578,-12.2881448734591,
112.946892627061)) ;
#171437 = CARTESIAN_POINT('Ctrl Pts',(-26.1331871172624,-12.2881448752694,
112.971123663643)) ;
#171438 = CARTESIAN_POINT('Ctrl Pts',(-26.059383272167,-12.2881448770796,
112.995354700226)) ;
#171439 = CARTESIAN_POINT('Ctrl Pts',(-26.0651797901007,-12.3617390442732,
113.013009958698)) ;
#171440 = CARTESIAN_POINT('Ctrl Pts',(-26.1654275204562,-12.3304471936261,
113.283082395496)) ;
#171441 = CARTESIAN_POINT('Ctrl Pts',(-26.1649626053493,-12.4063328156575,
113.281666339294)) ;
#171442 = CARTESIAN_POINT('Ctrl Pts',(-26.2387664519881,-12.4063328154178,
113.257435307412)) ;
#171443 = CARTESIAN_POINT('Ctrl Pts',(-26.3125702986269,-12.4063328151781,
113.23320427553)) ;
#171444 = CARTESIAN_POINT('Ctrl Pts',(-26.3130352137339,-12.3304471931467,
113.234620331733)) ;
#171445 = CARTESIAN_POINT('Ctrl Pts',(-26.3135001288408,-12.2545615711153,
113.236036387935)) ;
#171446 = CARTESIAN_POINT('Ctrl Pts',(-26.239696282202,-12.254561571355,113.260267419817)) ;
#171447 = CARTESIAN_POINT('Ctrl Pts',(-26.1658924355632,-12.2545615715947,
113.284498451699)) ;
#171448 = CARTESIAN_POINT('Ctrl Pts',(-26.1654275204562,-12.3304471936261,
113.283082395496)) ;
#171449 = CARTESIAN_POINT('Ctrl Pts',(-26.2657660829558,-12.376595059269,
113.553179153048)) ;
#171450 = CARTESIAN_POINT('Ctrl Pts',(-26.2590295101417,-12.4493688880087,
113.532660639538)) ;
#171451 = CARTESIAN_POINT('Ctrl Pts',(-26.3328333588651,-12.4493688924278,
113.508429614006)) ;
#171452 = CARTESIAN_POINT('Ctrl Pts',(-26.4066372075886,-12.4493688968469,
113.484198588473)) ;
#171453 = CARTESIAN_POINT('Ctrl Pts',(-26.4133737804027,-12.3765950681072,
113.504717101983)) ;
#171454 = CARTESIAN_POINT('Ctrl Pts',(-26.4201103532167,-12.3038212393674,
113.525235615492)) ;
#171455 = CARTESIAN_POINT('Ctrl Pts',(-26.3463065044933,-12.3038212349483,
113.549466641025)) ;
#171456 = CARTESIAN_POINT('Ctrl Pts',(-26.2725026557699,-12.3038212305292,
113.573697666557)) ;
#171457 = CARTESIAN_POINT('Ctrl Pts',(-26.2657660829558,-12.376595059269,
113.553179153048)) ;
#171458 = CARTESIAN_POINT('Ctrl Pts',(-26.359065116246,-12.4977240769561,
113.801833331804)) ;
#171459 = CARTESIAN_POINT('Ctrl Pts',(-26.3465394344376,-12.5621460088863,
113.763682126528)) ;
#171460 = CARTESIAN_POINT('Ctrl Pts',(-26.4203432848208,-12.5621460220276,
113.73945110605)) ;
#171461 = CARTESIAN_POINT('Ctrl Pts',(-26.4941471352039,-12.5621460351689,
113.715220085573)) ;
#171462 = CARTESIAN_POINT('Ctrl Pts',(-26.5066728170123,-12.4977241032387,
113.753371290849)) ;
#171463 = CARTESIAN_POINT('Ctrl Pts',(-26.5191984988206,-12.4333021713085,
113.791522496126)) ;
#171464 = CARTESIAN_POINT('Ctrl Pts',(-26.4453946484375,-12.4333021581672,
113.815753516603)) ;
#171465 = CARTESIAN_POINT('Ctrl Pts',(-26.3715907980544,-12.4333021450259,
113.83998453708)) ;
#171466 = CARTESIAN_POINT('Ctrl Pts',(-26.359065116246,-12.4977240769561,
113.801833331804)) ;
#171467 = CARTESIAN_POINT('Ctrl Pts',(-26.4393585568978,-12.6852356935121,
114.010845608305)) ;
#171468 = CARTESIAN_POINT('Ctrl Pts',(-26.4219441286147,-12.736658719336,
113.95780407024)) ;
#171469 = CARTESIAN_POINT('Ctrl Pts',(-26.4957479795408,-12.7366587448055,
113.933573051417)) ;
#171470 = CARTESIAN_POINT('Ctrl Pts',(-26.569551830467,-12.7366587702751,
113.909342032593)) ;
#171471 = CARTESIAN_POINT('Ctrl Pts',(-26.58696625875,-12.6852357444512,113.962383570658)) ;
#171472 = CARTESIAN_POINT('Ctrl Pts',(-26.6043806870331,-12.6338127186274,
114.015425108723)) ;
#171473 = CARTESIAN_POINT('Ctrl Pts',(-26.530576836107,-12.6338126931579,
114.039656127546)) ;
#171474 = CARTESIAN_POINT('Ctrl Pts',(-26.4567729851808,-12.6338126676883,
114.063887146369)) ;
#171475 = CARTESIAN_POINT('Ctrl Pts',(-26.4393585568978,-12.6852356935121,
114.010845608305)) ;
#171476 = CARTESIAN_POINT('Ctrl Pts',(-26.5012600267756,-12.9233901911912,
114.164108379881)) ;
#171477 = CARTESIAN_POINT('Ctrl Pts',(-26.4802286428052,-12.9582592987456,
114.100050178518)) ;
#171478 = CARTESIAN_POINT('Ctrl Pts',(-26.5540324923643,-12.958259335733,
114.075819155531)) ;
#171479 = CARTESIAN_POINT('Ctrl Pts',(-26.6278363419234,-12.9582593727203,
114.051588132544)) ;
#171480 = CARTESIAN_POINT('Ctrl Pts',(-26.6488677258939,-12.9233902651659,
114.115646333907)) ;
#171481 = CARTESIAN_POINT('Ctrl Pts',(-26.6698991098643,-12.8885211576114,
114.17970453527)) ;
#171482 = CARTESIAN_POINT('Ctrl Pts',(-26.5960952603051,-12.8885211206241,
114.203935558257)) ;
#171483 = CARTESIAN_POINT('Ctrl Pts',(-26.522291410746,-12.8885210836367,
114.228166581244)) ;
#171484 = CARTESIAN_POINT('Ctrl Pts',(-26.5012600267756,-12.9233901911912,
114.164108379881)) ;
#171485 = CARTESIAN_POINT('Ctrl Pts',(-26.5420541011494,-13.1995574427629,
114.252712502089)) ;
#171486 = CARTESIAN_POINT('Ctrl Pts',(-26.5188815950457,-13.2151953803477,
114.18213278838)) ;
#171487 = CARTESIAN_POINT('Ctrl Pts',(-26.5926854420113,-13.2151954315295,
114.157901757494)) ;
#171488 = CARTESIAN_POINT('Ctrl Pts',(-26.6664892889769,-13.2151954827113,
114.133670726607)) ;
#171489 = CARTESIAN_POINT('Ctrl Pts',(-26.6896617950807,-13.1995575451265,
114.204250440316)) ;
#171490 = CARTESIAN_POINT('Ctrl Pts',(-26.7128343011844,-13.1839196075417,
114.274830154024)) ;
#171491 = CARTESIAN_POINT('Ctrl Pts',(-26.6390304542188,-13.1839195563599,
114.299061184911)) ;
#171492 = CARTESIAN_POINT('Ctrl Pts',(-26.5652266072531,-13.1839195051781,
114.323292215797)) ;
#171493 = CARTESIAN_POINT('Ctrl Pts',(-26.5420541011494,-13.1995574427629,
114.252712502089)) ;
#171494 = CARTESIAN_POINT('Ctrl Pts',(-26.5586624454798,-13.4900175633602,
114.267844947108)) ;
#171495 = CARTESIAN_POINT('Ctrl Pts',(-26.5350304987127,-13.4853985697917,
114.195865851433)) ;
#171496 = CARTESIAN_POINT('Ctrl Pts',(-26.6088343410563,-13.4853986306042,
114.171634806468)) ;
#171497 = CARTESIAN_POINT('Ctrl Pts',(-26.6826381833999,-13.4853986914167,
114.147403761504)) ;
#171498 = CARTESIAN_POINT('Ctrl Pts',(-26.706270130167,-13.4900176849852,
114.219382857179)) ;
#171499 = CARTESIAN_POINT('Ctrl Pts',(-26.7299020769341,-13.4946366785538,
114.291361952854)) ;
#171500 = CARTESIAN_POINT('Ctrl Pts',(-26.6560982345905,-13.4946366177413,
114.315592997819)) ;
#171501 = CARTESIAN_POINT('Ctrl Pts',(-26.5822943922469,-13.4946365569288,
114.339824042783)) ;
#171502 = CARTESIAN_POINT('Ctrl Pts',(-26.5586624454798,-13.4900175633602,
114.267844947108)) ;
#171503 = CARTESIAN_POINT('Ctrl Pts',(-26.5511685763042,-13.7743854626431,
114.209679423832)) ;
#171504 = CARTESIAN_POINT('Ctrl Pts',(-26.5287570348701,-13.7499058485971,
114.141417486027)) ;
#171505 = CARTESIAN_POINT('Ctrl Pts',(-26.6025608715152,-13.7499059130724,
114.117186423706)) ;
#171506 = CARTESIAN_POINT('Ctrl Pts',(-26.6763647081602,-13.7499059775478,
114.092955361385)) ;
#171507 = CARTESIAN_POINT('Ctrl Pts',(-26.6987762495943,-13.7743855915938,
114.161217299189)) ;
#171508 = CARTESIAN_POINT('Ctrl Pts',(-26.7211877910284,-13.7988652056398,
114.229479236994)) ;
#171509 = CARTESIAN_POINT('Ctrl Pts',(-26.6473839543834,-13.7988651411644,
114.253710299315)) ;
#171510 = CARTESIAN_POINT('Ctrl Pts',(-26.5735801177383,-13.7988650766891,
114.277941361636)) ;
#171511 = CARTESIAN_POINT('Ctrl Pts',(-26.5511685763042,-13.7743854626431,
114.209679423832)) ;
#171512 = CARTESIAN_POINT('Ctrl Pts',(-26.5207255627321,-14.034295085312,
114.081488551575)) ;
#171513 = CARTESIAN_POINT('Ctrl Pts',(-26.5011408734775,-13.9916338194208,
114.021836749551)) ;
#171514 = CARTESIAN_POINT('Ctrl Pts',(-26.5749447036413,-13.9916338823601,
113.997605667489)) ;
#171515 = CARTESIAN_POINT('Ctrl Pts',(-26.648748533805,-13.9916339452994,
113.973374585426)) ;
#171516 = CARTESIAN_POINT('Ctrl Pts',(-26.6683332230596,-14.0342952111906,
114.033026387451)) ;
#171517 = CARTESIAN_POINT('Ctrl Pts',(-26.6879179123141,-14.0769564770818,
114.092678189475)) ;
#171518 = CARTESIAN_POINT('Ctrl Pts',(-26.6141140821504,-14.0769564141425,
114.116909271537)) ;
#171519 = CARTESIAN_POINT('Ctrl Pts',(-26.5403102519867,-14.0769563512032,
114.141140353599)) ;
#171520 = CARTESIAN_POINT('Ctrl Pts',(-26.5207255627321,-14.034295085312,
114.081488551575)) ;
#171521 = CARTESIAN_POINT('Ctrl Pts',(-26.4702129616919,-14.2500983716934,
113.892161270726)) ;
#171522 = CARTESIAN_POINT('Ctrl Pts',(-26.4548605002029,-14.1923084690493,
113.84540015175)) ;
#171523 = CARTESIAN_POINT('Ctrl Pts',(-26.5286643238617,-14.1923085231576,
113.821169049876)) ;
#171524 = CARTESIAN_POINT('Ctrl Pts',(-26.6024681475206,-14.192308577266,
113.796937948001)) ;
#171525 = CARTESIAN_POINT('Ctrl Pts',(-26.6178206090096,-14.2500984799102,
113.843699066976)) ;
#171526 = CARTESIAN_POINT('Ctrl Pts',(-26.6331730704987,-14.3078883825543,
113.890460185952)) ;
#171527 = CARTESIAN_POINT('Ctrl Pts',(-26.5593692468399,-14.307888328446,
113.914691287827)) ;
#171528 = CARTESIAN_POINT('Ctrl Pts',(-26.485565423181,-14.3078882743376,
113.938922389702)) ;
#171529 = CARTESIAN_POINT('Ctrl Pts',(-26.4702129616919,-14.2500983716934,
113.892161270726)) ;
#171530 = CARTESIAN_POINT('Ctrl Pts',(-26.4040228817349,-14.4061684747286,
113.655081180054)) ;
#171531 = CARTESIAN_POINT('Ctrl Pts',(-26.3940033136551,-14.3373982174877,
113.62456319407)) ;
#171532 = CARTESIAN_POINT('Ctrl Pts',(-26.467807131676,-14.3373982554781,
113.600332075023)) ;
#171533 = CARTESIAN_POINT('Ctrl Pts',(-26.5416109496969,-14.3373982934686,
113.576100955976)) ;
#171534 = CARTESIAN_POINT('Ctrl Pts',(-26.5516305177767,-14.4061685507095,
113.606618941959)) ;
#171535 = CARTESIAN_POINT('Ctrl Pts',(-26.5616500858565,-14.4749388079505,
113.637136927943)) ;
#171536 = CARTESIAN_POINT('Ctrl Pts',(-26.4878462678356,-14.47493876996,113.66136804699)) ;
#171537 = CARTESIAN_POINT('Ctrl Pts',(-26.4140424498147,-14.4749387319696,
113.685599166037)) ;
#171538 = CARTESIAN_POINT('Ctrl Pts',(-26.4040228817349,-14.4061684747286,
113.655081180054)) ;
#171539 = CARTESIAN_POINT('Ctrl Pts',(-26.3278700224272,-14.4915146282391,
113.3877465935)) ;
#171540 = CARTESIAN_POINT('Ctrl Pts',(-26.323884778629,-14.4166858315879,
113.375608185746)) ;
#171541 = CARTESIAN_POINT('Ctrl Pts',(-26.3976885927888,-14.4166858475525,
113.351377054938)) ;
#171542 = CARTESIAN_POINT('Ctrl Pts',(-26.4714924069487,-14.4166858635172,
113.327145924131)) ;
#171543 = CARTESIAN_POINT('Ctrl Pts',(-26.4754776507469,-14.4915146601683,
113.339284331886)) ;
#171544 = CARTESIAN_POINT('Ctrl Pts',(-26.4794628945451,-14.5663434568195,
113.351422739641)) ;
#171545 = CARTESIAN_POINT('Ctrl Pts',(-26.4056590803852,-14.5663434408549,
113.375653870448)) ;
#171546 = CARTESIAN_POINT('Ctrl Pts',(-26.3318552662254,-14.5663434248902,
113.399885001255)) ;
#171547 = CARTESIAN_POINT('Ctrl Pts',(-26.3278700224272,-14.4915146282391,
113.3877465935)) ;
#171548 = CARTESIAN_POINT('Ctrl Pts',(-26.2471359022358,-14.4998611303634,
113.106175912195)) ;
#171549 = CARTESIAN_POINT('Ctrl Pts',(-26.249519313875,-14.4243396117057,
113.113435401435)) ;
#171550 = CARTESIAN_POINT('Ctrl Pts',(-26.3233231259959,-14.4243396013487,
113.089204264417)) ;
#171551 = CARTESIAN_POINT('Ctrl Pts',(-26.3971269381168,-14.4243395909917,
113.0649731274)) ;
#171552 = CARTESIAN_POINT('Ctrl Pts',(-26.3947435264776,-14.4998611096494,
113.05771363816)) ;
#171553 = CARTESIAN_POINT('Ctrl Pts',(-26.3923601148385,-14.5753826283071,
113.05045414892)) ;
#171554 = CARTESIAN_POINT('Ctrl Pts',(-26.3185563027175,-14.5753826386642,
113.074685285938)) ;
#171555 = CARTESIAN_POINT('Ctrl Pts',(-26.2447524905966,-14.5753826490212,
113.098916422955)) ;
#171556 = CARTESIAN_POINT('Ctrl Pts',(-26.2471359022358,-14.4998611303634,
113.106175912195)) ;
#171557 = CARTESIAN_POINT('Ctrl Pts',(-26.1698468947087,-14.4309678249663,
112.835496447081)) ;
#171558 = CARTESIAN_POINT('Ctrl Pts',(-26.1783596457039,-14.3601461164253,
112.861424915088)) ;
#171559 = CARTESIAN_POINT('Ctrl Pts',(-26.2521634589948,-14.3601460788116,
112.837193781634)) ;
#171560 = CARTESIAN_POINT('Ctrl Pts',(-26.3259672722857,-14.3601460411978,
112.81296264818)) ;
#171561 = CARTESIAN_POINT('Ctrl Pts',(-26.3174545212904,-14.4309677497388,
112.787034180173)) ;
#171562 = CARTESIAN_POINT('Ctrl Pts',(-26.3089417702951,-14.5017894582798,
112.761105712166)) ;
#171563 = CARTESIAN_POINT('Ctrl Pts',(-26.2351379570042,-14.5017894958936,
112.78533684562)) ;
#171564 = CARTESIAN_POINT('Ctrl Pts',(-26.1613341437133,-14.5017895335074,
112.809567979074)) ;
#171565 = CARTESIAN_POINT('Ctrl Pts',(-26.1698468947087,-14.4309678249663,
112.835496447081)) ;
#171566 = CARTESIAN_POINT('Ctrl Pts',(-26.1008946624863,-14.2895356443573,
112.589987356344)) ;
#171567 = CARTESIAN_POINT('Ctrl Pts',(-26.114968245912,-14.2284839799428,
112.632853222754)) ;
#171568 = CARTESIAN_POINT('Ctrl Pts',(-26.1887720626717,-14.228483916303,
112.608622099865)) ;
#171569 = CARTESIAN_POINT('Ctrl Pts',(-26.2625758794314,-14.2284838526632,
112.584390976976)) ;
#171570 = CARTESIAN_POINT('Ctrl Pts',(-26.2485022960057,-14.2895355170776,
112.541525110567)) ;
#171571 = CARTESIAN_POINT('Ctrl Pts',(-26.2344287125799,-14.3505871814921,
112.498659244158)) ;
#171572 = CARTESIAN_POINT('Ctrl Pts',(-26.1606248958203,-14.3505872451319,
112.522890367047)) ;
#171573 = CARTESIAN_POINT('Ctrl Pts',(-26.0868210790606,-14.3505873087717,
112.547121489935)) ;
#171574 = CARTESIAN_POINT('Ctrl Pts',(-26.1008946624863,-14.2895356443573,
112.589987356344)) ;
#171575 = CARTESIAN_POINT('Ctrl Pts',(-26.0464820576728,-14.0847982621001,
112.388687807396)) ;
#171576 = CARTESIAN_POINT('Ctrl Pts',(-26.065111268296,-14.0379502045981,
112.445429379231)) ;
#171577 = CARTESIAN_POINT('Ctrl Pts',(-26.1389150910251,-14.0379501191932,
112.421198274525)) ;
#171578 = CARTESIAN_POINT('Ctrl Pts',(-26.2127189137541,-14.0379500337882,
112.396967169818)) ;
#171579 = CARTESIAN_POINT('Ctrl Pts',(-26.1940897031309,-14.0847980912902,
112.340225597982)) ;
#171580 = CARTESIAN_POINT('Ctrl Pts',(-26.1754604925076,-14.1316461487922,
112.283484026146)) ;
#171581 = CARTESIAN_POINT('Ctrl Pts',(-26.1016566697786,-14.1316462341972,
112.307715130853)) ;
#171582 = CARTESIAN_POINT('Ctrl Pts',(-26.0278528470495,-14.1316463196022,
112.33194623556)) ;
#171583 = CARTESIAN_POINT('Ctrl Pts',(-26.0464820576728,-14.0847982621001,
112.388687807396)) ;
#171584 = CARTESIAN_POINT('Ctrl Pts',(-26.0114557448713,-13.8335759567493,
112.246624845677)) ;
#171585 = CARTESIAN_POINT('Ctrl Pts',(-26.0332898940312,-13.8041981863265,
112.313128143188)) ;
#171586 = CARTESIAN_POINT('Ctrl Pts',(-26.1070937245407,-13.8041980860306,
112.288897062179)) ;
#171587 = CARTESIAN_POINT('Ctrl Pts',(-26.1808975550502,-13.8041979857347,
112.26466598117)) ;
#171588 = CARTESIAN_POINT('Ctrl Pts',(-26.1590634058903,-13.8335757561575,
112.198162683659)) ;
#171589 = CARTESIAN_POINT('Ctrl Pts',(-26.1372292567303,-13.8629535265802,
112.131659386148)) ;
#171590 = CARTESIAN_POINT('Ctrl Pts',(-26.0634254262208,-13.8629536268761,
112.155890467157)) ;
#171591 = CARTESIAN_POINT('Ctrl Pts',(-25.9896215957114,-13.8629537271721,
112.180121548166)) ;
#171592 = CARTESIAN_POINT('Ctrl Pts',(-26.0114557448713,-13.8335759567493,
112.246624845677)) ;
#171593 = CARTESIAN_POINT('Ctrl Pts',(-25.9988451272596,-13.5504534645936,
112.172558837349)) ;
#171594 = CARTESIAN_POINT('Ctrl Pts',(-26.0223300636128,-13.5407982837148,
112.244090166275)) ;
#171595 = CARTESIAN_POINT('Ctrl Pts',(-26.0961339029924,-13.540798177125,
112.219859112283)) ;
#171596 = CARTESIAN_POINT('Ctrl Pts',(-26.1699377423721,-13.5407980705352,
112.195628058292)) ;
#171597 = CARTESIAN_POINT('Ctrl Pts',(-26.1464528060189,-13.5504532514139,
112.124096729365)) ;
#171598 = CARTESIAN_POINT('Ctrl Pts',(-26.1229678696658,-13.5601084322927,
112.052565400439)) ;
#171599 = CARTESIAN_POINT('Ctrl Pts',(-26.0491640302861,-13.5601085388825,
112.076796454431)) ;
#171600 = CARTESIAN_POINT('Ctrl Pts',(-25.9753601909065,-13.5601086454724,
112.101027508423)) ;
#171601 = CARTESIAN_POINT('Ctrl Pts',(-25.9988451272596,-13.5504534645936,
112.172558837349)) ;
#171602 = CARTESIAN_POINT('Ctrl Pts',(-26.0103230578241,-13.261274370137,
112.172300104021)) ;
#171603 = CARTESIAN_POINT('Ctrl Pts',(-26.0337701125521,-13.2717947138784,
112.2437160516)) ;
#171604 = CARTESIAN_POINT('Ctrl Pts',(-26.107573960794,-13.2717946091373,
112.219485024601)) ;
#171605 = CARTESIAN_POINT('Ctrl Pts',(-26.1813778090358,-13.2717945043963,
112.195253997602)) ;
#171606 = CARTESIAN_POINT('Ctrl Pts',(-26.1579307543078,-13.2612741606549,
112.123838050023)) ;
#171607 = CARTESIAN_POINT('Ctrl Pts',(-26.1344836995798,-13.2507538169135,
112.052422102443)) ;
#171608 = CARTESIAN_POINT('Ctrl Pts',(-26.060679851338,-13.2507539216545,
112.076653129442)) ;
#171609 = CARTESIAN_POINT('Ctrl Pts',(-25.9868760030961,-13.2507540263956,
112.100884156441)) ;
#171610 = CARTESIAN_POINT('Ctrl Pts',(-26.0103230578241,-13.261274370137,
112.172300104021)) ;
#171611 = CARTESIAN_POINT('Ctrl Pts',(-26.045879708841,-12.9807689853667,
112.245060234104)) ;
#171612 = CARTESIAN_POINT('Ctrl Pts',(-26.0676147705679,-13.0108889686765,
112.31126172717)) ;
#171613 = CARTESIAN_POINT('Ctrl Pts',(-26.1414186269613,-13.0108888747282,
112.287030724999)) ;
#171614 = CARTESIAN_POINT('Ctrl Pts',(-26.2152224833546,-13.0108887807799,
112.262799722828)) ;
#171615 = CARTESIAN_POINT('Ctrl Pts',(-26.1934874216277,-12.9807687974702,
112.196598229762)) ;
#171616 = CARTESIAN_POINT('Ctrl Pts',(-26.1717523599008,-12.9506488141604,
112.130396736695)) ;
#171617 = CARTESIAN_POINT('Ctrl Pts',(-26.0979485035075,-12.9506489081087,
112.154627738866)) ;
#171618 = CARTESIAN_POINT('Ctrl Pts',(-26.0241446471141,-12.950649002057,
112.178858741037)) ;
#171619 = CARTESIAN_POINT('Ctrl Pts',(-26.045879708841,-12.9807689853667,
112.245060234104)) ;
#171620 = CARTESIAN_POINT('Ctrl Pts',(-26.1036567739015,-12.7323944980461,
112.385605838434)) ;
#171621 = CARTESIAN_POINT('Ctrl Pts',(-26.1221237155167,-12.7799004526929,
112.441853164873)) ;
#171622 = CARTESIAN_POINT('Ctrl Pts',(-26.195927578452,-12.7799003762679,
112.417622182628)) ;
#171623 = CARTESIAN_POINT('Ctrl Pts',(-26.2697314413873,-12.7799002998429,
112.393391200382)) ;
#171624 = CARTESIAN_POINT('Ctrl Pts',(-26.2512644997721,-12.7323943451961,
112.337143873943)) ;
#171625 = CARTESIAN_POINT('Ctrl Pts',(-26.2327975581568,-12.6848883905494,
112.280896547504)) ;
#171626 = CARTESIAN_POINT('Ctrl Pts',(-26.1589936952215,-12.6848884669744,
112.305127529749)) ;
#171627 = CARTESIAN_POINT('Ctrl Pts',(-26.0851898322863,-12.6848885433994,
112.329358511994)) ;
#171628 = CARTESIAN_POINT('Ctrl Pts',(-26.1036567739015,-12.7323944980461,
112.385605838434)) ;
#171629 = CARTESIAN_POINT('Ctrl Pts',(-26.1804617683959,-12.5325218808407,
112.58401318597)) ;
#171630 = CARTESIAN_POINT('Ctrl Pts',(-26.1943293123753,-12.594053905958,
112.626251489216)) ;
#171631 = CARTESIAN_POINT('Ctrl Pts',(-26.2681331796008,-12.5940538521665,
112.602020520038)) ;
#171632 = CARTESIAN_POINT('Ctrl Pts',(-26.3419370468262,-12.594053798375,
112.57778955086)) ;
#171633 = CARTESIAN_POINT('Ctrl Pts',(-26.3280695028469,-12.5325217732577,
112.535551247613)) ;
#171634 = CARTESIAN_POINT('Ctrl Pts',(-26.3142019588674,-12.4709897481403,
112.493312944367)) ;
#171635 = CARTESIAN_POINT('Ctrl Pts',(-26.240398091642,-12.4709898019318,
112.517543913545)) ;
#171636 = CARTESIAN_POINT('Ctrl Pts',(-26.1665942244165,-12.4709898557234,
112.541774882723)) ;
#171637 = CARTESIAN_POINT('Ctrl Pts',(-26.1804617683959,-12.5325218808407,
112.58401318597)) ;
#171638 = CARTESIAN_POINT('Ctrl Pts',(-26.2714753234597,-12.3964669498525,
112.825699877311)) ;
#171639 = CARTESIAN_POINT('Ctrl Pts',(-26.2797444860816,-12.4675909509527,
112.850886414112)) ;
#171640 = CARTESIAN_POINT('Ctrl Pts',(-26.3535483549948,-12.4675909216126,
112.826655450075)) ;
#171641 = CARTESIAN_POINT('Ctrl Pts',(-26.427352223908,-12.4675908922725,
112.802424486037)) ;
#171642 = CARTESIAN_POINT('Ctrl Pts',(-26.4190830612861,-12.3964668911723,
112.777237949236)) ;
#171643 = CARTESIAN_POINT('Ctrl Pts',(-26.4108138986641,-12.3253428900721,
112.752051412436)) ;
#171644 = CARTESIAN_POINT('Ctrl Pts',(-26.3370100297509,-12.3253429194122,
112.776282376473)) ;
#171645 = CARTESIAN_POINT('Ctrl Pts',(-26.2632061608377,-12.3253429487523,
112.800513340511)) ;
#171646 = CARTESIAN_POINT('Ctrl Pts',(-26.2714753234597,-12.3964669498525,
112.825699877311)) ;
#171647 = CARTESIAN_POINT('Ctrl Pts',(-26.3703204549318,-12.3339203423186,
113.09142883813)) ;
#171648 = CARTESIAN_POINT('Ctrl Pts',(-26.3724319867978,-12.4095182646376,
113.097860225065)) ;
#171649 = CARTESIAN_POINT('Ctrl Pts',(-26.4462358554049,-12.4095182584409,
113.073629260095)) ;
#171650 = CARTESIAN_POINT('Ctrl Pts',(-26.5200397240119,-12.4095182522441,
113.049398295125)) ;
#171651 = CARTESIAN_POINT('Ctrl Pts',(-26.5179281921459,-12.3339203299251,
113.04296690819)) ;
#171652 = CARTESIAN_POINT('Ctrl Pts',(-26.5158166602798,-12.2583224076062,
113.036535521254)) ;
#171653 = CARTESIAN_POINT('Ctrl Pts',(-26.4420127916727,-12.2583224138029,
113.060766486224)) ;
#171654 = CARTESIAN_POINT('Ctrl Pts',(-26.3682089230657,-12.2583224199996,
113.084997451194)) ;
#171655 = CARTESIAN_POINT('Ctrl Pts',(-26.3703204549318,-12.3339203423186,
113.09142883813)) ;
#171656 = CARTESIAN_POINT('Ctrl Pts',(-26.4715172701898,-12.3484596551531,
113.36420418221)) ;
#171657 = CARTESIAN_POINT('Ctrl Pts',(-26.467300144392,-12.4231567143316,
113.351359498885)) ;
#171658 = CARTESIAN_POINT('Ctrl Pts',(-26.5411040103548,-12.423156728635,
113.327128525861)) ;
#171659 = CARTESIAN_POINT('Ctrl Pts',(-26.6149078763176,-12.4231567429385,
113.302897552837)) ;
#171660 = CARTESIAN_POINT('Ctrl Pts',(-26.6191250021153,-12.34845968376,113.315742236161)) ;
#171661 = CARTESIAN_POINT('Ctrl Pts',(-26.6233421279131,-12.2737626245815,
113.328586919486)) ;
#171662 = CARTESIAN_POINT('Ctrl Pts',(-26.5495382619503,-12.2737626102781,
113.35281789251)) ;
#171663 = CARTESIAN_POINT('Ctrl Pts',(-26.4757343959875,-12.2737625959746,
113.377048865534)) ;
#171664 = CARTESIAN_POINT('Ctrl Pts',(-26.4715172701898,-12.3484596551531,
113.36420418221)) ;
#171665 = CARTESIAN_POINT('Ctrl Pts',(-26.5685528855363,-12.44015832593,113.624188802472)) ;
#171666 = CARTESIAN_POINT('Ctrl Pts',(-26.5582903689325,-12.5085664478243,
113.592930833998)) ;
#171667 = CARTESIAN_POINT('Ctrl Pts',(-26.6320942303672,-12.508566476899,
113.568699847182)) ;
#171668 = CARTESIAN_POINT('Ctrl Pts',(-26.705898091802,-12.5085665059736,
113.544468860367)) ;
#171669 = CARTESIAN_POINT('Ctrl Pts',(-26.7161606084058,-12.4401583840793,
113.575726828841)) ;
#171670 = CARTESIAN_POINT('Ctrl Pts',(-26.7264231250096,-12.371750262185,
113.606984797315)) ;
#171671 = CARTESIAN_POINT('Ctrl Pts',(-26.6526192635749,-12.3717502331104,
113.631215784131)) ;
#171672 = CARTESIAN_POINT('Ctrl Pts',(-26.5788154021401,-12.3717502040357,
113.655446770947)) ;
#171673 = CARTESIAN_POINT('Ctrl Pts',(-26.5685528855363,-12.44015832593,113.624188802472)) ;
#171674 = CARTESIAN_POINT('Ctrl Pts',(-26.6546342110012,-12.6016814204418,
113.8509185553)) ;
#171675 = CARTESIAN_POINT('Ctrl Pts',(-26.6390796449447,-12.6589156114348,
113.803541857899)) ;
#171676 = CARTESIAN_POINT('Ctrl Pts',(-26.7128835013392,-12.6589156492429,
113.779310855731)) ;
#171677 = CARTESIAN_POINT('Ctrl Pts',(-26.7866873577338,-12.6589156870509,
113.755079853564)) ;
#171678 = CARTESIAN_POINT('Ctrl Pts',(-26.8022419237903,-12.6016814960579,
113.802456550965)) ;
#171679 = CARTESIAN_POINT('Ctrl Pts',(-26.8177964898467,-12.5444473050649,
113.849833248366)) ;
#171680 = CARTESIAN_POINT('Ctrl Pts',(-26.7439926334522,-12.5444472672568,
113.874064250533)) ;
#171681 = CARTESIAN_POINT('Ctrl Pts',(-26.6701887770576,-12.5444472294488,
113.898295252701)) ;
#171682 = CARTESIAN_POINT('Ctrl Pts',(-26.6546342110012,-12.6016814204418,
113.8509185553)) ;
#171683 = CARTESIAN_POINT('Ctrl Pts',(-26.7247862104349,-12.8223735055108,
114.029031451425)) ;
#171684 = CARTESIAN_POINT('Ctrl Pts',(-26.7050456747767,-12.8642856579198,
113.968904965835)) ;
#171685 = CARTESIAN_POINT('Ctrl Pts',(-26.7788495259499,-12.8642856973606,
113.944673947764)) ;
#171686 = CARTESIAN_POINT('Ctrl Pts',(-26.8526533771231,-12.8642857368014,
113.920442929693)) ;
#171687 = CARTESIAN_POINT('Ctrl Pts',(-26.8723939127814,-12.8223735843924,
113.980569415283)) ;
#171688 = CARTESIAN_POINT('Ctrl Pts',(-26.8921344484396,-12.7804614319833,
114.040695900874)) ;
#171689 = CARTESIAN_POINT('Ctrl Pts',(-26.8183305972664,-12.7804613925425,
114.064926918944)) ;
#171690 = CARTESIAN_POINT('Ctrl Pts',(-26.7445267460932,-12.7804613531017,
114.089157937015)) ;
#171691 = CARTESIAN_POINT('Ctrl Pts',(-26.7247862104349,-12.8223735055108,
114.029031451425)) ;
#171692 = CARTESIAN_POINT('Ctrl Pts',(-26.7742244447704,-13.0840251447648,
114.144298922302)) ;
#171693 = CARTESIAN_POINT('Ctrl Pts',(-26.7517329509008,-13.1077315684995,
114.075793461726)) ;
#171694 = CARTESIAN_POINT('Ctrl Pts',(-26.8255367978803,-13.1077316062093,
114.051562430882)) ;
#171695 = CARTESIAN_POINT('Ctrl Pts',(-26.8993406448597,-13.1077316439191,
114.027331400038)) ;
#171696 = CARTESIAN_POINT('Ctrl Pts',(-26.9218321387293,-13.0840252201844,
114.095836860614)) ;
#171697 = CARTESIAN_POINT('Ctrl Pts',(-26.9443236325989,-13.0603187964498,
114.16434232119)) ;
#171698 = CARTESIAN_POINT('Ctrl Pts',(-26.8705197856195,-13.06031875874,114.188573352034)) ;
#171699 = CARTESIAN_POINT('Ctrl Pts',(-26.79671593864,-13.0603187210301,114.212804382878)) ;
#171700 = CARTESIAN_POINT('Ctrl Pts',(-26.7742244447704,-13.0840251447648,
114.144298922302)) ;
#171701 = CARTESIAN_POINT('Ctrl Pts',(-26.8008417401105,-13.370624374638,
114.189901457534)) ;
#171702 = CARTESIAN_POINT('Ctrl Pts',(-26.777191620752,-13.3743556073404,
114.117867010496)) ;
#171703 = CARTESIAN_POINT('Ctrl Pts',(-26.8509954643287,-13.3743556381557,
114.093635969288)) ;
#171704 = CARTESIAN_POINT('Ctrl Pts',(-26.9247993079053,-13.3743556689709,
114.069404928079)) ;
#171705 = CARTESIAN_POINT('Ctrl Pts',(-26.9484494272638,-13.3706244362685,
114.141439375117)) ;
#171706 = CARTESIAN_POINT('Ctrl Pts',(-26.9720995466223,-13.3668932035661,
114.213473822155)) ;
#171707 = CARTESIAN_POINT('Ctrl Pts',(-26.8982957030456,-13.3668931727509,
114.237704863364)) ;
#171708 = CARTESIAN_POINT('Ctrl Pts',(-26.8244918594689,-13.3668931419356,
114.261935904572)) ;
#171709 = CARTESIAN_POINT('Ctrl Pts',(-26.8008417401105,-13.370624374638,
114.189901457534)) ;
#171710 = CARTESIAN_POINT('Ctrl Pts',(-26.8030999803076,-13.6607958553262,
114.161291000141)) ;
#171711 = CARTESIAN_POINT('Ctrl Pts',(-26.7799907261469,-13.6442717980086,
114.090903941066)) ;
#171712 = CARTESIAN_POINT('Ctrl Pts',(-26.8537945677839,-13.6442718197528,
114.066672893949)) ;
#171713 = CARTESIAN_POINT('Ctrl Pts',(-26.927598409421,-13.6442718414971,
114.042441846833)) ;
#171714 = CARTESIAN_POINT('Ctrl Pts',(-26.9507076635816,-13.6607958988147,
114.112828905908)) ;
#171715 = CARTESIAN_POINT('Ctrl Pts',(-26.9738169177423,-13.6773199561323,
114.183215964983)) ;
#171716 = CARTESIAN_POINT('Ctrl Pts',(-26.9000130761053,-13.6773199343881,
114.207447012099)) ;
#171717 = CARTESIAN_POINT('Ctrl Pts',(-26.8262092344683,-13.6773199126438,
114.231678059216)) ;
#171718 = CARTESIAN_POINT('Ctrl Pts',(-26.8030999803076,-13.6607958553262,
114.161291000141)) ;
#171719 = CARTESIAN_POINT('Ctrl Pts',(-26.7817312465355,-13.9332273193549,
114.060772562073)) ;
#171720 = CARTESIAN_POINT('Ctrl Pts',(-26.7608123616796,-13.8976559253995,
113.997057014344)) ;
#171721 = CARTESIAN_POINT('Ctrl Pts',(-26.8346162026608,-13.8976559384048,
113.97282596523)) ;
#171722 = CARTESIAN_POINT('Ctrl Pts',(-26.908420043642,-13.8976559514102,
113.948594916116)) ;
#171723 = CARTESIAN_POINT('Ctrl Pts',(-26.9293389284979,-13.9332273453655,
114.012310463845)) ;
#171724 = CARTESIAN_POINT('Ctrl Pts',(-26.9502578133537,-13.9687987393209,
114.076026011573)) ;
#171725 = CARTESIAN_POINT('Ctrl Pts',(-26.8764539723725,-13.9687987263155,
114.100257060687)) ;
#171726 = CARTESIAN_POINT('Ctrl Pts',(-26.8026501313913,-13.9687987133102,
114.124488109801)) ;
#171727 = CARTESIAN_POINT('Ctrl Pts',(-26.7817312465355,-13.9332273193549,
114.060772562073)) ;
#171728 = CARTESIAN_POINT('Ctrl Pts',(-26.7386891506316,-14.1696161307288,
113.894076690003)) ;
#171729 = CARTESIAN_POINT('Ctrl Pts',(-26.7214807529589,-14.117484643747,
113.841662687406)) ;
#171730 = CARTESIAN_POINT('Ctrl Pts',(-26.7952845945881,-14.1174846489895,
113.817431640266)) ;
#171731 = CARTESIAN_POINT('Ctrl Pts',(-26.8690884362173,-14.117484654232,
113.793200593126)) ;
#171732 = CARTESIAN_POINT('Ctrl Pts',(-26.88629683389,-14.1696161412137,113.845614595723)) ;
#171733 = CARTESIAN_POINT('Ctrl Pts',(-26.9035052315627,-14.2217476281955,
113.89802859832)) ;
#171734 = CARTESIAN_POINT('Ctrl Pts',(-26.8297013899335,-14.221747622953,
113.92225964546)) ;
#171735 = CARTESIAN_POINT('Ctrl Pts',(-26.7558975483042,-14.2217476177105,
113.9464906926)) ;
#171736 = CARTESIAN_POINT('Ctrl Pts',(-26.7386891506316,-14.1696161307288,
113.894076690003)) ;
#171737 = CARTESIAN_POINT('Ctrl Pts',(-26.6786437912351,-14.3504842744957,
113.675940625879)) ;
#171738 = CARTESIAN_POINT('Ctrl Pts',(-26.6663317358567,-14.285645743084,
113.638440091808)) ;
#171739 = CARTESIAN_POINT('Ctrl Pts',(-26.7401355782558,-14.2856457445399,
113.614209047013)) ;
#171740 = CARTESIAN_POINT('Ctrl Pts',(-26.8139394206549,-14.2856457459958,
113.589978002218)) ;
#171741 = CARTESIAN_POINT('Ctrl Pts',(-26.8262514760333,-14.3504842774075,
113.627478536289)) ;
#171742 = CARTESIAN_POINT('Ctrl Pts',(-26.8385635314116,-14.4153228088192,
113.66497907036)) ;
#171743 = CARTESIAN_POINT('Ctrl Pts',(-26.7647596890125,-14.4153228073633,
113.689210115155)) ;
#171744 = CARTESIAN_POINT('Ctrl Pts',(-26.6909558466134,-14.4153228059074,
113.71344115995)) ;
#171745 = CARTESIAN_POINT('Ctrl Pts',(-26.6786437912351,-14.3504842744957,
113.675940625879)) ;
#171746 = CARTESIAN_POINT('Ctrl Pts',(-26.6051960375763,-14.4664314373378,
113.416506558969)) ;
#171747 = CARTESIAN_POINT('Ctrl Pts',(-26.5987335697604,-14.393398523113,
113.396822924687)) ;
#171748 = CARTESIAN_POINT('Ctrl Pts',(-26.6725374136152,-14.3933985223856,
113.372591884325)) ;
#171749 = CARTESIAN_POINT('Ctrl Pts',(-26.7463412574701,-14.3933985216583,
113.348360843964)) ;
#171750 = CARTESIAN_POINT('Ctrl Pts',(-26.752803725286,-14.4664314358832,
113.368044478246)) ;
#171751 = CARTESIAN_POINT('Ctrl Pts',(-26.7592661931018,-14.539464350108,
113.387728112529)) ;
#171752 = CARTESIAN_POINT('Ctrl Pts',(-26.685462349247,-14.5394643508353,
113.41195915289)) ;
#171753 = CARTESIAN_POINT('Ctrl Pts',(-26.6116585053922,-14.5394643515627,
113.436190193252)) ;
#171754 = CARTESIAN_POINT('Ctrl Pts',(-26.6051960375763,-14.4664314373378,
113.416506558969)) ;
#171755 = CARTESIAN_POINT('Ctrl Pts',(-26.5259715366712,-14.505814940549,
113.139853747979)) ;
#171756 = CARTESIAN_POINT('Ctrl Pts',(-26.5257630868686,-14.4299235771365,
113.139218843456)) ;
#171757 = CARTESIAN_POINT('Ctrl Pts',(-26.5995669312173,-14.4299235770663,
113.114987804598)) ;
#171758 = CARTESIAN_POINT('Ctrl Pts',(-26.673370775566,-14.429923576996,113.090756765741)) ;
#171759 = CARTESIAN_POINT('Ctrl Pts',(-26.6735792253686,-14.5058149404085,
113.091391670264)) ;
#171760 = CARTESIAN_POINT('Ctrl Pts',(-26.6737876751712,-14.5817063038209,
113.092026574788)) ;
#171761 = CARTESIAN_POINT('Ctrl Pts',(-26.5999838308225,-14.5817063038912,
113.116257613645)) ;
#171762 = CARTESIAN_POINT('Ctrl Pts',(-26.5261799864738,-14.5817063039614,
113.140488652502)) ;
#171763 = CARTESIAN_POINT('Ctrl Pts',(-26.5259715366712,-14.505814940549,
113.139853747979)) ;
#171764 = CARTESIAN_POINT('Ctrl Pts',(-26.4466835012553,-14.46830400306,112.863009454041)) ;
#171765 = CARTESIAN_POINT('Ctrl Pts',(-26.4527427661064,-14.3949198444241,
112.881464997054)) ;
#171766 = CARTESIAN_POINT('Ctrl Pts',(-26.5265466105033,-14.3949198453838,
112.857233958344)) ;
#171767 = CARTESIAN_POINT('Ctrl Pts',(-26.6003504549002,-14.3949198463436,
112.833002919634)) ;
#171768 = CARTESIAN_POINT('Ctrl Pts',(-26.5942911900492,-14.4683040049795,
112.81454737662)) ;
#171769 = CARTESIAN_POINT('Ctrl Pts',(-26.5882319251982,-14.5416881636154,
112.796091833607)) ;
#171770 = CARTESIAN_POINT('Ctrl Pts',(-26.5144280808013,-14.5416881626556,
112.820322872317)) ;
#171771 = CARTESIAN_POINT('Ctrl Pts',(-26.4406242364043,-14.5416881616959,
112.844553911027)) ;
#171772 = CARTESIAN_POINT('Ctrl Pts',(-26.4466835012553,-14.46830400306,112.863009454041)) ;
#171773 = CARTESIAN_POINT('Ctrl Pts',(-26.3730710354797,-14.3544455833434,
112.603124137994)) ;
#171774 = CARTESIAN_POINT('Ctrl Pts',(-26.3850179196596,-14.28890351008,112.639512419572)) ;
#171775 = CARTESIAN_POINT('Ctrl Pts',(-26.458821763171,-14.2889035106551,
112.615281378165)) ;
#171776 = CARTESIAN_POINT('Ctrl Pts',(-26.5326256066825,-14.2889035112301,
112.591050336758)) ;
#171777 = CARTESIAN_POINT('Ctrl Pts',(-26.5206787225026,-14.3544455844935,
112.554662055179)) ;
#171778 = CARTESIAN_POINT('Ctrl Pts',(-26.5087318383227,-14.4199876577569,
112.518273773601)) ;
#171779 = CARTESIAN_POINT('Ctrl Pts',(-26.4349279948113,-14.4199876571819,
112.542504815008)) ;
#171780 = CARTESIAN_POINT('Ctrl Pts',(-26.3611241512998,-14.4199876566068,
112.566735856416)) ;
#171781 = CARTESIAN_POINT('Ctrl Pts',(-26.3730710354797,-14.3544455833434,
112.603124137994)) ;
#171782 = CARTESIAN_POINT('Ctrl Pts',(-26.3124728977524,-14.1743504235921,
112.383177448969)) ;
#171783 = CARTESIAN_POINT('Ctrl Pts',(-26.3294005699097,-14.1212879349947,
112.434736407154)) ;
#171784 = CARTESIAN_POINT('Ctrl Pts',(-26.4032044125281,-14.121287932882,
112.410505363027)) ;
#171785 = CARTESIAN_POINT('Ctrl Pts',(-26.4770082551464,-14.1212879307693,
112.386274318899)) ;
#171786 = CARTESIAN_POINT('Ctrl Pts',(-26.4600805829891,-14.1743504193667,
112.334715360714)) ;
#171787 = CARTESIAN_POINT('Ctrl Pts',(-26.4431529108318,-14.2274129079642,
112.283156402529)) ;
#171788 = CARTESIAN_POINT('Ctrl Pts',(-26.3693490682134,-14.2274129100769,
112.307387446657)) ;
#171789 = CARTESIAN_POINT('Ctrl Pts',(-26.295545225595,-14.2274129121895,
112.331618490784)) ;
#171790 = CARTESIAN_POINT('Ctrl Pts',(-26.3124728977524,-14.1743504235921,
112.383177448969)) ;
#171791 = CARTESIAN_POINT('Ctrl Pts',(-26.2691441762916,-13.9404023706078,
112.215800956528)) ;
#171792 = CARTESIAN_POINT('Ctrl Pts',(-26.2898545563157,-13.9035978670998,
112.278881432632)) ;
#171793 = CARTESIAN_POINT('Ctrl Pts',(-26.3636583983287,-13.903597860184,
112.254650386661)) ;
#171794 = CARTESIAN_POINT('Ctrl Pts',(-26.4374622403416,-13.9035978532681,
112.23041934069)) ;
#171795 = CARTESIAN_POINT('Ctrl Pts',(-26.4167518603175,-13.940402356776,
112.167338864585)) ;
#171796 = CARTESIAN_POINT('Ctrl Pts',(-26.3960414802934,-13.977206860284,
112.10425838848)) ;
#171797 = CARTESIAN_POINT('Ctrl Pts',(-26.3222376382805,-13.9772068671999,
112.128489434452)) ;
#171798 = CARTESIAN_POINT('Ctrl Pts',(-26.2484337962675,-13.9772068741157,
112.152720480423)) ;
#171799 = CARTESIAN_POINT('Ctrl Pts',(-26.2691441762916,-13.9404023706078,
112.215800956528)) ;
#171800 = CARTESIAN_POINT('Ctrl Pts',(-26.2470669365409,-13.6671888266285,
112.112924558201)) ;
#171801 = CARTESIAN_POINT('Ctrl Pts',(-26.27008647726,-13.6494076085659,112.183038365355)) ;
#171802 = CARTESIAN_POINT('Ctrl Pts',(-26.3438903193133,-13.6494075929638,
112.158807319507)) ;
#171803 = CARTESIAN_POINT('Ctrl Pts',(-26.4176941613665,-13.6494075773616,
112.134576273658)) ;
#171804 = CARTESIAN_POINT('Ctrl Pts',(-26.3946746206473,-13.6671887954242,
112.064462466504)) ;
#171805 = CARTESIAN_POINT('Ctrl Pts',(-26.3716550799282,-13.6849700134867,
111.994348659349)) ;
#171806 = CARTESIAN_POINT('Ctrl Pts',(-26.297851237875,-13.6849700290889,
112.018579705198)) ;
#171807 = CARTESIAN_POINT('Ctrl Pts',(-26.2240473958217,-13.684970044691,
112.042810751047)) ;
#171808 = CARTESIAN_POINT('Ctrl Pts',(-26.2470669365409,-13.6671888266285,
112.112924558201)) ;
#171809 = CARTESIAN_POINT('Ctrl Pts',(-26.248777373754,-13.3783758394987,
112.082794816685)) ;
#171810 = CARTESIAN_POINT('Ctrl Pts',(-26.2724420195243,-13.3807343880949,
112.154873509865)) ;
#171811 = CARTESIAN_POINT('Ctrl Pts',(-26.3462458630014,-13.3807343653365,
112.130642468353)) ;
#171812 = CARTESIAN_POINT('Ctrl Pts',(-26.4200497064785,-13.3807343425781,
112.106411426841)) ;
#171813 = CARTESIAN_POINT('Ctrl Pts',(-26.3963850607081,-13.3783757939819,
112.034332733661)) ;
#171814 = CARTESIAN_POINT('Ctrl Pts',(-26.3727204149377,-13.3760172453858,
111.962254040481)) ;
#171815 = CARTESIAN_POINT('Ctrl Pts',(-26.2989165714607,-13.3760172681442,
111.986485081993)) ;
#171816 = CARTESIAN_POINT('Ctrl Pts',(-26.2251127279836,-13.3760172909026,
112.010716123505)) ;
#171817 = CARTESIAN_POINT('Ctrl Pts',(-26.248777373754,-13.3783758394987,
112.082794816685)) ;
#171818 = CARTESIAN_POINT('Ctrl Pts',(-26.2746776385701,-13.0914976589315,
112.126226095536)) ;
#171819 = CARTESIAN_POINT('Ctrl Pts',(-26.297301844828,-13.1138898142191,
112.19513577799)) ;
#171820 = CARTESIAN_POINT('Ctrl Pts',(-26.3711056909002,-13.113889784642,
112.170904744382)) ;
#171821 = CARTESIAN_POINT('Ctrl Pts',(-26.4449095369724,-13.1138897550648,
112.146673710775)) ;
#171822 = CARTESIAN_POINT('Ctrl Pts',(-26.4222853307145,-13.0914975997771,
112.07776402832)) ;
#171823 = CARTESIAN_POINT('Ctrl Pts',(-26.3996611244566,-13.0691054444894,
112.008854345866)) ;
#171824 = CARTESIAN_POINT('Ctrl Pts',(-26.3258572783844,-13.0691054740666,
112.033085379473)) ;
#171825 = CARTESIAN_POINT('Ctrl Pts',(-26.2520534323122,-13.0691055036438,
112.057316413081)) ;
#171826 = CARTESIAN_POINT('Ctrl Pts',(-26.2746776385701,-13.0914976589315,
112.126226095536)) ;
#171827 = CARTESIAN_POINT('Ctrl Pts',(-26.3237843579519,-12.827936357185,
112.24033766308)) ;
#171828 = CARTESIAN_POINT('Ctrl Pts',(-26.3437463716241,-12.8687628272745,
112.301138736626)) ;
#171829 = CARTESIAN_POINT('Ctrl Pts',(-26.4175502214732,-12.8687627938338,
112.276907714522)) ;
#171830 = CARTESIAN_POINT('Ctrl Pts',(-26.4913540713223,-12.868762760393,
112.252676692418)) ;
#171831 = CARTESIAN_POINT('Ctrl Pts',(-26.4713920576501,-12.8279362903035,
112.191875618872)) ;
#171832 = CARTESIAN_POINT('Ctrl Pts',(-26.4514300439778,-12.7871098202139,
112.131074545326)) ;
#171833 = CARTESIAN_POINT('Ctrl Pts',(-26.3776261941287,-12.7871098536547,
112.15530556743)) ;
#171834 = CARTESIAN_POINT('Ctrl Pts',(-26.3038223442796,-12.7871098870954,
112.179536589534)) ;
#171835 = CARTESIAN_POINT('Ctrl Pts',(-26.3237843579519,-12.827936357185,
112.24033766308)) ;
#171836 = CARTESIAN_POINT('Ctrl Pts',(-26.3935111615706,-12.6061166858968,
112.417162681011)) ;
#171837 = CARTESIAN_POINT('Ctrl Pts',(-26.4093694433139,-12.662489659223,
112.465464449421)) ;
#171838 = CARTESIAN_POINT('Ctrl Pts',(-26.4831732979266,-12.6624896260607,
112.441233441827)) ;
#171839 = CARTESIAN_POINT('Ctrl Pts',(-26.5569771525393,-12.6624895928983,
112.417002434232)) ;
#171840 = CARTESIAN_POINT('Ctrl Pts',(-26.541118870796,-12.6061166195721,
112.368700665822)) ;
#171841 = CARTESIAN_POINT('Ctrl Pts',(-26.5252605890526,-12.5497436462459,
112.320398897411)) ;
#171842 = CARTESIAN_POINT('Ctrl Pts',(-26.4514567344399,-12.5497436794083,
112.344629905006)) ;
#171843 = CARTESIAN_POINT('Ctrl Pts',(-26.3776528798272,-12.5497437125706,
112.3688609126)) ;
#171844 = CARTESIAN_POINT('Ctrl Pts',(-26.3935111615706,-12.6061166858968,
112.417162681011)) ;
#171845 = CARTESIAN_POINT('Ctrl Pts',(-26.4793526115935,-12.4431271546039,
112.643138615007)) ;
#171846 = CARTESIAN_POINT('Ctrl Pts',(-26.4899747011907,-12.5109613838961,
112.675491787168)) ;
#171847 = CARTESIAN_POINT('Ctrl Pts',(-26.5637785606393,-12.510961357698,
112.651260794302)) ;
#171848 = CARTESIAN_POINT('Ctrl Pts',(-26.6375824200879,-12.5109613315,112.627029801437)) ;
#171849 = CARTESIAN_POINT('Ctrl Pts',(-26.6269603304907,-12.4431271022078,
112.594676629277)) ;
#171850 = CARTESIAN_POINT('Ctrl Pts',(-26.6163382408936,-12.3752928729157,
112.562323457116)) ;
#171851 = CARTESIAN_POINT('Ctrl Pts',(-26.542534381445,-12.3752928991138,
112.586554449982)) ;
#171852 = CARTESIAN_POINT('Ctrl Pts',(-26.4687305219963,-12.3752929253118,
112.610785442847)) ;
#171853 = CARTESIAN_POINT('Ctrl Pts',(-26.4793526115935,-12.4431271546039,
112.643138615007)) ;
#171854 = CARTESIAN_POINT('Ctrl Pts',(-26.575504511702,-12.3502094912987,
112.900682431856)) ;
#171855 = CARTESIAN_POINT('Ctrl Pts',(-26.5801595812379,-12.4246287371788,
112.914861023821)) ;
#171856 = CARTESIAN_POINT('Ctrl Pts',(-26.6539634444303,-12.4246287241844,
112.890630042359)) ;
#171857 = CARTESIAN_POINT('Ctrl Pts',(-26.7277673076227,-12.42462871119,112.866399060897)) ;
#171858 = CARTESIAN_POINT('Ctrl Pts',(-26.7231122380868,-12.35020946531,112.852220468932)) ;
#171859 = CARTESIAN_POINT('Ctrl Pts',(-26.7184571685509,-12.2757902194299,
112.838041876967)) ;
#171860 = CARTESIAN_POINT('Ctrl Pts',(-26.6446533053586,-12.2757902324242,
112.862272858429)) ;
#171861 = CARTESIAN_POINT('Ctrl Pts',(-26.5708494421661,-12.2757902454186,
112.886503839892)) ;
#171862 = CARTESIAN_POINT('Ctrl Pts',(-26.575504511702,-12.3502094912987,
112.900682431856)) ;
#171863 = CARTESIAN_POINT('Ctrl Pts',(-26.6766988977771,-12.3330949628537,
113.1734359646)) ;
#171864 = CARTESIAN_POINT('Ctrl Pts',(-26.6750294757674,-12.4088168292008,
113.168351175927)) ;
#171865 = CARTESIAN_POINT('Ctrl Pts',(-26.7488333418635,-12.4088168339974,
113.144120203309)) ;
#171866 = CARTESIAN_POINT('Ctrl Pts',(-26.8226372079595,-12.408816838794,
113.119889230691)) ;
#171867 = CARTESIAN_POINT('Ctrl Pts',(-26.8243066299692,-12.3330949724469,
113.124974019364)) ;
#171868 = CARTESIAN_POINT('Ctrl Pts',(-26.8259760519788,-12.2573731060998,
113.130058808036)) ;
#171869 = CARTESIAN_POINT('Ctrl Pts',(-26.7521721858828,-12.2573731013032,
113.154289780654)) ;
#171870 = CARTESIAN_POINT('Ctrl Pts',(-26.6783683197867,-12.2573730965066,
113.178520753273)) ;
#171871 = CARTESIAN_POINT('Ctrl Pts',(-26.6766988977771,-12.3330949628537,
113.1734359646)) ;
#171872 = CARTESIAN_POINT('Ctrl Pts',(-26.7762581210695,-12.3941323979468,
113.441132115041)) ;
#171873 = CARTESIAN_POINT('Ctrl Pts',(-26.7683708300388,-12.4657028650143,
113.417108700738)) ;
#171874 = CARTESIAN_POINT('Ctrl Pts',(-26.8421746972999,-12.4657028918637,
113.392877731668)) ;
#171875 = CARTESIAN_POINT('Ctrl Pts',(-26.915978564561,-12.4657029187131,
113.368646762599)) ;
#171876 = CARTESIAN_POINT('Ctrl Pts',(-26.9238658555916,-12.3941324516456,
113.392670176902)) ;
#171877 = CARTESIAN_POINT('Ctrl Pts',(-26.9317531466222,-12.3225619845781,
113.416693591205)) ;
#171878 = CARTESIAN_POINT('Ctrl Pts',(-26.8579492793612,-12.3225619577287,
113.440924560275)) ;
#171879 = CARTESIAN_POINT('Ctrl Pts',(-26.7841454121001,-12.3225619308793,
113.465155529345)) ;
#171880 = CARTESIAN_POINT('Ctrl Pts',(-26.7762581210695,-12.3941323979468,
113.441132115041)) ;
#171881 = CARTESIAN_POINT('Ctrl Pts',(-26.8671458754654,-12.5280047279255,
113.682585935319)) ;
#171882 = CARTESIAN_POINT('Ctrl Pts',(-26.8536336294448,-12.5903323506603,
113.641429815818)) ;
#171883 = CARTESIAN_POINT('Ctrl Pts',(-26.9274374951756,-12.5903324003766,
113.617198842087)) ;
#171884 = CARTESIAN_POINT('Ctrl Pts',(-27.0012413609064,-12.5903324500929,
113.592967868356)) ;
#171885 = CARTESIAN_POINT('Ctrl Pts',(-27.014753606927,-12.5280048273581,
113.634123987858)) ;
#171886 = CARTESIAN_POINT('Ctrl Pts',(-27.0282658529477,-12.4656772046233,
113.67528010736)) ;
#171887 = CARTESIAN_POINT('Ctrl Pts',(-26.9544619872168,-12.465677154907,
113.699511081091)) ;
#171888 = CARTESIAN_POINT('Ctrl Pts',(-26.880658121486,-12.4656771051907,
113.723742054821)) ;
#171889 = CARTESIAN_POINT('Ctrl Pts',(-26.8671458754654,-12.5280047279255,
113.682585935319)) ;
#171890 = CARTESIAN_POINT('Ctrl Pts',(-26.9443518098183,-12.725823043926,
113.882266526049)) ;
#171891 = CARTESIAN_POINT('Ctrl Pts',(-26.9261637118994,-12.7744304923816,
113.82686851623)) ;
#171892 = CARTESIAN_POINT('Ctrl Pts',(-26.9999675739472,-12.7744305640523,
113.802637531282)) ;
#171893 = CARTESIAN_POINT('Ctrl Pts',(-27.073771435995,-12.7744306357229,
113.778406546333)) ;
#171894 = CARTESIAN_POINT('Ctrl Pts',(-27.091959533914,-12.7258231872673,
113.833804556152)) ;
#171895 = CARTESIAN_POINT('Ctrl Pts',(-27.1101476318329,-12.6772157388117,
113.889202565971)) ;
#171896 = CARTESIAN_POINT('Ctrl Pts',(-27.036343769785,-12.677215667141,113.91343355092)) ;
#171897 = CARTESIAN_POINT('Ctrl Pts',(-26.9625399077372,-12.6772155954704,
113.937664535868)) ;
#171898 = CARTESIAN_POINT('Ctrl Pts',(-26.9443518098183,-12.725823043926,
113.882266526049)) ;
#171899 = CARTESIAN_POINT('Ctrl Pts',(-27.0028790263338,-12.9740366931117,
114.024965068217)) ;
#171900 = CARTESIAN_POINT('Ctrl Pts',(-26.9813140704319,-13.0053860395,113.959281693945)) ;
#171901 = CARTESIAN_POINT('Ctrl Pts',(-27.0551179265467,-13.0053861296798,
113.935050690925)) ;
#171902 = CARTESIAN_POINT('Ctrl Pts',(-27.1289217826615,-13.0053862198596,
113.910819687906)) ;
#171903 = CARTESIAN_POINT('Ctrl Pts',(-27.1504867385634,-12.9740368734713,
113.976503062178)) ;
#171904 = CARTESIAN_POINT('Ctrl Pts',(-27.1720516944653,-12.942687527083,
114.04218643645)) ;
#171905 = CARTESIAN_POINT('Ctrl Pts',(-27.0982478383505,-12.9426874369032,
114.06641743947)) ;
#171906 = CARTESIAN_POINT('Ctrl Pts',(-27.0244439822357,-12.9426873467234,
114.090648442489)) ;
#171907 = CARTESIAN_POINT('Ctrl Pts',(-27.0028790263338,-12.9740366931117,
114.024965068217)) ;
#171908 = CARTESIAN_POINT('Ctrl Pts',(-27.0390249126838,-13.2534633118697,
114.099588598299)) ;
#171909 = CARTESIAN_POINT('Ctrl Pts',(-27.015638751867,-13.2653501074278,
114.028358127784)) ;
#171910 = CARTESIAN_POINT('Ctrl Pts',(-27.0894426002158,-13.2653502091921,
114.004127101111)) ;
#171911 = CARTESIAN_POINT('Ctrl Pts',(-27.1632464485645,-13.2653503109564,
113.979896074437)) ;
#171912 = CARTESIAN_POINT('Ctrl Pts',(-27.1866326093813,-13.2534635153983,
114.051126544952)) ;
#171913 = CARTESIAN_POINT('Ctrl Pts',(-27.210018770198,-13.2415767198401,
114.122357015466)) ;
#171914 = CARTESIAN_POINT('Ctrl Pts',(-27.1362149218493,-13.2415766180759,
114.14658804214)) ;
#171915 = CARTESIAN_POINT('Ctrl Pts',(-27.0624110735005,-13.2415765163116,
114.170819068813)) ;
#171916 = CARTESIAN_POINT('Ctrl Pts',(-27.0390249126838,-13.2534633118697,
114.099588598299)) ;
#171917 = CARTESIAN_POINT('Ctrl Pts',(-27.0511093886364,-13.5448240416985,
114.100900424596)) ;
#171918 = CARTESIAN_POINT('Ctrl Pts',(-27.02757960726,-13.5363866538712,114.029232509088)) ;
#171919 = CARTESIAN_POINT('Ctrl Pts',(-27.1013834468662,-13.5363867591239,
114.005001455786)) ;
#171920 = CARTESIAN_POINT('Ctrl Pts',(-27.1751872864724,-13.5363868643766,
113.980770402484)) ;
#171921 = CARTESIAN_POINT('Ctrl Pts',(-27.1987170678488,-13.544824252204,
114.052438317993)) ;
#171922 = CARTESIAN_POINT('Ctrl Pts',(-27.2222468492252,-13.5532616400314,
114.124106233501)) ;
#171923 = CARTESIAN_POINT('Ctrl Pts',(-27.148443009619,-13.5532615347787,
114.148337286803)) ;
#171924 = CARTESIAN_POINT('Ctrl Pts',(-27.0746391700128,-13.553261429526,
114.172568340105)) ;
#171925 = CARTESIAN_POINT('Ctrl Pts',(-27.0511093886364,-13.5448240416985,
114.100900424596)) ;
#171926 = CARTESIAN_POINT('Ctrl Pts',(-27.0391527832181,-13.8260554927979,
114.029131671761)) ;
#171927 = CARTESIAN_POINT('Ctrl Pts',(-27.017154679759,-13.7979711605236,
113.962129000086)) ;
#171928 = CARTESIAN_POINT('Ctrl Pts',(-27.0909585105926,-13.7979712603347,
113.937897920064)) ;
#171929 = CARTESIAN_POINT('Ctrl Pts',(-27.1647623414261,-13.7979713601458,
113.913666840042)) ;
#171930 = CARTESIAN_POINT('Ctrl Pts',(-27.1867604448851,-13.8260556924201,
113.980669511717)) ;
#171931 = CARTESIAN_POINT('Ctrl Pts',(-27.2087585483442,-13.8541400246944,
114.047672183392)) ;
#171932 = CARTESIAN_POINT('Ctrl Pts',(-27.1349547175107,-13.8541399248833,
114.071903263414)) ;
#171933 = CARTESIAN_POINT('Ctrl Pts',(-27.0611508866771,-13.8541398250722,
114.096134343436)) ;
#171934 = CARTESIAN_POINT('Ctrl Pts',(-27.0391527832181,-13.8260554927979,
114.029131671761)) ;
#171935 = CARTESIAN_POINT('Ctrl Pts',(-27.0044729766098,-14.0796928172426,
113.887914543523)) ;
#171936 = CARTESIAN_POINT('Ctrl Pts',(-26.9855998097285,-14.0338589352342,
113.830429924472)) ;
#171937 = CARTESIAN_POINT('Ctrl Pts',(-27.0594036325612,-14.033859021297,
113.806198820081)) ;
#171938 = CARTESIAN_POINT('Ctrl Pts',(-27.133207455394,-14.0338591073598,
113.78196771569)) ;
#171939 = CARTESIAN_POINT('Ctrl Pts',(-27.1520806222753,-14.0796929893683,
113.839452334741)) ;
#171940 = CARTESIAN_POINT('Ctrl Pts',(-27.1709537891566,-14.1255268713768,
113.896936953791)) ;
#171941 = CARTESIAN_POINT('Ctrl Pts',(-27.0971499663238,-14.1255267853139,
113.921168058182)) ;
#171942 = CARTESIAN_POINT('Ctrl Pts',(-27.023346143491,-14.1255266992511,
113.945399162573)) ;
#171943 = CARTESIAN_POINT('Ctrl Pts',(-27.0044729766098,-14.0796928172426,
113.887914543523)) ;
#171944 = CARTESIAN_POINT('Ctrl Pts',(-26.9509127407255,-14.2840883967328,
113.689505698665)) ;
#171945 = CARTESIAN_POINT('Ctrl Pts',(-26.9364810188695,-14.223916620712,
113.64554900453)) ;
#171946 = CARTESIAN_POINT('Ctrl Pts',(-27.0102848354058,-14.2239166860408,
113.621317880961)) ;
#171947 = CARTESIAN_POINT('Ctrl Pts',(-27.0840886519422,-14.2239167513696,
113.597086757393)) ;
#171948 = CARTESIAN_POINT('Ctrl Pts',(-27.0985203737982,-14.2840885273904,
113.641043451527)) ;
#171949 = CARTESIAN_POINT('Ctrl Pts',(-27.1129520956543,-14.3442603034112,
113.685000145661)) ;
#171950 = CARTESIAN_POINT('Ctrl Pts',(-27.0391482791179,-14.3442602380824,
113.70923126923)) ;
#171951 = CARTESIAN_POINT('Ctrl Pts',(-26.9653444625816,-14.3442601727535,
113.733462392799)) ;
#171952 = CARTESIAN_POINT('Ctrl Pts',(-26.9509127407255,-14.2840883967328,
113.689505698665)) ;
#171953 = CARTESIAN_POINT('Ctrl Pts',(-26.8822296015483,-14.4281001590278,
113.444744206038)) ;
#171954 = CARTESIAN_POINT('Ctrl Pts',(-26.8733074115915,-14.3577843512303,
113.41756865708)) ;
#171955 = CARTESIAN_POINT('Ctrl Pts',(-26.9471112241109,-14.3577843906291,
113.393337521276)) ;
#171956 = CARTESIAN_POINT('Ctrl Pts',(-27.0209150366302,-14.357784430028,
113.369106385472)) ;
#171957 = CARTESIAN_POINT('Ctrl Pts',(-27.0298372265869,-14.4281002378256,
113.39628193443)) ;
#171958 = CARTESIAN_POINT('Ctrl Pts',(-27.0387594165436,-14.4984160456232,
113.423457483389)) ;
#171959 = CARTESIAN_POINT('Ctrl Pts',(-26.9649556040243,-14.4984160062243,
113.447688619193)) ;
#171960 = CARTESIAN_POINT('Ctrl Pts',(-26.891151791505,-14.4984159668254,
113.471919754997)) ;
#171961 = CARTESIAN_POINT('Ctrl Pts',(-26.8822296015483,-14.4281001590278,
113.444744206038)) ;
#171962 = CARTESIAN_POINT('Ctrl Pts',(-26.8046693446462,-14.4990916302809,
113.173055466615)) ;
#171963 = CARTESIAN_POINT('Ctrl Pts',(-26.8018824452395,-14.4237145145617,
113.164567022696)) ;
#171964 = CARTESIAN_POINT('Ctrl Pts',(-26.8756862564281,-14.4237145258999,
113.140335882838)) ;
#171965 = CARTESIAN_POINT('Ctrl Pts',(-26.9494900676167,-14.4237145372381,
113.116104742981)) ;
#171966 = CARTESIAN_POINT('Ctrl Pts',(-26.9522769670233,-14.4990916529572,
113.124593186901)) ;
#171967 = CARTESIAN_POINT('Ctrl Pts',(-26.95506386643,-14.5744687686764,113.13308163082)) ;
#171968 = CARTESIAN_POINT('Ctrl Pts',(-26.8812600552414,-14.5744687573382,
113.157312770678)) ;
#171969 = CARTESIAN_POINT('Ctrl Pts',(-26.8074562440528,-14.574468746,113.181543910535)) ;
#171970 = CARTESIAN_POINT('Ctrl Pts',(-26.8046693446462,-14.4990916302809,
113.173055466615)) ;
#171971 = CARTESIAN_POINT('Ctrl Pts',(-26.7243601583869,-14.4927693074735,
112.892974720862)) ;
#171972 = CARTESIAN_POINT('Ctrl Pts',(-26.7279100215133,-14.4177207882231,
112.903787033113)) ;
#171973 = CARTESIAN_POINT('Ctrl Pts',(-26.8017138340692,-14.4177207722467,
112.879555897421)) ;
#171974 = CARTESIAN_POINT('Ctrl Pts',(-26.8755176466252,-14.4177207562703,
112.855324761728)) ;
#171975 = CARTESIAN_POINT('Ctrl Pts',(-26.8719677834988,-14.4927692755206,
112.844512449478)) ;
#171976 = CARTESIAN_POINT('Ctrl Pts',(-26.8684179203725,-14.567817794771,
112.833700137227)) ;
#171977 = CARTESIAN_POINT('Ctrl Pts',(-26.7946141078165,-14.5678178107474,
112.857931272919)) ;
#171978 = CARTESIAN_POINT('Ctrl Pts',(-26.7208102952605,-14.5678178267238,
112.882162408612)) ;
#171979 = CARTESIAN_POINT('Ctrl Pts',(-26.7243601583869,-14.4927693074735,
112.892974720862)) ;
#171980 = CARTESIAN_POINT('Ctrl Pts',(-26.6478394647209,-14.4094376546516,
112.624441415415)) ;
#171981 = CARTESIAN_POINT('Ctrl Pts',(-26.6574709542339,-14.3400945271198,
112.653777380281)) ;
#171982 = CARTESIAN_POINT('Ctrl Pts',(-26.7312747705731,-14.3400944873417,
112.629546256112)) ;
#171983 = CARTESIAN_POINT('Ctrl Pts',(-26.8050785869124,-14.3400944475637,
112.605315131943)) ;
#171984 = CARTESIAN_POINT('Ctrl Pts',(-26.7954470973993,-14.4094375750955,
112.575979167076)) ;
#171985 = CARTESIAN_POINT('Ctrl Pts',(-26.7858156078862,-14.4787807026274,
112.54664320221)) ;
#171986 = CARTESIAN_POINT('Ctrl Pts',(-26.712011791547,-14.4787807424054,
112.570874326379)) ;
#171987 = CARTESIAN_POINT('Ctrl Pts',(-26.6382079752078,-14.4787807821835,
112.595105450548)) ;
#171988 = CARTESIAN_POINT('Ctrl Pts',(-26.6478394647209,-14.4094376546516,
112.624441415415)) ;
#171989 = CARTESIAN_POINT('Ctrl Pts',(-26.5812947221216,-14.2549673486149,
112.386270724262)) ;
#171990 = CARTESIAN_POINT('Ctrl Pts',(-26.5963210143004,-14.1963046294673,
112.432038387488)) ;
#171991 = CARTESIAN_POINT('Ctrl Pts',(-26.6701248363186,-14.1963045717546,
112.407807280615)) ;
#171992 = CARTESIAN_POINT('Ctrl Pts',(-26.7439286583366,-14.1963045140418,
112.383576173743)) ;
#171993 = CARTESIAN_POINT('Ctrl Pts',(-26.7289023661578,-14.2549672331893,
112.337808510517)) ;
#171994 = CARTESIAN_POINT('Ctrl Pts',(-26.713876073979,-14.3136299523368,
112.292040847291)) ;
#171995 = CARTESIAN_POINT('Ctrl Pts',(-26.6400722519609,-14.3136300100496,
112.316271954164)) ;
#171996 = CARTESIAN_POINT('Ctrl Pts',(-26.5662684299428,-14.3136300677624,
112.340503061036)) ;
#171997 = CARTESIAN_POINT('Ctrl Pts',(-26.5812947221216,-14.2549673486149,
112.386270724262)) ;
#171998 = CARTESIAN_POINT('Ctrl Pts',(-26.5303911941234,-14.0408502140836,
112.195800520988)) ;
#171999 = CARTESIAN_POINT('Ctrl Pts',(-26.549727194973,-13.9970485144641,
112.254694861334)) ;
#172000 = CARTESIAN_POINT('Ctrl Pts',(-26.6235310236397,-13.9970484457834,
112.230463774713)) ;
#172001 = CARTESIAN_POINT('Ctrl Pts',(-26.6973348523065,-13.9970483771027,
112.206232688091)) ;
#172002 = CARTESIAN_POINT('Ctrl Pts',(-26.6779988514569,-14.0408500767222,
112.147338347744)) ;
#172003 = CARTESIAN_POINT('Ctrl Pts',(-26.6586628506072,-14.0846517763417,
112.088444007397)) ;
#172004 = CARTESIAN_POINT('Ctrl Pts',(-26.5848590219405,-14.0846518450224,
112.112675094019)) ;
#172005 = CARTESIAN_POINT('Ctrl Pts',(-26.5110551932737,-14.0846519137031,
112.136906180641)) ;
#172006 = CARTESIAN_POINT('Ctrl Pts',(-26.5303911941234,-14.0408502140836,
112.195800520988)) ;
#172007 = CARTESIAN_POINT('Ctrl Pts',(-26.4993318655355,-13.7824650273217,
112.065794986604)) ;
#172008 = CARTESIAN_POINT('Ctrl Pts',(-26.5215981506244,-13.7566374523408,
112.133614499815)) ;
#172009 = CARTESIAN_POINT('Ctrl Pts',(-26.5954019862457,-13.7566373798381,
112.109383434376)) ;
#172010 = CARTESIAN_POINT('Ctrl Pts',(-26.669205821867,-13.7566373073354,
112.085152368936)) ;
#172011 = CARTESIAN_POINT('Ctrl Pts',(-26.6469395367781,-13.7824648823164,
112.017332855726)) ;
#172012 = CARTESIAN_POINT('Ctrl Pts',(-26.6246732516892,-13.8082924572973,
111.949513342515)) ;
#172013 = CARTESIAN_POINT('Ctrl Pts',(-26.5508694160679,-13.8082925298,111.973744407954)) ;
#172014 = CARTESIAN_POINT('Ctrl Pts',(-26.4770655804466,-13.8082926023027,
111.997975473393)) ;
#172015 = CARTESIAN_POINT('Ctrl Pts',(-26.4993318655355,-13.7824650273217,
112.065794986604)) ;
#172016 = CARTESIAN_POINT('Ctrl Pts',(-26.4911724058639,-13.4963851494492,
112.005340368792)) ;
#172017 = CARTESIAN_POINT('Ctrl Pts',(-26.5147789143434,-13.4904923432814,
112.077241986031)) ;
#172018 = CARTESIAN_POINT('Ctrl Pts',(-26.5885827564685,-13.4904922758106,
112.053010940401)) ;
#172019 = CARTESIAN_POINT('Ctrl Pts',(-26.6623865985935,-13.4904922083398,
112.028779894771)) ;
#172020 = CARTESIAN_POINT('Ctrl Pts',(-26.6387800901139,-13.4963850145077,
111.956878277532)) ;
#172021 = CARTESIAN_POINT('Ctrl Pts',(-26.6151735816344,-13.5022778206756,
111.884976660293)) ;
#172022 = CARTESIAN_POINT('Ctrl Pts',(-26.5413697395093,-13.5022778881464,
111.909207705923)) ;
#172023 = CARTESIAN_POINT('Ctrl Pts',(-26.4675658973843,-13.5022779556171,
111.933438751553)) ;
#172024 = CARTESIAN_POINT('Ctrl Pts',(-26.4911724058639,-13.4963851494492,
112.005340368792)) ;
#172025 = CARTESIAN_POINT('Ctrl Pts',(-26.5072441166408,-13.2068554623175,
112.018962167354)) ;
#172026 = CARTESIAN_POINT('Ctrl Pts',(-26.5304952118972,-13.2211688965324,
112.089781253125)) ;
#172027 = CARTESIAN_POINT('Ctrl Pts',(-26.6042990591768,-13.2211688373046,
112.065550223195)) ;
#172028 = CARTESIAN_POINT('Ctrl Pts',(-26.6781029064563,-13.2211687780768,
112.041319193264)) ;
#172029 = CARTESIAN_POINT('Ctrl Pts',(-26.6548518111999,-13.2068553438618,
111.970500107494)) ;
#172030 = CARTESIAN_POINT('Ctrl Pts',(-26.6316007159434,-13.1925419096468,
111.899681021723)) ;
#172031 = CARTESIAN_POINT('Ctrl Pts',(-26.5577968686638,-13.1925419688746,
111.923912051654)) ;
#172032 = CARTESIAN_POINT('Ctrl Pts',(-26.4839930213843,-13.1925420281025,
111.948143081584)) ;
#172033 = CARTESIAN_POINT('Ctrl Pts',(-26.5072441166408,-13.2068554623175,
112.018962167354)) ;
#172034 = CARTESIAN_POINT('Ctrl Pts',(-26.5471201594015,-12.9311896303103,
112.104939986775)) ;
#172035 = CARTESIAN_POINT('Ctrl Pts',(-26.568356499574,-12.9647719930566,
112.169622453471)) ;
#172036 = CARTESIAN_POINT('Ctrl Pts',(-26.6421603504602,-12.9647719471212,
112.145391434527)) ;
#172037 = CARTESIAN_POINT('Ctrl Pts',(-26.7159642013465,-12.9647719011858,
112.121160415582)) ;
#172038 = CARTESIAN_POINT('Ctrl Pts',(-26.694727861174,-12.9311895384395,
112.056477948886)) ;
#172039 = CARTESIAN_POINT('Ctrl Pts',(-26.6734915210015,-12.8976071756931,
111.99179548219)) ;
#172040 = CARTESIAN_POINT('Ctrl Pts',(-26.5996876701152,-12.8976072216285,
112.016026501135)) ;
#172041 = CARTESIAN_POINT('Ctrl Pts',(-26.525883819229,-12.8976072675639,
112.04025752008)) ;
#172042 = CARTESIAN_POINT('Ctrl Pts',(-26.5471201594015,-12.9311896303103,
112.104939986775)) ;
#172043 = CARTESIAN_POINT('Ctrl Pts',(-26.6089561868409,-12.6901579122719,
112.257741738305)) ;
#172044 = CARTESIAN_POINT('Ctrl Pts',(-26.6266427444742,-12.7406206917642,
112.311612139959)) ;
#172045 = CARTESIAN_POINT('Ctrl Pts',(-26.7004465968938,-12.7406206607923,
112.287381125685)) ;
#172046 = CARTESIAN_POINT('Ctrl Pts',(-26.7742504493134,-12.7406206298204,
112.26315011141)) ;
#172047 = CARTESIAN_POINT('Ctrl Pts',(-26.75656389168,-12.6901578503282,112.209279709756)) ;
#172048 = CARTESIAN_POINT('Ctrl Pts',(-26.7388773340467,-12.639695070836,
112.155409308102)) ;
#172049 = CARTESIAN_POINT('Ctrl Pts',(-26.6650734816271,-12.6396951018078,
112.179640322377)) ;
#172050 = CARTESIAN_POINT('Ctrl Pts',(-26.5912696292076,-12.6396951327797,
112.203871336652)) ;
#172051 = CARTESIAN_POINT('Ctrl Pts',(-26.6089561868409,-12.6901579122719,
112.257741738305)) ;
#172052 = CARTESIAN_POINT('Ctrl Pts',(-26.6885029037196,-12.5020099307821,
112.464646899328)) ;
#172053 = CARTESIAN_POINT('Ctrl Pts',(-26.7013942584965,-12.5656860202673,
112.503911886632)) ;
#172054 = CARTESIAN_POINT('Ctrl Pts',(-26.775198111099,-12.565686002392,112.479680872915)) ;
#172055 = CARTESIAN_POINT('Ctrl Pts',(-26.8490019637015,-12.5656859845167,
112.455449859197)) ;
#172056 = CARTESIAN_POINT('Ctrl Pts',(-26.8361106089246,-12.5020098950315,
112.416184871893)) ;
#172057 = CARTESIAN_POINT('Ctrl Pts',(-26.8232192541478,-12.4383338055463,
112.376919884588)) ;
#172058 = CARTESIAN_POINT('Ctrl Pts',(-26.7494154015452,-12.4383338234216,
112.401150898306)) ;
#172059 = CARTESIAN_POINT('Ctrl Pts',(-26.6756115489428,-12.4383338412968,
112.425381912023)) ;
#172060 = CARTESIAN_POINT('Ctrl Pts',(-26.6885029037196,-12.5020099307821,
112.464646899328)) ;
#172061 = CARTESIAN_POINT('Ctrl Pts',(-26.7819225494163,-12.3786471033838,
112.713516599138)) ;
#172062 = CARTESIAN_POINT('Ctrl Pts',(-26.789048763939,-12.451033969766,112.735221899233)) ;
#172063 = CARTESIAN_POINT('Ctrl Pts',(-26.8628526146505,-12.4510339632927,
112.710990879756)) ;
#172064 = CARTESIAN_POINT('Ctrl Pts',(-26.9366564653619,-12.4510339568193,
112.686759860279)) ;
#172065 = CARTESIAN_POINT('Ctrl Pts',(-26.9295302508393,-12.378647090437,
112.665054560184)) ;
#172066 = CARTESIAN_POINT('Ctrl Pts',(-26.9224040363165,-12.3062602240548,
112.64334926009)) ;
#172067 = CARTESIAN_POINT('Ctrl Pts',(-26.848600185605,-12.3062602305281,
112.667580279567)) ;
#172068 = CARTESIAN_POINT('Ctrl Pts',(-26.7747963348935,-12.3062602370015,
112.691811299044)) ;
#172069 = CARTESIAN_POINT('Ctrl Pts',(-26.7819225494163,-12.3786471033838,
112.713516599138)) ;
#172070 = CARTESIAN_POINT('Ctrl Pts',(-26.8814570402713,-12.3306796608346,
112.981418521478)) ;
#172071 = CARTESIAN_POINT('Ctrl Pts',(-26.8823738632145,-12.4065247391554,
112.984211016587)) ;
#172072 = CARTESIAN_POINT('Ctrl Pts',(-26.9561777123211,-12.4065247391449,
112.959979992222)) ;
#172073 = CARTESIAN_POINT('Ctrl Pts',(-27.0299815614278,-12.4065247391344,
112.935748967856)) ;
#172074 = CARTESIAN_POINT('Ctrl Pts',(-27.0290647384846,-12.3306796608136,
112.932956472747)) ;
#172075 = CARTESIAN_POINT('Ctrl Pts',(-27.0281479155415,-12.2548345824928,
112.930163977638)) ;
#172076 = CARTESIAN_POINT('Ctrl Pts',(-26.9543440664348,-12.2548345825033,
112.954395002003)) ;
#172077 = CARTESIAN_POINT('Ctrl Pts',(-26.8805402173282,-12.2548345825139,
112.978626026368)) ;
#172078 = CARTESIAN_POINT('Ctrl Pts',(-26.8814570402713,-12.3306796608346,
112.981418521478)) ;
#172079 = CARTESIAN_POINT('Ctrl Pts',(-26.9826355598295,-12.360155377245,
113.254016856092)) ;
#172080 = CARTESIAN_POINT('Ctrl Pts',(-26.977225112592,-12.4340571826112,
113.23753750698)) ;
#172081 = CARTESIAN_POINT('Ctrl Pts',(-27.051028959111,-12.4340571856698,
113.213306474733)) ;
#172082 = CARTESIAN_POINT('Ctrl Pts',(-27.1248328056299,-12.4340571887285,
113.189075442486)) ;
#172083 = CARTESIAN_POINT('Ctrl Pts',(-27.1302432528673,-12.3601553833623,
113.205554791598)) ;
#172084 = CARTESIAN_POINT('Ctrl Pts',(-27.1356537001047,-12.2862535779961,
113.22203414071)) ;
#172085 = CARTESIAN_POINT('Ctrl Pts',(-27.0618498535858,-12.2862535749374,
113.246265172957)) ;
#172086 = CARTESIAN_POINT('Ctrl Pts',(-26.9880460070669,-12.2862535718788,
113.270496205204)) ;
#172087 = CARTESIAN_POINT('Ctrl Pts',(-26.9826355598295,-12.360155377245,
113.254016856092)) ;
#172088 = CARTESIAN_POINT('Ctrl Pts',(-27.077657915506,-12.4653999327267,
113.508037936239)) ;
#172089 = CARTESIAN_POINT('Ctrl Pts',(-27.0663369176674,-12.5320640126139,
113.473556003555)) ;
#172090 = CARTESIAN_POINT('Ctrl Pts',(-27.1401407623689,-12.5320640153815,
113.449324965773)) ;
#172091 = CARTESIAN_POINT('Ctrl Pts',(-27.2139446070704,-12.5320640181491,
113.42509392799)) ;
#172092 = CARTESIAN_POINT('Ctrl Pts',(-27.225265604909,-12.4653999382619,
113.459575860674)) ;
#172093 = CARTESIAN_POINT('Ctrl Pts',(-27.2365866027476,-12.3987358583746,
113.494057793358)) ;
#172094 = CARTESIAN_POINT('Ctrl Pts',(-27.1627827580461,-12.398735855607,
113.51828883114)) ;
#172095 = CARTESIAN_POINT('Ctrl Pts',(-27.0889789133446,-12.3987358528394,
113.542519868923)) ;
#172096 = CARTESIAN_POINT('Ctrl Pts',(-27.077657915506,-12.4653999327267,
113.508037936239)) ;
#172097 = CARTESIAN_POINT('Ctrl Pts',(-27.1610926480351,-12.6388027493961,
113.726711458191)) ;
#172098 = CARTESIAN_POINT('Ctrl Pts',(-27.1446624041515,-12.6934585985942,
113.67666758634)) ;
#172099 = CARTESIAN_POINT('Ctrl Pts',(-27.2184662475862,-12.6934585991624,
113.652436544699)) ;
#172100 = CARTESIAN_POINT('Ctrl Pts',(-27.2922700910208,-12.6934585997305,
113.628205503058)) ;
#172101 = CARTESIAN_POINT('Ctrl Pts',(-27.3087003349045,-12.6388027505324,
113.678249374909)) ;
#172102 = CARTESIAN_POINT('Ctrl Pts',(-27.3251305787881,-12.5841469013344,
113.728293246759)) ;
#172103 = CARTESIAN_POINT('Ctrl Pts',(-27.2513267353534,-12.5841469007662,
113.7525242884)) ;
#172104 = CARTESIAN_POINT('Ctrl Pts',(-27.1775228919187,-12.584146900198,
113.776755330041)) ;
#172105 = CARTESIAN_POINT('Ctrl Pts',(-27.1610926480351,-12.6388027493961,
113.726711458191)) ;
#172106 = CARTESIAN_POINT('Ctrl Pts',(-27.2275682495383,-12.8679196576227,
113.893744616973)) ;
#172107 = CARTESIAN_POINT('Ctrl Pts',(-27.2072050678216,-12.9066583901742,
113.831721651003)) ;
#172108 = CARTESIAN_POINT('Ctrl Pts',(-27.281008910791,-12.9066583881138,
113.807490607945)) ;
#172109 = CARTESIAN_POINT('Ctrl Pts',(-27.3548127537603,-12.9066583860534,
113.783259564886)) ;
#172110 = CARTESIAN_POINT('Ctrl Pts',(-27.3751759354771,-12.8679196535019,
113.845282530856)) ;
#172111 = CARTESIAN_POINT('Ctrl Pts',(-27.3955391171939,-12.8291809209503,
113.907305496826)) ;
#172112 = CARTESIAN_POINT('Ctrl Pts',(-27.3217352742245,-12.8291809230107,
113.931536539885)) ;
#172113 = CARTESIAN_POINT('Ctrl Pts',(-27.2479314312551,-12.8291809250711,
113.955767582943)) ;
#172114 = CARTESIAN_POINT('Ctrl Pts',(-27.2275682495383,-12.8679196576227,
113.893744616973)) ;
#172115 = CARTESIAN_POINT('Ctrl Pts',(-27.2731763594975,-13.1373001966588,
113.997106443516)) ;
#172116 = CARTESIAN_POINT('Ctrl Pts',(-27.2503338197893,-13.1572855705815,
113.927531753129)) ;
#172117 = CARTESIAN_POINT('Ctrl Pts',(-27.3241376629308,-13.1572855672865,
113.903300710595)) ;
#172118 = CARTESIAN_POINT('Ctrl Pts',(-27.3979415060724,-13.1572855639915,
113.879069668061)) ;
#172119 = CARTESIAN_POINT('Ctrl Pts',(-27.4207840457806,-13.1373001900688,
113.948644358448)) ;
#172120 = CARTESIAN_POINT('Ctrl Pts',(-27.4436265854888,-13.1173148161461,
114.018219048835)) ;
#172121 = CARTESIAN_POINT('Ctrl Pts',(-27.3698227423472,-13.1173148194411,
114.042450091369)) ;
#172122 = CARTESIAN_POINT('Ctrl Pts',(-27.2960188992057,-13.1173148227361,
114.066681133903)) ;
#172123 = CARTESIAN_POINT('Ctrl Pts',(-27.2731763594975,-13.1373001966588,
113.997106443516)) ;
#172124 = CARTESIAN_POINT('Ctrl Pts',(-27.2951340941749,-13.4255234275119,
114.028599916302)) ;
#172125 = CARTESIAN_POINT('Ctrl Pts',(-27.2714569883122,-13.425412168657,
113.956483272091)) ;
#172126 = CARTESIAN_POINT('Ctrl Pts',(-27.3452608317934,-13.4254121666008,
113.932252230592)) ;
#172127 = CARTESIAN_POINT('Ctrl Pts',(-27.4190646752745,-13.4254121645446,
113.908021189092)) ;
#172128 = CARTESIAN_POINT('Ctrl Pts',(-27.4427417811371,-13.4255234233994,
113.980137833302)) ;
#172129 = CARTESIAN_POINT('Ctrl Pts',(-27.4664188869999,-13.4256346822543,
114.052254477513)) ;
#172130 = CARTESIAN_POINT('Ctrl Pts',(-27.3926150435187,-13.4256346843105,
114.076485519012)) ;
#172131 = CARTESIAN_POINT('Ctrl Pts',(-27.3188112000376,-13.4256346863667,
114.100716560512)) ;
#172132 = CARTESIAN_POINT('Ctrl Pts',(-27.2951340941749,-13.4255234275119,
114.028599916302)) ;
#172133 = CARTESIAN_POINT('Ctrl Pts',(-27.2928744217611,-13.7140381962048,
113.986224206085)) ;
#172134 = CARTESIAN_POINT('Ctrl Pts',(-27.2700548445963,-13.6937806023833,
113.916719455991)) ;
#172135 = CARTESIAN_POINT('Ctrl Pts',(-27.3438586880103,-13.6937806037046,
113.892488414287)) ;
#172136 = CARTESIAN_POINT('Ctrl Pts',(-27.4176625314244,-13.6937806050258,
113.868257372583)) ;
#172137 = CARTESIAN_POINT('Ctrl Pts',(-27.4404821085892,-13.7140381988474,
113.937762122677)) ;
#172138 = CARTESIAN_POINT('Ctrl Pts',(-27.4633016857539,-13.7342957926689,
114.007266872771)) ;
#172139 = CARTESIAN_POINT('Ctrl Pts',(-27.3894978423399,-13.7342957913476,
114.031497914475)) ;
#172140 = CARTESIAN_POINT('Ctrl Pts',(-27.3156939989258,-13.7342957900263,
114.055728956179)) ;
#172141 = CARTESIAN_POINT('Ctrl Pts',(-27.2928744217611,-13.7140381962048,
113.986224206085)) ;
#172142 = CARTESIAN_POINT('Ctrl Pts',(-27.2671958080113,-13.981013641758,
113.872559420686)) ;
#172143 = CARTESIAN_POINT('Ctrl Pts',(-27.2468695790329,-13.9420847851826,
113.810649006962)) ;
#172144 = CARTESIAN_POINT('Ctrl Pts',(-27.3206734215819,-13.9420847906692,
113.786417962623)) ;
#172145 = CARTESIAN_POINT('Ctrl Pts',(-27.3944772641309,-13.9420847961559,
113.762186918284)) ;
#172146 = CARTESIAN_POINT('Ctrl Pts',(-27.4148034931093,-13.9810136527313,
113.824097332009)) ;
#172147 = CARTESIAN_POINT('Ctrl Pts',(-27.4351297220877,-14.0199425093067,
113.886007745734)) ;
#172148 = CARTESIAN_POINT('Ctrl Pts',(-27.3613258795387,-14.01994250382,113.910238790073)) ;
#172149 = CARTESIAN_POINT('Ctrl Pts',(-27.2875220369897,-14.0199424983334,
113.934469834411)) ;
#172150 = CARTESIAN_POINT('Ctrl Pts',(-27.2671958080113,-13.981013641758,
113.872559420686)) ;
#172151 = CARTESIAN_POINT('Ctrl Pts',(-27.220752401802,-14.2077526521797,
113.695645507844)) ;
#172152 = CARTESIAN_POINT('Ctrl Pts',(-27.2043731538913,-14.1529353062713,
113.645756961726)) ;
#172153 = CARTESIAN_POINT('Ctrl Pts',(-27.2781769946741,-14.1529353151086,
113.621525912007)) ;
#172154 = CARTESIAN_POINT('Ctrl Pts',(-27.3519808354569,-14.1529353239459,
113.597294862289)) ;
#172155 = CARTESIAN_POINT('Ctrl Pts',(-27.3683600833676,-14.2077526698542,
113.647183408407)) ;
#172156 = CARTESIAN_POINT('Ctrl Pts',(-27.3847393312783,-14.2625700157626,
113.697071954526)) ;
#172157 = CARTESIAN_POINT('Ctrl Pts',(-27.3109354904955,-14.2625700069253,
113.721303004244)) ;
#172158 = CARTESIAN_POINT('Ctrl Pts',(-27.2371316497127,-14.2625699980881,
113.745534053962)) ;
#172159 = CARTESIAN_POINT('Ctrl Pts',(-27.220752401802,-14.2077526521797,
113.695645507844)) ;
#172160 = CARTESIAN_POINT('Ctrl Pts',(-27.1574305770192,-14.3782190485839,
113.46724600276)) ;
#172161 = CARTESIAN_POINT('Ctrl Pts',(-27.1461841198955,-14.3114194784183,
113.432991109356)) ;
#172162 = CARTESIAN_POINT('Ctrl Pts',(-27.2199879579173,-14.3114194884178,
113.408760051228)) ;
#172163 = CARTESIAN_POINT('Ctrl Pts',(-27.2937917959392,-14.3114194984174,
113.384528993101)) ;
#172164 = CARTESIAN_POINT('Ctrl Pts',(-27.3050382530629,-14.378219068583,
113.418783886505)) ;
#172165 = CARTESIAN_POINT('Ctrl Pts',(-27.3162847101867,-14.4450186387486,
113.453038779909)) ;
#172166 = CARTESIAN_POINT('Ctrl Pts',(-27.2424808721648,-14.445018628749,
113.477269838037)) ;
#172167 = CARTESIAN_POINT('Ctrl Pts',(-27.168677034143,-14.4450186187495,
113.501500896165)) ;
#172168 = CARTESIAN_POINT('Ctrl Pts',(-27.1574305770192,-14.3782190485839,
113.46724600276)) ;
#172169 = CARTESIAN_POINT('Ctrl Pts',(-27.082808992056,-14.4794481619843,
113.204510282952)) ;
#172170 = CARTESIAN_POINT('Ctrl Pts',(-27.0774900416989,-14.4054839121495,
113.188309618911)) ;
#172171 = CARTESIAN_POINT('Ctrl Pts',(-27.1512938766968,-14.4054839189219,
113.164078551572)) ;
#172172 = CARTESIAN_POINT('Ctrl Pts',(-27.2250977116947,-14.4054839256943,
113.139847484234)) ;
#172173 = CARTESIAN_POINT('Ctrl Pts',(-27.2304166620517,-14.4794481755291,
113.156048148275)) ;
#172174 = CARTESIAN_POINT('Ctrl Pts',(-27.2357356124087,-14.5534124253639,
113.172248812316)) ;
#172175 = CARTESIAN_POINT('Ctrl Pts',(-27.1619317774109,-14.5534124185915,
113.196479879654)) ;
#172176 = CARTESIAN_POINT('Ctrl Pts',(-27.088127942413,-14.5534124118191,
113.220710946992)) ;
#172177 = CARTESIAN_POINT('Ctrl Pts',(-27.082808992056,-14.4794481619843,
113.204510282952)) ;
#172178 = CARTESIAN_POINT('Ctrl Pts',(-27.0028815148515,-14.5047934992133,
112.925619875355)) ;
#172179 = CARTESIAN_POINT('Ctrl Pts',(-27.0038689041954,-14.4289527181918,
112.928627304678)) ;
#172180 = CARTESIAN_POINT('Ctrl Pts',(-27.0776727363725,-14.4289527172552,
112.904396228748)) ;
#172181 = CARTESIAN_POINT('Ctrl Pts',(-27.1514765685496,-14.4289527163185,
112.880165152818)) ;
#172182 = CARTESIAN_POINT('Ctrl Pts',(-27.1504891792057,-14.5047934973399,
112.877157723495)) ;
#172183 = CARTESIAN_POINT('Ctrl Pts',(-27.1495017898618,-14.5806342783613,
112.874150294172)) ;
#172184 = CARTESIAN_POINT('Ctrl Pts',(-27.0756979576847,-14.580634279298,
112.898381370102)) ;
#172185 = CARTESIAN_POINT('Ctrl Pts',(-27.0018941255076,-14.5806342802347,
112.922612446032)) ;
#172186 = CARTESIAN_POINT('Ctrl Pts',(-27.0028815148515,-14.5047934992133,
112.925619875355)) ;
#172187 = CARTESIAN_POINT('Ctrl Pts',(-26.9239578130133,-14.4522183736054,
112.649725923238)) ;
#172188 = CARTESIAN_POINT('Ctrl Pts',(-26.9311917662438,-14.3799386549208,
112.671759378456)) ;
#172189 = CARTESIAN_POINT('Ctrl Pts',(-27.0049955962026,-14.3799386416776,
112.647528295769)) ;
#172190 = CARTESIAN_POINT('Ctrl Pts',(-27.0787994261614,-14.3799386284344,
112.623297213083)) ;
#172191 = CARTESIAN_POINT('Ctrl Pts',(-27.0715654729308,-14.452218347119,
112.601263757865)) ;
#172192 = CARTESIAN_POINT('Ctrl Pts',(-27.0643315197003,-14.5244980658035,
112.579230302647)) ;
#172193 = CARTESIAN_POINT('Ctrl Pts',(-26.9905276897416,-14.5244980790467,
112.603461385334)) ;
#172194 = CARTESIAN_POINT('Ctrl Pts',(-26.9167238597828,-14.5244980922899,
112.62769246802)) ;
#172195 = CARTESIAN_POINT('Ctrl Pts',(-26.9239578130133,-14.4522183736054,
112.649725923238)) ;
#172196 = CARTESIAN_POINT('Ctrl Pts',(-26.8526625334306,-14.3254100791536,
112.39709109002)) ;
#172197 = CARTESIAN_POINT('Ctrl Pts',(-26.8656188998339,-14.2618795112896,
112.436554092626)) ;
#172198 = CARTESIAN_POINT('Ctrl Pts',(-26.9394227290838,-14.2618794820993,
112.41232300778)) ;
#172199 = CARTESIAN_POINT('Ctrl Pts',(-27.0132265583337,-14.261879452909,
112.388091922934)) ;
#172200 = CARTESIAN_POINT('Ctrl Pts',(-27.0002701919304,-14.325410020773,
112.348628920329)) ;
#172201 = CARTESIAN_POINT('Ctrl Pts',(-26.9873138255271,-14.3889405886369,
112.309165917724)) ;
#172202 = CARTESIAN_POINT('Ctrl Pts',(-26.9135099962773,-14.3889406178272,
112.333397002569)) ;
#172203 = CARTESIAN_POINT('Ctrl Pts',(-26.8397061670274,-14.3889406470175,
112.357628087415)) ;
#172204 = CARTESIAN_POINT('Ctrl Pts',(-26.8526625334306,-14.3254100791536,
112.39709109002)) ;
#172205 = CARTESIAN_POINT('Ctrl Pts',(-26.7949314683662,-14.1342773327245,
112.185876310005)) ;
#172206 = CARTESIAN_POINT('Ctrl Pts',(-26.8126691907285,-14.0839997344191,
112.239902551541)) ;
#172207 = CARTESIAN_POINT('Ctrl Pts',(-26.8864730213214,-14.0839996884698,
112.215671470786)) ;
#172208 = CARTESIAN_POINT('Ctrl Pts',(-26.9602768519143,-14.0839996425206,
112.191440390031)) ;
#172209 = CARTESIAN_POINT('Ctrl Pts',(-26.942539129552,-14.134277240826,112.137414148495)) ;
#172210 = CARTESIAN_POINT('Ctrl Pts',(-26.9248014071897,-14.1845548391315,
112.083387906959)) ;
#172211 = CARTESIAN_POINT('Ctrl Pts',(-26.8509975765968,-14.1845548850807,
112.107618987714)) ;
#172212 = CARTESIAN_POINT('Ctrl Pts',(-26.7771937460039,-14.18455493103,112.131850068469)) ;
#172213 = CARTESIAN_POINT('Ctrl Pts',(-26.7949314683662,-14.1342773327245,
112.185876310005)) ;
#172214 = CARTESIAN_POINT('Ctrl Pts',(-26.7552541991608,-13.8911855385649,
112.029520728032)) ;
#172215 = CARTESIAN_POINT('Ctrl Pts',(-26.7765224521165,-13.8578071985554,
112.094300396273)) ;
#172216 = CARTESIAN_POINT('Ctrl Pts',(-26.8503262857672,-13.8578071355948,
112.070069324832)) ;
#172217 = CARTESIAN_POINT('Ctrl Pts',(-26.9241301194179,-13.8578070726341,
112.04583825339)) ;
#172218 = CARTESIAN_POINT('Ctrl Pts',(-26.9028618664622,-13.8911854126436,
111.981058585149)) ;
#172219 = CARTESIAN_POINT('Ctrl Pts',(-26.8815936135065,-13.9245637526531,
111.916278916907)) ;
#172220 = CARTESIAN_POINT('Ctrl Pts',(-26.8077897798558,-13.9245638156137,
111.940509988349)) ;
#172221 = CARTESIAN_POINT('Ctrl Pts',(-26.7339859462051,-13.9245638785744,
111.96474105979)) ;
#172222 = CARTESIAN_POINT('Ctrl Pts',(-26.7552541991608,-13.8911855385649,
112.029520728032)) ;
#172223 = CARTESIAN_POINT('Ctrl Pts',(-26.7375900351982,-13.6134122049751,
111.940137889731)) ;
#172224 = CARTESIAN_POINT('Ctrl Pts',(-26.7608587062214,-13.5993787020081,
112.011010508807)) ;
#172225 = CARTESIAN_POINT('Ctrl Pts',(-26.8346625450312,-13.5993786244693,
111.98677945308)) ;
#172226 = CARTESIAN_POINT('Ctrl Pts',(-26.9084663838411,-13.5993785469305,
111.962548397352)) ;
#172227 = CARTESIAN_POINT('Ctrl Pts',(-26.8851977128179,-13.6134120498975,
111.891675778276)) ;
#172228 = CARTESIAN_POINT('Ctrl Pts',(-26.8619290417947,-13.6274455528644,
111.8208031592)) ;
#172229 = CARTESIAN_POINT('Ctrl Pts',(-26.7881252029848,-13.6274456304033,
111.845034214927)) ;
#172230 = CARTESIAN_POINT('Ctrl Pts',(-26.7143213641749,-13.6274457079421,
111.869265270655)) ;
#172231 = CARTESIAN_POINT('Ctrl Pts',(-26.7375900351982,-13.6134122049751,
111.940137889731)) ;
#172232 = CARTESIAN_POINT('Ctrl Pts',(-26.7438066268346,-13.3239481087795,
111.923780754692)) ;
#172233 = CARTESIAN_POINT('Ctrl Pts',(-26.7674051375456,-13.3301038926875,
111.995658012347)) ;
#172234 = CARTESIAN_POINT('Ctrl Pts',(-26.8412089830833,-13.3301038083537,
111.971426977112)) ;
#172235 = CARTESIAN_POINT('Ctrl Pts',(-26.915012828621,-13.3301037240199,
111.947195941876)) ;
#172236 = CARTESIAN_POINT('Ctrl Pts',(-26.89141431791,-13.3239479401119,111.875318684221)) ;
#172237 = CARTESIAN_POINT('Ctrl Pts',(-26.867815807199,-13.3177921562039,
111.803441426566)) ;
#172238 = CARTESIAN_POINT('Ctrl Pts',(-26.7940119616613,-13.3177922405377,
111.827672461802)) ;
#172239 = CARTESIAN_POINT('Ctrl Pts',(-26.7202081161236,-13.3177923248715,
111.851903497037)) ;
#172240 = CARTESIAN_POINT('Ctrl Pts',(-26.7438066268346,-13.3239481087795,
111.923780754692)) ;
#172241 = CARTESIAN_POINT('Ctrl Pts',(-26.7742483994232,-13.0394391601657,
111.980982516589)) ;
#172242 = CARTESIAN_POINT('Ctrl Pts',(-26.7964908947302,-13.0654672913968,
112.048729570246)) ;
#172243 = CARTESIAN_POINT('Ctrl Pts',(-26.8702947479032,-13.0654672055952,
112.024498558267)) ;
#172244 = CARTESIAN_POINT('Ctrl Pts',(-26.9440986010763,-13.0654671197937,
112.000267546287)) ;
#172245 = CARTESIAN_POINT('Ctrl Pts',(-26.9218561057693,-13.0394389885626,
111.93252049263)) ;
#172246 = CARTESIAN_POINT('Ctrl Pts',(-26.8996136104623,-13.0134108573315,
111.864773438973)) ;
#172247 = CARTESIAN_POINT('Ctrl Pts',(-26.8258097572892,-13.0134109431331,
111.889004450952)) ;
#172248 = CARTESIAN_POINT('Ctrl Pts',(-26.7520059041162,-13.0134110289346,
111.913235462932)) ;
#172249 = CARTESIAN_POINT('Ctrl Pts',(-26.7742483994232,-13.0394391601657,
111.980982516589)) ;
#172250 = CARTESIAN_POINT('Ctrl Pts',(-26.8274212650553,-12.7825526473998,
112.107498381163)) ;
#172251 = CARTESIAN_POINT('Ctrl Pts',(-26.8467171534129,-12.8265535642734,
112.166270545589)) ;
#172252 = CARTESIAN_POINT('Ctrl Pts',(-26.9205210143309,-12.8265534855134,
112.1420395572)) ;
#172253 = CARTESIAN_POINT('Ctrl Pts',(-26.994324875249,-12.8265534067534,
112.11780856881)) ;
#172254 = CARTESIAN_POINT('Ctrl Pts',(-26.9750289868914,-12.7825524898798,
112.059036404385)) ;
#172255 = CARTESIAN_POINT('Ctrl Pts',(-26.9557330985337,-12.7385515730062,
112.000264239959)) ;
#172256 = CARTESIAN_POINT('Ctrl Pts',(-26.8819292376157,-12.7385516517662,
112.024495228348)) ;
#172257 = CARTESIAN_POINT('Ctrl Pts',(-26.8081253766976,-12.7385517305262,
112.048726216737)) ;
#172258 = CARTESIAN_POINT('Ctrl Pts',(-26.8274212650553,-12.7825526473998,
112.107498381163)) ;
#172259 = CARTESIAN_POINT('Ctrl Pts',(-26.9007740305024,-12.5702685769134,
112.295283657163)) ;
#172260 = CARTESIAN_POINT('Ctrl Pts',(-26.9157144494704,-12.6291549421708,
112.340789764681)) ;
#172261 = CARTESIAN_POINT('Ctrl Pts',(-26.9895183175866,-12.629154878069,
112.316558798216)) ;
#172262 = CARTESIAN_POINT('Ctrl Pts',(-27.0633221857027,-12.6291548139673,
112.292327831751)) ;
#172263 = CARTESIAN_POINT('Ctrl Pts',(-27.0483817667347,-12.57026844871,112.246821724232)) ;
#172264 = CARTESIAN_POINT('Ctrl Pts',(-27.0334413477666,-12.5113820834526,
112.201315616714)) ;
#172265 = CARTESIAN_POINT('Ctrl Pts',(-26.9596374796504,-12.5113821475544,
112.225546583179)) ;
#172266 = CARTESIAN_POINT('Ctrl Pts',(-26.8858336115343,-12.5113822116561,
112.249777549644)) ;
#172267 = CARTESIAN_POINT('Ctrl Pts',(-26.9007740305024,-12.5702685769134,
112.295283657163)) ;
#172268 = CARTESIAN_POINT('Ctrl Pts',(-26.9885711727641,-12.4204037087553,
112.52741789663)) ;
#172269 = CARTESIAN_POINT('Ctrl Pts',(-26.9981337239508,-12.4898390976006,
112.556543886653)) ;
#172270 = CARTESIAN_POINT('Ctrl Pts',(-27.0719375972436,-12.4898390557385,
112.532312935955)) ;
#172271 = CARTESIAN_POINT('Ctrl Pts',(-27.1457414705363,-12.4898390138765,
112.508081985257)) ;
#172272 = CARTESIAN_POINT('Ctrl Pts',(-27.1361789193497,-12.4204036250312,
112.478955995234)) ;
#172273 = CARTESIAN_POINT('Ctrl Pts',(-27.1266163681631,-12.3509682361859,
112.449830005211)) ;
#172274 = CARTESIAN_POINT('Ctrl Pts',(-27.0528124948703,-12.3509682780479,
112.474060955909)) ;
#172275 = CARTESIAN_POINT('Ctrl Pts',(-26.9790086215775,-12.35096831991,112.498291906607)) ;
#172276 = CARTESIAN_POINT('Ctrl Pts',(-26.9885711727641,-12.4204037087553,
112.52741789663)) ;
#172277 = CARTESIAN_POINT('Ctrl Pts',(-27.0866504642312,-12.3408608148814,
112.790617772586)) ;
#172278 = CARTESIAN_POINT('Ctrl Pts',(-27.0901148756422,-12.4159518832881,
112.801169812833)) ;
#172279 = CARTESIAN_POINT('Ctrl Pts',(-27.163918752128,-12.4159518680668,
112.776938871861)) ;
#172280 = CARTESIAN_POINT('Ctrl Pts',(-27.2377226286139,-12.4159518528455,
112.752707930889)) ;
#172281 = CARTESIAN_POINT('Ctrl Pts',(-27.2342582172029,-12.3408607844389,
112.742155890641)) ;
#172282 = CARTESIAN_POINT('Ctrl Pts',(-27.230793805792,-12.2657697160322,
112.731603850393)) ;
#172283 = CARTESIAN_POINT('Ctrl Pts',(-27.1569899293061,-12.2657697312535,
112.755834791366)) ;
#172284 = CARTESIAN_POINT('Ctrl Pts',(-27.0831860528202,-12.2657697464747,
112.780065732338)) ;
#172285 = CARTESIAN_POINT('Ctrl Pts',(-27.0866504642312,-12.3408608148814,
112.790617772586)) ;
#172286 = CARTESIAN_POINT('Ctrl Pts',(-27.1877685515325,-12.3387915853932,
113.063220104296)) ;
#172287 = CARTESIAN_POINT('Ctrl Pts',(-27.184910564043,-12.414137720195,113.054515137628)) ;
#172288 = CARTESIAN_POINT('Ctrl Pts',(-27.2587144409321,-12.4141377338266,
113.030284197884)) ;
#172289 = CARTESIAN_POINT('Ctrl Pts',(-27.3325183178212,-12.4141377474583,
113.00605325814)) ;
#172290 = CARTESIAN_POINT('Ctrl Pts',(-27.3353763053107,-12.3387916126566,
113.014758224807)) ;
#172291 = CARTESIAN_POINT('Ctrl Pts',(-27.3382342928002,-12.2634454778548,
113.023463191475)) ;
#172292 = CARTESIAN_POINT('Ctrl Pts',(-27.2644304159111,-12.2634454642232,
113.047694131219)) ;
#172293 = CARTESIAN_POINT('Ctrl Pts',(-27.190626539022,-12.2634454505915,
113.071925070963)) ;
#172294 = CARTESIAN_POINT('Ctrl Pts',(-27.1877685515325,-12.3387915853932,
113.063220104296)) ;
#172295 = CARTESIAN_POINT('Ctrl Pts',(-27.2861151852823,-12.4137122483728,
113.327284210003)) ;
#172296 = CARTESIAN_POINT('Ctrl Pts',(-27.2771210197373,-12.4839393117036,
113.299889435052)) ;
#172297 = CARTESIAN_POINT('Ctrl Pts',(-27.3509248943576,-12.4839393535464,
113.275658488397)) ;
#172298 = CARTESIAN_POINT('Ctrl Pts',(-27.4247287689778,-12.4839393953892,
113.251427541742)) ;
#172299 = CARTESIAN_POINT('Ctrl Pts',(-27.4337229345229,-12.4137123320584,
113.278822316694)) ;
#172300 = CARTESIAN_POINT('Ctrl Pts',(-27.442717100068,-12.3434852687276,
113.306217091645)) ;
#172301 = CARTESIAN_POINT('Ctrl Pts',(-27.3689132254477,-12.3434852268848,
113.330448038299)) ;
#172302 = CARTESIAN_POINT('Ctrl Pts',(-27.2951093508274,-12.343485185042,
113.354678984954)) ;
#172303 = CARTESIAN_POINT('Ctrl Pts',(-27.2861151852823,-12.4137122483728,
113.327284210003)) ;
#172304 = CARTESIAN_POINT('Ctrl Pts',(-27.3754145778794,-12.5618189977429,
113.56362900409)) ;
#172305 = CARTESIAN_POINT('Ctrl Pts',(-27.3609100234517,-12.6218107314417,
113.519450473671)) ;
#172306 = CARTESIAN_POINT('Ctrl Pts',(-27.4347138930807,-12.6218107975561,
113.495219511814)) ;
#172307 = CARTESIAN_POINT('Ctrl Pts',(-27.5085177627096,-12.6218108636706,
113.470988549956)) ;
#172308 = CARTESIAN_POINT('Ctrl Pts',(-27.5230223171373,-12.5618191299718,
113.515167080375)) ;
#172309 = CARTESIAN_POINT('Ctrl Pts',(-27.5375268715649,-12.501827396273,
113.559345610793)) ;
#172310 = CARTESIAN_POINT('Ctrl Pts',(-27.4637230019359,-12.5018273301586,
113.583576572651)) ;
#172311 = CARTESIAN_POINT('Ctrl Pts',(-27.389919132307,-12.5018272640442,
113.607807534508)) ;
#172312 = CARTESIAN_POINT('Ctrl Pts',(-27.3754145778794,-12.5618189977429,
113.56362900409)) ;
#172313 = CARTESIAN_POINT('Ctrl Pts',(-27.4488280555374,-12.7689119270669,
113.752013523521)) ;
#172314 = CARTESIAN_POINT('Ctrl Pts',(-27.429905270597,-12.814533735282,113.694377775808)) ;
#172315 = CARTESIAN_POINT('Ctrl Pts',(-27.5037091335364,-12.8145338199658,
113.670146793575)) ;
#172316 = CARTESIAN_POINT('Ctrl Pts',(-27.5775129964758,-12.8145339046497,
113.645915811343)) ;
#172317 = CARTESIAN_POINT('Ctrl Pts',(-27.5964357814161,-12.7689120964346,
113.703551559055)) ;
#172318 = CARTESIAN_POINT('Ctrl Pts',(-27.6153585663564,-12.7232902882195,
113.761187306768)) ;
#172319 = CARTESIAN_POINT('Ctrl Pts',(-27.541554703417,-12.7232902035356,
113.785418289001)) ;
#172320 = CARTESIAN_POINT('Ctrl Pts',(-27.4677508404777,-12.7232901188518,
113.809649271233)) ;
#172321 = CARTESIAN_POINT('Ctrl Pts',(-27.4488280555374,-12.7689119270669,
113.752013523521)) ;
#172322 = CARTESIAN_POINT('Ctrl Pts',(-27.5035776459415,-13.0251682484426,
113.883107535979)) ;
#172323 = CARTESIAN_POINT('Ctrl Pts',(-27.4815419694659,-13.052967781727,
113.815990422836)) ;
#172324 = CARTESIAN_POINT('Ctrl Pts',(-27.5553458241622,-13.0529678764172,
113.791759415496)) ;
#172325 = CARTESIAN_POINT('Ctrl Pts',(-27.6291496788585,-13.0529679711075,
113.767528408156)) ;
#172326 = CARTESIAN_POINT('Ctrl Pts',(-27.6511853553341,-13.025168437823,
113.834645521299)) ;
#172327 = CARTESIAN_POINT('Ctrl Pts',(-27.6732210318097,-12.9973689045386,
113.901762634441)) ;
#172328 = CARTESIAN_POINT('Ctrl Pts',(-27.5994171771134,-12.9973688098484,
113.925993641781)) ;
#172329 = CARTESIAN_POINT('Ctrl Pts',(-27.5256133224171,-12.9973687151582,
113.950224649121)) ;
#172330 = CARTESIAN_POINT('Ctrl Pts',(-27.5035776459415,-13.0251682484426,
113.883107535979)) ;
#172331 = CARTESIAN_POINT('Ctrl Pts',(-27.5351792728666,-13.3082750938872,
113.943914512976)) ;
#172332 = CARTESIAN_POINT('Ctrl Pts',(-27.5116376544627,-13.3163504016851,
113.872210543615)) ;
#172333 = CARTESIAN_POINT('Ctrl Pts',(-27.5854415007842,-13.3163504980826,
113.847979510767)) ;
#172334 = CARTESIAN_POINT('Ctrl Pts',(-27.6592453471057,-13.31635059448,113.823748477919)) ;
#172335 = CARTESIAN_POINT('Ctrl Pts',(-27.6827869655096,-13.3082752866821,
113.895452447279)) ;
#172336 = CARTESIAN_POINT('Ctrl Pts',(-27.7063285839134,-13.3001999788842,
113.967156416639)) ;
#172337 = CARTESIAN_POINT('Ctrl Pts',(-27.6325247375919,-13.3001998824867,
113.991387449487)) ;
#172338 = CARTESIAN_POINT('Ctrl Pts',(-27.5587208912704,-13.3001997860893,
114.015618482336)) ;
#172339 = CARTESIAN_POINT('Ctrl Pts',(-27.5351792728666,-13.3082750938872,
113.943914512976)) ;
#172340 = CARTESIAN_POINT('Ctrl Pts',(-27.5426920454856,-13.5983478962611,
113.931443511884)) ;
#172341 = CARTESIAN_POINT('Ctrl Pts',(-27.5193221646225,-13.5861829357955,
113.860262627273)) ;
#172342 = CARTESIAN_POINT('Ctrl Pts',(-27.5931260031213,-13.5861830266329,
113.836031570598)) ;
#172343 = CARTESIAN_POINT('Ctrl Pts',(-27.6669298416201,-13.5861831174704,
113.811800513923)) ;
#172344 = CARTESIAN_POINT('Ctrl Pts',(-27.6902997224832,-13.5983480779361,
113.882981398534)) ;
#172345 = CARTESIAN_POINT('Ctrl Pts',(-27.7136696033462,-13.6105130384017,
113.954162283145)) ;
#172346 = CARTESIAN_POINT('Ctrl Pts',(-27.6398657648474,-13.6105129475642,
113.97839333982)) ;
#172347 = CARTESIAN_POINT('Ctrl Pts',(-27.5660619263486,-13.6105128567267,
114.002624396495)) ;
#172348 = CARTESIAN_POINT('Ctrl Pts',(-27.5426920454856,-13.5983478962611,
113.931443511884)) ;
#172349 = CARTESIAN_POINT('Ctrl Pts',(-27.5263734044367,-13.8761876349326,
113.846318938576)) ;
#172350 = CARTESIAN_POINT('Ctrl Pts',(-27.5048406247926,-13.8446061027284,
113.780733567751)) ;
#172351 = CARTESIAN_POINT('Ctrl Pts',(-27.5786444566591,-13.8446061808087,
113.756502490876)) ;
#172352 = CARTESIAN_POINT('Ctrl Pts',(-27.6524482885256,-13.8446062588889,
113.732271414)) ;
#172353 = CARTESIAN_POINT('Ctrl Pts',(-27.6739810681696,-13.8761877910931,
113.797856784825)) ;
#172354 = CARTESIAN_POINT('Ctrl Pts',(-27.6955138478137,-13.9077693232973,
113.863442155649)) ;
#172355 = CARTESIAN_POINT('Ctrl Pts',(-27.6217100159472,-13.907769245217,
113.887673232525)) ;
#172356 = CARTESIAN_POINT('Ctrl Pts',(-27.5479061840807,-13.9077691671368,
113.911904309401)) ;
#172357 = CARTESIAN_POINT('Ctrl Pts',(-27.5263734044367,-13.8761876349326,
113.846318938576)) ;
#172358 = CARTESIAN_POINT('Ctrl Pts',(-27.4877132850847,-14.1226645874526,
113.692922737031)) ;
#172359 = CARTESIAN_POINT('Ctrl Pts',(-27.4695845649599,-14.0738264529784,
113.637705582096)) ;
#172360 = CARTESIAN_POINT('Ctrl Pts',(-27.5433883924307,-14.0738265118824,
113.613474491831)) ;
#172361 = CARTESIAN_POINT('Ctrl Pts',(-27.6171922199014,-14.0738265707863,
113.589243401567)) ;
#172362 = CARTESIAN_POINT('Ctrl Pts',(-27.6353209400262,-14.1226647052604,
113.644460556502)) ;
#172363 = CARTESIAN_POINT('Ctrl Pts',(-27.653449660151,-14.1715028397345,
113.699677711437)) ;
#172364 = CARTESIAN_POINT('Ctrl Pts',(-27.5796458326802,-14.1715027808306,
113.723908801702)) ;
#172365 = CARTESIAN_POINT('Ctrl Pts',(-27.5058420052094,-14.1715027219267,
113.748139891966)) ;
#172366 = CARTESIAN_POINT('Ctrl Pts',(-27.4877132850847,-14.1226645874526,
113.692922737031)) ;
#172367 = CARTESIAN_POINT('Ctrl Pts',(-27.4306473190199,-14.3171342011777,
113.483654238532)) ;
#172368 = CARTESIAN_POINT('Ctrl Pts',(-27.417209160534,-14.2546443269057,
113.442723777381)) ;
#172369 = CARTESIAN_POINT('Ctrl Pts',(-27.491012985715,-14.2546443659289,
113.418492680142)) ;
#172370 = CARTESIAN_POINT('Ctrl Pts',(-27.5648168108959,-14.2546444049521,
113.394261582903)) ;
#172371 = CARTESIAN_POINT('Ctrl Pts',(-27.5782549693818,-14.3171342792242,
113.435192044054)) ;
#172372 = CARTESIAN_POINT('Ctrl Pts',(-27.5916931278677,-14.3796241534962,
113.476122505205)) ;
#172373 = CARTESIAN_POINT('Ctrl Pts',(-27.5178893026867,-14.379624114473,
113.500353602444)) ;
#172374 = CARTESIAN_POINT('Ctrl Pts',(-27.4440854775058,-14.3796240754498,
113.524584699683)) ;
#172375 = CARTESIAN_POINT('Ctrl Pts',(-27.4306473190199,-14.3171342011777,
113.483654238532)) ;
#172376 = CARTESIAN_POINT('Ctrl Pts',(-27.3601955150723,-14.4470643657725,
113.233728201309)) ;
#172377 = CARTESIAN_POINT('Ctrl Pts',(-27.3523873320976,-14.375408398759,
113.209945737037)) ;
#172378 = CARTESIAN_POINT('Ctrl Pts',(-27.4261911567725,-14.3754084186234,
113.185714638256)) ;
#172379 = CARTESIAN_POINT('Ctrl Pts',(-27.4999949814474,-14.3754084384878,
113.161483539476)) ;
#172380 = CARTESIAN_POINT('Ctrl Pts',(-27.5078031644221,-14.4470644055013,
113.185266003749)) ;
#172381 = CARTESIAN_POINT('Ctrl Pts',(-27.5156113473968,-14.5187203725148,
113.209048468021)) ;
#172382 = CARTESIAN_POINT('Ctrl Pts',(-27.4418075227219,-14.5187203526504,
113.233279566802)) ;
#172383 = CARTESIAN_POINT('Ctrl Pts',(-27.368003698047,-14.5187203327861,
113.257510665582)) ;
#172384 = CARTESIAN_POINT('Ctrl Pts',(-27.3601955150723,-14.4470643657725,
113.233728201309)) ;
#172385 = CARTESIAN_POINT('Ctrl Pts',(-27.2816288073246,-14.503923953364,
112.958964415876)) ;
#172386 = CARTESIAN_POINT('Ctrl Pts',(-27.280028179883,-14.4281893560193,
112.954089164008)) ;
#172387 = CARTESIAN_POINT('Ctrl Pts',(-27.3538320062244,-14.4281893585944,
112.929858070304)) ;
#172388 = CARTESIAN_POINT('Ctrl Pts',(-27.4276358325657,-14.4281893611695,
112.905626976599)) ;
#172389 = CARTESIAN_POINT('Ctrl Pts',(-27.4292364600073,-14.5039239585142,
112.910502228467)) ;
#172390 = CARTESIAN_POINT('Ctrl Pts',(-27.4308370874489,-14.5796585558589,
112.915377480335)) ;
#172391 = CARTESIAN_POINT('Ctrl Pts',(-27.3570332611075,-14.5796585532838,
112.93960857404)) ;
#172392 = CARTESIAN_POINT('Ctrl Pts',(-27.2832294347662,-14.5796585507087,
112.963839667744)) ;
#172393 = CARTESIAN_POINT('Ctrl Pts',(-27.2816288073246,-14.503923953364,
112.958964415876)) ;
#172394 = CARTESIAN_POINT('Ctrl Pts',(-27.2014946791726,-14.4828378904359,
112.679399169153)) ;
#172395 = CARTESIAN_POINT('Ctrl Pts',(-27.2062211107245,-14.4084605775559,
112.693795117939)) ;
#172396 = CARTESIAN_POINT('Ctrl Pts',(-27.2800249401893,-14.4084605673929,
112.669564033748)) ;
#172397 = CARTESIAN_POINT('Ctrl Pts',(-27.3538287696541,-14.40846055723,112.645332949557)) ;
#172398 = CARTESIAN_POINT('Ctrl Pts',(-27.3491023381022,-14.48283787011,112.630937000771)) ;
#172399 = CARTESIAN_POINT('Ctrl Pts',(-27.3443759065502,-14.5572151829901,
112.616541051985)) ;
#172400 = CARTESIAN_POINT('Ctrl Pts',(-27.2705720770854,-14.557215193153,
112.640772136176)) ;
#172401 = CARTESIAN_POINT('Ctrl Pts',(-27.1967682476206,-14.557215203316,
112.665003220367)) ;
#172402 = CARTESIAN_POINT('Ctrl Pts',(-27.2014946791726,-14.4828378904359,
112.679399169153)) ;
#172403 = CARTESIAN_POINT('Ctrl Pts',(-27.1263680307239,-14.385601171439,
112.415108437441)) ;
#172404 = CARTESIAN_POINT('Ctrl Pts',(-27.1370810693772,-14.3179002562645,
112.447738625353)) ;
#172405 = CARTESIAN_POINT('Ctrl Pts',(-27.2108849026355,-14.3179002385077,
112.423507552716)) ;
#172406 = CARTESIAN_POINT('Ctrl Pts',(-27.2846887358938,-14.3179002207509,
112.39927648008)) ;
#172407 = CARTESIAN_POINT('Ctrl Pts',(-27.2739756972405,-14.3856011359254,
112.366646292167)) ;
#172408 = CARTESIAN_POINT('Ctrl Pts',(-27.2632626585871,-14.4533020510999,
112.334016104255)) ;
#172409 = CARTESIAN_POINT('Ctrl Pts',(-27.1894588253288,-14.4533020688567,
112.358247176892)) ;
#172410 = CARTESIAN_POINT('Ctrl Pts',(-27.1156549920705,-14.4533020866135,
112.382478249528)) ;
#172411 = CARTESIAN_POINT('Ctrl Pts',(-27.1263680307239,-14.385601171439,
112.415108437441)) ;
#172412 = CARTESIAN_POINT('Ctrl Pts',(-27.0621909151168,-14.2179717447503,
112.184017247317)) ;
#172413 = CARTESIAN_POINT('Ctrl Pts',(-27.0781384399911,-14.1618723407489,
112.232590835486)) ;
#172414 = CARTESIAN_POINT('Ctrl Pts',(-27.1519422772901,-14.161872321804,
112.208359775157)) ;
#172415 = CARTESIAN_POINT('Ctrl Pts',(-27.2257461145892,-14.1618723028591,
112.184128714828)) ;
#172416 = CARTESIAN_POINT('Ctrl Pts',(-27.2097985897148,-14.2179717068605,
112.135555126658)) ;
#172417 = CARTESIAN_POINT('Ctrl Pts',(-27.1938510648405,-14.2740711108619,
112.086981538488)) ;
#172418 = CARTESIAN_POINT('Ctrl Pts',(-27.1200472275414,-14.2740711298068,
112.111212598818)) ;
#172419 = CARTESIAN_POINT('Ctrl Pts',(-27.0462433902424,-14.2740711487517,
112.135443659147)) ;
#172420 = CARTESIAN_POINT('Ctrl Pts',(-27.0621909151168,-14.2179717447503,
112.184017247317)) ;
#172421 = CARTESIAN_POINT('Ctrl Pts',(-27.0150398235501,-13.9957363810985,
112.005222445318)) ;
#172422 = CARTESIAN_POINT('Ctrl Pts',(-27.0350315354715,-13.9550697800569,
112.066113974601)) ;
#172423 = CARTESIAN_POINT('Ctrl Pts',(-27.1088353754445,-13.95506976129,112.041882922416)) ;
#172424 = CARTESIAN_POINT('Ctrl Pts',(-27.1826392154175,-13.9550697425231,
112.017651870231)) ;
#172425 = CARTESIAN_POINT('Ctrl Pts',(-27.162647503496,-13.9957363435648,
111.956760340948)) ;
#172426 = CARTESIAN_POINT('Ctrl Pts',(-27.1426557915745,-14.0364029446064,
111.895868811665)) ;
#172427 = CARTESIAN_POINT('Ctrl Pts',(-27.0688519516015,-14.0364029633733,
111.92009986385)) ;
#172428 = CARTESIAN_POINT('Ctrl Pts',(-26.9950481116286,-14.0364029821402,
111.944330916035)) ;
#172429 = CARTESIAN_POINT('Ctrl Pts',(-27.0150398235501,-13.9957363810985,
112.005222445318)) ;
#172430 = CARTESIAN_POINT('Ctrl Pts',(-26.9879423735838,-13.7291995183929,
111.88704329511)) ;
#172431 = CARTESIAN_POINT('Ctrl Pts',(-27.0105941912921,-13.707082237132,
111.956037077241)) ;
#172432 = CARTESIAN_POINT('Ctrl Pts',(-27.0843980337561,-13.7070822245354,
111.931806032644)) ;
#172433 = CARTESIAN_POINT('Ctrl Pts',(-27.1582018762201,-13.7070822119389,
111.907574988046)) ;
#172434 = CARTESIAN_POINT('Ctrl Pts',(-27.1355500585118,-13.7291994931998,
111.838581205914)) ;
#172435 = CARTESIAN_POINT('Ctrl Pts',(-27.1128982408035,-13.7513167744608,
111.769587423783)) ;
#172436 = CARTESIAN_POINT('Ctrl Pts',(-27.0390943983395,-13.7513167870574,
111.79381846838)) ;
#172437 = CARTESIAN_POINT('Ctrl Pts',(-26.9652905558756,-13.7513167996539,
111.818049512978)) ;
#172438 = CARTESIAN_POINT('Ctrl Pts',(-26.9879423735838,-13.7291995183929,
111.88704329511)) ;
#172439 = CARTESIAN_POINT('Ctrl Pts',(-26.9843581372536,-13.4423294051305,
111.840765762246)) ;
#172440 = CARTESIAN_POINT('Ctrl Pts',(-27.0080260400951,-13.440209694869,
111.912854375641)) ;
#172441 = CARTESIAN_POINT('Ctrl Pts',(-27.081829883601,-13.4402096875426,
111.888623334217)) ;
#172442 = CARTESIAN_POINT('Ctrl Pts',(-27.1556337271069,-13.4402096802161,
111.864392292792)) ;
#172443 = CARTESIAN_POINT('Ctrl Pts',(-27.1319658242654,-13.4423293904776,
111.792303679397)) ;
#172444 = CARTESIAN_POINT('Ctrl Pts',(-27.1082979214239,-13.444449100739,
111.720215066002)) ;
#172445 = CARTESIAN_POINT('Ctrl Pts',(-27.034494077918,-13.4444491080655,
111.744446107426)) ;
#172446 = CARTESIAN_POINT('Ctrl Pts',(-26.9606902344121,-13.444449115392,
111.76867714885)) ;
#172447 = CARTESIAN_POINT('Ctrl Pts',(-26.9843581372536,-13.4423294051305,
111.840765762246)) ;
#172448 = CARTESIAN_POINT('Ctrl Pts',(-27.0050610704701,-13.1524216120436,
111.868286429054)) ;
#172449 = CARTESIAN_POINT('Ctrl Pts',(-27.0280544057654,-13.1705421865172,
111.938320418437)) ;
#172450 = CARTESIAN_POINT('Ctrl Pts',(-27.1018582494374,-13.1705421848694,
111.914089377519)) ;
#172451 = CARTESIAN_POINT('Ctrl Pts',(-27.1756620931093,-13.1705421832215,
111.889858336601)) ;
#172452 = CARTESIAN_POINT('Ctrl Pts',(-27.152668757814,-13.1524216087479,
111.819824347217)) ;
#172453 = CARTESIAN_POINT('Ctrl Pts',(-27.1296754225186,-13.1343010342744,
111.749790357834)) ;
#172454 = CARTESIAN_POINT('Ctrl Pts',(-27.0558715788467,-13.1343010359222,
111.774021398752)) ;
#172455 = CARTESIAN_POINT('Ctrl Pts',(-26.9820677351747,-13.1343010375701,
111.798252439671)) ;
#172456 = CARTESIAN_POINT('Ctrl Pts',(-27.0050610704701,-13.1524216120436,
111.868286429054)) ;
#172457 = CARTESIAN_POINT('Ctrl Pts',(-27.0492012117308,-12.8827428706973,
111.967358039858)) ;
#172458 = CARTESIAN_POINT('Ctrl Pts',(-27.0698787059065,-12.9197213640829,
112.030338350789)) ;
#172459 = CARTESIAN_POINT('Ctrl Pts',(-27.143682549157,-12.9197213654279,
112.006107308587)) ;
#172460 = CARTESIAN_POINT('Ctrl Pts',(-27.2174863924074,-12.919721366773,
111.981876266384)) ;
#172461 = CARTESIAN_POINT('Ctrl Pts',(-27.1968088982317,-12.8827428733873,
111.918895955454)) ;
#172462 = CARTESIAN_POINT('Ctrl Pts',(-27.176131404056,-12.8457643800017,
111.855915644523)) ;
#172463 = CARTESIAN_POINT('Ctrl Pts',(-27.1023275608056,-12.8457643786566,
111.880146686725)) ;
#172464 = CARTESIAN_POINT('Ctrl Pts',(-27.0285237175551,-12.8457643773116,
111.904377728927)) ;
#172465 = CARTESIAN_POINT('Ctrl Pts',(-27.0492012117308,-12.8827428706973,
111.967358039858)) ;
#172466 = CARTESIAN_POINT('Ctrl Pts',(-27.1146617710616,-12.6504179680888,
112.131229509415)) ;
#172467 = CARTESIAN_POINT('Ctrl Pts',(-27.1315339429113,-12.7036746706006,
112.18261942249)) ;
#172468 = CARTESIAN_POINT('Ctrl Pts',(-27.2053377856061,-12.7036746730312,
112.158388378596)) ;
#172469 = CARTESIAN_POINT('Ctrl Pts',(-27.2791416283009,-12.7036746754618,
112.134157334701)) ;
#172470 = CARTESIAN_POINT('Ctrl Pts',(-27.2622694564512,-12.65041797295,112.082767421626)) ;
#172471 = CARTESIAN_POINT('Ctrl Pts',(-27.2453972846015,-12.5971612704382,
112.031377508551)) ;
#172472 = CARTESIAN_POINT('Ctrl Pts',(-27.1715934419067,-12.5971612680076,
112.055608552446)) ;
#172473 = CARTESIAN_POINT('Ctrl Pts',(-27.0977895992119,-12.597161265577,
112.07983959634)) ;
#172474 = CARTESIAN_POINT('Ctrl Pts',(-27.1146617710616,-12.6504179680888,
112.131229509415)) ;
#172475 = CARTESIAN_POINT('Ctrl Pts',(-27.1972630412984,-12.4733695384466,
112.347366409406)) ;
#172476 = CARTESIAN_POINT('Ctrl Pts',(-27.2091258740215,-12.5390682481556,
112.383498683763)) ;
#172477 = CARTESIAN_POINT('Ctrl Pts',(-27.2829297166078,-12.5390682494468,
112.359267639538)) ;
#172478 = CARTESIAN_POINT('Ctrl Pts',(-27.3567335591942,-12.5390682507379,
112.335036595313)) ;
#172479 = CARTESIAN_POINT('Ctrl Pts',(-27.3448707264711,-12.4733695410289,
112.298904320956)) ;
#172480 = CARTESIAN_POINT('Ctrl Pts',(-27.3330078937479,-12.4076708313198,
112.262772046599)) ;
#172481 = CARTESIAN_POINT('Ctrl Pts',(-27.2592040511616,-12.4076708300287,
112.287003090824)) ;
#172482 = CARTESIAN_POINT('Ctrl Pts',(-27.1854002085753,-12.4076708287375,
112.311234135049)) ;
#172483 = CARTESIAN_POINT('Ctrl Pts',(-27.1972630412984,-12.4733695384466,
112.347366409406)) ;
#172484 = CARTESIAN_POINT('Ctrl Pts',(-27.2924020500798,-12.3637277646619,
112.601520160583)) ;
#172485 = CARTESIAN_POINT('Ctrl Pts',(-27.2983761879379,-12.4371796156444,
112.619716420582)) ;
#172486 = CARTESIAN_POINT('Ctrl Pts',(-27.3721800314205,-12.4371796152465,
112.595485379087)) ;
#172487 = CARTESIAN_POINT('Ctrl Pts',(-27.4459838749031,-12.4371796148486,
112.571254337592)) ;
#172488 = CARTESIAN_POINT('Ctrl Pts',(-27.4400097370451,-12.3637277638662,
112.553058077593)) ;
#172489 = CARTESIAN_POINT('Ctrl Pts',(-27.434035599187,-12.2902759128838,
112.534861817595)) ;
#172490 = CARTESIAN_POINT('Ctrl Pts',(-27.3602317557044,-12.2902759132816,
112.55909285909)) ;
#172491 = CARTESIAN_POINT('Ctrl Pts',(-27.2864279122218,-12.2902759136795,
112.583323900585)) ;
#172492 = CARTESIAN_POINT('Ctrl Pts',(-27.2924020500798,-12.3637277646619,
112.601520160583)) ;
#172493 = CARTESIAN_POINT('Ctrl Pts',(-27.3927913486772,-12.3302633026411,
112.871950604607)) ;
#172494 = CARTESIAN_POINT('Ctrl Pts',(-27.3924958222733,-12.4061588446246,
112.871050478946)) ;
#172495 = CARTESIAN_POINT('Ctrl Pts',(-27.4662996670084,-12.406158844275,
112.846819441266)) ;
#172496 = CARTESIAN_POINT('Ctrl Pts',(-27.5401035117436,-12.4061588439253,
112.822588403586)) ;
#172497 = CARTESIAN_POINT('Ctrl Pts',(-27.5403990381475,-12.3302633019418,
112.823488529247)) ;
#172498 = CARTESIAN_POINT('Ctrl Pts',(-27.5406945645514,-12.2543677599582,
112.824388654909)) ;
#172499 = CARTESIAN_POINT('Ctrl Pts',(-27.4668907198163,-12.2543677603079,
112.848619692589)) ;
#172500 = CARTESIAN_POINT('Ctrl Pts',(-27.3930868750811,-12.2543677606575,
112.872850730269)) ;
#172501 = CARTESIAN_POINT('Ctrl Pts',(-27.3927913486772,-12.3302633026411,
112.871950604607)) ;
#172502 = CARTESIAN_POINT('Ctrl Pts',(-27.4930345233602,-12.3743151570883,
113.14182288393)) ;
#172503 = CARTESIAN_POINT('Ctrl Pts',(-27.486472782332,-12.4472453738058,
113.121836879682)) ;
#172504 = CARTESIAN_POINT('Ctrl Pts',(-27.5602766287209,-12.4472453760978,
113.097605847039)) ;
#172505 = CARTESIAN_POINT('Ctrl Pts',(-27.6340804751099,-12.4472453783898,
113.073374814396)) ;
#172506 = CARTESIAN_POINT('Ctrl Pts',(-27.640642216138,-12.3743151616723,
113.093360818644)) ;
#172507 = CARTESIAN_POINT('Ctrl Pts',(-27.6472039571662,-12.3013849449547,
113.113346822893)) ;
#172508 = CARTESIAN_POINT('Ctrl Pts',(-27.5734001107772,-12.3013849426627,
113.137577855536)) ;
#172509 = CARTESIAN_POINT('Ctrl Pts',(-27.4995962643883,-12.3013849403707,
113.161808888179)) ;
#172510 = CARTESIAN_POINT('Ctrl Pts',(-27.4930345233602,-12.3743151570883,
113.14182288393)) ;
#172511 = CARTESIAN_POINT('Ctrl Pts',(-27.5863812625094,-12.4928395526405,
113.390726218169)) ;
#172512 = CARTESIAN_POINT('Ctrl Pts',(-27.5740251224026,-12.5575998714036,
113.353091409372)) ;
#172513 = CARTESIAN_POINT('Ctrl Pts',(-27.6478289702466,-12.5575998792926,
113.328860381161)) ;
#172514 = CARTESIAN_POINT('Ctrl Pts',(-27.7216328180906,-12.5575998871817,
113.30462935295)) ;
#172515 = CARTESIAN_POINT('Ctrl Pts',(-27.7339889581974,-12.4928395684187,
113.342264161746)) ;
#172516 = CARTESIAN_POINT('Ctrl Pts',(-27.7463450983042,-12.4280792496557,
113.379898970542)) ;
#172517 = CARTESIAN_POINT('Ctrl Pts',(-27.6725412504602,-12.4280792417666,
113.404129998754)) ;
#172518 = CARTESIAN_POINT('Ctrl Pts',(-27.5987374026162,-12.4280792338775,
113.428361026965)) ;
#172519 = CARTESIAN_POINT('Ctrl Pts',(-27.5863812625094,-12.4928395526405,
113.390726218169)) ;
#172520 = CARTESIAN_POINT('Ctrl Pts',(-27.6674288059213,-12.6792484033362,
113.601904231307)) ;
#172521 = CARTESIAN_POINT('Ctrl Pts',(-27.6501339912232,-12.7310874670911,
113.549227016744)) ;
#172522 = CARTESIAN_POINT('Ctrl Pts',(-27.7239378402491,-12.7310874856029,
113.524995992133)) ;
#172523 = CARTESIAN_POINT('Ctrl Pts',(-27.7977416892751,-12.7310875041147,
113.500764967522)) ;
#172524 = CARTESIAN_POINT('Ctrl Pts',(-27.8150365039733,-12.6792484403597,
113.553442182085)) ;
#172525 = CARTESIAN_POINT('Ctrl Pts',(-27.8323313186715,-12.6274093766048,
113.606119396648)) ;
#172526 = CARTESIAN_POINT('Ctrl Pts',(-27.7585274696455,-12.627409358093,
113.630350421259)) ;
#172527 = CARTESIAN_POINT('Ctrl Pts',(-27.6847236206195,-12.6274093395813,
113.65458144587)) ;
#172528 = CARTESIAN_POINT('Ctrl Pts',(-27.6674288059213,-12.6792484033362,
113.601904231307)) ;
#172529 = CARTESIAN_POINT('Ctrl Pts',(-27.7297752283218,-12.9157037711306,
113.756592636286)) ;
#172530 = CARTESIAN_POINT('Ctrl Pts',(-27.7088310990503,-12.9511079256509,
113.69280019846)) ;
#172531 = CARTESIAN_POINT('Ctrl Pts',(-27.7826349472372,-12.9511079534963,
113.668569171294)) ;
#172532 = CARTESIAN_POINT('Ctrl Pts',(-27.8564387954241,-12.9511079813417,
113.644338144128)) ;
#172533 = CARTESIAN_POINT('Ctrl Pts',(-27.8773829246957,-12.9157038268213,
113.708130581953)) ;
#172534 = CARTESIAN_POINT('Ctrl Pts',(-27.8983270539673,-12.880299672301,
113.771923019778)) ;
#172535 = CARTESIAN_POINT('Ctrl Pts',(-27.8245232057804,-12.8802996444556,
113.796154046944)) ;
#172536 = CARTESIAN_POINT('Ctrl Pts',(-27.7507193575934,-12.8802996166102,
113.820385074111)) ;
#172537 = CARTESIAN_POINT('Ctrl Pts',(-27.7297752283218,-12.9157037711306,
113.756592636286)) ;
#172538 = CARTESIAN_POINT('Ctrl Pts',(-27.7712714115266,-13.1914441677562,
113.847288780652)) ;
#172539 = CARTESIAN_POINT('Ctrl Pts',(-27.748138134954,-13.2076474543041,
113.776828553575)) ;
#172540 = CARTESIAN_POINT('Ctrl Pts',(-27.8219419813756,-13.2076474957357,
113.752597521032)) ;
#172541 = CARTESIAN_POINT('Ctrl Pts',(-27.8957458277972,-13.2076475371673,
113.728366488488)) ;
#172542 = CARTESIAN_POINT('Ctrl Pts',(-27.9188791043698,-13.1914442506193,
113.798826715565)) ;
#172543 = CARTESIAN_POINT('Ctrl Pts',(-27.9420123809424,-13.1752409640713,
113.869286942643)) ;
#172544 = CARTESIAN_POINT('Ctrl Pts',(-27.8682085345208,-13.1752409226398,
113.893517975186)) ;
#172545 = CARTESIAN_POINT('Ctrl Pts',(-27.7944046880992,-13.1752408812082,
113.917749007729)) ;
#172546 = CARTESIAN_POINT('Ctrl Pts',(-27.7712714115266,-13.1914441677562,
113.847288780652)) ;
#172547 = CARTESIAN_POINT('Ctrl Pts',(-27.7885541463279,-13.4802992555045,
113.864652632934)) ;
#172548 = CARTESIAN_POINT('Ctrl Pts',(-27.7649109140841,-13.4763581958197,
113.792639163296)) ;
#172549 = CARTESIAN_POINT('Ctrl Pts',(-27.8387147567996,-13.4763582452253,
113.768408119464)) ;
#172550 = CARTESIAN_POINT('Ctrl Pts',(-27.9125185995151,-13.4763582946309,
113.744177075633)) ;
#172551 = CARTESIAN_POINT('Ctrl Pts',(-27.9361618317589,-13.4802993543157,
113.816190545271)) ;
#172552 = CARTESIAN_POINT('Ctrl Pts',(-27.9598050640028,-13.4842404140005,
113.888204014908)) ;
#172553 = CARTESIAN_POINT('Ctrl Pts',(-27.8860012212873,-13.4842403645949,
113.91243505874)) ;
#172554 = CARTESIAN_POINT('Ctrl Pts',(-27.8121973785718,-13.4842403151893,
113.936666102571)) ;
#172555 = CARTESIAN_POINT('Ctrl Pts',(-27.7885541463279,-13.4802992555045,
113.864652632934)) ;
#172556 = CARTESIAN_POINT('Ctrl Pts',(-27.7818265483523,-13.7664087624137,
113.808666272862)) ;
#172557 = CARTESIAN_POINT('Ctrl Pts',(-27.7593533008919,-13.7424862734231,
113.740216388272)) ;
#172558 = CARTESIAN_POINT('Ctrl Pts',(-27.8331571387186,-13.7424863290053,
113.715985329549)) ;
#172559 = CARTESIAN_POINT('Ctrl Pts',(-27.9069609765453,-13.7424863845875,
113.691754270827)) ;
#172560 = CARTESIAN_POINT('Ctrl Pts',(-27.9294342240057,-13.766408873578,
113.760204155418)) ;
#172561 = CARTESIAN_POINT('Ctrl Pts',(-27.9519074714661,-13.7903313625685,
113.828654040009)) ;
#172562 = CARTESIAN_POINT('Ctrl Pts',(-27.8781036336394,-13.7903313069864,
113.852885098731)) ;
#172563 = CARTESIAN_POINT('Ctrl Pts',(-27.8042997958127,-13.7903312514042,
113.877116157453)) ;
#172564 = CARTESIAN_POINT('Ctrl Pts',(-27.7818265483523,-13.7664087624137,
113.808666272862)) ;
#172565 = CARTESIAN_POINT('Ctrl Pts',(-27.7518733154646,-14.0278445854345,
113.681886834829)) ;
#172566 = CARTESIAN_POINT('Ctrl Pts',(-27.732194294108,-13.98563446645,113.621947712281)) ;
#172567 = CARTESIAN_POINT('Ctrl Pts',(-27.805998125884,-13.9856345227655,
113.597716635129)) ;
#172568 = CARTESIAN_POINT('Ctrl Pts',(-27.8798019576601,-13.985634579081,
113.573485557978)) ;
#172569 = CARTESIAN_POINT('Ctrl Pts',(-27.8994809790166,-14.0278446980655,
113.633424680526)) ;
#172570 = CARTESIAN_POINT('Ctrl Pts',(-27.9191600003732,-14.07005481705,113.693363803075)) ;
#172571 = CARTESIAN_POINT('Ctrl Pts',(-27.8453561685971,-14.0700547607345,
113.717594880226)) ;
#172572 = CARTESIAN_POINT('Ctrl Pts',(-27.7715523368211,-14.070054704419,
113.741825957378)) ;
#172573 = CARTESIAN_POINT('Ctrl Pts',(-27.7518733154646,-14.0278445854345,
113.681886834829)) ;
#172574 = CARTESIAN_POINT('Ctrl Pts',(-27.7020071019376,-14.2444016591037,
113.494631735179)) ;
#172575 = CARTESIAN_POINT('Ctrl Pts',(-27.6865130848051,-14.1870110797581,
113.447439460386)) ;
#172576 = CARTESIAN_POINT('Ctrl Pts',(-27.7603169106574,-14.1870111286872,
113.423208365192)) ;
#172577 = CARTESIAN_POINT('Ctrl Pts',(-27.8341207365098,-14.1870111776162,
113.398977269998)) ;
#172578 = CARTESIAN_POINT('Ctrl Pts',(-27.8496147536422,-14.2444017569618,
113.446169544791)) ;
#172579 = CARTESIAN_POINT('Ctrl Pts',(-27.8651087707747,-14.3017923363074,
113.493361819585)) ;
#172580 = CARTESIAN_POINT('Ctrl Pts',(-27.7913049449223,-14.3017922873783,
113.517592914779)) ;
#172581 = CARTESIAN_POINT('Ctrl Pts',(-27.71750111907,-14.3017922384493,113.541824009973)) ;
#172582 = CARTESIAN_POINT('Ctrl Pts',(-27.7020071019376,-14.2444016591037,
113.494631735179)) ;
#172583 = CARTESIAN_POINT('Ctrl Pts',(-27.6362880745386,-14.4026063876543,
113.259009109115)) ;
#172584 = CARTESIAN_POINT('Ctrl Pts',(-27.6260934718267,-14.3340872602138,
113.227957995732)) ;
#172585 = CARTESIAN_POINT('Ctrl Pts',(-27.699897292193,-14.3340872957345,
113.203726883828)) ;
#172586 = CARTESIAN_POINT('Ctrl Pts',(-27.7737011125594,-14.3340873312552,
113.179495771925)) ;
#172587 = CARTESIAN_POINT('Ctrl Pts',(-27.7838957152713,-14.4026064586957,
113.210546885308)) ;
#172588 = CARTESIAN_POINT('Ctrl Pts',(-27.7940903179833,-14.4711255861363,
113.241597998692)) ;
#172589 = CARTESIAN_POINT('Ctrl Pts',(-27.7202864976169,-14.4711255506156,
113.265829110596)) ;
#172590 = CARTESIAN_POINT('Ctrl Pts',(-27.6464826772506,-14.4711255150949,
113.290060222499)) ;
#172591 = CARTESIAN_POINT('Ctrl Pts',(-27.6362880745386,-14.4026063876543,
113.259009109115)) ;
#172592 = CARTESIAN_POINT('Ctrl Pts',(-27.5597118203589,-14.4903817315252,
112.990103568615)) ;
#172593 = CARTESIAN_POINT('Ctrl Pts',(-27.5555865779174,-14.4156342594261,
112.977538747483)) ;
#172594 = CARTESIAN_POINT('Ctrl Pts',(-27.6293903936794,-14.4156342751567,
112.953307621556)) ;
#172595 = CARTESIAN_POINT('Ctrl Pts',(-27.7031942094413,-14.4156342908872,
112.929076495628)) ;
#172596 = CARTESIAN_POINT('Ctrl Pts',(-27.7073194518829,-14.4903817629863,
112.94164131676)) ;
#172597 = CARTESIAN_POINT('Ctrl Pts',(-27.7114446943244,-14.5651292350854,
112.954206137892)) ;
#172598 = CARTESIAN_POINT('Ctrl Pts',(-27.6376408785625,-14.5651292193548,
112.97843726382)) ;
#172599 = CARTESIAN_POINT('Ctrl Pts',(-27.5638370628005,-14.5651292036242,
113.002668389747)) ;
#172600 = CARTESIAN_POINT('Ctrl Pts',(-27.5597118203589,-14.4903817315252,
112.990103568615)) ;
#172601 = CARTESIAN_POINT('Ctrl Pts',(-27.4797523581831,-14.5006966747965,
112.711230829165)) ;
#172602 = CARTESIAN_POINT('Ctrl Pts',(-27.4819346624663,-14.4251205193326,
112.71787777773)) ;
#172603 = CARTESIAN_POINT('Ctrl Pts',(-27.5557384764387,-14.425120510433,
112.693646646351)) ;
#172604 = CARTESIAN_POINT('Ctrl Pts',(-27.6295422904111,-14.4251205015334,
112.669415514973)) ;
#172605 = CARTESIAN_POINT('Ctrl Pts',(-27.6273599861279,-14.5006966569974,
112.662768566408)) ;
#172606 = CARTESIAN_POINT('Ctrl Pts',(-27.6251776818447,-14.5762728124613,
112.656121617843)) ;
#172607 = CARTESIAN_POINT('Ctrl Pts',(-27.5513738678723,-14.5762728213609,
112.680352749221)) ;
#172608 = CARTESIAN_POINT('Ctrl Pts',(-27.4775700538999,-14.5762728302605,
112.7045838806)) ;
#172609 = CARTESIAN_POINT('Ctrl Pts',(-27.4797523581831,-14.5006966747965,
112.711230829165)) ;
#172610 = CARTESIAN_POINT('Ctrl Pts',(-27.4018724922626,-14.4339382681578,
112.438561635708)) ;
#172611 = CARTESIAN_POINT('Ctrl Pts',(-27.410228957115,-14.3629125582236,
112.464014081264)) ;
#172612 = CARTESIAN_POINT('Ctrl Pts',(-27.4840327714468,-14.3629125229021,
112.43978295098)) ;
#172613 = CARTESIAN_POINT('Ctrl Pts',(-27.5578365857786,-14.3629124875806,
112.415551820697)) ;
#172614 = CARTESIAN_POINT('Ctrl Pts',(-27.5494801209262,-14.4339381975148,
112.39009937514)) ;
#172615 = CARTESIAN_POINT('Ctrl Pts',(-27.5411236560738,-14.504963907449,
112.364646929584)) ;
#172616 = CARTESIAN_POINT('Ctrl Pts',(-27.467319841742,-14.5049639427705,
112.388878059868)) ;
#172617 = CARTESIAN_POINT('Ctrl Pts',(-27.3935160274102,-14.504963978092,
112.413109190151)) ;
#172618 = CARTESIAN_POINT('Ctrl Pts',(-27.4018724922626,-14.4339382681578,
112.438561635708)) ;
#172619 = CARTESIAN_POINT('Ctrl Pts',(-27.3324980422359,-14.293783753758,
112.191696223905)) ;
#172620 = CARTESIAN_POINT('Ctrl Pts',(-27.3464460369964,-14.2324386627931,
112.234179567453)) ;
#172621 = CARTESIAN_POINT('Ctrl Pts',(-27.4202498542642,-14.2324386013355,
112.209948446112)) ;
#172622 = CARTESIAN_POINT('Ctrl Pts',(-27.494053671532,-14.2324385398779,
112.185717324771)) ;
#172623 = CARTESIAN_POINT('Ctrl Pts',(-27.4801056767715,-14.2937836308428,
112.143233981223)) ;
#172624 = CARTESIAN_POINT('Ctrl Pts',(-27.466157682011,-14.3551287218076,
112.100750637675)) ;
#172625 = CARTESIAN_POINT('Ctrl Pts',(-27.3923538647432,-14.3551287832652,
112.124981759016)) ;
#172626 = CARTESIAN_POINT('Ctrl Pts',(-27.3185500474754,-14.3551288447229,
112.149212880357)) ;
#172627 = CARTESIAN_POINT('Ctrl Pts',(-27.3324980422359,-14.293783753758,
112.191696223905)) ;
#172628 = CARTESIAN_POINT('Ctrl Pts',(-27.2777747513304,-14.0908689343358,
111.989522154825)) ;
#172629 = CARTESIAN_POINT('Ctrl Pts',(-27.2962983047962,-14.0436003014087,
112.045941911977)) ;
#172630 = CARTESIAN_POINT('Ctrl Pts',(-27.3701021276253,-14.0436002177779,
112.021710807575)) ;
#172631 = CARTESIAN_POINT('Ctrl Pts',(-27.4439059504545,-14.0436001341472,
111.997479703173)) ;
#172632 = CARTESIAN_POINT('Ctrl Pts',(-27.4253823969886,-14.0908687670742,
111.941059946021)) ;
#172633 = CARTESIAN_POINT('Ctrl Pts',(-27.4068588435228,-14.1381374000013,
111.88464018887)) ;
#172634 = CARTESIAN_POINT('Ctrl Pts',(-27.3330550206936,-14.1381374836321,
111.908871293272)) ;
#172635 = CARTESIAN_POINT('Ctrl Pts',(-27.2592511978645,-14.1381375672628,
111.933102397674)) ;
#172636 = CARTESIAN_POINT('Ctrl Pts',(-27.2777747513304,-14.0908689343358,
111.989522154825)) ;
#172637 = CARTESIAN_POINT('Ctrl Pts',(-27.2422913767248,-13.8416080598376,
111.846186549763)) ;
#172638 = CARTESIAN_POINT('Ctrl Pts',(-27.2640489773755,-13.8116727384737,
111.912456692852)) ;
#172639 = CARTESIAN_POINT('Ctrl Pts',(-27.3378528076801,-13.8116726391883,
111.888225611219)) ;
#172640 = CARTESIAN_POINT('Ctrl Pts',(-27.4116566379846,-13.8116725399028,
111.863994529586)) ;
#172641 = CARTESIAN_POINT('Ctrl Pts',(-27.3898990373339,-13.8416078612666,
111.797724386496)) ;
#172642 = CARTESIAN_POINT('Ctrl Pts',(-27.3681414366833,-13.8715431826305,
111.731454243407)) ;
#172643 = CARTESIAN_POINT('Ctrl Pts',(-27.2943376063787,-13.871543281916,
111.75568532504)) ;
#172644 = CARTESIAN_POINT('Ctrl Pts',(-27.2205337760742,-13.8715433812015,
111.779916406673)) ;
#172645 = CARTESIAN_POINT('Ctrl Pts',(-27.2422913767248,-13.8416080598376,
111.846186549763)) ;
#172646 = CARTESIAN_POINT('Ctrl Pts',(-27.2289317162675,-13.5600342116363,
111.76994926141)) ;
#172647 = CARTESIAN_POINT('Ctrl Pts',(-27.2523897657781,-13.5497128461305,
111.841398697373)) ;
#172648 = CARTESIAN_POINT('Ctrl Pts',(-27.3261936047793,-13.5497127385965,
111.817167642229)) ;
#172649 = CARTESIAN_POINT('Ctrl Pts',(-27.3999974437804,-13.5497126310626,
111.792936587084)) ;
#172650 = CARTESIAN_POINT('Ctrl Pts',(-27.3765393942697,-13.5600339965684,
111.721487151121)) ;
#172651 = CARTESIAN_POINT('Ctrl Pts',(-27.3530813447591,-13.5703553620741,
111.650037715158)) ;
#172652 = CARTESIAN_POINT('Ctrl Pts',(-27.279277505758,-13.5703554696081,
111.674268770302)) ;
#172653 = CARTESIAN_POINT('Ctrl Pts',(-27.2054736667568,-13.570355577142,
111.698499825447)) ;
#172654 = CARTESIAN_POINT('Ctrl Pts',(-27.2289317162675,-13.5600342116363,
111.76994926141)) ;
#172655 = CARTESIAN_POINT('Ctrl Pts',(-27.2396919341479,-13.2694053226454,
111.767331334353)) ;
#172656 = CARTESIAN_POINT('Ctrl Pts',(-27.2631657848898,-13.2793593921655,
111.838828898307)) ;
#172657 = CARTESIAN_POINT('Ctrl Pts',(-27.3369696329492,-13.2793592852709,
111.814597870752)) ;
#172658 = CARTESIAN_POINT('Ctrl Pts',(-27.4107734810085,-13.2793591783763,
111.790366843197)) ;
#172659 = CARTESIAN_POINT('Ctrl Pts',(-27.3872996302666,-13.2694051088563,
111.718869279243)) ;
#172660 = CARTESIAN_POINT('Ctrl Pts',(-27.3638257795247,-13.2594510393362,
111.647371715289)) ;
#172661 = CARTESIAN_POINT('Ctrl Pts',(-27.2900219314654,-13.2594511462308,
111.671602742844)) ;
#172662 = CARTESIAN_POINT('Ctrl Pts',(-27.216218083406,-13.2594512531254,
111.695833770399)) ;
#172663 = CARTESIAN_POINT('Ctrl Pts',(-27.2396919341479,-13.2694053226454,
111.767331334353)) ;
#172664 = CARTESIAN_POINT('Ctrl Pts',(-27.2747065150055,-12.9879324368107,
111.838387958707)) ;
#172665 = CARTESIAN_POINT('Ctrl Pts',(-27.2965072947084,-13.0175527392448,
111.904789618186)) ;
#172666 = CARTESIAN_POINT('Ctrl Pts',(-27.3703111512458,-13.0175526420622,
111.880558616454)) ;
#172667 = CARTESIAN_POINT('Ctrl Pts',(-27.4441150077832,-13.0175525448795,
111.856327614721)) ;
#172668 = CARTESIAN_POINT('Ctrl Pts',(-27.4223142280803,-12.9879322424453,
111.789925955243)) ;
#172669 = CARTESIAN_POINT('Ctrl Pts',(-27.4005134483774,-12.9583119400111,
111.723524295764)) ;
#172670 = CARTESIAN_POINT('Ctrl Pts',(-27.32670959184,-12.9583120371938,111.747755297496)) ;
#172671 = CARTESIAN_POINT('Ctrl Pts',(-27.2529057353027,-12.9583121343765,
111.771986299228)) ;
#172672 = CARTESIAN_POINT('Ctrl Pts',(-27.2747065150055,-12.9879324368107,
111.838387958707)) ;
#172673 = CARTESIAN_POINT('Ctrl Pts',(-27.3317369332919,-12.7391527795793,
111.976760771784)) ;
#172674 = CARTESIAN_POINT('Ctrl Pts',(-27.3503195226965,-12.786186317019,
112.033360342819)) ;
#172675 = CARTESIAN_POINT('Ctrl Pts',(-27.4241233863091,-12.7861862364123,
112.009129362637)) ;
#172676 = CARTESIAN_POINT('Ctrl Pts',(-27.4979272499217,-12.7861861558057,
111.984898382455)) ;
#172677 = CARTESIAN_POINT('Ctrl Pts',(-27.4793446605171,-12.739152618366,
111.92829881142)) ;
#172678 = CARTESIAN_POINT('Ctrl Pts',(-27.4607620711125,-12.6921190809264,
111.871699240384)) ;
#172679 = CARTESIAN_POINT('Ctrl Pts',(-27.3869582074999,-12.692119161533,
111.895930220567)) ;
#172680 = CARTESIAN_POINT('Ctrl Pts',(-27.3131543438873,-12.6921192421396,
111.920161200749)) ;
#172681 = CARTESIAN_POINT('Ctrl Pts',(-27.3317369332919,-12.7391527795793,
111.976760771784)) ;
#172682 = CARTESIAN_POINT('Ctrl Pts',(-27.4079460102453,-12.5377712145214,
112.173389855419)) ;
#172683 = CARTESIAN_POINT('Ctrl Pts',(-27.4219701244179,-12.5989350569668,
112.216105046329)) ;
#172684 = CARTESIAN_POINT('Ctrl Pts',(-27.495773993018,-12.5989349988532,
112.191874081337)) ;
#172685 = CARTESIAN_POINT('Ctrl Pts',(-27.569577861618,-12.5989349407397,
112.167643116346)) ;
#172686 = CARTESIAN_POINT('Ctrl Pts',(-27.5555537474453,-12.5377710982944,
112.124927925436)) ;
#172687 = CARTESIAN_POINT('Ctrl Pts',(-27.5415296332727,-12.476607255849,
112.082212734526)) ;
#172688 = CARTESIAN_POINT('Ctrl Pts',(-27.4677257646726,-12.4766073139625,
112.106443699517)) ;
#172689 = CARTESIAN_POINT('Ctrl Pts',(-27.3939218960726,-12.476607372076,
112.130674664508)) ;
#172690 = CARTESIAN_POINT('Ctrl Pts',(-27.4079460102453,-12.5377712145214,
112.173389855419)) ;
#172691 = CARTESIAN_POINT('Ctrl Pts',(-27.4985458011396,-12.3995925801182,
112.413836694041)) ;
#172692 = CARTESIAN_POINT('Ctrl Pts',(-27.5070002124818,-12.4704956782947,
112.439587468698)) ;
#172693 = CARTESIAN_POINT('Ctrl Pts',(-27.5808040834856,-12.4704956456056,
112.415356511028)) ;
#172694 = CARTESIAN_POINT('Ctrl Pts',(-27.6546079544894,-12.4704956129164,
112.391125553358)) ;
#172695 = CARTESIAN_POINT('Ctrl Pts',(-27.6461535431472,-12.39959251474,112.365374778702)) ;
#172696 = CARTESIAN_POINT('Ctrl Pts',(-27.6376991318051,-12.3286894165636,
112.339624004045)) ;
#172697 = CARTESIAN_POINT('Ctrl Pts',(-27.5638952608012,-12.3286894492527,
112.363854961715)) ;
#172698 = CARTESIAN_POINT('Ctrl Pts',(-27.4900913897974,-12.3286894819418,
112.388085919384)) ;
#172699 = CARTESIAN_POINT('Ctrl Pts',(-27.4985458011396,-12.3995925801182,
112.413836694041)) ;
#172700 = CARTESIAN_POINT('Ctrl Pts',(-27.5975500958584,-12.33457880474,112.679937373876)) ;
#172701 = CARTESIAN_POINT('Ctrl Pts',(-27.5998384646325,-12.4101277476762,
112.686907377645)) ;
#172702 = CARTESIAN_POINT('Ctrl Pts',(-27.6736423355571,-12.4101277401761,
112.662676419734)) ;
#172703 = CARTESIAN_POINT('Ctrl Pts',(-27.7474462064816,-12.410127732676,
112.638445461823)) ;
#172704 = CARTESIAN_POINT('Ctrl Pts',(-27.7451578377076,-12.3345787897397,
112.631475458053)) ;
#172705 = CARTESIAN_POINT('Ctrl Pts',(-27.7428694689335,-12.2590298468035,
112.624505454283)) ;
#172706 = CARTESIAN_POINT('Ctrl Pts',(-27.6690655980089,-12.2590298543036,
112.648736412195)) ;
#172707 = CARTESIAN_POINT('Ctrl Pts',(-27.5952617270843,-12.2590298618037,
112.672967370106)) ;
#172708 = CARTESIAN_POINT('Ctrl Pts',(-27.5975500958584,-12.33457880474,112.679937373876)) ;
#172709 = CARTESIAN_POINT('Ctrl Pts',(-27.6987081284443,-12.3470312097476,
112.952618142842)) ;
#172710 = CARTESIAN_POINT('Ctrl Pts',(-27.6946703520646,-12.4218246112721,
112.940319729069)) ;
#172711 = CARTESIAN_POINT('Ctrl Pts',(-27.7684742206581,-12.4218246263605,
112.916088764058)) ;
#172712 = CARTESIAN_POINT('Ctrl Pts',(-27.8422780892516,-12.4218246414487,
112.891857799047)) ;
#172713 = CARTESIAN_POINT('Ctrl Pts',(-27.8463158656312,-12.3470312399242,
112.904156212819)) ;
#172714 = CARTESIAN_POINT('Ctrl Pts',(-27.8503536420109,-12.2722378383997,
112.916454626591)) ;
#172715 = CARTESIAN_POINT('Ctrl Pts',(-27.7765497734175,-12.2722378233114,
112.940685591603)) ;
#172716 = CARTESIAN_POINT('Ctrl Pts',(-27.7027459048239,-12.2722378082231,
112.964916556614)) ;
#172717 = CARTESIAN_POINT('Ctrl Pts',(-27.6987081284443,-12.3470312097476,
112.952618142842)) ;
#172718 = CARTESIAN_POINT('Ctrl Pts',(-27.7957338413212,-12.4361986060041,
113.212662497894)) ;
#172719 = CARTESIAN_POINT('Ctrl Pts',(-27.7856498769021,-12.5048795255924,
113.181948370757)) ;
#172720 = CARTESIAN_POINT('Ctrl Pts',(-27.8594537412216,-12.5048795584336,
113.157717392728)) ;
#172721 = CARTESIAN_POINT('Ctrl Pts',(-27.9332576055411,-12.5048795912748,
113.133486414699)) ;
#172722 = CARTESIAN_POINT('Ctrl Pts',(-27.9433415699602,-12.4361986716865,
113.164200541836)) ;
#172723 = CARTESIAN_POINT('Ctrl Pts',(-27.9534255343793,-12.3675177520983,
113.194914668972)) ;
#172724 = CARTESIAN_POINT('Ctrl Pts',(-27.8796216700598,-12.367517719257,
113.219145647001)) ;
#172725 = CARTESIAN_POINT('Ctrl Pts',(-27.8058178057402,-12.3675176864158,
113.24337662503)) ;
#172726 = CARTESIAN_POINT('Ctrl Pts',(-27.7957338413212,-12.4361986060041,
113.212662497894)) ;
#172727 = CARTESIAN_POINT('Ctrl Pts',(-27.8823349907965,-12.5959885808789,
113.440924329999)) ;
#172728 = CARTESIAN_POINT('Ctrl Pts',(-27.8669240730479,-12.6536171134987,
113.39398516236)) ;
#172729 = CARTESIAN_POINT('Ctrl Pts',(-27.9407279319121,-12.6536171574683,
113.369754167714)) ;
#172730 = CARTESIAN_POINT('Ctrl Pts',(-28.0145317907762,-12.653617201438,
113.345523173069)) ;
#172731 = CARTESIAN_POINT('Ctrl Pts',(-28.0299427085247,-12.5959886688182,
113.392462340708)) ;
#172732 = CARTESIAN_POINT('Ctrl Pts',(-28.0453536262733,-12.5383601361984,
113.439401508348)) ;
#172733 = CARTESIAN_POINT('Ctrl Pts',(-27.9715497674092,-12.5383600922288,
113.463632502993)) ;
#172734 = CARTESIAN_POINT('Ctrl Pts',(-27.897745908545,-12.5383600482591,
113.487863497639)) ;
#172735 = CARTESIAN_POINT('Ctrl Pts',(-27.8823349907965,-12.5959885808789,
113.440924329999)) ;
#172736 = CARTESIAN_POINT('Ctrl Pts',(-27.9528390482715,-12.8143066918053,
113.620229888243)) ;
#172737 = CARTESIAN_POINT('Ctrl Pts',(-27.9332154668164,-12.8567794160869,
113.560459626507)) ;
#172738 = CARTESIAN_POINT('Ctrl Pts',(-28.0070193200838,-12.8567794648258,
113.536228614815)) ;
#172739 = CARTESIAN_POINT('Ctrl Pts',(-28.0808231733512,-12.8567795135646,
113.511997603122)) ;
#172740 = CARTESIAN_POINT('Ctrl Pts',(-28.1004467548063,-12.814306789283,
113.571767864859)) ;
#172741 = CARTESIAN_POINT('Ctrl Pts',(-28.1200703362614,-12.7718340650015,
113.631538126595)) ;
#172742 = CARTESIAN_POINT('Ctrl Pts',(-28.046266482994,-12.7718340162626,
113.655769138288)) ;
#172743 = CARTESIAN_POINT('Ctrl Pts',(-27.9724626297266,-12.7718339675238,
113.68000014998)) ;
#172744 = CARTESIAN_POINT('Ctrl Pts',(-27.9528390482715,-12.8143066918053,
113.620229888243)) ;
#172745 = CARTESIAN_POINT('Ctrl Pts',(-28.0032144890018,-13.0760276863323,
113.738192855668)) ;
#172746 = CARTESIAN_POINT('Ctrl Pts',(-27.9807778893923,-13.1002911910354,
113.669854594344)) ;
#172747 = CARTESIAN_POINT('Ctrl Pts',(-28.0545817373889,-13.1002912381593,
113.645623566597)) ;
#172748 = CARTESIAN_POINT('Ctrl Pts',(-28.1283855853854,-13.1002912852831,
113.621392538851)) ;
#172749 = CARTESIAN_POINT('Ctrl Pts',(-28.150822184995,-13.07602778058,113.689730800176)) ;
#172750 = CARTESIAN_POINT('Ctrl Pts',(-28.1732587846045,-13.0517642758768,
113.758069061501)) ;
#172751 = CARTESIAN_POINT('Ctrl Pts',(-28.0994549366079,-13.051764228753,
113.782300089247)) ;
#172752 = CARTESIAN_POINT('Ctrl Pts',(-28.0256510886113,-13.0517641816292,
113.806531116993)) ;
#172753 = CARTESIAN_POINT('Ctrl Pts',(-28.0032144890018,-13.0760276863323,
113.738192855668)) ;
#172754 = CARTESIAN_POINT('Ctrl Pts',(-28.0304977945719,-13.3628060373472,
113.785759354195)) ;
#172755 = CARTESIAN_POINT('Ctrl Pts',(-28.0068574169751,-13.3670829170375,
113.713754579168)) ;
#172756 = CARTESIAN_POINT('Ctrl Pts',(-28.0806612607687,-13.3670829569658,
113.68952353862)) ;
#172757 = CARTESIAN_POINT('Ctrl Pts',(-28.1544651045623,-13.3670829968941,
113.665292498073)) ;
#172758 = CARTESIAN_POINT('Ctrl Pts',(-28.1781054821591,-13.3628061172038,
113.7372972731)) ;
#172759 = CARTESIAN_POINT('Ctrl Pts',(-28.2017458597559,-13.3585292375136,
113.809302048127)) ;
#172760 = CARTESIAN_POINT('Ctrl Pts',(-28.1279420159623,-13.3585291975852,
113.833533088674)) ;
#172761 = CARTESIAN_POINT('Ctrl Pts',(-28.0541381721687,-13.3585291576569,
113.857764129222)) ;
#172762 = CARTESIAN_POINT('Ctrl Pts',(-28.0304977945719,-13.3628060373472,
113.785759354195)) ;
#172763 = CARTESIAN_POINT('Ctrl Pts',(-28.0334235158312,-13.6523296523906,
113.759282572633)) ;
#172764 = CARTESIAN_POINT('Ctrl Pts',(-28.0102753813997,-13.6363976370677,
113.688777090714)) ;
#172765 = CARTESIAN_POINT('Ctrl Pts',(-28.0840792224513,-13.636397668316,
113.664546041814)) ;
#172766 = CARTESIAN_POINT('Ctrl Pts',(-28.157883063503,-13.6363976995644,
113.640314992915)) ;
#172767 = CARTESIAN_POINT('Ctrl Pts',(-28.1810311979345,-13.6523297148873,
113.710820474834)) ;
#172768 = CARTESIAN_POINT('Ctrl Pts',(-28.2041793323661,-13.6682617302103,
113.781325956754)) ;
#172769 = CARTESIAN_POINT('Ctrl Pts',(-28.1303754913144,-13.6682616989619,
113.805557005653)) ;
#172770 = CARTESIAN_POINT('Ctrl Pts',(-28.0565716502628,-13.6682616677135,
113.829788054553)) ;
#172771 = CARTESIAN_POINT('Ctrl Pts',(-28.0334235158312,-13.6523296523906,
113.759282572633)) ;
#172772 = CARTESIAN_POINT('Ctrl Pts',(-28.012789007875,-13.9253061411165,
113.661037033332)) ;
#172773 = CARTESIAN_POINT('Ctrl Pts',(-27.9917790894458,-13.8902899618178,
113.597044212208)) ;
#172774 = CARTESIAN_POINT('Ctrl Pts',(-28.0655829290732,-13.8902899830873,
113.57281315897)) ;
#172775 = CARTESIAN_POINT('Ctrl Pts',(-28.1393867687006,-13.8902900043567,
113.548582105733)) ;
#172776 = CARTESIAN_POINT('Ctrl Pts',(-28.1603966871298,-13.9253061836553,
113.612574926857)) ;
#172777 = CARTESIAN_POINT('Ctrl Pts',(-28.1814066055589,-13.960322362954,
113.676567747981)) ;
#172778 = CARTESIAN_POINT('Ctrl Pts',(-28.1076027659315,-13.9603223416845,
113.700798801219)) ;
#172779 = CARTESIAN_POINT('Ctrl Pts',(-28.0337989263041,-13.9603223204151,
113.725029854456)) ;
#172780 = CARTESIAN_POINT('Ctrl Pts',(-28.012789007875,-13.9253061411165,
113.661037033332)) ;
#172781 = CARTESIAN_POINT('Ctrl Pts',(-27.9702967268525,-14.1634851116196,
113.495964568205)) ;
#172782 = CARTESIAN_POINT('Ctrl Pts',(-27.9529596170839,-14.1117847123966,
113.443158529478)) ;
#172783 = CARTESIAN_POINT('Ctrl Pts',(-28.0267634570671,-14.1117847230889,
113.418927477324)) ;
#172784 = CARTESIAN_POINT('Ctrl Pts',(-28.1005672970504,-14.1117847337813,
113.39469642517)) ;
#172785 = CARTESIAN_POINT('Ctrl Pts',(-28.1179044068189,-14.1634851330044,
113.447502463897)) ;
#172786 = CARTESIAN_POINT('Ctrl Pts',(-28.1352415165875,-14.2151855322274,
113.500308502624)) ;
#172787 = CARTESIAN_POINT('Ctrl Pts',(-28.0614376766043,-14.215185521535,
113.524539554778)) ;
#172788 = CARTESIAN_POINT('Ctrl Pts',(-27.987633836621,-14.2151855108427,
113.548770606932)) ;
#172789 = CARTESIAN_POINT('Ctrl Pts',(-27.9702967268525,-14.1634851116196,
113.495964568205)) ;
#172790 = CARTESIAN_POINT('Ctrl Pts',(-27.9105275341347,-14.3462889334782,
113.278595975283)) ;
#172791 = CARTESIAN_POINT('Ctrl Pts',(-27.8980686802056,-14.2817465742021,
113.240648316631)) ;
#172792 = CARTESIAN_POINT('Ctrl Pts',(-27.9718725209529,-14.2817465788419,
113.216417266805)) ;
#172793 = CARTESIAN_POINT('Ctrl Pts',(-28.0456763617003,-14.2817465834817,
113.192186216979)) ;
#172794 = CARTESIAN_POINT('Ctrl Pts',(-28.0581352156294,-14.3462889427578,
113.23013387563)) ;
#172795 = CARTESIAN_POINT('Ctrl Pts',(-28.0705940695586,-14.4108313020339,
113.268081534282)) ;
#172796 = CARTESIAN_POINT('Ctrl Pts',(-27.9967902288112,-14.4108312973941,
113.292312584108)) ;
#172797 = CARTESIAN_POINT('Ctrl Pts',(-27.9229863880639,-14.4108312927542,
113.316543633935)) ;
#172798 = CARTESIAN_POINT('Ctrl Pts',(-27.9105275341347,-14.3462889334782,
113.278595975283)) ;
#172799 = CARTESIAN_POINT('Ctrl Pts',(-27.8378250216826,-14.463737953108,
113.021649522263)) ;
#172800 = CARTESIAN_POINT('Ctrl Pts',(-27.8311587392697,-14.3908972873577,
113.001345101705)) ;
#172801 = CARTESIAN_POINT('Ctrl Pts',(-27.9049625815246,-14.3908972879061,
112.977114056471)) ;
#172802 = CARTESIAN_POINT('Ctrl Pts',(-27.9787664237794,-14.3908972884545,
112.952883011236)) ;
#172803 = CARTESIAN_POINT('Ctrl Pts',(-27.9854327061922,-14.4637379542048,
112.973187431793)) ;
#172804 = CARTESIAN_POINT('Ctrl Pts',(-27.9920989886051,-14.5365786199551,
112.993491852351)) ;
#172805 = CARTESIAN_POINT('Ctrl Pts',(-27.9182951463503,-14.5365786194067,
113.017722897585)) ;
#172806 = CARTESIAN_POINT('Ctrl Pts',(-27.8444913040955,-14.5365786188583,
113.04195394282)) ;
#172807 = CARTESIAN_POINT('Ctrl Pts',(-27.8378250216826,-14.463737953108,
113.021649522263)) ;
#172808 = CARTESIAN_POINT('Ctrl Pts',(-27.7583865450976,-14.5058926586063,
112.744197147275)) ;
#172809 = CARTESIAN_POINT('Ctrl Pts',(-27.7579918688641,-14.4299991748241,
112.742995027138)) ;
#172810 = CARTESIAN_POINT('Ctrl Pts',(-27.8317957124424,-14.4299991745337,
112.718763985934)) ;
#172811 = CARTESIAN_POINT('Ctrl Pts',(-27.9055995560207,-14.4299991742434,
112.69453294473)) ;
#172812 = CARTESIAN_POINT('Ctrl Pts',(-27.9059942322542,-14.5058926580256,
112.695735064867)) ;
#172813 = CARTESIAN_POINT('Ctrl Pts',(-27.9063889084876,-14.5817861418077,
112.696937185004)) ;
#172814 = CARTESIAN_POINT('Ctrl Pts',(-27.8325850649093,-14.5817861420981,
112.721168226207)) ;
#172815 = CARTESIAN_POINT('Ctrl Pts',(-27.758781221331,-14.5817861423884,
112.745399267411)) ;
#172816 = CARTESIAN_POINT('Ctrl Pts',(-27.7583865450976,-14.5058926586063,
112.744197147275)) ;
#172817 = CARTESIAN_POINT('Ctrl Pts',(-27.6788939974933,-14.4703114180475,
112.466675473693)) ;
#172818 = CARTESIAN_POINT('Ctrl Pts',(-27.6847821157798,-14.3967894542526,
112.484609731894)) ;
#172819 = CARTESIAN_POINT('Ctrl Pts',(-27.7585859600674,-14.3967894548516,
112.460378692851)) ;
#172820 = CARTESIAN_POINT('Ctrl Pts',(-27.832389804355,-14.3967894554506,
112.436147653808)) ;
#172821 = CARTESIAN_POINT('Ctrl Pts',(-27.8265016860686,-14.4703114192455,
112.418213395607)) ;
#172822 = CARTESIAN_POINT('Ctrl Pts',(-27.8206135677821,-14.5438333830403,
112.400279137406)) ;
#172823 = CARTESIAN_POINT('Ctrl Pts',(-27.7468097234945,-14.5438333824413,
112.424510176449)) ;
#172824 = CARTESIAN_POINT('Ctrl Pts',(-27.6730058792069,-14.5438333818423,
112.448741215493)) ;
#172825 = CARTESIAN_POINT('Ctrl Pts',(-27.6788939974933,-14.4703114180475,
112.466675473693)) ;
#172826 = CARTESIAN_POINT('Ctrl Pts',(-27.6052569535695,-14.359046732277,
112.206841206659)) ;
#172827 = CARTESIAN_POINT('Ctrl Pts',(-27.6170316417398,-14.2931851690986,
112.242705006923)) ;
#172828 = CARTESIAN_POINT('Ctrl Pts',(-27.6908354860316,-14.2931851708445,
112.218473967892)) ;
#172829 = CARTESIAN_POINT('Ctrl Pts',(-27.7646393303234,-14.2931851725905,
112.194242928862)) ;
#172830 = CARTESIAN_POINT('Ctrl Pts',(-27.7528646421531,-14.3590467357689,
112.158379128598)) ;
#172831 = CARTESIAN_POINT('Ctrl Pts',(-27.7410899539827,-14.4249082989473,
112.122515328334)) ;
#172832 = CARTESIAN_POINT('Ctrl Pts',(-27.667286109691,-14.4249082972013,
112.146746367365)) ;
#172833 = CARTESIAN_POINT('Ctrl Pts',(-27.5934822653991,-14.4249082954554,
112.170977406395)) ;
#172834 = CARTESIAN_POINT('Ctrl Pts',(-27.6052569535695,-14.359046732277,
112.206841206659)) ;
#172835 = CARTESIAN_POINT('Ctrl Pts',(-27.5439718545756,-14.1801475215603,
111.984669178458)) ;
#172836 = CARTESIAN_POINT('Ctrl Pts',(-27.5607781855889,-14.1266811735188,
112.035858551013)) ;
#172837 = CARTESIAN_POINT('Ctrl Pts',(-27.6345820291766,-14.1266811744766,
112.011627509838)) ;
#172838 = CARTESIAN_POINT('Ctrl Pts',(-27.7083858727642,-14.1266811754344,
111.987396468662)) ;
#172839 = CARTESIAN_POINT('Ctrl Pts',(-27.6915795417509,-14.1801475234759,
111.936207096108)) ;
#172840 = CARTESIAN_POINT('Ctrl Pts',(-27.6747732107375,-14.2336138715174,
111.885017723554)) ;
#172841 = CARTESIAN_POINT('Ctrl Pts',(-27.6009693671499,-14.2336138705596,
111.909248764729)) ;
#172842 = CARTESIAN_POINT('Ctrl Pts',(-27.5271655235622,-14.2336138696018,
111.933479805904)) ;
#172843 = CARTESIAN_POINT('Ctrl Pts',(-27.5439718545756,-14.1801475215603,
111.984669178458)) ;
#172844 = CARTESIAN_POINT('Ctrl Pts',(-27.5001849340851,-13.9475293921824,
111.815922351132)) ;
#172845 = CARTESIAN_POINT('Ctrl Pts',(-27.5208054293407,-13.9102276293421,
111.878729052622)) ;
#172846 = CARTESIAN_POINT('Ctrl Pts',(-27.5946092722882,-13.9102276274691,
111.854498009497)) ;
#172847 = CARTESIAN_POINT('Ctrl Pts',(-27.6684131152357,-13.910227625596,
111.830266966372)) ;
#172848 = CARTESIAN_POINT('Ctrl Pts',(-27.64779261998,-13.9475293884362,111.767460264882)) ;
#172849 = CARTESIAN_POINT('Ctrl Pts',(-27.6271721247244,-13.9848311512765,
111.704653563392)) ;
#172850 = CARTESIAN_POINT('Ctrl Pts',(-27.5533682817769,-13.9848311531496,
111.728884606518)) ;
#172851 = CARTESIAN_POINT('Ctrl Pts',(-27.4795644388295,-13.9848311550226,
111.753115649643)) ;
#172852 = CARTESIAN_POINT('Ctrl Pts',(-27.5001849340851,-13.9475293921824,
111.815922351132)) ;
#172853 = CARTESIAN_POINT('Ctrl Pts',(-27.4775139177375,-13.6767289638667,
111.711432637832)) ;
#172854 = CARTESIAN_POINT('Ctrl Pts',(-27.5004808337837,-13.6582814319255,
111.781386158554)) ;
#172855 = CARTESIAN_POINT('Ctrl Pts',(-27.5742846765045,-13.6582814248753,
111.757155114738)) ;
#172856 = CARTESIAN_POINT('Ctrl Pts',(-27.6480885192253,-13.658281417825,
111.732924070923)) ;
#172857 = CARTESIAN_POINT('Ctrl Pts',(-27.6251216031791,-13.6767289497662,
111.662970550201)) ;
#172858 = CARTESIAN_POINT('Ctrl Pts',(-27.6021546871329,-13.6951764817073,
111.59301702948)) ;
#172859 = CARTESIAN_POINT('Ctrl Pts',(-27.5283508444121,-13.6951764887576,
111.617248073295)) ;
#172860 = CARTESIAN_POINT('Ctrl Pts',(-27.4545470016913,-13.6951764958078,
111.641479117111)) ;
#172861 = CARTESIAN_POINT('Ctrl Pts',(-27.4775139177375,-13.6767289638667,
111.711432637832)) ;
#172862 = CARTESIAN_POINT('Ctrl Pts',(-27.4783712957127,-13.3875048973073,
111.67862173555)) ;
#172863 = CARTESIAN_POINT('Ctrl Pts',(-27.5020447372821,-13.3892252145517,
111.750727219135)) ;
#172864 = CARTESIAN_POINT('Ctrl Pts',(-27.5758485805916,-13.3892252011116,
111.726496177112)) ;
#172865 = CARTESIAN_POINT('Ctrl Pts',(-27.6496524239011,-13.3892251876716,
111.70226513509)) ;
#172866 = CARTESIAN_POINT('Ctrl Pts',(-27.6259789823316,-13.3875048704272,
111.630159651505)) ;
#172867 = CARTESIAN_POINT('Ctrl Pts',(-27.6023055407622,-13.3857845531828,
111.558054167921)) ;
#172868 = CARTESIAN_POINT('Ctrl Pts',(-27.5285016974527,-13.3857845666228,
111.582285209944)) ;
#172869 = CARTESIAN_POINT('Ctrl Pts',(-27.4546978541432,-13.3857845800629,
111.606516251966)) ;
#172870 = CARTESIAN_POINT('Ctrl Pts',(-27.4783712957127,-13.3875048973073,
111.67862173555)) ;
#172871 = CARTESIAN_POINT('Ctrl Pts',(-27.5037549225319,-13.0987597443669,
111.720294424521)) ;
#172872 = CARTESIAN_POINT('Ctrl Pts',(-27.5264280564151,-13.1206437742592,
111.789353132464)) ;
#172873 = CARTESIAN_POINT('Ctrl Pts',(-27.6002319016533,-13.1206437527101,
111.765122096317)) ;
#172874 = CARTESIAN_POINT('Ctrl Pts',(-27.6740357468916,-13.120643731161,
111.740891060169)) ;
#172875 = CARTESIAN_POINT('Ctrl Pts',(-27.6513626130085,-13.0987597012687,
111.671832352226)) ;
#172876 = CARTESIAN_POINT('Ctrl Pts',(-27.6286894791254,-13.0768756713763,
111.602773644283)) ;
#172877 = CARTESIAN_POINT('Ctrl Pts',(-27.5548856338871,-13.0768756929254,
111.627004680431)) ;
#172878 = CARTESIAN_POINT('Ctrl Pts',(-27.4810817886488,-13.0768757144745,
111.651235716578)) ;
#172879 = CARTESIAN_POINT('Ctrl Pts',(-27.5037549225319,-13.0987597443669,
111.720294424521)) ;
#172880 = CARTESIAN_POINT('Ctrl Pts',(-27.5521194249204,-12.8352678817982,
111.832269007795)) ;
#172881 = CARTESIAN_POINT('Ctrl Pts',(-27.5721795947561,-12.8755807524781,
111.893369048984)) ;
#172882 = CARTESIAN_POINT('Ctrl Pts',(-27.6459834428958,-12.8755807274115,
111.869138021673)) ;
#172883 = CARTESIAN_POINT('Ctrl Pts',(-27.7197872910354,-12.8755807023449,
111.844906994363)) ;
#172884 = CARTESIAN_POINT('Ctrl Pts',(-27.6997271211997,-12.8352678316651,
111.783806953174)) ;
#172885 = CARTESIAN_POINT('Ctrl Pts',(-27.6796669513639,-12.7949549609852,
111.722706911984)) ;
#172886 = CARTESIAN_POINT('Ctrl Pts',(-27.6058631032243,-12.7949549860518,
111.746937939295)) ;
#172887 = CARTESIAN_POINT('Ctrl Pts',(-27.5320592550846,-12.7949550111184,
111.771168966605)) ;
#172888 = CARTESIAN_POINT('Ctrl Pts',(-27.5521194249204,-12.8352678817982,
111.832269007795)) ;
#172889 = CARTESIAN_POINT('Ctrl Pts',(-27.6210545802362,-12.6124277096966,
112.006776869347)) ;
#172890 = CARTESIAN_POINT('Ctrl Pts',(-27.6370643810052,-12.6683576543549,
112.055540140046)) ;
#172891 = CARTESIAN_POINT('Ctrl Pts',(-27.710868232941,-12.6683576284383,
112.031309124298)) ;
#172892 = CARTESIAN_POINT('Ctrl Pts',(-27.784672084877,-12.6683576025217,
112.00707810855)) ;
#172893 = CARTESIAN_POINT('Ctrl Pts',(-27.768662284108,-12.6124276578634,
111.958314837852)) ;
#172894 = CARTESIAN_POINT('Ctrl Pts',(-27.7526524833391,-12.5564977132051,
111.909551567153)) ;
#172895 = CARTESIAN_POINT('Ctrl Pts',(-27.6788486314032,-12.5564977391217,
111.933782582901)) ;
#172896 = CARTESIAN_POINT('Ctrl Pts',(-27.6050447794673,-12.5564977650383,
111.958013598649)) ;
#172897 = CARTESIAN_POINT('Ctrl Pts',(-27.6210545802362,-12.6124277096966,
112.006776869347)) ;
#172898 = CARTESIAN_POINT('Ctrl Pts',(-27.7066454648907,-12.4469021309738,
112.231908874782)) ;
#172899 = CARTESIAN_POINT('Ctrl Pts',(-27.7174384370252,-12.5144700927407,
112.264782527379)) ;
#172900 = CARTESIAN_POINT('Ctrl Pts',(-27.7912422935081,-12.5144700706049,
112.240551525481)) ;
#172901 = CARTESIAN_POINT('Ctrl Pts',(-27.865046149991,-12.514470048469,112.216320523583)) ;
#172902 = CARTESIAN_POINT('Ctrl Pts',(-27.8542531778566,-12.4469020867021,
112.183446870986)) ;
#172903 = CARTESIAN_POINT('Ctrl Pts',(-27.8434602057222,-12.3793341249352,
112.150573218388)) ;
#172904 = CARTESIAN_POINT('Ctrl Pts',(-27.7696563492392,-12.3793341470711,
112.174804220286)) ;
#172905 = CARTESIAN_POINT('Ctrl Pts',(-27.6958524927563,-12.3793341692069,
112.199035222185)) ;
#172906 = CARTESIAN_POINT('Ctrl Pts',(-27.7066454648907,-12.4469021309738,
112.231908874782)) ;
#172907 = CARTESIAN_POINT('Ctrl Pts',(-27.803058956122,-12.3516623128813,
112.490078822438)) ;
#172908 = CARTESIAN_POINT('Ctrl Pts',(-27.8078704096533,-12.425977537866,
112.504733734657)) ;
#172909 = CARTESIAN_POINT('Ctrl Pts',(-27.8816742702308,-12.4259775261186,
112.48050274523)) ;
#172910 = CARTESIAN_POINT('Ctrl Pts',(-27.9554781308084,-12.4259775143711,
112.456271755804)) ;
#172911 = CARTESIAN_POINT('Ctrl Pts',(-27.9506666772771,-12.3516622893864,
112.441616843585)) ;
#172912 = CARTESIAN_POINT('Ctrl Pts',(-27.9458552237458,-12.2773470644017,
112.426961931365)) ;
#172913 = CARTESIAN_POINT('Ctrl Pts',(-27.8720513631682,-12.2773470761492,
112.451192920792)) ;
#172914 = CARTESIAN_POINT('Ctrl Pts',(-27.7982475025907,-12.2773470878966,
112.475423910219)) ;
#172915 = CARTESIAN_POINT('Ctrl Pts',(-27.803058956122,-12.3516623128813,
112.490078822438)) ;
#172916 = CARTESIAN_POINT('Ctrl Pts',(-27.903680048157,-12.3325403630455,
112.761274392716)) ;
#172917 = CARTESIAN_POINT('Ctrl Pts',(-27.9022032625788,-12.4082975181779,
112.756776343341)) ;
#172918 = CARTESIAN_POINT('Ctrl Pts',(-27.9760071256183,-12.4082975217576,
112.732545361413)) ;
#172919 = CARTESIAN_POINT('Ctrl Pts',(-28.0498109886578,-12.4082975253373,
112.708314379486)) ;
#172920 = CARTESIAN_POINT('Ctrl Pts',(-28.051287774236,-12.3325403702048,
112.71281242886)) ;
#172921 = CARTESIAN_POINT('Ctrl Pts',(-28.0527645598142,-12.2567832150723,
112.717310478235)) ;
#172922 = CARTESIAN_POINT('Ctrl Pts',(-27.9789606967747,-12.2567832114927,
112.741541460163)) ;
#172923 = CARTESIAN_POINT('Ctrl Pts',(-27.9051568337352,-12.256783207913,
112.765772442091)) ;
#172924 = CARTESIAN_POINT('Ctrl Pts',(-27.903680048157,-12.3325403630455,
112.761274392716)) ;
#172925 = CARTESIAN_POINT('Ctrl Pts',(-28.0035102323783,-12.3912337324793,
113.029751907953)) ;
#172926 = CARTESIAN_POINT('Ctrl Pts',(-27.9957978082671,-12.4630030921761,
113.006261109903)) ;
#172927 = CARTESIAN_POINT('Ctrl Pts',(-28.069601673032,-12.4630031154162,
112.982030133231)) ;
#172928 = CARTESIAN_POINT('Ctrl Pts',(-28.1434055377969,-12.4630031386562,
112.957799156558)) ;
#172929 = CARTESIAN_POINT('Ctrl Pts',(-28.1511179619081,-12.3912337789595,
112.981289954608)) ;
#172930 = CARTESIAN_POINT('Ctrl Pts',(-28.1588303860193,-12.3194644192627,
113.004780752658)) ;
#172931 = CARTESIAN_POINT('Ctrl Pts',(-28.0850265212543,-12.3194643960226,
113.029011729331)) ;
#172932 = CARTESIAN_POINT('Ctrl Pts',(-28.0112226564894,-12.3194643727826,
113.053242706003)) ;
#172933 = CARTESIAN_POINT('Ctrl Pts',(-28.0035102323783,-12.3912337324793,
113.029751907953)) ;
#172934 = CARTESIAN_POINT('Ctrl Pts',(-28.0947250172942,-12.5231371749147,
113.272201796469)) ;
#172935 = CARTESIAN_POINT('Ctrl Pts',(-28.0813650498466,-12.5858011581757,
113.231509492776)) ;
#172936 = CARTESIAN_POINT('Ctrl Pts',(-28.155168913654,-12.5858012027222,
113.207278513187)) ;
#172937 = CARTESIAN_POINT('Ctrl Pts',(-28.2289727774614,-12.5858012472688,
113.183047533598)) ;
#172938 = CARTESIAN_POINT('Ctrl Pts',(-28.242332744909,-12.5231372640078,
113.223739837291)) ;
#172939 = CARTESIAN_POINT('Ctrl Pts',(-28.2556927123566,-12.4604732807469,
113.264432140985)) ;
#172940 = CARTESIAN_POINT('Ctrl Pts',(-28.1818888485492,-12.4604732362004,
113.288663120574)) ;
#172941 = CARTESIAN_POINT('Ctrl Pts',(-28.1080849847418,-12.4604731916538,
113.312894100163)) ;
#172942 = CARTESIAN_POINT('Ctrl Pts',(-28.0947250172942,-12.5231371749147,
113.272201796469)) ;
#172943 = CARTESIAN_POINT('Ctrl Pts',(-28.1723924962388,-12.7192715563506,
113.473290319783)) ;
#172944 = CARTESIAN_POINT('Ctrl Pts',(-28.1543246541495,-12.7683330936011,
113.41825858968)) ;
#172945 = CARTESIAN_POINT('Ctrl Pts',(-28.2281285149571,-12.7683331592754,
113.394027600954)) ;
#172946 = CARTESIAN_POINT('Ctrl Pts',(-28.3019323757647,-12.7683332249497,
113.369796612228)) ;
#172947 = CARTESIAN_POINT('Ctrl Pts',(-28.320000217854,-12.7192716876992,
113.424828342331)) ;
#172948 = CARTESIAN_POINT('Ctrl Pts',(-28.3380680599432,-12.6702101504487,
113.479860072434)) ;
#172949 = CARTESIAN_POINT('Ctrl Pts',(-28.2642641991356,-12.6702100847745,
113.50409106116)) ;
#172950 = CARTESIAN_POINT('Ctrl Pts',(-28.190460338328,-12.6702100191002,
113.528322049886)) ;
#172951 = CARTESIAN_POINT('Ctrl Pts',(-28.1723924962388,-12.7192715563506,
113.473290319783)) ;
#172952 = CARTESIAN_POINT('Ctrl Pts',(-28.2314642131708,-12.9657766439547,
113.617711015076)) ;
#172953 = CARTESIAN_POINT('Ctrl Pts',(-28.2099804696281,-12.9976995891968,
113.552275000424)) ;
#172954 = CARTESIAN_POINT('Ctrl Pts',(-28.2837843251922,-12.9976996732378,
113.528043995727)) ;
#172955 = CARTESIAN_POINT('Ctrl Pts',(-28.3575881807563,-12.9976997572788,
113.503812991031)) ;
#172956 = CARTESIAN_POINT('Ctrl Pts',(-28.379071924299,-12.9657768120367,
113.569249005683)) ;
#172957 = CARTESIAN_POINT('Ctrl Pts',(-28.4005556678416,-12.9338538667946,
113.634685020334)) ;
#172958 = CARTESIAN_POINT('Ctrl Pts',(-28.3267518122775,-12.9338537827536,
113.658916025031)) ;
#172959 = CARTESIAN_POINT('Ctrl Pts',(-28.2529479567134,-12.9338536987126,
113.683147029728)) ;
#172960 = CARTESIAN_POINT('Ctrl Pts',(-28.2314642131708,-12.9657766439547,
113.617711015076)) ;
#172961 = CARTESIAN_POINT('Ctrl Pts',(-28.2683502437793,-13.2450968718509,
113.694515096532)) ;
#172962 = CARTESIAN_POINT('Ctrl Pts',(-28.2449953018678,-13.2575654456473,
113.623379713674)) ;
#172963 = CARTESIAN_POINT('Ctrl Pts',(-28.3187991502527,-13.2575655425572,
113.599148687111)) ;
#172964 = CARTESIAN_POINT('Ctrl Pts',(-28.3926029986376,-13.2575656394672,
113.574917660547)) ;
#172965 = CARTESIAN_POINT('Ctrl Pts',(-28.4159579405491,-13.2450970656709,
113.646053043406)) ;
#172966 = CARTESIAN_POINT('Ctrl Pts',(-28.4393128824606,-13.2326284918745,
113.717188426264)) ;
#172967 = CARTESIAN_POINT('Ctrl Pts',(-28.3655090340758,-13.2326283949646,
113.741419452827)) ;
#172968 = CARTESIAN_POINT('Ctrl Pts',(-28.2917051856909,-13.2326282980546,
113.765650479391)) ;
#172969 = CARTESIAN_POINT('Ctrl Pts',(-28.2683502437793,-13.2450968718509,
113.694515096532)) ;
#172970 = CARTESIAN_POINT('Ctrl Pts',(-28.2811758969267,-13.5349426349563,
113.698268361909)) ;
#172971 = CARTESIAN_POINT('Ctrl Pts',(-28.2576221389113,-13.527193346992,
113.626527417346)) ;
#172972 = CARTESIAN_POINT('Ctrl Pts',(-28.331425978995,-13.5271934482019,
113.602296365499)) ;
#172973 = CARTESIAN_POINT('Ctrl Pts',(-28.4052298190787,-13.5271935494119,
113.578065313651)) ;
#172974 = CARTESIAN_POINT('Ctrl Pts',(-28.428783577094,-13.5349428373762,
113.649806258214)) ;
#172975 = CARTESIAN_POINT('Ctrl Pts',(-28.4523373351094,-13.5426921253405,
113.721547202778)) ;
#172976 = CARTESIAN_POINT('Ctrl Pts',(-28.3785334950258,-13.5426920241306,
113.745778254625)) ;
#172977 = CARTESIAN_POINT('Ctrl Pts',(-28.3047296549421,-13.5426919229206,
113.770009306473)) ;
#172978 = CARTESIAN_POINT('Ctrl Pts',(-28.2811758969267,-13.5349426349563,
113.698268361909)) ;
#172979 = CARTESIAN_POINT('Ctrl Pts',(-28.2698660181599,-13.8188180807124,
113.628205800714)) ;
#172980 = CARTESIAN_POINT('Ctrl Pts',(-28.2478040607929,-13.791238496166,
113.561008640298)) ;
#172981 = CARTESIAN_POINT('Ctrl Pts',(-28.3216078921359,-13.7912385944122,
113.536777561828)) ;
#172982 = CARTESIAN_POINT('Ctrl Pts',(-28.395411723479,-13.7912386926585,
113.512546483358)) ;
#172983 = CARTESIAN_POINT('Ctrl Pts',(-28.417473680846,-13.8188182772049,
113.579743643773)) ;
#172984 = CARTESIAN_POINT('Ctrl Pts',(-28.439535638213,-13.8463978617513,
113.646940804189)) ;
#172985 = CARTESIAN_POINT('Ctrl Pts',(-28.36573180687,-13.846397763505,113.671171882659)) ;
#172986 = CARTESIAN_POINT('Ctrl Pts',(-28.2919279755269,-13.8463976652588,
113.695402961129)) ;
#172987 = CARTESIAN_POINT('Ctrl Pts',(-28.2698660181599,-13.8188180807124,
113.628205800714)) ;
#172988 = CARTESIAN_POINT('Ctrl Pts',(-28.2358683922085,-14.0726519250138,
113.48919153583)) ;
#172989 = CARTESIAN_POINT('Ctrl Pts',(-28.2168813064894,-14.027309972795,
113.431359938362)) ;
#172990 = CARTESIAN_POINT('Ctrl Pts',(-28.2906851297376,-14.027310058674,
113.407128835236)) ;
#172991 = CARTESIAN_POINT('Ctrl Pts',(-28.3644889529858,-14.027310144553,
113.382897732111)) ;
#172992 = CARTESIAN_POINT('Ctrl Pts',(-28.383476038705,-14.0726520967719,
113.440729329579)) ;
#172993 = CARTESIAN_POINT('Ctrl Pts',(-28.402463124424,-14.1179940489907,
113.498560927047)) ;
#172994 = CARTESIAN_POINT('Ctrl Pts',(-28.3286593011758,-14.1179939631117,
113.522792030172)) ;
#172995 = CARTESIAN_POINT('Ctrl Pts',(-28.2548554779276,-14.1179938772327,
113.547023133298)) ;
#172996 = CARTESIAN_POINT('Ctrl Pts',(-28.2358683922085,-14.0726519250138,
113.48919153583)) ;
#172997 = CARTESIAN_POINT('Ctrl Pts',(-28.1827369648301,-14.2790221021537,
113.292024183099)) ;
#172998 = CARTESIAN_POINT('Ctrl Pts',(-28.1681625859469,-14.2192053591173,
113.247632978682)) ;
#172999 = CARTESIAN_POINT('Ctrl Pts',(-28.2419664026165,-14.2192054253214,
113.223401855519)) ;
#173000 = CARTESIAN_POINT('Ctrl Pts',(-28.3157702192861,-14.2192054915256,
113.199170732356)) ;
#173001 = CARTESIAN_POINT('Ctrl Pts',(-28.3303445981694,-14.279022234562,
113.243561936774)) ;
#173002 = CARTESIAN_POINT('Ctrl Pts',(-28.3449189770527,-14.3388389775984,
113.287953141191)) ;
#173003 = CARTESIAN_POINT('Ctrl Pts',(-28.2711151603831,-14.3388389113943,
113.312184264354)) ;
#173004 = CARTESIAN_POINT('Ctrl Pts',(-28.1973113437134,-14.3388388451902,
113.336415387517)) ;
#173005 = CARTESIAN_POINT('Ctrl Pts',(-28.1827369648301,-14.2790221021537,
113.292024183099)) ;
#173006 = CARTESIAN_POINT('Ctrl Pts',(-28.1145891487937,-14.4246999098251,
113.048988420366)) ;
#173007 = CARTESIAN_POINT('Ctrl Pts',(-28.1054848872704,-14.3546239086375,
113.021258310826)) ;
#173008 = CARTESIAN_POINT('Ctrl Pts',(-28.1792886994093,-14.3546239496232,
112.997027173864)) ;
#173009 = CARTESIAN_POINT('Ctrl Pts',(-28.2530925115482,-14.3546239906089,
112.972796036901)) ;
#173010 = CARTESIAN_POINT('Ctrl Pts',(-28.2621967730714,-14.4246999917965,
113.000526146441)) ;
#173011 = CARTESIAN_POINT('Ctrl Pts',(-28.2713010345947,-14.4947759929842,
113.02825625598)) ;
#173012 = CARTESIAN_POINT('Ctrl Pts',(-28.1974972224558,-14.4947759519985,
113.052487392943)) ;
#173013 = CARTESIAN_POINT('Ctrl Pts',(-28.1236934103169,-14.4947759110128,
113.076718529906)) ;
#173014 = CARTESIAN_POINT('Ctrl Pts',(-28.1145891487937,-14.4246999098251,
113.048988420366)) ;
#173015 = CARTESIAN_POINT('Ctrl Pts',(-28.0369433110204,-14.4982101688668,
112.776913098185)) ;
#173016 = CARTESIAN_POINT('Ctrl Pts',(-28.033982577611,-14.4228974545996,
112.767895183996)) ;
#173017 = CARTESIAN_POINT('Ctrl Pts',(-28.107786387942,-14.4228974671485,
112.743664041527)) ;
#173018 = CARTESIAN_POINT('Ctrl Pts',(-28.181590198273,-14.4228974796974,
112.719432899057)) ;
#173019 = CARTESIAN_POINT('Ctrl Pts',(-28.1845509316824,-14.4982101939646,
112.728450813246)) ;
#173020 = CARTESIAN_POINT('Ctrl Pts',(-28.1875116650917,-14.5735229082318,
112.737468727435)) ;
#173021 = CARTESIAN_POINT('Ctrl Pts',(-28.1137078547607,-14.5735228956829,
112.761699869904)) ;
#173022 = CARTESIAN_POINT('Ctrl Pts',(-28.0399040444297,-14.573522883134,
112.785931012374)) ;
#173023 = CARTESIAN_POINT('Ctrl Pts',(-28.0369433110204,-14.4982101688668,
112.776913098185)) ;
#173024 = CARTESIAN_POINT('Ctrl Pts',(-27.9566667707584,-14.4940193671701,
112.496956548577)) ;
#173025 = CARTESIAN_POINT('Ctrl Pts',(-27.9600397432089,-14.4188869609571,
112.50723008045)) ;
#173026 = CARTESIAN_POINT('Ctrl Pts',(-28.0338435544589,-14.4188869452096,
112.48299894078)) ;
#173027 = CARTESIAN_POINT('Ctrl Pts',(-28.107647365709,-14.4188869294622,
112.45876780111)) ;
#173028 = CARTESIAN_POINT('Ctrl Pts',(-28.1042743932586,-14.4940193356751,
112.448494269237)) ;
#173029 = CARTESIAN_POINT('Ctrl Pts',(-28.1009014208082,-14.5691517418881,
112.438220737365)) ;
#173030 = CARTESIAN_POINT('Ctrl Pts',(-28.0270976095581,-14.5691517576355,
112.462451877035)) ;
#173031 = CARTESIAN_POINT('Ctrl Pts',(-27.953293798308,-14.569151773383,112.486683016705)) ;
#173032 = CARTESIAN_POINT('Ctrl Pts',(-27.9566667707584,-14.4940193671701,
112.496956548577)) ;
#173033 = CARTESIAN_POINT('Ctrl Pts',(-27.8798943064057,-14.4126640845972,
112.227622938821)) ;
#173034 = CARTESIAN_POINT('Ctrl Pts',(-27.8893668566243,-14.3430991702555,
112.256474800339)) ;
#173035 = CARTESIAN_POINT('Ctrl Pts',(-27.9631706714083,-14.3430991291711,
112.232243671433)) ;
#173036 = CARTESIAN_POINT('Ctrl Pts',(-28.0369744861922,-14.3430990880866,
112.208012542526)) ;
#173037 = CARTESIAN_POINT('Ctrl Pts',(-28.0275019359736,-14.4126640024283,
112.179160681008)) ;
#173038 = CARTESIAN_POINT('Ctrl Pts',(-28.018029385755,-14.48222891677,112.150308819489)) ;
#173039 = CARTESIAN_POINT('Ctrl Pts',(-27.9442255709711,-14.4822289578544,
112.174539948395)) ;
#173040 = CARTESIAN_POINT('Ctrl Pts',(-27.8704217561871,-14.4822289989389,
112.198771077302)) ;
#173041 = CARTESIAN_POINT('Ctrl Pts',(-27.8798943064057,-14.4126640845972,
112.227622938821)) ;
#173042 = CARTESIAN_POINT('Ctrl Pts',(-27.8131986851945,-14.2606219622614,
111.989110261264)) ;
#173043 = CARTESIAN_POINT('Ctrl Pts',(-27.828073796266,-14.2015682240357,
112.034417451361)) ;
#173044 = CARTESIAN_POINT('Ctrl Pts',(-27.9018776164657,-14.2015681626728,
112.01018633895)) ;
#173045 = CARTESIAN_POINT('Ctrl Pts',(-27.9756814366654,-14.2015681013099,
111.985955226539)) ;
#173046 = CARTESIAN_POINT('Ctrl Pts',(-27.9608063255939,-14.2606218395355,
111.940648036442)) ;
#173047 = CARTESIAN_POINT('Ctrl Pts',(-27.9459312145223,-14.3196755777612,
111.895340846344)) ;
#173048 = CARTESIAN_POINT('Ctrl Pts',(-27.8721273943226,-14.3196756391241,
111.919571958755)) ;
#173049 = CARTESIAN_POINT('Ctrl Pts',(-27.798323574123,-14.319675700487,111.943803071166)) ;
#173050 = CARTESIAN_POINT('Ctrl Pts',(-27.8131986851945,-14.2606219622614,
111.989110261264)) ;
#173051 = CARTESIAN_POINT('Ctrl Pts',(-27.7615962317299,-14.047641669402,
111.796421873509)) ;
#173052 = CARTESIAN_POINT('Ctrl Pts',(-27.7808313920181,-14.003368790847,
111.855009069918)) ;
#173053 = CARTESIAN_POINT('Ctrl Pts',(-27.8546352192211,-14.0033687165429,
111.830777978838)) ;
#173054 = CARTESIAN_POINT('Ctrl Pts',(-27.928439046424,-14.0033686422388,
111.806546887757)) ;
#173055 = CARTESIAN_POINT('Ctrl Pts',(-27.9092038861358,-14.0476415207938,
111.747959691349)) ;
#173056 = CARTESIAN_POINT('Ctrl Pts',(-27.8899687258476,-14.0919143993488,
111.689372494941)) ;
#173057 = CARTESIAN_POINT('Ctrl Pts',(-27.8161648986446,-14.0919144736529,
111.713603586021)) ;
#173058 = CARTESIAN_POINT('Ctrl Pts',(-27.7423610714416,-14.0919145479569,
111.737834677101)) ;
#173059 = CARTESIAN_POINT('Ctrl Pts',(-27.7615962317299,-14.047641669402,
111.796421873509)) ;
#173060 = CARTESIAN_POINT('Ctrl Pts',(-27.7298973111856,-13.7890886844739,
111.664327213788)) ;
#173061 = CARTESIAN_POINT('Ctrl Pts',(-27.7521102111039,-13.7628006589206,
111.731984124516)) ;
#173062 = CARTESIAN_POINT('Ctrl Pts',(-27.8259140458139,-13.7628005801191,
111.707753056301)) ;
#173063 = CARTESIAN_POINT('Ctrl Pts',(-27.8997178805239,-13.7628005013175,
111.683521988087)) ;
#173064 = CARTESIAN_POINT('Ctrl Pts',(-27.8775049806057,-13.7890885268708,
111.615865077358)) ;
#173065 = CARTESIAN_POINT('Ctrl Pts',(-27.8552920806875,-13.8153765524241,
111.54820816663)) ;
#173066 = CARTESIAN_POINT('Ctrl Pts',(-27.7814882459774,-13.8153766312257,
111.572439234845)) ;
#173067 = CARTESIAN_POINT('Ctrl Pts',(-27.7076844112674,-13.8153767100272,
111.59667030306)) ;
#173068 = CARTESIAN_POINT('Ctrl Pts',(-27.7298973111856,-13.7890886844739,
111.664327213788)) ;
#173069 = CARTESIAN_POINT('Ctrl Pts',(-27.7211529443622,-13.5048564724281,
111.602268903286)) ;
#173070 = CARTESIAN_POINT('Ctrl Pts',(-27.7447429129393,-13.4983736613525,
111.674120142827)) ;
#173071 = CARTESIAN_POINT('Ctrl Pts',(-27.818546754637,-13.4983735848724,
111.649889095895)) ;
#173072 = CARTESIAN_POINT('Ctrl Pts',(-27.8923505963348,-13.4983735083923,
111.625658048964)) ;
#173073 = CARTESIAN_POINT('Ctrl Pts',(-27.8687606277577,-13.5048563194679,
111.553806809424)) ;
#173074 = CARTESIAN_POINT('Ctrl Pts',(-27.8451706591806,-13.5113391305435,
111.481955569883)) ;
#173075 = CARTESIAN_POINT('Ctrl Pts',(-27.7713668174828,-13.5113392070236,
111.506186616814)) ;
#173076 = CARTESIAN_POINT('Ctrl Pts',(-27.697562975785,-13.5113392835037,
111.530417663746)) ;
#173077 = CARTESIAN_POINT('Ctrl Pts',(-27.7211529443622,-13.5048564724281,
111.602268903286)) ;
#173078 = CARTESIAN_POINT('Ctrl Pts',(-27.7365275470258,-13.2147190164361,
111.613706256659)) ;
#173079 = CARTESIAN_POINT('Ctrl Pts',(-27.7598120222788,-13.2284837281292,
111.684627012687)) ;
#173080 = CARTESIAN_POINT('Ctrl Pts',(-27.8336158699542,-13.2284836599234,
111.660395983963)) ;
#173081 = CARTESIAN_POINT('Ctrl Pts',(-27.9074197176295,-13.2284835917175,
111.636164955238)) ;
#173082 = CARTESIAN_POINT('Ctrl Pts',(-27.8841352423765,-13.2147188800244,
111.56524419921)) ;
#173083 = CARTESIAN_POINT('Ctrl Pts',(-27.8608507671235,-13.2009541683313,
111.494323443181)) ;
#173084 = CARTESIAN_POINT('Ctrl Pts',(-27.7870469194481,-13.2009542365372,
111.518554471906)) ;
#173085 = CARTESIAN_POINT('Ctrl Pts',(-27.7132430717728,-13.200954304743,
111.54278550063)) ;
#173086 = CARTESIAN_POINT('Ctrl Pts',(-27.7365275470258,-13.2147190164361,
111.613706256659)) ;
#173087 = CARTESIAN_POINT('Ctrl Pts',(-27.7758074412185,-12.9381997507725,
111.697848661622)) ;
#173088 = CARTESIAN_POINT('Ctrl Pts',(-27.7971192532817,-12.9712919342548,
111.762761003699)) ;
#173089 = CARTESIAN_POINT('Ctrl Pts',(-27.8709231053441,-12.9712918799021,
111.738529988336)) ;
#173090 = CARTESIAN_POINT('Ctrl Pts',(-27.9447269574064,-12.9712918255494,
111.714298972973)) ;
#173091 = CARTESIAN_POINT('Ctrl Pts',(-27.9234151453431,-12.9381996420671,
111.649386630897)) ;
#173092 = CARTESIAN_POINT('Ctrl Pts',(-27.9021033332798,-12.9051074585849,
111.584474288821)) ;
#173093 = CARTESIAN_POINT('Ctrl Pts',(-27.8282994812175,-12.9051075129375,
111.608705304183)) ;
#173094 = CARTESIAN_POINT('Ctrl Pts',(-27.7544956291552,-12.9051075672902,
111.632936319546)) ;
#173095 = CARTESIAN_POINT('Ctrl Pts',(-27.7758074412185,-12.9381997507725,
111.697848661622)) ;
#173096 = CARTESIAN_POINT('Ctrl Pts',(-27.8372160580513,-12.695688487741,
111.849295864408)) ;
#173097 = CARTESIAN_POINT('Ctrl Pts',(-27.8550092108468,-12.745763523541,
111.903490937894)) ;
#173098 = CARTESIAN_POINT('Ctrl Pts',(-27.9288130649844,-12.7457634857973,
111.879259928853)) ;
#173099 = CARTESIAN_POINT('Ctrl Pts',(-28.002616919122,-12.7457634480537,
111.855028919811)) ;
#173100 = CARTESIAN_POINT('Ctrl Pts',(-27.9848237663266,-12.6956884122536,
111.800833846325)) ;
#173101 = CARTESIAN_POINT('Ctrl Pts',(-27.9670306135311,-12.6456133764535,
111.746638772839)) ;
#173102 = CARTESIAN_POINT('Ctrl Pts',(-27.8932267593934,-12.6456134141972,
111.77086978188)) ;
#173103 = CARTESIAN_POINT('Ctrl Pts',(-27.8194229052558,-12.6456134519409,
111.795100790922)) ;
#173104 = CARTESIAN_POINT('Ctrl Pts',(-27.8372160580513,-12.695688487741,
111.849295864408)) ;
#173105 = CARTESIAN_POINT('Ctrl Pts',(-27.9160580941386,-12.5067830863174,
112.054188473819)) ;
#173106 = CARTESIAN_POINT('Ctrl Pts',(-27.9291025894933,-12.5701233290617,
112.093919902817)) ;
#173107 = CARTESIAN_POINT('Ctrl Pts',(-28.0029064447615,-12.5701233053132,
112.069688897219)) ;
#173108 = CARTESIAN_POINT('Ctrl Pts',(-28.0767103000296,-12.5701232815646,
112.04545789162)) ;
#173109 = CARTESIAN_POINT('Ctrl Pts',(-28.0636658046749,-12.5067830388203,
112.005726462623)) ;
#173110 = CARTESIAN_POINT('Ctrl Pts',(-28.0506213093203,-12.443442796076,
111.965995033625)) ;
#173111 = CARTESIAN_POINT('Ctrl Pts',(-27.9768174540521,-12.4434428198246,
111.990226039223)) ;
#173112 = CARTESIAN_POINT('Ctrl Pts',(-27.903013598784,-12.4434428435731,
112.014457044821)) ;
#173113 = CARTESIAN_POINT('Ctrl Pts',(-27.9160580941386,-12.5067830863174,
112.054188473819)) ;
#173114 = CARTESIAN_POINT('Ctrl Pts',(-28.008667920428,-12.3815987000844,
112.300764968466)) ;
#173115 = CARTESIAN_POINT('Ctrl Pts',(-28.0160005465217,-12.4537757553205,
112.323098965097)) ;
#173116 = CARTESIAN_POINT('Ctrl Pts',(-28.0898044002542,-12.4537757450517,
112.298867954821)) ;
#173117 = CARTESIAN_POINT('Ctrl Pts',(-28.1636082539867,-12.453775734783,
112.274636944545)) ;
#173118 = CARTESIAN_POINT('Ctrl Pts',(-28.1562756278929,-12.3815986795469,
112.252302947915)) ;
#173119 = CARTESIAN_POINT('Ctrl Pts',(-28.1489430017991,-12.3094216243108,
112.229968951285)) ;
#173120 = CARTESIAN_POINT('Ctrl Pts',(-28.0751391480667,-12.3094216345796,
112.25419996156)) ;
#173121 = CARTESIAN_POINT('Ctrl Pts',(-28.0013352943342,-12.3094216448483,
112.278430971836)) ;
#173122 = CARTESIAN_POINT('Ctrl Pts',(-28.008667920428,-12.3815987000844,
112.300764968466)) ;
#173123 = CARTESIAN_POINT('Ctrl Pts',(-28.1086587938519,-12.3308693682488,
112.569848181414)) ;
#173124 = CARTESIAN_POINT('Ctrl Pts',(-28.1097549437029,-12.4066980840519,
112.573186877588)) ;
#173125 = CARTESIAN_POINT('Ctrl Pts',(-28.1835587964667,-12.4066980849149,
112.548955864362)) ;
#173126 = CARTESIAN_POINT('Ctrl Pts',(-28.2573626492306,-12.4066980857778,
112.524724851136)) ;
#173127 = CARTESIAN_POINT('Ctrl Pts',(-28.2562664993797,-12.3308693699746,
112.521386154962)) ;
#173128 = CARTESIAN_POINT('Ctrl Pts',(-28.2551703495287,-12.2550406541715,
112.518047458789)) ;
#173129 = CARTESIAN_POINT('Ctrl Pts',(-28.1813664967649,-12.2550406533085,
112.542278472015)) ;
#173130 = CARTESIAN_POINT('Ctrl Pts',(-28.107562644001,-12.2550406524456,
112.566509485241)) ;
#173131 = CARTESIAN_POINT('Ctrl Pts',(-28.1086587938519,-12.3308693682488,
112.569848181414)) ;
#173132 = CARTESIAN_POINT('Ctrl Pts',(-28.2098713901146,-12.3583046491224,
112.842561582163)) ;
#173133 = CARTESIAN_POINT('Ctrl Pts',(-28.2046378959205,-12.4323324318187,
112.826621203442)) ;
#173134 = CARTESIAN_POINT('Ctrl Pts',(-28.2784417425771,-12.4323324320423,
112.802390171614)) ;
#173135 = CARTESIAN_POINT('Ctrl Pts',(-28.3522455892337,-12.4323324322659,
112.778159139786)) ;
#173136 = CARTESIAN_POINT('Ctrl Pts',(-28.3574790834278,-12.3583046495696,
112.794099518507)) ;
#173137 = CARTESIAN_POINT('Ctrl Pts',(-28.362712577622,-12.2842768668734,
112.810039897228)) ;
#173138 = CARTESIAN_POINT('Ctrl Pts',(-28.2889087309654,-12.2842768666498,
112.834270929056)) ;
#173139 = CARTESIAN_POINT('Ctrl Pts',(-28.2151048843088,-12.2842768664262,
112.858501960883)) ;
#173140 = CARTESIAN_POINT('Ctrl Pts',(-28.2098713901146,-12.3583046491224,
112.842561582163)) ;
#173141 = CARTESIAN_POINT('Ctrl Pts',(-28.3051249657282,-12.4612718878677,
113.097301430193)) ;
#173142 = CARTESIAN_POINT('Ctrl Pts',(-28.2939651434437,-12.5282228863583,
113.063310412817)) ;
#173143 = CARTESIAN_POINT('Ctrl Pts',(-28.3677689949065,-12.5282229072686,
113.039079395629)) ;
#173144 = CARTESIAN_POINT('Ctrl Pts',(-28.4415728463693,-12.5282229281789,
113.01484837844)) ;
#173145 = CARTESIAN_POINT('Ctrl Pts',(-28.4527326686539,-12.4612719296883,
113.048839395816)) ;
#173146 = CARTESIAN_POINT('Ctrl Pts',(-28.4638924909383,-12.3943209311977,
113.082830413191)) ;
#173147 = CARTESIAN_POINT('Ctrl Pts',(-28.3900886394755,-12.3943209102874,
113.10706143038)) ;
#173148 = CARTESIAN_POINT('Ctrl Pts',(-28.3162847880127,-12.3943208893771,
113.131292447568)) ;
#173149 = CARTESIAN_POINT('Ctrl Pts',(-28.3051249657282,-12.4612718878677,
113.097301430193)) ;
#173150 = CARTESIAN_POINT('Ctrl Pts',(-28.3893018558163,-12.6338543702633,
113.318075545151)) ;
#173151 = CARTESIAN_POINT('Ctrl Pts',(-28.3729836452501,-12.6888516916321,
113.268372907815)) ;
#173152 = CARTESIAN_POINT('Ctrl Pts',(-28.4467874809231,-12.6888516559685,
113.244141842533)) ;
#173153 = CARTESIAN_POINT('Ctrl Pts',(-28.520591316596,-12.6888516203049,
113.219910777251)) ;
#173154 = CARTESIAN_POINT('Ctrl Pts',(-28.5369095271621,-12.6338542989361,
113.269613414587)) ;
#173155 = CARTESIAN_POINT('Ctrl Pts',(-28.5532277377282,-12.5788569775673,
113.319316051923)) ;
#173156 = CARTESIAN_POINT('Ctrl Pts',(-28.4794239020553,-12.5788570132309,
113.343547117205)) ;
#173157 = CARTESIAN_POINT('Ctrl Pts',(-28.4056200663824,-12.5788570488945,
113.367778182487)) ;
#173158 = CARTESIAN_POINT('Ctrl Pts',(-28.3893018558163,-12.6338543702633,
113.318075545151)) ;
#173159 = CARTESIAN_POINT('Ctrl Pts',(-28.4559528062998,-12.8606317098419,
113.485811899978)) ;
#173160 = CARTESIAN_POINT('Ctrl Pts',(-28.4356875294123,-12.8998873118664,
113.424087138298)) ;
#173161 = CARTESIAN_POINT('Ctrl Pts',(-28.5094913849229,-12.8998874003437,
113.399856133438)) ;
#173162 = CARTESIAN_POINT('Ctrl Pts',(-28.5832952404334,-12.8998874888211,
113.375625128578)) ;
#173163 = CARTESIAN_POINT('Ctrl Pts',(-28.6035605173208,-12.8606318867965,
113.437349890258)) ;
#173164 = CARTESIAN_POINT('Ctrl Pts',(-28.6238257942082,-12.821376284772,
113.499074651938)) ;
#173165 = CARTESIAN_POINT('Ctrl Pts',(-28.5500219386977,-12.8213761962946,
113.523305656798)) ;
#173166 = CARTESIAN_POINT('Ctrl Pts',(-28.4762180831872,-12.8213761078173,
113.547536661658)) ;
#173167 = CARTESIAN_POINT('Ctrl Pts',(-28.4559528062998,-12.8606317098419,
113.485811899978)) ;
#173168 = CARTESIAN_POINT('Ctrl Pts',(-28.5023209234415,-13.129518595729,
113.591432315876)) ;
#173169 = CARTESIAN_POINT('Ctrl Pts',(-28.4795225725677,-13.1500300138352,
113.521992214164)) ;
#173170 = CARTESIAN_POINT('Ctrl Pts',(-28.5533264028797,-13.1500298440004,
113.497761132554)) ;
#173171 = CARTESIAN_POINT('Ctrl Pts',(-28.6271302331918,-13.1500296741656,
113.473530050943)) ;
#173172 = CARTESIAN_POINT('Ctrl Pts',(-28.6499285840656,-13.1295182560594,
113.542970152655)) ;
#173173 = CARTESIAN_POINT('Ctrl Pts',(-28.6727269349394,-13.1090068379532,
113.612410254366)) ;
#173174 = CARTESIAN_POINT('Ctrl Pts',(-28.5989231046273,-13.109007007788,
113.636641335977)) ;
#173175 = CARTESIAN_POINT('Ctrl Pts',(-28.5251192743152,-13.1090071776228,
113.660872417588)) ;
#173176 = CARTESIAN_POINT('Ctrl Pts',(-28.5023209234415,-13.129518595729,
113.591432315876)) ;
#173177 = CARTESIAN_POINT('Ctrl Pts',(-28.5173598286699,-13.3215354698077,
113.613640637198)) ;
#173178 = CARTESIAN_POINT('Ctrl Pts',(-28.4939782962573,-13.3286998701254,
113.542424265285)) ;
#173179 = CARTESIAN_POINT('Ctrl Pts',(-28.5677821471769,-13.3287000326328,
113.518193246442)) ;
#173180 = CARTESIAN_POINT('Ctrl Pts',(-28.6415859980966,-13.3287001951402,
113.493962227599)) ;
#173181 = CARTESIAN_POINT('Ctrl Pts',(-28.6649675305092,-13.3215357948224,
113.565178599512)) ;
#173182 = CARTESIAN_POINT('Ctrl Pts',(-28.6883490629218,-13.3143713945047,
113.636394971425)) ;
#173183 = CARTESIAN_POINT('Ctrl Pts',(-28.6145452120022,-13.3143712319973,
113.660625990268)) ;
#173184 = CARTESIAN_POINT('Ctrl Pts',(-28.5407413610825,-13.31437106949,113.684857009111)) ;
#173185 = CARTESIAN_POINT('Ctrl Pts',(-28.5173598286699,-13.3215354698077,
113.613640637198)) ;
#173186 = CARTESIAN_POINT('Ctrl Pts',(-28.520878677028,-13.4175644257172,
113.612558746724)) ;
#173187 = CARTESIAN_POINT('Ctrl Pts',(-28.4974839627901,-13.4180062659798,
113.541302223353)) ;
#173188 = CARTESIAN_POINT('Ctrl Pts',(-28.5712878061994,-13.4180063413679,
113.517071181635)) ;
#173189 = CARTESIAN_POINT('Ctrl Pts',(-28.6450916496088,-13.4180064167561,
113.492840139917)) ;
#173190 = CARTESIAN_POINT('Ctrl Pts',(-28.6684863638467,-13.4175645764935,
113.564096663288)) ;
#173191 = CARTESIAN_POINT('Ctrl Pts',(-28.6918810780846,-13.4171227362309,
113.635353186659)) ;
#173192 = CARTESIAN_POINT('Ctrl Pts',(-28.6180772346753,-13.4171226608428,
113.659584228377)) ;
#173193 = CARTESIAN_POINT('Ctrl Pts',(-28.5442733912659,-13.4171225854547,
113.683815270095)) ;
#173194 = CARTESIAN_POINT('Ctrl Pts',(-28.520878677028,-13.4175644257172,
113.612558746724)) ;
#173195 = CARTESIAN_POINT('',(-17.4415366461909,-12.9727494438644,115.08882743648)) ;
#173196 = CARTESIAN_POINT('',(-17.7467422306782,-14.4181080989129,116.018434402089)) ;
#173197 = CARTESIAN_POINT('Ctrl Pts',(-17.4415366461909,-12.9727494438642,
115.08882743648)) ;
#173198 = CARTESIAN_POINT('Ctrl Pts',(-17.4416493049237,-12.9729113566649,
115.089170576803)) ;
#173199 = CARTESIAN_POINT('Ctrl Pts',(-17.4417445866774,-12.9731380019779,
115.089460789651)) ;
#173200 = CARTESIAN_POINT('Ctrl Pts',(-17.4419266128785,-12.9737505696882,
115.09001521209)) ;
#173201 = CARTESIAN_POINT('Ctrl Pts',(-17.4420039390573,-12.9741371839328,
115.090250735154)) ;
#173202 = CARTESIAN_POINT('Ctrl Pts',(-17.4422222411396,-12.9755496760444,
115.090915648074)) ;
#173203 = CARTESIAN_POINT('Ctrl Pts',(-17.4423092903792,-12.9768233272532,
115.091180786012)) ;
#173204 = CARTESIAN_POINT('Ctrl Pts',(-17.4424780367696,-12.9812525255357,
115.09169476029)) ;
#173205 = CARTESIAN_POINT('Ctrl Pts',(-17.4424107635199,-12.9855810222862,
115.091489856826)) ;
#173206 = CARTESIAN_POINT('Ctrl Pts',(-17.4417642698842,-13.0025035797018,
115.089520741523)) ;
#173207 = CARTESIAN_POINT('Ctrl Pts',(-17.4406256616663,-13.0192459488914,
115.086052724601)) ;
#173208 = CARTESIAN_POINT('Ctrl Pts',(-17.4357398541899,-13.0885454351124,
115.07117134335)) ;
#173209 = CARTESIAN_POINT('Ctrl Pts',(-17.4306638807193,-13.1573238043937,
115.055710747168)) ;
#173210 = CARTESIAN_POINT('Ctrl Pts',(-17.4232190844825,-13.3846429728215,
115.033035099044)) ;
#173211 = CARTESIAN_POINT('Ctrl Pts',(-17.4270784747103,-13.5028371896587,
115.044790178968)) ;
#173212 = CARTESIAN_POINT('Ctrl Pts',(-17.4422801026987,-13.7248060299084,
115.091091885046)) ;
#173213 = CARTESIAN_POINT('Ctrl Pts',(-17.4575003868623,-13.842674137476,
115.137450414823)) ;
#173214 = CARTESIAN_POINT('Ctrl Pts',(-17.5022901009571,-14.0637456275397,
115.273872657162)) ;
#173215 = CARTESIAN_POINT('Ctrl Pts',(-17.5324113344876,-14.1629071646496,
115.365617074455)) ;
#173216 = CARTESIAN_POINT('Ctrl Pts',(-17.5943601419139,-14.2984535233359,
115.554303146472)) ;
#173217 = CARTESIAN_POINT('Ctrl Pts',(-17.6236281361654,-14.3434390384379,
115.643448734658)) ;
#173218 = CARTESIAN_POINT('Ctrl Pts',(-17.6844950745686,-14.4029494275453,
115.82883960819)) ;
#173219 = CARTESIAN_POINT('Ctrl Pts',(-17.7154604463368,-14.4178650105577,
115.923155134283)) ;
#173220 = CARTESIAN_POINT('Ctrl Pts',(-17.7467422306786,-14.4181080983633,
116.018434402091)) ;
#173221 = CARTESIAN_POINT('',(-17.7467422306782,-14.5678329207423,116.018434402089)) ;
#173222 = CARTESIAN_POINT('Ctrl Pts',(-17.7467422306795,-14.5678329226988,
116.018434402093)) ;
#173223 = CARTESIAN_POINT('Ctrl Pts',(-17.7837999493661,-14.5675899683414,
116.131306233972)) ;
#173224 = CARTESIAN_POINT('Ctrl Pts',(-17.820553393073,-14.5486809816127,
116.243251293388)) ;
#173225 = CARTESIAN_POINT('Ctrl Pts',(-17.8912458202562,-14.474265964022,
116.458569020407)) ;
#173226 = CARTESIAN_POINT('Ctrl Pts',(-17.9245709673636,-14.4189847550274,
116.560072041471)) ;
#173227 = CARTESIAN_POINT('Ctrl Pts',(-17.9911651174408,-14.261499390111,
116.76290707768)) ;
#173228 = CARTESIAN_POINT('Ctrl Pts',(-18.0222422523085,-14.1522077768049,
116.857563016237)) ;
#173229 = CARTESIAN_POINT('Ctrl Pts',(-18.0682059255952,-13.906320914405,
116.997560948857)) ;
#173230 = CARTESIAN_POINT('Ctrl Pts',(-18.0833283498345,-13.7731365150372,
117.04362141307)) ;
#173231 = CARTESIAN_POINT('Ctrl Pts',(-18.0968448267067,-13.4847220177906,
117.084790420747)) ;
#173232 = CARTESIAN_POINT('Ctrl Pts',(-18.0920710740004,-13.3621596026309,
117.070250340363)) ;
#173233 = CARTESIAN_POINT('Ctrl Pts',(-18.0838242795246,-13.2522859045863,
117.045131935005)) ;
#173234 = CARTESIAN_POINT('Ctrl Pts',(-18.0807506711114,-13.2255158773084,
117.035770219586)) ;
#173235 = CARTESIAN_POINT('Ctrl Pts',(-18.0778088901523,-13.2094171488094,
117.026810029439)) ;
#173236 = CARTESIAN_POINT('Ctrl Pts',(-18.0771326193299,-13.20622369284,117.024750217551)) ;
#173237 = CARTESIAN_POINT('Ctrl Pts',(-18.0762733506409,-13.2039870459225,
117.022133023767)) ;
#173238 = CARTESIAN_POINT('Ctrl Pts',(-18.0760666869366,-13.2035491479374,
117.021503559547)) ;
#173239 = CARTESIAN_POINT('Ctrl Pts',(-18.075717002172,-13.2031450748714,
117.020438476176)) ;
#173240 = CARTESIAN_POINT('Ctrl Pts',(-18.0755794005162,-13.2030585898593,
117.020019363734)) ;
#173241 = CARTESIAN_POINT('Ctrl Pts',(-18.0753222220269,-13.2030933380485,
117.019236039552)) ;
#173242 = CARTESIAN_POINT('Ctrl Pts',(-18.0752104635191,-13.2031822301836,
117.018895641169)) ;
#173243 = CARTESIAN_POINT('Ctrl Pts',(-18.0749846821218,-13.2035184810667,
117.018207947462)) ;
#173244 = CARTESIAN_POINT('Ctrl Pts',(-18.0748787895421,-13.2037736716702,
117.01788541575)) ;
#173245 = CARTESIAN_POINT('Ctrl Pts',(-18.0746299615403,-13.2045590817022,
117.017127525805)) ;
#173246 = CARTESIAN_POINT('Ctrl Pts',(-18.0745028132178,-13.2051773697714,
117.01674025253)) ;
#173247 = CARTESIAN_POINT('Ctrl Pts',(-18.0741650784759,-13.2071977532132,
117.015711567)) ;
#173248 = CARTESIAN_POINT('Ctrl Pts',(-18.0739890260903,-13.2089958124963,
117.015175339839)) ;
#173249 = CARTESIAN_POINT('Ctrl Pts',(-18.073432868927,-13.2164449755183,
117.013481374855)) ;
#173250 = CARTESIAN_POINT('Ctrl Pts',(-18.0732286091857,-13.2246311944403,
117.012859232641)) ;
#173251 = CARTESIAN_POINT('Ctrl Pts',(-18.0723882663157,-13.2885837862774,
117.010299683847)) ;
#173252 = CARTESIAN_POINT('Ctrl Pts',(-18.0747562393785,-13.4061630903225,
117.017512147145)) ;
#173253 = CARTESIAN_POINT('Ctrl Pts',(-18.0579338010805,-13.6895955424722,
116.96627371438)) ;
#173254 = CARTESIAN_POINT('Ctrl Pts',(-18.0424550542148,-13.8180971458136,
116.919127949494)) ;
#173255 = CARTESIAN_POINT('Ctrl Pts',(-17.9964872591334,-14.0512183347413,
116.779117462552)) ;
#173256 = CARTESIAN_POINT('Ctrl Pts',(-17.9667139535318,-14.1518807047038,
116.688432777588)) ;
#173257 = CARTESIAN_POINT('Ctrl Pts',(-17.9047052645825,-14.2916003512213,
116.499564316113)) ;
#173258 = CARTESIAN_POINT('Ctrl Pts',(-17.8747540318166,-14.3392564455703,
116.408337693765)) ;
#173259 = CARTESIAN_POINT('Ctrl Pts',(-17.8119658998287,-14.4025181298819,
116.217095174557)) ;
#173260 = CARTESIAN_POINT('Ctrl Pts',(-17.7794837034873,-14.4183625292707,
116.118159645449)) ;
#173261 = CARTESIAN_POINT('Ctrl Pts',(-17.7467422306786,-14.4181080983633,
116.018434402091)) ;
#173262 = CARTESIAN_POINT('Ctrl Pts',(-17.7467422940615,-14.5678329187858,
116.018434377539)) ;
#173263 = CARTESIAN_POINT('Ctrl Pts',(-17.7332949369721,-14.567921082103,
115.977475887229)) ;
#173264 = CARTESIAN_POINT('Ctrl Pts',(-17.7198338964835,-14.5655508478998,
115.936475957776)) ;
#173265 = CARTESIAN_POINT('Ctrl Pts',(-17.7064533679514,-14.5607116311535,
115.895721026807)) ;
#173266 = CARTESIAN_POINT('Ctrl Pts',(-17.7008963178764,-14.5587018622779,
115.878795148906)) ;
#173267 = CARTESIAN_POINT('Ctrl Pts',(-17.6953526550133,-14.556266107077,
115.861910046291)) ;
#173268 = CARTESIAN_POINT('Ctrl Pts',(-17.6898291283943,-14.5534035696439,
115.845086275428)) ;
#173269 = CARTESIAN_POINT('Ctrl Pts',(-17.6639931539809,-14.540014217337,
115.766394065983)) ;
#173270 = CARTESIAN_POINT('Ctrl Pts',(-17.6386072513392,-14.5172883204702,
115.689072933564)) ;
#173271 = CARTESIAN_POINT('Ctrl Pts',(-17.6143647373925,-14.4859963413085,
115.615233985268)) ;
#173272 = CARTESIAN_POINT('Ctrl Pts',(-17.6088324961802,-14.4788553831919,
115.598383634115)) ;
#173273 = CARTESIAN_POINT('Ctrl Pts',(-17.603359769088,-14.4712685294603,
115.58171455876)) ;
#173274 = CARTESIAN_POINT('Ctrl Pts',(-17.5979547370195,-14.463245285136,
115.565251703178)) ;
#173275 = CARTESIAN_POINT('Ctrl Pts',(-17.5737703925387,-14.4273459783174,
115.491590092019)) ;
#173276 = CARTESIAN_POINT('Ctrl Pts',(-17.5509423402976,-14.382706735496,
115.422059045954)) ;
#173277 = CARTESIAN_POINT('Ctrl Pts',(-17.5299755060472,-14.3303836683843,
115.358197794957)) ;
#173278 = CARTESIAN_POINT('Ctrl Pts',(-17.5257169917526,-14.3197564784817,
115.34522711722)) ;
#173279 = CARTESIAN_POINT('Ctrl Pts',(-17.5215352397186,-14.3088124559326,
115.33249024464)) ;
#173280 = CARTESIAN_POINT('Ctrl Pts',(-17.5174344587667,-14.2975606758145,
115.319999927519)) ;
#173281 = CARTESIAN_POINT('Ctrl Pts',(-17.4986027738424,-14.2458900353905,
115.262641653721)) ;
#173282 = CARTESIAN_POINT('Ctrl Pts',(-17.4814806589956,-14.1877300152538,
115.210488620322)) ;
#173283 = CARTESIAN_POINT('Ctrl Pts',(-17.4664920220727,-14.1246319652759,
115.164836776727)) ;
#173284 = CARTESIAN_POINT('Ctrl Pts',(-17.4621338516685,-14.1062852633449,
115.151562820284)) ;
#173285 = CARTESIAN_POINT('Ctrl Pts',(-17.4579560289739,-14.0875212502652,
115.138838227179)) ;
#173286 = CARTESIAN_POINT('Ctrl Pts',(-17.4539689063096,-14.0683784694332,
115.126694094864)) ;
#173287 = CARTESIAN_POINT('Ctrl Pts',(-17.4412184801284,-14.0071617388599,
115.08785835399)) ;
#173288 = CARTESIAN_POINT('Ctrl Pts',(-17.4304212800358,-13.9420796939717,
115.054965888367)) ;
#173289 = CARTESIAN_POINT('Ctrl Pts',(-17.421751954825,-13.8743660366251,
115.02856349937)) ;
#173290 = CARTESIAN_POINT('Ctrl Pts',(-17.4183697530646,-13.8479486113346,
115.018263019878)) ;
#173291 = CARTESIAN_POINT('Ctrl Pts',(-17.4153115283899,-13.8211309228484,
115.008949959065)) ;
#173292 = CARTESIAN_POINT('Ctrl Pts',(-17.4125881147126,-13.7939873904681,
115.000654880426)) ;
#173293 = CARTESIAN_POINT('Ctrl Pts',(-17.4101304422485,-13.7694924293578,
114.993169206644)) ;
#173294 = CARTESIAN_POINT('Ctrl Pts',(-17.4079126625351,-13.7443945944633,
114.986414068217)) ;
#173295 = CARTESIAN_POINT('Ctrl Pts',(-17.4059708022617,-13.7189305603966,
114.980499460854)) ;
#173296 = CARTESIAN_POINT('Ctrl Pts',(-17.4040278340081,-13.6934519971441,
114.974581478754)) ;
#173297 = CARTESIAN_POINT('Ctrl Pts',(-17.4023611764262,-13.6676074929265,
114.969505197951)) ;
#173298 = CARTESIAN_POINT('Ctrl Pts',(-17.4009916769738,-13.6416518046287,
114.965334020056)) ;
#173299 = CARTESIAN_POINT('Ctrl Pts',(-17.3996215525311,-13.6156842710883,
114.961160938584)) ;
#173300 = CARTESIAN_POINT('Ctrl Pts',(-17.3985488961501,-13.5896061785694,
114.957893876415)) ;
#173301 = CARTESIAN_POINT('Ctrl Pts',(-17.3977784667299,-13.5636797249837,
114.955547240168)) ;
#173302 = CARTESIAN_POINT('Ctrl Pts',(-17.397095896066,-13.5407098900154,
114.953468211227)) ;
#173303 = CARTESIAN_POINT('Ctrl Pts',(-17.3966503194363,-13.5178594986711,
114.952110927568)) ;
#173304 = CARTESIAN_POINT('Ctrl Pts',(-17.3964343054011,-13.4953086850252,
114.95145298367)) ;
#173305 = CARTESIAN_POINT('Ctrl Pts',(-17.3962500641307,-13.4760747933397,
114.950891814488)) ;
#173306 = CARTESIAN_POINT('Ctrl Pts',(-17.3962259892308,-13.4562541583979,
114.950817703317)) ;
#173307 = CARTESIAN_POINT('Ctrl Pts',(-17.3963872225811,-13.4361251533928,
114.951308483242)) ;
#173308 = CARTESIAN_POINT('Ctrl Pts',(-17.3965481904285,-13.4160292948047,
114.951798454999)) ;
#173309 = CARTESIAN_POINT('Ctrl Pts',(-17.396893950264,-13.3956265064346,
114.952851695746)) ;
#173310 = CARTESIAN_POINT('Ctrl Pts',(-17.39743331335,-13.3751969407048,114.954494975785)) ;
#173311 = CARTESIAN_POINT('Ctrl Pts',(-17.3979644398562,-13.3550793535936,
114.956113161397)) ;
#173312 = CARTESIAN_POINT('Ctrl Pts',(-17.398683284971,-13.3349362383174,
114.958303394013)) ;
#173313 = CARTESIAN_POINT('Ctrl Pts',(-17.399582038043,-13.3150316956181,
114.961041335508)) ;
#173314 = CARTESIAN_POINT('Ctrl Pts',(-17.4005016975791,-13.2946641407519,
114.963842965993)) ;
#173315 = CARTESIAN_POINT('Ctrl Pts',(-17.4016097540901,-13.274546874533,
114.967218079118)) ;
#173316 = CARTESIAN_POINT('Ctrl Pts',(-17.402880521455,-13.2549521381172,
114.971088309475)) ;
#173317 = CARTESIAN_POINT('Ctrl Pts',(-17.40415128882,-13.2353574017014,114.974958539832)) ;
#173318 = CARTESIAN_POINT('Ctrl Pts',(-17.4055846503689,-13.2162855561395,
114.979323458039)) ;
#173319 = CARTESIAN_POINT('Ctrl Pts',(-17.4071386136518,-13.1979917937502,
114.984056579468)) ;
#173320 = CARTESIAN_POINT('Ctrl Pts',(-17.4082540624649,-13.1848603666647,
114.987454056576)) ;
#173321 = CARTESIAN_POINT('Ctrl Pts',(-17.4094975291958,-13.1713626479554,
114.991241248254)) ;
#173322 = CARTESIAN_POINT('Ctrl Pts',(-17.4108532972022,-13.1578519278584,
114.995370749509)) ;
#173323 = CARTESIAN_POINT('Ctrl Pts',(-17.4122190841212,-13.1442413656632,
114.99953076713)) ;
#173324 = CARTESIAN_POINT('Ctrl Pts',(-17.413698885255,-13.1306181206681,
115.004038216471)) ;
#173325 = CARTESIAN_POINT('Ctrl Pts',(-17.4152606318803,-13.1173287413436,
115.0087950996)) ;
#173326 = CARTESIAN_POINT('Ctrl Pts',(-17.4168223785057,-13.1040393620192,
115.01355198273)) ;
#173327 = CARTESIAN_POINT('Ctrl Pts',(-17.4184659685917,-13.0910842149795,
115.018557874953)) ;
#173328 = CARTESIAN_POINT('Ctrl Pts',(-17.4201438439888,-13.078788559479,
115.023668412688)) ;
#173329 = CARTESIAN_POINT('Ctrl Pts',(-17.4213745941723,-13.0697694867344,
115.027417079166)) ;
#173330 = CARTESIAN_POINT('Ctrl Pts',(-17.4227127612408,-13.0604578336814,
115.03149283626)) ;
#173331 = CARTESIAN_POINT('Ctrl Pts',(-17.4241123561879,-13.0513039505984,
115.035755849477)) ;
#173332 = CARTESIAN_POINT('Ctrl Pts',(-17.4255204089638,-13.0420947500989,
115.040044624317)) ;
#173333 = CARTESIAN_POINT('Ctrl Pts',(-17.4269906419727,-13.0330456384297,
115.044522707934)) ;
#173334 = CARTESIAN_POINT('Ctrl Pts',(-17.4284614092985,-13.0245905007224,
115.049002382908)) ;
#173335 = CARTESIAN_POINT('Ctrl Pts',(-17.4286223070298,-13.0236655328831,
115.049492446515)) ;
#173336 = CARTESIAN_POINT('Ctrl Pts',(-17.4287831970196,-13.0227476464621,
115.049982488066)) ;
#173337 = CARTESIAN_POINT('Ctrl Pts',(-17.4289439883956,-13.0218373893616,
115.050472232653)) ;
#173338 = CARTESIAN_POINT('Ctrl Pts',(-17.4300528502253,-13.0155600044732,
115.053849646872)) ;
#173339 = CARTESIAN_POINT('Ctrl Pts',(-17.4312557380411,-13.0090948676773,
115.057513461095)) ;
#173340 = CARTESIAN_POINT('Ctrl Pts',(-17.4324741489107,-13.0030224151988,
115.061224556432)) ;
#173341 = CARTESIAN_POINT('Ctrl Pts',(-17.4330581911971,-13.0001115998757,
115.063003460954)) ;
#173342 = CARTESIAN_POINT('Ctrl Pts',(-17.4336455972628,-12.9972905938871,
115.064792574661)) ;
#173343 = CARTESIAN_POINT('Ctrl Pts',(-17.4342266207035,-12.9946208870877,
115.066562278314)) ;
#173344 = CARTESIAN_POINT('Ctrl Pts',(-17.4352177538382,-12.9900667939414,
115.069581109923)) ;
#173345 = CARTESIAN_POINT('Ctrl Pts',(-17.4362883606204,-12.9855090222264,
115.07284200544)) ;
#173346 = CARTESIAN_POINT('Ctrl Pts',(-17.4373159276886,-12.9817420257543,
115.075971808932)) ;
#173347 = CARTESIAN_POINT('Ctrl Pts',(-17.4379198548086,-12.9795280667821,
115.077811273497)) ;
#173348 = CARTESIAN_POINT('Ctrl Pts',(-17.4385432102028,-12.977460262646,
115.07970991335)) ;
#173349 = CARTESIAN_POINT('Ctrl Pts',(-17.4391363740831,-12.9758473023832,
115.081516594823)) ;
#173350 = CARTESIAN_POINT('Ctrl Pts',(-17.4400557041536,-12.9733474150479,
115.084316725884)) ;
#173351 = CARTESIAN_POINT('Ctrl Pts',(-17.4409267509016,-12.9718729041419,
115.086969793835)) ;
#173352 = CARTESIAN_POINT('Ctrl Pts',(-17.4415366461909,-12.9727494438644,
115.08882743648)) ;
#173353 = CARTESIAN_POINT('',(-6.34456572554058,-13.1500241806476,118.666226584225)) ;
#173354 = CARTESIAN_POINT('Ctrl Pts',(-6.34456572554058,-13.1500241806476,
118.666226584225)) ;
#173355 = CARTESIAN_POINT('Ctrl Pts',(-6.34529362630125,-13.1438552129684,
118.667661018198)) ;
#173356 = CARTESIAN_POINT('Ctrl Pts',(-6.35716264371204,-13.045472096163,
118.691303794064)) ;
#173357 = CARTESIAN_POINT('Ctrl Pts',(-6.38921314251039,-12.8597742993635,
118.764325222303)) ;
#173358 = CARTESIAN_POINT('Ctrl Pts',(-6.45615197626408,-12.6327839415056,
118.932852707777)) ;
#173359 = CARTESIAN_POINT('Ctrl Pts',(-6.53996330725217,-12.4610780963096,
119.152681494851)) ;
#173360 = CARTESIAN_POINT('Ctrl Pts',(-6.63588982776904,-12.3578311300529,
119.409231710552)) ;
#173361 = CARTESIAN_POINT('Ctrl Pts',(-6.736259431342,-12.3309709098726,119.679683383479)) ;
#173362 = CARTESIAN_POINT('Ctrl Pts',(-6.83652100223137,-12.3817310335918,
119.949488204916)) ;
#173363 = CARTESIAN_POINT('Ctrl Pts',(-6.92897537929249,-12.5067458714326,
120.195657155914)) ;
#173364 = CARTESIAN_POINT('Ctrl Pts',(-7.00828982195215,-12.6971218835384,
120.401748881771)) ;
#173365 = CARTESIAN_POINT('Ctrl Pts',(-7.06933695913004,-12.9391053860727,
120.552223222998)) ;
#173366 = CARTESIAN_POINT('Ctrl Pts',(-7.10853205803656,-13.2152764852227,
120.63614997259)) ;
#173367 = CARTESIAN_POINT('Ctrl Pts',(-7.12391162690117,-13.505784356226,
120.64756404441)) ;
#173368 = CARTESIAN_POINT('Ctrl Pts',(-7.11491785946518,-13.7916119971123,
120.584527953854)) ;
#173369 = CARTESIAN_POINT('Ctrl Pts',(-7.08327931847018,-14.0480477215918,
120.452871020505)) ;
#173370 = CARTESIAN_POINT('Ctrl Pts',(-7.03177476396055,-14.2608003622883,
120.260526319525)) ;
#173371 = CARTESIAN_POINT('Ctrl Pts',(-6.96488777055259,-14.4130997833176,
120.021344897526)) ;
#173372 = CARTESIAN_POINT('Ctrl Pts',(-6.88794749547868,-14.494276858583,
119.751438472986)) ;
#173373 = CARTESIAN_POINT('Ctrl Pts',(-6.80764424999997,-14.4979516536895,
119.471388070987)) ;
#173374 = CARTESIAN_POINT('Ctrl Pts',(-6.73039780792071,-14.4245500702158,
119.200701305624)) ;
#173375 = CARTESIAN_POINT('Ctrl Pts',(-6.66228119436863,-14.27912481409,118.957786696)) ;
#173376 = CARTESIAN_POINT('Ctrl Pts',(-6.60891474419106,-14.0717728276009,
118.75974735927)) ;
#173377 = CARTESIAN_POINT('Ctrl Pts',(-6.57501586876472,-13.8168218187551,
118.62092447149)) ;
#173378 = CARTESIAN_POINT('Ctrl Pts',(-6.56385556381707,-13.535324035321,
118.551622243501)) ;
#173379 = CARTESIAN_POINT('Ctrl Pts',(-6.57670200274292,-13.2440746292406,
118.55526577413)) ;
#173380 = CARTESIAN_POINT('Ctrl Pts',(-6.61375984173444,-12.9648031401168,
118.632582291307)) ;
#173381 = CARTESIAN_POINT('Ctrl Pts',(-6.67258342631208,-12.7194345507308,
118.776404079392)) ;
#173382 = CARTESIAN_POINT('Ctrl Pts',(-6.75039015970557,-12.5228537207888,
118.97784552327)) ;
#173383 = CARTESIAN_POINT('Ctrl Pts',(-6.84171874623714,-12.3910219564108,
119.220611387595)) ;
#173384 = CARTESIAN_POINT('Ctrl Pts',(-6.94152390518599,-12.3324946198483,
119.489024176868)) ;
#173385 = CARTESIAN_POINT('Ctrl Pts',(-7.04230587420137,-12.3517941049946,
119.760653819778)) ;
#173386 = CARTESIAN_POINT('Ctrl Pts',(-7.13886766534031,-12.4476532719571,
120.019204540318)) ;
#173387 = CARTESIAN_POINT('Ctrl Pts',(-7.22405843886179,-12.6128436094032,
120.24325293471)) ;
#173388 = CARTESIAN_POINT('Ctrl Pts',(-7.29301191518833,-12.8354722898284,
120.417835047233)) ;
#173389 = CARTESIAN_POINT('Ctrl Pts',(-7.34159724157024,-13.101408894203,
120.530187095211)) ;
#173390 = CARTESIAN_POINT('Ctrl Pts',(-7.36657138807077,-13.3874022195482,
120.570964865022)) ;
#173391 = CARTESIAN_POINT('Ctrl Pts',(-7.36752626591963,-13.6768759171903,
120.538418289664)) ;
#173392 = CARTESIAN_POINT('Ctrl Pts',(-7.34470605061851,-13.948608493865,
120.433347699827)) ;
#173393 = CARTESIAN_POINT('Ctrl Pts',(-7.30074221590675,-14.181257681225,
120.264014178484)) ;
#173394 = CARTESIAN_POINT('Ctrl Pts',(-7.23958451504645,-14.3592650506284,
120.042343425265)) ;
#173395 = CARTESIAN_POINT('Ctrl Pts',(-7.16614529781219,-14.4703402370834,
119.783202402502)) ;
#173396 = CARTESIAN_POINT('Ctrl Pts',(-7.08630537122041,-14.5059089260168,
119.504470384707)) ;
#173397 = CARTESIAN_POINT('Ctrl Pts',(-7.00714711584661,-14.4635906108697,
119.22798980315)) ;
#173398 = CARTESIAN_POINT('Ctrl Pts',(-6.9343979792678,-14.3462861335646,
118.970893409468)) ;
#173399 = CARTESIAN_POINT('Ctrl Pts',(-6.87439561306881,-14.1620807273187,
118.752616009014)) ;
#173400 = CARTESIAN_POINT('Ctrl Pts',(-6.83231279792918,-13.9257450561724,
118.589088105333)) ;
#173401 = CARTESIAN_POINT('Ctrl Pts',(-6.81152149947454,-13.6518932520307,
118.490235528419)) ;
#173402 = CARTESIAN_POINT('Ctrl Pts',(-6.81458866379034,-13.361350209501,
118.464074361768)) ;
#173403 = CARTESIAN_POINT('Ctrl Pts',(-6.84190912425954,-13.0754523993138,
118.511850887542)) ;
#173404 = CARTESIAN_POINT('Ctrl Pts',(-6.89221998106671,-12.8139381990977,
118.629651920743)) ;
#173405 = CARTESIAN_POINT('Ctrl Pts',(-6.96317166541847,-12.5948180944483,
118.810143346469)) ;
#173406 = CARTESIAN_POINT('Ctrl Pts',(-7.04930238281719,-12.4362800048722,
119.037190426179)) ;
#173407 = CARTESIAN_POINT('Ctrl Pts',(-7.14639896583729,-12.346922078608,
119.29741677471)) ;
#173408 = CARTESIAN_POINT('Ctrl Pts',(-7.24765406779605,-12.3346186385411,
119.570362985162)) ;
#173409 = CARTESIAN_POINT('Ctrl Pts',(-7.34665382402801,-12.3998225687949,
119.836445852581)) ;
#173410 = CARTESIAN_POINT('Ctrl Pts',(-7.4370740592955,-12.5378477500096,
120.076408147661)) ;
#173411 = CARTESIAN_POINT('Ctrl Pts',(-7.5133452204639,-12.7392396507352,
120.273212489585)) ;
#173412 = CARTESIAN_POINT('Ctrl Pts',(-7.57051158312834,-12.989236405783,
120.411850909373)) ;
#173413 = CARTESIAN_POINT('Ctrl Pts',(-7.60526793750275,-13.269049028932,
120.482338834054)) ;
#173414 = CARTESIAN_POINT('Ctrl Pts',(-7.61610217928452,-13.560604521515,
120.479829556645)) ;
#173415 = CARTESIAN_POINT('Ctrl Pts',(-7.60265701261583,-13.8423158077137,
120.4033105886)) ;
#173416 = CARTESIAN_POINT('Ctrl Pts',(-7.56703031046435,-14.0920492190499,
120.259455200578)) ;
#173417 = CARTESIAN_POINT('Ctrl Pts',(-7.51204303377268,-14.2950965364046,
120.056387264096)) ;
#173418 = CARTESIAN_POINT('Ctrl Pts',(-7.44273831121475,-14.434335219557,
119.809815786678)) ;
#173419 = CARTESIAN_POINT('Ctrl Pts',(-7.36521040000063,-14.5007530721094,
119.538381721836)) ;
#173420 = CARTESIAN_POINT('Ctrl Pts',(-7.28479809434297,-14.4901437351793,
119.257926243117)) ;
#173421 = CARTESIAN_POINT('Ctrl Pts',(-7.20843821052364,-14.402041943339,
118.989761053497)) ;
#173422 = CARTESIAN_POINT('Ctrl Pts',(-7.1427835920666,-14.243691286176,118.754343222241)) ;
#173423 = CARTESIAN_POINT('Ctrl Pts',(-7.09305076334606,-14.0272168477211,
118.567541759605)) ;
#173424 = CARTESIAN_POINT('Ctrl Pts',(-7.06320365437595,-13.7664028194368,
118.441170630651)) ;
#173425 = CARTESIAN_POINT('Ctrl Pts',(-7.05638533636368,-13.4798811075686,
118.384860283325)) ;
#173426 = CARTESIAN_POINT('Ctrl Pts',(-7.07408092560861,-13.1885796838075,
118.403166688914)) ;
#173427 = CARTESIAN_POINT('Ctrl Pts',(-7.11507198338345,-12.9166253502417,
118.492814113544)) ;
#173428 = CARTESIAN_POINT('Ctrl Pts',(-7.1780574208389,-12.6775835687805,
118.649064501798)) ;
#173429 = CARTESIAN_POINT('Ctrl Pts',(-7.25891893918462,-12.4925681740676,
118.859833268336)) ;
#173430 = CARTESIAN_POINT('Ctrl Pts',(-7.35188793041178,-12.3743553948694,
119.107715107246)) ;
#173431 = CARTESIAN_POINT('Ctrl Pts',(-7.45265031525607,-12.3300586716913,
119.37899047094)) ;
#173432 = CARTESIAN_POINT('Ctrl Pts',(-7.55337524562207,-12.3643855283945,
119.650314676817)) ;
#173433 = CARTESIAN_POINT('Ctrl Pts',(-7.64773366833853,-12.4735026256636,
119.902366613272)) ;
#173434 = CARTESIAN_POINT('Ctrl Pts',(-7.73041986817396,-12.6505044221707,
120.118738891923)) ;
#173435 = CARTESIAN_POINT('Ctrl Pts',(-7.79595012127722,-12.883421947767,
120.282755379935)) ;
#173436 = CARTESIAN_POINT('Ctrl Pts',(-7.83999077408972,-13.1527514798463,
120.381574983125)) ;
#173437 = CARTESIAN_POINT('Ctrl Pts',(-7.86072974007722,-13.4437023579035,
120.40908356129)) ;
#173438 = CARTESIAN_POINT('Ctrl Pts',(-7.85692244140455,-13.7306193771303,
120.362100112163)) ;
#173439 = CARTESIAN_POINT('Ctrl Pts',(-7.83012410737516,-13.9949086675026,
120.245151518457)) ;
#173440 = CARTESIAN_POINT('Ctrl Pts',(-7.78237083717385,-14.2196906214034,
120.06409456817)) ;
#173441 = CARTESIAN_POINT('Ctrl Pts',(-7.71854875724072,-14.3856064052365,
119.834353268658)) ;
#173442 = CARTESIAN_POINT('Ctrl Pts',(-7.64334502750247,-14.4829720573525,
119.569777363778)) ;
#173443 = CARTESIAN_POINT('Ctrl Pts',(-7.56338289868114,-14.5039687036518,
119.290821303275)) ;
#173444 = CARTESIAN_POINT('Ctrl Pts',(-7.48437547453331,-14.4466173797893,
119.014508165448)) ;
#173445 = CARTESIAN_POINT('Ctrl Pts',(-7.41403834460529,-14.3162716014842,
118.764955621569)) ;
#173446 = CARTESIAN_POINT('Ctrl Pts',(-7.35704039989976,-14.1214968775469,
118.555885778132)) ;
#173447 = CARTESIAN_POINT('Ctrl Pts',(-7.31852311276589,-13.8749956323593,
118.402954989973)) ;
#173448 = CARTESIAN_POINT('Ctrl Pts',(-7.30231103568058,-13.5974682752699,
118.318202627209)) ;
#173449 = CARTESIAN_POINT('Ctrl Pts',(-7.30987663537963,-13.3070931499256,
118.305860700972)) ;
#173450 = CARTESIAN_POINT('Ctrl Pts',(-7.34175942853511,-13.0233508116479,
118.36742076646)) ;
#173451 = CARTESIAN_POINT('Ctrl Pts',(-7.39618528009665,-12.7688607554056,
118.497769967232)) ;
#173452 = CARTESIAN_POINT('Ctrl Pts',(-7.47020228300154,-12.5604071436069,
118.687726339368)) ;
#173453 = CARTESIAN_POINT('Ctrl Pts',(-7.55906350518853,-12.4137261008746,
118.922952330464)) ;
#173454 = CARTESIAN_POINT('Ctrl Pts',(-7.65717245038672,-12.3387040702925,
119.186368813652)) ;
#173455 = CARTESIAN_POINT('Ctrl Pts',(-7.75884035692309,-12.3410592400664,
119.460451576393)) ;
#173456 = CARTESIAN_POINT('Ctrl Pts',(-7.85654736634483,-12.4205041979803,
119.722651987663)) ;
#173457 = CARTESIAN_POINT('Ctrl Pts',(-7.94481318053513,-12.5715202421064,
119.956000118428)) ;
#173458 = CARTESIAN_POINT('Ctrl Pts',(-8.01771408381364,-12.7831706996134,
120.142578445181)) ;
#173459 = CARTESIAN_POINT('Ctrl Pts',(-8.07085503105618,-13.0400861903177,
120.268992723008)) ;
#173460 = CARTESIAN_POINT('Ctrl Pts',(-8.1012449479731,-13.3242719779506,
120.326083671067)) ;
#173461 = CARTESIAN_POINT('Ctrl Pts',(-8.10739844779683,-13.6152878377403,
120.309341878199)) ;
#173462 = CARTESIAN_POINT('Ctrl Pts',(-8.08962004095609,-13.8920338673762,
120.219720905231)) ;
#173463 = CARTESIAN_POINT('Ctrl Pts',(-8.05001723486067,-14.1346381572922,
120.063660745971)) ;
#173464 = CARTESIAN_POINT('Ctrl Pts',(-7.992024762362,-14.3262307223465,119.85152566265)) ;
#173465 = CARTESIAN_POINT('Ctrl Pts',(-7.92087420413947,-14.4523301137118,
119.599430244914)) ;
#173466 = CARTESIAN_POINT('Ctrl Pts',(-7.84204196997817,-14.5048566464616,
119.323854472488)) ;
#173467 = CARTESIAN_POINT('Ctrl Pts',(-7.76186601911956,-14.4792282215674,
119.044096181178)) ;
#173468 = CARTESIAN_POINT('Ctrl Pts',(-7.68732567425835,-14.3776591931245,
118.781625479166)) ;
#173469 = CARTESIAN_POINT('Ctrl Pts',(-7.62415597339361,-14.2073582471136,
118.553754081591)) ;
#173470 = CARTESIAN_POINT('Ctrl Pts',(-7.57772822356053,-13.980463190757,
118.376876023582)) ;
#173471 = CARTESIAN_POINT('Ctrl Pts',(-7.55211423680401,-13.7134648384933,
118.263415580786)) ;
#173472 = CARTESIAN_POINT('Ctrl Pts',(-7.54988396928805,-13.4252028157263,
118.221162235282)) ;
#173473 = CARTESIAN_POINT('Ctrl Pts',(-7.57190400588021,-13.136660084581,
118.252804065339)) ;
#173474 = CARTESIAN_POINT('Ctrl Pts',(-7.61755830701388,-12.8674128564449,
118.356315160482)) ;
#173475 = CARTESIAN_POINT('Ctrl Pts',(-7.68406859821228,-12.6383938778605,
118.523453892796)) ;
#173476 = CARTESIAN_POINT('Ctrl Pts',(-7.76755837693475,-12.465038874388,
118.74228416299)) ;
#173477 = CARTESIAN_POINT('Ctrl Pts',(-7.86272316977547,-12.3599344396702,
118.99669592537)) ;
#173478 = CARTESIAN_POINT('Ctrl Pts',(-7.96381251944024,-12.3306429195518,
119.269059347859)) ;
#173479 = CARTESIAN_POINT('Ctrl Pts',(-8.06368380821921,-12.3792038030185,
119.537856629935)) ;
#173480 = CARTESIAN_POINT('Ctrl Pts',(-8.15659748944132,-12.502250920438,
119.785364900155)) ;
#173481 = CARTESIAN_POINT('Ctrl Pts',(-8.23623754753109,-12.690704289041,
119.992502391065)) ;
#173482 = CARTESIAN_POINT('Ctrl Pts',(-8.29787978612712,-12.9312491813812,
120.144802031741)) ;
#173483 = CARTESIAN_POINT('Ctrl Pts',(-8.33778763616187,-13.2069304836541,
120.230868966777)) ;
#173484 = CARTESIAN_POINT('Ctrl Pts',(-8.35386611104003,-13.4971323588194,
120.244433805866)) ;
#173485 = CARTESIAN_POINT('Ctrl Pts',(-8.34559176606117,-13.7832858649534,
120.183607286869)) ;
#173486 = CARTESIAN_POINT('Ctrl Pts',(-8.31464185127322,-14.0408293277911,
120.054056184709)) ;
#173487 = CARTESIAN_POINT('Ctrl Pts',(-8.26340664177902,-14.255952322556,
119.862377902584)) ;
#173488 = CARTESIAN_POINT('Ctrl Pts',(-8.1971249772834,-14.4094466686143,
119.625180693076)) ;
#173489 = CARTESIAN_POINT('Ctrl Pts',(-8.12040152389499,-14.4929694646286,
119.35593056019)) ;
#173490 = CARTESIAN_POINT('Ctrl Pts',(-8.04009022848257,-14.4990155260453,
119.075851461994)) ;
#173491 = CARTESIAN_POINT('Ctrl Pts',(-7.9625098388441,-14.4275804860338,
118.804068220134)) ;
#173492 = CARTESIAN_POINT('Ctrl Pts',(-7.8941100124004,-14.284309082368,118.560336785865)) ;
#173493 = CARTESIAN_POINT('Ctrl Pts',(-7.84012347499757,-14.0775350374868,
118.360268383229)) ;
#173494 = CARTESIAN_POINT('Ctrl Pts',(-7.80588583848825,-13.8261134335288,
118.220747745965)) ;
#173495 = CARTESIAN_POINT('Ctrl Pts',(-7.79385768957157,-13.5428648342343,
118.148500404782)) ;
#173496 = CARTESIAN_POINT('Ctrl Pts',(-7.80612682657335,-13.252182353688,
118.150461687266)) ;
#173497 = CARTESIAN_POINT('Ctrl Pts',(-7.84228893480843,-12.9730234465435,
118.225161565708)) ;
#173498 = CARTESIAN_POINT('Ctrl Pts',(-7.90103421558884,-12.724731390434,
118.368470996422)) ;
#173499 = CARTESIAN_POINT('Ctrl Pts',(-7.97782116130876,-12.5280561031159,
118.567077843843)) ;
#173500 = CARTESIAN_POINT('Ctrl Pts',(-8.0692686377754,-12.3935893009494,
118.810023631757)) ;
#173501 = CARTESIAN_POINT('Ctrl Pts',(-8.16837016553241,-12.333081965445,
119.076502994386)) ;
#173502 = CARTESIAN_POINT('Ctrl Pts',(-8.27009279108481,-12.3505128306963,
119.350670896121)) ;
#173503 = CARTESIAN_POINT('Ctrl Pts',(-8.3658449010965,-12.4433828921911,
119.60714075347)) ;
#173504 = CARTESIAN_POINT('Ctrl Pts',(-8.45197505795687,-12.607349424796,
119.833841108759)) ;
#173505 = CARTESIAN_POINT('Ctrl Pts',(-8.52120977492203,-12.8279036385121,
120.00940010572)) ;
#173506 = CARTESIAN_POINT('Ctrl Pts',(-8.57055325895007,-13.0930059035689,
120.124025527535)) ;
#173507 = CARTESIAN_POINT('Ctrl Pts',(-8.59625204583721,-13.3789266137586,
120.166977376249)) ;
#173508 = CARTESIAN_POINT('Ctrl Pts',(-8.59788852250651,-13.6686885717782,
120.136495690536)) ;
#173509 = CARTESIAN_POINT('Ctrl Pts',(-8.57580906244584,-13.9407698971193,
120.033752331659)) ;
#173510 = CARTESIAN_POINT('Ctrl Pts',(-8.53228870836988,-14.1754452261927,
119.865663575393)) ;
#173511 = CARTESIAN_POINT('Ctrl Pts',(-8.47162858688881,-14.3550939223612,
119.645549235714)) ;
#173512 = CARTESIAN_POINT('Ctrl Pts',(-8.39799248590873,-14.468598908444,
119.385596001449)) ;
#173513 = CARTESIAN_POINT('Ctrl Pts',(-8.31877491440371,-14.5058659881171,
119.109007145666)) ;
#173514 = CARTESIAN_POINT('Ctrl Pts',(-8.23941378855136,-14.465907705861,
118.831859781048)) ;
#173515 = CARTESIAN_POINT('Ctrl Pts',(-8.16647270185438,-14.3507454275659,
118.574221540228)) ;
#173516 = CARTESIAN_POINT('Ctrl Pts',(-8.10601871451368,-14.1684902162708,
118.354580107972)) ;
#173517 = CARTESIAN_POINT('Ctrl Pts',(-8.06327379464778,-13.9330107336615,
118.188967146787)) ;
#173518 = CARTESIAN_POINT('Ctrl Pts',(-8.04188464728271,-13.6600763512271,
118.088315145107)) ;
#173519 = CARTESIAN_POINT('Ctrl Pts',(-8.04415984284868,-13.3704757504778,
118.059833665652)) ;
#173520 = CARTESIAN_POINT('Ctrl Pts',(-8.07098859328993,-13.0823700026988,
118.105885959188)) ;
#173521 = CARTESIAN_POINT('Ctrl Pts',(-8.120503467602,-12.8213180178566,118.221441446184)) ;
#173522 = CARTESIAN_POINT('Ctrl Pts',(-8.19068066224925,-12.6009816910039,
118.399651162582)) ;
#173523 = CARTESIAN_POINT('Ctrl Pts',(-8.27663038654765,-12.4399155910324,
118.626049746092)) ;
#173524 = CARTESIAN_POINT('Ctrl Pts',(-8.37377653671491,-12.3483508718252,
118.886335164228)) ;
#173525 = CARTESIAN_POINT('Ctrl Pts',(-8.47470424960895,-12.3338872424077,
119.158388022071)) ;
#173526 = CARTESIAN_POINT('Ctrl Pts',(-8.5740859453798,-12.396923495094,119.425556245681)) ;
#173527 = CARTESIAN_POINT('Ctrl Pts',(-8.6649277864638,-12.5334553693914,
119.666748762957)) ;
#173528 = CARTESIAN_POINT('Ctrl Pts',(-8.74128429943828,-12.7322215761211,
119.863992617795)) ;
#173529 = CARTESIAN_POINT('Ctrl Pts',(-8.79916573819104,-12.9810049412899,
120.004790749052)) ;
#173530 = CARTESIAN_POINT('Ctrl Pts',(-8.83469320205863,-13.2609753303157,
120.077533333241)) ;
#173531 = CARTESIAN_POINT('Ctrl Pts',(-8.84616539838749,-13.5522070361543,
120.07700191012)) ;
#173532 = CARTESIAN_POINT('Ctrl Pts',(-8.83352879857719,-13.8335794690488,
120.003072712917)) ;
#173533 = CARTESIAN_POINT('Ctrl Pts',(-8.79840525558534,-14.0854850074698,
119.86061077159)) ;
#173534 = CARTESIAN_POINT('Ctrl Pts',(-8.74411665331808,-14.2893882283517,
119.659805611785)) ;
#173535 = CARTESIAN_POINT('Ctrl Pts',(-8.67521497823715,-14.4310416708449,
119.414456500244)) ;
#173536 = CARTESIAN_POINT('Ctrl Pts',(-8.59746348536126,-14.4999960091202,
119.142167399687)) ;
#173537 = CARTESIAN_POINT('Ctrl Pts',(-8.51725220866625,-14.4914668725251,
118.862420893709)) ;
#173538 = CARTESIAN_POINT('Ctrl Pts',(-8.44094453814601,-14.4062237339893,
118.594550823069)) ;
#173539 = CARTESIAN_POINT('Ctrl Pts',(-8.37461958404781,-14.2495321967945,
118.356968882225)) ;
#173540 = CARTESIAN_POINT('Ctrl Pts',(-8.32425634296907,-14.0340281298451,
118.168167653125)) ;
#173541 = CARTESIAN_POINT('Ctrl Pts',(-8.29382206288613,-13.7742259092907,
118.040014681808)) ;
#173542 = CARTESIAN_POINT('Ctrl Pts',(-8.28631480334285,-13.488993839479,
117.981708548653)) ;
#173543 = CARTESIAN_POINT('Ctrl Pts',(-8.30320195637338,-13.1975717487405,
117.997560479062)) ;
#173544 = CARTESIAN_POINT('Ctrl Pts',(-8.3436703131233,-12.9237175982201,
118.085475777875)) ;
#173545 = CARTESIAN_POINT('Ctrl Pts',(-8.4062239104521,-12.6833926232874,
118.240377888327)) ;
#173546 = CARTESIAN_POINT('Ctrl Pts',(-8.48615190099208,-12.4975233316372,
118.448503252107)) ;
#173547 = CARTESIAN_POINT('Ctrl Pts',(-8.57934667074232,-12.3765652756753,
118.696871045336)) ;
#173548 = CARTESIAN_POINT('Ctrl Pts',(-8.67942447659642,-12.3303669115662,
118.966269185261)) ;
#173549 = CARTESIAN_POINT('Ctrl Pts',(-8.78046560292115,-12.3620831181533,
119.23847587387)) ;
#173550 = CARTESIAN_POINT('Ctrl Pts',(-8.87549407917763,-12.4697592102098,
119.49241363428)) ;
#173551 = CARTESIAN_POINT('Ctrl Pts',(-8.95832054343873,-12.6447797711106,
119.709301795168)) ;
#173552 = CARTESIAN_POINT('Ctrl Pts',(-9.02420754409074,-12.8750273852739,
119.874571217192)) ;
#173553 = CARTESIAN_POINT('Ctrl Pts',(-9.06917668282671,-13.1453257818208,
119.975977828757)) ;
#173554 = CARTESIAN_POINT('Ctrl Pts',(-9.09047067571145,-13.4336234546741,
120.005474883971)) ;
#173555 = CARTESIAN_POINT('Ctrl Pts',(-9.08746787607695,-13.7229316022969,
119.960694301127)) ;
#173556 = CARTESIAN_POINT('Ctrl Pts',(-9.06117191970581,-13.9881204584926,
119.845257989114)) ;
#173557 = CARTESIAN_POINT('Ctrl Pts',(-9.01419630762022,-14.2135626266573,
119.66671241156)) ;
#173558 = CARTESIAN_POINT('Ctrl Pts',(-8.95045579816424,-14.3820856851378,
119.437041610208)) ;
#173559 = CARTESIAN_POINT('Ctrl Pts',(-8.87581727914137,-14.4811007735871,
119.174352555604)) ;
#173560 = CARTESIAN_POINT('Ctrl Pts',(-8.79562316232527,-14.5043853087956,
118.894554465702)) ;
#173561 = CARTESIAN_POINT('Ctrl Pts',(-8.71698219857194,-14.4497319209782,
118.619592459032)) ;
#173562 = CARTESIAN_POINT('Ctrl Pts',(-8.64580441276013,-14.3208489038209,
118.36724001526)) ;
#173563 = CARTESIAN_POINT('Ctrl Pts',(-8.5883553866719,-14.1269083086763,
118.156726837458)) ;
#173564 = CARTESIAN_POINT('Ctrl Pts',(-8.54955936673305,-13.8839530008224,
118.003271664693)) ;
#173565 = CARTESIAN_POINT('Ctrl Pts',(-8.53248329253628,-13.6058131007772,
117.915704634662)) ;
#173566 = CARTESIAN_POINT('Ctrl Pts',(-8.53937026013509,-13.3154623494247,
117.901296893058)) ;
#173567 = CARTESIAN_POINT('Ctrl Pts',(-8.57069168239456,-13.0305252756843,
117.961054033285)) ;
#173568 = CARTESIAN_POINT('Ctrl Pts',(-8.62430702145784,-12.7760411077928,
118.089081673625)) ;
#173569 = CARTESIAN_POINT('Ctrl Pts',(-8.69778013803695,-12.5658693797106,
118.277375059853)) ;
#173570 = CARTESIAN_POINT('Ctrl Pts',(-8.78628545767639,-12.4170609140262,
118.511509776539)) ;
#173571 = CARTESIAN_POINT('Ctrl Pts',(-8.88463232709871,-12.3396249333132,
118.775501151269)) ;
#173572 = CARTESIAN_POINT('Ctrl Pts',(-8.9861492359783,-12.340046412335,119.04917803503)) ;
#173573 = CARTESIAN_POINT('Ctrl Pts',(-9.08378193823022,-12.4170460254182,
119.311248494083)) ;
#173574 = CARTESIAN_POINT('Ctrl Pts',(-9.17250255530307,-12.5662136094611,
119.545947051563)) ;
#173575 = CARTESIAN_POINT('Ctrl Pts',(-9.24585112857785,-12.7760199991739,
119.733930887948)) ;
#173576 = CARTESIAN_POINT('Ctrl Pts',(-9.29969159508292,-13.0322696653641,
119.862416821601)) ;
#173577 = CARTESIAN_POINT('Ctrl Pts',(-9.33072971583805,-13.3151090323585,
119.921587753964)) ;
#173578 = CARTESIAN_POINT('Ctrl Pts',(-9.33762134165996,-13.6075492018493,
119.906927850832)) ;
#173579 = CARTESIAN_POINT('Ctrl Pts',(-9.32055446084888,-13.8839937911961,
119.819605029903)) ;
#173580 = CARTESIAN_POINT('Ctrl Pts',(-9.28147726722591,-14.1283418739825,
119.665069210431)) ;
#173581 = CARTESIAN_POINT('Ctrl Pts',(-9.22417716238159,-14.321085337762,
119.455168775729)) ;
#173582 = CARTESIAN_POINT('Ctrl Pts',(-9.1528918141783,-14.4501544762085,
119.202433516862)) ;
#173583 = CARTESIAN_POINT('Ctrl Pts',(-9.07410157725992,-14.504350239421,
118.926962323926)) ;
#173584 = CARTESIAN_POINT('Ctrl Pts',(-8.99439714763998,-14.4811635345991,
118.648874617531)) ;
#173585 = CARTESIAN_POINT('Ctrl Pts',(-8.91938092952298,-14.3816036851556,
118.384850057937)) ;
#173586 = CARTESIAN_POINT('Ctrl Pts',(-8.8558492241993,-14.2132115910195,
118.155902462999)) ;
#173587 = CARTESIAN_POINT('Ctrl Pts',(-8.80875359263179,-13.9871283531687,
117.97689596451)) ;
#173588 = CARTESIAN_POINT('Ctrl Pts',(-8.78260162901795,-13.7209751384546,
117.86180531742)) ;
#173589 = CARTESIAN_POINT('Ctrl Pts',(-8.7796418761099,-13.4341833204507,
117.817471206849)) ;
#173590 = CARTESIAN_POINT('Ctrl Pts',(-8.80108831291345,-13.1440226446982,
117.847195297999)) ;
#173591 = CARTESIAN_POINT('Ctrl Pts',(-8.84592426043001,-12.8750223963181,
117.948364040509)) ;
#173592 = CARTESIAN_POINT('Ctrl Pts',(-8.91216833972909,-12.6437154561283,
118.114539740324)) ;
#173593 = CARTESIAN_POINT('Ctrl Pts',(-8.99483011325719,-12.4695015573388,
118.331032618802)) ;
#173594 = CARTESIAN_POINT('Ctrl Pts',(-9.08998111303647,-12.3618253102505,
118.585299380963)) ;
#173595 = CARTESIAN_POINT('Ctrl Pts',(-9.1909709333649,-12.3304086987919,
118.857374561843)) ;
#173596 = CARTESIAN_POINT('Ctrl Pts',(-9.29090632432286,-12.3767667157857,
119.126380154863)) ;
#173597 = CARTESIAN_POINT('Ctrl Pts',(-9.38394796937826,-12.4973266925111,
119.374354583408)) ;
#173598 = CARTESIAN_POINT('Ctrl Pts',(-9.4644362377349,-12.6849702880242,
119.583900943341)) ;
#173599 = CARTESIAN_POINT('Ctrl Pts',(-9.5264642676195,-12.9239536141708,
119.737443599299)) ;
#173600 = CARTESIAN_POINT('Ctrl Pts',(-9.56699499377198,-13.198264514804,
119.825482569648)) ;
#173601 = CARTESIAN_POINT('Ctrl Pts',(-9.58379794756891,-13.4887696764051,
119.841196258796)) ;
#173602 = CARTESIAN_POINT('Ctrl Pts',(-9.57628694483019,-13.7747050880232,
119.782787604556)) ;
#173603 = CARTESIAN_POINT('Ctrl Pts',(-9.54578275574017,-14.0346989777519,
119.65439454944)) ;
#173604 = CARTESIAN_POINT('Ctrl Pts',(-9.49516719411495,-14.2504823475427,
119.464718649369)) ;
#173605 = CARTESIAN_POINT('Ctrl Pts',(-9.42925750378619,-14.4061007577842,
119.228637274552)) ;
#173606 = CARTESIAN_POINT('Ctrl Pts',(-9.35244000585146,-14.4917978275685,
118.958975475398)) ;
#173607 = CARTESIAN_POINT('Ctrl Pts',(-9.27254720983972,-14.4998539330622,
118.680348428381)) ;
#173608 = CARTESIAN_POINT('Ctrl Pts',(-9.19483422021103,-14.4309092256038,
118.408185227294)) ;
#173609 = CARTESIAN_POINT('Ctrl Pts',(-9.12600873086239,-14.2894596882656,
118.163115988674)) ;
#173610 = CARTESIAN_POINT('Ctrl Pts',(-9.07154849099475,-14.0846391379262,
117.961648450783)) ;
#173611 = CARTESIAN_POINT('Ctrl Pts',(-9.036633988908,-13.833584389583,117.819961399887)) ;
#173612 = CARTESIAN_POINT('Ctrl Pts',(-9.02391466502751,-13.5522887119168,
117.745782719323)) ;
#173613 = CARTESIAN_POINT('Ctrl Pts',(-9.03557274648368,-13.2592972529684,
117.745601612871)) ;
#173614 = CARTESIAN_POINT('Ctrl Pts',(-9.07098090557538,-12.9811038250668,
117.818197097558)) ;
#173615 = CARTESIAN_POINT('Ctrl Pts',(-9.1288816653457,-12.7319954339599,
117.959013661815)) ;
#173616 = CARTESIAN_POINT('Ctrl Pts',(-9.20542108821079,-12.5329045763516,
118.156747660811)) ;
#173617 = CARTESIAN_POINT('Ctrl Pts',(-9.2965722776736,-12.3964115152595,
118.398783809131)) ;
#173618 = CARTESIAN_POINT('Ctrl Pts',(-9.39560158322444,-12.3338312624075,
118.665015098447)) ;
#173619 = CARTESIAN_POINT('Ctrl Pts',(-9.4968318946719,-12.3486707517994,
118.937874104534)) ;
#173620 = CARTESIAN_POINT('Ctrl Pts',(-9.59343723857601,-12.4397941697449,
119.196716726627)) ;
#173621 = CARTESIAN_POINT('Ctrl Pts',(-9.67989153670841,-12.6021170084136,
119.424415022172)) ;
#173622 = CARTESIAN_POINT('Ctrl Pts',(-9.74951237514481,-12.8208593941247,
119.601209318802)) ;
#173623 = CARTESIAN_POINT('Ctrl Pts',(-9.79944954754396,-13.084370773037,
119.717716848365)) ;
#173624 = CARTESIAN_POINT('Ctrl Pts',(-9.82597149657916,-13.3711928765175,
119.763016540292)) ;
#173625 = CARTESIAN_POINT('Ctrl Pts',(-9.82819214417096,-13.6609866789311,
119.734331572361)) ;
#173626 = CARTESIAN_POINT('Ctrl Pts',(-9.8068991329201,-13.9327616913683,
119.63413267067)) ;
#173627 = CARTESIAN_POINT('Ctrl Pts',(-9.76382464831486,-14.1696775509721,
119.467276311035)) ;
#173628 = CARTESIAN_POINT('Ctrl Pts',(-9.7036673139555,-14.3505522399701,
119.248758719857)) ;
#173629 = CARTESIAN_POINT('Ctrl Pts',(-9.63071094051081,-14.4659895814683,
118.991045032151)) ;
#173630 = CARTESIAN_POINT('Ctrl Pts',(-9.55101925277455,-14.5060552317741,
118.712756531787)) ;
#173631 = CARTESIAN_POINT('Ctrl Pts',(-9.4714813916173,-14.4677867862301,
118.435025022222)) ;
#173632 = CARTESIAN_POINT('Ctrl Pts',(-9.39862983053746,-14.3553856703914,
118.177844077314)) ;
#173633 = CARTESIAN_POINT('Ctrl Pts',(-9.33739442485482,-14.1738642018268,
117.955618487218)) ;
#173634 = CARTESIAN_POINT('Ctrl Pts',(-9.29429158603599,-13.9401973275635,
117.789022041494)) ;
#173635 = CARTESIAN_POINT('Ctrl Pts',(-9.27225194137694,-13.6684975496401,
117.686437026218)) ;
#173636 = CARTESIAN_POINT('Ctrl Pts',(-9.27379869131216,-13.3792258998284,
117.65575130022)) ;
#173637 = CARTESIAN_POINT('Ctrl Pts',(-9.29992444127897,-13.0905267308239,
117.699639537515)) ;
#173638 = CARTESIAN_POINT('Ctrl Pts',(-9.34881358143102,-12.8284630006125,
117.813282587224)) ;
#173639 = CARTESIAN_POINT('Ctrl Pts',(-9.41846234787993,-12.6065365051644,
117.989873611575)) ;
#173640 = CARTESIAN_POINT('Ctrl Pts',(-9.50417588053103,-12.4434900571409,
118.215497616744)) ;
#173641 = CARTESIAN_POINT('Ctrl Pts',(-9.60073723451511,-12.3500508502058,
118.474134121631)) ;
#173642 = CARTESIAN_POINT('Ctrl Pts',(-9.70194573753584,-12.3331953888952,
118.746927131276)) ;
#173643 = CARTESIAN_POINT('Ctrl Pts',(-9.80131762641198,-12.3940161187778,
119.014124252987)) ;
#173644 = CARTESIAN_POINT('Ctrl Pts',(-9.89248329484562,-12.5284976067023,
119.256301286483)) ;
#173645 = CARTESIAN_POINT('Ctrl Pts',(-9.9693440763676,-12.7253590046235,
119.455101779986)) ;
#173646 = CARTESIAN_POINT('Ctrl Pts',(-10.0281574646971,-12.9750336085797,
119.598466100957)) ;
#173647 = CARTESIAN_POINT('Ctrl Pts',(-10.0639625581,-13.2518773391213,119.672384712737)) ;
#173648 = CARTESIAN_POINT('Ctrl Pts',(-10.0762711870781,-13.5442043587849,
119.674255680769)) ;
#173649 = CARTESIAN_POINT('Ctrl Pts',(-10.0642632265541,-13.8259451748865,
119.602266518667)) ;
#173650 = CARTESIAN_POINT('Ctrl Pts',(-10.0296964583947,-14.0792480619856,
119.461456237366)) ;
#173651 = CARTESIAN_POINT('Ctrl Pts',(-9.97588775903519,-14.2845087011992,
119.262132122512)) ;
#173652 = CARTESIAN_POINT('Ctrl Pts',(-9.90744210014645,-14.4278905637469,
119.018229253178)) ;
#173653 = CARTESIAN_POINT('Ctrl Pts',(-9.82982242385163,-14.49909499359,118.746322529544)) ;
#173654 = CARTESIAN_POINT('Ctrl Pts',(-9.74956192660519,-14.492829252027,
118.466414353285)) ;
#173655 = CARTESIAN_POINT('Ctrl Pts',(-9.67283879350772,-14.4093444300335,
118.197174970448)) ;
#173656 = CARTESIAN_POINT('Ctrl Pts',(-9.60626579738372,-14.2544052422715,
117.958871810111)) ;
#173657 = CARTESIAN_POINT('Ctrl Pts',(-9.55553746479956,-14.0410991720381,
117.769068814144)) ;
#173658 = CARTESIAN_POINT('Ctrl Pts',(-9.52441285793816,-13.7816895970119,
117.638727760598)) ;
#173659 = CARTESIAN_POINT('Ctrl Pts',(-9.51628185017245,-13.4976199910735,
117.578613119079)) ;
#173660 = CARTESIAN_POINT('Ctrl Pts',(-9.53237212691088,-13.2063007087737,
117.592070626438)) ;
#173661 = CARTESIAN_POINT('Ctrl Pts',(-9.57232919510587,-12.9308185504047,
117.678310643569)) ;
#173662 = CARTESIAN_POINT('Ctrl Pts',(-9.634113078639,-12.690040453889,117.830986128613)) ;
#173663 = CARTESIAN_POINT('Ctrl Pts',(-9.713580692807,-12.5021903792694,118.037691814633)) ;
#173664 = CARTESIAN_POINT('Ctrl Pts',(-9.80659684966496,-12.3790435207342,
118.285471103814)) ;
#173665 = CARTESIAN_POINT('Ctrl Pts',(-9.90658661047469,-12.3305042760163,
118.554594905817)) ;
#173666 = CARTESIAN_POINT('Ctrl Pts',(-10.008066495342,-12.3604684800267,
118.827998813982)) ;
#173667 = CARTESIAN_POINT('Ctrl Pts',(-10.1026122259296,-12.4650891112354,
119.080754567184)) ;
#173668 = CARTESIAN_POINT('Ctrl Pts',(-10.1865625678926,-12.6397680496829,
119.300758559966)) ;
#173669 = CARTESIAN_POINT('Ctrl Pts',(-10.2525551850904,-12.8673926753431,
119.466570849935)) ;
#173670 = CARTESIAN_POINT('Ctrl Pts',(-10.2984413344148,-13.138383085188,
119.5705591487)) ;
#173671 = CARTESIAN_POINT('Ctrl Pts',(-10.3201874020919,-13.4250580301084,
119.601606079011)) ;
#173672 = CARTESIAN_POINT('Ctrl Pts',(-10.3180530372285,-13.713663843469,
119.559606091718)) ;
#173673 = CARTESIAN_POINT('Ctrl Pts',(-10.2921786001434,-13.9818996954329,
119.445166371893)) ;
#173674 = CARTESIAN_POINT('Ctrl Pts',(-10.245938215231,-14.2073240866329,
119.269059645356)) ;
#173675 = CARTESIAN_POINT('Ctrl Pts',(-10.1827043131007,-14.3779496982449,
119.040941067964)) ;
#173676 = CARTESIAN_POINT('Ctrl Pts',(-10.1079403524329,-14.4795452062324,
118.777702483988)) ;
#173677 = CARTESIAN_POINT('Ctrl Pts',(-10.0277788315133,-14.504675613756,
118.497994836855)) ;
#173678 = CARTESIAN_POINT('Ctrl Pts',(-9.94934961424335,-14.4524935600785,
118.223832977652)) ;
#173679 = CARTESIAN_POINT('Ctrl Pts',(-9.8776805943081,-14.3253673837965,
117.969892660447)) ;
#173680 = CARTESIAN_POINT('Ctrl Pts',(-9.81989105535084,-14.1335026343525,
117.758421157027)) ;
#173681 = CARTESIAN_POINT('Ctrl Pts',(-9.78045273451247,-13.8914689377216,
117.602957988204)) ;
#173682 = CARTESIAN_POINT('Ctrl Pts',(-9.76271568007487,-13.6147208150664,
117.513467417372)) ;
#173683 = CARTESIAN_POINT('Ctrl Pts',(-9.76890870119331,-13.3237687258409,
117.4968563122)) ;
#173684 = CARTESIAN_POINT('Ctrl Pts',(-9.79936071736111,-13.0396242352637,
117.554132453179)) ;
#173685 = CARTESIAN_POINT('Ctrl Pts',(-9.85239927743223,-12.7830678889279,
117.680294085095)) ;
#173686 = CARTESIAN_POINT('Ctrl Pts',(-9.9257847579806,-12.5704752635878,
117.868146840537)) ;
#173687 = CARTESIAN_POINT('Ctrl Pts',(-10.0135422022618,-12.4206416986158,
118.100172237485)) ;
#173688 = CARTESIAN_POINT('Ctrl Pts',(-10.1114862816905,-12.3408954926335,
118.363002383417)) ;
#173689 = CARTESIAN_POINT('Ctrl Pts',(-10.2131168846024,-12.3388375024718,
118.636985267721)) ;
#173690 = CARTESIAN_POINT('Ctrl Pts',(-10.3111631418804,-12.413706142133,
118.900239883285)) ;
#173691 = CARTESIAN_POINT('Ctrl Pts',(-10.4005037459975,-12.5617183582742,
119.136700846574)) ;
#173692 = CARTESIAN_POINT('Ctrl Pts',(-10.4738998219897,-12.7688407831079,
119.325034793762)) ;
#173693 = CARTESIAN_POINT('Ctrl Pts',(-10.528497781938,-13.0241117816514,
119.455791678547)) ;
#173694 = CARTESIAN_POINT('Ctrl Pts',(-10.5602307777131,-13.3070010234793,
119.517011250028)) ;
#173695 = CARTESIAN_POINT('Ctrl Pts',(-10.5678547390295,-13.5985554109386,
119.504704332823)) ;
#173696 = CARTESIAN_POINT('Ctrl Pts',(-10.5513598758863,-13.8770852609277,
119.418937728725)) ;
#173697 = CARTESIAN_POINT('Ctrl Pts',(-10.5130330103292,-14.1214182763711,
119.266862919213)) ;
#173698 = CARTESIAN_POINT('Ctrl Pts',(-10.4561208615973,-14.3164119676812,
119.058063869766)) ;
#173699 = CARTESIAN_POINT('Ctrl Pts',(-10.3852189870946,-14.4472714989735,
118.806537992562)) ;
#173700 = CARTESIAN_POINT('Ctrl Pts',(-10.3066385089528,-14.5039655219921,
118.531734459687)) ;
#173701 = CARTESIAN_POINT('Ctrl Pts',(-10.2263549450695,-14.4826373105238,
118.251644902637)) ;
#173702 = CARTESIAN_POINT('Ctrl Pts',(-10.1515928117172,-14.3855815012644,
117.988618093193)) ;
#173703 = CARTESIAN_POINT('Ctrl Pts',(-10.0875742094217,-14.2190969785884,
117.758158308275)) ;
#173704 = CARTESIAN_POINT('Ctrl Pts',(-10.0400271797391,-13.9949296481822,
117.577849034879)) ;
#173705 = CARTESIAN_POINT('Ctrl Pts',(-10.013089520595,-13.7298783707897,
117.46036854867)) ;
#173706 = CARTESIAN_POINT('Ctrl Pts',(-10.0095205229371,-13.4411780607526,
117.413901364897)) ;
#173707 = CARTESIAN_POINT('Ctrl Pts',(-10.0300438994439,-13.1535366585443,
117.441164670617)) ;
#173708 = CARTESIAN_POINT('Ctrl Pts',(-10.0745982760158,-12.8812078446008,
117.541146052817)) ;
#173709 = CARTESIAN_POINT('Ctrl Pts',(-10.1399166575301,-12.6502697095916,
117.704747539768)) ;
#173710 = CARTESIAN_POINT('Ctrl Pts',(-10.2222158366404,-12.4736381112203,
117.920071829275)) ;
#173711 = CARTESIAN_POINT('Ctrl Pts',(-10.3174784950143,-12.3636957343507,
118.174552893488)) ;
#173712 = CARTESIAN_POINT('Ctrl Pts',(-10.4179636590566,-12.3303161657527,
118.445239950958)) ;
#173713 = CARTESIAN_POINT('Ctrl Pts',(-10.5180970410555,-12.3741418831008,
118.71482587813)) ;
#173714 = CARTESIAN_POINT('Ctrl Pts',(-10.611946558723,-12.4937241519796,
118.965043678186)) ;
#173715 = CARTESIAN_POINT('Ctrl Pts',(-10.6922395149728,-12.6783961032596,
119.174263610413)) ;
#173716 = CARTESIAN_POINT('Ctrl Pts',(-10.7550368562695,-12.9163766433386,
119.330077430903)) ;
#173717 = CARTESIAN_POINT('Ctrl Pts',(-10.7962673301715,-13.1903758945546,
119.420199225543)) ;
#173718 = CARTESIAN_POINT('Ctrl Pts',(-10.8137492360295,-13.481432819081,
119.437894714578)) ;
#173719 = CARTESIAN_POINT('Ctrl Pts',(-10.8068277964098,-13.7673558416161,
119.38132985396)) ;
#173720 = CARTESIAN_POINT('Ctrl Pts',(-10.7770884508321,-14.0271101613543,
119.255429248926)) ;
#173721 = CARTESIAN_POINT('Ctrl Pts',(-10.7271574214564,-14.2445027860115,
119.067879150203)) ;
#173722 = CARTESIAN_POINT('Ctrl Pts',(-10.6612093802085,-14.4028029107363,
118.831466877353)) ;
#173723 = CARTESIAN_POINT('Ctrl Pts',(-10.5852730928227,-14.4900131921161,
118.564801583323)) ;
#173724 = CARTESIAN_POINT('Ctrl Pts',(-10.5049910429359,-14.5009049303826,
118.284799184651)) ;
#173725 = CARTESIAN_POINT('Ctrl Pts',(-10.4268806844919,-14.4337694493022,
118.011321719883)) ;
#173726 = CARTESIAN_POINT('Ctrl Pts',(-10.3576955154029,-14.2939322119372,
117.765123850201)) ;
#173727 = CARTESIAN_POINT('Ctrl Pts',(-10.3029320432203,-14.0911613446941,
117.562827612356)) ;
#173728 = CARTESIAN_POINT('Ctrl Pts',(-10.2673499177128,-13.8412394795533,
117.419099337292)) ;
#173729 = CARTESIAN_POINT('Ctrl Pts',(-10.254056072628,-13.5592605313859,
117.343020397243)) ;
#173730 = CARTESIAN_POINT('Ctrl Pts',(-10.2648180246204,-13.2696223387077,
117.34052655831)) ;
#173731 = CARTESIAN_POINT('Ctrl Pts',(-10.2997358790123,-12.9883139496615,
117.411316976137)) ;
#173732 = CARTESIAN_POINT('Ctrl Pts',(-10.3569669367904,-12.7386910562247,
117.550180832731)) ;
#173733 = CARTESIAN_POINT('Ctrl Pts',(-10.4331834431151,-12.5375785963018,
117.746852091262)) ;
#173734 = CARTESIAN_POINT('Ctrl Pts',(-10.5236752561247,-12.3995778757378,
117.98701193378)) ;
#173735 = CARTESIAN_POINT('Ctrl Pts',(-10.6227835579732,-12.3345174279643,
118.253393687995)) ;
#173736 = CARTESIAN_POINT('Ctrl Pts',(-10.7239238622889,-12.3471393395654,
118.526024465767)) ;
#173737 = CARTESIAN_POINT('Ctrl Pts',(-10.8207516399519,-12.4360428670471,
118.785542422515)) ;
#173738 = CARTESIAN_POINT('Ctrl Pts',(-10.9075644967453,-12.5962612233629,
119.014358156929)) ;
#173739 = CARTESIAN_POINT('Ctrl Pts',(-10.9778413211601,-12.8139558923281,
119.19307998567)) ;
#173740 = CARTESIAN_POINT('Ctrl Pts',(-11.0282836106079,-13.0756188660845,
119.311240887642)) ;
#173741 = CARTESIAN_POINT('Ctrl Pts',(-11.0555791922085,-13.3624251132735,
119.358838014228)) ;
#173742 = CARTESIAN_POINT('Ctrl Pts',(-11.0586048593759,-13.651982180129,
119.332672404455)) ;
#173743 = CARTESIAN_POINT('Ctrl Pts',(-11.0376843527776,-13.9268736432231,
119.23328044909)) ;
#173744 = CARTESIAN_POINT('Ctrl Pts',(-10.9956210330096,-14.1624927779437,
119.069898286994)) ;
#173745 = CARTESIAN_POINT('Ctrl Pts',(-10.9354933314548,-14.3467872124729,
118.851183898762)) ;
#173746 = CARTESIAN_POINT('Ctrl Pts',(-10.8629481065443,-14.4636106389172,
118.594821165369)) ;
#173747 = CARTESIAN_POINT('Ctrl Pts',(-10.7836225816458,-14.505904926533,
118.317753204467)) ;
#173748 = CARTESIAN_POINT('Ctrl Pts',(-10.7040268941245,-14.4703681622542,
118.039876785396)) ;
#173749 = CARTESIAN_POINT('Ctrl Pts',(-10.6303958446743,-14.359008640194,
117.780055371545)) ;
#173750 = CARTESIAN_POINT('Ctrl Pts',(-10.5692768535784,-14.1808823670753,
117.558510542006)) ;
#173751 = CARTESIAN_POINT('Ctrl Pts',(-10.525296106505,-13.9476582149858,
117.389059170047)) ;
#173752 = CARTESIAN_POINT('Ctrl Pts',(-10.5026217165176,-13.6767014389998,
117.284544765499)) ;
#173753 = CARTESIAN_POINT('Ctrl Pts',(-10.503514877856,-13.3872299120028,
117.251810399679)) ;
#173754 = CARTESIAN_POINT('Ctrl Pts',(-10.5287931159004,-13.0993467868879,
117.2932723904)) ;
#173755 = CARTESIAN_POINT('Ctrl Pts',(-10.5772819647789,-12.8349662721153,
117.405511188278)) ;
#173756 = CARTESIAN_POINT('Ctrl Pts',(-10.6462390061054,-12.6123125745559,
117.580099001699)) ;
#173757 = CARTESIAN_POINT('Ctrl Pts',(-10.7316789245276,-12.447065748415,
117.804830116923)) ;
#173758 = CARTESIAN_POINT('Ctrl Pts',(-10.8280555786512,-12.3516677675638,
118.062896940008)) ;
#173759 = CARTESIAN_POINT('Ctrl Pts',(-10.9289420861559,-12.3325934792249,
118.334805693187)) ;
#173760 = CARTESIAN_POINT('Ctrl Pts',(-11.0285549216706,-12.3910918553195,
118.602705295816)) ;
#173761 = CARTESIAN_POINT('Ctrl Pts',(-11.1202575355664,-12.5239274893633,
118.846436016608)) ;
#173762 = CARTESIAN_POINT('Ctrl Pts',(-11.1974790053523,-12.7192927751428,
119.046348283817)) ;
#173763 = CARTESIAN_POINT('Ctrl Pts',(-11.256570149613,-12.9658343070978,
119.190811409268)) ;
#173764 = CARTESIAN_POINT('Ctrl Pts',(-11.2934413311918,-13.2443245338218,
119.267674974483)) ;
#173765 = CARTESIAN_POINT('Ctrl Pts',(-11.3062978123674,-13.5367809605308,
119.271198329631)) ;
#173766 = CARTESIAN_POINT('Ctrl Pts',(-11.2949986489025,-13.8179726435299,
119.201501210985)) ;
#173767 = CARTESIAN_POINT('Ctrl Pts',(-11.2610571461274,-14.0724753431544,
119.062587049155)) ;
#173768 = CARTESIAN_POINT('Ctrl Pts',(-11.2078251507878,-14.279096140685,
118.865063933435)) ;
#173769 = CARTESIAN_POINT('Ctrl Pts',(-11.1396467770328,-14.4248617955916,
118.621919734993)) ;
#173770 = CARTESIAN_POINT('Ctrl Pts',(-11.0618371790876,-14.4982152843021,
118.349277506824)) ;
#173771 = CARTESIAN_POINT('Ctrl Pts',(-10.9820685755435,-14.4941260357652,
118.071094122751)) ;
#173772 = CARTESIAN_POINT('Ctrl Pts',(-10.9049115286395,-14.4126782343137,
117.800421801026)) ;
#173773 = CARTESIAN_POINT('Ctrl Pts',(-10.8381211251888,-14.2599648668114,
117.561542528994)) ;
#173774 = CARTESIAN_POINT('Ctrl Pts',(-10.7868067530969,-14.0478524029628,
117.369893536837)) ;
#173775 = CARTESIAN_POINT('Ctrl Pts',(-10.7550957653846,-13.7904112840523,
117.237886359139)) ;
#173776 = CARTESIAN_POINT('Ctrl Pts',(-10.7462257200646,-13.5044552055669,
117.175225916484)) ;
#173777 = CARTESIAN_POINT('Ctrl Pts',(-10.7617483985087,-13.2137879040768,
117.187050717025)) ;
#173778 = CARTESIAN_POINT('Ctrl Pts',(-10.8009076226651,-12.9385963486889,
117.270982185733)) ;
#173779 = CARTESIAN_POINT('Ctrl Pts',(-10.8619688891867,-12.6966955833364,
117.421502681034)) ;
#173780 = CARTESIAN_POINT('Ctrl Pts',(-10.9413222714456,-12.5064217313258,
117.627710657807)) ;
#173781 = CARTESIAN_POINT('Ctrl Pts',(-11.0338914556794,-12.3814205030376,
117.874194374824)) ;
#173782 = CARTESIAN_POINT('Ctrl Pts',(-11.1342884555144,-12.3309490204366,
118.144369386401)) ;
#173783 = CARTESIAN_POINT('Ctrl Pts',(-11.2344352101216,-12.3579787522632,
118.414220057428)) ;
#173784 = CARTESIAN_POINT('Ctrl Pts',(-11.3303750050126,-12.461461206882,
118.670792503069)) ;
#173785 = CARTESIAN_POINT('Ctrl Pts',(-11.4139998494669,-12.6327579824641,
118.890139759141)) ;
#173786 = CARTESIAN_POINT('Ctrl Pts',(-11.4811854191605,-12.8610649262646,
119.059239036713)) ;
#173787 = CARTESIAN_POINT('Ctrl Pts',(-11.5272358980316,-13.1282120035714,
119.164129227647)) ;
#173788 = CARTESIAN_POINT('Ctrl Pts',(-11.550031999704,-13.4170777357306,
119.198051643061)) ;
#173789 = CARTESIAN_POINT('Ctrl Pts',(-11.5484863559817,-13.7056413839055,
119.157890620187)) ;
#173790 = CARTESIAN_POINT('Ctrl Pts',(-11.5233022878553,-13.9747406301587,
119.04555969316)) ;
#173791 = CARTESIAN_POINT('Ctrl Pts',(-11.4774772491034,-14.201974810105,
118.870644857214)) ;
#173792 = CARTESIAN_POINT('Ctrl Pts',(-11.4147391200156,-14.3739130003505,
118.644102382187)) ;
#173793 = CARTESIAN_POINT('Ctrl Pts',(-11.3404625025784,-14.4775305035498,
118.382452018192)) ;
#173794 = CARTESIAN_POINT('Ctrl Pts',(-11.2600762837107,-14.5050608269986,
118.101928838668)) ;
#173795 = CARTESIAN_POINT('Ctrl Pts',(-11.1816706187826,-14.4551363613954,
117.827909095909)) ;
#173796 = CARTESIAN_POINT('Ctrl Pts',(-11.1096219883487,-14.3298705824412,
117.57276605832)) ;
#173797 = CARTESIAN_POINT('Ctrl Pts',(-11.0516186729526,-14.1407879039854,
117.36082074906)) ;
#173798 = CARTESIAN_POINT('Ctrl Pts',(-11.01133249899,-13.8991517087972,117.202620381188)) ;
#173799 = CARTESIAN_POINT('Ctrl Pts',(-10.9929531483878,-13.622377664187,
117.111093121158)) ;
#173800 = CARTESIAN_POINT('Ctrl Pts',(-10.9984700935864,-13.3324243748073,
117.092526186947)) ;
#173801 = CARTESIAN_POINT('Ctrl Pts',(-11.0281068838988,-13.0478498918573,
117.147341996027)) ;
#173802 = CARTESIAN_POINT('Ctrl Pts',(-11.081052628238,-12.7884262570381,
117.272939564718)) ;
#173803 = CARTESIAN_POINT('Ctrl Pts',(-11.1532846644103,-12.5764203972658,
117.457617573228)) ;
#173804 = CARTESIAN_POINT('Ctrl Pts',(-11.2410864798589,-12.4236100991773,
117.689588048581)) ;
#173805 = CARTESIAN_POINT('Ctrl Pts',(-11.3390837070061,-12.3419562515338,
117.95250976013)) ;
#173806 = CARTESIAN_POINT('Ctrl Pts',(-11.440496530574,-12.3379525743983,
118.225901103267)) ;
#173807 = CARTESIAN_POINT('Ctrl Pts',(-11.5383739159563,-12.4104778611719,
118.488760855449)) ;
#173808 = CARTESIAN_POINT('Ctrl Pts',(-11.6278480336845,-12.5557718304403,
118.725738663281)) ;
#173809 = CARTESIAN_POINT('Ctrl Pts',(-11.7021593126348,-12.7621800376528,
118.916687014316)) ;
#173810 = CARTESIAN_POINT('Ctrl Pts',(-11.7573807659036,-13.0168738808962,
119.049290511668)) ;
#173811 = CARTESIAN_POINT('Ctrl Pts',(-11.7896803869344,-13.2984278863564,
119.112337306604)) ;
#173812 = CARTESIAN_POINT('Ctrl Pts',(-11.7980400482597,-13.5897265030932,
119.102308017698)) ;
#173813 = CARTESIAN_POINT('Ctrl Pts',(-11.7822956103083,-13.8688372211758,
119.018847493834)) ;
#173814 = CARTESIAN_POINT('Ctrl Pts',(-11.7444566994981,-14.1152016754008,
118.868145849198)) ;
#173815 = CARTESIAN_POINT('Ctrl Pts',(-11.6880197549201,-14.3116011164225,
118.660817745576)) ;
#173816 = CARTESIAN_POINT('Ctrl Pts',(-11.6176369249549,-14.4442909382302,
118.410962690409)) ;
#173817 = CARTESIAN_POINT('Ctrl Pts',(-11.5390960272606,-14.5033545209173,
118.136228492371)) ;
#173818 = CARTESIAN_POINT('Ctrl Pts',(-11.4590251392824,-14.4845849990311,
117.856907062077)) ;
#173819 = CARTESIAN_POINT('Ctrl Pts',(-11.383664627329,-14.3894948595566,
117.591898604544)) ;
#173820 = CARTESIAN_POINT('Ctrl Pts',(-11.3191676650949,-14.2243477865837,
117.359917217915)) ;
#173821 = CARTESIAN_POINT('Ctrl Pts',(-11.2712397649004,-14.0022176408066,
117.178548503574)) ;
#173822 = CARTESIAN_POINT('Ctrl Pts',(-11.2436435716615,-13.738467096939,
117.059098820409)) ;
#173823 = CARTESIAN_POINT('Ctrl Pts',(-11.2393171495216,-13.4497089979361,
117.010273305457)) ;
#173824 = CARTESIAN_POINT('Ctrl Pts',(-11.2592549423813,-13.1612741016994,
117.035679695456)) ;
#173825 = CARTESIAN_POINT('Ctrl Pts',(-11.3028442445725,-12.8897094409154,
117.132937982061)) ;
#173826 = CARTESIAN_POINT('Ctrl Pts',(-11.3677649574765,-12.6562456914582,
117.295185497117)) ;
#173827 = CARTESIAN_POINT('Ctrl Pts',(-11.4498623668221,-12.4776727385034,
117.509821759606)) ;
#173828 = CARTESIAN_POINT('Ctrl Pts',(-11.5443175113425,-12.3662041520314,
117.762040087288)) ;
#173829 = CARTESIAN_POINT('Ctrl Pts',(-11.6448025118947,-12.3300379060018,
118.032692201155)) ;
#173830 = CARTESIAN_POINT('Ctrl Pts',(-11.7455128333517,-12.3719948524369,
118.303864829156)) ;
#173831 = CARTESIAN_POINT('Ctrl Pts',(-11.8390028851572,-12.4886302946211,
118.553235459183)) ;
#173832 = CARTESIAN_POINT('Ctrl Pts',(-11.9200724717719,-12.6716133926028,
118.764723942327)) ;
#173833 = CARTESIAN_POINT('Ctrl Pts',(-11.983729776495,-12.9096205473869,
118.922975846097)) ;
#173834 = CARTESIAN_POINT('Ctrl Pts',(-12.0254107822208,-13.1819739695916,
119.014592567458)) ;
#173835 = CARTESIAN_POINT('Ctrl Pts',(-12.0436296355972,-13.4720244815185,
119.034627026831)) ;
#173836 = CARTESIAN_POINT('Ctrl Pts',(-12.0374852966316,-13.7591219512168,
118.980348270067)) ;
#173837 = CARTESIAN_POINT('Ctrl Pts',(-12.0081585226799,-14.0209982570872,
118.855533677512)) ;
#173838 = CARTESIAN_POINT('Ctrl Pts',(-11.9589803424424,-14.2386408615737,
118.670464829268)) ;
#173839 = CARTESIAN_POINT('Ctrl Pts',(-11.8933789786321,-14.3991847031552,
118.435064542878)) ;
#173840 = CARTESIAN_POINT('Ctrl Pts',(-11.8176447978217,-14.4885294284138,
118.169014818533)) ;
#173841 = CARTESIAN_POINT('Ctrl Pts',(-11.7374057481524,-14.5016597743674,
117.889145533914)) ;
#173842 = CARTESIAN_POINT('Ctrl Pts',(-11.6592539148603,-14.437009415365,
117.615605436135)) ;
#173843 = CARTESIAN_POINT('Ctrl Pts',(-11.5896054471436,-14.2988734246617,
117.367922624978)) ;
#173844 = CARTESIAN_POINT('Ctrl Pts',(-11.5345577224684,-14.0989764690058,
117.164944532834)) ;
#173845 = CARTESIAN_POINT('Ctrl Pts',(-11.4980687401448,-13.8484694868484,
117.018190484838)) ;
#173846 = CARTESIAN_POINT('Ctrl Pts',(-11.484185252244,-13.5679794956402,
116.940440639052)) ;
#173847 = CARTESIAN_POINT('Ctrl Pts',(-11.4942413352023,-13.2778704302602,
116.935732247541)) ;
#173848 = CARTESIAN_POINT('Ctrl Pts',(-11.5283649580948,-12.9966579805532,
117.004198786349)) ;
#173849 = CARTESIAN_POINT('Ctrl Pts',(-11.5851655684408,-12.7449733317735,
117.141625652285)) ;
#173850 = CARTESIAN_POINT('Ctrl Pts',(-11.6608769322514,-12.5424420519023,
117.336783089927)) ;
#173851 = CARTESIAN_POINT('Ctrl Pts',(-11.751128641274,-12.4024494998622,
117.576178163021)) ;
#173852 = CARTESIAN_POINT('Ctrl Pts',(-11.849749431196,-12.33540698977,117.841192600071)) ;
#173853 = CARTESIAN_POINT('Ctrl Pts',(-11.9511794851965,-12.3455818235887,
118.114616538353)) ;
#173854 = CARTESIAN_POINT('Ctrl Pts',(-12.048568512048,-12.433061741337,118.375702938129)) ;
#173855 = CARTESIAN_POINT('Ctrl Pts',(-12.1352985452608,-12.5907670484714,
118.604444245422)) ;
#173856 = CARTESIAN_POINT('Ctrl Pts',(-12.2062338243243,-12.8072730343164,
118.785110454359)) ;
#173857 = CARTESIAN_POINT('Ctrl Pts',(-12.2572961681927,-13.0681776762317,
118.90514030015)) ;
#173858 = CARTESIAN_POINT('Ctrl Pts',(-12.2852469770119,-13.3550287065478,
118.954680417514)) ;
#173859 = CARTESIAN_POINT('Ctrl Pts',(-12.288870726614,-13.6436167217993,
118.930470264435)) ;
#173860 = CARTESIAN_POINT('Ctrl Pts',(-12.2688371151345,-13.9180811572707,
118.833953017997)) ;
#173861 = CARTESIAN_POINT('Ctrl Pts',(-12.2271646134758,-14.156549136634,
118.671552459278)) ;
#173862 = CARTESIAN_POINT('Ctrl Pts',(-12.1674566622439,-14.3423727651068,
118.454127809899)) ;
#173863 = CARTESIAN_POINT('Ctrl Pts',(-12.0952414310603,-14.4613427108393,
118.198784751216)) ;
#173864 = CARTESIAN_POINT('Ctrl Pts',(-12.0156536366213,-14.5057889124528,
117.920757945584)) ;
#173865 = CARTESIAN_POINT('Ctrl Pts',(-11.9363592364177,-14.4724226584541,
117.643968542152)) ;
#173866 = CARTESIAN_POINT('Ctrl Pts',(-11.8623371282566,-14.3630839653471,
117.382899183667)) ;
#173867 = CARTESIAN_POINT('Ctrl Pts',(-11.8008173863079,-14.1865023299291,
117.160124591948)) ;
#173868 = CARTESIAN_POINT('Ctrl Pts',(-11.7563748042704,-13.9552367476643,
116.989354134913)) ;
#173869 = CARTESIAN_POINT('Ctrl Pts',(-11.7329833978953,-13.6844063432408,
116.882563304078)) ;
#173870 = CARTESIAN_POINT('Ctrl Pts',(-11.7332475390205,-13.395616216205,
116.847967590773)) ;
#173871 = CARTESIAN_POINT('Ctrl Pts',(-11.7576801957441,-13.1080920804484,
116.886949996486)) ;
#173872 = CARTESIAN_POINT('Ctrl Pts',(-11.8057887216514,-12.8414911099526,
116.997851240026)) ;
#173873 = CARTESIAN_POINT('Ctrl Pts',(-11.8738646701692,-12.6185827250958,
117.169942474425)) ;
#173874 = CARTESIAN_POINT('Ctrl Pts',(-11.959020038101,-12.4509854490646,
117.393736018184)) ;
#173875 = CARTESIAN_POINT('Ctrl Pts',(-12.0550313167262,-12.3534810644787,
117.650738776618)) ;
#173876 = CARTESIAN_POINT('Ctrl Pts',(-12.1561839108002,-12.3320089256095,
117.923345972253)) ;
#173877 = CARTESIAN_POINT('Ctrl Pts',(-12.2558122040571,-12.3884256006082,
118.1913322941)) ;
#173878 = CARTESIAN_POINT('Ctrl Pts',(-12.3475394657345,-12.5185566369419,
118.43526353432)) ;
#173879 = CARTESIAN_POINT('Ctrl Pts',(-12.4255960408986,-12.7128146761132,
118.637581654736)) ;
#173880 = CARTESIAN_POINT('Ctrl Pts',(-12.4854118400066,-12.9591843124397,
118.784128401409)) ;
#173881 = CARTESIAN_POINT('Ctrl Pts',(-12.5227062774273,-13.2359003760254,
118.862430198041)) ;
#173882 = CARTESIAN_POINT('Ctrl Pts',(-12.5363357220994,-13.5269168879405,
118.86847314923)) ;
#173883 = CARTESIAN_POINT('Ctrl Pts',(-12.5257513802662,-13.8100818853549,
118.80078051953)) ;
#173884 = CARTESIAN_POINT('Ctrl Pts',(-12.4923757936398,-14.0658493622321,
118.663565106864)) ;
#173885 = CARTESIAN_POINT('Ctrl Pts',(-12.4395119409733,-14.2744004374724,
118.467090668042)) ;
#173886 = CARTESIAN_POINT('Ctrl Pts',(-12.371795140951,-14.4215076088756,
118.225429654782)) ;
#173887 = CARTESIAN_POINT('Ctrl Pts',(-12.2946403903294,-14.4970287487176,
117.954986337942)) ;
#173888 = CARTESIAN_POINT('Ctrl Pts',(-12.2142494904348,-14.495364180026,
117.674634887753)) ;
#173889 = CARTESIAN_POINT('Ctrl Pts',(-12.1371207254048,-14.4159600881982,
117.404140731358)) ;
#173890 = CARTESIAN_POINT('Ctrl Pts',(-12.0701819932153,-14.2660479877099,
117.164946413806)) ;
#173891 = CARTESIAN_POINT('Ctrl Pts',(-12.0180738968896,-14.0549162780305,
116.970748910434)) ;
#173892 = CARTESIAN_POINT('Ctrl Pts',(-11.9857272141969,-13.7973888984154,
116.836670452939)) ;
#173893 = CARTESIAN_POINT('Ctrl Pts',(-11.9762272551923,-13.5143192821472,
116.772389751235)) ;
#173894 = CARTESIAN_POINT('Ctrl Pts',(-11.9909277151902,-13.2228141005811,
116.78161966851)) ;
#173895 = CARTESIAN_POINT('Ctrl Pts',(-12.0294614824962,-12.9463122499942,
116.863581031885)) ;
#173896 = CARTESIAN_POINT('Ctrl Pts',(-12.0901776028958,-12.7025112775513,
117.012934916738)) ;
#173897 = CARTESIAN_POINT('Ctrl Pts',(-12.1687375174296,-12.5113386435153,
117.216879767183)) ;
#173898 = CARTESIAN_POINT('Ctrl Pts',(-12.2612290461381,-12.3839986409936,
117.463033125205)) ;
#173899 = CARTESIAN_POINT('Ctrl Pts',(-12.3609719875208,-12.3313598679509,
117.731405074504)) ;
#173900 = CARTESIAN_POINT('Ctrl Pts',(-12.4619148744611,-12.3561484752169,
118.003421771831)) ;
#173901 = CARTESIAN_POINT('Ctrl Pts',(-12.558035703025,-12.4578681360596,
118.260559283857)) ;
#173902 = CARTESIAN_POINT('Ctrl Pts',(-12.6418650591551,-12.6270814220524,
118.480600547495)) ;
#173903 = CARTESIAN_POINT('Ctrl Pts',(-12.709500616301,-12.8533401319523,
118.65115248197)) ;
#173904 = CARTESIAN_POINT('Ctrl Pts',(-12.7564269379405,-13.1210491167834,
118.758518890216)) ;
#173905 = CARTESIAN_POINT('Ctrl Pts',(-12.7797729830741,-13.40900770729,118.794199282391)) ;
#173906 = CARTESIAN_POINT('Ctrl Pts',(-12.7789054138412,-13.6972694862933,
118.756166722536)) ;
#173907 = CARTESIAN_POINT('Ctrl Pts',(-12.7545947470765,-13.9663054532962,
118.646647736907)) ;
#173908 = CARTESIAN_POINT('Ctrl Pts',(-12.708953623995,-14.1969043333081,
118.471990317947)) ;
#173909 = CARTESIAN_POINT('Ctrl Pts',(-12.6467531532713,-14.3698914257013,
118.24719675644)) ;
#173910 = CARTESIAN_POINT('Ctrl Pts',(-12.5727418641631,-14.4755193866787,
117.986353001203)) ;
#173911 = CARTESIAN_POINT('Ctrl Pts',(-12.4928027634597,-14.5054697818126,
117.707363787146)) ;
#173912 = CARTESIAN_POINT('Ctrl Pts',(-12.4137352350169,-14.4574393177702,
117.431077181479)) ;
#173913 = CARTESIAN_POINT('Ctrl Pts',(-12.3418324266654,-14.3349211938034,
117.176601530105)) ;
#173914 = CARTESIAN_POINT('Ctrl Pts',(-12.2830970975097,-14.1470800055845,
116.962290261975)) ;
#173915 = CARTESIAN_POINT('Ctrl Pts',(-12.2422554856577,-13.9065331674936,
116.80239048803)) ;
#173916 = CARTESIAN_POINT('Ctrl Pts',(-12.2232261811748,-13.630738678715,
116.708912567899)) ;
#173917 = CARTESIAN_POINT('Ctrl Pts',(-12.2280126456687,-13.3408270196336,
116.688112612688)) ;
#173918 = CARTESIAN_POINT('Ctrl Pts',(-12.2570791816381,-13.0553492265632,
116.741127681574)) ;
#173919 = CARTESIAN_POINT('Ctrl Pts',(-12.3090343418545,-12.7963986353394,
116.863927628217)) ;
#173920 = CARTESIAN_POINT('Ctrl Pts',(-12.3809755753915,-12.581755675213,
117.047570548939)) ;
#173921 = CARTESIAN_POINT('Ctrl Pts',(-12.4684134110327,-12.4271874700909,
117.278442488482)) ;
#173922 = CARTESIAN_POINT('Ctrl Pts',(-12.5658597005341,-12.3434882644401,
117.539803720469)) ;
#173923 = CARTESIAN_POINT('Ctrl Pts',(-12.6672936908425,-12.3367187774922,
117.813250325772)) ;
#173924 = CARTESIAN_POINT('Ctrl Pts',(-12.765948884936,-12.4076100218016,
118.078256939231)) ;
#173925 = CARTESIAN_POINT('Ctrl Pts',(-12.8553355026567,-12.5503272886106,
118.315139856333)) ;
#173926 = CARTESIAN_POINT('Ctrl Pts',(-12.9304176070875,-12.7556871760659,
118.508319195545)) ;
#173927 = CARTESIAN_POINT('Ctrl Pts',(-12.9861723417227,-13.0091921750313,
118.642571963292)) ;
#173928 = CARTESIAN_POINT('Ctrl Pts',(-13.0191734609878,-13.2902503547293,
118.707745845769)) ;
#173929 = CARTESIAN_POINT('Ctrl Pts',(-13.028209715569,-13.5823834440121,
118.699683255514)) ;
#173930 = CARTESIAN_POINT('Ctrl Pts',(-13.0130366717192,-13.8618181146796,
118.617988137292)) ;
#173931 = CARTESIAN_POINT('Ctrl Pts',(-12.9759659852745,-14.1083106024044,
118.469780251358)) ;
#173932 = CARTESIAN_POINT('Ctrl Pts',(-12.9198792403032,-14.3070623418306,
118.263416505571)) ;
#173933 = CARTESIAN_POINT('Ctrl Pts',(-12.849560606782,-14.4418892785907,
118.013651989613)) ;
#173934 = CARTESIAN_POINT('Ctrl Pts',(-12.7712938037721,-14.502692884587,
117.739819479159)) ;
#173935 = CARTESIAN_POINT('Ctrl Pts',(-12.691443150556,-14.4862255258319,
117.461283982672)) ;
#173936 = CARTESIAN_POINT('Ctrl Pts',(-12.6158746315244,-14.3934141564473,
117.195652815533)) ;
#173937 = CARTESIAN_POINT('Ctrl Pts',(-12.5509163096876,-14.2302607448999,
116.962257398382)) ;
#173938 = CARTESIAN_POINT('Ctrl Pts',(-12.5022332898898,-14.0081666908763,
116.778385267356)) ;
#173939 = CARTESIAN_POINT('Ctrl Pts',(-12.4742506823548,-13.7466548362381,
116.657950049822)) ;
#173940 = CARTESIAN_POINT('Ctrl Pts',(-12.4691100549571,-13.4587847124533,
116.606699386214)) ;
#173941 = CARTESIAN_POINT('Ctrl Pts',(-12.4885192361608,-13.1685102080527,
116.630294437279)) ;
#173942 = CARTESIAN_POINT('Ctrl Pts',(-12.5312093541707,-12.8978336872395,
116.725034238603)) ;
#173943 = CARTESIAN_POINT('Ctrl Pts',(-12.5957395733222,-12.6619537350285,
116.885954892402)) ;
#173944 = CARTESIAN_POINT('Ctrl Pts',(-12.6776143419512,-12.4816257056073,
117.099854766256)) ;
#173945 = CARTESIAN_POINT('Ctrl Pts',(-12.7713529617644,-12.3684889471066,
117.350055385643)) ;
#173946 = CARTESIAN_POINT('Ctrl Pts',(-12.8723202400041,-12.3299903879882,
117.621972650026)) ;
#173947 = CARTESIAN_POINT('Ctrl Pts',(-12.9724385289638,-12.3696139932957,
117.891584408557)) ;
#173948 = CARTESIAN_POINT('Ctrl Pts',(-13.0664515487238,-12.4839372794238,
118.142479880966)) ;
#173949 = CARTESIAN_POINT('Ctrl Pts',(-13.1484405032608,-12.6667316342934,
118.356525775525)) ;
#173950 = CARTESIAN_POINT('Ctrl Pts',(-13.2121850011556,-12.9020313562946,
118.515277498017)) ;
#173951 = CARTESIAN_POINT('Ctrl Pts',(-13.2546371352095,-13.1740426154344,
118.609174623203)) ;
#173952 = CARTESIAN_POINT('Ctrl Pts',(-13.2734900958146,-13.4634545824485,
118.631199247328)) ;
#173953 = CARTESIAN_POINT('Ctrl Pts',(-13.2680796257058,-13.7505708131454,
118.579201045788)) ;
#173954 = CARTESIAN_POINT('Ctrl Pts',(-13.2394962360415,-14.0133363300327,
118.456684613439)) ;
#173955 = CARTESIAN_POINT('Ctrl Pts',(-13.1905999974754,-14.2335678065818,
118.272293478368)) ;
#173956 = CARTESIAN_POINT('Ctrl Pts',(-13.1253712311633,-14.3958087768564,
118.038043104771)) ;
#173957 = CARTESIAN_POINT('Ctrl Pts',(-13.0496091296525,-14.4872051600084,
117.771802663667)) ;
#173958 = CARTESIAN_POINT('Ctrl Pts',(-12.9697977471393,-14.5023836342265,
117.493417412762)) ;
#173959 = CARTESIAN_POINT('Ctrl Pts',(-12.8911729784752,-14.4395233841403,
117.218279983479)) ;
#173960 = CARTESIAN_POINT('Ctrl Pts',(-12.8215722521092,-14.3038981389521,
116.970926660863)) ;
#173961 = CARTESIAN_POINT('Ctrl Pts',(-12.765908924504,-14.1052991872385,
116.765996341192)) ;
#173962 = CARTESIAN_POINT('Ctrl Pts',(-12.7289194558588,-13.8563431079666,
116.617783489361)) ;
#173963 = CARTESIAN_POINT('Ctrl Pts',(-12.7143046569284,-13.5768529523028,
116.537845772707)) ;
#173964 = CARTESIAN_POINT('Ctrl Pts',(-12.7237017190187,-13.2855121533732,
116.530980294664)) ;
#173965 = CARTESIAN_POINT('Ctrl Pts',(-12.7572168622974,-13.0041275578471,
116.597631042541)) ;
#173966 = CARTESIAN_POINT('Ctrl Pts',(-12.8130794083186,-12.7524010633512,
116.732371814801)) ;
#173967 = CARTESIAN_POINT('Ctrl Pts',(-12.88854761512,-12.5474082659178,116.92665451824)) ;
#173968 = CARTESIAN_POINT('Ctrl Pts',(-12.9782123177536,-12.4057612857423,
117.164359360981)) ;
#173969 = CARTESIAN_POINT('Ctrl Pts',(-13.0770064791105,-12.3361751661113,
117.429775138385)) ;
#173970 = CARTESIAN_POINT('Ctrl Pts',(-13.1783190413846,-12.3442704255669,
117.702890794258)) ;
#173971 = CARTESIAN_POINT('Ctrl Pts',(-13.2756527267231,-12.4291570429794,
117.963909021848)) ;
#173972 = CARTESIAN_POINT('Ctrl Pts',(-13.36292678935,-12.5849331529663,118.194259899517)) ;
#173973 = CARTESIAN_POINT('Ctrl Pts',(-13.4345794652228,-12.8005108515807,
118.377018028647)) ;
#173974 = CARTESIAN_POINT('Ctrl Pts',(-13.4861674949149,-13.060269126664,
118.498676029101)) ;
#173975 = CARTESIAN_POINT('Ctrl Pts',(-13.5147933718825,-13.3453693583979,
118.550429429881)) ;
#173976 = CARTESIAN_POINT('Ctrl Pts',(-13.5191703640909,-13.6361640667827,
118.528261672456)) ;
#173977 = CARTESIAN_POINT('Ctrl Pts',(-13.4997846887976,-13.9104324089111,
118.433833737107)) ;
#173978 = CARTESIAN_POINT('Ctrl Pts',(-13.4587413574297,-14.1501784561149,
118.27335686083)) ;
#173979 = CARTESIAN_POINT('Ctrl Pts',(-13.39950930923,-14.3377944456025,118.057390334685)) ;
#173980 = CARTESIAN_POINT('Ctrl Pts',(-13.32749153125,-14.4588735568458,117.802602901111)) ;
#173981 = CARTESIAN_POINT('Ctrl Pts',(-13.2483458924945,-14.5056122473976,
117.526071610546)) ;
#173982 = CARTESIAN_POINT('Ctrl Pts',(-13.1685437749415,-14.4743736272664,
117.247539732196)) ;
#173983 = CARTESIAN_POINT('Ctrl Pts',(-13.0946020226361,-14.3676054099568,
116.986884001878)) ;
#173984 = CARTESIAN_POINT('Ctrl Pts',(-13.0324910029511,-14.1926642104704,
116.762231273457)) ;
#173985 = CARTESIAN_POINT('Ctrl Pts',(-12.9874746142067,-13.9629645552833,
116.589736773677)) ;
#173986 = CARTESIAN_POINT('Ctrl Pts',(-12.9633562559811,-13.6916669453695,
116.48056065792)) ;
#173987 = CARTESIAN_POINT('Ctrl Pts',(-12.9629691653421,-13.4042886281479,
116.444129256868)) ;
#173988 = CARTESIAN_POINT('Ctrl Pts',(-12.9867239596031,-13.1160881842174,
116.481000353099)) ;
#173989 = CARTESIAN_POINT('Ctrl Pts',(-13.0339690435015,-12.8495738757798,
116.589413701142)) ;
#173990 = CARTESIAN_POINT('Ctrl Pts',(-13.1016362988514,-12.6242652876755,
116.76014561289)) ;
#173991 = CARTESIAN_POINT('Ctrl Pts',(-13.1868381515301,-12.4543477917217,
116.98391806025)) ;
#173992 = CARTESIAN_POINT('Ctrl Pts',(-13.282130994495,-12.3553371823295,
117.238917231087)) ;
#173993 = CARTESIAN_POINT('Ctrl Pts',(-13.3835527278556,-12.3315537600446,
117.512226746283)) ;
#173994 = CARTESIAN_POINT('Ctrl Pts',(-13.4828912406925,-12.3856473127391,
117.779479511165)) ;
#173995 = CARTESIAN_POINT('Ctrl Pts',(-13.5751280064643,-12.513656004823,
118.024906933845)) ;
#173996 = CARTESIAN_POINT('Ctrl Pts',(-13.6539134068514,-12.707439556573,
118.229281918463)) ;
#173997 = CARTESIAN_POINT('Ctrl Pts',(-13.7137234776106,-12.9500051005904,
118.376179984501)) ;
#173998 = CARTESIAN_POINT('Ctrl Pts',(-13.7520689708624,-13.2274462581565,
118.457479335507)) ;
#173999 = CARTESIAN_POINT('Ctrl Pts',(-13.7663393260749,-13.5192262317475,
118.465377287378)) ;
#174000 = CARTESIAN_POINT('Ctrl Pts',(-13.7564573176797,-13.8018769048648,
118.399949096535)) ;
#174001 = CARTESIAN_POINT('Ctrl Pts',(-13.7237468055255,-14.058784271986,
118.264759363062)) ;
#174002 = CARTESIAN_POINT('Ctrl Pts',(-13.6714025576082,-14.2690401451517,
118.069862285334)) ;
#174003 = CARTESIAN_POINT('Ctrl Pts',(-13.6038901489006,-14.418345814643,
117.828744781992)) ;
#174004 = CARTESIAN_POINT('Ctrl Pts',(-13.5270066699605,-14.4960013207205,
117.559173432525)) ;
#174005 = CARTESIAN_POINT('Ctrl Pts',(-13.4463172125483,-14.4962457299704,
117.277772265082)) ;
#174006 = CARTESIAN_POINT('Ctrl Pts',(-13.3696988473351,-14.4198799151553,
117.009166760654)) ;
#174007 = CARTESIAN_POINT('Ctrl Pts',(-13.3017866089322,-14.2709014086462,
116.76670550127)) ;
#174008 = CARTESIAN_POINT('Ctrl Pts',(-13.2493889815294,-14.0614284920593,
116.571702252918)) ;
#174009 = CARTESIAN_POINT('Ctrl Pts',(-13.2164243628667,-13.8059370930909,
116.435853274894)) ;
#174010 = CARTESIAN_POINT('Ctrl Pts',(-13.2062477246467,-13.5211628984478,
116.369237660814)) ;
#174011 = CARTESIAN_POINT('Ctrl Pts',(-13.2201829843462,-13.2317212421624,
116.376408413708)) ;
#174012 = CARTESIAN_POINT('Ctrl Pts',(-13.2582351273943,-12.953209842425,
116.456720631326)) ;
#174013 = CARTESIAN_POINT('Ctrl Pts',(-13.3179987777289,-12.7094642616823,
116.60338316649)) ;
#174014 = CARTESIAN_POINT('Ctrl Pts',(-13.3968395702768,-12.5150572905195,
116.807856696789)) ;
#174015 = CARTESIAN_POINT('Ctrl Pts',(-13.4880657336334,-12.3871819681861,
117.050541251165)) ;
#174016 = CARTESIAN_POINT('Ctrl Pts',(-13.5882207279045,-12.3316884564228,
117.319958997263)) ;
#174017 = CARTESIAN_POINT('Ctrl Pts',(-13.6888941607603,-12.3542922095437,
117.591275254107)) ;
#174018 = CARTESIAN_POINT('Ctrl Pts',(-13.7853698113562,-12.4537268763868,
117.849457635997)) ;
#174019 = CARTESIAN_POINT('Ctrl Pts',(-13.8696982601704,-12.6212675456056,
118.070986029358)) ;
#174020 = CARTESIAN_POINT('Ctrl Pts',(-13.9378798134609,-12.846192059173,
118.243189707452)) ;
#174021 = CARTESIAN_POINT('Ctrl Pts',(-13.9854016724836,-13.1124184461725,
118.352441492381)) ;
#174022 = CARTESIAN_POINT('Ctrl Pts',(-14.0095130072085,-13.400879749144,
118.390345126407)) ;
#174023 = CARTESIAN_POINT('Ctrl Pts',(-14.0093724892591,-13.6891262166377,
118.354574264124)) ;
#174024 = CARTESIAN_POINT('Ctrl Pts',(-13.985414910218,-13.9605413879786,
118.245894494186)) ;
#174025 = CARTESIAN_POINT('Ctrl Pts',(-13.9409451108123,-14.1894540736428,
118.075288407443)) ;
#174026 = CARTESIAN_POINT('Ctrl Pts',(-13.8788030525502,-14.3660067048925,
117.850395877402)) ;
#174027 = CARTESIAN_POINT('Ctrl Pts',(-13.805049295041,-14.4734792612079,
117.590360278057)) ;
#174028 = CARTESIAN_POINT('Ctrl Pts',(-13.7251059804211,-14.5056975632985,
117.311316857951)) ;
#174029 = CARTESIAN_POINT('Ctrl Pts',(-13.6460687434891,-14.4599236721213,
117.035189019244)) ;
#174030 = CARTESIAN_POINT('Ctrl Pts',(-13.5738853047407,-14.3395761921465,
116.779866121718)) ;
#174031 = CARTESIAN_POINT('Ctrl Pts',(-13.5146382184193,-14.1535350418836,
116.563988746602)) ;
#174032 = CARTESIAN_POINT('Ctrl Pts',(-13.4731069605417,-13.9130985111844,
116.401832242531)) ;
#174033 = CARTESIAN_POINT('Ctrl Pts',(-13.4535360973529,-13.6395736822347,
116.306908957539)) ;
#174034 = CARTESIAN_POINT('Ctrl Pts',(-13.4576157743933,-13.3487006076146,
116.283814176628)) ;
#174035 = CARTESIAN_POINT('Ctrl Pts',(-13.4859406302875,-13.0636371844073,
116.334679965118)) ;
#174036 = CARTESIAN_POINT('Ctrl Pts',(-13.537302484578,-12.803286823163,116.455624512449)) ;
#174037 = CARTESIAN_POINT('Ctrl Pts',(-13.6086911430819,-12.5872505028287,
116.637604570861)) ;
#174038 = CARTESIAN_POINT('Ctrl Pts',(-13.6958832608641,-12.4304809457012,
116.867672531912)) ;
#174039 = CARTESIAN_POINT('Ctrl Pts',(-13.7933144950255,-12.3447676693836,
117.128927982332)) ;
#174040 = CARTESIAN_POINT('Ctrl Pts',(-13.8942106173158,-12.3358385329225,
117.400917482378)) ;
#174041 = CARTESIAN_POINT('Ctrl Pts',(-13.9931058830893,-12.4042599768703,
117.666636589428)) ;
#174042 = CARTESIAN_POINT('Ctrl Pts',(-14.0830802598219,-12.5454038835963,
117.905215825566)) ;
#174043 = CARTESIAN_POINT('Ctrl Pts',(-14.1585388443987,-12.7490645526663,
118.099576579279)) ;
#174044 = CARTESIAN_POINT('Ctrl Pts',(-14.2147792241185,-13.0004109945635,
118.235435558541)) ;
#174045 = CARTESIAN_POINT('Ctrl Pts',(-14.2486273894212,-13.281956740539,
118.303050309436)) ;
#174046 = CARTESIAN_POINT('Ctrl Pts',(-14.2583346166308,-13.573019683806,
118.297166121252)) ;
#174047 = CARTESIAN_POINT('Ctrl Pts',(-14.2439797697,-13.8532505028034,118.217957846964)) ;
#174048 = CARTESIAN_POINT('Ctrl Pts',(-14.2073259241701,-14.1021597581384,
118.070845549194)) ;
#174049 = CARTESIAN_POINT('Ctrl Pts',(-14.1518319080389,-14.3018608409922,
117.866383830764)) ;
#174050 = CARTESIAN_POINT('Ctrl Pts',(-14.0821691837154,-14.4384983198451,
117.618753194085)) ;
#174051 = CARTESIAN_POINT('Ctrl Pts',(-14.0038053646086,-14.5020770602936,
117.344502812886)) ;
#174052 = CARTESIAN_POINT('Ctrl Pts',(-13.9237302084394,-14.48777877411,117.065203884427)) ;
#174053 = CARTESIAN_POINT('Ctrl Pts',(-13.8479693987333,-14.3970097456745,
116.798993617263)) ;
#174054 = CARTESIAN_POINT('Ctrl Pts',(-13.782799826033,-14.2362612997962,
116.5650573821)) ;
#174055 = CARTESIAN_POINT('Ctrl Pts',(-13.733518100292,-14.0159101115065,
116.379369583749)) ;
#174056 = CARTESIAN_POINT('Ctrl Pts',(-13.7047590259111,-13.7543350935969,
116.256429298379)) ;
#174057 = CARTESIAN_POINT('Ctrl Pts',(-13.699032750653,-13.4665595551094,
116.203361929234)) ;
#174058 = CARTESIAN_POINT('Ctrl Pts',(-13.7175768117472,-13.1776643244991,
116.224521765399)) ;
#174059 = CARTESIAN_POINT('Ctrl Pts',(-13.7598364090687,-12.90467088677,116.317749177515)) ;
#174060 = CARTESIAN_POINT('Ctrl Pts',(-13.8234518415385,-12.6688603640825,
116.476089051097)) ;
#174061 = CARTESIAN_POINT('Ctrl Pts',(-13.9049557333608,-12.48602188738,116.688787580776)) ;
#174062 = CARTESIAN_POINT('Ctrl Pts',(-13.9989576689692,-12.3704601308902,
116.939602004027)) ;
#174063 = CARTESIAN_POINT('Ctrl Pts',(-14.0992273955684,-12.3301504850153,
117.209607062401)) ;
#174064 = CARTESIAN_POINT('Ctrl Pts',(-14.1995620772837,-12.3670848663884,
117.479845083354)) ;
#174065 = CARTESIAN_POINT('Ctrl Pts',(-14.2945308343906,-12.4806961242678,
117.733368848111)) ;
#174066 = CARTESIAN_POINT('Ctrl Pts',(-14.3760228392886,-12.659847054779,
117.946296624332)) ;
#174067 = CARTESIAN_POINT('Ctrl Pts',(-14.4406901314542,-12.8944266812495,
118.107719161995)) ;
#174068 = CARTESIAN_POINT('Ctrl Pts',(-14.4837690484985,-13.1656332510844,
118.203535687924)) ;
#174069 = CARTESIAN_POINT('Ctrl Pts',(-14.5033674776862,-13.455130793988,
118.227791066086)) ;
#174070 = CARTESIAN_POINT('Ctrl Pts',(-14.4986092754277,-13.7427936624919,
118.177758141915)) ;
#174071 = CARTESIAN_POINT('Ctrl Pts',(-14.4707221810934,-14.0059776158613,
118.057435006683)) ;
#174072 = CARTESIAN_POINT('Ctrl Pts',(-14.422360755841,-14.2279037819529,
117.874652010575)) ;
#174073 = CARTESIAN_POINT('Ctrl Pts',(-14.3575106947756,-14.3919406672911,
117.641551257708)) ;
#174074 = CARTESIAN_POINT('Ctrl Pts',(-14.2822303298045,-14.4855253459423,
117.376890300863)) ;
#174075 = CARTESIAN_POINT('Ctrl Pts',(-14.2019505143216,-14.5029122651219,
117.09684616291)) ;
#174076 = CARTESIAN_POINT('Ctrl Pts',(-14.1238906002577,-14.4429567945224,
116.823764513881)) ;
#174077 = CARTESIAN_POINT('Ctrl Pts',(-14.0534400115056,-14.3088313127917,
116.573580387455)) ;
#174078 = CARTESIAN_POINT('Ctrl Pts',(-13.9973344587926,-14.1118280044828,
116.36732016952)) ;
#174079 = CARTESIAN_POINT('Ctrl Pts',(-13.9596840563562,-13.8633524569287,
116.216996890361)) ;
#174080 = CARTESIAN_POINT('Ctrl Pts',(-13.9444872281656,-13.5856086171591,
116.135434675017)) ;
#174081 = CARTESIAN_POINT('Ctrl Pts',(-13.9531206776375,-13.29429050433,116.126236655127)) ;
#174082 = CARTESIAN_POINT('Ctrl Pts',(-13.9859156053883,-13.0122145331766,
116.19068657179)) ;
#174083 = CARTESIAN_POINT('Ctrl Pts',(-14.0414265852797,-12.7583429519339,
116.324206721183)) ;
#174084 = CARTESIAN_POINT('Ctrl Pts',(-14.1163566701285,-12.5522896132778,
116.516904433369)) ;
#174085 = CARTESIAN_POINT('Ctrl Pts',(-14.2054208500919,-12.4090180636989,
116.75287655481)) ;
#174086 = CARTESIAN_POINT('Ctrl Pts',(-14.3041315741692,-12.3371174607651,
117.018003366661)) ;
#174087 = CARTESIAN_POINT('Ctrl Pts',(-14.4053499510961,-12.3428658905722,
117.290874128105)) ;
#174088 = CARTESIAN_POINT('Ctrl Pts',(-14.5030362331871,-12.4257351119528,
117.55290734156)) ;
#174089 = CARTESIAN_POINT('Ctrl Pts',(-14.5904621270827,-12.5790185234623,
117.783826332769)) ;
#174090 = CARTESIAN_POINT('Ctrl Pts',(-14.6629652552051,-12.7940406828703,
117.969008479269)) ;
#174091 = CARTESIAN_POINT('Ctrl Pts',(-14.7149782729242,-13.0518842131347,
118.092091883262)) ;
#174092 = CARTESIAN_POINT('Ctrl Pts',(-14.7443671066665,-13.3370763555055,
118.146092536195)) ;
#174093 = CARTESIAN_POINT('Ctrl Pts',(-14.7494764883566,-13.6270297095458,
118.126281327732)) ;
#174094 = CARTESIAN_POINT('Ctrl Pts',(-14.7306708206297,-13.9038567932623,
118.033390708072)) ;
#174095 = CARTESIAN_POINT('Ctrl Pts',(-14.690027558541,-14.1447030861545,
117.874109045323)) ;
#174096 = CARTESIAN_POINT('Ctrl Pts',(-14.6316472186503,-14.332817774621,
117.660971076182)) ;
#174097 = CARTESIAN_POINT('Ctrl Pts',(-14.5597455784243,-14.45646682902,117.406433016193)) ;
#174098 = CARTESIAN_POINT('Ctrl Pts',(-14.4807629365922,-14.5053560860543,
117.130424369544)) ;
#174099 = CARTESIAN_POINT('Ctrl Pts',(-14.4006764355962,-14.4762759602464,
116.850932976369)) ;
#174100 = CARTESIAN_POINT('Ctrl Pts',(-14.3265390078925,-14.3712943997113,
116.589686458049)) ;
#174101 = CARTESIAN_POINT('Ctrl Pts',(-14.2642291252365,-14.1990455522355,
116.364581017991)) ;
#174102 = CARTESIAN_POINT('Ctrl Pts',(-14.2184481514674,-13.969268231171,
116.189542795207)) ;
#174103 = CARTESIAN_POINT('Ctrl Pts',(-14.1938561787033,-13.7012052922517,
116.079239578809)) ;
#174104 = CARTESIAN_POINT('Ctrl Pts',(-14.1927076708075,-13.4115854195081,
116.040169663763)) ;
#174105 = CARTESIAN_POINT('Ctrl Pts',(-14.2158186831131,-13.1240520278943,
116.075200920001)) ;
#174106 = CARTESIAN_POINT('Ctrl Pts',(-14.2623847117566,-12.8565945311091,
116.181543563239)) ;
#174107 = CARTESIAN_POINT('Ctrl Pts',(-14.3295805648497,-12.6299321000607,
116.350826699486)) ;
#174108 = CARTESIAN_POINT('Ctrl Pts',(-14.4139535876279,-12.458754218581,
116.572235100756)) ;
#174109 = CARTESIAN_POINT('Ctrl Pts',(-14.5094836498744,-12.3569969390507,
116.827772100287)) ;
#174110 = CARTESIAN_POINT('Ctrl Pts',(-14.6106904064239,-12.3311725454961,
117.10048536176)) ;
#174111 = CARTESIAN_POINT('Ctrl Pts',(-14.7103650458112,-12.3830921654557,
117.368691273652)) ;
#174112 = CARTESIAN_POINT('Ctrl Pts',(-14.8029787361383,-12.5097082549453,
117.615209351864)) ;
#174113 = CARTESIAN_POINT('Ctrl Pts',(-14.8815949767115,-12.6999655173835,
117.819379893254)) ;
#174114 = CARTESIAN_POINT('Ctrl Pts',(-14.9425172204992,-12.9431519741363,
117.969375033027)) ;
#174115 = CARTESIAN_POINT('Ctrl Pts',(-14.9812992054159,-13.2187420743147,
118.052168315938)) ;
#174116 = CARTESIAN_POINT('Ctrl Pts',(-14.9963500333539,-13.5111774969548,
118.062342681364)) ;
#174117 = CARTESIAN_POINT('Ctrl Pts',(-14.9871457345053,-13.7940494918521,
117.999019373326)) ;
#174118 = CARTESIAN_POINT('Ctrl Pts',(-14.9548742901699,-14.0529110285333,
117.865026253004)) ;
#174119 = CARTESIAN_POINT('Ctrl Pts',(-14.9032500009219,-14.2634870650102,
117.672503574574)) ;
#174120 = CARTESIAN_POINT('Ctrl Pts',(-14.8361924144871,-14.4148461022599,
117.432794192959)) ;
#174121 = CARTESIAN_POINT('Ctrl Pts',(-14.7594134311292,-14.494780073978,
117.16350011444)) ;
#174122 = CARTESIAN_POINT('Ctrl Pts',(-14.6788165394104,-14.4974507314962,
116.882424493313)) ;
#174123 = CARTESIAN_POINT('Ctrl Pts',(-14.6018098242213,-14.4229495346006,
116.612531368624)) ;
#174124 = CARTESIAN_POINT('Ctrl Pts',(-14.5338249366433,-14.2768020033666,
116.370022693878)) ;
#174125 = CARTESIAN_POINT('Ctrl Pts',(-14.4805103340185,-14.0672719747909,
116.171945276152)) ;
#174126 = CARTESIAN_POINT('Ctrl Pts',(-14.4472092133991,-13.8140437794069,
116.035263380737)) ;
#174127 = CARTESIAN_POINT('Ctrl Pts',(-14.4362486432515,-13.5305545368903,
115.96633944488)) ;
#174128 = CARTESIAN_POINT('Ctrl Pts',(-14.449486240473,-13.2400469135056,
115.971266296655)) ;
#174129 = CARTESIAN_POINT('Ctrl Pts',(-14.4868824566312,-12.9607801917685,
116.04957346963)) ;
#174130 = CARTESIAN_POINT('Ctrl Pts',(-14.5461400633249,-12.7157522020321,
116.194666581357)) ;
#174131 = CARTESIAN_POINT('Ctrl Pts',(-14.6240444846692,-12.5205021117526,
116.396478689841)) ;
#174132 = CARTESIAN_POINT('Ctrl Pts',(-14.7155078962198,-12.3896091910669,
116.639659815513)) ;
#174133 = CARTESIAN_POINT('Ctrl Pts',(-14.8155283401331,-12.3322116649338,
116.908678402663)) ;
#174134 = CARTESIAN_POINT('Ctrl Pts',(-14.9160696924354,-12.3526193896652,
117.179651593861)) ;
#174135 = CARTESIAN_POINT('Ctrl Pts',(-15.0126074976825,-12.4495335034968,
117.438097138294)) ;
#174136 = CARTESIAN_POINT('Ctrl Pts',(-15.0977303726993,-12.6159519111974,
117.661885772396)) ;
#174137 = CARTESIAN_POINT('Ctrl Pts',(-15.1663307990368,-12.8395609374739,
117.835382986547)) ;
#174138 = CARTESIAN_POINT('Ctrl Pts',(-15.2143261495517,-13.1036924153161,
117.946224932861)) ;
#174139 = CARTESIAN_POINT('Ctrl Pts',(-15.2392646854199,-13.3927905140901,
117.986526462558)) ;
#174140 = CARTESIAN_POINT('Ctrl Pts',(-15.2397192982517,-13.6807940128297,
117.9526185938)) ;
#174141 = CARTESIAN_POINT('Ctrl Pts',(-15.2167475033035,-13.9516407801447,
117.847166620473)) ;
#174142 = CARTESIAN_POINT('Ctrl Pts',(-15.1722328786369,-14.1848191645832,
117.675959254401)) ;
#174143 = CARTESIAN_POINT('Ctrl Pts',(-15.1111116959615,-14.3611535147467,
117.45455531879)) ;
#174144 = CARTESIAN_POINT('Ctrl Pts',(-15.03716340119,-14.4717132500286,117.193678534081)) ;
#174145 = CARTESIAN_POINT('Ctrl Pts',(-14.9574931202988,-14.5058049610956,
116.91556782578)) ;
#174146 = CARTESIAN_POINT('Ctrl Pts',(-14.8782558620267,-14.4622432474708,
116.638782637704)) ;
#174147 = CARTESIAN_POINT('Ctrl Pts',(-14.8058079691528,-14.343914063795,
116.382668771781)) ;
#174148 = CARTESIAN_POINT('Ctrl Pts',(-14.7461096383968,-14.1592285094383,
116.165376277947)) ;
#174149 = CARTESIAN_POINT('Ctrl Pts',(-14.7042341925757,-13.9218383285055,
116.002418128098)) ;
#174150 = CARTESIAN_POINT('Ctrl Pts',(-14.6838147453501,-13.6477929587425,
115.904727451076)) ;
#174151 = CARTESIAN_POINT('Ctrl Pts',(-14.6872087463539,-13.3573882946602,
115.879587299227)) ;
#174152 = CARTESIAN_POINT('Ctrl Pts',(-14.7148769500706,-13.0713760146383,
115.928387341854)) ;
#174153 = CARTESIAN_POINT('Ctrl Pts',(-14.7656221631295,-12.8101300373193,
116.047465559082)) ;
#174154 = CARTESIAN_POINT('Ctrl Pts',(-14.836499389826,-12.5926203368979,
116.227885615043)) ;
#174155 = CARTESIAN_POINT('Ctrl Pts',(-14.9232190242914,-12.4341144288436,
116.456553356206)) ;
#174156 = CARTESIAN_POINT('Ctrl Pts',(-15.0204191933641,-12.346259851331,
116.717108536912)) ;
#174157 = CARTESIAN_POINT('Ctrl Pts',(-15.1212516203235,-12.3348158852733,
116.98892332195)) ;
#174158 = CARTESIAN_POINT('Ctrl Pts',(-15.2210253617375,-12.4019396871859,
117.257046128186)) ;
#174159 = CARTESIAN_POINT('Ctrl Pts',(-15.3104774186011,-12.5400212389952,
117.494364772624)) ;
#174160 = CARTESIAN_POINT('Ctrl Pts',(-15.386781464252,-12.7426569389483,
117.691155444074)) ;
#174161 = CARTESIAN_POINT('Ctrl Pts',(-15.4435452552671,-12.9928209893326,
117.828633943598)) ;
#174162 = CARTESIAN_POINT('Ctrl Pts',(-15.4780991318046,-13.274121349933,
117.89835399274)) ;
#174163 = CARTESIAN_POINT('Ctrl Pts',(-15.4884434105682,-13.5650423075934,
117.894429498399)) ;
#174164 = CARTESIAN_POINT('Ctrl Pts',(-15.4747873042015,-13.8454220244642,
117.817406765733)) ;
#174165 = CARTESIAN_POINT('Ctrl Pts',(-15.4387248228193,-14.095635489283,
117.672076552588)) ;
#174166 = CARTESIAN_POINT('Ctrl Pts',(-15.3836965141025,-14.2970558104585,
117.469021551389)) ;
#174167 = CARTESIAN_POINT('Ctrl Pts',(-15.3141371945857,-14.4359480747077,
117.221601988843)) ;
#174168 = CARTESIAN_POINT('Ctrl Pts',(-15.2359817859273,-14.501304829004,
116.948020668741)) ;
#174169 = CARTESIAN_POINT('Ctrl Pts',(-15.1561240539043,-14.4893139259723,
116.669494222094)) ;
#174170 = CARTESIAN_POINT('Ctrl Pts',(-15.0799694117837,-14.4004454436412,
116.401998946719)) ;
#174171 = CARTESIAN_POINT('Ctrl Pts',(-15.0146075791838,-14.2418718140722,
116.167568446909)) ;
#174172 = CARTESIAN_POINT('Ctrl Pts',(-14.9647824826636,-14.0233785235775,
115.98025836275)) ;
#174173 = CARTESIAN_POINT('Ctrl Pts',(-14.9353130383132,-13.7618917263419,
115.855036424513)) ;
#174174 = CARTESIAN_POINT('Ctrl Pts',(-14.9289325059808,-13.4754623735639,
115.800094097423)) ;
#174175 = CARTESIAN_POINT('Ctrl Pts',(-14.9467156400316,-13.1862230579374,
115.818918808621)) ;
#174176 = CARTESIAN_POINT('Ctrl Pts',(-14.9883696704994,-12.9121173454345,
115.910257352319)) ;
#174177 = CARTESIAN_POINT('Ctrl Pts',(-15.0514075082548,-12.6748571224349,
116.066831542999)) ;
#174178 = CARTESIAN_POINT('Ctrl Pts',(-15.1328444729729,-12.4898752939566,
116.279188009529)) ;
#174179 = CARTESIAN_POINT('Ctrl Pts',(-15.2258152326025,-12.3730682967797,
116.527146434279)) ;
#174180 = CARTESIAN_POINT('Ctrl Pts',(-15.3267957548085,-12.330125354393,
116.799022433184)) ;
#174181 = CARTESIAN_POINT('Ctrl Pts',(-15.4267371080215,-12.3650026478225,
117.068234016832)) ;
#174182 = CARTESIAN_POINT('Ctrl Pts',(-15.5220396277674,-12.4764750890778,
117.322748096145)) ;
#174183 = CARTESIAN_POINT('Ctrl Pts',(-15.6038717305927,-12.6535586984017,
117.536764515105)) ;
#174184 = CARTESIAN_POINT('Ctrl Pts',(-15.6692705920402,-12.8875907025722,
117.700299247988)) ;
#174185 = CARTESIAN_POINT('Ctrl Pts',(-15.7128057696858,-13.1564738506933,
117.797702690961)) ;
#174186 = CARTESIAN_POINT('Ctrl Pts',(-15.7332548587096,-13.4476180482474,
117.824312090504)) ;
#174187 = CARTESIAN_POINT('Ctrl Pts',(-15.7291353924876,-13.7346448783816,
117.776350799521)) ;
#174188 = CARTESIAN_POINT('Ctrl Pts',(-15.7018297830167,-13.9993799399049,
117.657715317448)) ;
#174189 = CARTESIAN_POINT('Ctrl Pts',(-15.6540905337258,-14.2219559568416,
117.476929036007)) ;
#174190 = CARTESIAN_POINT('Ctrl Pts',(-15.5899295337492,-14.3877271051732,
117.246044868715)) ;
#174191 = CARTESIAN_POINT('Ctrl Pts',(-15.5142887883934,-14.4840522417127,
116.980008252819)) ;
#174192 = CARTESIAN_POINT('Ctrl Pts',(-15.4346677192972,-14.5035551456864,
116.702251625481)) ;
#174193 = CARTESIAN_POINT('Ctrl Pts',(-15.3559292275796,-14.4455933724693,
116.426856756554)) ;
#174194 = CARTESIAN_POINT('Ctrl Pts',(-15.285414304366,-14.3137077173971,
116.176599635695)) ;
#174195 = CARTESIAN_POINT('Ctrl Pts',(-15.2287932761951,-14.118290994482,
115.968741900664)) ;
#174196 = CARTESIAN_POINT('Ctrl Pts',(-15.190662017011,-13.8721339097932,
115.817104400349)) ;
#174197 = CARTESIAN_POINT('Ctrl Pts',(-15.1746169230128,-13.5943341067766,
115.732853741077)) ;
#174198 = CARTESIAN_POINT('Ctrl Pts',(-15.1826673766295,-13.3016132059809,
115.721705106696)) ;
#174199 = CARTESIAN_POINT('Ctrl Pts',(-15.2146933752457,-13.0203974601351,
115.783981898111)) ;
#174200 = CARTESIAN_POINT('Ctrl Pts',(-15.269404025713,-12.7657619407627,
115.915129891759)) ;
#174201 = CARTESIAN_POINT('Ctrl Pts',(-15.3438708491905,-12.5577255499837,
116.10637631446)) ;
#174202 = CARTESIAN_POINT('Ctrl Pts',(-15.4327636159981,-12.4120606642955,
116.34175086754)) ;
#174203 = CARTESIAN_POINT('Ctrl Pts',(-15.5316685213714,-12.3380220880362,
116.60734315125)) ;
#174204 = CARTESIAN_POINT('Ctrl Pts',(-15.6323103361434,-12.3416277493325,
116.878663222145)) ;
#174205 = CARTESIAN_POINT('Ctrl Pts',(-15.7303191792415,-12.4221117178776,
117.141642652826)) ;
#174206 = CARTESIAN_POINT('Ctrl Pts',(-15.818253094992,-12.5739000669618,
117.37404115853)) ;
#174207 = CARTESIAN_POINT('Ctrl Pts',(-15.8910677122169,-12.7865530350162,
117.560294460758)) ;
#174208 = CARTESIAN_POINT('Ctrl Pts',(-15.943961350988,-13.044698151263,117.685874037695)) ;
#174209 = CARTESIAN_POINT('Ctrl Pts',(-15.973861910085,-13.328059924083,117.741608955228)) ;
#174210 = CARTESIAN_POINT('Ctrl Pts',(-15.9797490331987,-13.6187777866059,
117.724086355187)) ;
#174211 = CARTESIAN_POINT('Ctrl Pts',(-15.9616058932464,-13.8959727795492,
117.633255070877)) ;
#174212 = CARTESIAN_POINT('Ctrl Pts',(-15.92165968614,-14.1380897314584,117.476125293794)) ;
#174213 = CARTESIAN_POINT('Ctrl Pts',(-15.8633008249773,-14.3289912800735,
117.262814844311)) ;
#174214 = CARTESIAN_POINT('Ctrl Pts',(-15.7921118917969,-14.4536834307714,
117.01067142375)) ;
#174215 = CARTESIAN_POINT('Ctrl Pts',(-15.7132086075603,-14.5050447602448,
116.734875307883)) ;
#174216 = CARTESIAN_POINT('Ctrl Pts',(-15.6332196110999,-14.4782940097224,
116.455753006044)) ;
#174217 = CARTESIAN_POINT('Ctrl Pts',(-15.5587696998728,-14.3758709565101,
116.193557985972)) ;
#174218 = CARTESIAN_POINT('Ctrl Pts',(-15.4956323923376,-14.2038414128419,
115.965654894124)) ;
#174219 = CARTESIAN_POINT('Ctrl Pts',(-15.4497236558171,-13.9777022974474,
115.790578372436)) ;
#174220 = CARTESIAN_POINT('Ctrl Pts',(-15.4242298945828,-13.7081471730545,
115.677198196239)) ;
#174221 = CARTESIAN_POINT('Ctrl Pts',(-15.4224756486748,-13.4207218926891,
115.636530543552)) ;
#174222 = CARTESIAN_POINT('Ctrl Pts',(-15.4448455283626,-13.1323473586493,
115.669233043994)) ;
#174223 = CARTESIAN_POINT('Ctrl Pts',(-15.4907259221535,-12.8640039527127,
115.773502605509)) ;
#174224 = CARTESIAN_POINT('Ctrl Pts',(-15.5576964345495,-12.6351955964259,
115.941952413121)) ;
#174225 = CARTESIAN_POINT('Ctrl Pts',(-15.6410494594336,-12.4633049543151,
116.160508256525)) ;
#174226 = CARTESIAN_POINT('Ctrl Pts',(-15.73692924491,-12.3586842738095,116.416876897232)) ;
#174227 = CARTESIAN_POINT('Ctrl Pts',(-15.837547597677,-12.3308701665295,
116.687989713795)) ;
#174228 = CARTESIAN_POINT('Ctrl Pts',(-15.9375214249544,-12.3804185210795,
116.95704231323)) ;
#174229 = CARTESIAN_POINT('Ctrl Pts',(-16.0302559090412,-12.5045865657479,
117.204009987315)) ;
#174230 = CARTESIAN_POINT('Ctrl Pts',(-16.1096439036277,-12.6936012415773,
117.410410771102)) ;
#174231 = CARTESIAN_POINT('Ctrl Pts',(-16.1712738995267,-12.9362801376937,
117.56247016244)) ;
#174232 = CARTESIAN_POINT('Ctrl Pts',(-16.2106239956556,-13.2112926431605,
117.646987028832)) ;
#174233 = CARTESIAN_POINT('Ctrl Pts',(-16.2263302334408,-13.5026318637497,
117.659280382526)) ;
#174234 = CARTESIAN_POINT('Ctrl Pts',(-16.2177424879971,-13.7865927515763,
117.59774844092)) ;
#174235 = CARTESIAN_POINT('Ctrl Pts',(-16.1863917194238,-14.0445932154009,
117.466837858413)) ;
#174236 = CARTESIAN_POINT('Ctrl Pts',(-16.1351369456625,-14.2581092551482,
117.275260073732)) ;
#174237 = CARTESIAN_POINT('Ctrl Pts',(-16.0682061521682,-14.4117380229187,
117.035830487134)) ;
#174238 = CARTESIAN_POINT('Ctrl Pts',(-15.9915317982417,-14.4936441507055,
116.76682264577)) ;
#174239 = CARTESIAN_POINT('Ctrl Pts',(-15.9111646098176,-14.4983888239063,
116.486541384417)) ;
#174240 = CARTESIAN_POINT('Ctrl Pts',(-15.8339367194652,-14.426207251784,
116.215966892118)) ;
#174241 = CARTESIAN_POINT('Ctrl Pts',(-15.7654080575456,-14.2809809264381,
115.971651595224)) ;
#174242 = CARTESIAN_POINT('Ctrl Pts',(-15.7121638592197,-14.0755731076895,
115.774205354296)) ;
#174243 = CARTESIAN_POINT('Ctrl Pts',(-15.6778558958867,-13.8214647968314,
115.634145099666)) ;
#174244 = CARTESIAN_POINT('Ctrl Pts',(-15.6663008904224,-13.5390721929965,
115.563497706539)) ;
#174245 = CARTESIAN_POINT('Ctrl Pts',(-15.6788710235298,-13.2479213210197,
115.566312381468)) ;
#174246 = CARTESIAN_POINT('Ctrl Pts',(-15.7154570310451,-12.9689956696526,
115.642283838143)) ;
#174247 = CARTESIAN_POINT('Ctrl Pts',(-15.7742309880506,-12.7220961737177,
115.785813685881)) ;
#174248 = CARTESIAN_POINT('Ctrl Pts',(-15.8515784407682,-12.5254520180373,
115.985975276655)) ;
#174249 = CARTESIAN_POINT('Ctrl Pts',(-15.94270937751,-12.3924871288094,116.22814157512)) ;
#174250 = CARTESIAN_POINT('Ctrl Pts',(-16.0425166341127,-12.3327720085306,
116.496536154784)) ;
#174251 = CARTESIAN_POINT('Ctrl Pts',(-16.1432965454572,-12.3509988977752,
116.768165464397)) ;
#174252 = CARTESIAN_POINT('Ctrl Pts',(-16.2397734663179,-12.4453838611795,
117.026540426964)) ;
#174253 = CARTESIAN_POINT('Ctrl Pts',(-16.3254447848863,-12.6100760699984,
117.251940625839)) ;
#174254 = CARTESIAN_POINT('Ctrl Pts',(-16.3945559404646,-12.8316470477012,
117.427060764436)) ;
#174255 = CARTESIAN_POINT('Ctrl Pts',(-16.4435312853677,-13.0973555362981,
117.540560244616)) ;
#174256 = CARTESIAN_POINT('Ctrl Pts',(-16.4688621130792,-13.3829827267331,
117.582449970111)) ;
#174257 = CARTESIAN_POINT('Ctrl Pts',(-16.470124542703,-13.6735145155205,
117.550719313167)) ;
#174258 = CARTESIAN_POINT('Ctrl Pts',(-16.4477134830108,-13.9443960540442,
117.447059781621)) ;
#174259 = CARTESIAN_POINT('Ctrl Pts',(-16.4040416496053,-14.1780473237906,
117.278577420489)) ;
#174260 = CARTESIAN_POINT('Ctrl Pts',(-16.3431014881368,-14.3571729772058,
117.057559267268)) ;
#174261 = CARTESIAN_POINT('Ctrl Pts',(-16.2692843220695,-14.4697035049953,
116.797034589842)) ;
#174262 = CARTESIAN_POINT('Ctrl Pts',(-16.189974204939,-14.5058316151569,
116.520142021784)) ;
#174263 = CARTESIAN_POINT('Ctrl Pts',(-16.1107202304642,-14.4647781183691,
116.243348321315)) ;
#174264 = CARTESIAN_POINT('Ctrl Pts',(-16.03788617739,-14.3484987257117,115.986015587949)) ;
#174265 = CARTESIAN_POINT('Ctrl Pts',(-15.9776687836141,-14.1655053892491,
115.767116814539)) ;
#174266 = CARTESIAN_POINT('Ctrl Pts',(-15.9351536436701,-13.9286208259661,
115.602105173613)) ;
#174267 = CARTESIAN_POINT('Ctrl Pts',(-15.9141622270948,-13.6565946963034,
115.502836000379)) ;
#174268 = CARTESIAN_POINT('Ctrl Pts',(-15.9168400704658,-13.3650274692435,
115.475347116262)) ;
#174269 = CARTESIAN_POINT('Ctrl Pts',(-15.943917468856,-13.0788343995772,
115.522370330454)) ;
#174270 = CARTESIAN_POINT('Ctrl Pts',(-15.9938421820601,-12.8175211583994,
115.639074782229)) ;
#174271 = CARTESIAN_POINT('Ctrl Pts',(-16.0641439891467,-12.5984995679009,
115.817749196681)) ;
#174272 = CARTESIAN_POINT('Ctrl Pts',(-16.1502868270294,-12.4381081950322,
116.044719588303)) ;
#174273 = CARTESIAN_POINT('Ctrl Pts',(-16.2478432903342,-12.3474840033873,
116.306149605933)) ;
#174274 = CARTESIAN_POINT('Ctrl Pts',(-16.3485101468529,-12.3342746176406,
116.577507728098)) ;
#174275 = CARTESIAN_POINT('Ctrl Pts',(-16.4477907403322,-12.3983523506611,
116.844372055818)) ;
#174276 = CARTESIAN_POINT('Ctrl Pts',(-16.5383794781962,-12.5353914606374,
117.084853142342)) ;
#174277 = CARTESIAN_POINT('Ctrl Pts',(-16.6151024200091,-12.7368848040207,
117.282902758644)) ;
#174278 = CARTESIAN_POINT('Ctrl Pts',(-16.6722339594684,-12.9849643669818,
117.421634700217)) ;
#174279 = CARTESIAN_POINT('Ctrl Pts',(-16.7074953741335,-13.2657001242146,
117.493501410732)) ;
#174280 = CARTESIAN_POINT('Ctrl Pts',(-16.7185435095042,-13.5562446654925,
117.491765214544)) ;
#174281 = CARTESIAN_POINT('Ctrl Pts',(-16.7056071827156,-13.837740260252,
117.416879374421)) ;
#174282 = CARTESIAN_POINT('Ctrl Pts',(-16.6698983566585,-14.0900089023239,
117.272469305418)) ;
#174283 = CARTESIAN_POINT('Ctrl Pts',(-16.615678314691,-14.2916996646196,
117.072102717414)) ;
#174284 = CARTESIAN_POINT('Ctrl Pts',(-16.5462715072985,-14.4330905333239,
116.82503637481)) ;
#174285 = CARTESIAN_POINT('Ctrl Pts',(-16.4684461424741,-14.5004556458798,
116.552546390901)) ;
#174286 = CARTESIAN_POINT('Ctrl Pts',(-16.3884429132822,-14.4906784452632,
116.273515768952)) ;
#174287 = CARTESIAN_POINT('Ctrl Pts',(-16.3122978006783,-14.4044504861589,
116.006169416252)) ;
#174288 = CARTESIAN_POINT('Ctrl Pts',(-16.2460229579914,-14.2464177648016,
115.768663223049)) ;
#174289 = CARTESIAN_POINT('Ctrl Pts',(-16.1959322208732,-14.0296079395376,
115.58064014647)) ;
#174290 = CARTESIAN_POINT('Ctrl Pts',(-16.1659524449804,-13.7700542634679,
115.453985376571)) ;
#174291 = CARTESIAN_POINT('Ctrl Pts',(-16.1588094450499,-13.4844393542531,
115.396766680954)) ;
#174292 = CARTESIAN_POINT('Ctrl Pts',(-16.1759899887603,-13.1938467066394,
115.413606223146)) ;
#174293 = CARTESIAN_POINT('Ctrl Pts',(-16.2169131908586,-12.9193998282655,
115.502784611301)) ;
#174294 = CARTESIAN_POINT('Ctrl Pts',(-16.2798288449759,-12.679977460876,
115.658797492625)) ;
#174295 = CARTESIAN_POINT('Ctrl Pts',(-16.3596321413727,-12.4956043021029,
115.866685267832)) ;
#174296 = CARTESIAN_POINT('Ctrl Pts',(-16.4533735886139,-12.3751190535725,
116.11656191809)) ;
#174297 = CARTESIAN_POINT('Ctrl Pts',(-16.5533514223054,-12.3303020351126,
116.385717677923)) ;
#174298 = CARTESIAN_POINT('Ctrl Pts',(-16.6543061351395,-12.3631774170788,
116.657672551658)) ;
#174299 = CARTESIAN_POINT('Ctrl Pts',(-16.7488808914051,-12.4713342743348,
116.91035898593)) ;
#174300 = CARTESIAN_POINT('Ctrl Pts',(-16.8318207118205,-12.6476404276989,
117.12747273466)) ;
#174301 = CARTESIAN_POINT('Ctrl Pts',(-16.8975001296176,-12.8790215196565,
117.292056197982)) ;
#174302 = CARTESIAN_POINT('Ctrl Pts',(-16.942134561038,-13.1499133657009,
117.392426703096)) ;
#174303 = CARTESIAN_POINT('Ctrl Pts',(-16.9630233535542,-13.4386144880716,
117.420658950536)) ;
#174304 = CARTESIAN_POINT('Ctrl Pts',(-16.9596443378371,-13.7268235527867,
117.37484372471)) ;
#174305 = CARTESIAN_POINT('Ctrl Pts',(-16.9330916364897,-13.9914324144424,
117.258649259076)) ;
#174306 = CARTESIAN_POINT('Ctrl Pts',(-16.8858015410838,-14.2164140691066,
117.079108171634)) ;
#174307 = CARTESIAN_POINT('Ctrl Pts',(-16.8218713013157,-14.384032579335,
116.848865519025)) ;
#174308 = CARTESIAN_POINT('Ctrl Pts',(-16.7469781937031,-14.4820529544929,
116.585338242812)) ;
#174309 = CARTESIAN_POINT('Ctrl Pts',(-16.6668754248099,-14.5042250600488,
116.305877110692)) ;
#174310 = CARTESIAN_POINT('Ctrl Pts',(-16.5879598850496,-14.4479097103847,
116.029910236852)) ;
#174311 = CARTESIAN_POINT('Ctrl Pts',(-16.5174994343308,-14.3189148106109,
115.780020371028)) ;
#174312 = CARTESIAN_POINT('Ctrl Pts',(-16.4601033314479,-14.1239822238445,
115.569589941592)) ;
#174313 = CARTESIAN_POINT('Ctrl Pts',(-16.4215747130303,-13.8804446676162,
115.416952493218)) ;
#174314 = CARTESIAN_POINT('Ctrl Pts',(-16.4047818629355,-13.6007259227713,
115.330092652858)) ;
#174315 = CARTESIAN_POINT('Ctrl Pts',(-16.4121369550956,-13.310886389785,
115.317177989403)) ;
#174316 = CARTESIAN_POINT('Ctrl Pts',(-16.4435486385353,-13.0275729196668,
115.377389997303)) ;
#174317 = CARTESIAN_POINT('Ctrl Pts',(-16.4978834158618,-12.7715214711428,
115.507323795441)) ;
#174318 = CARTESIAN_POINT('Ctrl Pts',(-16.5717603357923,-12.5625540682405,
115.696844987537)) ;
#174319 = CARTESIAN_POINT('Ctrl Pts',(-16.6600063471763,-12.4155360311479,
115.930369190556)) ;
#174320 = CARTESIAN_POINT('Ctrl Pts',(-16.7583961657612,-12.339199302571,
116.194502768036)) ;
#174321 = CARTESIAN_POINT('Ctrl Pts',(-16.8595422687567,-12.3403409953756,
116.467185667784)) ;
#174322 = CARTESIAN_POINT('Ctrl Pts',(-16.9578689738167,-12.4190382667156,
116.731080805892)) ;
#174323 = CARTESIAN_POINT('Ctrl Pts',(-17.0458999041783,-12.5685297170459,
116.963876177155)) ;
#174324 = CARTESIAN_POINT('Ctrl Pts',(-17.1191748552296,-12.7793086778933,
117.151568386626)) ;
#174325 = CARTESIAN_POINT('Ctrl Pts',(-17.1727252854914,-13.0361487300971,
117.279168850677)) ;
#174326 = CARTESIAN_POINT('Ctrl Pts',(-17.2034288318534,-13.3199156358865,
117.337236471295)) ;
#174327 = CARTESIAN_POINT('Ctrl Pts',(-17.2099599842142,-13.61053350134,117.321699031089)) ;
#174328 = CARTESIAN_POINT('Ctrl Pts',(-17.1925797786754,-13.8877845324202,
117.233281417969)) ;
#174329 = CARTESIAN_POINT('Ctrl Pts',(-17.1531888988296,-14.1315208949384,
117.077791857519)) ;
#174330 = CARTESIAN_POINT('Ctrl Pts',(-17.0955345319982,-14.3236676354294,
116.866747533545)) ;
#174331 = CARTESIAN_POINT('Ctrl Pts',(-17.0243702739968,-14.451213086268,
116.614520189238)) ;
#174332 = CARTESIAN_POINT('Ctrl Pts',(-16.9454296666756,-14.5046478984509,
116.338545787343)) ;
#174333 = CARTESIAN_POINT('Ctrl Pts',(-16.8656122340257,-14.4801334339684,
116.060046712965)) ;
#174334 = CARTESIAN_POINT('Ctrl Pts',(-16.790980956793,-14.3800974324411,
115.797335713982)) ;
#174335 = CARTESIAN_POINT('Ctrl Pts',(-16.7272992435064,-14.2097836883392,
115.567723704897)) ;
#174336 = CARTESIAN_POINT('Ctrl Pts',(-16.6808108315259,-13.9844447661634,
115.3908060488)) ;
#174337 = CARTESIAN_POINT('Ctrl Pts',(-16.6547738612727,-13.7175338810347,
115.275995973862)) ;
#174338 = CARTESIAN_POINT('Ctrl Pts',(-16.6522344647069,-13.4290941380284,
115.232763303442)) ;
#174339 = CARTESIAN_POINT('Ctrl Pts',(-16.6738872742428,-13.1407025280343,
115.263323344163)) ;
#174340 = CARTESIAN_POINT('Ctrl Pts',(-16.7192914965339,-12.8707969653127,
115.366034947544)) ;
#174341 = CARTESIAN_POINT('Ctrl Pts',(-16.7852951087572,-12.6417711077458,
115.53174600974)) ;
#174342 = CARTESIAN_POINT('Ctrl Pts',(-16.8687385029215,-12.4670674817275,
115.750354845925)) ;
#174343 = CARTESIAN_POINT('Ctrl Pts',(-16.9635606886986,-12.3610581795072,
116.003803286491)) ;
#174344 = CARTESIAN_POINT('Ctrl Pts',(-17.0649420670116,-12.3304705905987,
116.27693713892)) ;
#174345 = CARTESIAN_POINT('Ctrl Pts',(-17.1648109896159,-12.3780041179342,
116.545751053977)) ;
#174346 = CARTESIAN_POINT('Ctrl Pts',(-17.2579372276331,-12.5002675543906,
116.79387021803)) ;
#174347 = CARTESIAN_POINT('Ctrl Pts',(-17.3375779201861,-12.6872113223539,
117.001122929289)) ;
#174348 = CARTESIAN_POINT('Ctrl Pts',(-17.3998316457169,-12.928470822573,
117.155087519117)) ;
#174349 = CARTESIAN_POINT('Ctrl Pts',(-17.4399174994754,-13.2034657060163,
117.241757837914)) ;
#174350 = CARTESIAN_POINT('Ctrl Pts',(-17.4562690855038,-13.4939400108665,
117.256107218264)) ;
#174351 = CARTESIAN_POINT('Ctrl Pts',(-17.4483972852435,-13.7785749983251,
117.196730556268)) ;
#174352 = CARTESIAN_POINT('Ctrl Pts',(-17.4176717828043,-14.0376123935157,
117.067726587636)) ;
#174353 = CARTESIAN_POINT('Ctrl Pts',(-17.3669381628985,-14.2526152270872,
116.877737714805)) ;
#174354 = CARTESIAN_POINT('Ctrl Pts',(-17.300521743148,-14.4080507138092,
116.639938676009)) ;
#174355 = CARTESIAN_POINT('Ctrl Pts',(-17.2239015581171,-14.4922598223547,
116.371021974036)) ;
#174356 = CARTESIAN_POINT('Ctrl Pts',(-17.1439517410193,-14.4995566650645,
116.092195902509)) ;
#174357 = CARTESIAN_POINT('Ctrl Pts',(-17.0659766810491,-14.4291954268347,
115.819082015723)) ;
#174358 = CARTESIAN_POINT('Ctrl Pts',(-16.9973489861747,-14.2862746553945,
115.574590132372)) ;
#174359 = CARTESIAN_POINT('Ctrl Pts',(-16.943507599311,-14.0821782924177,
115.375260361907)) ;
#174360 = CARTESIAN_POINT('Ctrl Pts',(-16.9086511894243,-13.8298750263426,
115.233624849604)) ;
#174361 = CARTESIAN_POINT('Ctrl Pts',(-16.8963479197035,-13.5470860719876,
115.160572447035)) ;
#174362 = CARTESIAN_POINT('Ctrl Pts',(-16.90824578111,-13.2560613841224,115.161364252542)) ;
#174363 = CARTESIAN_POINT('Ctrl Pts',(-16.9442254493305,-12.9762949722028,
115.235455446136)) ;
#174364 = CARTESIAN_POINT('Ctrl Pts',(-17.0022072372073,-12.729021213087,
115.376690040029)) ;
#174365 = CARTESIAN_POINT('Ctrl Pts',(-17.0792272362676,-12.5300504685621,
115.575764889513)) ;
#174366 = CARTESIAN_POINT('Ctrl Pts',(-17.1704529515286,-12.3949013412461,
115.818078836631)) ;
#174367 = CARTESIAN_POINT('Ctrl Pts',(-17.2696316491355,-12.3334783627152,
116.084736767084)) ;
#174368 = CARTESIAN_POINT('Ctrl Pts',(-17.3706199437548,-12.3494129205617,
116.356939612366)) ;
#174369 = CARTESIAN_POINT('Ctrl Pts',(-17.4673694639669,-12.4418688951199,
116.61612522571)) ;
#174370 = CARTESIAN_POINT('Ctrl Pts',(-17.5535183531139,-12.6051421932678,
116.842927305494)) ;
#174371 = CARTESIAN_POINT('Ctrl Pts',(-17.6228267175663,-12.824581983231,
117.018781891196)) ;
#174372 = CARTESIAN_POINT('Ctrl Pts',(-17.6723197045104,-13.0878606072953,
117.134031445032)) ;
#174373 = CARTESIAN_POINT('Ctrl Pts',(-17.6985731634041,-13.3747557627756,
117.178522404017)) ;
#174374 = CARTESIAN_POINT('Ctrl Pts',(-17.7004702306017,-13.6654070056361,
117.148736694593)) ;
#174375 = CARTESIAN_POINT('Ctrl Pts',(-17.6787592525954,-13.9370542943595,
117.047221465574)) ;
#174376 = CARTESIAN_POINT('Ctrl Pts',(-17.6354116057115,-14.1729033532404,
116.879576215049)) ;
#174377 = CARTESIAN_POINT('Ctrl Pts',(-17.5750711191891,-14.3528610645483,
116.660517699246)) ;
#174378 = CARTESIAN_POINT('Ctrl Pts',(-17.5017177853474,-14.4673900074207,
116.401484107417)) ;
#174379 = CARTESIAN_POINT('Ctrl Pts',(-17.4223560273365,-14.5059091307987,
116.124370136875)) ;
#174380 = CARTESIAN_POINT('Ctrl Pts',(-17.3429501969861,-14.467003448986,
115.847090385579)) ;
#174381 = CARTESIAN_POINT('Ctrl Pts',(-17.2698268935793,-14.3526296857438,
115.58886231961)) ;
#174382 = CARTESIAN_POINT('Ctrl Pts',(-17.209359096455,-14.1719531187117,
115.369308707155)) ;
#174383 = CARTESIAN_POINT('Ctrl Pts',(-17.1661919090706,-13.936583984801,
115.202313468294)) ;
#174384 = CARTESIAN_POINT('Ctrl Pts',(-17.1445055243567,-13.6642946874373,
115.100795313256)) ;
#174385 = CARTESIAN_POINT('Ctrl Pts',(-17.1464540999734,-13.3747428455626,
115.07130654278)) ;
#174386 = CARTESIAN_POINT('Ctrl Pts',(-17.1727178775642,-13.0876482903165,
115.115799669676)) ;
#174387 = CARTESIAN_POINT('Ctrl Pts',(-17.2222028953257,-12.8243385253649,
115.231028671208)) ;
#174388 = CARTESIAN_POINT('Ctrl Pts',(-17.2919810291401,-12.6038922563675,
115.408113946603)) ;
#174389 = CARTESIAN_POINT('Ctrl Pts',(-17.3779184788419,-12.4415502102937,
115.634396370926)) ;
#174390 = CARTESIAN_POINT('Ctrl Pts',(-17.4746658472938,-12.3493107874977,
115.89357675197)) ;
#174391 = CARTESIAN_POINT('Ctrl Pts',(-17.5755185168944,-12.3333698024851,
116.165420915511)) ;
#174392 = CARTESIAN_POINT('Ctrl Pts',(-17.6754893328123,-12.3958418590805,
116.434192181454)) ;
#174393 = CARTESIAN_POINT('Ctrl Pts',(-17.7659177540856,-12.5305465195612,
116.674353272671)) ;
#174394 = CARTESIAN_POINT('Ctrl Pts',(-17.8428696280429,-12.7291635452138,
116.873260297753)) ;
#174395 = CARTESIAN_POINT('Ctrl Pts',(-17.900952909542,-12.9771312925897,
117.014719731031)) ;
#174396 = CARTESIAN_POINT('Ctrl Pts',(-17.9368966294271,-13.2574946761857,
117.088639322891)) ;
#174397 = CARTESIAN_POINT('Ctrl Pts',(-17.9486369502931,-13.5486172877669,
117.088938884935)) ;
#174398 = CARTESIAN_POINT('Ctrl Pts',(-17.9363162489277,-13.8299622964239,
117.016005420011)) ;
#174399 = CARTESIAN_POINT('Ctrl Pts',(-17.9015308192628,-14.082140489746,
116.874612226591)) ;
#174400 = CARTESIAN_POINT('Ctrl Pts',(-17.8474297188587,-14.2871395255682,
116.67433526165)) ;
#174401 = CARTESIAN_POINT('Ctrl Pts',(-17.7784858967829,-14.4298488440199,
116.428771121435)) ;
#174402 = CARTESIAN_POINT('Ctrl Pts',(-17.7011619828439,-14.4994383097765,
116.157945215762)) ;
#174403 = CARTESIAN_POINT('Ctrl Pts',(-17.6208255769599,-14.4922423916848,
115.877768836137)) ;
#174404 = CARTESIAN_POINT('Ctrl Pts',(-17.5442238721124,-14.4074859363464,
115.60889672167)) ;
#174405 = CARTESIAN_POINT('Ctrl Pts',(-17.4781148630412,-14.2527213410347,
115.372193987303)) ;
#174406 = CARTESIAN_POINT('Ctrl Pts',(-17.4272659714627,-14.0372448891262,
115.181771156024)) ;
#174407 = CARTESIAN_POINT('Ctrl Pts',(-17.3965606435217,-13.7782273369584,
115.052841406963)) ;
#174408 = CARTESIAN_POINT('Ctrl Pts',(-17.3887643996198,-13.4921296981973,
114.993517684583)) ;
#174409 = CARTESIAN_POINT('Ctrl Pts',(-17.4043330444271,-13.217409939261,
115.007409012445)) ;
#174410 = CARTESIAN_POINT('Ctrl Pts',(-17.4280438693922,-13.0469696088692,
115.057750935805)) ;
#174411 = CARTESIAN_POINT('Ctrl Pts',(-17.4415366461909,-12.9727494438644,
115.08882743648)) ;
#174412 = CARTESIAN_POINT('',(-6.39568111142174,-13.1317299129408,118.572890161645)) ;
#174413 = CARTESIAN_POINT('Origin',(-6.41836956894997,-13.1500241806476,118.641995542507)) ;
#174414 = CARTESIAN_POINT('',(-6.44105802647819,-13.1683184483544,118.711100923369)) ;
#174415 = CARTESIAN_POINT('Origin',(-6.41836956894997,-13.1500241806476,118.641995542507)) ;
#174416 = CARTESIAN_POINT('Origin',(-6.41836956894997,-13.1500241806476,118.641995542507)) ;
#174417 = CARTESIAN_POINT('Ctrl Pts',(-6.34456572554058,-13.1500241806476,
118.666226584225)) ;
#174418 = CARTESIAN_POINT('Ctrl Pts',(-6.34331320628583,-13.1861488576831,
118.656365702645)) ;
#174419 = CARTESIAN_POINT('Ctrl Pts',(-6.34019257639539,-13.2629207728781,
118.653629878536)) ;
#174420 = CARTESIAN_POINT('Ctrl Pts',(-6.33463380664346,-13.3681754735787,
118.700728440715)) ;
#174421 = CARTESIAN_POINT('Ctrl Pts',(-6.32932953020779,-13.4419954208924,
118.789585923991)) ;
#174422 = CARTESIAN_POINT('Ctrl Pts',(-6.3266820427946,-13.4603090867706,
118.864513089041)) ;
#174423 = CARTESIAN_POINT('Ctrl Pts',(-6.32571868123136,-13.4607127643287,
118.902106572586)) ;
#174424 = CARTESIAN_POINT('Ctrl Pts',(-6.36725418306881,-13.1683184483544,
118.735331965087)) ;
#174425 = CARTESIAN_POINT('Ctrl Pts',(-6.36636841296643,-13.1940059114669,
118.728126747212)) ;
#174426 = CARTESIAN_POINT('Ctrl Pts',(-6.36415538975798,-13.2486867737934,
118.725794983451)) ;
#174427 = CARTESIAN_POINT('Ctrl Pts',(-6.36019871534406,-13.3239058135206,
118.758824526017)) ;
#174428 = CARTESIAN_POINT('Ctrl Pts',(-6.35641083129055,-13.3769362528745,
118.821760884763)) ;
#174429 = CARTESIAN_POINT('Ctrl Pts',(-6.35451160798637,-13.3903536795156,
118.87504961753)) ;
#174430 = CARTESIAN_POINT('Ctrl Pts',(-6.35381761696714,-13.3908270508895,
118.901830161472)) ;
#174431 = CARTESIAN_POINT('Ctrl Pts',(-6.44105802647819,-13.1683184483544,
118.711100923369)) ;
#174432 = CARTESIAN_POINT('Ctrl Pts',(-6.44002943016128,-13.1977103078297,
118.703455895044)) ;
#174433 = CARTESIAN_POINT('Ctrl Pts',(-6.43747870841564,-13.2599976587319,
118.701985311717)) ;
#174434 = CARTESIAN_POINT('Ctrl Pts',(-6.43296369962062,-13.3449026924378,
118.741207405795)) ;
#174435 = CARTESIAN_POINT('Ctrl Pts',(-6.4286795521859,-13.4039111623081,
118.813989174412)) ;
#174436 = CARTESIAN_POINT('Ctrl Pts',(-6.42655805213203,-13.4180394153483,
118.874932709186)) ;
#174437 = CARTESIAN_POINT('Ctrl Pts',(-6.42579176677498,-13.4180036036418,
118.905424525735)) ;
#174438 = CARTESIAN_POINT('Ctrl Pts',(-6.51486186988758,-13.1683184483544,
118.686869881651)) ;
#174439 = CARTESIAN_POINT('Ctrl Pts',(-6.51369044735612,-13.2014147041926,
118.678785042876)) ;
#174440 = CARTESIAN_POINT('Ctrl Pts',(-6.5108020270733,-13.2713085436704,
118.678175639983)) ;
#174441 = CARTESIAN_POINT('Ctrl Pts',(-6.50572868389717,-13.365899571355,
118.723590285574)) ;
#174442 = CARTESIAN_POINT('Ctrl Pts',(-6.50094827308125,-13.4308860717416,
118.806217464061)) ;
#174443 = CARTESIAN_POINT('Ctrl Pts',(-6.49860449627767,-13.4457251511809,
118.874815800842)) ;
#174444 = CARTESIAN_POINT('Ctrl Pts',(-6.49776591658281,-13.445180156394,
118.909018889999)) ;
#174445 = CARTESIAN_POINT('Ctrl Pts',(-6.49217341235936,-13.1500241806476,
118.617764500789)) ;
#174446 = CARTESIAN_POINT('Ctrl Pts',(-6.49063524067551,-13.1935576504088,
118.607023998309)) ;
#174447 = CARTESIAN_POINT('Ctrl Pts',(-6.48683921371072,-13.2855425427551,
118.606010535068)) ;
#174448 = CARTESIAN_POINT('Ctrl Pts',(-6.48016377519658,-13.4101692314131,
118.665494200272)) ;
#174449 = CARTESIAN_POINT('Ctrl Pts',(-6.47386697199849,-13.4959452397595,
118.774042503289)) ;
#174450 = CARTESIAN_POINT('Ctrl Pts',(-6.4707749310859,-13.515680558436,118.864279272352)) ;
#174451 = CARTESIAN_POINT('Ctrl Pts',(-6.46966698084703,-13.5150658698332,
118.909295301113)) ;
#174452 = CARTESIAN_POINT('Ctrl Pts',(-6.46948495483114,-13.1317299129408,
118.548659119927)) ;
#174453 = CARTESIAN_POINT('Ctrl Pts',(-6.4675800339949,-13.185700596625,118.535262953743)) ;
#174454 = CARTESIAN_POINT('Ctrl Pts',(-6.46287640034814,-13.2997765418398,
118.533845430152)) ;
#174455 = CARTESIAN_POINT('Ctrl Pts',(-6.45459886649599,-13.4544388914713,
118.60739811497)) ;
#174456 = CARTESIAN_POINT('Ctrl Pts',(-6.44678567091572,-13.5610044077774,
118.741867542516)) ;
#174457 = CARTESIAN_POINT('Ctrl Pts',(-6.44294536589413,-13.585635965691,
118.853742743863)) ;
#174458 = CARTESIAN_POINT('Ctrl Pts',(-6.44156804511125,-13.5849515832724,
118.909571712227)) ;
#174459 = CARTESIAN_POINT('Ctrl Pts',(-6.39568111142176,-13.1317299129408,
118.572890161645)) ;
#174460 = CARTESIAN_POINT('Ctrl Pts',(-6.39391901680005,-13.1819962002622,
118.559933805911)) ;
#174461 = CARTESIAN_POINT('Ctrl Pts',(-6.38955308169047,-13.2884656569013,
118.557655101886)) ;
#174462 = CARTESIAN_POINT('Ctrl Pts',(-6.38183388221942,-13.433442012554,
118.625015235192)) ;
#174463 = CARTESIAN_POINT('Ctrl Pts',(-6.37451695002037,-13.5340294983438,
118.749639252867)) ;
#174464 = CARTESIAN_POINT('Ctrl Pts',(-6.37089892174848,-13.5579502298583,
118.853859652207)) ;
#174465 = CARTESIAN_POINT('Ctrl Pts',(-6.36959389530342,-13.5577750305201,
118.905977347964)) ;
#174466 = CARTESIAN_POINT('Ctrl Pts',(-6.32187726801236,-13.1317299129408,
118.597121203363)) ;
#174467 = CARTESIAN_POINT('Ctrl Pts',(-6.32025799960521,-13.1782918038993,
118.584604658079)) ;
#174468 = CARTESIAN_POINT('Ctrl Pts',(-6.31622976303281,-13.2771547719628,
118.58146477362)) ;
#174469 = CARTESIAN_POINT('Ctrl Pts',(-6.30906889794287,-13.4124451336368,
118.642632355413)) ;
#174470 = CARTESIAN_POINT('Ctrl Pts',(-6.30224822912501,-13.5070545889103,
118.757410963219)) ;
#174471 = CARTESIAN_POINT('Ctrl Pts',(-6.29885247760283,-13.5302644940257,
118.853976560551)) ;
#174472 = CARTESIAN_POINT('Ctrl Pts',(-6.29761974549558,-13.5305984777679,
118.9023829837)) ;
#174473 = CARTESIAN_POINT('Ctrl Pts',(-6.34456572554058,-13.1500241806476,
118.666226584225)) ;
#174474 = CARTESIAN_POINT('Ctrl Pts',(-6.34331320628583,-13.1861488576831,
118.656365702645)) ;
#174475 = CARTESIAN_POINT('Ctrl Pts',(-6.34019257639539,-13.2629207728781,
118.653629878536)) ;
#174476 = CARTESIAN_POINT('Ctrl Pts',(-6.33463380664346,-13.3681754735787,
118.700728440715)) ;
#174477 = CARTESIAN_POINT('Ctrl Pts',(-6.32932953020779,-13.4419954208924,
118.789585923991)) ;
#174478 = CARTESIAN_POINT('Ctrl Pts',(-6.3266820427946,-13.4603090867706,
118.864513089041)) ;
#174479 = CARTESIAN_POINT('Ctrl Pts',(-6.32571868123136,-13.4607127643287,
118.902106572586)) ;
#174480 = CARTESIAN_POINT('',(-6.32571868123136,-13.4607127643287,118.902106572586)) ;
#174481 = CARTESIAN_POINT('Ctrl Pts',(-6.34456572554058,-13.1500241806476,
118.666226584225)) ;
#174482 = CARTESIAN_POINT('Ctrl Pts',(-6.34331320628583,-13.1861488576831,
118.656365702645)) ;
#174483 = CARTESIAN_POINT('Ctrl Pts',(-6.34019257639539,-13.2629207728781,
118.653629878536)) ;
#174484 = CARTESIAN_POINT('Ctrl Pts',(-6.33463380664346,-13.3681754735787,
118.700728440715)) ;
#174485 = CARTESIAN_POINT('Ctrl Pts',(-6.32932953020779,-13.4419954208924,
118.789585923991)) ;
#174486 = CARTESIAN_POINT('Ctrl Pts',(-6.3266820427946,-13.4603090867706,
118.864513089041)) ;
#174487 = CARTESIAN_POINT('Ctrl Pts',(-6.32571868123136,-13.4607127643287,
118.902106572586)) ;
#174488 = CARTESIAN_POINT('Origin',(-6.39769283103919,-13.4878893170809,118.905700936849)) ;
#174489 = CARTESIAN_POINT('Ctrl Pts',(-6.32571868123136,-13.4607127643287,
118.902106572586)) ;
#174490 = CARTESIAN_POINT('Ctrl Pts',(-6.31605107706768,-13.4607136600768,
119.285257587653)) ;
#174491 = CARTESIAN_POINT('Ctrl Pts',(-6.30638347290399,-13.460714555825,
119.668408602719)) ;
#174492 = CARTESIAN_POINT('Ctrl Pts',(-6.29671586874031,-13.4607154515732,
120.051559617786)) ;
#174493 = CARTESIAN_POINT('Ctrl Pts',(-6.35381761696714,-13.3908270508895,
118.901830161472)) ;
#174494 = CARTESIAN_POINT('Ctrl Pts',(-6.34415001280346,-13.3908279466377,
119.284981176539)) ;
#174495 = CARTESIAN_POINT('Ctrl Pts',(-6.33448240863977,-13.3908288423858,
119.668132191605)) ;
#174496 = CARTESIAN_POINT('Ctrl Pts',(-6.32481480447609,-13.390829738134,
120.051283206672)) ;
#174497 = CARTESIAN_POINT('Ctrl Pts',(-6.42579176677498,-13.4180036036418,
118.905424525735)) ;
#174498 = CARTESIAN_POINT('Ctrl Pts',(-6.41612416261129,-13.4180044993899,
119.288575540802)) ;
#174499 = CARTESIAN_POINT('Ctrl Pts',(-6.4064565584476,-13.4180053951381,
119.671726555869)) ;
#174500 = CARTESIAN_POINT('Ctrl Pts',(-6.39678895428392,-13.4180062908863,
120.054877570935)) ;
#174501 = CARTESIAN_POINT('Ctrl Pts',(-6.49776591658281,-13.445180156394,
118.909018889999)) ;
#174502 = CARTESIAN_POINT('Ctrl Pts',(-6.48809831241913,-13.4451810521422,
119.292169905065)) ;
#174503 = CARTESIAN_POINT('Ctrl Pts',(-6.47843070825543,-13.4451819478904,
119.675320920132)) ;
#174504 = CARTESIAN_POINT('Ctrl Pts',(-6.46876310409176,-13.4451828436386,
120.058471935199)) ;
#174505 = CARTESIAN_POINT('Ctrl Pts',(-6.46966698084703,-13.5150658698332,
118.909295301113)) ;
#174506 = CARTESIAN_POINT('Ctrl Pts',(-6.45999937668335,-13.5150667655814,
119.29244631618)) ;
#174507 = CARTESIAN_POINT('Ctrl Pts',(-6.45033177251965,-13.5150676613296,
119.675597331246)) ;
#174508 = CARTESIAN_POINT('Ctrl Pts',(-6.44066416835598,-13.5150685570778,
120.058748346313)) ;
#174509 = CARTESIAN_POINT('Ctrl Pts',(-6.44156804511125,-13.5849515832724,
118.909571712227)) ;
#174510 = CARTESIAN_POINT('Ctrl Pts',(-6.43190044094756,-13.5849524790206,
119.292722727294)) ;
#174511 = CARTESIAN_POINT('Ctrl Pts',(-6.42223283678388,-13.5849533747688,
119.67587374236)) ;
#174512 = CARTESIAN_POINT('Ctrl Pts',(-6.4125652326202,-13.5849542705169,
120.059024757427)) ;
#174513 = CARTESIAN_POINT('Ctrl Pts',(-6.36959389530342,-13.5577750305201,
118.905977347964)) ;
#174514 = CARTESIAN_POINT('Ctrl Pts',(-6.35992629113973,-13.5577759262683,
119.28912836303)) ;
#174515 = CARTESIAN_POINT('Ctrl Pts',(-6.35025868697604,-13.5577768220165,
119.672279378097)) ;
#174516 = CARTESIAN_POINT('Ctrl Pts',(-6.34059108281237,-13.5577777177647,
120.055430393163)) ;
#174517 = CARTESIAN_POINT('Ctrl Pts',(-6.29761974549558,-13.5305984777679,
118.9023829837)) ;
#174518 = CARTESIAN_POINT('Ctrl Pts',(-6.2879521413319,-13.530599373516,119.285533998767)) ;
#174519 = CARTESIAN_POINT('Ctrl Pts',(-6.2782845371682,-13.5306002692642,
119.668685013833)) ;
#174520 = CARTESIAN_POINT('Ctrl Pts',(-6.26861693300453,-13.5306011650124,
120.0518360289)) ;
#174521 = CARTESIAN_POINT('Ctrl Pts',(-6.32571868123136,-13.4607127643287,
118.902106572586)) ;
#174522 = CARTESIAN_POINT('Ctrl Pts',(-6.31605107706768,-13.4607136600768,
119.285257587653)) ;
#174523 = CARTESIAN_POINT('Ctrl Pts',(-6.30638347290399,-13.460714555825,
119.668408602719)) ;
#174524 = CARTESIAN_POINT('Ctrl Pts',(-6.29671586874031,-13.4607154515732,
120.051559617786)) ;
#174525 = CARTESIAN_POINT('',(-6.29671586874031,-13.4607154515732,120.051559617786)) ;
#174526 = CARTESIAN_POINT('',(-6.32571868123136,-13.4607127643287,118.902106572586)) ;
#174527 = CARTESIAN_POINT('',(-6.36858491589695,-13.562875855635,120.056714214132)) ;
#174528 = CARTESIAN_POINT('Origin',(-6.36869001854814,-13.4878920043255,120.055153982049)) ;
#174529 = CARTESIAN_POINT('',(-6.36879525992063,-13.4129081530202,120.053593755801)) ;
#174530 = CARTESIAN_POINT('Origin',(-6.36869001854814,-13.4878920043255,120.055153982049)) ;
#174531 = CARTESIAN_POINT('Origin',(-6.36869001854814,-13.4878920043255,120.055153982049)) ;
#174532 = CARTESIAN_POINT('Ctrl Pts',(-6.29671586874031,-13.4607154515732,
120.051559617786)) ;
#174533 = CARTESIAN_POINT('Ctrl Pts',(-6.28976012863649,-13.4607154515732,
120.117372634366)) ;
#174534 = CARTESIAN_POINT('Ctrl Pts',(-6.25432280440511,-13.4607154515732,
120.250618929773)) ;
#174535 = CARTESIAN_POINT('Ctrl Pts',(-6.140310678484,-13.4607154515732,120.428143665408)) ;
#174536 = CARTESIAN_POINT('Ctrl Pts',(-5.97568444568715,-13.4607154515732,
120.563316664804)) ;
#174537 = CARTESIAN_POINT('Ctrl Pts',(-5.78097860437995,-13.4607154515732,
120.642680062699)) ;
#174538 = CARTESIAN_POINT('Ctrl Pts',(-5.57200742713837,-13.4607154515732,
120.662582212011)) ;
#174539 = CARTESIAN_POINT('Ctrl Pts',(-5.36445339342349,-13.4607154515732,
120.618928922871)) ;
#174540 = CARTESIAN_POINT('Ctrl Pts',(-5.18265709814504,-13.4607154515732,
120.514149932282)) ;
#174541 = CARTESIAN_POINT('Ctrl Pts',(-5.04597897894181,-13.4607154515732,
120.362468390451)) ;
#174542 = CARTESIAN_POINT('Ctrl Pts',(-4.96280251429834,-13.4607154515732,
120.177172641054)) ;
#174543 = CARTESIAN_POINT('Ctrl Pts',(-4.94189991062264,-13.4607154515732,
119.97127049429)) ;
#174544 = CARTESIAN_POINT('Ctrl Pts',(-4.98833964154144,-13.4607154515732,
119.767982106043)) ;
#174545 = CARTESIAN_POINT('Ctrl Pts',(-5.09419415993757,-13.4607154515732,
119.590012717272)) ;
#174546 = CARTESIAN_POINT('Ctrl Pts',(-5.24909308706152,-13.4607154515732,
119.449653557218)) ;
#174547 = CARTESIAN_POINT('Ctrl Pts',(-5.44305976208226,-13.4607154515732,
119.359449641273)) ;
#174548 = CARTESIAN_POINT('Ctrl Pts',(-5.65504200079475,-13.4607154515732,
119.332086511174)) ;
#174549 = CARTESIAN_POINT('Ctrl Pts',(-5.7931791132922,-13.4607154515732,
119.35624483207)) ;
#174550 = CARTESIAN_POINT('Ctrl Pts',(-5.85699395434883,-13.4607154515732,
119.377580402306)) ;
#174551 = CARTESIAN_POINT('Ctrl Pts',(-6.32481480447609,-13.390829738134,
120.051283206672)) ;
#174552 = CARTESIAN_POINT('Ctrl Pts',(-6.31782971791387,-13.390829738134,
120.119848720537)) ;
#174553 = CARTESIAN_POINT('Ctrl Pts',(-6.28144487665748,-13.390829738134,
120.258747479054)) ;
#174554 = CARTESIAN_POINT('Ctrl Pts',(-6.16339232015985,-13.390829738134,
120.444052341949)) ;
#174555 = CARTESIAN_POINT('Ctrl Pts',(-5.99245343202574,-13.390829738134,
120.585439812146)) ;
#174556 = CARTESIAN_POINT('Ctrl Pts',(-5.78996355328214,-13.390829738134,
120.668817841647)) ;
#174557 = CARTESIAN_POINT('Ctrl Pts',(-5.57238022299922,-13.390829738134,
120.690324475555)) ;
#174558 = CARTESIAN_POINT('Ctrl Pts',(-5.35602195824038,-13.390829738134,
120.6456373742)) ;
#174559 = CARTESIAN_POINT('Ctrl Pts',(-5.16625123437035,-13.390829738134,
120.53719608567)) ;
#174560 = CARTESIAN_POINT('Ctrl Pts',(-5.02328983170725,-13.390829738134,
120.379740742889)) ;
#174561 = CARTESIAN_POINT('Ctrl Pts',(-4.93592236622143,-13.390829738134,
120.187078915218)) ;
#174562 = CARTESIAN_POINT('Ctrl Pts',(-4.91333724036518,-13.390829738134,
119.972724565564)) ;
#174563 = CARTESIAN_POINT('Ctrl Pts',(-4.9609054258806,-13.390829738134,119.760840908715)) ;
#174564 = CARTESIAN_POINT('Ctrl Pts',(-5.07045935759837,-13.390829738134,
119.575103418979)) ;
#174565 = CARTESIAN_POINT('Ctrl Pts',(-5.23124591495442,-13.390829738134,
119.428351239574)) ;
#174566 = CARTESIAN_POINT('Ctrl Pts',(-5.43292307170264,-13.390829738134,
119.333686344338)) ;
#174567 = CARTESIAN_POINT('Ctrl Pts',(-5.65361322097818,-13.390829738134,
119.304398393744)) ;
#174568 = CARTESIAN_POINT('Ctrl Pts',(-5.79759063622383,-13.390829738134,
119.329041972343)) ;
#174569 = CARTESIAN_POINT('Ctrl Pts',(-5.86414369407748,-13.390829738134,
119.351023259812)) ;
#174570 = CARTESIAN_POINT('Ctrl Pts',(-6.39678895428392,-13.4180062908863,
120.054877570935)) ;
#174571 = CARTESIAN_POINT('Ctrl Pts',(-6.38928263696362,-13.4180062908863,
120.130502647309)) ;
#174572 = CARTESIAN_POINT('Ctrl Pts',(-6.34955616782122,-13.4180062908863,
120.28376286067)) ;
#174573 = CARTESIAN_POINT('Ctrl Pts',(-6.21989971795512,-13.4180062908863,
120.488415929437)) ;
#174574 = CARTESIAN_POINT('Ctrl Pts',(-6.03179411045853,-13.4180062908863,
120.644785453841)) ;
#174575 = CARTESIAN_POINT('Ctrl Pts',(-5.80872751617359,-13.4180062908863,
120.737274468594)) ;
#174576 = CARTESIAN_POINT('Ctrl Pts',(-5.56883823195218,-13.4180062908863,
120.76157980652)) ;
#174577 = CARTESIAN_POINT('Ctrl Pts',(-5.33010991940545,-13.4180062908863,
120.712891018481)) ;
#174578 = CARTESIAN_POINT('Ctrl Pts',(-5.12051933501212,-13.4180062908863,
120.593829347392)) ;
#174579 = CARTESIAN_POINT('Ctrl Pts',(-4.96240938664547,-13.4180062908863,
120.42059364654)) ;
#174580 = CARTESIAN_POINT('Ctrl Pts',(-4.8655073932878,-13.4180062908863,
120.208385475096)) ;
#174581 = CARTESIAN_POINT('Ctrl Pts',(-4.8399851269984,-13.4180062908863,
119.972081541481)) ;
#174582 = CARTESIAN_POINT('Ctrl Pts',(-4.89183506722446,-13.4180062908863,
119.738311675287)) ;
#174583 = CARTESIAN_POINT('Ctrl Pts',(-5.0121179866212,-13.4180062908863,
119.533204612542)) ;
#174584 = CARTESIAN_POINT('Ctrl Pts',(-5.18901219649234,-13.4180062908863,
119.370947050179)) ;
#174585 = CARTESIAN_POINT('Ctrl Pts',(-5.41115011774361,-13.4180062908863,
119.266014389055)) ;
#174586 = CARTESIAN_POINT('Ctrl Pts',(-5.65444326492148,-13.4180062908863,
119.233120285394)) ;
#174587 = CARTESIAN_POINT('Ctrl Pts',(-5.81329239186224,-13.4180062908863,
119.259903763088)) ;
#174588 = CARTESIAN_POINT('Ctrl Pts',(-5.88675024835855,-13.4180062908863,
119.283961627338)) ;
#174589 = CARTESIAN_POINT('Ctrl Pts',(-6.46876310409176,-13.4451828436386,
120.058471935199)) ;
#174590 = CARTESIAN_POINT('Ctrl Pts',(-6.46073555601338,-13.4451828436386,
120.141156574081)) ;
#174591 = CARTESIAN_POINT('Ctrl Pts',(-6.41766745898496,-13.4451828436386,
120.308778242286)) ;
#174592 = CARTESIAN_POINT('Ctrl Pts',(-6.27640711575039,-13.4451828436386,
120.532779516925)) ;
#174593 = CARTESIAN_POINT('Ctrl Pts',(-6.07113478889131,-13.4451828436386,
120.704131095535)) ;
#174594 = CARTESIAN_POINT('Ctrl Pts',(-5.82749147906504,-13.4451828436386,
120.805731095541)) ;
#174595 = CARTESIAN_POINT('Ctrl Pts',(-5.56529624090513,-13.4451828436386,
120.832835137485)) ;
#174596 = CARTESIAN_POINT('Ctrl Pts',(-5.30419788057051,-13.4451828436386,
120.780144662762)) ;
#174597 = CARTESIAN_POINT('Ctrl Pts',(-5.07478743565387,-13.4451828436386,
120.650462609113)) ;
#174598 = CARTESIAN_POINT('Ctrl Pts',(-4.90152894158368,-13.4451828436386,
120.461446550191)) ;
#174599 = CARTESIAN_POINT('Ctrl Pts',(-4.79509242035417,-13.4451828436386,
120.229692034974)) ;
#174600 = CARTESIAN_POINT('Ctrl Pts',(-4.76663301363163,-13.4451828436386,
119.971438517398)) ;
#174601 = CARTESIAN_POINT('Ctrl Pts',(-4.82276470856832,-13.4451828436386,
119.71578244186)) ;
#174602 = CARTESIAN_POINT('Ctrl Pts',(-4.95377661564404,-13.4451828436386,
119.491305806106)) ;
#174603 = CARTESIAN_POINT('Ctrl Pts',(-5.14677847803024,-13.4451828436386,
119.313542860783)) ;
#174604 = CARTESIAN_POINT('Ctrl Pts',(-5.38937716378458,-13.4451828436386,
119.198342433773)) ;
#174605 = CARTESIAN_POINT('Ctrl Pts',(-5.6552733088648,-13.4451828436386,
119.161842177043)) ;
#174606 = CARTESIAN_POINT('Ctrl Pts',(-5.82899414750066,-13.4451828436386,
119.190765553834)) ;
#174607 = CARTESIAN_POINT('Ctrl Pts',(-5.90935680263961,-13.4451828436386,
119.216899994865)) ;
#174608 = CARTESIAN_POINT('Ctrl Pts',(-6.44066416835598,-13.5150685570778,
120.058748346313)) ;
#174609 = CARTESIAN_POINT('Ctrl Pts',(-6.43266596673601,-13.5150685570778,
120.13868048791)) ;
#174610 = CARTESIAN_POINT('Ctrl Pts',(-6.39054538673258,-13.5150685570778,
120.300649693005)) ;
#174611 = CARTESIAN_POINT('Ctrl Pts',(-6.25332547407455,-13.5150685570778,
120.516870840384)) ;
#174612 = CARTESIAN_POINT('Ctrl Pts',(-6.05436580255273,-13.5150685570778,
120.682007948193)) ;
#174613 = CARTESIAN_POINT('Ctrl Pts',(-5.81850653016284,-13.5150685570778,
120.779593316593)) ;
#174614 = CARTESIAN_POINT('Ctrl Pts',(-5.56492344504428,-13.5150685570778,
120.805092873941)) ;
#174615 = CARTESIAN_POINT('Ctrl Pts',(-5.31262931575362,-13.5150685570778,
120.753436211433)) ;
#174616 = CARTESIAN_POINT('Ctrl Pts',(-5.09119329942855,-13.5150685570778,
120.627416455725)) ;
#174617 = CARTESIAN_POINT('Ctrl Pts',(-4.92421808881825,-13.5150685570778,
120.444174197752)) ;
#174618 = CARTESIAN_POINT('Ctrl Pts',(-4.82197256843109,-13.5150685570778,
120.219785760809)) ;
#174619 = CARTESIAN_POINT('Ctrl Pts',(-4.79519568388909,-13.5150685570778,
119.969984446124)) ;
#174620 = CARTESIAN_POINT('Ctrl Pts',(-4.85019892422917,-13.5150685570778,
119.722923639187)) ;
#174621 = CARTESIAN_POINT('Ctrl Pts',(-4.97751141798325,-13.5150685570778,
119.5062151044)) ;
#174622 = CARTESIAN_POINT('Ctrl Pts',(-5.16462565013734,-13.5150685570778,
119.334845178426)) ;
#174623 = CARTESIAN_POINT('Ctrl Pts',(-5.39951385416421,-13.5150685570778,
119.224105730708)) ;
#174624 = CARTESIAN_POINT('Ctrl Pts',(-5.65670208868136,-13.5150685570778,
119.189530294473)) ;
#174625 = CARTESIAN_POINT('Ctrl Pts',(-5.82458262456902,-13.5150685570778,
119.21796841356)) ;
#174626 = CARTESIAN_POINT('Ctrl Pts',(-5.90220706291095,-13.5150685570778,
119.243457137359)) ;
#174627 = CARTESIAN_POINT('Ctrl Pts',(-6.4125652326202,-13.5849542705169,
120.059024757427)) ;
#174628 = CARTESIAN_POINT('Ctrl Pts',(-6.40459637745865,-13.5849542705169,
120.136204401739)) ;
#174629 = CARTESIAN_POINT('Ctrl Pts',(-6.3634233144802,-13.5849542705169,
120.292521143724)) ;
#174630 = CARTESIAN_POINT('Ctrl Pts',(-6.23024383239871,-13.5849542705169,
120.500962163843)) ;
#174631 = CARTESIAN_POINT('Ctrl Pts',(-6.03759681621414,-13.5849542705169,
120.659884800851)) ;
#174632 = CARTESIAN_POINT('Ctrl Pts',(-5.80952158126064,-13.5849542705169,
120.753455537645)) ;
#174633 = CARTESIAN_POINT('Ctrl Pts',(-5.56455064918341,-13.5849542705169,
120.777350610398)) ;
#174634 = CARTESIAN_POINT('Ctrl Pts',(-5.32106075093673,-13.5849542705169,
120.726727760105)) ;
#174635 = CARTESIAN_POINT('Ctrl Pts',(-5.10759916320323,-13.5849542705169,
120.604370302337)) ;
#174636 = CARTESIAN_POINT('Ctrl Pts',(-4.94690723605281,-13.5849542705169,
120.426901845314)) ;
#174637 = CARTESIAN_POINT('Ctrl Pts',(-4.848852716508,-13.5849542705169,120.209879486644)) ;
#174638 = CARTESIAN_POINT('Ctrl Pts',(-4.82375835414656,-13.5849542705169,
119.96853037485)) ;
#174639 = CARTESIAN_POINT('Ctrl Pts',(-4.87763313989,-13.5849542705169,119.730064836515)) ;
#174640 = CARTESIAN_POINT('Ctrl Pts',(-5.00124622032246,-13.5849542705169,
119.521124402693)) ;
#174641 = CARTESIAN_POINT('Ctrl Pts',(-5.18247282224443,-13.5849542705169,
119.356147496069)) ;
#174642 = CARTESIAN_POINT('Ctrl Pts',(-5.40965054454383,-13.5849542705169,
119.249869027643)) ;
#174643 = CARTESIAN_POINT('Ctrl Pts',(-5.65813086849792,-13.5849542705169,
119.217218411902)) ;
#174644 = CARTESIAN_POINT('Ctrl Pts',(-5.82017110163739,-13.5849542705169,
119.245171273287)) ;
#174645 = CARTESIAN_POINT('Ctrl Pts',(-5.89505732318229,-13.5849542705169,
119.270014279853)) ;
#174646 = CARTESIAN_POINT('Ctrl Pts',(-6.34059108281237,-13.5577777177647,
120.055430393163)) ;
#174647 = CARTESIAN_POINT('Ctrl Pts',(-6.33314345840889,-13.5577777177647,
120.125550474967)) ;
#174648 = CARTESIAN_POINT('Ctrl Pts',(-6.29531202331647,-13.5577777177647,
120.267505762107)) ;
#174649 = CARTESIAN_POINT('Ctrl Pts',(-6.17373643460343,-13.5577777177647,
120.456598576355)) ;
#174650 = CARTESIAN_POINT('Ctrl Pts',(-5.99825613778136,-13.5577777177647,
120.600539159156)) ;
#174651 = CARTESIAN_POINT('Ctrl Pts',(-5.7907576183692,-13.5577777177647,
120.684998910698)) ;
#174652 = CARTESIAN_POINT('Ctrl Pts',(-5.56809264023046,-13.5577777177647,
120.706095279433)) ;
#174653 = CARTESIAN_POINT('Ctrl Pts',(-5.34697278977167,-13.5577777177647,
120.659474115823)) ;
#174654 = CARTESIAN_POINT('Ctrl Pts',(-5.15333106256147,-13.5577777177647,
120.547737040615)) ;
#174655 = CARTESIAN_POINT('Ctrl Pts',(-5.0077876811146,-13.5577777177647,
120.386048941664)) ;
#174656 = CARTESIAN_POINT('Ctrl Pts',(-4.91926768944164,-13.5577777177647,
120.188572926766)) ;
#174657 = CARTESIAN_POINT('Ctrl Pts',(-4.89711046751333,-13.5577777177647,
119.969173398933)) ;
#174658 = CARTESIAN_POINT('Ctrl Pts',(-4.94670349854615,-13.5577777177647,
119.752594069943)) ;
#174659 = CARTESIAN_POINT('Ctrl Pts',(-5.05958759129963,-13.5577777177647,
119.563023209129)) ;
#174660 = CARTESIAN_POINT('Ctrl Pts',(-5.22470654070653,-13.5577777177647,
119.413551685465)) ;
#174661 = CARTESIAN_POINT('Ctrl Pts',(-5.43142349850286,-13.5577777177647,
119.317540982926)) ;
#174662 = CARTESIAN_POINT('Ctrl Pts',(-5.65730082455462,-13.5577777177647,
119.288496520253)) ;
#174663 = CARTESIAN_POINT('Ctrl Pts',(-5.80446934599897,-13.5577777177647,
119.314309482542)) ;
#174664 = CARTESIAN_POINT('Ctrl Pts',(-5.87245076890124,-13.5577777177647,
119.337075912327)) ;
#174665 = CARTESIAN_POINT('Ctrl Pts',(-6.26861693300453,-13.5306011650124,
120.0518360289)) ;
#174666 = CARTESIAN_POINT('Ctrl Pts',(-6.26169053935913,-13.5306011650124,
120.114896548195)) ;
#174667 = CARTESIAN_POINT('Ctrl Pts',(-6.22720073215273,-13.5306011650124,
120.242490380491)) ;
#174668 = CARTESIAN_POINT('Ctrl Pts',(-6.11722903680817,-13.5306011650124,
120.412234988866)) ;
#174669 = CARTESIAN_POINT('Ctrl Pts',(-5.95891545934857,-13.5306011650124,
120.541193517462)) ;
#174670 = CARTESIAN_POINT('Ctrl Pts',(-5.77199365547776,-13.5306011650124,
120.616542283751)) ;
#174671 = CARTESIAN_POINT('Ctrl Pts',(-5.57163463127751,-13.5306011650124,
120.634839948468)) ;
#174672 = CARTESIAN_POINT('Ctrl Pts',(-5.37288482860661,-13.5306011650124,
120.592220471542)) ;
#174673 = CARTESIAN_POINT('Ctrl Pts',(-5.19906296191971,-13.5306011650124,
120.491103778893)) ;
#174674 = CARTESIAN_POINT('Ctrl Pts',(-5.06866812617638,-13.5306011650124,
120.345196038013)) ;
#174675 = CARTESIAN_POINT('Ctrl Pts',(-4.98968266237526,-13.5306011650124,
120.167266366889)) ;
#174676 = CARTESIAN_POINT('Ctrl Pts',(-4.9704625808801,-13.5306011650124,
119.969816423016)) ;
#174677 = CARTESIAN_POINT('Ctrl Pts',(-5.01577385720228,-13.5306011650124,
119.77512330337)) ;
#174678 = CARTESIAN_POINT('Ctrl Pts',(-5.11792896227678,-13.5306011650124,
119.604922015565)) ;
#174679 = CARTESIAN_POINT('Ctrl Pts',(-5.26694025916861,-13.5306011650124,
119.470955874861)) ;
#174680 = CARTESIAN_POINT('Ctrl Pts',(-5.45319645246189,-13.5306011650124,
119.385212938208)) ;
#174681 = CARTESIAN_POINT('Ctrl Pts',(-5.6564707806113,-13.5306011650124,
119.359774628604)) ;
#174682 = CARTESIAN_POINT('Ctrl Pts',(-5.78876759036056,-13.5306011650124,
119.383447691797)) ;
#174683 = CARTESIAN_POINT('Ctrl Pts',(-5.84984421462017,-13.5306011650124,
119.4041375448)) ;
#174684 = CARTESIAN_POINT('Ctrl Pts',(-6.29671586874031,-13.4607154515732,
120.051559617786)) ;
#174685 = CARTESIAN_POINT('Ctrl Pts',(-6.28976012863649,-13.4607154515732,
120.117372634366)) ;
#174686 = CARTESIAN_POINT('Ctrl Pts',(-6.25432280440511,-13.4607154515732,
120.250618929773)) ;
#174687 = CARTESIAN_POINT('Ctrl Pts',(-6.140310678484,-13.4607154515732,120.428143665408)) ;
#174688 = CARTESIAN_POINT('Ctrl Pts',(-5.97568444568715,-13.4607154515732,
120.563316664804)) ;
#174689 = CARTESIAN_POINT('Ctrl Pts',(-5.78097860437995,-13.4607154515732,
120.642680062699)) ;
#174690 = CARTESIAN_POINT('Ctrl Pts',(-5.57200742713837,-13.4607154515732,
120.662582212011)) ;
#174691 = CARTESIAN_POINT('Ctrl Pts',(-5.36445339342349,-13.4607154515732,
120.618928922871)) ;
#174692 = CARTESIAN_POINT('Ctrl Pts',(-5.18265709814504,-13.4607154515732,
120.514149932282)) ;
#174693 = CARTESIAN_POINT('Ctrl Pts',(-5.04597897894181,-13.4607154515732,
120.362468390451)) ;
#174694 = CARTESIAN_POINT('Ctrl Pts',(-4.96280251429834,-13.4607154515732,
120.177172641054)) ;
#174695 = CARTESIAN_POINT('Ctrl Pts',(-4.94189991062264,-13.4607154515732,
119.97127049429)) ;
#174696 = CARTESIAN_POINT('Ctrl Pts',(-4.98833964154144,-13.4607154515732,
119.767982106043)) ;
#174697 = CARTESIAN_POINT('Ctrl Pts',(-5.09419415993757,-13.4607154515732,
119.590012717272)) ;
#174698 = CARTESIAN_POINT('Ctrl Pts',(-5.24909308706152,-13.4607154515732,
119.449653557218)) ;
#174699 = CARTESIAN_POINT('Ctrl Pts',(-5.44305976208226,-13.4607154515732,
119.359449641273)) ;
#174700 = CARTESIAN_POINT('Ctrl Pts',(-5.65504200079475,-13.4607154515732,
119.332086511174)) ;
#174701 = CARTESIAN_POINT('Ctrl Pts',(-5.7931791132922,-13.4607154515732,
119.35624483207)) ;
#174702 = CARTESIAN_POINT('Ctrl Pts',(-5.85699395434883,-13.4607154515732,
119.377580402306)) ;
#174703 = CARTESIAN_POINT('Ctrl Pts',(-6.29671586874031,-13.4607154515732,
120.051559617786)) ;
#174704 = CARTESIAN_POINT('Ctrl Pts',(-6.28976012863649,-13.4607154515732,
120.117372634366)) ;
#174705 = CARTESIAN_POINT('Ctrl Pts',(-6.25432280440511,-13.4607154515732,
120.250618929773)) ;
#174706 = CARTESIAN_POINT('Ctrl Pts',(-6.140310678484,-13.4607154515732,120.428143665408)) ;
#174707 = CARTESIAN_POINT('Ctrl Pts',(-5.97568444568715,-13.4607154515732,
120.563316664804)) ;
#174708 = CARTESIAN_POINT('Ctrl Pts',(-5.78097860437995,-13.4607154515732,
120.642680062699)) ;
#174709 = CARTESIAN_POINT('Ctrl Pts',(-5.57200742713837,-13.4607154515732,
120.662582212011)) ;
#174710 = CARTESIAN_POINT('Ctrl Pts',(-5.36445339342349,-13.4607154515732,
120.618928922871)) ;
#174711 = CARTESIAN_POINT('Ctrl Pts',(-5.18265709814504,-13.4607154515732,
120.514149932282)) ;
#174712 = CARTESIAN_POINT('Ctrl Pts',(-5.04597897894181,-13.4607154515732,
120.362468390451)) ;
#174713 = CARTESIAN_POINT('Ctrl Pts',(-4.96280251429834,-13.4607154515732,
120.177172641054)) ;
#174714 = CARTESIAN_POINT('Ctrl Pts',(-4.94189991062264,-13.4607154515732,
119.97127049429)) ;
#174715 = CARTESIAN_POINT('Ctrl Pts',(-4.98833964154144,-13.4607154515732,
119.767982106043)) ;
#174716 = CARTESIAN_POINT('Ctrl Pts',(-5.09419415993757,-13.4607154515732,
119.590012717272)) ;
#174717 = CARTESIAN_POINT('Ctrl Pts',(-5.24909308706152,-13.4607154515732,
119.449653557218)) ;
#174718 = CARTESIAN_POINT('Ctrl Pts',(-5.44305976208226,-13.4607154515732,
119.359449641273)) ;
#174719 = CARTESIAN_POINT('Ctrl Pts',(-5.65504200079475,-13.4607154515732,
119.332086511174)) ;
#174720 = CARTESIAN_POINT('Ctrl Pts',(-5.7931791132922,-13.4607154515732,
119.35624483207)) ;
#174721 = CARTESIAN_POINT('Ctrl Pts',(-5.85699395434883,-13.4607154515732,
119.377580402306)) ;
#174722 = CARTESIAN_POINT('Origin',(-29.5801015914784,-13.4878920043255,112.829331611621)) ;
#174723 = CARTESIAN_POINT('',(-29.6364905070076,-13.4607154515732,112.659288401873)) ;
#174724 = CARTESIAN_POINT('Origin',(-29.6138839527266,-13.4878920043255,112.726350034346)) ;
#174725 = CARTESIAN_POINT('Ctrl Pts',(-29.1489187358159,-13.1500241806476,
113.370642219953)) ;
#174726 = CARTESIAN_POINT('Ctrl Pts',(-29.1262302782877,-13.1683184483544,
113.301536839092)) ;
#174727 = CARTESIAN_POINT('Ctrl Pts',(-29.0524264348783,-13.1683184483544,
113.32576788081)) ;
#174728 = CARTESIAN_POINT('Ctrl Pts',(-28.9786225914689,-13.1683184483544,
113.349998922528)) ;
#174729 = CARTESIAN_POINT('Ctrl Pts',(-29.0013110489971,-13.1500241806476,
113.41910430339)) ;
#174730 = CARTESIAN_POINT('Ctrl Pts',(-29.0239995065253,-13.1317299129408,
113.488209684252)) ;
#174731 = CARTESIAN_POINT('Ctrl Pts',(-29.0978033499347,-13.1317299129408,
113.463978642533)) ;
#174732 = CARTESIAN_POINT('Ctrl Pts',(-29.1716071933441,-13.1317299129408,
113.439747600815)) ;
#174733 = CARTESIAN_POINT('Ctrl Pts',(-29.1489187358159,-13.1500241806476,
113.370642219953)) ;
#174734 = CARTESIAN_POINT('Ctrl Pts',(-29.1481908350552,-13.1438552129684,
113.369207785981)) ;
#174735 = CARTESIAN_POINT('Ctrl Pts',(-29.1255364269104,-13.1625827638083,
113.300206114203)) ;
#174736 = CARTESIAN_POINT('Ctrl Pts',(-29.0517325842656,-13.1625827713816,
113.32443715825)) ;
#174737 = CARTESIAN_POINT('Ctrl Pts',(-28.9779287416207,-13.1625827789549,
113.348668202297)) ;
#174738 = CARTESIAN_POINT('Ctrl Pts',(-29.0005831497655,-13.143855228115,
113.417669874074)) ;
#174739 = CARTESIAN_POINT('Ctrl Pts',(-29.0232375579103,-13.1251276772751,
113.486671545852)) ;
#174740 = CARTESIAN_POINT('Ctrl Pts',(-29.0970414005551,-13.1251276697018,
113.462440501806)) ;
#174741 = CARTESIAN_POINT('Ctrl Pts',(-29.1708452432,-13.1251276621286,113.438209457759)) ;
#174742 = CARTESIAN_POINT('Ctrl Pts',(-29.1481908350552,-13.1438552129684,
113.369207785981)) ;
#174743 = CARTESIAN_POINT('Ctrl Pts',(-29.1363218176444,-13.045472096163,
113.345565010115)) ;
#174744 = CARTESIAN_POINT('Ctrl Pts',(-29.1142262333781,-13.0710887780094,
113.27826542217)) ;
#174745 = CARTESIAN_POINT('Ctrl Pts',(-29.0404223713575,-13.0710886158947,
113.302496407201)) ;
#174746 = CARTESIAN_POINT('Ctrl Pts',(-28.9666185093369,-13.07108845378,113.326727392232)) ;
#174747 = CARTESIAN_POINT('Ctrl Pts',(-28.9887140936032,-13.0454717719336,
113.394026980177)) ;
#174748 = CARTESIAN_POINT('Ctrl Pts',(-29.0108096778695,-13.0198550900872,
113.461326568122)) ;
#174749 = CARTESIAN_POINT('Ctrl Pts',(-29.0846135398901,-13.0198552522019,
113.437095583091)) ;
#174750 = CARTESIAN_POINT('Ctrl Pts',(-29.1584174019107,-13.0198554143166,
113.41286459806)) ;
#174751 = CARTESIAN_POINT('Ctrl Pts',(-29.1363218176444,-13.045472096163,
113.345565010115)) ;
#174752 = CARTESIAN_POINT('Ctrl Pts',(-29.1042713188461,-12.8597742993635,
113.272543581875)) ;
#174753 = CARTESIAN_POINT('Ctrl Pts',(-29.0838803914435,-12.8983625293638,
113.210436108561)) ;
#174754 = CARTESIAN_POINT('Ctrl Pts',(-29.0100765562992,-12.8983626007157,
113.234667175454)) ;
#174755 = CARTESIAN_POINT('Ctrl Pts',(-28.9362727211549,-12.8983626720675,
113.258898242346)) ;
#174756 = CARTESIAN_POINT('Ctrl Pts',(-28.9566636485575,-12.8597744420672,
113.32100571566)) ;
#174757 = CARTESIAN_POINT('Ctrl Pts',(-28.97705457596,-12.821186212067,113.383113188974)) ;
#174758 = CARTESIAN_POINT('Ctrl Pts',(-29.0508584111043,-12.8211861407151,
113.358882122082)) ;
#174759 = CARTESIAN_POINT('Ctrl Pts',(-29.1246622462486,-12.8211860693632,
113.334651055189)) ;
#174760 = CARTESIAN_POINT('Ctrl Pts',(-29.1042713188461,-12.8597742993635,
113.272543581875)) ;
#174761 = CARTESIAN_POINT('Ctrl Pts',(-29.0373324850924,-12.6327839415056,
113.104016096402)) ;
#174762 = CARTESIAN_POINT('Ctrl Pts',(-29.020854571842,-12.6872840912264,
113.053827030836)) ;
#174763 = CARTESIAN_POINT('Ctrl Pts',(-28.9470507251008,-12.6872840678826,
113.078058062406)) ;
#174764 = CARTESIAN_POINT('Ctrl Pts',(-28.8732468783596,-12.6872840445389,
113.102289093976)) ;
#174765 = CARTESIAN_POINT('Ctrl Pts',(-28.88972479161,-12.6327838948181,113.152478159542)) ;
#174766 = CARTESIAN_POINT('Ctrl Pts',(-28.9062027048603,-12.5782837450973,
113.202667225107)) ;
#174767 = CARTESIAN_POINT('Ctrl Pts',(-28.9800065516015,-12.578283768441,
113.178436193537)) ;
#174768 = CARTESIAN_POINT('Ctrl Pts',(-29.0538103983427,-12.5782837917848,
113.154205161967)) ;
#174769 = CARTESIAN_POINT('Ctrl Pts',(-29.0373324850924,-12.6327839415056,
113.104016096402)) ;
#174770 = CARTESIAN_POINT('Ctrl Pts',(-28.9535211541043,-12.4610780963096,
112.884187309328)) ;
#174771 = CARTESIAN_POINT('Ctrl Pts',(-28.9421376564659,-12.5276451730564,
112.849515012138)) ;
#174772 = CARTESIAN_POINT('Ctrl Pts',(-28.8683338107351,-12.52764517241,112.873746046785)) ;
#174773 = CARTESIAN_POINT('Ctrl Pts',(-28.7945299650043,-12.5276451717636,
112.897977081433)) ;
#174774 = CARTESIAN_POINT('Ctrl Pts',(-28.8059134626427,-12.4610780950169,
112.932649378623)) ;
#174775 = CARTESIAN_POINT('Ctrl Pts',(-28.817296960281,-12.3945110182701,
112.967321675813)) ;
#174776 = CARTESIAN_POINT('Ctrl Pts',(-28.8911008060119,-12.3945110189165,
112.943090641166)) ;
#174777 = CARTESIAN_POINT('Ctrl Pts',(-28.9649046517427,-12.3945110195628,
112.918859606518)) ;
#174778 = CARTESIAN_POINT('Ctrl Pts',(-28.9535211541043,-12.4610780963096,
112.884187309328)) ;
#174779 = CARTESIAN_POINT('Ctrl Pts',(-28.8575946335874,-12.3578311300529,
112.627637093626)) ;
#174780 = CARTESIAN_POINT('Ctrl Pts',(-28.8521552951405,-12.431704833434,
112.611069745946)) ;
#174781 = CARTESIAN_POINT('Ctrl Pts',(-28.7783514457022,-12.4317048270663,
112.635300769301)) ;
#174782 = CARTESIAN_POINT('Ctrl Pts',(-28.7045475962638,-12.4317048206985,
112.659531792655)) ;
#174783 = CARTESIAN_POINT('Ctrl Pts',(-28.7099869347107,-12.3578311173174,
112.676099140336)) ;
#174784 = CARTESIAN_POINT('Ctrl Pts',(-28.7154262731576,-12.2839574139363,
112.692666488017)) ;
#174785 = CARTESIAN_POINT('Ctrl Pts',(-28.7892301225959,-12.283957420304,
112.668435464662)) ;
#174786 = CARTESIAN_POINT('Ctrl Pts',(-28.8630339720343,-12.2839574266718,
112.644204441307)) ;
#174787 = CARTESIAN_POINT('Ctrl Pts',(-28.8575946335874,-12.3578311300529,
112.627637093626)) ;
#174788 = CARTESIAN_POINT('Ctrl Pts',(-28.7572250300145,-12.3309709098726,
112.357185420699)) ;
#174789 = CARTESIAN_POINT('Ctrl Pts',(-28.7580561715402,-12.4068262743209,
112.359716943198)) ;
#174790 = CARTESIAN_POINT('Ctrl Pts',(-28.684252320216,-12.4068262750749,
112.383947960808)) ;
#174791 = CARTESIAN_POINT('Ctrl Pts',(-28.6104484688917,-12.4068262758288,
112.408178978419)) ;
#174792 = CARTESIAN_POINT('Ctrl Pts',(-28.609617327366,-12.3309709113806,
112.405647455921)) ;
#174793 = CARTESIAN_POINT('Ctrl Pts',(-28.6087861858402,-12.2551155469323,
112.403115933422)) ;
#174794 = CARTESIAN_POINT('Ctrl Pts',(-28.6825900371645,-12.2551155461783,
112.378884915812)) ;
#174795 = CARTESIAN_POINT('Ctrl Pts',(-28.7563938884887,-12.2551155454244,
112.354653898201)) ;
#174796 = CARTESIAN_POINT('Ctrl Pts',(-28.7572250300145,-12.3309709098726,
112.357185420699)) ;
#174797 = CARTESIAN_POINT('Ctrl Pts',(-28.6569634591251,-12.3817310335918,
112.087380599263)) ;
#174798 = CARTESIAN_POINT('Ctrl Pts',(-28.6640600261264,-12.4541523823842,
112.108995596646)) ;
#174799 = CARTESIAN_POINT('Ctrl Pts',(-28.5902561722792,-12.4541523921254,
112.133226606572)) ;
#174800 = CARTESIAN_POINT('Ctrl Pts',(-28.5164523184319,-12.4541524018665,
112.157457616498)) ;
#174801 = CARTESIAN_POINT('Ctrl Pts',(-28.5093557514307,-12.3817310530741,
112.135842619115)) ;
#174802 = CARTESIAN_POINT('Ctrl Pts',(-28.5022591844293,-12.3093097042818,
112.114227621731)) ;
#174803 = CARTESIAN_POINT('Ctrl Pts',(-28.5760630382766,-12.3093096945406,
112.089996611805)) ;
#174804 = CARTESIAN_POINT('Ctrl Pts',(-28.6498668921238,-12.3093096847995,
112.065765601879)) ;
#174805 = CARTESIAN_POINT('Ctrl Pts',(-28.6569634591251,-12.3817310335918,
112.087380599263)) ;
#174806 = CARTESIAN_POINT('Ctrl Pts',(-28.564509082064,-12.5067458714326,
111.841211648264)) ;
#174807 = CARTESIAN_POINT('Ctrl Pts',(-28.5773378755298,-12.5705432422448,
111.880286082408)) ;
#174808 = CARTESIAN_POINT('Ctrl Pts',(-28.5035340207076,-12.57054326527,111.904517089365)) ;
#174809 = CARTESIAN_POINT('Ctrl Pts',(-28.4297301658854,-12.5705432882951,
111.928748096321)) ;
#174810 = CARTESIAN_POINT('Ctrl Pts',(-28.4169013724195,-12.5067459174828,
111.889673662177)) ;
#174811 = CARTESIAN_POINT('Ctrl Pts',(-28.4040725789537,-12.4429485466705,
111.850599228033)) ;
#174812 = CARTESIAN_POINT('Ctrl Pts',(-28.4778764337759,-12.4429485236454,
111.826368221076)) ;
#174813 = CARTESIAN_POINT('Ctrl Pts',(-28.5516802885981,-12.4429485006203,
111.80213721412)) ;
#174814 = CARTESIAN_POINT('Ctrl Pts',(-28.564509082064,-12.5067458714326,
111.841211648264)) ;
#174815 = CARTESIAN_POINT('Ctrl Pts',(-28.4851946394043,-12.6971218835384,
111.635119922408)) ;
#174816 = CARTESIAN_POINT('Ctrl Pts',(-28.5028453351627,-12.7477196021645,
111.688881092751)) ;
#174817 = CARTESIAN_POINT('Ctrl Pts',(-28.4290414807966,-12.7477196406968,
111.713112101097)) ;
#174818 = CARTESIAN_POINT('Ctrl Pts',(-28.3552376264306,-12.7477196792291,
111.737343109443)) ;
#174819 = CARTESIAN_POINT('Ctrl Pts',(-28.3375869306722,-12.697121960603,
111.6835819391)) ;
#174820 = CARTESIAN_POINT('Ctrl Pts',(-28.3199362349139,-12.646524241977,
111.629820768757)) ;
#174821 = CARTESIAN_POINT('Ctrl Pts',(-28.3937400892799,-12.6465242034447,
111.605589760411)) ;
#174822 = CARTESIAN_POINT('Ctrl Pts',(-28.4675439436459,-12.6465241649123,
111.581358752065)) ;
#174823 = CARTESIAN_POINT('Ctrl Pts',(-28.4851946394043,-12.6971218835384,
111.635119922408)) ;
#174824 = CARTESIAN_POINT('Ctrl Pts',(-28.4241475022264,-12.9391053860727,
111.48464558118)) ;
#174825 = CARTESIAN_POINT('Ctrl Pts',(-28.4453520755906,-12.9728813246928,
111.549231289129)) ;
#174826 = CARTESIAN_POINT('Ctrl Pts',(-28.3715482236367,-12.9728813789312,
111.573462304821)) ;
#174827 = CARTESIAN_POINT('Ctrl Pts',(-28.2977443716827,-12.9728814331696,
111.597693320514)) ;
#174828 = CARTESIAN_POINT('Ctrl Pts',(-28.2765397983185,-12.9391054945495,
111.533107612566)) ;
#174829 = CARTESIAN_POINT('Ctrl Pts',(-28.2553352249542,-12.9053295559293,
111.468521904618)) ;
#174830 = CARTESIAN_POINT('Ctrl Pts',(-28.3291390769082,-12.9053295016909,
111.444290888925)) ;
#174831 = CARTESIAN_POINT('Ctrl Pts',(-28.4029429288622,-12.9053294474525,
111.420059873232)) ;
#174832 = CARTESIAN_POINT('Ctrl Pts',(-28.4241475022264,-12.9391053860727,
111.48464558118)) ;
#174833 = CARTESIAN_POINT('Ctrl Pts',(-28.3849524033199,-13.2152764852227,
111.400718831589)) ;
#174834 = CARTESIAN_POINT('Ctrl Pts',(-28.4081905270802,-13.2298195844166,
111.471498405773)) ;
#174835 = CARTESIAN_POINT('Ctrl Pts',(-28.3343866794691,-13.2298196519975,
111.495729434694)) ;
#174836 = CARTESIAN_POINT('Ctrl Pts',(-28.260582831858,-13.2298197195784,
111.519960463614)) ;
#174837 = CARTESIAN_POINT('Ctrl Pts',(-28.2373447080977,-13.2152766203844,
111.44918088943)) ;
#174838 = CARTESIAN_POINT('Ctrl Pts',(-28.2141065843374,-13.2007335211905,
111.378401315245)) ;
#174839 = CARTESIAN_POINT('Ctrl Pts',(-28.2879104319485,-13.2007334536096,
111.354170286325)) ;
#174840 = CARTESIAN_POINT('Ctrl Pts',(-28.3617142795596,-13.2007333860287,
111.329939257405)) ;
#174841 = CARTESIAN_POINT('Ctrl Pts',(-28.3849524033199,-13.2152764852227,
111.400718831589)) ;
#174842 = CARTESIAN_POINT('Ctrl Pts',(-28.3695728344553,-13.505784356226,
111.389304759768)) ;
#174843 = CARTESIAN_POINT('Ctrl Pts',(-28.3931852419853,-13.5000660445819,
111.461224341778)) ;
#174844 = CARTESIAN_POINT('Ctrl Pts',(-28.3193814002774,-13.5000661208921,
111.485455388679)) ;
#174845 = CARTESIAN_POINT('Ctrl Pts',(-28.2455775585696,-13.5000661972022,
111.50968643558)) ;
#174846 = CARTESIAN_POINT('Ctrl Pts',(-28.2219651510396,-13.5057845088464,
111.437766853569)) ;
#174847 = CARTESIAN_POINT('Ctrl Pts',(-28.1983527435096,-13.5115028204905,
111.365847271559)) ;
#174848 = CARTESIAN_POINT('Ctrl Pts',(-28.2721565852175,-13.5115027441803,
111.341616224659)) ;
#174849 = CARTESIAN_POINT('Ctrl Pts',(-28.3459604269253,-13.5115026678702,
111.317385177758)) ;
#174850 = CARTESIAN_POINT('Ctrl Pts',(-28.3695728344553,-13.505784356226,
111.389304759768)) ;
#174851 = CARTESIAN_POINT('Ctrl Pts',(-28.3785666018913,-13.7916119971123,
111.452340850324)) ;
#174852 = CARTESIAN_POINT('Ctrl Pts',(-28.4008480409797,-13.7659297998844,
111.520206517047)) ;
#174853 = CARTESIAN_POINT('Ctrl Pts',(-28.3270442065118,-13.7659298799449,
111.544437585999)) ;
#174854 = CARTESIAN_POINT('Ctrl Pts',(-28.2532403720439,-13.7659299600053,
111.568668654952)) ;
#174855 = CARTESIAN_POINT('Ctrl Pts',(-28.2309589329554,-13.7916121572332,
111.500802988229)) ;
#174856 = CARTESIAN_POINT('Ctrl Pts',(-28.2086774938669,-13.817294354461,
111.432937321506)) ;
#174857 = CARTESIAN_POINT('Ctrl Pts',(-28.2824813283349,-13.8172942744006,
111.408706252554)) ;
#174858 = CARTESIAN_POINT('Ctrl Pts',(-28.3562851628028,-13.8172941943401,
111.384475183601)) ;
#174859 = CARTESIAN_POINT('Ctrl Pts',(-28.3785666018913,-13.7916119971123,
111.452340850324)) ;
#174860 = CARTESIAN_POINT('Ctrl Pts',(-28.4102051428863,-14.0480477215918,
111.583997783673)) ;
#174861 = CARTESIAN_POINT('Ctrl Pts',(-28.4295796916699,-14.00442476396,111.643009531454)) ;
#174862 = CARTESIAN_POINT('Ctrl Pts',(-28.3557758644425,-14.0044248376781,
111.66724062246)) ;
#174863 = CARTESIAN_POINT('Ctrl Pts',(-28.2819720372152,-14.0044249113963,
111.691471713466)) ;
#174864 = CARTESIAN_POINT('Ctrl Pts',(-28.2625974884316,-14.0480478690281,
111.632459965685)) ;
#174865 = CARTESIAN_POINT('Ctrl Pts',(-28.2432229396479,-14.0916708266599,
111.573448217904)) ;
#174866 = CARTESIAN_POINT('Ctrl Pts',(-28.3170267668753,-14.0916707529417,
111.549217126898)) ;
#174867 = CARTESIAN_POINT('Ctrl Pts',(-28.3908305941027,-14.0916706792236,
111.524986035892)) ;
#174868 = CARTESIAN_POINT('Ctrl Pts',(-28.4102051428863,-14.0480477215918,
111.583997783673)) ;
#174869 = CARTESIAN_POINT('Ctrl Pts',(-28.4617096973959,-14.2608003622883,
111.776342484654)) ;
#174870 = CARTESIAN_POINT('Ctrl Pts',(-28.4767827056386,-14.2022602348381,
111.822252433888)) ;
#174871 = CARTESIAN_POINT('Ctrl Pts',(-28.4029788852957,-14.2022602957698,
111.846483545863)) ;
#174872 = CARTESIAN_POINT('Ctrl Pts',(-28.3291750649528,-14.2022603567015,
111.870714657838)) ;
#174873 = CARTESIAN_POINT('Ctrl Pts',(-28.3141020567101,-14.2608004841518,
111.824804708603)) ;
#174874 = CARTESIAN_POINT('Ctrl Pts',(-28.2990290484674,-14.319340611602,
111.778894759369)) ;
#174875 = CARTESIAN_POINT('Ctrl Pts',(-28.3728328688103,-14.3193405506703,
111.754663647394)) ;
#174876 = CARTESIAN_POINT('Ctrl Pts',(-28.4466366891532,-14.3193404897386,
111.730432535419)) ;
#174877 = CARTESIAN_POINT('Ctrl Pts',(-28.4617096973959,-14.2608003622883,
111.776342484654)) ;
#174878 = CARTESIAN_POINT('Ctrl Pts',(-28.5285966908039,-14.4130997833176,
112.015523906653)) ;
#174879 = CARTESIAN_POINT('Ctrl Pts',(-28.5382883279063,-14.3438411557226,
112.045043067585)) ;
#174880 = CARTESIAN_POINT('Ctrl Pts',(-28.464484513117,-14.3438411966561,
112.069274196476)) ;
#174881 = CARTESIAN_POINT('Ctrl Pts',(-28.3906806983278,-14.3438412375897,
112.093505325366)) ;
#174882 = CARTESIAN_POINT('Ctrl Pts',(-28.3809890612254,-14.4130998651847,
112.063986164433)) ;
#174883 = CARTESIAN_POINT('Ctrl Pts',(-28.371297424123,-14.4823584927798,
112.034467003501)) ;
#174884 = CARTESIAN_POINT('Ctrl Pts',(-28.4451012389122,-14.4823584518462,
112.010235874611)) ;
#174885 = CARTESIAN_POINT('Ctrl Pts',(-28.5189050537015,-14.4823584109127,
111.98600474572)) ;
#174886 = CARTESIAN_POINT('Ctrl Pts',(-28.5285966908039,-14.4130997833176,
112.015523906653)) ;
#174887 = CARTESIAN_POINT('Ctrl Pts',(-28.6055369658778,-14.494276858583,
112.285430331193)) ;
#174888 = CARTESIAN_POINT('Ctrl Pts',(-28.6091354502607,-14.419248986888,
112.296390731991)) ;
#174889 = CARTESIAN_POINT('Ctrl Pts',(-28.5353316390701,-14.4192490024428,
112.320621871842)) ;
#174890 = CARTESIAN_POINT('Ctrl Pts',(-28.4615278278796,-14.4192490179976,
112.344853011694)) ;
#174891 = CARTESIAN_POINT('Ctrl Pts',(-28.4579293434966,-14.4942768896926,
112.333892610895)) ;
#174892 = CARTESIAN_POINT('Ctrl Pts',(-28.4543308591137,-14.5693047613875,
112.322932210097)) ;
#174893 = CARTESIAN_POINT('Ctrl Pts',(-28.5281346703043,-14.5693047458327,
112.298701070246)) ;
#174894 = CARTESIAN_POINT('Ctrl Pts',(-28.6019384814949,-14.569304730278,
112.274469930394)) ;
#174895 = CARTESIAN_POINT('Ctrl Pts',(-28.6055369658778,-14.494276858583,
112.285430331193)) ;
#174896 = CARTESIAN_POINT('Ctrl Pts',(-28.6858402113565,-14.4979516536895,
112.565480733191)) ;
#174897 = CARTESIAN_POINT('Ctrl Pts',(-28.6831038105203,-14.4225568687656,
112.557146095696)) ;
#174898 = CARTESIAN_POINT('Ctrl Pts',(-28.6093000001973,-14.4225568559479,
112.58137723819)) ;
#174899 = CARTESIAN_POINT('Ctrl Pts',(-28.5354961898742,-14.4225568431301,
112.605608380683)) ;
#174900 = CARTESIAN_POINT('Ctrl Pts',(-28.5382325907104,-14.497951628054,
112.613943018178)) ;
#174901 = CARTESIAN_POINT('Ctrl Pts',(-28.5409689915465,-14.5733464129779,
112.622277655674)) ;
#174902 = CARTESIAN_POINT('Ctrl Pts',(-28.6147728018696,-14.5733464257956,
112.59804651318)) ;
#174903 = CARTESIAN_POINT('Ctrl Pts',(-28.6885766121926,-14.5733464386134,
112.573815370686)) ;
#174904 = CARTESIAN_POINT('Ctrl Pts',(-28.6858402113565,-14.4979516536895,
112.565480733191)) ;
#174905 = CARTESIAN_POINT('Ctrl Pts',(-28.7630866534358,-14.4245500702158,
112.836167498554)) ;
#174906 = CARTESIAN_POINT('Ctrl Pts',(-28.754220545165,-14.3541688694618,
112.809162761213)) ;
#174907 = CARTESIAN_POINT('Ctrl Pts',(-28.6804167329619,-14.3541688284501,
112.83339389798)) ;
#174908 = CARTESIAN_POINT('Ctrl Pts',(-28.6066129207587,-14.3541687874384,
112.857625034748)) ;
#174909 = CARTESIAN_POINT('Ctrl Pts',(-28.6154790290295,-14.4245499881925,
112.884629772089)) ;
#174910 = CARTESIAN_POINT('Ctrl Pts',(-28.6243451373003,-14.4949311889465,
112.91163450943)) ;
#174911 = CARTESIAN_POINT('Ctrl Pts',(-28.6981489495034,-14.4949312299582,
112.887403372663)) ;
#174912 = CARTESIAN_POINT('Ctrl Pts',(-28.7719527617065,-14.4949312709699,
112.863172235896)) ;
#174913 = CARTESIAN_POINT('Ctrl Pts',(-28.7630866534358,-14.4245500702158,
112.836167498554)) ;
#174914 = CARTESIAN_POINT('Ctrl Pts',(-28.8312032669878,-14.27912481409,113.079082108179)) ;
#174915 = CARTESIAN_POINT('Ctrl Pts',(-28.8168350433287,-14.2187925848184,
113.035318815122)) ;
#174916 = CARTESIAN_POINT('Ctrl Pts',(-28.7430312266753,-14.2187925185092,
113.059549938334)) ;
#174917 = CARTESIAN_POINT('Ctrl Pts',(-28.6692274100218,-14.2187924522,113.083781061547)) ;
#174918 = CARTESIAN_POINT('Ctrl Pts',(-28.6835956336809,-14.2791246814716,
113.127544354603)) ;
#174919 = CARTESIAN_POINT('Ctrl Pts',(-28.69796385734,-14.3394569107431,113.17130764766)) ;
#174920 = CARTESIAN_POINT('Ctrl Pts',(-28.7717676739935,-14.3394569770523,
113.147076524447)) ;
#174921 = CARTESIAN_POINT('Ctrl Pts',(-28.8455714906469,-14.3394570433615,
113.122845401235)) ;
#174922 = CARTESIAN_POINT('Ctrl Pts',(-28.8312032669878,-14.27912481409,113.079082108179)) ;
#174923 = CARTESIAN_POINT('Ctrl Pts',(-28.8845697171654,-14.0717728276009,
113.277121444909)) ;
#174924 = CARTESIAN_POINT('Ctrl Pts',(-28.8657198886564,-14.0258274816855,
113.2197079066)) ;
#174925 = CARTESIAN_POINT('Ctrl Pts',(-28.79191606536,-14.0258273955752,113.243939009579)) ;
#174926 = CARTESIAN_POINT('Ctrl Pts',(-28.7181122420636,-14.025827309465,
113.268170112557)) ;
#174927 = CARTESIAN_POINT('Ctrl Pts',(-28.7369620705726,-14.0717726553804,
113.325583650866)) ;
#174928 = CARTESIAN_POINT('Ctrl Pts',(-28.7558118990816,-14.1177180012958,
113.382997189175)) ;
#174929 = CARTESIAN_POINT('Ctrl Pts',(-28.829615722378,-14.1177180874061,
113.358766086196)) ;
#174930 = CARTESIAN_POINT('Ctrl Pts',(-28.9034195456744,-14.1177181735163,
113.334534983217)) ;
#174931 = CARTESIAN_POINT('Ctrl Pts',(-28.8845697171654,-14.0717728276009,
113.277121444909)) ;
#174932 = CARTESIAN_POINT('Ctrl Pts',(-28.9184685925918,-13.8168218187551,
113.415944332688)) ;
#174933 = CARTESIAN_POINT('Ctrl Pts',(-28.8964878467621,-13.7886075890761,
113.348994525439)) ;
#174934 = CARTESIAN_POINT('Ctrl Pts',(-28.8226840152995,-13.7886074911404,
113.373225603545)) ;
#174935 = CARTESIAN_POINT('Ctrl Pts',(-28.748880183837,-13.7886073932047,
113.397456681651)) ;
#174936 = CARTESIAN_POINT('Ctrl Pts',(-28.7708609296667,-13.8168216228837,
113.464406488901)) ;
#174937 = CARTESIAN_POINT('Ctrl Pts',(-28.7928416754963,-13.8450358525627,
113.53135629615)) ;
#174938 = CARTESIAN_POINT('Ctrl Pts',(-28.8666455069589,-13.8450359504984,
113.507125218044)) ;
#174939 = CARTESIAN_POINT('Ctrl Pts',(-28.9404493384214,-13.8450360484341,
113.482894139938)) ;
#174940 = CARTESIAN_POINT('Ctrl Pts',(-28.9184685925918,-13.8168218187551,
113.415944332688)) ;
#174941 = CARTESIAN_POINT('Ctrl Pts',(-28.9296288975394,-13.535324035321,
113.485246560678)) ;
#174942 = CARTESIAN_POINT('Ctrl Pts',(-28.9061056378455,-13.5267213387171,
113.413598505133)) ;
#174943 = CARTESIAN_POINT('Ctrl Pts',(-28.8323017977866,-13.5267212367711,
113.437829557056)) ;
#174944 = CARTESIAN_POINT('Ctrl Pts',(-28.7584979577277,-13.526721134825,
113.462060608979)) ;
#174945 = CARTESIAN_POINT('Ctrl Pts',(-28.7820212174216,-13.5353238314288,
113.533708664524)) ;
#174946 = CARTESIAN_POINT('Ctrl Pts',(-28.8055444771154,-13.5439265280327,
113.605356720069)) ;
#174947 = CARTESIAN_POINT('Ctrl Pts',(-28.8793483171744,-13.5439266299788,
113.581125668146)) ;
#174948 = CARTESIAN_POINT('Ctrl Pts',(-28.9531521572333,-13.5439267319248,
113.556894616223)) ;
#174949 = CARTESIAN_POINT('Ctrl Pts',(-28.9296288975394,-13.535324035321,
113.485246560678)) ;
#174950 = CARTESIAN_POINT('Ctrl Pts',(-28.9167824586136,-13.2440746292406,
113.481603030049)) ;
#174951 = CARTESIAN_POINT('Ctrl Pts',(-28.893386607582,-13.2557932048074,
113.410343040812)) ;
#174952 = CARTESIAN_POINT('Ctrl Pts',(-28.8195827591104,-13.2557931077727,
113.434574067111)) ;
#174953 = CARTESIAN_POINT('Ctrl Pts',(-28.7457789106387,-13.2557930107381,
113.45880509341)) ;
#174954 = CARTESIAN_POINT('Ctrl Pts',(-28.7691747616702,-13.2440744351713,
113.530065082647)) ;
#174955 = CARTESIAN_POINT('Ctrl Pts',(-28.7925706127017,-13.2323558596045,
113.601325071884)) ;
#174956 = CARTESIAN_POINT('Ctrl Pts',(-28.8663744611734,-13.2323559566392,
113.577094045585)) ;
#174957 = CARTESIAN_POINT('Ctrl Pts',(-28.940178309645,-13.2323560536738,
113.552863019286)) ;
#174958 = CARTESIAN_POINT('Ctrl Pts',(-28.9167824586136,-13.2440746292406,
113.481603030049)) ;
#174959 = CARTESIAN_POINT('Ctrl Pts',(-28.879724619622,-12.9648031401168,
113.404286512872)) ;
#174960 = CARTESIAN_POINT('Ctrl Pts',(-28.8581450995204,-12.9960374765742,
113.338558774695)) ;
#174961 = CARTESIAN_POINT('Ctrl Pts',(-28.784341243934,-12.9960373926029,
113.362789779324)) ;
#174962 = CARTESIAN_POINT('Ctrl Pts',(-28.7105373883475,-12.9960373086315,
113.387020783953)) ;
#174963 = CARTESIAN_POINT('Ctrl Pts',(-28.7321169084492,-12.964802972174,
113.452748522129)) ;
#174964 = CARTESIAN_POINT('Ctrl Pts',(-28.7536964285508,-12.9335686357166,
113.518476260305)) ;
#174965 = CARTESIAN_POINT('Ctrl Pts',(-28.8275002841372,-12.933568719688,
113.494245255677)) ;
#174966 = CARTESIAN_POINT('Ctrl Pts',(-28.9013041397237,-12.9335688036593,
113.470014251048)) ;
#174967 = CARTESIAN_POINT('Ctrl Pts',(-28.879724619622,-12.9648031401168,
113.404286512872)) ;
#174968 = CARTESIAN_POINT('Ctrl Pts',(-28.8209010350444,-12.7194345507308,
113.260464724787)) ;
#174969 = CARTESIAN_POINT('Ctrl Pts',(-28.8026647225913,-12.7678470581872,
113.204919857785)) ;
#174970 = CARTESIAN_POINT('Ctrl Pts',(-28.7288608615466,-12.7678469916176,
113.229150845788)) ;
#174971 = CARTESIAN_POINT('Ctrl Pts',(-28.6550570005018,-12.767846925048,
113.253381833792)) ;
#174972 = CARTESIAN_POINT('Ctrl Pts',(-28.6732933129549,-12.7194344175916,
113.308926700794)) ;
#174973 = CARTESIAN_POINT('Ctrl Pts',(-28.691529625408,-12.6710219101352,
113.364471567796)) ;
#174974 = CARTESIAN_POINT('Ctrl Pts',(-28.7653334864528,-12.6710219767048,
113.340240579793)) ;
#174975 = CARTESIAN_POINT('Ctrl Pts',(-28.8391373474975,-12.6710220432744,
113.316009591789)) ;
#174976 = CARTESIAN_POINT('Ctrl Pts',(-28.8209010350444,-12.7194345507308,
113.260464724787)) ;
#174977 = CARTESIAN_POINT('Ctrl Pts',(-28.7430943016509,-12.5228537207888,
113.059023280909)) ;
#174978 = CARTESIAN_POINT('Ctrl Pts',(-28.7295272533621,-12.5850644655665,
113.017700239312)) ;
#174979 = CARTESIAN_POINT('Ctrl Pts',(-28.6557233893278,-12.5850644207041,
113.04193121821)) ;
#174980 = CARTESIAN_POINT('Ctrl Pts',(-28.5819195252936,-12.5850643758416,
113.066162197108)) ;
#174981 = CARTESIAN_POINT('Ctrl Pts',(-28.5954865735824,-12.522853631064,
113.107485238705)) ;
#174982 = CARTESIAN_POINT('Ctrl Pts',(-28.6090536218712,-12.4606428862864,
113.148808280301)) ;
#174983 = CARTESIAN_POINT('Ctrl Pts',(-28.6828574859055,-12.4606429311488,
113.124577301403)) ;
#174984 = CARTESIAN_POINT('Ctrl Pts',(-28.7566613499397,-12.4606429760112,
113.100346322505)) ;
#174985 = CARTESIAN_POINT('Ctrl Pts',(-28.7430943016509,-12.5228537207888,
113.059023280909)) ;
#174986 = CARTESIAN_POINT('Ctrl Pts',(-28.6517657151193,-12.3910219564108,
112.816257416584)) ;
#174987 = CARTESIAN_POINT('Ctrl Pts',(-28.6438220478864,-12.4625310700348,
112.792062286491)) ;
#174988 = CARTESIAN_POINT('Ctrl Pts',(-28.5700181829588,-12.4625310467126,
112.816293262668)) ;
#174989 = CARTESIAN_POINT('Ctrl Pts',(-28.4962143180312,-12.4625310233905,
112.840524238845)) ;
#174990 = CARTESIAN_POINT('Ctrl Pts',(-28.5041579852641,-12.3910219097665,
112.864719368938)) ;
#174991 = CARTESIAN_POINT('Ctrl Pts',(-28.5121016524971,-12.3195127961425,
112.888914499031)) ;
#174992 = CARTESIAN_POINT('Ctrl Pts',(-28.5859055174246,-12.3195128194647,
112.864683522854)) ;
#174993 = CARTESIAN_POINT('Ctrl Pts',(-28.6597093823522,-12.3195128427868,
112.840452546677)) ;
#174994 = CARTESIAN_POINT('Ctrl Pts',(-28.6517657151193,-12.3910219564108,
112.816257416584)) ;
#174995 = CARTESIAN_POINT('Ctrl Pts',(-28.5519605561705,-12.3324946198483,
112.547844627311)) ;
#174996 = CARTESIAN_POINT('Ctrl Pts',(-28.5502370298838,-12.408198760168,
112.542595043101)) ;
#174997 = CARTESIAN_POINT('Ctrl Pts',(-28.4764331666314,-12.4081987566325,
112.56682602438)) ;
#174998 = CARTESIAN_POINT('Ctrl Pts',(-28.402629303379,-12.4081987530971,
112.59105700566)) ;
#174999 = CARTESIAN_POINT('Ctrl Pts',(-28.4043528296657,-12.3324946127775,
112.59630658987)) ;
#175000 = CARTESIAN_POINT('Ctrl Pts',(-28.4060763559524,-12.2567904724578,
112.60155617408)) ;
#175001 = CARTESIAN_POINT('Ctrl Pts',(-28.4798802192048,-12.2567904759932,
112.577325192801)) ;
#175002 = CARTESIAN_POINT('Ctrl Pts',(-28.5536840824571,-12.2567904795287,
112.553094211521)) ;
#175003 = CARTESIAN_POINT('Ctrl Pts',(-28.5519605561705,-12.3324946198483,
112.547844627311)) ;
#175004 = CARTESIAN_POINT('Ctrl Pts',(-28.4511785871551,-12.3517941049946,
112.2762149844)) ;
#175005 = CARTESIAN_POINT('Ctrl Pts',(-28.4557579295196,-12.426265134033,
112.290162921278)) ;
#175006 = CARTESIAN_POINT('Ctrl Pts',(-28.3819540689083,-12.426265145997,
112.314393910602)) ;
#175007 = CARTESIAN_POINT('Ctrl Pts',(-28.308150208297,-12.4262651579609,
112.338624899925)) ;
#175008 = CARTESIAN_POINT('Ctrl Pts',(-28.3035708659325,-12.3517941289225,
112.324676963048)) ;
#175009 = CARTESIAN_POINT('Ctrl Pts',(-28.298991523568,-12.2773230998841,
112.310729026171)) ;
#175010 = CARTESIAN_POINT('Ctrl Pts',(-28.3727953841793,-12.2773230879201,
112.286498036847)) ;
#175011 = CARTESIAN_POINT('Ctrl Pts',(-28.4465992447906,-12.2773230759562,
112.262267047523)) ;
#175012 = CARTESIAN_POINT('Ctrl Pts',(-28.4511785871551,-12.3517941049946,
112.2762149844)) ;
#175013 = CARTESIAN_POINT('Ctrl Pts',(-28.3546167960162,-12.4476532719571,
112.01766426386)) ;
#175014 = CARTESIAN_POINT('Ctrl Pts',(-28.365209322812,-12.5155445566341,
112.049927390478)) ;
#175015 = CARTESIAN_POINT('Ctrl Pts',(-28.2914054664986,-12.5155445785794,
112.074158392892)) ;
#175016 = CARTESIAN_POINT('Ctrl Pts',(-28.2176016101851,-12.5155446005247,
112.098389395307)) ;
#175017 = CARTESIAN_POINT('Ctrl Pts',(-28.2070090833893,-12.4476533158478,
112.066126268689)) ;
#175018 = CARTESIAN_POINT('Ctrl Pts',(-28.1964165565935,-12.3797620311708,
112.033863142072)) ;
#175019 = CARTESIAN_POINT('Ctrl Pts',(-28.2702204129069,-12.3797620092255,
112.009632139657)) ;
#175020 = CARTESIAN_POINT('Ctrl Pts',(-28.3440242692203,-12.3797619872802,
111.985401137243)) ;
#175021 = CARTESIAN_POINT('Ctrl Pts',(-28.3546167960162,-12.4476532719571,
112.01766426386)) ;
#175022 = CARTESIAN_POINT('Ctrl Pts',(-28.2694260224947,-12.6128436094032,
111.793615869469)) ;
#175023 = CARTESIAN_POINT('Ctrl Pts',(-28.2852496876729,-12.6693038141033,
111.841812199719)) ;
#175024 = CARTESIAN_POINT('Ctrl Pts',(-28.211445835532,-12.669303840492,111.866043214843)) ;
#175025 = CARTESIAN_POINT('Ctrl Pts',(-28.1376419833911,-12.6693038668807,
111.890274229966)) ;
#175026 = CARTESIAN_POINT('Ctrl Pts',(-28.1218183182129,-12.6128436621805,
111.842077899716)) ;
#175027 = CARTESIAN_POINT('Ctrl Pts',(-28.1059946530346,-12.5563834574804,
111.793881569465)) ;
#175028 = CARTESIAN_POINT('Ctrl Pts',(-28.1797985051756,-12.5563834310917,
111.769650554342)) ;
#175029 = CARTESIAN_POINT('Ctrl Pts',(-28.2536023573165,-12.556383404703,
111.745419539218)) ;
#175030 = CARTESIAN_POINT('Ctrl Pts',(-28.2694260224947,-12.6128436094032,
111.793615869469)) ;
#175031 = CARTESIAN_POINT('Ctrl Pts',(-28.2004725461681,-12.8354722898284,
111.619033756946)) ;
#175032 = CARTESIAN_POINT('Ctrl Pts',(-28.2204013581391,-12.8764735343339,
111.679733702125)) ;
#175033 = CARTESIAN_POINT('Ctrl Pts',(-28.1465975099213,-12.8764735602594,
111.703964729197)) ;
#175034 = CARTESIAN_POINT('Ctrl Pts',(-28.0727936617034,-12.8764735861849,
111.728195756269)) ;
#175035 = CARTESIAN_POINT('Ctrl Pts',(-28.0528648497324,-12.8354723416794,
111.667495811091)) ;
#175036 = CARTESIAN_POINT('Ctrl Pts',(-28.0329360377614,-12.794471097174,
111.606795865912)) ;
#175037 = CARTESIAN_POINT('Ctrl Pts',(-28.1067398859793,-12.7944710712485,
111.582564838839)) ;
#175038 = CARTESIAN_POINT('Ctrl Pts',(-28.1805437341971,-12.794471045323,
111.558333811767)) ;
#175039 = CARTESIAN_POINT('Ctrl Pts',(-28.2004725461681,-12.8354722898284,
111.619033756946)) ;
#175040 = CARTESIAN_POINT('Ctrl Pts',(-28.1518872197862,-13.101408894203,
111.506681708968)) ;
#175041 = CARTESIAN_POINT('Ctrl Pts',(-28.1745014661494,-13.1239035578376,
111.575561054197)) ;
#175042 = CARTESIAN_POINT('Ctrl Pts',(-28.1006976210795,-13.1239035777503,
111.599792090857)) ;
#175043 = CARTESIAN_POINT('Ctrl Pts',(-28.0268937760095,-13.1239035976629,
111.624023127518)) ;
#175044 = CARTESIAN_POINT('Ctrl Pts',(-28.0042795296463,-13.1014089340283,
111.555143782289)) ;
#175045 = CARTESIAN_POINT('Ctrl Pts',(-27.9816652832831,-13.0789142703937,
111.48626443706)) ;
#175046 = CARTESIAN_POINT('Ctrl Pts',(-28.0554691283531,-13.078914250481,
111.462033400399)) ;
#175047 = CARTESIAN_POINT('Ctrl Pts',(-28.129272973423,-13.0789142305684,
111.437802363739)) ;
#175048 = CARTESIAN_POINT('Ctrl Pts',(-28.1518872197862,-13.101408894203,
111.506681708968)) ;
#175049 = CARTESIAN_POINT('Ctrl Pts',(-28.1269130732857,-13.3874022195482,
111.465903939157)) ;
#175050 = CARTESIAN_POINT('Ctrl Pts',(-28.150574864272,-13.3899614744304,
111.537973936401)) ;
#175051 = CARTESIAN_POINT('Ctrl Pts',(-28.0767710208941,-13.389961489155,
111.562204978215)) ;
#175052 = CARTESIAN_POINT('Ctrl Pts',(-28.0029671775161,-13.3899615038795,
111.586436020028)) ;
#175053 = CARTESIAN_POINT('Ctrl Pts',(-27.9793053865298,-13.3874022489973,
111.514366022785)) ;
#175054 = CARTESIAN_POINT('Ctrl Pts',(-27.9556435955435,-13.384842994115,
111.442296025541)) ;
#175055 = CARTESIAN_POINT('Ctrl Pts',(-28.0294474389214,-13.3848429793905,
111.418064983727)) ;
#175056 = CARTESIAN_POINT('Ctrl Pts',(-28.1032512822994,-13.3848429646659,
111.393833941913)) ;
#175057 = CARTESIAN_POINT('Ctrl Pts',(-28.1269130732857,-13.3874022195482,
111.465903939157)) ;
#175058 = CARTESIAN_POINT('Ctrl Pts',(-28.1259581954368,-13.6768759171903,
111.498450514514)) ;
#175059 = CARTESIAN_POINT('Ctrl Pts',(-28.1489886412209,-13.6592264507691,
111.568597536266)) ;
#175060 = CARTESIAN_POINT('Ctrl Pts',(-28.0751847985998,-13.6592264585441,
111.592828580385)) ;
#175061 = CARTESIAN_POINT('Ctrl Pts',(-28.0013809559787,-13.6592264663191,
111.617059624505)) ;
#175062 = CARTESIAN_POINT('Ctrl Pts',(-27.9783505101947,-13.6768759327404,
111.546912602753)) ;
#175063 = CARTESIAN_POINT('Ctrl Pts',(-27.9553200644106,-13.6945253991617,
111.476765581001)) ;
#175064 = CARTESIAN_POINT('Ctrl Pts',(-28.0291239070317,-13.6945253913867,
111.452534536881)) ;
#175065 = CARTESIAN_POINT('Ctrl Pts',(-28.1029277496528,-13.6945253836116,
111.428303492762)) ;
#175066 = CARTESIAN_POINT('Ctrl Pts',(-28.1259581954368,-13.6768759171903,
111.498450514514)) ;
#175067 = CARTESIAN_POINT('Ctrl Pts',(-28.1487784107379,-13.948608493865,
111.603521104352)) ;
#175068 = CARTESIAN_POINT('Ctrl Pts',(-28.1695141104945,-13.9119580024122,
111.666678700074)) ;
#175069 = CARTESIAN_POINT('Ctrl Pts',(-28.095710267544,-13.9119580041773,
111.69090974319)) ;
#175070 = CARTESIAN_POINT('Ctrl Pts',(-28.0219064245936,-13.9119580059424,
111.715140786306)) ;
#175071 = CARTESIAN_POINT('Ctrl Pts',(-28.001170724837,-13.9486084973951,
111.651983190584)) ;
#175072 = CARTESIAN_POINT('Ctrl Pts',(-27.9804350250805,-13.9852589888479,
111.588825594862)) ;
#175073 = CARTESIAN_POINT('Ctrl Pts',(-28.0542388680309,-13.9852589870828,
111.564594551746)) ;
#175074 = CARTESIAN_POINT('Ctrl Pts',(-28.1280427109814,-13.9852589853178,
111.54036350863)) ;
#175075 = CARTESIAN_POINT('Ctrl Pts',(-28.1487784107379,-13.948608493865,
111.603521104352)) ;
#175076 = CARTESIAN_POINT('Ctrl Pts',(-28.1927422454497,-14.181257681225,
111.772854625694)) ;
#175077 = CARTESIAN_POINT('Ctrl Pts',(-28.209705905835,-14.12830707033,111.824523198175)) ;
#175078 = CARTESIAN_POINT('Ctrl Pts',(-28.135902062206,-14.1283070692883,
111.848754239225)) ;
#175079 = CARTESIAN_POINT('Ctrl Pts',(-28.0620982185771,-14.1283070682466,
111.872985280274)) ;
#175080 = CARTESIAN_POINT('Ctrl Pts',(-28.0451345581918,-14.1812576791416,
111.821316707793)) ;
#175081 = CARTESIAN_POINT('Ctrl Pts',(-28.0281708978066,-14.2342082900366,
111.769648135312)) ;
#175082 = CARTESIAN_POINT('Ctrl Pts',(-28.1019747414355,-14.2342082910783,
111.745417094263)) ;
#175083 = CARTESIAN_POINT('Ctrl Pts',(-28.1757785850644,-14.23420829212,111.721186053214)) ;
#175084 = CARTESIAN_POINT('Ctrl Pts',(-28.1927422454497,-14.181257681225,
111.772854625694)) ;
#175085 = CARTESIAN_POINT('Ctrl Pts',(-28.25389994631,-14.3592650506284,111.994525378914)) ;
#175086 = CARTESIAN_POINT('Ctrl Pts',(-28.2658858395401,-14.2938058183535,
112.031032475836)) ;
#175087 = CARTESIAN_POINT('Ctrl Pts',(-28.1920819953039,-14.2938058167003,
112.055263515036)) ;
#175088 = CARTESIAN_POINT('Ctrl Pts',(-28.1182781510676,-14.293805815047,
112.079494554236)) ;
#175089 = CARTESIAN_POINT('Ctrl Pts',(-28.1062922578376,-14.359265047322,
112.042987457314)) ;
#175090 = CARTESIAN_POINT('Ctrl Pts',(-28.0943063646075,-14.4247242795969,
112.006480360391)) ;
#175091 = CARTESIAN_POINT('Ctrl Pts',(-28.1681102088437,-14.4247242812501,
111.982249321192)) ;
#175092 = CARTESIAN_POINT('Ctrl Pts',(-28.24191405308,-14.4247242829034,111.958018281992)) ;
#175093 = CARTESIAN_POINT('Ctrl Pts',(-28.25389994631,-14.3592650506284,111.994525378914)) ;
#175094 = CARTESIAN_POINT('Ctrl Pts',(-28.3273391635443,-14.4703402370834,
112.253666401676)) ;
#175095 = CARTESIAN_POINT('Ctrl Pts',(-28.3334807725046,-14.3970277006435,
112.272372751686)) ;
#175096 = CARTESIAN_POINT('Ctrl Pts',(-28.2596769281304,-14.3970276999611,
112.296603790465)) ;
#175097 = CARTESIAN_POINT('Ctrl Pts',(-28.1858730837562,-14.3970276992787,
112.320834829245)) ;
#175098 = CARTESIAN_POINT('Ctrl Pts',(-28.1797314747959,-14.4703402357187,
112.302128479236)) ;
#175099 = CARTESIAN_POINT('Ctrl Pts',(-28.1735898658356,-14.5436527721586,
112.283422129226)) ;
#175100 = CARTESIAN_POINT('Ctrl Pts',(-28.2473937102098,-14.543652772841,
112.259191090447)) ;
#175101 = CARTESIAN_POINT('Ctrl Pts',(-28.321197554584,-14.5436527735234,
112.234960051667)) ;
#175102 = CARTESIAN_POINT('Ctrl Pts',(-28.3273391635443,-14.4703402370834,
112.253666401676)) ;
#175103 = CARTESIAN_POINT('Ctrl Pts',(-28.4071790901361,-14.5059089260168,
112.532398419472)) ;
#175104 = CARTESIAN_POINT('Ctrl Pts',(-28.4070188716446,-14.4300045540626,
112.531910419809)) ;
#175105 = CARTESIAN_POINT('Ctrl Pts',(-28.3332150280579,-14.4300045543585,
112.556141460987)) ;
#175106 = CARTESIAN_POINT('Ctrl Pts',(-28.2594111844711,-14.4300045546544,
112.580372502165)) ;
#175107 = CARTESIAN_POINT('Ctrl Pts',(-28.2595714029626,-14.5059089266086,
112.580860501828)) ;
#175108 = CARTESIAN_POINT('Ctrl Pts',(-28.259731621454,-14.5818132985628,
112.581348501491)) ;
#175109 = CARTESIAN_POINT('Ctrl Pts',(-28.3335354650407,-14.5818132982669,
112.557117460313)) ;
#175110 = CARTESIAN_POINT('Ctrl Pts',(-28.4073393086275,-14.581813297971,
112.532886419135)) ;
#175111 = CARTESIAN_POINT('Ctrl Pts',(-28.4071790901361,-14.5059089260168,
112.532398419472)) ;
#175112 = CARTESIAN_POINT('Ctrl Pts',(-28.4863373455099,-14.4635906108697,
112.808879001028)) ;
#175113 = CARTESIAN_POINT('Ctrl Pts',(-28.4799175167862,-14.3905302812958,
112.789325238511)) ;
#175114 = CARTESIAN_POINT('Ctrl Pts',(-28.4061136743483,-14.3905302808225,
112.813556283188)) ;
#175115 = CARTESIAN_POINT('Ctrl Pts',(-28.3323098319104,-14.3905302803492,
112.837787327865)) ;
#175116 = CARTESIAN_POINT('Ctrl Pts',(-28.3387296606341,-14.4635906099231,
112.857341090383)) ;
#175117 = CARTESIAN_POINT('Ctrl Pts',(-28.3451494893579,-14.536650939497,
112.8768948529)) ;
#175118 = CARTESIAN_POINT('Ctrl Pts',(-28.4189533317957,-14.5366509399703,
112.852663808223)) ;
#175119 = CARTESIAN_POINT('Ctrl Pts',(-28.4927571742336,-14.5366509404436,
112.828432763546)) ;
#175120 = CARTESIAN_POINT('Ctrl Pts',(-28.4863373455099,-14.4635906108697,
112.808879001028)) ;
#175121 = CARTESIAN_POINT('Ctrl Pts',(-28.5590864820887,-14.3462861335646,
113.06597539471)) ;
#175122 = CARTESIAN_POINT('Ctrl Pts',(-28.5468426175345,-14.2813098903358,
113.028682558647)) ;
#175123 = CARTESIAN_POINT('Ctrl Pts',(-28.4730387765814,-14.2813098862363,
113.052913607847)) ;
#175124 = CARTESIAN_POINT('Ctrl Pts',(-28.3992349356284,-14.2813098821367,
113.077144657047)) ;
#175125 = CARTESIAN_POINT('Ctrl Pts',(-28.4114788001826,-14.3462861253655,
113.11443749311)) ;
#175126 = CARTESIAN_POINT('Ctrl Pts',(-28.4237226647368,-14.4112623685942,
113.151730329173)) ;
#175127 = CARTESIAN_POINT('Ctrl Pts',(-28.4975265056898,-14.4112623726938,
113.127499279973)) ;
#175128 = CARTESIAN_POINT('Ctrl Pts',(-28.5713303466429,-14.4112623767934,
113.103268230773)) ;
#175129 = CARTESIAN_POINT('Ctrl Pts',(-28.5590864820887,-14.3462861335646,
113.06597539471)) ;
#175130 = CARTESIAN_POINT('Ctrl Pts',(-28.6190888482877,-14.1620807273187,
113.284252795165)) ;
#175131 = CARTESIAN_POINT('Ctrl Pts',(-28.6019025244461,-14.1098718676652,
113.231906025436)) ;
#175132 = CARTESIAN_POINT('Ctrl Pts',(-28.5280986845969,-14.1098718563613,
113.256137077998)) ;
#175133 = CARTESIAN_POINT('Ctrl Pts',(-28.4542948447477,-14.1098718450575,
113.28036813056)) ;
#175134 = CARTESIAN_POINT('Ctrl Pts',(-28.4714811685893,-14.162080704711,
113.332714900289)) ;
#175135 = CARTESIAN_POINT('Ctrl Pts',(-28.4886674924309,-14.2142895643646,
113.385061670018)) ;
#175136 = CARTESIAN_POINT('Ctrl Pts',(-28.5624713322801,-14.2142895756684,
113.360830617456)) ;
#175137 = CARTESIAN_POINT('Ctrl Pts',(-28.6362751721293,-14.2142895869723,
113.336599564894)) ;
#175138 = CARTESIAN_POINT('Ctrl Pts',(-28.6190888482877,-14.1620807273187,
113.284252795165)) ;
#175139 = CARTESIAN_POINT('Ctrl Pts',(-28.6611716634273,-13.9257450561724,
113.447780698845)) ;
#175140 = CARTESIAN_POINT('Ctrl Pts',(-28.6402906964383,-13.8899621379748,
113.384180642091)) ;
#175141 = CARTESIAN_POINT('Ctrl Pts',(-28.5664868565058,-13.8899621182589,
113.408411694399)) ;
#175142 = CARTESIAN_POINT('Ctrl Pts',(-28.4926830165733,-13.889962098543,
113.432642746707)) ;
#175143 = CARTESIAN_POINT('Ctrl Pts',(-28.5135639835622,-13.9257450167406,
113.496242803462)) ;
#175144 = CARTESIAN_POINT('Ctrl Pts',(-28.5344449505512,-13.9615279349381,
113.559842860216)) ;
#175145 = CARTESIAN_POINT('Ctrl Pts',(-28.6082487904837,-13.961527954654,
113.535611807908)) ;
#175146 = CARTESIAN_POINT('Ctrl Pts',(-28.6820526304163,-13.9615279743699,
113.5113807556)) ;
#175147 = CARTESIAN_POINT('Ctrl Pts',(-28.6611716634273,-13.9257450561724,
113.447780698845)) ;
#175148 = CARTESIAN_POINT('Ctrl Pts',(-28.6819629618819,-13.6518932520307,
113.54663327576)) ;
#175149 = CARTESIAN_POINT('Ctrl Pts',(-28.6588649077152,-13.6351791904555,
113.476280329019)) ;
#175150 = CARTESIAN_POINT('Ctrl Pts',(-28.5850610666532,-13.6351791600229,
113.500511377887)) ;
#175151 = CARTESIAN_POINT('Ctrl Pts',(-28.5112572255911,-13.6351791295903,
113.524742426755)) ;
#175152 = CARTESIAN_POINT('Ctrl Pts',(-28.5343552797579,-13.6518931911655,
113.595095373495)) ;
#175153 = CARTESIAN_POINT('Ctrl Pts',(-28.5574533339246,-13.6686072527407,
113.665448320236)) ;
#175154 = CARTESIAN_POINT('Ctrl Pts',(-28.6312571749866,-13.6686072831733,
113.641217271368)) ;
#175155 = CARTESIAN_POINT('Ctrl Pts',(-28.7050610160487,-13.6686073136059,
113.6169862225)) ;
#175156 = CARTESIAN_POINT('Ctrl Pts',(-28.6819629618819,-13.6518932520307,
113.54663327576)) ;
#175157 = CARTESIAN_POINT('Ctrl Pts',(-28.6788957975661,-13.361350209501,
113.572794442411)) ;
#175158 = CARTESIAN_POINT('Ctrl Pts',(-28.6552438087377,-13.3648978107094,
113.500754299894)) ;
#175159 = CARTESIAN_POINT('Ctrl Pts',(-28.58143996491,-13.3648977704052,113.524985340338)) ;
#175160 = CARTESIAN_POINT('Ctrl Pts',(-28.5076361210823,-13.364897730101,
113.549216380782)) ;
#175161 = CARTESIAN_POINT('Ctrl Pts',(-28.5312881099107,-13.3613501288926,
113.621256523299)) ;
#175162 = CARTESIAN_POINT('Ctrl Pts',(-28.5549400987392,-13.3578025276842,
113.693296665815)) ;
#175163 = CARTESIAN_POINT('Ctrl Pts',(-28.6287439425669,-13.3578025679884,
113.669065625371)) ;
#175164 = CARTESIAN_POINT('Ctrl Pts',(-28.7025477863946,-13.3578026082926,
113.644834584927)) ;
#175165 = CARTESIAN_POINT('Ctrl Pts',(-28.6788957975661,-13.361350209501,
113.572794442411)) ;
#175166 = CARTESIAN_POINT('Ctrl Pts',(-28.6515753370969,-13.0754523993138,
113.525017916636)) ;
#175167 = CARTESIAN_POINT('Ctrl Pts',(-28.629063419331,-13.0989663539562,
113.456450246463)) ;
#175168 = CARTESIAN_POINT('Ctrl Pts',(-28.5552595713404,-13.0989663074807,
113.480681274228)) ;
#175169 = CARTESIAN_POINT('Ctrl Pts',(-28.4814557233498,-13.0989662610053,
113.504912301992)) ;
#175170 = CARTESIAN_POINT('Ctrl Pts',(-28.5039676411157,-13.0754523063629,
113.573479972165)) ;
#175171 = CARTESIAN_POINT('Ctrl Pts',(-28.5264795588817,-13.0519383517206,
113.642047642338)) ;
#175172 = CARTESIAN_POINT('Ctrl Pts',(-28.6002834068723,-13.051938398196,
113.617816614573)) ;
#175173 = CARTESIAN_POINT('Ctrl Pts',(-28.6740872548629,-13.0519384446715,
113.593585586809)) ;
#175174 = CARTESIAN_POINT('Ctrl Pts',(-28.6515753370969,-13.0754523993138,
113.525017916636)) ;
#175175 = CARTESIAN_POINT('Ctrl Pts',(-28.6012644802897,-12.8139381990977,
113.407216883436)) ;
#175176 = CARTESIAN_POINT('Ctrl Pts',(-28.5814994051075,-12.8557446579336,
113.347015652409)) ;
#175177 = CARTESIAN_POINT('Ctrl Pts',(-28.5076955520102,-12.8557446099044,
113.371246664619)) ;
#175178 = CARTESIAN_POINT('Ctrl Pts',(-28.4338916989129,-12.8557445618753,
113.395477676829)) ;
#175179 = CARTESIAN_POINT('Ctrl Pts',(-28.4536567740952,-12.8139381030394,
113.455678907856)) ;
#175180 = CARTESIAN_POINT('Ctrl Pts',(-28.4734218492774,-12.7721316442036,
113.515880138883)) ;
#175181 = CARTESIAN_POINT('Ctrl Pts',(-28.5472257023747,-12.7721316922327,
113.491649126673)) ;
#175182 = CARTESIAN_POINT('Ctrl Pts',(-28.621029555472,-12.7721317402619,
113.467418114463)) ;
#175183 = CARTESIAN_POINT('Ctrl Pts',(-28.6012644802897,-12.8139381990977,
113.407216883436)) ;
#175184 = CARTESIAN_POINT('Ctrl Pts',(-28.530312795938,-12.5948180944483,
113.22672545771)) ;
#175185 = CARTESIAN_POINT('Ctrl Pts',(-28.5147357585645,-12.6519838381849,
113.17928031392)) ;
#175186 = CARTESIAN_POINT('Ctrl Pts',(-28.4409318994849,-12.6519837938663,
113.20351130791)) ;
#175187 = CARTESIAN_POINT('Ctrl Pts',(-28.3671280404052,-12.6519837495477,
113.227742301899)) ;
#175188 = CARTESIAN_POINT('Ctrl Pts',(-28.3827050777788,-12.5948180058111,
113.275187445688)) ;
#175189 = CARTESIAN_POINT('Ctrl Pts',(-28.3982821151524,-12.5376522620745,
113.322632589477)) ;
#175190 = CARTESIAN_POINT('Ctrl Pts',(-28.472085974232,-12.537652306393,113.298401595488)) ;
#175191 = CARTESIAN_POINT('Ctrl Pts',(-28.5458898333115,-12.5376523507116,
113.274170601499)) ;
#175192 = CARTESIAN_POINT('Ctrl Pts',(-28.530312795938,-12.5948180944483,
113.22672545771)) ;
#175193 = CARTESIAN_POINT('Ctrl Pts',(-28.4441820785393,-12.4362800048722,
112.999678378)) ;
#175194 = CARTESIAN_POINT('Ctrl Pts',(-28.4338657622434,-12.5045968794166,
112.968256541675)) ;
#175195 = CARTESIAN_POINT('Ctrl Pts',(-28.3600618982417,-12.5045968472639,
112.992487520672)) ;
#175196 = CARTESIAN_POINT('Ctrl Pts',(-28.28625803424,-12.5045968151111,113.016718499669)) ;
#175197 = CARTESIAN_POINT('Ctrl Pts',(-28.2965743505358,-12.4362799405667,
113.048140335994)) ;
#175198 = CARTESIAN_POINT('Ctrl Pts',(-28.3068906668317,-12.3679630660223,
113.079562172319)) ;
#175199 = CARTESIAN_POINT('Ctrl Pts',(-28.3806945308334,-12.367963098175,
113.055331193322)) ;
#175200 = CARTESIAN_POINT('Ctrl Pts',(-28.4544983948351,-12.3679631303278,
113.031100214324)) ;
#175201 = CARTESIAN_POINT('Ctrl Pts',(-28.4441820785393,-12.4362800048722,
112.999678378)) ;
#175202 = CARTESIAN_POINT('Ctrl Pts',(-28.3470854955192,-12.346922078608,
112.739452029468)) ;
#175203 = CARTESIAN_POINT('Ctrl Pts',(-28.3427983341584,-12.4215768384595,
112.726394026123)) ;
#175204 = CARTESIAN_POINT('Ctrl Pts',(-28.2689944658137,-12.4215768235296,
112.750624991892)) ;
#175205 = CARTESIAN_POINT('Ctrl Pts',(-28.195190597469,-12.4215768085998,
112.774855957661)) ;
#175206 = CARTESIAN_POINT('Ctrl Pts',(-28.1994777588298,-12.3469220487482,
112.787913961007)) ;
#175207 = CARTESIAN_POINT('Ctrl Pts',(-28.2037649201905,-12.2722672888967,
112.800971964352)) ;
#175208 = CARTESIAN_POINT('Ctrl Pts',(-28.2775687885352,-12.2722673038266,
112.776740998583)) ;
#175209 = CARTESIAN_POINT('Ctrl Pts',(-28.3513726568799,-12.2722673187564,
112.752510032814)) ;
#175210 = CARTESIAN_POINT('Ctrl Pts',(-28.3470854955192,-12.346922078608,
112.739452029468)) ;
#175211 = CARTESIAN_POINT('Ctrl Pts',(-28.2458303935604,-12.3346186385411,
112.466505819017)) ;
#175212 = CARTESIAN_POINT('Ctrl Pts',(-28.2478725713665,-12.4102408597983,
112.472725961409)) ;
#175213 = CARTESIAN_POINT('Ctrl Pts',(-28.1740687006002,-12.4102408673589,
112.496956919802)) ;
#175214 = CARTESIAN_POINT('Ctrl Pts',(-28.1002648298339,-12.4102408749196,
112.521187878196)) ;
#175215 = CARTESIAN_POINT('Ctrl Pts',(-28.0982226520278,-12.3346186536624,
112.514967735804)) ;
#175216 = CARTESIAN_POINT('Ctrl Pts',(-28.0961804742218,-12.2589964324052,
112.508747593412)) ;
#175217 = CARTESIAN_POINT('Ctrl Pts',(-28.1699843449881,-12.2589964248446,
112.484516635018)) ;
#175218 = CARTESIAN_POINT('Ctrl Pts',(-28.2437882157544,-12.2589964172839,
112.460285676625)) ;
#175219 = CARTESIAN_POINT('Ctrl Pts',(-28.2458303935604,-12.3346186385411,
112.466505819017)) ;
#175220 = CARTESIAN_POINT('Ctrl Pts',(-28.1468306373285,-12.3998225687949,
112.200422951598)) ;
#175221 = CARTESIAN_POINT('Ctrl Pts',(-28.1550539935489,-12.4710025852177,
112.225469965997)) ;
#175222 = CARTESIAN_POINT('Ctrl Pts',(-28.0812501226881,-12.4710026178869,
112.249700924103)) ;
#175223 = CARTESIAN_POINT('Ctrl Pts',(-28.0074462518273,-12.4710026505561,
112.273931882208)) ;
#175224 = CARTESIAN_POINT('Ctrl Pts',(-27.9992228956068,-12.3998226341332,
112.248884867808)) ;
#175225 = CARTESIAN_POINT('Ctrl Pts',(-27.9909995393864,-12.3286426177104,
112.223837853409)) ;
#175226 = CARTESIAN_POINT('Ctrl Pts',(-28.0648034102472,-12.3286425850412,
112.199606895303)) ;
#175227 = CARTESIAN_POINT('Ctrl Pts',(-28.138607281108,-12.328642552372,112.175375937198)) ;
#175228 = CARTESIAN_POINT('Ctrl Pts',(-28.1468306373285,-12.3998225687949,
112.200422951598)) ;
#175229 = CARTESIAN_POINT('Ctrl Pts',(-28.056410402061,-12.5378477500096,
111.960460656517)) ;
#175230 = CARTESIAN_POINT('Ctrl Pts',(-28.0702251886927,-12.599495230749,
112.002538265681)) ;
#175231 = CARTESIAN_POINT('Ctrl Pts',(-27.9964213202855,-12.5994952885301,
112.026769231259)) ;
#175232 = CARTESIAN_POINT('Ctrl Pts',(-27.9226174518782,-12.5994953463112,
112.051000196837)) ;
#175233 = CARTESIAN_POINT('Ctrl Pts',(-27.9088026652464,-12.5378478655717,
112.008922587674)) ;
#175234 = CARTESIAN_POINT('Ctrl Pts',(-27.8949878786146,-12.4762003848323,
111.966844978511)) ;
#175235 = CARTESIAN_POINT('Ctrl Pts',(-27.9687917470219,-12.4762003270512,
111.942614012932)) ;
#175236 = CARTESIAN_POINT('Ctrl Pts',(-28.0425956154292,-12.4762002692701,
111.918383047354)) ;
#175237 = CARTESIAN_POINT('Ctrl Pts',(-28.056410402061,-12.5378477500096,
111.960460656517)) ;
#175238 = CARTESIAN_POINT('Ctrl Pts',(-27.9801392408926,-12.7392396507352,
111.763656314593)) ;
#175239 = CARTESIAN_POINT('Ctrl Pts',(-27.9985645664945,-12.7869171442881,
111.81977688147)) ;
#175240 = CARTESIAN_POINT('Ctrl Pts',(-27.9247607029675,-12.7869172246325,
111.844007861913)) ;
#175241 = CARTESIAN_POINT('Ctrl Pts',(-27.8509568394405,-12.786917304977,
111.868238842356)) ;
#175242 = CARTESIAN_POINT('Ctrl Pts',(-27.8325315138385,-12.7392398114241,
111.812118275479)) ;
#175243 = CARTESIAN_POINT('Ctrl Pts',(-27.8141061882366,-12.6915623178712,
111.755997708602)) ;
#175244 = CARTESIAN_POINT('Ctrl Pts',(-27.8879100517636,-12.6915622375267,
111.731766728159)) ;
#175245 = CARTESIAN_POINT('Ctrl Pts',(-27.9617139152906,-12.6915621571823,
111.707535747716)) ;
#175246 = CARTESIAN_POINT('Ctrl Pts',(-27.9801392408926,-12.7392396507352,
111.763656314593)) ;
#175247 = CARTESIAN_POINT('Ctrl Pts',(-27.9229728782281,-12.989236405783,
111.625017894805)) ;
#175248 = CARTESIAN_POINT('Ctrl Pts',(-27.9446822619997,-13.019530175167,
111.69114117293)) ;
#175249 = CARTESIAN_POINT('Ctrl Pts',(-27.8708784055218,-13.019530272485,
111.715372174843)) ;
#175250 = CARTESIAN_POINT('Ctrl Pts',(-27.7970745490438,-13.0195303698031,
111.739603176756)) ;
#175251 = CARTESIAN_POINT('Ctrl Pts',(-27.7753651652723,-12.9892366004191,
111.673479898632)) ;
#175252 = CARTESIAN_POINT('Ctrl Pts',(-27.7536557815007,-12.9589428310352,
111.607356620507)) ;
#175253 = CARTESIAN_POINT('Ctrl Pts',(-27.8274596379786,-12.9589427337171,
111.583125618594)) ;
#175254 = CARTESIAN_POINT('Ctrl Pts',(-27.9012634944566,-12.9589426363991,
111.558894616681)) ;
#175255 = CARTESIAN_POINT('Ctrl Pts',(-27.9229728782281,-12.989236405783,
111.625017894805)) ;
#175256 = CARTESIAN_POINT('Ctrl Pts',(-27.8882165238537,-13.269049028932,
111.554529970124)) ;
#175257 = CARTESIAN_POINT('Ctrl Pts',(-27.9116524234391,-13.279851801729,
111.625911936813)) ;
#175258 = CARTESIAN_POINT('Ctrl Pts',(-27.8378485754109,-13.2798519083315,
111.650142964463)) ;
#175259 = CARTESIAN_POINT('Ctrl Pts',(-27.7640447273828,-13.279852014934,
111.674373992113)) ;
#175260 = CARTESIAN_POINT('Ctrl Pts',(-27.7406088277974,-13.269049242137,
111.602992025424)) ;
#175261 = CARTESIAN_POINT('Ctrl Pts',(-27.717172928212,-13.2582464693401,
111.531610058736)) ;
#175262 = CARTESIAN_POINT('Ctrl Pts',(-27.7909767762402,-13.2582463627375,
111.507379031086)) ;
#175263 = CARTESIAN_POINT('Ctrl Pts',(-27.8647806242683,-13.258246256135,
111.483148003436)) ;
#175264 = CARTESIAN_POINT('Ctrl Pts',(-27.8882165238537,-13.269049028932,
111.554529970124)) ;
#175265 = CARTESIAN_POINT('Ctrl Pts',(-27.8773822820719,-13.560604521515,
111.557039247534)) ;
#175266 = CARTESIAN_POINT('Ctrl Pts',(-27.9008745338674,-13.5510680943663,
111.628592853945)) ;
#175267 = CARTESIAN_POINT('Ctrl Pts',(-27.827070694905,-13.5510682019353,
111.652823909208)) ;
#175268 = CARTESIAN_POINT('Ctrl Pts',(-27.7532668559424,-13.5510683095042,
111.67705496447)) ;
#175269 = CARTESIAN_POINT('Ctrl Pts',(-27.7297746041469,-13.5606047366529,
111.605501358059)) ;
#175270 = CARTESIAN_POINT('Ctrl Pts',(-27.7062823523514,-13.5701411638016,
111.533947751647)) ;
#175271 = CARTESIAN_POINT('Ctrl Pts',(-27.7800861913139,-13.5701410562327,
111.509716696385)) ;
#175272 = CARTESIAN_POINT('Ctrl Pts',(-27.8538900302764,-13.5701409486637,
111.485485641123)) ;
#175273 = CARTESIAN_POINT('Ctrl Pts',(-27.8773822820719,-13.560604521515,
111.557039247534)) ;
#175274 = CARTESIAN_POINT('Ctrl Pts',(-27.8908274487406,-13.8423158077137,
111.633558215579)) ;
#175275 = CARTESIAN_POINT('Ctrl Pts',(-27.912680022347,-13.8130971975032,
111.700117626799)) ;
#175276 = CARTESIAN_POINT('Ctrl Pts',(-27.8388761921,-13.8130972967894,111.724348708607)) ;
#175277 = CARTESIAN_POINT('Ctrl Pts',(-27.765072361853,-13.8130973960757,
111.748579790416)) ;
#175278 = CARTESIAN_POINT('Ctrl Pts',(-27.7432197882467,-13.8423160062862,
111.682020379196)) ;
#175279 = CARTESIAN_POINT('Ctrl Pts',(-27.7213672146404,-13.8715346164967,
111.615460967976)) ;
#175280 = CARTESIAN_POINT('Ctrl Pts',(-27.7951710448874,-13.8715345172104,
111.591229886167)) ;
#175281 = CARTESIAN_POINT('Ctrl Pts',(-27.8689748751343,-13.8715344179242,
111.566998804359)) ;
#175282 = CARTESIAN_POINT('Ctrl Pts',(-27.8908274487406,-13.8423158077137,
111.633558215579)) ;
#175283 = CARTESIAN_POINT('Ctrl Pts',(-27.9264541508921,-14.0920492190499,
111.777413603601)) ;
#175284 = CARTESIAN_POINT('Ctrl Pts',(-27.9451204832836,-14.0453516515009,
111.834268238205)) ;
#175285 = CARTESIAN_POINT('Ctrl Pts',(-27.8713166605116,-14.0453517349523,
111.858499342782)) ;
#175286 = CARTESIAN_POINT('Ctrl Pts',(-27.7975128377397,-14.0453518184037,
111.882730447358)) ;
#175287 = CARTESIAN_POINT('Ctrl Pts',(-27.7788465053482,-14.0920493859528,
111.825875812753)) ;
#175288 = CARTESIAN_POINT('Ctrl Pts',(-27.7601801729567,-14.1387469535018,
111.769021178149)) ;
#175289 = CARTESIAN_POINT('Ctrl Pts',(-27.8339839957287,-14.1387468700504,
111.744790073572)) ;
#175290 = CARTESIAN_POINT('Ctrl Pts',(-27.9077878185007,-14.138746786599,
111.720558968996)) ;
#175291 = CARTESIAN_POINT('Ctrl Pts',(-27.9264541508921,-14.0920492190499,
111.777413603601)) ;
#175292 = CARTESIAN_POINT('Ctrl Pts',(-27.9814414275838,-14.2950965364046,
111.980481540082)) ;
#175293 = CARTESIAN_POINT('Ctrl Pts',(-27.9955603817965,-14.2341530477557,
112.02348559453)) ;
#175294 = CARTESIAN_POINT('Ctrl Pts',(-27.9217565644726,-14.2341531086755,
112.0477167157)) ;
#175295 = CARTESIAN_POINT('Ctrl Pts',(-27.8479527471487,-14.2341531695953,
112.07194783687)) ;
#175296 = CARTESIAN_POINT('Ctrl Pts',(-27.833833792936,-14.2950966582441,
112.028943782423)) ;
#175297 = CARTESIAN_POINT('Ctrl Pts',(-27.8197148387233,-14.3560401468929,
111.985939727975)) ;
#175298 = CARTESIAN_POINT('Ctrl Pts',(-27.8935186560472,-14.3560400859732,
111.961708606805)) ;
#175299 = CARTESIAN_POINT('Ctrl Pts',(-27.9673224733711,-14.3560400250534,
111.937477485635)) ;
#175300 = CARTESIAN_POINT('Ctrl Pts',(-27.9814414275838,-14.2950965364046,
111.980481540082)) ;
#175301 = CARTESIAN_POINT('Ctrl Pts',(-28.0507461501417,-14.434335219557,
112.227053017501)) ;
#175302 = CARTESIAN_POINT('Ctrl Pts',(-28.0593134198574,-14.3635791231233,
112.25314753681)) ;
#175303 = CARTESIAN_POINT('Ctrl Pts',(-27.9855096054518,-14.3635791582218,
112.277378666869)) ;
#175304 = CARTESIAN_POINT('Ctrl Pts',(-27.9117057910462,-14.3635791933204,
112.301609796927)) ;
#175305 = CARTESIAN_POINT('Ctrl Pts',(-27.9031385213306,-14.4343352897541,
112.275515277618)) ;
#175306 = CARTESIAN_POINT('Ctrl Pts',(-27.8945712516149,-14.5050913861879,
112.249420758309)) ;
#175307 = CARTESIAN_POINT('Ctrl Pts',(-27.9683750660205,-14.5050913510893,
112.22518962825)) ;
#175308 = CARTESIAN_POINT('Ctrl Pts',(-28.0421788804261,-14.5050913159907,
112.200958498192)) ;
#175309 = CARTESIAN_POINT('Ctrl Pts',(-28.0507461501417,-14.434335219557,
112.227053017501)) ;
#175310 = CARTESIAN_POINT('Ctrl Pts',(-28.1282740613558,-14.5007530721094,
112.498487082343)) ;
#175311 = CARTESIAN_POINT('Ctrl Pts',(-28.1307109212733,-14.4252541131167,
112.505909362619)) ;
#175312 = CARTESIAN_POINT('Ctrl Pts',(-28.0569071075311,-14.4252541219683,
112.530140494699)) ;
#175313 = CARTESIAN_POINT('Ctrl Pts',(-27.9831032937888,-14.4252541308198,
112.554371626778)) ;
#175314 = CARTESIAN_POINT('Ctrl Pts',(-27.9806664338714,-14.5007530898126,
112.546949346501)) ;
#175315 = CARTESIAN_POINT('Ctrl Pts',(-27.9782295739539,-14.5762520488053,
112.539527066225)) ;
#175316 = CARTESIAN_POINT('Ctrl Pts',(-28.0520333876961,-14.5762520399537,
112.515295934145)) ;
#175317 = CARTESIAN_POINT('Ctrl Pts',(-28.1258372014383,-14.5762520311022,
112.491064802066)) ;
#175318 = CARTESIAN_POINT('Ctrl Pts',(-28.1282740613558,-14.5007530721094,
112.498487082343)) ;
#175319 = CARTESIAN_POINT('Ctrl Pts',(-28.2086863670135,-14.4901437351793,
112.778942561062)) ;
#175320 = CARTESIAN_POINT('Ctrl Pts',(-28.204777466643,-14.415271701562,112.767036679503)) ;
#175321 = CARTESIAN_POINT('Ctrl Pts',(-28.1309736506996,-14.4152716856427,
112.791267804878)) ;
#175322 = CARTESIAN_POINT('Ctrl Pts',(-28.0571698347562,-14.4152716697234,
112.815498930253)) ;
#175323 = CARTESIAN_POINT('Ctrl Pts',(-28.0610787351267,-14.4901437033406,
112.827404811812)) ;
#175324 = CARTESIAN_POINT('Ctrl Pts',(-28.0649876354972,-14.5650157369579,
112.83931069337)) ;
#175325 = CARTESIAN_POINT('Ctrl Pts',(-28.1387914514406,-14.5650157528772,
112.815079567995)) ;
#175326 = CARTESIAN_POINT('Ctrl Pts',(-28.2125952673839,-14.5650157687965,
112.79084844262)) ;
#175327 = CARTESIAN_POINT('Ctrl Pts',(-28.2086863670135,-14.4901437351793,
112.778942561062)) ;
#175328 = CARTESIAN_POINT('Ctrl Pts',(-28.2850462508329,-14.402041943339,
113.047107750682)) ;
#175329 = CARTESIAN_POINT('Ctrl Pts',(-28.2750637657936,-14.3332076954044,
113.016702710337)) ;
#175330 = CARTESIAN_POINT('Ctrl Pts',(-28.2012599453933,-14.3332076598222,
113.040933822138)) ;
#175331 = CARTESIAN_POINT('Ctrl Pts',(-28.127456124993,-14.33320762424,113.065164933938)) ;
#175332 = CARTESIAN_POINT('Ctrl Pts',(-28.1374386100323,-14.4020418721746,
113.095569974282)) ;
#175333 = CARTESIAN_POINT('Ctrl Pts',(-28.1474210950715,-14.4708761201093,
113.125975014626)) ;
#175334 = CARTESIAN_POINT('Ctrl Pts',(-28.2212249154718,-14.4708761556915,
113.101743902826)) ;
#175335 = CARTESIAN_POINT('Ctrl Pts',(-28.2950287358721,-14.4708761912736,
113.077512791026)) ;
#175336 = CARTESIAN_POINT('Ctrl Pts',(-28.2850462508329,-14.402041943339,
113.047107750682)) ;
#175337 = CARTESIAN_POINT('Ctrl Pts',(-28.3507008692899,-14.243691286176,
113.282525581938)) ;
#175338 = CARTESIAN_POINT('Ctrl Pts',(-28.3353858951182,-14.18580899599,113.23587864023)) ;
#175339 = CARTESIAN_POINT('Ctrl Pts',(-28.2615820692535,-14.1858089469242,
113.260109735386)) ;
#175340 = CARTESIAN_POINT('Ctrl Pts',(-28.1877782433888,-14.1858088978584,
113.284340830543)) ;
#175341 = CARTESIAN_POINT('Ctrl Pts',(-28.2030932175605,-14.2436911880444,
113.33098777225)) ;
#175342 = CARTESIAN_POINT('Ctrl Pts',(-28.2184081917321,-14.3015734782304,
113.377634713958)) ;
#175343 = CARTESIAN_POINT('Ctrl Pts',(-28.2922120175968,-14.3015735272962,
113.353403618801)) ;
#175344 = CARTESIAN_POINT('Ctrl Pts',(-28.3660158434615,-14.301573576362,
113.329172523645)) ;
#175345 = CARTESIAN_POINT('Ctrl Pts',(-28.3507008692899,-14.243691286176,
113.282525581938)) ;
#175346 = CARTESIAN_POINT('Ctrl Pts',(-28.4004336980104,-14.0272168477211,
113.469327044574)) ;
#175347 = CARTESIAN_POINT('Ctrl Pts',(-28.3808923587898,-13.9843615039812,
113.409807276976)) ;
#175348 = CARTESIAN_POINT('Ctrl Pts',(-28.3070885270855,-13.9843614472663,
113.434038354347)) ;
#175349 = CARTESIAN_POINT('Ctrl Pts',(-28.2332846953813,-13.9843613905514,
113.458269431717)) ;
#175350 = CARTESIAN_POINT('Ctrl Pts',(-28.252826034602,-14.0272167342913,
113.517789199314)) ;
#175351 = CARTESIAN_POINT('Ctrl Pts',(-28.2723673738227,-14.0700720780313,
113.577308966911)) ;
#175352 = CARTESIAN_POINT('Ctrl Pts',(-28.3461712055269,-14.0700721347462,
113.553077889541)) ;
#175353 = CARTESIAN_POINT('Ctrl Pts',(-28.4199750372311,-14.0700721914611,
113.528846812171)) ;
#175354 = CARTESIAN_POINT('Ctrl Pts',(-28.4004336980104,-14.0272168477211,
113.469327044574)) ;
#175355 = CARTESIAN_POINT('Ctrl Pts',(-28.4302808069805,-13.7664028194368,
113.595698173527)) ;
#175356 = CARTESIAN_POINT('Ctrl Pts',(-28.4078921270372,-13.7416926429616,
113.527505865666)) ;
#175357 = CARTESIAN_POINT('Ctrl Pts',(-28.3340882893571,-13.7416925860971,
113.551736924834)) ;
#175358 = CARTESIAN_POINT('Ctrl Pts',(-28.260284451677,-13.7416925292327,
113.575967984003)) ;
#175359 = CARTESIAN_POINT('Ctrl Pts',(-28.2826731316204,-13.7664027057079,
113.644160291865)) ;
#175360 = CARTESIAN_POINT('Ctrl Pts',(-28.3050618115637,-13.791112882183,
113.712352599726)) ;
#175361 = CARTESIAN_POINT('Ctrl Pts',(-28.3788656492438,-13.7911129390475,
113.688121540558)) ;
#175362 = CARTESIAN_POINT('Ctrl Pts',(-28.4526694869239,-13.7911129959119,
113.663890481389)) ;
#175363 = CARTESIAN_POINT('Ctrl Pts',(-28.4302808069805,-13.7664028194368,
113.595698173527)) ;
#175364 = CARTESIAN_POINT('Ctrl Pts',(-28.4370991249928,-13.4798811075686,
113.652008520853)) ;
#175365 = CARTESIAN_POINT('Ctrl Pts',(-28.4134648567007,-13.4751386073872,
113.580022352038)) ;
#175366 = CARTESIAN_POINT('Ctrl Pts',(-28.3396610138886,-13.4751385570953,
113.604253395576)) ;
#175367 = CARTESIAN_POINT('Ctrl Pts',(-28.2658571710766,-13.4751385068035,
113.628484439113)) ;
#175368 = CARTESIAN_POINT('Ctrl Pts',(-28.2894914393687,-13.4798810069848,
113.700470607928)) ;
#175369 = CARTESIAN_POINT('Ctrl Pts',(-28.3131257076607,-13.4846235071661,
113.772456776744)) ;
#175370 = CARTESIAN_POINT('Ctrl Pts',(-28.3869295504728,-13.484623557458,
113.748225733206)) ;
#175371 = CARTESIAN_POINT('Ctrl Pts',(-28.4607333932849,-13.4846236077499,
113.723994689669)) ;
#175372 = CARTESIAN_POINT('Ctrl Pts',(-28.4370991249928,-13.4798811075686,
113.652008520853)) ;
#175373 = CARTESIAN_POINT('Ctrl Pts',(-28.4194035357479,-13.1885796838075,
113.633702115265)) ;
#175374 = CARTESIAN_POINT('Ctrl Pts',(-28.3962323278668,-13.2041693777773,
113.563126353939)) ;
#175375 = CARTESIAN_POINT('Ctrl Pts',(-28.3224284815918,-13.2041693384602,
113.587357386929)) ;
#175376 = CARTESIAN_POINT('Ctrl Pts',(-28.2486246353168,-13.2041692991432,
113.611588419919)) ;
#175377 = CARTESIAN_POINT('Ctrl Pts',(-28.2717958431979,-13.1885796051734,
113.682164181245)) ;
#175378 = CARTESIAN_POINT('Ctrl Pts',(-28.294967051079,-13.1729899112036,
113.75273994257)) ;
#175379 = CARTESIAN_POINT('Ctrl Pts',(-28.368770897354,-13.1729899505207,
113.72850890958)) ;
#175380 = CARTESIAN_POINT('Ctrl Pts',(-28.442574743629,-13.1729899898377,
113.70427787659)) ;
#175381 = CARTESIAN_POINT('Ctrl Pts',(-28.4194035357479,-13.1885796838075,
113.633702115265)) ;
#175382 = CARTESIAN_POINT('Ctrl Pts',(-28.378412477973,-12.9166253502417,
113.544054690634)) ;
#175383 = CARTESIAN_POINT('Ctrl Pts',(-28.3573399589958,-12.9512269476541,
113.479871197205)) ;
#175384 = CARTESIAN_POINT('Ctrl Pts',(-28.2835361104725,-12.951226917539,
113.504102223347)) ;
#175385 = CARTESIAN_POINT('Ctrl Pts',(-28.2097322619491,-12.951226887424,
113.528333249489)) ;
#175386 = CARTESIAN_POINT('Ctrl Pts',(-28.2308047809263,-12.9166252900117,
113.592516742918)) ;
#175387 = CARTESIAN_POINT('Ctrl Pts',(-28.2518772999035,-12.8820236925993,
113.656700236347)) ;
#175388 = CARTESIAN_POINT('Ctrl Pts',(-28.3256811484268,-12.8820237227144,
113.632469210205)) ;
#175389 = CARTESIAN_POINT('Ctrl Pts',(-28.3994849969502,-12.8820237528294,
113.608238184063)) ;
#175390 = CARTESIAN_POINT('Ctrl Pts',(-28.378412477973,-12.9166253502417,
113.544054690634)) ;
#175391 = CARTESIAN_POINT('Ctrl Pts',(-28.3154270405176,-12.6775835687805,
113.387804302381)) ;
#175392 = CARTESIAN_POINT('Ctrl Pts',(-28.2979837813993,-12.7289285556427,
113.334674949088)) ;
#175393 = CARTESIAN_POINT('Ctrl Pts',(-28.224179932538,-12.728928538127,113.358905974201)) ;
#175394 = CARTESIAN_POINT('Ctrl Pts',(-28.1503760836767,-12.7289285206112,
113.383136999314)) ;
#175395 = CARTESIAN_POINT('Ctrl Pts',(-28.167819342795,-12.6775835337489,
113.436266352606)) ;
#175396 = CARTESIAN_POINT('Ctrl Pts',(-28.1852626019133,-12.6262385468866,
113.489395705899)) ;
#175397 = CARTESIAN_POINT('Ctrl Pts',(-28.2590664507746,-12.6262385644024,
113.465164680786)) ;
#175398 = CARTESIAN_POINT('Ctrl Pts',(-28.3328702996358,-12.6262385819182,
113.440933655674)) ;
#175399 = CARTESIAN_POINT('Ctrl Pts',(-28.3154270405176,-12.6775835687805,
113.387804302381)) ;
#175400 = CARTESIAN_POINT('Ctrl Pts',(-28.2345655221718,-12.4925681740676,
113.177035535843)) ;
#175401 = CARTESIAN_POINT('Ctrl Pts',(-28.2220068985588,-12.5569096995895,
113.138783994323)) ;
#175402 = CARTESIAN_POINT('Ctrl Pts',(-28.1482030506511,-12.5569096913385,
113.16301502234)) ;
#175403 = CARTESIAN_POINT('Ctrl Pts',(-28.0743992027434,-12.5569096830874,
113.187246050357)) ;
#175404 = CARTESIAN_POINT('Ctrl Pts',(-28.0869578263564,-12.4925681575655,
113.225497591877)) ;
#175405 = CARTESIAN_POINT('Ctrl Pts',(-28.0995164499695,-12.4282266320435,
113.263749133397)) ;
#175406 = CARTESIAN_POINT('Ctrl Pts',(-28.1733202978772,-12.4282266402946,
113.23951810538)) ;
#175407 = CARTESIAN_POINT('Ctrl Pts',(-28.2471241457849,-12.4282266485456,
113.215287077363)) ;
#175408 = CARTESIAN_POINT('Ctrl Pts',(-28.2345655221718,-12.4925681740676,
113.177035535843)) ;
#175409 = CARTESIAN_POINT('Ctrl Pts',(-28.1415965309447,-12.3743553948694,
112.929153696932)) ;
#175410 = CARTESIAN_POINT('Ctrl Pts',(-28.1347803018979,-12.4470477080891,
112.908392562837)) ;
#175411 = CARTESIAN_POINT('Ctrl Pts',(-28.0609764551353,-12.447047705519,
112.932623594341)) ;
#175412 = CARTESIAN_POINT('Ctrl Pts',(-27.9871726083727,-12.4470477029489,
112.956854625846)) ;
#175413 = CARTESIAN_POINT('Ctrl Pts',(-27.9939888374195,-12.3743553897291,
112.977615759942)) ;
#175414 = CARTESIAN_POINT('Ctrl Pts',(-28.0008050664662,-12.3016630765093,
112.998376894037)) ;
#175415 = CARTESIAN_POINT('Ctrl Pts',(-28.0746089132289,-12.3016630790795,
112.974145862532)) ;
#175416 = CARTESIAN_POINT('Ctrl Pts',(-28.1484127599915,-12.3016630816496,
112.949914831028)) ;
#175417 = CARTESIAN_POINT('Ctrl Pts',(-28.1415965309447,-12.3743553948694,
112.929153696932)) ;
#175418 = CARTESIAN_POINT('Ctrl Pts',(-28.0408341461004,-12.3300586716913,
112.657878333238)) ;
#175419 = CARTESIAN_POINT('Ctrl Pts',(-28.0403061969979,-12.4059540802535,
112.656270285379)) ;
#175420 = CARTESIAN_POINT('Ctrl Pts',(-27.9665023523273,-12.4059540807321,
112.680501323255)) ;
#175421 = CARTESIAN_POINT('Ctrl Pts',(-27.8926985076568,-12.4059540812107,
112.704732361132)) ;
#175422 = CARTESIAN_POINT('Ctrl Pts',(-27.8932264567592,-12.3300586726485,
112.706340408992)) ;
#175423 = CARTESIAN_POINT('Ctrl Pts',(-27.8937544058617,-12.2541632640863,
112.707948456852)) ;
#175424 = CARTESIAN_POINT('Ctrl Pts',(-27.9675582505323,-12.2541632636077,
112.683717418975)) ;
#175425 = CARTESIAN_POINT('Ctrl Pts',(-28.0413620952029,-12.254163263129,
112.659486381098)) ;
#175426 = CARTESIAN_POINT('Ctrl Pts',(-28.0408341461004,-12.3300586716913,
112.657878333238)) ;
#175427 = CARTESIAN_POINT('Ctrl Pts',(-27.9401092157344,-12.3643855283945,
112.386554127362)) ;
#175428 = CARTESIAN_POINT('Ctrl Pts',(-27.9458798751018,-12.4379977305632,
112.404130624705)) ;
#175429 = CARTESIAN_POINT('Ctrl Pts',(-27.8720760317625,-12.4379977307755,
112.428361666637)) ;
#175430 = CARTESIAN_POINT('Ctrl Pts',(-27.7982721884232,-12.4379977309879,
112.452592708569)) ;
#175431 = CARTESIAN_POINT('Ctrl Pts',(-27.7925015290558,-12.3643855288192,
112.435016211225)) ;
#175432 = CARTESIAN_POINT('Ctrl Pts',(-27.7867308696884,-12.2907733266505,
112.417439713881)) ;
#175433 = CARTESIAN_POINT('Ctrl Pts',(-27.8605347130277,-12.2907733264382,
112.39320867195)) ;
#175434 = CARTESIAN_POINT('Ctrl Pts',(-27.934338556367,-12.2907733262258,
112.368977630018)) ;
#175435 = CARTESIAN_POINT('Ctrl Pts',(-27.9401092157344,-12.3643855283945,
112.386554127362)) ;
#175436 = CARTESIAN_POINT('Ctrl Pts',(-27.8457507930179,-12.4735026256636,
112.134502190906)) ;
#175437 = CARTESIAN_POINT('Ctrl Pts',(-27.857387277919,-12.5396050352221,
112.169945046424)) ;
#175438 = CARTESIAN_POINT('Ctrl Pts',(-27.7835834352188,-12.5396050341181,
112.194176090302)) ;
#175439 = CARTESIAN_POINT('Ctrl Pts',(-27.7097795925186,-12.5396050330141,
112.21840713418)) ;
#175440 = CARTESIAN_POINT('Ctrl Pts',(-27.6981431076176,-12.4735026234556,
112.182964278663)) ;
#175441 = CARTESIAN_POINT('Ctrl Pts',(-27.6865066227165,-12.4074002138971,
112.147521423146)) ;
#175442 = CARTESIAN_POINT('Ctrl Pts',(-27.7603104654167,-12.4074002150011,
112.123290379267)) ;
#175443 = CARTESIAN_POINT('Ctrl Pts',(-27.8341143081169,-12.4074002161051,
112.099059335389)) ;
#175444 = CARTESIAN_POINT('Ctrl Pts',(-27.8457507930179,-12.4735026256636,
112.134502190906)) ;
#175445 = CARTESIAN_POINT('Ctrl Pts',(-27.7630645931825,-12.6505044221707,
111.918129912256)) ;
#175446 = CARTESIAN_POINT('Ctrl Pts',(-27.77975811883,-12.7043450691342,111.968975697955)) ;
#175447 = CARTESIAN_POINT('Ctrl Pts',(-27.7059542761778,-12.7043450666146,
111.99320674198)) ;
#175448 = CARTESIAN_POINT('Ctrl Pts',(-27.6321504335255,-12.7043450640951,
112.017437786004)) ;
#175449 = CARTESIAN_POINT('Ctrl Pts',(-27.615456907878,-12.6505044171317,
111.966592000305)) ;
#175450 = CARTESIAN_POINT('Ctrl Pts',(-27.5987633822305,-12.5966637701682,
111.915746214605)) ;
#175451 = CARTESIAN_POINT('Ctrl Pts',(-27.6725672248828,-12.5966637726878,
111.891515170581)) ;
#175452 = CARTESIAN_POINT('Ctrl Pts',(-27.746371067535,-12.5966637752073,
111.867284126556)) ;
#175453 = CARTESIAN_POINT('Ctrl Pts',(-27.7630645931825,-12.6505044221707,
111.918129912256)) ;
#175454 = CARTESIAN_POINT('Ctrl Pts',(-27.6975343400792,-12.883421947767,
111.754113424243)) ;
#175455 = CARTESIAN_POINT('Ctrl Pts',(-27.7180922115168,-12.9210776018657,
111.816729383672)) ;
#175456 = CARTESIAN_POINT('Ctrl Pts',(-27.6442883682897,-12.9210776004055,
111.840960425945)) ;
#175457 = CARTESIAN_POINT('Ctrl Pts',(-27.5704845250626,-12.9210775989452,
111.865191468218)) ;
#175458 = CARTESIAN_POINT('Ctrl Pts',(-27.5499266536251,-12.8834219448465,
111.80257550879)) ;
#175459 = CARTESIAN_POINT('Ctrl Pts',(-27.5293687821876,-12.8457662907479,
111.739959549362)) ;
#175460 = CARTESIAN_POINT('Ctrl Pts',(-27.6031726254146,-12.8457662922081,
111.715728507089)) ;
#175461 = CARTESIAN_POINT('Ctrl Pts',(-27.6769764686417,-12.8457662936684,
111.691497464815)) ;
#175462 = CARTESIAN_POINT('Ctrl Pts',(-27.6975343400792,-12.883421947767,
111.754113424243)) ;
#175463 = CARTESIAN_POINT('Ctrl Pts',(-27.6534936872668,-13.1527514798463,
111.655293821054)) ;
#175464 = CARTESIAN_POINT('Ctrl Pts',(-27.6764258063521,-13.1716560829413,
111.725141355679)) ;
#175465 = CARTESIAN_POINT('Ctrl Pts',(-27.6026219627207,-13.1716560841151,
111.749372396721)) ;
#175466 = CARTESIAN_POINT('Ctrl Pts',(-27.5288181190892,-13.1716560852888,
111.773603437763)) ;
#175467 = CARTESIAN_POINT('Ctrl Pts',(-27.5058860000039,-13.1527514821937,
111.703755903138)) ;
#175468 = CARTESIAN_POINT('Ctrl Pts',(-27.4829538809186,-13.1338468790986,
111.633908368513)) ;
#175469 = CARTESIAN_POINT('Ctrl Pts',(-27.55675772455,-13.1338468779249,111.609677327471)) ;
#175470 = CARTESIAN_POINT('Ctrl Pts',(-27.6305615681814,-13.1338468767512,
111.585446286429)) ;
#175471 = CARTESIAN_POINT('Ctrl Pts',(-27.6534936872668,-13.1527514798463,
111.655293821054)) ;
#175472 = CARTESIAN_POINT('Ctrl Pts',(-27.6327547212792,-13.4437023579035,
111.627785242889)) ;
#175473 = CARTESIAN_POINT('Ctrl Pts',(-27.6564307043907,-13.4423185568972,
111.699898467197)) ;
#175474 = CARTESIAN_POINT('Ctrl Pts',(-27.5826268608532,-13.442318564338,
111.724129508525)) ;
#175475 = CARTESIAN_POINT('Ctrl Pts',(-27.5088230173157,-13.4423185717788,
111.748360549853)) ;
#175476 = CARTESIAN_POINT('Ctrl Pts',(-27.4851470342043,-13.443702372785,
111.676247325545)) ;
#175477 = CARTESIAN_POINT('Ctrl Pts',(-27.4614710510928,-13.4450861737913,
111.604134101237)) ;
#175478 = CARTESIAN_POINT('Ctrl Pts',(-27.5352748946303,-13.4450861663505,
111.579903059909)) ;
#175479 = CARTESIAN_POINT('Ctrl Pts',(-27.6090787381678,-13.4450861589097,
111.555672018581)) ;
#175480 = CARTESIAN_POINT('Ctrl Pts',(-27.6327547212792,-13.4437023579035,
111.627785242889)) ;
#175481 = CARTESIAN_POINT('Ctrl Pts',(-27.6365620199519,-13.7306193771303,
111.674768692016)) ;
#175482 = CARTESIAN_POINT('Ctrl Pts',(-27.6592742254984,-13.7091999974399,
111.74394640525)) ;
#175483 = CARTESIAN_POINT('Ctrl Pts',(-27.5854703831493,-13.7092000104109,
111.768177450198)) ;
#175484 = CARTESIAN_POINT('Ctrl Pts',(-27.5116665408002,-13.7092000233819,
111.792408495146)) ;
#175485 = CARTESIAN_POINT('Ctrl Pts',(-27.4889543352537,-13.7306194030722,
111.723230781911)) ;
#175486 = CARTESIAN_POINT('Ctrl Pts',(-27.4662421297072,-13.7520387827626,
111.654053068677)) ;
#175487 = CARTESIAN_POINT('Ctrl Pts',(-27.5400459720564,-13.7520387697916,
111.629822023729)) ;
#175488 = CARTESIAN_POINT('Ctrl Pts',(-27.6138498144055,-13.7520387568206,
111.605590978781)) ;
#175489 = CARTESIAN_POINT('Ctrl Pts',(-27.6365620199519,-13.7306193771303,
111.674768692016)) ;
#175490 = CARTESIAN_POINT('Ctrl Pts',(-27.6633603539813,-13.9949086675026,
111.791717285722)) ;
#175491 = CARTESIAN_POINT('Ctrl Pts',(-27.6835032907012,-13.9550051326843,
111.853069420544)) ;
#175492 = CARTESIAN_POINT('Ctrl Pts',(-27.609699450319,-13.9550051495312,
111.877300471483)) ;
#175493 = CARTESIAN_POINT('Ctrl Pts',(-27.5358956099367,-13.9550051663781,
111.901531522421)) ;
#175494 = CARTESIAN_POINT('Ctrl Pts',(-27.5157526732168,-13.9949087011963,
111.840179387599)) ;
#175495 = CARTESIAN_POINT('Ctrl Pts',(-27.4956097364969,-14.0348122360146,
111.778827252776)) ;
#175496 = CARTESIAN_POINT('Ctrl Pts',(-27.5694135768792,-14.0348122191677,
111.754596201838)) ;
#175497 = CARTESIAN_POINT('Ctrl Pts',(-27.6432174172614,-14.0348122023208,
111.730365150899)) ;
#175498 = CARTESIAN_POINT('Ctrl Pts',(-27.6633603539813,-13.9949086675026,
111.791717285722)) ;
#175499 = CARTESIAN_POINT('Ctrl Pts',(-27.7111136241826,-14.2196906214034,
111.972774236008)) ;
#175500 = CARTESIAN_POINT('Ctrl Pts',(-27.727214755997,-14.1640342666894,
112.021815685053)) ;
#175501 = CARTESIAN_POINT('Ctrl Pts',(-27.653410919021,-14.1640342866179,
112.046046746366)) ;
#175502 = CARTESIAN_POINT('Ctrl Pts',(-27.579607082045,-14.1640343065465,
112.070277807679)) ;
#175503 = CARTESIAN_POINT('Ctrl Pts',(-27.5635059502306,-14.2196906612605,
112.021236358635)) ;
#175504 = CARTESIAN_POINT('Ctrl Pts',(-27.5474048184161,-14.2753470159745,
111.97219490959)) ;
#175505 = CARTESIAN_POINT('Ctrl Pts',(-27.6212086553922,-14.275346996046,
111.947963848277)) ;
#175506 = CARTESIAN_POINT('Ctrl Pts',(-27.6950124923682,-14.2753469761174,
111.923732786964)) ;
#175507 = CARTESIAN_POINT('Ctrl Pts',(-27.7111136241826,-14.2196906214034,
111.972774236008)) ;
#175508 = CARTESIAN_POINT('Ctrl Pts',(-27.7749357041157,-14.3856064052365,
112.20251553552)) ;
#175509 = CARTESIAN_POINT('Ctrl Pts',(-27.7858724825749,-14.3182855334349,
112.235827197368)) ;
#175510 = CARTESIAN_POINT('Ctrl Pts',(-27.7120686490727,-14.3182855505584,
112.260058269261)) ;
#175511 = CARTESIAN_POINT('Ctrl Pts',(-27.6382648155704,-14.318285567682,
112.284289341155)) ;
#175512 = CARTESIAN_POINT('Ctrl Pts',(-27.6273280371112,-14.3856064394836,
112.250977679308)) ;
#175513 = CARTESIAN_POINT('Ctrl Pts',(-27.616391258652,-14.4529273112853,
112.217666017461)) ;
#175514 = CARTESIAN_POINT('Ctrl Pts',(-27.6901950921543,-14.4529272941617,
112.193434945567)) ;
#175515 = CARTESIAN_POINT('Ctrl Pts',(-27.7639989256566,-14.4529272770382,
112.169203873673)) ;
#175516 = CARTESIAN_POINT('Ctrl Pts',(-27.7749357041157,-14.3856064052365,
112.20251553552)) ;
#175517 = CARTESIAN_POINT('Ctrl Pts',(-27.850139433854,-14.4829720573525,
112.467091440401)) ;
#175518 = CARTESIAN_POINT('Ctrl Pts',(-27.8551063751374,-14.4087556909408,
112.482219941263)) ;
#175519 = CARTESIAN_POINT('Ctrl Pts',(-27.7813025454846,-14.4087557009118,
112.506451024881)) ;
#175520 = CARTESIAN_POINT('Ctrl Pts',(-27.7074987158318,-14.4087557108828,
112.530682108499)) ;
#175521 = CARTESIAN_POINT('Ctrl Pts',(-27.7025317745484,-14.4829720772946,
112.515553607637)) ;
#175522 = CARTESIAN_POINT('Ctrl Pts',(-27.6975648332649,-14.5571884437063,
112.500425106775)) ;
#175523 = CARTESIAN_POINT('Ctrl Pts',(-27.7713686629178,-14.5571884337353,
112.476194023157)) ;
#175524 = CARTESIAN_POINT('Ctrl Pts',(-27.8451724925706,-14.5571884237643,
112.451962939539)) ;
#175525 = CARTESIAN_POINT('Ctrl Pts',(-27.850139433854,-14.4829720573525,
112.467091440401)) ;
#175526 = CARTESIAN_POINT('Ctrl Pts',(-27.9301015626753,-14.5039687036518,
112.746047500903)) ;
#175527 = CARTESIAN_POINT('Ctrl Pts',(-27.9287602067411,-14.4281793222941,
112.741961946123)) ;
#175528 = CARTESIAN_POINT('Ctrl Pts',(-27.8549563799724,-14.4281793198172,
112.766193038526)) ;
#175529 = CARTESIAN_POINT('Ctrl Pts',(-27.7811525532036,-14.4281793173403,
112.790424130929)) ;
#175530 = CARTESIAN_POINT('Ctrl Pts',(-27.7824939091379,-14.503968698698,
112.794509685709)) ;
#175531 = CARTESIAN_POINT('Ctrl Pts',(-27.7838352650722,-14.5797580800556,
112.798595240489)) ;
#175532 = CARTESIAN_POINT('Ctrl Pts',(-27.8576390918409,-14.5797580825325,
112.774364148086)) ;
#175533 = CARTESIAN_POINT('Ctrl Pts',(-27.9314429186096,-14.5797580850095,
112.750133055684)) ;
#175534 = CARTESIAN_POINT('Ctrl Pts',(-27.9301015626753,-14.5039687036518,
112.746047500903)) ;
#175535 = CARTESIAN_POINT('Ctrl Pts',(-28.0091089868232,-14.4466173797893,
113.02236063873)) ;
#175536 = CARTESIAN_POINT('Ctrl Pts',(-28.0015114372109,-14.3747219587681,
112.999219727237)) ;
#175537 = CARTESIAN_POINT('Ctrl Pts',(-27.9277076127128,-14.3747219386736,
113.023450826556)) ;
#175538 = CARTESIAN_POINT('Ctrl Pts',(-27.8539037882146,-14.3747219185791,
113.047681925874)) ;
#175539 = CARTESIAN_POINT('Ctrl Pts',(-27.8615013378269,-14.4466173396002,
113.070822837368)) ;
#175540 = CARTESIAN_POINT('Ctrl Pts',(-27.8690988874391,-14.5185127606213,
113.093963748861)) ;
#175541 = CARTESIAN_POINT('Ctrl Pts',(-27.9429027119373,-14.5185127807159,
113.069732649542)) ;
#175542 = CARTESIAN_POINT('Ctrl Pts',(-28.0167065364354,-14.5185128008104,
113.045501550224)) ;
#175543 = CARTESIAN_POINT('Ctrl Pts',(-28.0091089868232,-14.4466173797893,
113.02236063873)) ;
#175544 = CARTESIAN_POINT('Ctrl Pts',(-28.0794461167512,-14.3162716014842,
113.27191318261)) ;
#175545 = CARTESIAN_POINT('Ctrl Pts',(-28.0661960468092,-14.2533730380978,
113.231555606093)) ;
#175546 = CARTESIAN_POINT('Ctrl Pts',(-27.9923922216887,-14.2533729987048,
113.255786703516)) ;
#175547 = CARTESIAN_POINT('Ctrl Pts',(-27.9185883965682,-14.2533729593119,
113.280017800938)) ;
#175548 = CARTESIAN_POINT('Ctrl Pts',(-27.9318384665101,-14.3162715226984,
113.320375377456)) ;
#175549 = CARTESIAN_POINT('Ctrl Pts',(-27.945088536452,-14.3791700860849,
113.360732953973)) ;
#175550 = CARTESIAN_POINT('Ctrl Pts',(-28.0188923615726,-14.3791701254778,
113.33650185655)) ;
#175551 = CARTESIAN_POINT('Ctrl Pts',(-28.0926961866931,-14.3791701648707,
113.312270759127)) ;
#175552 = CARTESIAN_POINT('Ctrl Pts',(-28.0794461167512,-14.3162716014842,
113.27191318261)) ;
#175553 = CARTESIAN_POINT('Ctrl Pts',(-28.1364440614567,-14.1214968775469,
113.480983026046)) ;
#175554 = CARTESIAN_POINT('Ctrl Pts',(-28.1184615726977,-14.0721057771866,
113.426211265236)) ;
#175555 = CARTESIAN_POINT('Ctrl Pts',(-28.044657745267,-14.0721057178665,
113.450442355622)) ;
#175556 = CARTESIAN_POINT('Ctrl Pts',(-27.9708539178362,-14.0721056585463,
113.474673446009)) ;
#175557 = CARTESIAN_POINT('Ctrl Pts',(-27.9888364065952,-14.1214967589066,
113.529445206819)) ;
#175558 = CARTESIAN_POINT('Ctrl Pts',(-28.0068188953542,-14.170887859267,
113.58421696763)) ;
#175559 = CARTESIAN_POINT('Ctrl Pts',(-28.080622722785,-14.1708879185871,
113.559985877244)) ;
#175560 = CARTESIAN_POINT('Ctrl Pts',(-28.1544265502157,-14.1708879779072,
113.535754786857)) ;
#175561 = CARTESIAN_POINT('Ctrl Pts',(-28.1364440614567,-14.1214968775469,
113.480983026046)) ;
#175562 = CARTESIAN_POINT('Ctrl Pts',(-28.1749613485906,-13.8749956323593,
113.633913814206)) ;
#175563 = CARTESIAN_POINT('Ctrl Pts',(-28.153526591033,-13.8427423803111,
113.568626999499)) ;
#175564 = CARTESIAN_POINT('Ctrl Pts',(-28.0797227591213,-13.8427423020325,
113.592858076237)) ;
#175565 = CARTESIAN_POINT('Ctrl Pts',(-28.0059189272095,-13.8427422237539,
113.617089152975)) ;
#175566 = CARTESIAN_POINT('Ctrl Pts',(-28.0273536847671,-13.8749954758022,
113.682375967682)) ;
#175567 = CARTESIAN_POINT('Ctrl Pts',(-28.0487884423247,-13.9072487278505,
113.747662782389)) ;
#175568 = CARTESIAN_POINT('Ctrl Pts',(-28.1225922742364,-13.907248806129,
113.723431705651)) ;
#175569 = CARTESIAN_POINT('Ctrl Pts',(-28.1963961061482,-13.9072488844076,
113.699200628913)) ;
#175570 = CARTESIAN_POINT('Ctrl Pts',(-28.1749613485906,-13.8749956323593,
113.633913814206)) ;
#175571 = CARTESIAN_POINT('Ctrl Pts',(-28.1911734256759,-13.5974682752699,
113.718666176969)) ;
#175572 = CARTESIAN_POINT('Ctrl Pts',(-28.1678437469537,-13.5845442893725,
113.647607738033)) ;
#175573 = CARTESIAN_POINT('Ctrl Pts',(-28.0940399083953,-13.584544198723,
113.671838794527)) ;
#175574 = CARTESIAN_POINT('Ctrl Pts',(-28.0202360698369,-13.5845441080735,
113.69606985102)) ;
#175575 = CARTESIAN_POINT('Ctrl Pts',(-28.0435657485591,-13.597468093971,
113.767128289956)) ;
#175576 = CARTESIAN_POINT('Ctrl Pts',(-28.0668954272813,-13.6103920798684,
113.838186728891)) ;
#175577 = CARTESIAN_POINT('Ctrl Pts',(-28.1406992658397,-13.6103921705179,
113.813955672398)) ;
#175578 = CARTESIAN_POINT('Ctrl Pts',(-28.2145031043981,-13.6103922611673,
113.789724615905)) ;
#175579 = CARTESIAN_POINT('Ctrl Pts',(-28.1911734256759,-13.5974682752699,
113.718666176969)) ;
#175580 = CARTESIAN_POINT('Ctrl Pts',(-28.1836078259768,-13.3070931499256,
113.731008103206)) ;
#175581 = CARTESIAN_POINT('Ctrl Pts',(-28.160040222229,-13.3144232873773,
113.659224982936)) ;
#175582 = CARTESIAN_POINT('Ctrl Pts',(-28.0862363758644,-13.3144231909102,
113.683456015653)) ;
#175583 = CARTESIAN_POINT('Ctrl Pts',(-28.0124325294998,-13.314423094443,
113.70768704837)) ;
#175584 = CARTESIAN_POINT('Ctrl Pts',(-28.0360001332477,-13.3070929569913,
113.77947016864)) ;
#175585 = CARTESIAN_POINT('Ctrl Pts',(-28.0595677369956,-13.2997628195396,
113.851253288911)) ;
#175586 = CARTESIAN_POINT('Ctrl Pts',(-28.1333715833601,-13.2997629160068,
113.827022256194)) ;
#175587 = CARTESIAN_POINT('Ctrl Pts',(-28.2071754297247,-13.2997630124739,
113.802791223477)) ;
#175588 = CARTESIAN_POINT('Ctrl Pts',(-28.1836078259768,-13.3070931499256,
113.731008103206)) ;
#175589 = CARTESIAN_POINT('Ctrl Pts',(-28.1517250328214,-13.0233508116479,
113.669448037719)) ;
#175590 = CARTESIAN_POINT('Ctrl Pts',(-28.1296132234237,-13.0505014151777,
113.602099032054)) ;
#175591 = CARTESIAN_POINT('Ctrl Pts',(-28.0558093685922,-13.0505013202395,
113.626330038982)) ;
#175592 = CARTESIAN_POINT('Ctrl Pts',(-27.9820055137606,-13.0505012253013,
113.65056104591)) ;
#175593 = CARTESIAN_POINT('Ctrl Pts',(-28.0041173231583,-13.0233506217714,
113.717910051575)) ;
#175594 = CARTESIAN_POINT('Ctrl Pts',(-28.0262291325559,-12.9962000182415,
113.785259057239)) ;
#175595 = CARTESIAN_POINT('Ctrl Pts',(-28.1000329873874,-12.9962001131797,
113.761028050311)) ;
#175596 = CARTESIAN_POINT('Ctrl Pts',(-28.173836842219,-12.996200208118,113.736797043383)) ;
#175597 = CARTESIAN_POINT('Ctrl Pts',(-28.1517250328214,-13.0233508116479,
113.669448037719)) ;
#175598 = CARTESIAN_POINT('Ctrl Pts',(-28.0972991812598,-12.7688607554056,
113.539098836946)) ;
#175599 = CARTESIAN_POINT('Ctrl Pts',(-28.0782218167453,-12.8138186885295,
113.480992260729)) ;
#175600 = CARTESIAN_POINT('Ctrl Pts',(-28.0044179538581,-12.8138186042271,
113.505223243121)) ;
#175601 = CARTESIAN_POINT('Ctrl Pts',(-27.930614090971,-12.8138185199248,
113.529454225513)) ;
#175602 = CARTESIAN_POINT('Ctrl Pts',(-27.9496914554855,-12.7688605868009,
113.58756080173)) ;
#175603 = CARTESIAN_POINT('Ctrl Pts',(-27.96876882,-12.723902653677,113.645667377947)) ;
#175604 = CARTESIAN_POINT('Ctrl Pts',(-28.0425726828872,-12.7239027379794,
113.621436395555)) ;
#175605 = CARTESIAN_POINT('Ctrl Pts',(-28.1163765457744,-12.7239028222818,
113.597205413164)) ;
#175606 = CARTESIAN_POINT('Ctrl Pts',(-28.0972991812598,-12.7688607554056,
113.539098836946)) ;
#175607 = CARTESIAN_POINT('Ctrl Pts',(-28.0232821783549,-12.5604071436069,
113.349142464811)) ;
#175608 = CARTESIAN_POINT('Ctrl Pts',(-28.0086100031326,-12.6199846631104,
113.304453384358)) ;
#175609 = CARTESIAN_POINT('Ctrl Pts',(-27.9348061333776,-12.6199845970407,
113.328684345831)) ;
#175610 = CARTESIAN_POINT('Ctrl Pts',(-27.8610022636226,-12.6199845309711,
113.352915307305)) ;
#175611 = CARTESIAN_POINT('Ctrl Pts',(-27.8756744388449,-12.5604070114677,
113.397604387758)) ;
#175612 = CARTESIAN_POINT('Ctrl Pts',(-27.8903466140673,-12.5008294919642,
113.442293468211)) ;
#175613 = CARTESIAN_POINT('Ctrl Pts',(-27.9641504838223,-12.5008295580339,
113.418062506738)) ;
#175614 = CARTESIAN_POINT('Ctrl Pts',(-28.0379543535773,-12.5008296241035,
113.393831545264)) ;
#175615 = CARTESIAN_POINT('Ctrl Pts',(-28.0232821783549,-12.5604071436069,
113.349142464811)) ;
#175616 = CARTESIAN_POINT('Ctrl Pts',(-27.9344209561679,-12.4137261008746,
113.113916473714)) ;
#175617 = CARTESIAN_POINT('Ctrl Pts',(-27.9251979860237,-12.4836322376362,
113.085824792683)) ;
#175618 = CARTESIAN_POINT('Ctrl Pts',(-27.8513941114389,-12.4836321960017,
113.110055739446)) ;
#175619 = CARTESIAN_POINT('Ctrl Pts',(-27.7775902368542,-12.4836321543672,
113.134286686209)) ;
#175620 = CARTESIAN_POINT('Ctrl Pts',(-27.7868132069984,-12.4137260176056,
113.16237836724)) ;
#175621 = CARTESIAN_POINT('Ctrl Pts',(-27.7960361771427,-12.343819880844,
113.190470048271)) ;
#175622 = CARTESIAN_POINT('Ctrl Pts',(-27.8698400517275,-12.3438199224785,
113.166239101509)) ;
#175623 = CARTESIAN_POINT('Ctrl Pts',(-27.9436439263122,-12.343819964113,
113.142008154746)) ;
#175624 = CARTESIAN_POINT('Ctrl Pts',(-27.9344209561679,-12.4137261008746,
113.113916473714)) ;
#175625 = CARTESIAN_POINT('Ctrl Pts',(-27.8363120109697,-12.3387040702925,
112.850499990527)) ;
#175626 = CARTESIAN_POINT('Ctrl Pts',(-27.8331923780007,-12.4139513070211,
112.840998089759)) ;
#175627 = CARTESIAN_POINT('Ctrl Pts',(-27.7593885010528,-12.4139512934304,
112.865229029324)) ;
#175628 = CARTESIAN_POINT('Ctrl Pts',(-27.6855846241048,-12.4139512798397,
112.889459968889)) ;
#175629 = CARTESIAN_POINT('Ctrl Pts',(-27.6887042570738,-12.3387040431111,
112.898961869656)) ;
#175630 = CARTESIAN_POINT('Ctrl Pts',(-27.6918238900428,-12.2634568063825,
112.908463770423)) ;
#175631 = CARTESIAN_POINT('Ctrl Pts',(-27.7656277669908,-12.2634568199732,
112.884232830859)) ;
#175632 = CARTESIAN_POINT('Ctrl Pts',(-27.8394316439388,-12.2634568335639,
112.860001891294)) ;
#175633 = CARTESIAN_POINT('Ctrl Pts',(-27.8363120109697,-12.3387040702925,
112.850499990527)) ;
#175634 = CARTESIAN_POINT('Ctrl Pts',(-27.7346441044334,-12.3410592400664,
112.576417227786)) ;
#175635 = CARTESIAN_POINT('Ctrl Pts',(-27.7378816475841,-12.4162542159503,
112.586278259778)) ;
#175636 = CARTESIAN_POINT('Ctrl Pts',(-27.6640777711242,-12.4162542313705,
112.610509200829)) ;
#175637 = CARTESIAN_POINT('Ctrl Pts',(-27.5902738946642,-12.4162542467908,
112.63474014188)) ;
#175638 = CARTESIAN_POINT('Ctrl Pts',(-27.5870363515135,-12.3410592709069,
112.624879109888)) ;
#175639 = CARTESIAN_POINT('Ctrl Pts',(-27.5837988083628,-12.265864295023,
112.615018077896)) ;
#175640 = CARTESIAN_POINT('Ctrl Pts',(-27.6576026848227,-12.2658642796027,
112.590787136845)) ;
#175641 = CARTESIAN_POINT('Ctrl Pts',(-27.7314065612827,-12.2658642641825,
112.566556195793)) ;
#175642 = CARTESIAN_POINT('Ctrl Pts',(-27.7346441044334,-12.3410592400664,
112.576417227786)) ;
#175643 = CARTESIAN_POINT('Ctrl Pts',(-27.6369370950116,-12.4205041979803,
112.314216816515)) ;
#175644 = CARTESIAN_POINT('Ctrl Pts',(-27.6462685982017,-12.4902644552577,
112.342639067573)) ;
#175645 = CARTESIAN_POINT('Ctrl Pts',(-27.5724647248296,-12.4902644973908,
112.366870018029)) ;
#175646 = CARTESIAN_POINT('Ctrl Pts',(-27.4986608514575,-12.4902645395239,
112.391100968485)) ;
#175647 = CARTESIAN_POINT('Ctrl Pts',(-27.4893293482674,-12.4205042822464,
112.362678717428)) ;
#175648 = CARTESIAN_POINT('Ctrl Pts',(-27.4799978450774,-12.350744024969,
112.334256466371)) ;
#175649 = CARTESIAN_POINT('Ctrl Pts',(-27.5538017184495,-12.3507439828359,
112.310025515914)) ;
#175650 = CARTESIAN_POINT('Ctrl Pts',(-27.6276055918215,-12.3507439407028,
112.285794565458)) ;
#175651 = CARTESIAN_POINT('Ctrl Pts',(-27.6369370950116,-12.4205041979803,
112.314216816515)) ;
#175652 = CARTESIAN_POINT('Ctrl Pts',(-27.5486712808213,-12.5715202421064,
112.080868685751)) ;
#175653 = CARTESIAN_POINT('Ctrl Pts',(-27.563444732966,-12.6308413998765,
112.125866235335)) ;
#175654 = CARTESIAN_POINT('Ctrl Pts',(-27.4896408650169,-12.6308414639116,
112.150097202309)) ;
#175655 = CARTESIAN_POINT('Ctrl Pts',(-27.4158369970678,-12.6308415279467,
112.174328169283)) ;
#175656 = CARTESIAN_POINT('Ctrl Pts',(-27.4010635449232,-12.5715203701767,
112.129330619699)) ;
#175657 = CARTESIAN_POINT('Ctrl Pts',(-27.3862900927785,-12.5121992124066,
112.084333070114)) ;
#175658 = CARTESIAN_POINT('Ctrl Pts',(-27.4600939607276,-12.5121991483715,
112.06010210314)) ;
#175659 = CARTESIAN_POINT('Ctrl Pts',(-27.5338978286767,-12.5121990843364,
112.035871136166)) ;
#175660 = CARTESIAN_POINT('Ctrl Pts',(-27.5486712808213,-12.5715202421064,
112.080868685751)) ;
#175661 = CARTESIAN_POINT('Ctrl Pts',(-27.4757703775428,-12.7831706996134,
111.894290358998)) ;
#175662 = CARTESIAN_POINT('Ctrl Pts',(-27.4949218870949,-12.827803906149,
111.952622765135)) ;
#175663 = CARTESIAN_POINT('Ctrl Pts',(-27.4211180261548,-12.8278039851649,
111.976853753457)) ;
#175664 = CARTESIAN_POINT('Ctrl Pts',(-27.3473141652147,-12.8278040641808,
112.00108474178)) ;
#175665 = CARTESIAN_POINT('Ctrl Pts',(-27.3281626556626,-12.7831708576452,
111.942752335642)) ;
#175666 = CARTESIAN_POINT('Ctrl Pts',(-27.3090111461105,-12.7385376511096,
111.884419929505)) ;
#175667 = CARTESIAN_POINT('Ctrl Pts',(-27.3828150070506,-12.7385375720937,
111.860188941183)) ;
#175668 = CARTESIAN_POINT('Ctrl Pts',(-27.4566188679907,-12.7385374930778,
111.835957952861)) ;
#175669 = CARTESIAN_POINT('Ctrl Pts',(-27.4757703775428,-12.7831706996134,
111.894290358998)) ;
#175670 = CARTESIAN_POINT('Ctrl Pts',(-27.4226294303003,-13.0400861903177,
111.76787608117)) ;
#175671 = CARTESIAN_POINT('Ctrl Pts',(-27.4447864917915,-13.0668491450616,
111.835362913672)) ;
#175672 = CARTESIAN_POINT('Ctrl Pts',(-27.3709826386055,-13.0668492312408,
111.859593925612)) ;
#175673 = CARTESIAN_POINT('Ctrl Pts',(-27.2971787854195,-13.06684931742,111.883824937552)) ;
#175674 = CARTESIAN_POINT('Ctrl Pts',(-27.2750217239283,-13.0400863626762,
111.81633810505)) ;
#175675 = CARTESIAN_POINT('Ctrl Pts',(-27.2528646624371,-13.0133234079323,
111.748851272549)) ;
#175676 = CARTESIAN_POINT('Ctrl Pts',(-27.3266685156231,-13.0133233217531,
111.724620260609)) ;
#175677 = CARTESIAN_POINT('Ctrl Pts',(-27.4004723688091,-13.0133232355738,
111.700389248669)) ;
#175678 = CARTESIAN_POINT('Ctrl Pts',(-27.4226294303003,-13.0400861903177,
111.76787608117)) ;
#175679 = CARTESIAN_POINT('Ctrl Pts',(-27.3922395133834,-13.3242719779506,
111.710785133111)) ;
#175680 = CARTESIAN_POINT('Ctrl Pts',(-27.4158177602532,-13.3312338876365,
111.78260066709)) ;
#175681 = CARTESIAN_POINT('Ctrl Pts',(-27.3420139147462,-13.3312339727679,
111.806831702419)) ;
#175682 = CARTESIAN_POINT('Ctrl Pts',(-27.2682100692392,-13.3312340578993,
111.831062737749)) ;
#175683 = CARTESIAN_POINT('Ctrl Pts',(-27.2446318223695,-13.3242721482135,
111.75924720377)) ;
#175684 = CARTESIAN_POINT('Ctrl Pts',(-27.2210535754997,-13.3173102385276,
111.687431669791)) ;
#175685 = CARTESIAN_POINT('Ctrl Pts',(-27.2948574210066,-13.3173101533962,
111.663200634461)) ;
#175686 = CARTESIAN_POINT('Ctrl Pts',(-27.3686612665136,-13.3173100682647,
111.638969599132)) ;
#175687 = CARTESIAN_POINT('Ctrl Pts',(-27.3922395133834,-13.3242719779506,
111.710785133111)) ;
#175688 = CARTESIAN_POINT('Ctrl Pts',(-27.3860860135596,-13.6152878377403,
111.727526925979)) ;
#175689 = CARTESIAN_POINT('Ctrl Pts',(-27.4093952705665,-13.601941852712,
111.798523160376)) ;
#175690 = CARTESIAN_POINT('Ctrl Pts',(-27.3355914317948,-13.6019419294696,
111.82275421622)) ;
#175691 = CARTESIAN_POINT('Ctrl Pts',(-27.2617875930231,-13.6019420062272,
111.846985272064)) ;
#175692 = CARTESIAN_POINT('Ctrl Pts',(-27.2384783360162,-13.6152879912555,
111.775989037666)) ;
#175693 = CARTESIAN_POINT('Ctrl Pts',(-27.2151690790093,-13.6286339762838,
111.704992803269)) ;
#175694 = CARTESIAN_POINT('Ctrl Pts',(-27.288972917781,-13.6286338995262,
111.680761747426)) ;
#175695 = CARTESIAN_POINT('Ctrl Pts',(-27.3627767565527,-13.6286338227686,
111.656530691582)) ;
#175696 = CARTESIAN_POINT('Ctrl Pts',(-27.3860860135596,-13.6152878377403,
111.727526925979)) ;
#175697 = CARTESIAN_POINT('Ctrl Pts',(-27.4038644204004,-13.8920338673762,
111.817147898947)) ;
#175698 = CARTESIAN_POINT('Ctrl Pts',(-27.4252336909941,-13.8593453805719,
111.882235247896)) ;
#175699 = CARTESIAN_POINT('Ctrl Pts',(-27.3514298573554,-13.8593454436439,
111.906466319374)) ;
#175700 = CARTESIAN_POINT('Ctrl Pts',(-27.2776260237166,-13.859345506716,
111.930697390851)) ;
#175701 = CARTESIAN_POINT('Ctrl Pts',(-27.2562567531229,-13.8920339935203,
111.865610041903)) ;
#175702 = CARTESIAN_POINT('Ctrl Pts',(-27.2348874825291,-13.9247224803246,
111.800522692954)) ;
#175703 = CARTESIAN_POINT('Ctrl Pts',(-27.3086913161678,-13.9247224172525,
111.776291621476)) ;
#175704 = CARTESIAN_POINT('Ctrl Pts',(-27.3824951498066,-13.9247223541804,
111.752060549998)) ;
#175705 = CARTESIAN_POINT('Ctrl Pts',(-27.4038644204004,-13.8920338673762,
111.817147898947)) ;
#175706 = CARTESIAN_POINT('Ctrl Pts',(-27.4434672264958,-14.1346381572922,
111.973208058208)) ;
#175707 = CARTESIAN_POINT('Ctrl Pts',(-27.4613705016364,-14.0849615058488,
112.027738544396)) ;
#175708 = CARTESIAN_POINT('Ctrl Pts',(-27.3875666712477,-14.0849615523416,
112.051969625773)) ;
#175709 = CARTESIAN_POINT('Ctrl Pts',(-27.3137628408591,-14.0849615988343,
112.07620070715)) ;
#175710 = CARTESIAN_POINT('Ctrl Pts',(-27.2958595657186,-14.1346382502777,
112.021670220963)) ;
#175711 = CARTESIAN_POINT('Ctrl Pts',(-27.277956290578,-14.1843149017211,
111.967139734775)) ;
#175712 = CARTESIAN_POINT('Ctrl Pts',(-27.3517601209666,-14.1843148552283,
111.942908653398)) ;
#175713 = CARTESIAN_POINT('Ctrl Pts',(-27.4255639513552,-14.1843148087356,
111.91867757202)) ;
#175714 = CARTESIAN_POINT('Ctrl Pts',(-27.4434672264958,-14.1346381572922,
111.973208058208)) ;
#175715 = CARTESIAN_POINT('Ctrl Pts',(-27.5014596989945,-14.3262307223465,
112.185343141529)) ;
#175716 = CARTESIAN_POINT('Ctrl Pts',(-27.5146064763552,-14.263101480961,
112.225386103109)) ;
#175717 = CARTESIAN_POINT('Ctrl Pts',(-27.4408026470349,-14.2631015098285,
112.24961718774)) ;
#175718 = CARTESIAN_POINT('Ctrl Pts',(-27.3669988177146,-14.263101538696,
112.273848272371)) ;
#175719 = CARTESIAN_POINT('Ctrl Pts',(-27.3538520403539,-14.3262307800815,
112.233805310791)) ;
#175720 = CARTESIAN_POINT('Ctrl Pts',(-27.3407052629932,-14.3893600214671,
112.193762349211)) ;
#175721 = CARTESIAN_POINT('Ctrl Pts',(-27.4145090923135,-14.3893599925996,
112.16953126458)) ;
#175722 = CARTESIAN_POINT('Ctrl Pts',(-27.4883129216338,-14.3893599637321,
112.145300179949)) ;
#175723 = CARTESIAN_POINT('Ctrl Pts',(-27.5014596989945,-14.3262307223465,
112.185343141529)) ;
#175724 = CARTESIAN_POINT('Ctrl Pts',(-27.572610257217,-14.4523301137118,
112.437438559264)) ;
#175725 = CARTESIAN_POINT('Ctrl Pts',(-27.5800769215645,-14.380300846747,
112.460180813242)) ;
#175726 = CARTESIAN_POINT('Ctrl Pts',(-27.5062730917788,-14.3803008602231,
112.484411896455)) ;
#175727 = CARTESIAN_POINT('Ctrl Pts',(-27.432469261993,-14.3803008736991,
112.508642979669)) ;
#175728 = CARTESIAN_POINT('Ctrl Pts',(-27.4250025976456,-14.4523301406639,
112.485900725692)) ;
#175729 = CARTESIAN_POINT('Ctrl Pts',(-27.4175359332981,-14.5243594076287,
112.463158471714)) ;
#175730 = CARTESIAN_POINT('Ctrl Pts',(-27.4913397630838,-14.5243593941527,
112.438927388501)) ;
#175731 = CARTESIAN_POINT('Ctrl Pts',(-27.5651435928695,-14.5243593806767,
112.414696305287)) ;
#175732 = CARTESIAN_POINT('Ctrl Pts',(-27.572610257217,-14.4523301137118,
112.437438559264)) ;
#175733 = CARTESIAN_POINT('Ctrl Pts',(-27.6514424913783,-14.5048566464616,
112.713014331691)) ;
#175734 = CARTESIAN_POINT('Ctrl Pts',(-27.6526823497262,-14.4290505733795,
112.716790739453)) ;
#175735 = CARTESIAN_POINT('Ctrl Pts',(-27.5788785178575,-14.4290505742608,
112.741021816322)) ;
#175736 = CARTESIAN_POINT('Ctrl Pts',(-27.5050746859887,-14.429050575142,
112.765252893191)) ;
#175737 = CARTESIAN_POINT('Ctrl Pts',(-27.5038348276408,-14.5048566482241,
112.761476485429)) ;
#175738 = CARTESIAN_POINT('Ctrl Pts',(-27.5025949692929,-14.5806627213062,
112.757700077666)) ;
#175739 = CARTESIAN_POINT('Ctrl Pts',(-27.5763988011616,-14.580662720425,
112.733469000797)) ;
#175740 = CARTESIAN_POINT('Ctrl Pts',(-27.6502026330304,-14.5806627195438,
112.709237923928)) ;
#175741 = CARTESIAN_POINT('Ctrl Pts',(-27.6514424913783,-14.5048566464616,
112.713014331691)) ;
#175742 = CARTESIAN_POINT('Ctrl Pts',(-27.7316184422369,-14.4792282215674,
112.992772623)) ;
#175743 = CARTESIAN_POINT('Ctrl Pts',(-27.7265262449823,-14.405096385773,
112.977262611251)) ;
#175744 = CARTESIAN_POINT('Ctrl Pts',(-27.6527224099425,-14.4050963789129,
113.001493678461)) ;
#175745 = CARTESIAN_POINT('Ctrl Pts',(-27.5789185749027,-14.4050963720528,
113.025724745672)) ;
#175746 = CARTESIAN_POINT('Ctrl Pts',(-27.5840107721573,-14.4792282078472,
113.041234757421)) ;
#175747 = CARTESIAN_POINT('Ctrl Pts',(-27.5891029694118,-14.5533600436416,
113.056744769171)) ;
#175748 = CARTESIAN_POINT('Ctrl Pts',(-27.6629068044517,-14.5533600505017,
113.03251370196)) ;
#175749 = CARTESIAN_POINT('Ctrl Pts',(-27.7367106394915,-14.5533600573618,
113.00828263475)) ;
#175750 = CARTESIAN_POINT('Ctrl Pts',(-27.7316184422369,-14.4792282215674,
112.992772623)) ;
#175751 = CARTESIAN_POINT('Ctrl Pts',(-27.8061587870981,-14.3776591931245,
113.255243325012)) ;
#175752 = CARTESIAN_POINT('Ctrl Pts',(-27.7951209341155,-14.3105071713144,
113.221623805391)) ;
#175753 = CARTESIAN_POINT('Ctrl Pts',(-27.7213170961176,-14.3105071612984,
113.245854863592)) ;
#175754 = CARTESIAN_POINT('Ctrl Pts',(-27.6475132581198,-14.3105071512824,
113.270085921793)) ;
#175755 = CARTESIAN_POINT('Ctrl Pts',(-27.6585511111024,-14.3776591730925,
113.303705441414)) ;
#175756 = CARTESIAN_POINT('Ctrl Pts',(-27.669588964085,-14.4448111949025,
113.337324961035)) ;
#175757 = CARTESIAN_POINT('Ctrl Pts',(-27.7433928020829,-14.4448112049185,
113.313093902834)) ;
#175758 = CARTESIAN_POINT('Ctrl Pts',(-27.8171966400807,-14.4448112149345,
113.288862844633)) ;
#175759 = CARTESIAN_POINT('Ctrl Pts',(-27.8061587870981,-14.3776591931245,
113.255243325012)) ;
#175760 = CARTESIAN_POINT('Ctrl Pts',(-27.8693284879629,-14.2073582471136,
113.483114722588)) ;
#175761 = CARTESIAN_POINT('Ctrl Pts',(-27.8531291806685,-14.1519959883529,
113.433774246071)) ;
#175762 = CARTESIAN_POINT('Ctrl Pts',(-27.7793253400122,-14.1519959791231,
113.458005296175)) ;
#175763 = CARTESIAN_POINT('Ctrl Pts',(-27.705521499356,-14.1519959698933,
113.482236346279)) ;
#175764 = CARTESIAN_POINT('Ctrl Pts',(-27.7217208066503,-14.207358228654,
113.531576822795)) ;
#175765 = CARTESIAN_POINT('Ctrl Pts',(-27.7379201139447,-14.2627204874147,
113.580917299312)) ;
#175766 = CARTESIAN_POINT('Ctrl Pts',(-27.8117239546009,-14.2627204966445,
113.556686249208)) ;
#175767 = CARTESIAN_POINT('Ctrl Pts',(-27.8855277952572,-14.2627205058743,
113.532455199104)) ;
#175768 = CARTESIAN_POINT('Ctrl Pts',(-27.8693284879629,-14.2073582471136,
113.483114722588)) ;
#175769 = CARTESIAN_POINT('Ctrl Pts',(-27.9157562377959,-13.980463190757,
113.659992780597)) ;
#175770 = CARTESIAN_POINT('Ctrl Pts',(-27.8955566894573,-13.9408606598198,
113.598468215417)) ;
#175771 = CARTESIAN_POINT('Ctrl Pts',(-27.8217528469617,-13.9408606539983,
113.622699259918)) ;
#175772 = CARTESIAN_POINT('Ctrl Pts',(-27.7479490044661,-13.9408606481768,
113.64693030442)) ;
#175773 = CARTESIAN_POINT('Ctrl Pts',(-27.7681485528048,-13.9804631791139,
113.7084548696)) ;
#175774 = CARTESIAN_POINT('Ctrl Pts',(-27.7883481011434,-14.0200657100511,
113.76997943478)) ;
#175775 = CARTESIAN_POINT('Ctrl Pts',(-27.862151943639,-14.0200657158726,
113.745748390279)) ;
#175776 = CARTESIAN_POINT('Ctrl Pts',(-27.9359557861346,-14.0200657216941,
113.721517345777)) ;
#175777 = CARTESIAN_POINT('Ctrl Pts',(-27.9157562377959,-13.980463190757,
113.659992780597)) ;
#175778 = CARTESIAN_POINT('Ctrl Pts',(-27.9413702245525,-13.7134648384933,
113.773453223393)) ;
#175779 = CARTESIAN_POINT('Ctrl Pts',(-27.9186183026862,-13.6924464842837,
113.704154540366)) ;
#175780 = CARTESIAN_POINT('Ctrl Pts',(-27.8448144593015,-13.6924464826294,
113.728385582159)) ;
#175781 = CARTESIAN_POINT('Ctrl Pts',(-27.7710106159168,-13.6924464809751,
113.752616623953)) ;
#175782 = CARTESIAN_POINT('Ctrl Pts',(-27.7937625377831,-13.7134648351847,
113.82191530698)) ;
#175783 = CARTESIAN_POINT('Ctrl Pts',(-27.8165144596494,-13.7344831893942,
113.891213990007)) ;
#175784 = CARTESIAN_POINT('Ctrl Pts',(-27.8903183030341,-13.7344831910485,
113.866982948213)) ;
#175785 = CARTESIAN_POINT('Ctrl Pts',(-27.9641221464188,-13.7344831927028,
113.84275190642)) ;
#175786 = CARTESIAN_POINT('Ctrl Pts',(-27.9413702245525,-13.7134648384933,
113.773453223393)) ;
#175787 = CARTESIAN_POINT('Ctrl Pts',(-27.9436004920684,-13.4252028157263,
113.815706568897)) ;
#175788 = CARTESIAN_POINT('Ctrl Pts',(-27.9199249631736,-13.4242817506044,
113.74359472795)) ;
#175789 = CARTESIAN_POINT('Ctrl Pts',(-27.8461211196883,-13.4242817523867,
113.767825769437)) ;
#175790 = CARTESIAN_POINT('Ctrl Pts',(-27.7723172762029,-13.4242817541689,
113.792056810924)) ;
#175791 = CARTESIAN_POINT('Ctrl Pts',(-27.7959928050977,-13.4252028192908,
113.864168651871)) ;
#175792 = CARTESIAN_POINT('Ctrl Pts',(-27.8196683339925,-13.4261238844127,
113.936280492817)) ;
#175793 = CARTESIAN_POINT('Ctrl Pts',(-27.8934721774779,-13.4261238826305,
113.91204945133)) ;
#175794 = CARTESIAN_POINT('Ctrl Pts',(-27.9672760209632,-13.4261238808483,
113.887818409844)) ;
#175795 = CARTESIAN_POINT('Ctrl Pts',(-27.9436004920684,-13.4252028157263,
113.815706568897)) ;
#175796 = CARTESIAN_POINT('Ctrl Pts',(-27.9215804554763,-13.136660084581,
113.78406473884)) ;
#175797 = CARTESIAN_POINT('Ctrl Pts',(-27.8986741696855,-13.1558861878268,
113.714295888302)) ;
#175798 = CARTESIAN_POINT('Ctrl Pts',(-27.824870326538,-13.1558861911127,
113.738526930818)) ;
#175799 = CARTESIAN_POINT('Ctrl Pts',(-27.7510664833906,-13.1558861943986,
113.762757973334)) ;
#175800 = CARTESIAN_POINT('Ctrl Pts',(-27.7739727691814,-13.1366600911528,
113.832526823872)) ;
#175801 = CARTESIAN_POINT('Ctrl Pts',(-27.7968790549722,-13.117433987907,
113.90229567441)) ;
#175802 = CARTESIAN_POINT('Ctrl Pts',(-27.8706828981197,-13.1174339846211,
113.878064631894)) ;
#175803 = CARTESIAN_POINT('Ctrl Pts',(-27.9444867412671,-13.1174339813352,
113.853833589377)) ;
#175804 = CARTESIAN_POINT('Ctrl Pts',(-27.9215804554763,-13.136660084581,
113.78406473884)) ;
#175805 = CARTESIAN_POINT('Ctrl Pts',(-27.8759261543426,-12.8674128564449,
113.680553643697)) ;
#175806 = CARTESIAN_POINT('Ctrl Pts',(-27.8554383685418,-12.9054690960976,
113.61815115389)) ;
#175807 = CARTESIAN_POINT('Ctrl Pts',(-27.7816345255925,-12.9054690982831,
113.64238219701)) ;
#175808 = CARTESIAN_POINT('Ctrl Pts',(-27.7078306826432,-12.9054691004687,
113.666613240129)) ;
#175809 = CARTESIAN_POINT('Ctrl Pts',(-27.728318468444,-12.867412860816,113.729015729936)) ;
#175810 = CARTESIAN_POINT('Ctrl Pts',(-27.7488062542447,-12.8293566211633,
113.791418219742)) ;
#175811 = CARTESIAN_POINT('Ctrl Pts',(-27.8226100971941,-12.8293566189777,
113.767187176623)) ;
#175812 = CARTESIAN_POINT('Ctrl Pts',(-27.8964139401434,-12.8293566167922,
113.742956133503)) ;
#175813 = CARTESIAN_POINT('Ctrl Pts',(-27.8759261543426,-12.8674128564449,
113.680553643697)) ;
#175814 = CARTESIAN_POINT('Ctrl Pts',(-27.8094158631442,-12.6383938778605,
113.513414911382)) ;
#175815 = CARTESIAN_POINT('Ctrl Pts',(-27.7928087845804,-12.6924977231703,
113.462832429616)) ;
#175816 = CARTESIAN_POINT('Ctrl Pts',(-27.7190049412073,-12.6924977228183,
113.487063471445)) ;
#175817 = CARTESIAN_POINT('Ctrl Pts',(-27.6452010978342,-12.6924977224664,
113.511294513273)) ;
#175818 = CARTESIAN_POINT('Ctrl Pts',(-27.6618081763979,-12.6383938771567,
113.561876995039)) ;
#175819 = CARTESIAN_POINT('Ctrl Pts',(-27.6784152549617,-12.5842900318469,
113.612459476805)) ;
#175820 = CARTESIAN_POINT('Ctrl Pts',(-27.7522190983348,-12.5842900321988,
113.588228434977)) ;
#175821 = CARTESIAN_POINT('Ctrl Pts',(-27.8260229417079,-12.5842900325507,
113.563997393148)) ;
#175822 = CARTESIAN_POINT('Ctrl Pts',(-27.8094158631442,-12.6383938778605,
113.513414911382)) ;
#175823 = CARTESIAN_POINT('Ctrl Pts',(-27.7259260844217,-12.465038874388,
113.294584641188)) ;
#175824 = CARTESIAN_POINT('Ctrl Pts',(-27.7143905181872,-12.531326536537,
113.259449167606)) ;
#175825 = CARTESIAN_POINT('Ctrl Pts',(-27.6405866735841,-12.5313265339241,
113.283680205688)) ;
#175826 = CARTESIAN_POINT('Ctrl Pts',(-27.566782828981,-12.5313265313111,
113.30791124377)) ;
#175827 = CARTESIAN_POINT('Ctrl Pts',(-27.5783183952155,-12.4650388691621,
113.343046717353)) ;
#175828 = CARTESIAN_POINT('Ctrl Pts',(-27.5898539614499,-12.3987512070131,
113.378182190936)) ;
#175829 = CARTESIAN_POINT('Ctrl Pts',(-27.6636578060531,-12.3987512096261,
113.353951152854)) ;
#175830 = CARTESIAN_POINT('Ctrl Pts',(-27.7374616506562,-12.398751212239,
113.329720114771)) ;
#175831 = CARTESIAN_POINT('Ctrl Pts',(-27.7259260844217,-12.465038874388,
113.294584641188)) ;
#175832 = CARTESIAN_POINT('Ctrl Pts',(-27.630761291581,-12.3599344396702,
113.040172878809)) ;
#175833 = CARTESIAN_POINT('Ctrl Pts',(-27.6251202578705,-12.4336574817887,
113.022991200105)) ;
#175834 = CARTESIAN_POINT('Ctrl Pts',(-27.5513164113796,-12.4336574787988,
113.047222232437)) ;
#175835 = CARTESIAN_POINT('Ctrl Pts',(-27.4775125648887,-12.4336574758088,
113.07145326477)) ;
#175836 = CARTESIAN_POINT('Ctrl Pts',(-27.4831535985992,-12.3599344336902,
113.088634943473)) ;
#175837 = CARTESIAN_POINT('Ctrl Pts',(-27.4887946323096,-12.2862113915716,
113.105816622177)) ;
#175838 = CARTESIAN_POINT('Ctrl Pts',(-27.5625984788005,-12.2862113945616,
113.081585589845)) ;
#175839 = CARTESIAN_POINT('Ctrl Pts',(-27.6364023252914,-12.2862113975516,
113.057354557512)) ;
#175840 = CARTESIAN_POINT('Ctrl Pts',(-27.630761291581,-12.3599344396702,
113.040172878809)) ;
#175841 = CARTESIAN_POINT('Ctrl Pts',(-27.5296719419162,-12.3306429195518,
112.767809456319)) ;
#175842 = CARTESIAN_POINT('Ctrl Pts',(-27.5303457069297,-12.4065184959483,
112.769861635494)) ;
#175843 = CARTESIAN_POINT('Ctrl Pts',(-27.4565418579544,-12.4065184959014,
112.794092660259)) ;
#175844 = CARTESIAN_POINT('Ctrl Pts',(-27.3827380089791,-12.4065184958546,
112.818323685024)) ;
#175845 = CARTESIAN_POINT('Ctrl Pts',(-27.3820642439656,-12.330642919458,
112.81627150585)) ;
#175846 = CARTESIAN_POINT('Ctrl Pts',(-27.3813904789522,-12.2547673430615,
112.814219326675)) ;
#175847 = CARTESIAN_POINT('Ctrl Pts',(-27.4551943279275,-12.2547673431084,
112.78998830191)) ;
#175848 = CARTESIAN_POINT('Ctrl Pts',(-27.5289981769028,-12.2547673431553,
112.765757277145)) ;
#175849 = CARTESIAN_POINT('Ctrl Pts',(-27.5296719419162,-12.3306429195518,
112.767809456319)) ;
#175850 = CARTESIAN_POINT('Ctrl Pts',(-27.4298006531373,-12.3792038030185,
112.499012174243)) ;
#175851 = CARTESIAN_POINT('Ctrl Pts',(-27.4367161594043,-12.4517984874487,
112.520075690037)) ;
#175852 = CARTESIAN_POINT('Ctrl Pts',(-27.3629123084857,-12.4517984942269,
112.544306708883)) ;
#175853 = CARTESIAN_POINT('Ctrl Pts',(-27.2891084575671,-12.4517985010052,
112.568537727729)) ;
#175854 = CARTESIAN_POINT('Ctrl Pts',(-27.2821929513001,-12.379203816575,
112.547474211936)) ;
#175855 = CARTESIAN_POINT('Ctrl Pts',(-27.275277445033,-12.3066091321447,
112.526410696142)) ;
#175856 = CARTESIAN_POINT('Ctrl Pts',(-27.3490812959516,-12.3066091253665,
112.502179677296)) ;
#175857 = CARTESIAN_POINT('Ctrl Pts',(-27.4228851468702,-12.3066091185883,
112.47794865845)) ;
#175858 = CARTESIAN_POINT('Ctrl Pts',(-27.4298006531373,-12.3792038030185,
112.499012174243)) ;
#175859 = CARTESIAN_POINT('Ctrl Pts',(-27.3368869719151,-12.502250920438,
112.251503904024)) ;
#175860 = CARTESIAN_POINT('Ctrl Pts',(-27.3495653984223,-12.5663594268052,
112.29012034486)) ;
#175861 = CARTESIAN_POINT('Ctrl Pts',(-27.2757615460824,-12.5663594442773,
112.314351359377)) ;
#175862 = CARTESIAN_POINT('Ctrl Pts',(-27.2019576937426,-12.5663594617495,
112.338582373895)) ;
#175863 = CARTESIAN_POINT('Ctrl Pts',(-27.1892792672354,-12.5022509553824,
112.299965933058)) ;
#175864 = CARTESIAN_POINT('Ctrl Pts',(-27.1766008407283,-12.4381424490152,
112.261349492222)) ;
#175865 = CARTESIAN_POINT('Ctrl Pts',(-27.2504046930681,-12.4381424315431,
112.237118477705)) ;
#175866 = CARTESIAN_POINT('Ctrl Pts',(-27.324208545408,-12.4381424140709,
112.212887463188)) ;
#175867 = CARTESIAN_POINT('Ctrl Pts',(-27.3368869719151,-12.502250920438,
112.251503904024)) ;
#175868 = CARTESIAN_POINT('Ctrl Pts',(-27.2572469138254,-12.690704289041,
112.044366413114)) ;
#175869 = CARTESIAN_POINT('Ctrl Pts',(-27.2747709167392,-12.7417475393675,
112.097741697693)) ;
#175870 = CARTESIAN_POINT('Ctrl Pts',(-27.2009670644347,-12.7417475700136,
112.121972712318)) ;
#175871 = CARTESIAN_POINT('Ctrl Pts',(-27.1271632121303,-12.7417476006596,
112.146203726943)) ;
#175872 = CARTESIAN_POINT('Ctrl Pts',(-27.1096392092165,-12.6907043503331,
112.092828442364)) ;
#175873 = CARTESIAN_POINT('Ctrl Pts',(-27.0921152063027,-12.6396611000066,
112.039453157785)) ;
#175874 = CARTESIAN_POINT('Ctrl Pts',(-27.1659190586071,-12.6396610693606,
112.01522214316)) ;
#175875 = CARTESIAN_POINT('Ctrl Pts',(-27.2397229109116,-12.6396610387145,
111.990991128535)) ;
#175876 = CARTESIAN_POINT('Ctrl Pts',(-27.2572469138254,-12.690704289041,
112.044366413114)) ;
#175877 = CARTESIAN_POINT('Ctrl Pts',(-27.1956046752294,-12.9312491813812,
111.892066772438)) ;
#175878 = CARTESIAN_POINT('Ctrl Pts',(-27.2167242051917,-12.9655714979513,
111.956393452104)) ;
#175879 = CARTESIAN_POINT('Ctrl Pts',(-27.1429203545228,-12.9655715427417,
111.980624471711)) ;
#175880 = CARTESIAN_POINT('Ctrl Pts',(-27.0691165038539,-12.9655715875322,
112.004855491318)) ;
#175881 = CARTESIAN_POINT('Ctrl Pts',(-27.0479969738915,-12.9312492709622,
111.940528811651)) ;
#175882 = CARTESIAN_POINT('Ctrl Pts',(-27.0268774439292,-12.8969269543922,
111.876202131985)) ;
#175883 = CARTESIAN_POINT('Ctrl Pts',(-27.1006812945981,-12.8969269096017,
111.851971112378)) ;
#175884 = CARTESIAN_POINT('Ctrl Pts',(-27.174485145267,-12.8969268648112,
111.827740092771)) ;
#175885 = CARTESIAN_POINT('Ctrl Pts',(-27.1956046752294,-12.9312491813812,
111.892066772438)) ;
#175886 = CARTESIAN_POINT('Ctrl Pts',(-27.1556968251946,-13.2069304836541,
111.805999837402)) ;
#175887 = CARTESIAN_POINT('Ctrl Pts',(-27.1788989285037,-13.2220547357584,
111.87666969929)) ;
#175888 = CARTESIAN_POINT('Ctrl Pts',(-27.1050950812972,-13.2220547937704,
111.900900729442)) ;
#175889 = CARTESIAN_POINT('Ctrl Pts',(-27.0312912340907,-13.2220548517825,
111.925131759595)) ;
#175890 = CARTESIAN_POINT('Ctrl Pts',(-27.0080891307815,-13.2069305996783,
111.854461897707)) ;
#175891 = CARTESIAN_POINT('Ctrl Pts',(-26.9848870274724,-13.191806347574,
111.783792035819)) ;
#175892 = CARTESIAN_POINT('Ctrl Pts',(-27.0586908746789,-13.191806289562,
111.759561005666)) ;
#175893 = CARTESIAN_POINT('Ctrl Pts',(-27.1324947218855,-13.1918062315499,
111.735329975513)) ;
#175894 = CARTESIAN_POINT('Ctrl Pts',(-27.1556968251946,-13.2069304836541,
111.805999837402)) ;
#175895 = CARTESIAN_POINT('Ctrl Pts',(-27.1396183503164,-13.4971323588194,
111.792434998313)) ;
#175896 = CARTESIAN_POINT('Ctrl Pts',(-27.163243869223,-13.4920171795336,
111.864394515641)) ;
#175897 = CARTESIAN_POINT('Ctrl Pts',(-27.0894400270983,-13.4920172465716,
111.888625561272)) ;
#175898 = CARTESIAN_POINT('Ctrl Pts',(-27.0156361849736,-13.4920173136096,
111.912856606903)) ;
#175899 = CARTESIAN_POINT('Ctrl Pts',(-26.992010666067,-13.4971324928954,
111.840897089575)) ;
#175900 = CARTESIAN_POINT('Ctrl Pts',(-26.9683851471604,-13.5022476721812,
111.768937572246)) ;
#175901 = CARTESIAN_POINT('Ctrl Pts',(-27.0421889892851,-13.5022476051432,
111.744706526615)) ;
#175902 = CARTESIAN_POINT('Ctrl Pts',(-27.1159928314098,-13.5022475381053,
111.720475480984)) ;
#175903 = CARTESIAN_POINT('Ctrl Pts',(-27.1396183503164,-13.4971323588194,
111.792434998313)) ;
#175904 = CARTESIAN_POINT('Ctrl Pts',(-27.1478926952953,-13.7832858649534,
111.853261517309)) ;
#175905 = CARTESIAN_POINT('Ctrl Pts',(-27.1702377683041,-13.7581847544607,
111.921321002853)) ;
#175906 = CARTESIAN_POINT('Ctrl Pts',(-27.0964339327126,-13.7581848266256,
111.945552068383)) ;
#175907 = CARTESIAN_POINT('Ctrl Pts',(-27.0226300971212,-13.7581848987905,
111.969783133914)) ;
#175908 = CARTESIAN_POINT('Ctrl Pts',(-27.0002850241124,-13.7832860092831,
111.90172364837)) ;
#175909 = CARTESIAN_POINT('Ctrl Pts',(-26.9779399511036,-13.8083871197758,
111.833664162826)) ;
#175910 = CARTESIAN_POINT('Ctrl Pts',(-27.0517437866951,-13.808387047611,
111.809433097296)) ;
#175911 = CARTESIAN_POINT('Ctrl Pts',(-27.1255476222865,-13.8083869754461,
111.785202031766)) ;
#175912 = CARTESIAN_POINT('Ctrl Pts',(-27.1478926952953,-13.7832858649534,
111.853261517309)) ;
#175913 = CARTESIAN_POINT('Ctrl Pts',(-27.1788426100833,-14.0408293277911,
111.98281261947)) ;
#175914 = CARTESIAN_POINT('Ctrl Pts',(-27.1983290352884,-13.9977110227071,
112.042165124933)) ;
#175915 = CARTESIAN_POINT('Ctrl Pts',(-27.1245252064214,-13.997711090453,
112.066396210945)) ;
#175916 = CARTESIAN_POINT('Ctrl Pts',(-27.0507213775545,-13.9977111581989,
112.090627296957)) ;
#175917 = CARTESIAN_POINT('Ctrl Pts',(-27.0312349523494,-14.0408294632829,
112.031274791494)) ;
#175918 = CARTESIAN_POINT('Ctrl Pts',(-27.0117485271443,-14.0839477683669,
111.971922286031)) ;
#175919 = CARTESIAN_POINT('Ctrl Pts',(-27.0855523560112,-14.083947700621,
111.947691200019)) ;
#175920 = CARTESIAN_POINT('Ctrl Pts',(-27.1593561848781,-14.0839476328751,
111.923460114007)) ;
#175921 = CARTESIAN_POINT('Ctrl Pts',(-27.1788426100833,-14.0408293277911,
111.98281261947)) ;
#175922 = CARTESIAN_POINT('Ctrl Pts',(-27.2300778195774,-14.255952322556,
112.174490901595)) ;
#175923 = CARTESIAN_POINT('Ctrl Pts',(-27.2452785325984,-14.1977519640159,
112.220789819091)) ;
#175924 = CARTESIAN_POINT('Ctrl Pts',(-27.1714747106939,-14.1977520218044,
112.24502092631)) ;
#175925 = CARTESIAN_POINT('Ctrl Pts',(-27.0976708887894,-14.1977520795929,
112.269252033528)) ;
#175926 = CARTESIAN_POINT('Ctrl Pts',(-27.0824701757685,-14.2559524381331,
112.222953116032)) ;
#175927 = CARTESIAN_POINT('Ctrl Pts',(-27.0672694627476,-14.3141527966732,
112.176654198535)) ;
#175928 = CARTESIAN_POINT('Ctrl Pts',(-27.141073284652,-14.3141527388846,
112.152423091316)) ;
#175929 = CARTESIAN_POINT('Ctrl Pts',(-27.2148771065565,-14.3141526810961,
112.128191984098)) ;
#175930 = CARTESIAN_POINT('Ctrl Pts',(-27.2300778195774,-14.255952322556,
112.174490901595)) ;
#175931 = CARTESIAN_POINT('Ctrl Pts',(-27.2963594840731,-14.4094466686143,
112.411688111103)) ;
#175932 = CARTESIAN_POINT('Ctrl Pts',(-27.3062239782014,-14.3404453655438,
112.441733766757)) ;
#175933 = CARTESIAN_POINT('Ctrl Pts',(-27.2324201616656,-14.3404454048825,
112.465964890328)) ;
#175934 = CARTESIAN_POINT('Ctrl Pts',(-27.1586163451298,-14.3404454442213,
112.490196013899)) ;
#175935 = CARTESIAN_POINT('Ctrl Pts',(-27.1487518510015,-14.4094467472918,
112.460150358244)) ;
#175936 = CARTESIAN_POINT('Ctrl Pts',(-27.1388873568732,-14.4784480503623,
112.43010470259)) ;
#175937 = CARTESIAN_POINT('Ctrl Pts',(-27.212691173409,-14.4784480110235,
112.405873579019)) ;
#175938 = CARTESIAN_POINT('Ctrl Pts',(-27.2864949899448,-14.4784479716848,
112.381642455449)) ;
#175939 = CARTESIAN_POINT('Ctrl Pts',(-27.2963594840731,-14.4094466686143,
112.411688111103)) ;
#175940 = CARTESIAN_POINT('Ctrl Pts',(-27.3730829374615,-14.4929694646286,
112.680938243989)) ;
#175941 = CARTESIAN_POINT('Ctrl Pts',(-27.3768695303142,-14.4180358803258,
112.692471592919)) ;
#175942 = CARTESIAN_POINT('Ctrl Pts',(-27.3030657177336,-14.4180358961808,
112.716702728537)) ;
#175943 = CARTESIAN_POINT('Ctrl Pts',(-27.2292619051531,-14.4180359120358,
112.740933864154)) ;
#175944 = CARTESIAN_POINT('Ctrl Pts',(-27.2254753123004,-14.4929694963386,
112.729400515224)) ;
#175945 = CARTESIAN_POINT('Ctrl Pts',(-27.2216887194477,-14.5679030806414,
112.717867166294)) ;
#175946 = CARTESIAN_POINT('Ctrl Pts',(-27.2954925320283,-14.5679030647864,
112.693636030676)) ;
#175947 = CARTESIAN_POINT('Ctrl Pts',(-27.3692963446088,-14.5679030489314,
112.669404895059)) ;
#175948 = CARTESIAN_POINT('Ctrl Pts',(-27.3730829374615,-14.4929694646286,
112.680938243989)) ;
#175949 = CARTESIAN_POINT('Ctrl Pts',(-27.4533942328739,-14.4990155260453,
112.961017342185)) ;
#175950 = CARTESIAN_POINT('Ctrl Pts',(-27.4508455544286,-14.4235500005798,
112.953254476862)) ;
#175951 = CARTESIAN_POINT('Ctrl Pts',(-27.3770417432059,-14.4235499890681,
112.977485616615)) ;
#175952 = CARTESIAN_POINT('Ctrl Pts',(-27.3032379319832,-14.4235499775565,
113.001716756368)) ;
#175953 = CARTESIAN_POINT('Ctrl Pts',(-27.3057866104284,-14.499015503022,
113.009479621691)) ;
#175954 = CARTESIAN_POINT('Ctrl Pts',(-27.3083352888737,-14.5744810284875,
113.017242487014)) ;
#175955 = CARTESIAN_POINT('Ctrl Pts',(-27.3821391000964,-14.5744810399991,
112.993011347261)) ;
#175956 = CARTESIAN_POINT('Ctrl Pts',(-27.4559429113192,-14.5744810515108,
112.968780207508)) ;
#175957 = CARTESIAN_POINT('Ctrl Pts',(-27.4533942328739,-14.4990155260453,
112.961017342185)) ;
#175958 = CARTESIAN_POINT('Ctrl Pts',(-27.5309746225123,-14.4275804860338,
113.232800584045)) ;
#175959 = CARTESIAN_POINT('Ctrl Pts',(-27.5222715844995,-14.3569912762542,
113.20629253243)) ;
#175960 = CARTESIAN_POINT('Ctrl Pts',(-27.4484677719345,-14.3569912367052,
113.230523668094)) ;
#175961 = CARTESIAN_POINT('Ctrl Pts',(-27.3746639593695,-14.3569911971563,
113.254754803759)) ;
#175962 = CARTESIAN_POINT('Ctrl Pts',(-27.3833669973824,-14.4275804069359,
113.281262855375)) ;
#175963 = CARTESIAN_POINT('Ctrl Pts',(-27.3920700353952,-14.4981696167155,
113.30777090699)) ;
#175964 = CARTESIAN_POINT('Ctrl Pts',(-27.4658738479602,-14.4981696562644,
113.283539771325)) ;
#175965 = CARTESIAN_POINT('Ctrl Pts',(-27.5396776605252,-14.4981696958134,
113.25930863566)) ;
#175966 = CARTESIAN_POINT('Ctrl Pts',(-27.5309746225123,-14.4275804860338,
113.232800584045)) ;
#175967 = CARTESIAN_POINT('Ctrl Pts',(-27.5993744489561,-14.284309082368,
113.476532018314)) ;
#175968 = CARTESIAN_POINT('Ctrl Pts',(-27.5851507849207,-14.223618657059,
113.433209030554)) ;
#175969 = CARTESIAN_POINT('Ctrl Pts',(-27.5113469683492,-14.2236185917218,
113.457440154016)) ;
#175970 = CARTESIAN_POINT('Ctrl Pts',(-27.4375431517776,-14.2236185263845,
113.481671277477)) ;
#175971 = CARTESIAN_POINT('Ctrl Pts',(-27.4517668158129,-14.2843089516935,
113.524994265237)) ;
#175972 = CARTESIAN_POINT('Ctrl Pts',(-27.4659904798483,-14.3449993770025,
113.568317252997)) ;
#175973 = CARTESIAN_POINT('Ctrl Pts',(-27.5397942964199,-14.3449994423398,
113.544086129535)) ;
#175974 = CARTESIAN_POINT('Ctrl Pts',(-27.6135981129914,-14.3449995076771,
113.519855006074)) ;
#175975 = CARTESIAN_POINT('Ctrl Pts',(-27.5993744489561,-14.284309082368,
113.476532018314)) ;
#175976 = CARTESIAN_POINT('Ctrl Pts',(-27.6533609863589,-14.0775350374868,
113.67660042095)) ;
#175977 = CARTESIAN_POINT('Ctrl Pts',(-27.634609746819,-14.0311904705444,
113.619487168718)) ;
#175978 = CARTESIAN_POINT('Ctrl Pts',(-27.5608059238945,-14.0311903843125,
113.643718272829)) ;
#175979 = CARTESIAN_POINT('Ctrl Pts',(-27.4870021009699,-14.0311902980806,
113.66794937694)) ;
#175980 = CARTESIAN_POINT('Ctrl Pts',(-27.5057533405098,-14.0775348650229,
113.725062629172)) ;
#175981 = CARTESIAN_POINT('Ctrl Pts',(-27.5245045800497,-14.1238794319653,
113.782175881404)) ;
#175982 = CARTESIAN_POINT('Ctrl Pts',(-27.5983084029742,-14.1238795181972,
113.757944777293)) ;
#175983 = CARTESIAN_POINT('Ctrl Pts',(-27.6721122258988,-14.1238796044292,
113.733713673182)) ;
#175984 = CARTESIAN_POINT('Ctrl Pts',(-27.6533609863589,-14.0775350374868,
113.67660042095)) ;
#175985 = CARTESIAN_POINT('Ctrl Pts',(-27.6875986228682,-13.8261134335288,
113.816121058213)) ;
#175986 = CARTESIAN_POINT('Ctrl Pts',(-27.665700207824,-13.7972540806325,
113.749422017201)) ;
#175987 = CARTESIAN_POINT('Ctrl Pts',(-27.5918963769847,-13.7972539806286,
113.773653097205)) ;
#175988 = CARTESIAN_POINT('Ctrl Pts',(-27.5180925461453,-13.7972538806247,
113.797884177209)) ;
#175989 = CARTESIAN_POINT('Ctrl Pts',(-27.5399909611896,-13.826113233521,
113.864583218222)) ;
#175990 = CARTESIAN_POINT('Ctrl Pts',(-27.5618893762338,-13.8549725864173,
113.931282259234)) ;
#175991 = CARTESIAN_POINT('Ctrl Pts',(-27.6356932070732,-13.8549726864212,
113.90705117923)) ;
#175992 = CARTESIAN_POINT('Ctrl Pts',(-27.7094970379125,-13.8549727864252,
113.882820099226)) ;
#175993 = CARTESIAN_POINT('Ctrl Pts',(-27.6875986228682,-13.8261134335288,
113.816121058213)) ;
#175994 = CARTESIAN_POINT('Ctrl Pts',(-27.6996267717849,-13.5428648342343,
113.888368399397)) ;
#175995 = CARTESIAN_POINT('Ctrl Pts',(-27.676119024517,-13.5337376171051,
113.816767592136)) ;
#175996 = CARTESIAN_POINT('Ctrl Pts',(-27.6023151848084,-13.5337375120109,
113.840998645126)) ;
#175997 = CARTESIAN_POINT('Ctrl Pts',(-27.5285113450998,-13.5337374069167,
113.865229698116)) ;
#175998 = CARTESIAN_POINT('Ctrl Pts',(-27.5520190923677,-13.5428646240459,
113.936830505377)) ;
#175999 = CARTESIAN_POINT('Ctrl Pts',(-27.5755268396356,-13.551991841175,
114.008431312637)) ;
#176000 = CARTESIAN_POINT('Ctrl Pts',(-27.6493306793442,-13.5519919462692,
113.984200259648)) ;
#176001 = CARTESIAN_POINT('Ctrl Pts',(-27.7231345190528,-13.5519920513634,
113.959969206658)) ;
#176002 = CARTESIAN_POINT('Ctrl Pts',(-27.6996267717849,-13.5428648342343,
113.888368399397)) ;
#176003 = CARTESIAN_POINT('Ctrl Pts',(-27.6873576347831,-13.252182353688,
113.886407116913)) ;
#176004 = CARTESIAN_POINT('Ctrl Pts',(-27.6639387565465,-13.263336213575,
113.815076990438)) ;
#176005 = CARTESIAN_POINT('Ctrl Pts',(-27.5901349081512,-13.2633361119795,
113.83930801697)) ;
#176006 = CARTESIAN_POINT('Ctrl Pts',(-27.5163310597558,-13.2633360103841,
113.863539043501)) ;
#176007 = CARTESIAN_POINT('Ctrl Pts',(-27.5397499379924,-13.2521821504971,
113.934869169976)) ;
#176008 = CARTESIAN_POINT('Ctrl Pts',(-27.563168816229,-13.2410282906101,
114.00619929645)) ;
#176009 = CARTESIAN_POINT('Ctrl Pts',(-27.6369726646243,-13.2410283922056,
113.981968269918)) ;
#176010 = CARTESIAN_POINT('Ctrl Pts',(-27.7107765130197,-13.241028493801,
113.957737243387)) ;
#176011 = CARTESIAN_POINT('Ctrl Pts',(-27.6873576347831,-13.252182353688,
113.886407116913)) ;
#176012 = CARTESIAN_POINT('Ctrl Pts',(-27.651195526548,-12.9730234465435,
113.811707238471)) ;
#176013 = CARTESIAN_POINT('Ctrl Pts',(-27.6295329359788,-13.0036840588297,
113.745726480929)) ;
#176014 = CARTESIAN_POINT('Ctrl Pts',(-27.5557290797921,-13.0036839686776,
113.769957483729)) ;
#176015 = CARTESIAN_POINT('Ctrl Pts',(-27.4819252236053,-13.0036838785254,
113.794188486529)) ;
#176016 = CARTESIAN_POINT('Ctrl Pts',(-27.5035878141745,-12.9730232662392,
113.860169244071)) ;
#176017 = CARTESIAN_POINT('Ctrl Pts',(-27.5252504047438,-12.9423626539529,
113.926150001612)) ;
#176018 = CARTESIAN_POINT('Ctrl Pts',(-27.5990542609305,-12.942362744105,
113.901918998812)) ;
#176019 = CARTESIAN_POINT('Ctrl Pts',(-27.6728581171173,-12.9423628342572,
113.877687996012)) ;
#176020 = CARTESIAN_POINT('Ctrl Pts',(-27.651195526548,-12.9730234465435,
113.811707238471)) ;
#176021 = CARTESIAN_POINT('Ctrl Pts',(-27.5924502457676,-12.724731390434,
113.668397807756)) ;
#176022 = CARTESIAN_POINT('Ctrl Pts',(-27.5741193939568,-12.77277340565,113.612564989016)) ;
#176023 = CARTESIAN_POINT('Ctrl Pts',(-27.5003155319448,-12.7727733343003,
113.636795974073)) ;
#176024 = CARTESIAN_POINT('Ctrl Pts',(-27.4265116699327,-12.7727732629506,
113.66102695913)) ;
#176025 = CARTESIAN_POINT('Ctrl Pts',(-27.4448425217436,-12.7247312477346,
113.716859777871)) ;
#176026 = CARTESIAN_POINT('Ctrl Pts',(-27.4631733735544,-12.6766892325185,
113.772692596611)) ;
#176027 = CARTESIAN_POINT('Ctrl Pts',(-27.5369772355664,-12.6766893038683,
113.748461611554)) ;
#176028 = CARTESIAN_POINT('Ctrl Pts',(-27.6107810975784,-12.676689375218,
113.724230626497)) ;
#176029 = CARTESIAN_POINT('Ctrl Pts',(-27.5924502457676,-12.724731390434,
113.668397807756)) ;
#176030 = CARTESIAN_POINT('Ctrl Pts',(-27.5156633000477,-12.5280561031159,
113.469790960335)) ;
#176031 = CARTESIAN_POINT('Ctrl Pts',(-27.5019362584244,-12.5899016984486,
113.427980604694)) ;
#176032 = CARTESIAN_POINT('Ctrl Pts',(-27.4281323923887,-12.5899016481567,
113.452211577496)) ;
#176033 = CARTESIAN_POINT('Ctrl Pts',(-27.354328526353,-12.5899015978648,
113.476442550298)) ;
#176034 = CARTESIAN_POINT('Ctrl Pts',(-27.3680555679764,-12.5280560025322,
113.518252905939)) ;
#176035 = CARTESIAN_POINT('Ctrl Pts',(-27.3817826095997,-12.4662104071995,
113.560063261581)) ;
#176036 = CARTESIAN_POINT('Ctrl Pts',(-27.4555864756354,-12.4662104574914,
113.535832288779)) ;
#176037 = CARTESIAN_POINT('Ctrl Pts',(-27.5293903416711,-12.4662105077833,
113.511601315976)) ;
#176038 = CARTESIAN_POINT('Ctrl Pts',(-27.5156633000477,-12.5280561031159,
113.469790960335)) ;
#176039 = CARTESIAN_POINT('Ctrl Pts',(-27.4242158235811,-12.3935893009494,
113.226845172422)) ;
#176040 = CARTESIAN_POINT('Ctrl Pts',(-27.4161163215766,-12.4649167907205,
113.202175394608)) ;
#176041 = CARTESIAN_POINT('Ctrl Pts',(-27.3423124544162,-12.464916764178,
113.226406363984)) ;
#176042 = CARTESIAN_POINT('Ctrl Pts',(-27.2685085872558,-12.4649167376354,
113.250637333361)) ;
#176043 = CARTESIAN_POINT('Ctrl Pts',(-27.2766080892603,-12.3935892478642,
113.275307111174)) ;
#176044 = CARTESIAN_POINT('Ctrl Pts',(-27.2847075912648,-12.322261758093,
113.299976888988)) ;
#176045 = CARTESIAN_POINT('Ctrl Pts',(-27.3585114584252,-12.3222617846356,
113.275745919611)) ;
#176046 = CARTESIAN_POINT('Ctrl Pts',(-27.4323153255855,-12.3222618111782,
113.251514950235)) ;
#176047 = CARTESIAN_POINT('Ctrl Pts',(-27.4242158235811,-12.3935893009494,
113.226845172422)) ;
#176048 = CARTESIAN_POINT('Ctrl Pts',(-27.3251142958241,-12.333081965445,
112.960365809793)) ;
#176049 = CARTESIAN_POINT('Ctrl Pts',(-27.3231899346653,-12.4087416290775,
112.954504514769)) ;
#176050 = CARTESIAN_POINT('Ctrl Pts',(-27.2493860682454,-12.4087416242859,
112.9787354864)) ;
#176051 = CARTESIAN_POINT('Ctrl Pts',(-27.1755822018255,-12.4087416194943,
113.002966458032)) ;
#176052 = CARTESIAN_POINT('Ctrl Pts',(-27.1775065629843,-12.3330819558618,
113.008827753056)) ;
#176053 = CARTESIAN_POINT('Ctrl Pts',(-27.179430924143,-12.2574222922293,
113.01468904808)) ;
#176054 = CARTESIAN_POINT('Ctrl Pts',(-27.2532347905629,-12.2574222970209,
112.990458076449)) ;
#176055 = CARTESIAN_POINT('Ctrl Pts',(-27.3270386569828,-12.2574223018125,
112.966227104817)) ;
#176056 = CARTESIAN_POINT('Ctrl Pts',(-27.3251142958241,-12.333081965445,
112.960365809793)) ;
#176057 = CARTESIAN_POINT('Ctrl Pts',(-27.2233916702717,-12.3505128306963,
112.686197908057)) ;
#176058 = CARTESIAN_POINT('Ctrl Pts',(-27.2278287044319,-12.4250706656238,
112.699712396958)) ;
#176059 = CARTESIAN_POINT('Ctrl Pts',(-27.1540248414432,-12.4250706786686,
112.723943379041)) ;
#176060 = CARTESIAN_POINT('Ctrl Pts',(-27.0802209784545,-12.4250706917134,
112.748174361124)) ;
#176061 = CARTESIAN_POINT('Ctrl Pts',(-27.0757839442942,-12.3505128567859,
112.734659872223)) ;
#176062 = CARTESIAN_POINT('Ctrl Pts',(-27.0713469101339,-12.2759550218584,
112.721145383321)) ;
#176063 = CARTESIAN_POINT('Ctrl Pts',(-27.1451507731226,-12.2759550088136,
112.696914401239)) ;
#176064 = CARTESIAN_POINT('Ctrl Pts',(-27.2189546361114,-12.2759549957688,
112.672683419156)) ;
#176065 = CARTESIAN_POINT('Ctrl Pts',(-27.2233916702717,-12.3505128306963,
112.686197908057)) ;
#176066 = CARTESIAN_POINT('Ctrl Pts',(-27.12763956026,-12.4433828921911,112.429728050708)) ;
#176067 = CARTESIAN_POINT('Ctrl Pts',(-27.1380408629042,-12.5115686405398,
112.46140873919)) ;
#176068 = CARTESIAN_POINT('Ctrl Pts',(-27.0642370032903,-12.5115686671103,
112.485639731552)) ;
#176069 = CARTESIAN_POINT('Ctrl Pts',(-26.9904331436763,-12.5115686936807,
112.509870723913)) ;
#176070 = CARTESIAN_POINT('Ctrl Pts',(-26.980031841032,-12.443382945332,112.478190035431)) ;
#176071 = CARTESIAN_POINT('Ctrl Pts',(-26.9696305383877,-12.3751971969833,
112.446509346949)) ;
#176072 = CARTESIAN_POINT('Ctrl Pts',(-27.0434343980017,-12.3751971704129,
112.422278354588)) ;
#176073 = CARTESIAN_POINT('Ctrl Pts',(-27.1172382576157,-12.3751971438424,
112.398047362226)) ;
#176074 = CARTESIAN_POINT('Ctrl Pts',(-27.12763956026,-12.4433828921911,112.429728050708)) ;
#176075 = CARTESIAN_POINT('Ctrl Pts',(-27.0415094033996,-12.607349424796,
112.20302769542)) ;
#176076 = CARTESIAN_POINT('Ctrl Pts',(-27.0572028168899,-12.6641907157574,
112.25082729986)) ;
#176077 = CARTESIAN_POINT('Ctrl Pts',(-26.9833989624742,-12.6641907484467,
112.275058308054)) ;
#176078 = CARTESIAN_POINT('Ctrl Pts',(-26.9095951080584,-12.664190781136,
112.299289316249)) ;
#176079 = CARTESIAN_POINT('Ctrl Pts',(-26.8939016945682,-12.6073494901747,
112.251489711809)) ;
#176080 = CARTESIAN_POINT('Ctrl Pts',(-26.8782082810779,-12.5505081992133,
112.203690107369)) ;
#176081 = CARTESIAN_POINT('Ctrl Pts',(-26.9520121354936,-12.5505081665239,
112.179459099174)) ;
#176082 = CARTESIAN_POINT('Ctrl Pts',(-27.0258159899093,-12.5505081338346,
112.15522809098)) ;
#176083 = CARTESIAN_POINT('Ctrl Pts',(-27.0415094033996,-12.607349424796,
112.20302769542)) ;
#176084 = CARTESIAN_POINT('Ctrl Pts',(-26.9722746864344,-12.8279036385121,
112.027468698458)) ;
#176085 = CARTESIAN_POINT('Ctrl Pts',(-26.9920950650029,-12.8694313461383,
112.087838372784)) ;
#176086 = CARTESIAN_POINT('Ctrl Pts',(-26.9182912149163,-12.8694313807778,
112.112069394164)) ;
#176087 = CARTESIAN_POINT('Ctrl Pts',(-26.8444873648296,-12.8694314154173,
112.136300415545)) ;
#176088 = CARTESIAN_POINT('Ctrl Pts',(-26.8246669862611,-12.8279037077911,
112.075930741219)) ;
#176089 = CARTESIAN_POINT('Ctrl Pts',(-26.8048466076927,-12.7863760001649,
112.015561066893)) ;
#176090 = CARTESIAN_POINT('Ctrl Pts',(-26.8786504577793,-12.7863759655254,
111.991330045513)) ;
#176091 = CARTESIAN_POINT('Ctrl Pts',(-26.9524543078659,-12.7863759308859,
111.967099024132)) ;
#176092 = CARTESIAN_POINT('Ctrl Pts',(-26.9722746864344,-12.8279036385121,
112.027468698458)) ;
#176093 = CARTESIAN_POINT('Ctrl Pts',(-26.9229312024064,-13.0930059035689,
111.912843276643)) ;
#176094 = CARTESIAN_POINT('Ctrl Pts',(-26.9454890591512,-13.1160865947577,
111.981550868007)) ;
#176095 = CARTESIAN_POINT('Ctrl Pts',(-26.8716852131677,-13.1160866238806,
112.005781901885)) ;
#176096 = CARTESIAN_POINT('Ctrl Pts',(-26.7978813671843,-13.1160866530036,
112.030012935763)) ;
#176097 = CARTESIAN_POINT('Ctrl Pts',(-26.7753235104395,-13.0930059618148,
111.961305344399)) ;
#176098 = CARTESIAN_POINT('Ctrl Pts',(-26.7527656536947,-13.069925270626,
111.892597753036)) ;
#176099 = CARTESIAN_POINT('Ctrl Pts',(-26.8265694996782,-13.069925241503,
111.868366719158)) ;
#176100 = CARTESIAN_POINT('Ctrl Pts',(-26.9003733456616,-13.0699252123801,
111.84413568528)) ;
#176101 = CARTESIAN_POINT('Ctrl Pts',(-26.9229312024064,-13.0930059035689,
111.912843276643)) ;
#176102 = CARTESIAN_POINT('Ctrl Pts',(-26.8972324155193,-13.3789266137586,
111.86989142793)) ;
#176103 = CARTESIAN_POINT('Ctrl Pts',(-26.9208877456924,-13.3820781397035,
111.941941746411)) ;
#176104 = CARTESIAN_POINT('Ctrl Pts',(-26.8470839022087,-13.3820781631016,
111.966172787903)) ;
#176105 = CARTESIAN_POINT('Ctrl Pts',(-26.7732800587249,-13.3820781864996,
111.990403829394)) ;
#176106 = CARTESIAN_POINT('Ctrl Pts',(-26.7496247285517,-13.3789266605547,
111.918353510913)) ;
#176107 = CARTESIAN_POINT('Ctrl Pts',(-26.7259693983785,-13.3757751346097,
111.846303192431)) ;
#176108 = CARTESIAN_POINT('Ctrl Pts',(-26.7997732418623,-13.3757751112117,
111.82207215094)) ;
#176109 = CARTESIAN_POINT('Ctrl Pts',(-26.8735770853461,-13.3757750878137,
111.797841109448)) ;
#176110 = CARTESIAN_POINT('Ctrl Pts',(-26.8972324155193,-13.3789266137586,
111.86989142793)) ;
#176111 = CARTESIAN_POINT('Ctrl Pts',(-26.89559593885,-13.6686885717782,111.900373113643)) ;
#176112 = CARTESIAN_POINT('Ctrl Pts',(-26.9186673845928,-13.6516124113894,
111.970645014506)) ;
#176113 = CARTESIAN_POINT('Ctrl Pts',(-26.8448635425279,-13.6516124266104,
111.99487606032)) ;
#176114 = CARTESIAN_POINT('Ctrl Pts',(-26.771059700463,-13.6516124418314,
112.019107106133)) ;
#176115 = CARTESIAN_POINT('Ctrl Pts',(-26.7479882547202,-13.6686886022201,
111.94883520527)) ;
#176116 = CARTESIAN_POINT('Ctrl Pts',(-26.7249168089774,-13.6857647626089,
111.878563304406)) ;
#176117 = CARTESIAN_POINT('Ctrl Pts',(-26.7987206510423,-13.6857647473879,
111.854332258593)) ;
#176118 = CARTESIAN_POINT('Ctrl Pts',(-26.8725244931072,-13.6857647321669,
111.83010121278)) ;
#176119 = CARTESIAN_POINT('Ctrl Pts',(-26.89559593885,-13.6686885717782,111.900373113643)) ;
#176120 = CARTESIAN_POINT('Ctrl Pts',(-26.9176753989106,-13.9407698971193,
112.00311647252)) ;
#176121 = CARTESIAN_POINT('Ctrl Pts',(-26.9385054854947,-13.9046696710089,
112.066561555162)) ;
#176122 = CARTESIAN_POINT('Ctrl Pts',(-26.8647016435677,-13.904669678464,
112.090792601395)) ;
#176123 = CARTESIAN_POINT('Ctrl Pts',(-26.7908978016408,-13.9046696859191,
112.115023647629)) ;
#176124 = CARTESIAN_POINT('Ctrl Pts',(-26.7700677150567,-13.9407699120296,
112.051578564986)) ;
#176125 = CARTESIAN_POINT('Ctrl Pts',(-26.7492376284726,-13.97687013814,111.988133482344)) ;
#176126 = CARTESIAN_POINT('Ctrl Pts',(-26.8230414703995,-13.9768701306849,
111.963902436111)) ;
#176127 = CARTESIAN_POINT('Ctrl Pts',(-26.8968453123265,-13.9768701232298,
111.939671389877)) ;
#176128 = CARTESIAN_POINT('Ctrl Pts',(-26.9176753989106,-13.9407698971193,
112.00311647252)) ;
#176129 = CARTESIAN_POINT('Ctrl Pts',(-26.9611957529866,-14.1754452261927,
112.171205228785)) ;
#176130 = CARTESIAN_POINT('Ctrl Pts',(-26.978282970121,-14.122903887043,112.223250135106)) ;
#176131 = CARTESIAN_POINT('Ctrl Pts',(-26.9044791274635,-14.1229038889288,
112.247481179114)) ;
#176132 = CARTESIAN_POINT('Ctrl Pts',(-26.8306752848061,-14.1229038908147,
112.271712223123)) ;
#176133 = CARTESIAN_POINT('Ctrl Pts',(-26.8135880676717,-14.1754452299645,
112.219667316802)) ;
#176134 = CARTESIAN_POINT('Ctrl Pts',(-26.7965008505373,-14.2279865691142,
112.167622410482)) ;
#176135 = CARTESIAN_POINT('Ctrl Pts',(-26.8703046931948,-14.2279865672284,
112.143391366473)) ;
#176136 = CARTESIAN_POINT('Ctrl Pts',(-26.9441085358522,-14.2279865653425,
112.119160322465)) ;
#176137 = CARTESIAN_POINT('Ctrl Pts',(-26.9611957529866,-14.1754452261927,
112.171205228785)) ;
#176138 = CARTESIAN_POINT('Ctrl Pts',(-27.0218558744677,-14.3550939223612,
112.391319568465)) ;
#176139 = CARTESIAN_POINT('Ctrl Pts',(-27.034001323059,-14.2899298530335,
112.428312645225)) ;
#176140 = CARTESIAN_POINT('Ctrl Pts',(-26.9601974795246,-14.2899298524596,
112.452543686563)) ;
#176141 = CARTESIAN_POINT('Ctrl Pts',(-26.8863936359901,-14.2899298518858,
112.4767747279)) ;
#176142 = CARTESIAN_POINT('Ctrl Pts',(-26.8742481873988,-14.3550939212134,
112.43978165114)) ;
#176143 = CARTESIAN_POINT('Ctrl Pts',(-26.8621027388075,-14.4202579905411,
112.402788574379)) ;
#176144 = CARTESIAN_POINT('Ctrl Pts',(-26.9359065823419,-14.420257991115,
112.378557533042)) ;
#176145 = CARTESIAN_POINT('Ctrl Pts',(-27.0097104258763,-14.4202579916889,
112.354326491705)) ;
#176146 = CARTESIAN_POINT('Ctrl Pts',(-27.0218558744677,-14.3550939223612,
112.391319568465)) ;
#176147 = CARTESIAN_POINT('Ctrl Pts',(-27.0954919754477,-14.468598908444,
112.65127280273)) ;
#176148 = CARTESIAN_POINT('Ctrl Pts',(-27.1017753646167,-14.3954110161889,
112.670410992381)) ;
#176149 = CARTESIAN_POINT('Ctrl Pts',(-27.0279715202262,-14.3954110152214,
112.694642031111)) ;
#176150 = CARTESIAN_POINT('Ctrl Pts',(-26.9541676758356,-14.395411014254,
112.718873069841)) ;
#176151 = CARTESIAN_POINT('Ctrl Pts',(-26.9478842866667,-14.4685989065091,
112.69973488019)) ;
#176152 = CARTESIAN_POINT('Ctrl Pts',(-26.9416008974978,-14.5417867987642,
112.680596690539)) ;
#176153 = CARTESIAN_POINT('Ctrl Pts',(-27.0154047418883,-14.5417867997317,
112.656365651809)) ;
#176154 = CARTESIAN_POINT('Ctrl Pts',(-27.0892085862788,-14.5417868006991,
112.632134613079)) ;
#176155 = CARTESIAN_POINT('Ctrl Pts',(-27.0954919754477,-14.468598908444,
112.65127280273)) ;
#176156 = CARTESIAN_POINT('Ctrl Pts',(-27.1747095469528,-14.5058659881171,
112.927861658512)) ;
#176157 = CARTESIAN_POINT('Ctrl Pts',(-27.1747399305109,-14.4299679241318,
112.927954201987)) ;
#176158 = CARTESIAN_POINT('Ctrl Pts',(-27.1009360861394,-14.4299679242476,
112.952185240775)) ;
#176159 = CARTESIAN_POINT('Ctrl Pts',(-27.027132241768,-14.4299679243634,
112.976416279563)) ;
#176160 = CARTESIAN_POINT('Ctrl Pts',(-27.0271018582099,-14.5058659883488,
112.976323736088)) ;
#176161 = CARTESIAN_POINT('Ctrl Pts',(-27.0270714746518,-14.5817640523341,
112.976231192613)) ;
#176162 = CARTESIAN_POINT('Ctrl Pts',(-27.1008753190232,-14.5817640522183,
112.952000153825)) ;
#176163 = CARTESIAN_POINT('Ctrl Pts',(-27.1746791633947,-14.5817640521025,
112.927769115037)) ;
#176164 = CARTESIAN_POINT('Ctrl Pts',(-27.1747095469528,-14.5058659881171,
112.927861658512)) ;
#176165 = CARTESIAN_POINT('Ctrl Pts',(-27.2540706728051,-14.465907705861,
113.205009023131)) ;
#176166 = CARTESIAN_POINT('Ctrl Pts',(-27.247826374031,-14.3926881487027,
113.185989896604)) ;
#176167 = CARTESIAN_POINT('Ctrl Pts',(-27.1740225302469,-14.3926881492861,
113.210220937181)) ;
#176168 = CARTESIAN_POINT('Ctrl Pts',(-27.1002186864629,-14.3926881498695,
113.234451977758)) ;
#176169 = CARTESIAN_POINT('Ctrl Pts',(-27.106462985237,-14.4659077070278,
113.253471104285)) ;
#176170 = CARTESIAN_POINT('Ctrl Pts',(-27.112707284011,-14.5391272641861,
113.272490230812)) ;
#176171 = CARTESIAN_POINT('Ctrl Pts',(-27.1865111277951,-14.5391272636027,
113.248259190235)) ;
#176172 = CARTESIAN_POINT('Ctrl Pts',(-27.2603149715792,-14.5391272630193,
113.224028149658)) ;
#176173 = CARTESIAN_POINT('Ctrl Pts',(-27.2540706728051,-14.465907705861,
113.205009023131)) ;
#176174 = CARTESIAN_POINT('Ctrl Pts',(-27.3270117595021,-14.3507454275659,
113.462647263951)) ;
#176175 = CARTESIAN_POINT('Ctrl Pts',(-27.3149310079399,-14.2854599330561,
113.425851243866)) ;
#176176 = CARTESIAN_POINT('Ctrl Pts',(-27.2411271652632,-14.2854599321569,
113.450082287816)) ;
#176177 = CARTESIAN_POINT('Ctrl Pts',(-27.1673233225865,-14.2854599312576,
113.474313331766)) ;
#176178 = CARTESIAN_POINT('Ctrl Pts',(-27.1794040741487,-14.3507454257675,
113.51110935185)) ;
#176179 = CARTESIAN_POINT('Ctrl Pts',(-27.1914848257109,-14.4160309202774,
113.547905371935)) ;
#176180 = CARTESIAN_POINT('Ctrl Pts',(-27.2652886683876,-14.4160309211766,
113.523674327985)) ;
#176181 = CARTESIAN_POINT('Ctrl Pts',(-27.3390925110643,-14.4160309220758,
113.499443284035)) ;
#176182 = CARTESIAN_POINT('Ctrl Pts',(-27.3270117595021,-14.3507454275659,
113.462647263951)) ;
#176183 = CARTESIAN_POINT('Ctrl Pts',(-27.3874657468428,-14.1684902162708,
113.682288696207)) ;
#176184 = CARTESIAN_POINT('Ctrl Pts',(-27.3704113071499,-14.1158354027091,
113.63034362447)) ;
#176185 = CARTESIAN_POINT('Ctrl Pts',(-27.2966074655942,-14.1158353972228,
113.654574671834)) ;
#176186 = CARTESIAN_POINT('Ctrl Pts',(-27.2228036240385,-14.1158353917364,
113.678805719198)) ;
#176187 = CARTESIAN_POINT('Ctrl Pts',(-27.2398580637314,-14.1684902052981,
113.730750790935)) ;
#176188 = CARTESIAN_POINT('Ctrl Pts',(-27.2569125034242,-14.2211450188598,
113.782695862672)) ;
#176189 = CARTESIAN_POINT('Ctrl Pts',(-27.33071634498,-14.2211450243462,113.758464815308)) ;
#176190 = CARTESIAN_POINT('Ctrl Pts',(-27.4045201865357,-14.2211450298325,
113.734233767944)) ;
#176191 = CARTESIAN_POINT('Ctrl Pts',(-27.3874657468428,-14.1684902162708,
113.682288696207)) ;
#176192 = CARTESIAN_POINT('Ctrl Pts',(-27.4302106667087,-13.9330107336615,
113.847901657391)) ;
#176193 = CARTESIAN_POINT('Ctrl Pts',(-27.4094139181739,-13.8967214466837,
113.784558116622)) ;
#176194 = CARTESIAN_POINT('Ctrl Pts',(-27.3356100770456,-13.8967214344113,
113.808789165288)) ;
#176195 = CARTESIAN_POINT('Ctrl Pts',(-27.2618062359173,-13.8967214221389,
113.833020213954)) ;
#176196 = CARTESIAN_POINT('Ctrl Pts',(-27.282602984452,-13.9330107091168,
113.896363754723)) ;
#176197 = CARTESIAN_POINT('Ctrl Pts',(-27.3033997329868,-13.9692999960946,
113.959707295493)) ;
#176198 = CARTESIAN_POINT('Ctrl Pts',(-27.3772035741151,-13.969300008367,
113.935476246827)) ;
#176199 = CARTESIAN_POINT('Ctrl Pts',(-27.4510074152434,-13.9693000206394,
113.911245198161)) ;
#176200 = CARTESIAN_POINT('Ctrl Pts',(-27.4302106667087,-13.9330107336615,
113.847901657391)) ;
#176201 = CARTESIAN_POINT('Ctrl Pts',(-27.4515998140738,-13.6600763512271,
113.948553659072)) ;
#176202 = CARTESIAN_POINT('Ctrl Pts',(-27.4285447209372,-13.6427914121404,
113.878331564877)) ;
#176203 = CARTESIAN_POINT('Ctrl Pts',(-27.3547408792523,-13.6427913908253,
113.902562611848)) ;
#176204 = CARTESIAN_POINT('Ctrl Pts',(-27.2809370375673,-13.6427913695102,
113.926793658818)) ;
#176205 = CARTESIAN_POINT('Ctrl Pts',(-27.3039921307039,-13.6600763085969,
113.997015753013)) ;
#176206 = CARTESIAN_POINT('Ctrl Pts',(-27.3270472238404,-13.6773612476836,
114.067237847207)) ;
#176207 = CARTESIAN_POINT('Ctrl Pts',(-27.4008510655254,-13.6773612689987,
114.043006800237)) ;
#176208 = CARTESIAN_POINT('Ctrl Pts',(-27.4746549072103,-13.6773612903137,
114.018775753266)) ;
#176209 = CARTESIAN_POINT('Ctrl Pts',(-27.4515998140738,-13.6600763512271,
113.948553659072)) ;
#176210 = CARTESIAN_POINT('Ctrl Pts',(-27.4493246185078,-13.3704757504778,
113.977035138527)) ;
#176211 = CARTESIAN_POINT('Ctrl Pts',(-27.4256622922529,-13.3733860820227,
113.904963510084)) ;
#176212 = CARTESIAN_POINT('Ctrl Pts',(-27.3518584487016,-13.3733860523621,
113.92919455137)) ;
#176213 = CARTESIAN_POINT('Ctrl Pts',(-27.2780546051503,-13.3733860227015,
113.953425592656)) ;
#176214 = CARTESIAN_POINT('Ctrl Pts',(-27.3017169314052,-13.3704756911566,
114.025497221099)) ;
#176215 = CARTESIAN_POINT('Ctrl Pts',(-27.3253792576601,-13.3675653596117,
114.097568849542)) ;
#176216 = CARTESIAN_POINT('Ctrl Pts',(-27.3991831012114,-13.3675653892723,
114.073337808256)) ;
#176217 = CARTESIAN_POINT('Ctrl Pts',(-27.4729869447627,-13.3675654189329,
114.04910676697)) ;
#176218 = CARTESIAN_POINT('Ctrl Pts',(-27.4493246185078,-13.3704757504778,
113.977035138527)) ;
#176219 = CARTESIAN_POINT('Ctrl Pts',(-27.4224958680665,-13.0823700026988,
113.93098284499)) ;
#176220 = CARTESIAN_POINT('Ctrl Pts',(-27.3999343634008,-13.1054004112685,
113.862264141289)) ;
#176221 = CARTESIAN_POINT('Ctrl Pts',(-27.3261305163557,-13.1054003729185,
113.886495171933)) ;
#176222 = CARTESIAN_POINT('Ctrl Pts',(-27.2523266693107,-13.1054003345686,
113.910726202578)) ;
#176223 = CARTESIAN_POINT('Ctrl Pts',(-27.2748881739764,-13.0823699259989,
113.979444906279)) ;
#176224 = CARTESIAN_POINT('Ctrl Pts',(-27.2974496786422,-13.0593395174292,
114.048163609981)) ;
#176225 = CARTESIAN_POINT('Ctrl Pts',(-27.3712535256872,-13.0593395557792,
114.023932579336)) ;
#176226 = CARTESIAN_POINT('Ctrl Pts',(-27.4450573727323,-13.0593395941291,
113.999701548692)) ;
#176227 = CARTESIAN_POINT('Ctrl Pts',(-27.4224958680665,-13.0823700026988,
113.93098284499)) ;
#176228 = CARTESIAN_POINT('Ctrl Pts',(-27.3729809937545,-12.8213180178566,
113.815427357995)) ;
#176229 = CARTESIAN_POINT('Ctrl Pts',(-27.3531145848407,-12.8626079589609,
113.754917480972)) ;
#176230 = CARTESIAN_POINT('Ctrl Pts',(-27.2793107335955,-12.862607919451,
113.779148498824)) ;
#176231 = CARTESIAN_POINT('Ctrl Pts',(-27.2055068823504,-12.8626078799411,
113.803379516675)) ;
#176232 = CARTESIAN_POINT('Ctrl Pts',(-27.2253732912641,-12.8213179388368,
113.863889393698)) ;
#176233 = CARTESIAN_POINT('Ctrl Pts',(-27.2452397001779,-12.7800279977325,
113.92439927072)) ;
#176234 = CARTESIAN_POINT('Ctrl Pts',(-27.3190435514231,-12.7800280372424,
113.900168252869)) ;
#176235 = CARTESIAN_POINT('Ctrl Pts',(-27.3928474026682,-12.7800280767523,
113.875937235017)) ;
#176236 = CARTESIAN_POINT('Ctrl Pts',(-27.3729809937545,-12.8213180178566,
113.815427357995)) ;
#176237 = CARTESIAN_POINT('Ctrl Pts',(-27.3028037991072,-12.6009816910039,
113.637217641596)) ;
#176238 = CARTESIAN_POINT('Ctrl Pts',(-27.2870729381168,-12.6577150521394,
113.589303976099)) ;
#176239 = CARTESIAN_POINT('Ctrl Pts',(-27.2132690817063,-12.6577150144821,
113.613534978217)) ;
#176240 = CARTESIAN_POINT('Ctrl Pts',(-27.1394652252959,-12.6577149768248,
113.637765980336)) ;
#176241 = CARTESIAN_POINT('Ctrl Pts',(-27.1551960862862,-12.6009816156892,
113.685679645834)) ;
#176242 = CARTESIAN_POINT('Ctrl Pts',(-27.1709269472766,-12.5442482545536,
113.733593311332)) ;
#176243 = CARTESIAN_POINT('Ctrl Pts',(-27.2447308036871,-12.5442482922109,
113.709362309213)) ;
#176244 = CARTESIAN_POINT('Ctrl Pts',(-27.3185346600976,-12.5442483298683,
113.685131307094)) ;
#176245 = CARTESIAN_POINT('Ctrl Pts',(-27.3028037991072,-12.6009816910039,
113.637217641596)) ;
#176246 = CARTESIAN_POINT('Ctrl Pts',(-27.2168540748088,-12.4399155910324,
113.410819058086)) ;
#176247 = CARTESIAN_POINT('Ctrl Pts',(-27.2063690680483,-12.5079761461326,
113.378883418007)) ;
#176248 = CARTESIAN_POINT('Ctrl Pts',(-27.132565206792,-12.5079761174331,
113.403114405366)) ;
#176249 = CARTESIAN_POINT('Ctrl Pts',(-27.0587613455356,-12.5079760887335,
113.427345392725)) ;
#176250 = CARTESIAN_POINT('Ctrl Pts',(-27.0692463522961,-12.4399155336333,
113.459281032804)) ;
#176251 = CARTESIAN_POINT('Ctrl Pts',(-27.0797313590565,-12.3718549785331,
113.491216672884)) ;
#176252 = CARTESIAN_POINT('Ctrl Pts',(-27.1535352203129,-12.3718550072327,
113.466985685525)) ;
#176253 = CARTESIAN_POINT('Ctrl Pts',(-27.2273390815693,-12.3718550359322,
113.442754698166)) ;
#176254 = CARTESIAN_POINT('Ctrl Pts',(-27.2168540748088,-12.4399155910324,
113.410819058086)) ;
#176255 = CARTESIAN_POINT('Ctrl Pts',(-27.1197079246416,-12.3483508718252,
113.15053363995)) ;
#176256 = CARTESIAN_POINT('Ctrl Pts',(-27.1152534269706,-12.4229031690547,
113.136965957357)) ;
#176257 = CARTESIAN_POINT('Ctrl Pts',(-27.0414495611112,-12.4229031549688,
113.161196930696)) ;
#176258 = CARTESIAN_POINT('Ctrl Pts',(-26.9676456952518,-12.4229031408829,
113.185427904035)) ;
#176259 = CARTESIAN_POINT('Ctrl Pts',(-26.9721001929228,-12.3483508436534,
113.198995586628)) ;
#176260 = CARTESIAN_POINT('Ctrl Pts',(-26.9765546905938,-12.2737985464239,
113.212563269221)) ;
#176261 = CARTESIAN_POINT('Ctrl Pts',(-27.0503585564532,-12.2737985605098,
113.188332295882)) ;
#176262 = CARTESIAN_POINT('Ctrl Pts',(-27.1241624223126,-12.2737985745957,
113.164101322543)) ;
#176263 = CARTESIAN_POINT('Ctrl Pts',(-27.1197079246416,-12.3483508718252,
113.15053363995)) ;
#176264 = CARTESIAN_POINT('Ctrl Pts',(-27.0187802117475,-12.3338872424077,
112.878480782108)) ;
#176265 = CARTESIAN_POINT('Ctrl Pts',(-27.0206341859005,-12.4095571114995,
112.884127686696)) ;
#176266 = CARTESIAN_POINT('Ctrl Pts',(-26.9468303176289,-12.4095571176329,
112.908358652687)) ;
#176267 = CARTESIAN_POINT('Ctrl Pts',(-26.8730264493573,-12.4095571237664,
112.932589618679)) ;
#176268 = CARTESIAN_POINT('Ctrl Pts',(-26.8711724752043,-12.3338872546745,
112.926942714091)) ;
#176269 = CARTESIAN_POINT('Ctrl Pts',(-26.8693185010513,-12.2582173855827,
112.921295809504)) ;
#176270 = CARTESIAN_POINT('Ctrl Pts',(-26.9431223693229,-12.2582173794493,
112.897064843512)) ;
#176271 = CARTESIAN_POINT('Ctrl Pts',(-27.0169262375945,-12.2582173733159,
112.87283387752)) ;
#176272 = CARTESIAN_POINT('Ctrl Pts',(-27.0187802117475,-12.3338872424077,
112.878480782108)) ;
#176273 = CARTESIAN_POINT('Ctrl Pts',(-26.9193985159767,-12.396923495094,
112.611312558498)) ;
#176274 = CARTESIAN_POINT('Ctrl Pts',(-26.9274584480283,-12.4683025104667,
112.635861809373)) ;
#176275 = CARTESIAN_POINT('Ctrl Pts',(-26.8536545789805,-12.4683025400751,
112.660092773001)) ;
#176276 = CARTESIAN_POINT('Ctrl Pts',(-26.7798507099327,-12.4683025696834,
112.684323736628)) ;
#176277 = CARTESIAN_POINT('Ctrl Pts',(-26.7717907778811,-12.3969235543106,
112.659774485753)) ;
#176278 = CARTESIAN_POINT('Ctrl Pts',(-26.7637308458295,-12.3255445389379,
112.635225234877)) ;
#176279 = CARTESIAN_POINT('Ctrl Pts',(-26.8375347148773,-12.3255445093296,
112.61099427125)) ;
#176280 = CARTESIAN_POINT('Ctrl Pts',(-26.9113385839251,-12.3255444797213,
112.586763307622)) ;
#176281 = CARTESIAN_POINT('Ctrl Pts',(-26.9193985159767,-12.396923495094,
112.611312558498)) ;
#176282 = CARTESIAN_POINT('Ctrl Pts',(-26.8285566748927,-12.5334553693914,
112.370120041222)) ;
#176283 = CARTESIAN_POINT('Ctrl Pts',(-26.8422361287122,-12.595406254364,
112.411785448577)) ;
#176284 = CARTESIAN_POINT('Ctrl Pts',(-26.7684322615119,-12.5954063084814,
112.436016417832)) ;
#176285 = CARTESIAN_POINT('Ctrl Pts',(-26.6946283943116,-12.5954063625988,
112.460247387086)) ;
#176286 = CARTESIAN_POINT('Ctrl Pts',(-26.6809489404921,-12.5334554776262,
112.418581979731)) ;
#176287 = CARTESIAN_POINT('Ctrl Pts',(-26.6672694866725,-12.4715045926535,
112.376916572376)) ;
#176288 = CARTESIAN_POINT('Ctrl Pts',(-26.7410733538728,-12.4715045385361,
112.352685603122)) ;
#176289 = CARTESIAN_POINT('Ctrl Pts',(-26.8148772210732,-12.4715044844187,
112.328454633867)) ;
#176290 = CARTESIAN_POINT('Ctrl Pts',(-26.8285566748927,-12.5334553693914,
112.370120041222)) ;
#176291 = CARTESIAN_POINT('Ctrl Pts',(-26.7522001619182,-12.7322215761211,
112.172876186384)) ;
#176292 = CARTESIAN_POINT('Ctrl Pts',(-26.7704995100276,-12.7803853400704,
112.228613046245)) ;
#176293 = CARTESIAN_POINT('Ctrl Pts',(-26.696695647293,-12.7803854158274,
112.252844029101)) ;
#176294 = CARTESIAN_POINT('Ctrl Pts',(-26.6228917845584,-12.7803854915845,
112.277075011958)) ;
#176295 = CARTESIAN_POINT('Ctrl Pts',(-26.604592436449,-12.7322217276352,
112.221338152097)) ;
#176296 = CARTESIAN_POINT('Ctrl Pts',(-26.5862930883396,-12.6840579636859,
112.165601292236)) ;
#176297 = CARTESIAN_POINT('Ctrl Pts',(-26.6600969510742,-12.6840578879289,
112.141370309379)) ;
#176298 = CARTESIAN_POINT('Ctrl Pts',(-26.7339008138088,-12.6840578121718,
112.117139326523)) ;
#176299 = CARTESIAN_POINT('Ctrl Pts',(-26.7522001619182,-12.7322215761211,
112.172876186384)) ;
#176300 = CARTESIAN_POINT('Ctrl Pts',(-26.6943187231654,-12.9810049412899,
112.032078055127)) ;
#176301 = CARTESIAN_POINT('Ctrl Pts',(-26.7159513885438,-13.0118702151138,
112.097967661475)) ;
#176302 = CARTESIAN_POINT('Ctrl Pts',(-26.6421475322302,-13.0118703086727,
112.122198663889)) ;
#176303 = CARTESIAN_POINT('Ctrl Pts',(-26.5683436759166,-13.0118704022315,
112.146429666303)) ;
#176304 = CARTESIAN_POINT('Ctrl Pts',(-26.5467110105383,-12.9810051284076,
112.080540059955)) ;
#176305 = CARTESIAN_POINT('Ctrl Pts',(-26.52507834516,-12.9501398545836,112.014650453607)) ;
#176306 = CARTESIAN_POINT('Ctrl Pts',(-26.5988822014735,-12.9501397610248,
111.990419451193)) ;
#176307 = CARTESIAN_POINT('Ctrl Pts',(-26.6726860577871,-12.9501396674659,
111.966188448779)) ;
#176308 = CARTESIAN_POINT('Ctrl Pts',(-26.6943187231654,-12.9810049412899,
112.032078055127)) ;
#176309 = CARTESIAN_POINT('Ctrl Pts',(-26.6587912592978,-13.2609753303157,
111.959335470938)) ;
#176310 = CARTESIAN_POINT('Ctrl Pts',(-26.6822021833276,-13.2723394892272,
112.030641366156)) ;
#176311 = CARTESIAN_POINT('Ctrl Pts',(-26.6083983351151,-13.2723395935458,
112.054872393245)) ;
#176312 = CARTESIAN_POINT('Ctrl Pts',(-26.5345944869027,-13.2723396978644,
112.079103420333)) ;
#176313 = CARTESIAN_POINT('Ctrl Pts',(-26.511183562873,-13.260975538953,112.007797525115)) ;
#176314 = CARTESIAN_POINT('Ctrl Pts',(-26.4877726388432,-13.2496113800415,
111.936491629897)) ;
#176315 = CARTESIAN_POINT('Ctrl Pts',(-26.5615764870557,-13.2496112757229,
111.912260602808)) ;
#176316 = CARTESIAN_POINT('Ctrl Pts',(-26.6353803352681,-13.2496111714043,
111.88802957572)) ;
#176317 = CARTESIAN_POINT('Ctrl Pts',(-26.6587912592978,-13.2609753303157,
111.959335470938)) ;
#176318 = CARTESIAN_POINT('Ctrl Pts',(-26.647319062969,-13.5522070361543,
111.959866894059)) ;
#176319 = CARTESIAN_POINT('Ctrl Pts',(-26.6708314077499,-13.5432552863656,
112.031481700481)) ;
#176320 = CARTESIAN_POINT('Ctrl Pts',(-26.59702756845,-13.5432553930549,112.055712754716)) ;
#176321 = CARTESIAN_POINT('Ctrl Pts',(-26.52322372915,-13.5432554997441,112.079943808951)) ;
#176322 = CARTESIAN_POINT('Ctrl Pts',(-26.4997113843691,-13.5522072495328,
112.008329002528)) ;
#176323 = CARTESIAN_POINT('Ctrl Pts',(-26.4761990395882,-13.5611589993214,
111.936714196106)) ;
#176324 = CARTESIAN_POINT('Ctrl Pts',(-26.5500028788881,-13.5611588926322,
111.912483141871)) ;
#176325 = CARTESIAN_POINT('Ctrl Pts',(-26.623806718188,-13.5611587859429,
111.888252087637)) ;
#176326 = CARTESIAN_POINT('Ctrl Pts',(-26.647319062969,-13.5522070361543,
111.959866894059)) ;
#176327 = CARTESIAN_POINT('Ctrl Pts',(-26.6599556627793,-13.8335794690488,
112.033796091262)) ;
#176328 = CARTESIAN_POINT('Ctrl Pts',(-26.6818871675792,-13.8049701426201,
112.100595914152)) ;
#176329 = CARTESIAN_POINT('Ctrl Pts',(-26.6080833370899,-13.8049702427903,
112.124826995223)) ;
#176330 = CARTESIAN_POINT('Ctrl Pts',(-26.5342795066006,-13.8049703429605,
112.149058076293)) ;
#176331 = CARTESIAN_POINT('Ctrl Pts',(-26.5123480018007,-13.8335796693892,
112.082258253403)) ;
#176332 = CARTESIAN_POINT('Ctrl Pts',(-26.4904164970008,-13.862188995818,
112.015458430512)) ;
#176333 = CARTESIAN_POINT('Ctrl Pts',(-26.5642203274901,-13.8621888956478,
111.991227349442)) ;
#176334 = CARTESIAN_POINT('Ctrl Pts',(-26.6380241579794,-13.8621887954776,
111.966996268371)) ;
#176335 = CARTESIAN_POINT('Ctrl Pts',(-26.6599556627793,-13.8335794690488,
112.033796091262)) ;
#176336 = CARTESIAN_POINT('Ctrl Pts',(-26.6950792057711,-14.0854850074698,
112.176258032588)) ;
#176337 = CARTESIAN_POINT('Ctrl Pts',(-26.7138568726991,-14.0392461681425,
112.233451774195)) ;
#176338 = CARTESIAN_POINT('Ctrl Pts',(-26.6400530500181,-14.0392462534928,
112.257682879048)) ;
#176339 = CARTESIAN_POINT('Ctrl Pts',(-26.5662492273371,-14.039246338843,
112.281913983902)) ;
#176340 = CARTESIAN_POINT('Ctrl Pts',(-26.5474715604091,-14.0854851781703,
112.224720242295)) ;
#176341 = CARTESIAN_POINT('Ctrl Pts',(-26.5286938934811,-14.1317240174977,
112.167526500688)) ;
#176342 = CARTESIAN_POINT('Ctrl Pts',(-26.6024977161621,-14.1317239321474,
112.143295395835)) ;
#176343 = CARTESIAN_POINT('Ctrl Pts',(-26.6763015388431,-14.1317238467972,
112.119064290982)) ;
#176344 = CARTESIAN_POINT('Ctrl Pts',(-26.6950792057711,-14.0854850074698,
112.176258032588)) ;
#176345 = CARTESIAN_POINT('Ctrl Pts',(-26.7493678080384,-14.2893882283517,
112.377063192394)) ;
#176346 = CARTESIAN_POINT('Ctrl Pts',(-26.7636496039739,-14.2288448467623,
112.42056323639)) ;
#176347 = CARTESIAN_POINT('Ctrl Pts',(-26.6898457872909,-14.2288449105474,
112.444794359512)) ;
#176348 = CARTESIAN_POINT('Ctrl Pts',(-26.6160419706078,-14.2288449743324,
112.469025482634)) ;
#176349 = CARTESIAN_POINT('Ctrl Pts',(-26.6017601746723,-14.2893883559219,
112.425525438638)) ;
#176350 = CARTESIAN_POINT('Ctrl Pts',(-26.5874783787368,-14.3499317375113,
112.382025394642)) ;
#176351 = CARTESIAN_POINT('Ctrl Pts',(-26.6612821954199,-14.3499316737262,
112.35779427152)) ;
#176352 = CARTESIAN_POINT('Ctrl Pts',(-26.7350860121029,-14.3499316099411,
112.333563148398)) ;
#176353 = CARTESIAN_POINT('Ctrl Pts',(-26.7493678080384,-14.2893882283517,
112.377063192394)) ;
#176354 = CARTESIAN_POINT('Ctrl Pts',(-26.8182694831193,-14.4310416708449,
112.622412303935)) ;
#176355 = CARTESIAN_POINT('Ctrl Pts',(-26.8270278462195,-14.3605181681089,
112.649088862766)) ;
#176356 = CARTESIAN_POINT('Ctrl Pts',(-26.7532240331301,-14.3605182058442,
112.673319996834)) ;
#176357 = CARTESIAN_POINT('Ctrl Pts',(-26.6794202200406,-14.3605182435796,
112.697551130901)) ;
#176358 = CARTESIAN_POINT('Ctrl Pts',(-26.6706618569405,-14.4310417463156,
112.67087457207)) ;
#176359 = CARTESIAN_POINT('Ctrl Pts',(-26.6619034938403,-14.5015652490516,
112.644198013239)) ;
#176360 = CARTESIAN_POINT('Ctrl Pts',(-26.7357073069297,-14.5015652113162,
112.619966879171)) ;
#176361 = CARTESIAN_POINT('Ctrl Pts',(-26.8095111200191,-14.5015651735809,
112.595735745103)) ;
#176362 = CARTESIAN_POINT('Ctrl Pts',(-26.8182694831193,-14.4310416708449,
112.622412303935)) ;
#176363 = CARTESIAN_POINT('Ctrl Pts',(-26.8960209759952,-14.4999960091202,
112.894701404491)) ;
#176364 = CARTESIAN_POINT('Ctrl Pts',(-26.8986301066341,-14.4245527843061,
112.902648393491)) ;
#176365 = CARTESIAN_POINT('Ctrl Pts',(-26.8248262944529,-14.4245527944394,
112.926879530325)) ;
#176366 = CARTESIAN_POINT('Ctrl Pts',(-26.7510224822716,-14.4245528045727,
112.951110667159)) ;
#176367 = CARTESIAN_POINT('Ctrl Pts',(-26.7484133516328,-14.4999960293868,
112.943163678159)) ;
#176368 = CARTESIAN_POINT('Ctrl Pts',(-26.7458042209939,-14.5754392542009,
112.93521668916)) ;
#176369 = CARTESIAN_POINT('Ctrl Pts',(-26.8196080331751,-14.5754392440676,
112.910985552326)) ;
#176370 = CARTESIAN_POINT('Ctrl Pts',(-26.8934118453563,-14.5754392339344,
112.886754415492)) ;
#176371 = CARTESIAN_POINT('Ctrl Pts',(-26.8960209759952,-14.4999960091202,
112.894701404491)) ;
#176372 = CARTESIAN_POINT('Ctrl Pts',(-26.9762322526902,-14.4914668725251,
113.174447910469)) ;
#176373 = CARTESIAN_POINT('Ctrl Pts',(-26.9725118930449,-14.4165060453907,
113.163116293409)) ;
#176374 = CARTESIAN_POINT('Ctrl Pts',(-26.8987080792064,-14.4165060293028,
113.187347425195)) ;
#176375 = CARTESIAN_POINT('Ctrl Pts',(-26.8249042653679,-14.416506013215,
113.211578556981)) ;
#176376 = CARTESIAN_POINT('Ctrl Pts',(-26.8286246250133,-14.4914668403494,
113.222910174041)) ;
#176377 = CARTESIAN_POINT('Ctrl Pts',(-26.8323449846586,-14.5664276674838,
113.234241791102)) ;
#176378 = CARTESIAN_POINT('Ctrl Pts',(-26.906148798497,-14.5664276835716,
113.210010659315)) ;
#176379 = CARTESIAN_POINT('Ctrl Pts',(-26.9799526123356,-14.5664276996595,
113.185779527529)) ;
#176380 = CARTESIAN_POINT('Ctrl Pts',(-26.9762322526902,-14.4914668725251,
113.174447910469)) ;
#176381 = CARTESIAN_POINT('Ctrl Pts',(-27.0525399232105,-14.4062237339893,
113.44231798111)) ;
#176382 = CARTESIAN_POINT('Ctrl Pts',(-27.0427528161706,-14.3371017134928,
113.412508030457)) ;
#176383 = CARTESIAN_POINT('Ctrl Pts',(-26.9689489983906,-14.337101674971,
113.436739150238)) ;
#176384 = CARTESIAN_POINT('Ctrl Pts',(-26.8951451806107,-14.3371016364492,
113.460970270019)) ;
#176385 = CARTESIAN_POINT('Ctrl Pts',(-26.9049322876505,-14.4062236569457,
113.490780220672)) ;
#176386 = CARTESIAN_POINT('Ctrl Pts',(-26.9147193946903,-14.4753456774423,
113.520590171325)) ;
#176387 = CARTESIAN_POINT('Ctrl Pts',(-26.9885232124703,-14.4753457159641,
113.496359051544)) ;
#176388 = CARTESIAN_POINT('Ctrl Pts',(-27.0623270302503,-14.4753457544858,
113.472127931763)) ;
#176389 = CARTESIAN_POINT('Ctrl Pts',(-27.0525399232105,-14.4062237339893,
113.44231798111)) ;
#176390 = CARTESIAN_POINT('Ctrl Pts',(-27.1188648773087,-14.2495321967945,
113.679899921954)) ;
#176391 = CARTESIAN_POINT('Ctrl Pts',(-27.103696319169,-14.1912456004984,
113.633698939684)) ;
#176392 = CARTESIAN_POINT('Ctrl Pts',(-27.0298924955446,-14.1912455461204,
113.657930041664)) ;
#176393 = CARTESIAN_POINT('Ctrl Pts',(-26.9560886719202,-14.1912454917425,
113.682161143644)) ;
#176394 = CARTESIAN_POINT('Ctrl Pts',(-26.9712572300598,-14.2495320880387,
113.728362125914)) ;
#176395 = CARTESIAN_POINT('Ctrl Pts',(-26.9864257881994,-14.3078186843349,
113.774563108183)) ;
#176396 = CARTESIAN_POINT('Ctrl Pts',(-27.0602296118238,-14.3078187387128,
113.750332006204)) ;
#176397 = CARTESIAN_POINT('Ctrl Pts',(-27.1340334354483,-14.3078187930907,
113.726100904224)) ;
#176398 = CARTESIAN_POINT('Ctrl Pts',(-27.1188648773087,-14.2495321967945,
113.679899921954)) ;
#176399 = CARTESIAN_POINT('Ctrl Pts',(-27.1692281183874,-14.0340281298451,
113.868701151054)) ;
#176400 = CARTESIAN_POINT('Ctrl Pts',(-27.149787780751,-13.990699945468,113.809489017816)) ;
#176401 = CARTESIAN_POINT('Ctrl Pts',(-27.075983950736,-13.9906998817967,
113.833720100331)) ;
#176402 = CARTESIAN_POINT('Ctrl Pts',(-27.0021801207209,-13.9906998181254,
113.857951182846)) ;
#176403 = CARTESIAN_POINT('Ctrl Pts',(-27.0216204583573,-14.0340280025025,
113.917163316084)) ;
#176404 = CARTESIAN_POINT('Ctrl Pts',(-27.0410607959936,-14.0773561868796,
113.976375449322)) ;
#176405 = CARTESIAN_POINT('Ctrl Pts',(-27.1148646260087,-14.0773562505509,
113.952144366807)) ;
#176406 = CARTESIAN_POINT('Ctrl Pts',(-27.1886684560238,-14.0773563142222,
113.927913284292)) ;
#176407 = CARTESIAN_POINT('Ctrl Pts',(-27.1692281183874,-14.0340281298451,
113.868701151054)) ;
#176408 = CARTESIAN_POINT('Ctrl Pts',(-27.1996623984703,-13.7742259092907,
113.99685412237)) ;
#176409 = CARTESIAN_POINT('Ctrl Pts',(-27.1773340852671,-13.7489714833696,
113.928845681678)) ;
#176410 = CARTESIAN_POINT('Ctrl Pts',(-27.1035302487081,-13.7489714178304,
113.953076744261)) ;
#176411 = CARTESIAN_POINT('Ctrl Pts',(-27.0297264121491,-13.7489713522911,
113.977307806844)) ;
#176412 = CARTESIAN_POINT('Ctrl Pts',(-27.0520547253523,-13.7742257782122,
114.045316247537)) ;
#176413 = CARTESIAN_POINT('Ctrl Pts',(-27.0743830385556,-13.7994802041333,
114.113324688229)) ;
#176414 = CARTESIAN_POINT('Ctrl Pts',(-27.1481868751146,-13.7994802696726,
114.089093625646)) ;
#176415 = CARTESIAN_POINT('Ctrl Pts',(-27.2219907116736,-13.7994803352118,
114.064862563063)) ;
#176416 = CARTESIAN_POINT('Ctrl Pts',(-27.1996623984703,-13.7742259092907,
113.99685412237)) ;
#176417 = CARTESIAN_POINT('Ctrl Pts',(-27.2071696580136,-13.488993839479,
114.055160255525)) ;
#176418 = CARTESIAN_POINT('Ctrl Pts',(-27.1835500172681,-13.4836161224244,
113.983218639649)) ;
#176419 = CARTESIAN_POINT('Ctrl Pts',(-27.1097461748366,-13.4836160614426,
114.007449684346)) ;
#176420 = CARTESIAN_POINT('Ctrl Pts',(-27.0359423324051,-13.4836160004609,
114.031680729042)) ;
#176421 = CARTESIAN_POINT('Ctrl Pts',(-27.0595619731506,-13.4889937175154,
114.103622344918)) ;
#176422 = CARTESIAN_POINT('Ctrl Pts',(-27.0831816138961,-13.49437143457,114.175563960794)) ;
#176423 = CARTESIAN_POINT('Ctrl Pts',(-27.1569854563276,-13.4943714955518,
114.151332916098)) ;
#176424 = CARTESIAN_POINT('Ctrl Pts',(-27.2307892987591,-13.4943715565336,
114.127101871401)) ;
#176425 = CARTESIAN_POINT('Ctrl Pts',(-27.2071696580136,-13.488993839479,
114.055160255525)) ;
#176426 = CARTESIAN_POINT('Ctrl Pts',(-27.1902825049831,-13.1975717487405,
114.039308325117)) ;
#176427 = CARTESIAN_POINT('Ctrl Pts',(-27.1670696758155,-13.2125333094721,
113.968605791857)) ;
#176428 = CARTESIAN_POINT('Ctrl Pts',(-27.0932658289276,-13.2125332593627,
113.99283682298)) ;
#176429 = CARTESIAN_POINT('Ctrl Pts',(-27.0194619820398,-13.2125332092533,
114.017067854103)) ;
#176430 = CARTESIAN_POINT('Ctrl Pts',(-27.0426748112073,-13.1975716485217,
114.087770387363)) ;
#176431 = CARTESIAN_POINT('Ctrl Pts',(-27.0658876403749,-13.1826100877902,
114.158472920623)) ;
#176432 = CARTESIAN_POINT('Ctrl Pts',(-27.1396914872628,-13.1826101378995,
114.1342418895)) ;
#176433 = CARTESIAN_POINT('Ctrl Pts',(-27.2134953341506,-13.1826101880089,
114.110010858377)) ;
#176434 = CARTESIAN_POINT('Ctrl Pts',(-27.1902825049831,-13.1975717487405,
114.039308325117)) ;
#176435 = CARTESIAN_POINT('Ctrl Pts',(-27.1498141482332,-12.9237175982201,
113.951393026303)) ;
#176436 = CARTESIAN_POINT('Ctrl Pts',(-27.1286603816229,-12.9578227208983,
113.88696206551)) ;
#176437 = CARTESIAN_POINT('Ctrl Pts',(-27.0548565317877,-12.9578226823066,
113.911193087656)) ;
#176438 = CARTESIAN_POINT('Ctrl Pts',(-26.9810526819526,-12.9578226437149,
113.935424109803)) ;
#176439 = CARTESIAN_POINT('Ctrl Pts',(-27.002206448563,-12.9237175210368,
113.999855070596)) ;
#176440 = CARTESIAN_POINT('Ctrl Pts',(-27.0233602151733,-12.8896123983586,
114.064286031389)) ;
#176441 = CARTESIAN_POINT('Ctrl Pts',(-27.0971640650084,-12.8896124369503,
114.040055009243)) ;
#176442 = CARTESIAN_POINT('Ctrl Pts',(-27.1709679148435,-12.889612475542,
114.015823987097)) ;
#176443 = CARTESIAN_POINT('Ctrl Pts',(-27.1498141482332,-12.9237175982201,
113.951393026303)) ;
#176444 = CARTESIAN_POINT('Ctrl Pts',(-27.0872605509044,-12.6833926232874,
113.796490915852)) ;
#176445 = CARTESIAN_POINT('Ctrl Pts',(-27.069705007748,-12.7343299181759,
113.743019563325)) ;
#176446 = CARTESIAN_POINT('Ctrl Pts',(-26.9959011570845,-12.7343298939571,
113.767250582949)) ;
#176447 = CARTESIAN_POINT('Ctrl Pts',(-26.9220973064211,-12.7343298697383,
113.791481602572)) ;
#176448 = CARTESIAN_POINT('Ctrl Pts',(-26.9396528495775,-12.6833925748499,
113.844952955098)) ;
#176449 = CARTESIAN_POINT('Ctrl Pts',(-26.9572083927339,-12.6324552799614,
113.898424307625)) ;
#176450 = CARTESIAN_POINT('Ctrl Pts',(-27.0310122433973,-12.6324553041802,
113.874193288001)) ;
#176451 = CARTESIAN_POINT('Ctrl Pts',(-27.1048160940608,-12.632455328399,
113.849962268378)) ;
#176452 = CARTESIAN_POINT('Ctrl Pts',(-27.0872605509044,-12.6833926232874,
113.796490915852)) ;
#176453 = CARTESIAN_POINT('Ctrl Pts',(-27.0073325603644,-12.4975233316372,
113.588365552072)) ;
#176454 = CARTESIAN_POINT('Ctrl Pts',(-26.994600389807,-12.5615155230103,
113.549585414369)) ;
#176455 = CARTESIAN_POINT('Ctrl Pts',(-26.9207965392856,-12.5615155094136,
113.573816434425)) ;
#176456 = CARTESIAN_POINT('Ctrl Pts',(-26.8469926887642,-12.561515495817,
113.598047454481)) ;
#176457 = CARTESIAN_POINT('Ctrl Pts',(-26.8597248593216,-12.4975233044439,
113.636827592184)) ;
#176458 = CARTESIAN_POINT('Ctrl Pts',(-26.872457029879,-12.4335311130708,
113.675607729887)) ;
#176459 = CARTESIAN_POINT('Ctrl Pts',(-26.9462608804004,-12.4335311266674,
113.651376709831)) ;
#176460 = CARTESIAN_POINT('Ctrl Pts',(-27.0200647309218,-12.433531140264,
113.627145689775)) ;
#176461 = CARTESIAN_POINT('Ctrl Pts',(-27.0073325603644,-12.4975233316372,
113.588365552072)) ;
#176462 = CARTESIAN_POINT('Ctrl Pts',(-26.9141377906141,-12.3765652756753,
113.339997758843)) ;
#176463 = CARTESIAN_POINT('Ctrl Pts',(-26.907159197438,-12.4491001941253,
113.318742089663)) ;
#176464 = CARTESIAN_POINT('Ctrl Pts',(-26.8333553484405,-12.44910018943,113.342973114361)) ;
#176465 = CARTESIAN_POINT('Ctrl Pts',(-26.759551499443,-12.4491001847347,
113.367204139058)) ;
#176466 = CARTESIAN_POINT('Ctrl Pts',(-26.7665300926192,-12.3765652662847,
113.388459808238)) ;
#176467 = CARTESIAN_POINT('Ctrl Pts',(-26.7735086857953,-12.3040303478347,
113.409715477419)) ;
#176468 = CARTESIAN_POINT('Ctrl Pts',(-26.8473125347928,-12.30403035253,113.385484452721)) ;
#176469 = CARTESIAN_POINT('Ctrl Pts',(-26.9211163837903,-12.3040303572253,
113.361253428023)) ;
#176470 = CARTESIAN_POINT('Ctrl Pts',(-26.9141377906141,-12.3765652756753,
113.339997758843)) ;
#176471 = CARTESIAN_POINT('Ctrl Pts',(-26.8140599847601,-12.3303669115662,
113.070599618917)) ;
#176472 = CARTESIAN_POINT('Ctrl Pts',(-26.8133257493235,-12.4062370893219,
113.068363256019)) ;
#176473 = CARTESIAN_POINT('Ctrl Pts',(-26.7395219022542,-12.4062370896233,
113.09259428659)) ;
#176474 = CARTESIAN_POINT('Ctrl Pts',(-26.6657180551848,-12.4062370899248,
113.11682531716)) ;
#176475 = CARTESIAN_POINT('Ctrl Pts',(-26.6664522906214,-12.3303669121692,
113.119061680059)) ;
#176476 = CARTESIAN_POINT('Ctrl Pts',(-26.6671865260579,-12.2544967344135,
113.121298042957)) ;
#176477 = CARTESIAN_POINT('Ctrl Pts',(-26.7409903731273,-12.2544967341121,
113.097067012386)) ;
#176478 = CARTESIAN_POINT('Ctrl Pts',(-26.8147942201966,-12.2544967338106,
113.072835981815)) ;
#176479 = CARTESIAN_POINT('Ctrl Pts',(-26.8140599847601,-12.3303669115662,
113.070599618917)) ;
#176480 = CARTESIAN_POINT('Ctrl Pts',(-26.7130188584353,-12.3620831181533,
112.798392930309)) ;
#176481 = CARTESIAN_POINT('Ctrl Pts',(-26.7186032170259,-12.4358532268962,
112.815401985444)) ;
#176482 = CARTESIAN_POINT('Ctrl Pts',(-26.6447993721143,-12.4358532286459,
112.839633022587)) ;
#176483 = CARTESIAN_POINT('Ctrl Pts',(-26.5709955272026,-12.4358532303956,
112.863864059729)) ;
#176484 = CARTESIAN_POINT('Ctrl Pts',(-26.565411168612,-12.3620831216526,
112.846855004594)) ;
#176485 = CARTESIAN_POINT('Ctrl Pts',(-26.5598268100214,-12.2883130129096,
112.829845949458)) ;
#176486 = CARTESIAN_POINT('Ctrl Pts',(-26.6336306549331,-12.28831301116,112.805614912316)) ;
#176487 = CARTESIAN_POINT('Ctrl Pts',(-26.7074344998447,-12.2883130094103,
112.781383875173)) ;
#176488 = CARTESIAN_POINT('Ctrl Pts',(-26.7130188584353,-12.3620831181533,
112.798392930309)) ;
#176489 = CARTESIAN_POINT('Ctrl Pts',(-26.6179903821788,-12.4697592102098,
112.544455169899)) ;
#176490 = CARTESIAN_POINT('Ctrl Pts',(-26.6294840061736,-12.536121336536,
112.579462894091)) ;
#176491 = CARTESIAN_POINT('Ctrl Pts',(-26.5556801627136,-12.5361213369903,
112.603693935654)) ;
#176492 = CARTESIAN_POINT('Ctrl Pts',(-26.4818763192536,-12.5361213374447,
112.627924977218)) ;
#176493 = CARTESIAN_POINT('Ctrl Pts',(-26.4703826952588,-12.4697592111185,
112.592917253027)) ;
#176494 = CARTESIAN_POINT('Ctrl Pts',(-26.458889071264,-12.4033970847922,
112.557909528835)) ;
#176495 = CARTESIAN_POINT('Ctrl Pts',(-26.532692914724,-12.4033970843379,
112.533678487271)) ;
#176496 = CARTESIAN_POINT('Ctrl Pts',(-26.6064967581841,-12.4033970838835,
112.509447445707)) ;
#176497 = CARTESIAN_POINT('Ctrl Pts',(-26.6179903821788,-12.4697592102098,
112.544455169899)) ;
#176498 = CARTESIAN_POINT('Ctrl Pts',(-26.5351639179177,-12.6447797711106,
112.32756700901)) ;
#176499 = CARTESIAN_POINT('Ctrl Pts',(-26.5517258863331,-12.6990195583039,
112.378012092584)) ;
#176500 = CARTESIAN_POINT('Ctrl Pts',(-26.4779220434683,-12.69901955683,112.40224313596)) ;
#176501 = CARTESIAN_POINT('Ctrl Pts',(-26.4041182006034,-12.6990195553562,
112.426474179337)) ;
#176502 = CARTESIAN_POINT('Ctrl Pts',(-26.3875562321881,-12.6447797681629,
112.376029095764)) ;
#176503 = CARTESIAN_POINT('Ctrl Pts',(-26.3709942637727,-12.5905399809696,
112.325584012191)) ;
#176504 = CARTESIAN_POINT('Ctrl Pts',(-26.4447981066375,-12.5905399824434,
112.301352968814)) ;
#176505 = CARTESIAN_POINT('Ctrl Pts',(-26.5186019495023,-12.5905399839173,
112.277121925437)) ;
#176506 = CARTESIAN_POINT('Ctrl Pts',(-26.5351639179177,-12.6447797711106,
112.32756700901)) ;
#176507 = CARTESIAN_POINT('Ctrl Pts',(-26.4692769172657,-12.8750273852739,
112.162297586987)) ;
#176508 = CARTESIAN_POINT('Ctrl Pts',(-26.4897314257756,-12.9132697898462,
112.224598719652)) ;
#176509 = CARTESIAN_POINT('Ctrl Pts',(-26.4159275829037,-12.9132697868245,
112.248829763007)) ;
#176510 = CARTESIAN_POINT('Ctrl Pts',(-26.3421237400317,-12.9132697838028,
112.273060806362)) ;
#176511 = CARTESIAN_POINT('Ctrl Pts',(-26.3216692315218,-12.8750273792305,
112.210759673697)) ;
#176512 = CARTESIAN_POINT('Ctrl Pts',(-26.3012147230119,-12.8367849746583,
112.148458541031)) ;
#176513 = CARTESIAN_POINT('Ctrl Pts',(-26.3750185658839,-12.8367849776799,
112.124227497676)) ;
#176514 = CARTESIAN_POINT('Ctrl Pts',(-26.4488224087558,-12.8367849807016,
112.099996454321)) ;
#176515 = CARTESIAN_POINT('Ctrl Pts',(-26.4692769172657,-12.8750273852739,
112.162297586987)) ;
#176516 = CARTESIAN_POINT('Ctrl Pts',(-26.4243077785298,-13.1453257818208,
112.060890975421)) ;
#176517 = CARTESIAN_POINT('Ctrl Pts',(-26.4471967824451,-13.1647498113274,
112.13060718826)) ;
#176518 = CARTESIAN_POINT('Ctrl Pts',(-26.3733929391465,-13.1647498092517,
112.154838230316)) ;
#176519 = CARTESIAN_POINT('Ctrl Pts',(-26.2995890958478,-13.164749807176,
112.179069272371)) ;
#176520 = CARTESIAN_POINT('Ctrl Pts',(-26.2767000919324,-13.1453257776693,
112.109353059532)) ;
#176521 = CARTESIAN_POINT('Ctrl Pts',(-26.2538110880171,-13.1259017481627,
112.039636846693)) ;
#176522 = CARTESIAN_POINT('Ctrl Pts',(-26.3276149313157,-13.1259017502384,
112.015405804637)) ;
#176523 = CARTESIAN_POINT('Ctrl Pts',(-26.4014187746144,-13.1259017523141,
111.991174762582)) ;
#176524 = CARTESIAN_POINT('Ctrl Pts',(-26.4243077785298,-13.1453257818208,
112.060890975421)) ;
#176525 = CARTESIAN_POINT('Ctrl Pts',(-26.403013785645,-13.4336234546741,
112.031393920208)) ;
#176526 = CARTESIAN_POINT('Ctrl Pts',(-26.4266913940733,-13.4329452228824,
112.103512095099)) ;
#176527 = CARTESIAN_POINT('Ctrl Pts',(-26.3528875505435,-13.4329452235498,
112.127743136451)) ;
#176528 = CARTESIAN_POINT('Ctrl Pts',(-26.2790837070136,-13.4329452242172,
112.151974177802)) ;
#176529 = CARTESIAN_POINT('Ctrl Pts',(-26.2554060985854,-13.433623456009,
112.07985600291)) ;
#176530 = CARTESIAN_POINT('Ctrl Pts',(-26.2317284901571,-13.4343016878008,
112.007737828018)) ;
#176531 = CARTESIAN_POINT('Ctrl Pts',(-26.3055323336869,-13.4343016871333,
111.983506786667)) ;
#176532 = CARTESIAN_POINT('Ctrl Pts',(-26.3793361772167,-13.4343016864659,
111.959275745316)) ;
#176533 = CARTESIAN_POINT('Ctrl Pts',(-26.403013785645,-13.4336234546741,
112.031393920208)) ;
#176534 = CARTESIAN_POINT('Ctrl Pts',(-26.4060165852795,-13.7229316022969,
112.076174503052)) ;
#176535 = CARTESIAN_POINT('Ctrl Pts',(-26.4287818404388,-13.7020508739217,
112.145513796983)) ;
#176536 = CARTESIAN_POINT('Ctrl Pts',(-26.3549779974329,-13.7020508801849,
112.16974483993)) ;
#176537 = CARTESIAN_POINT('Ctrl Pts',(-26.281174154427,-13.7020508864481,
112.193975882877)) ;
#176538 = CARTESIAN_POINT('Ctrl Pts',(-26.2584088992677,-13.7229316148234,
112.124636588946)) ;
#176539 = CARTESIAN_POINT('Ctrl Pts',(-26.2356436441084,-13.7438123431986,
112.055297295015)) ;
#176540 = CARTESIAN_POINT('Ctrl Pts',(-26.3094474871143,-13.7438123369354,
112.031066252067)) ;
#176541 = CARTESIAN_POINT('Ctrl Pts',(-26.3832513301202,-13.7438123306722,
112.00683520912)) ;
#176542 = CARTESIAN_POINT('Ctrl Pts',(-26.4060165852795,-13.7229316022969,
112.076174503052)) ;
#176543 = CARTESIAN_POINT('Ctrl Pts',(-26.4323125416507,-13.9881204584926,
112.191610815065)) ;
#176544 = CARTESIAN_POINT('Ctrl Pts',(-26.4525433595489,-13.948693047744,
112.253230621924)) ;
#176545 = CARTESIAN_POINT('Ctrl Pts',(-26.3787395179286,-13.9486930580491,
112.277461669092)) ;
#176546 = CARTESIAN_POINT('Ctrl Pts',(-26.3049356763083,-13.9486930683542,
112.301692716259)) ;
#176547 = CARTESIAN_POINT('Ctrl Pts',(-26.2847048584101,-13.9881204791028,
112.2400729094)) ;
#176548 = CARTESIAN_POINT('Ctrl Pts',(-26.2644740405119,-14.0275478898515,
112.17845310254)) ;
#176549 = CARTESIAN_POINT('Ctrl Pts',(-26.3382778821322,-14.0275478795464,
112.154222055372)) ;
#176550 = CARTESIAN_POINT('Ctrl Pts',(-26.4120817237525,-14.0275478692412,
112.129991008205)) ;
#176551 = CARTESIAN_POINT('Ctrl Pts',(-26.4323125416507,-13.9881204584926,
112.191610815065)) ;
#176552 = CARTESIAN_POINT('Ctrl Pts',(-26.4792881537362,-14.2135626266573,
112.370156392619)) ;
#176553 = CARTESIAN_POINT('Ctrl Pts',(-26.4955344715119,-14.1583369427659,
112.419640054866)) ;
#176554 = CARTESIAN_POINT('Ctrl Pts',(-26.4217306322404,-14.1583369561378,
112.443871109188)) ;
#176555 = CARTESIAN_POINT('Ctrl Pts',(-26.347926792969,-14.1583369695098,
112.468102163509)) ;
#176556 = CARTESIAN_POINT('Ctrl Pts',(-26.3316804751934,-14.2135626534012,
112.418618501262)) ;
#176557 = CARTESIAN_POINT('Ctrl Pts',(-26.3154341574177,-14.2687883372926,
112.369134839015)) ;
#176558 = CARTESIAN_POINT('Ctrl Pts',(-26.3892379966892,-14.2687883239207,
112.344903784693)) ;
#176559 = CARTESIAN_POINT('Ctrl Pts',(-26.4630418359606,-14.2687883105487,
112.320672730372)) ;
#176560 = CARTESIAN_POINT('Ctrl Pts',(-26.4792881537362,-14.2135626266573,
112.370156392619)) ;
#176561 = CARTESIAN_POINT('Ctrl Pts',(-26.5430286631922,-14.3820856851378,
112.599827193971)) ;
#176562 = CARTESIAN_POINT('Ctrl Pts',(-26.5541128714066,-14.3150132250762,
112.633587903234)) ;
#176563 = CARTESIAN_POINT('Ctrl Pts',(-26.4803090354461,-14.3150132383268,
112.65781896764)) ;
#176564 = CARTESIAN_POINT('Ctrl Pts',(-26.4065051994856,-14.3150132515775,
112.682050032046)) ;
#176565 = CARTESIAN_POINT('Ctrl Pts',(-26.3954209912713,-14.3820857116392,
112.648289322784)) ;
#176566 = CARTESIAN_POINT('Ctrl Pts',(-26.3843367830569,-14.4491581717009,
112.614528613521)) ;
#176567 = CARTESIAN_POINT('Ctrl Pts',(-26.4581406190174,-14.4491581584502,
112.590297549115)) ;
#176568 = CARTESIAN_POINT('Ctrl Pts',(-26.5319444549779,-14.4491581451995,
112.566066484708)) ;
#176569 = CARTESIAN_POINT('Ctrl Pts',(-26.5430286631922,-14.3820856851378,
112.599827193971)) ;
#176570 = CARTESIAN_POINT('Ctrl Pts',(-26.6176671822151,-14.4811007735871,
112.862516248575)) ;
#176571 = CARTESIAN_POINT('Ctrl Pts',(-26.6228245412953,-14.4070183383993,
112.878224731527)) ;
#176572 = CARTESIAN_POINT('Ctrl Pts',(-26.5490207083938,-14.4070183464706,
112.902455805251)) ;
#176573 = CARTESIAN_POINT('Ctrl Pts',(-26.4752168754924,-14.4070183545419,
112.926686878974)) ;
#176574 = CARTESIAN_POINT('Ctrl Pts',(-26.4700595164122,-14.4811007897297,
112.910978396022)) ;
#176575 = CARTESIAN_POINT('Ctrl Pts',(-26.464902157332,-14.5551832249176,
112.89526991307)) ;
#176576 = CARTESIAN_POINT('Ctrl Pts',(-26.5387059902335,-14.5551832168463,
112.871038839346)) ;
#176577 = CARTESIAN_POINT('Ctrl Pts',(-26.6125098231349,-14.555183208775,
112.846807765623)) ;
#176578 = CARTESIAN_POINT('Ctrl Pts',(-26.6176671822151,-14.4811007735871,
112.862516248575)) ;
#176579 = CARTESIAN_POINT('Ctrl Pts',(-26.6978612990312,-14.5043853087956,
113.142314338476)) ;
#176580 = CARTESIAN_POINT('Ctrl Pts',(-26.6966915575993,-14.4285698473868,
113.138751493961)) ;
#176581 = CARTESIAN_POINT('Ctrl Pts',(-26.622887727907,-14.4285698457663,
113.16298257746)) ;
#176582 = CARTESIAN_POINT('Ctrl Pts',(-26.5490838982148,-14.4285698441458,
113.187213660958)) ;
#176583 = CARTESIAN_POINT('Ctrl Pts',(-26.5502536396466,-14.5043853055546,
113.190776505473)) ;
#176584 = CARTESIAN_POINT('Ctrl Pts',(-26.5514233810785,-14.5802007669634,
113.194339349988)) ;
#176585 = CARTESIAN_POINT('Ctrl Pts',(-26.6252272107708,-14.5802007685839,
113.17010826649)) ;
#176586 = CARTESIAN_POINT('Ctrl Pts',(-26.6990310404631,-14.5802007702044,
113.145877182991)) ;
#176587 = CARTESIAN_POINT('Ctrl Pts',(-26.6978612990312,-14.5043853087956,
113.142314338476)) ;
#176588 = CARTESIAN_POINT('Ctrl Pts',(-26.7765022627845,-14.4497319209782,
113.417276345146)) ;
#176589 = CARTESIAN_POINT('Ctrl Pts',(-26.769106971723,-14.3776228604659,
113.394751480785)) ;
#176590 = CARTESIAN_POINT('Ctrl Pts',(-26.6953031438992,-14.3776228445383,
113.418982569975)) ;
#176591 = CARTESIAN_POINT('Ctrl Pts',(-26.6214993160755,-14.3776228286107,
113.443213659164)) ;
#176592 = CARTESIAN_POINT('Ctrl Pts',(-26.628894607137,-14.449731889123,113.465738523525)) ;
#176593 = CARTESIAN_POINT('Ctrl Pts',(-26.6362898981985,-14.5218409496353,
113.488263387886)) ;
#176594 = CARTESIAN_POINT('Ctrl Pts',(-26.7100937260223,-14.5218409655629,
113.464032298697)) ;
#176595 = CARTESIAN_POINT('Ctrl Pts',(-26.7838975538461,-14.5218409814906,
113.439801209507)) ;
#176596 = CARTESIAN_POINT('Ctrl Pts',(-26.7765022627845,-14.4497319209782,
113.417276345146)) ;
#176597 = CARTESIAN_POINT('Ctrl Pts',(-26.8476800485963,-14.3208489038209,
113.669628788919)) ;
#176598 = CARTESIAN_POINT('Ctrl Pts',(-26.83456878888,-14.25763373208,113.62969400612)) ;
#176599 = CARTESIAN_POINT('Ctrl Pts',(-26.7607649616458,-14.2576336982123,
113.653925097105)) ;
#176600 = CARTESIAN_POINT('Ctrl Pts',(-26.6869611344116,-14.2576336643446,
113.67815618809)) ;
#176601 = CARTESIAN_POINT('Ctrl Pts',(-26.700072394128,-14.3208488360855,
113.718090970889)) ;
#176602 = CARTESIAN_POINT('Ctrl Pts',(-26.7131836538443,-14.3840640078265,
113.758025753688)) ;
#176603 = CARTESIAN_POINT('Ctrl Pts',(-26.7869874810785,-14.3840640416942,
113.733794662703)) ;
#176604 = CARTESIAN_POINT('Ctrl Pts',(-26.8607913083127,-14.3840640755619,
113.709563571718)) ;
#176605 = CARTESIAN_POINT('Ctrl Pts',(-26.8476800485963,-14.3208489038209,
113.669628788919)) ;
#176606 = CARTESIAN_POINT('Ctrl Pts',(-26.9051290746846,-14.1269083086763,
113.880141966721)) ;
#176607 = CARTESIAN_POINT('Ctrl Pts',(-26.8872525909099,-14.0771420046429,
113.825693080136)) ;
#176608 = CARTESIAN_POINT('Ctrl Pts',(-26.8134487620136,-14.0771419513953,
113.849924166059)) ;
#176609 = CARTESIAN_POINT('Ctrl Pts',(-26.7396449331174,-14.0771418981477,
113.874155251982)) ;
#176610 = CARTESIAN_POINT('Ctrl Pts',(-26.7575214168921,-14.1269082021811,
113.928604138566)) ;
#176611 = CARTESIAN_POINT('Ctrl Pts',(-26.7753979006668,-14.1766745062146,
113.983053025151)) ;
#176612 = CARTESIAN_POINT('Ctrl Pts',(-26.8492017295631,-14.1766745594622,
113.958821939228)) ;
#176613 = CARTESIAN_POINT('Ctrl Pts',(-26.9230055584593,-14.1766746127098,
113.934590853305)) ;
#176614 = CARTESIAN_POINT('Ctrl Pts',(-26.9051290746846,-14.1269083086763,
113.880141966721)) ;
#176615 = CARTESIAN_POINT('Ctrl Pts',(-26.9439250946234,-13.8839530008224,
114.033597139485)) ;
#176616 = CARTESIAN_POINT('Ctrl Pts',(-26.9225840143864,-13.8510774674815,
113.968595650967)) ;
#176617 = CARTESIAN_POINT('Ctrl Pts',(-26.8487801814222,-13.8510773982051,
113.992826724499)) ;
#176618 = CARTESIAN_POINT('Ctrl Pts',(-26.774976348458,-13.8510773289287,
114.017057798032)) ;
#176619 = CARTESIAN_POINT('Ctrl Pts',(-26.7963174286951,-13.8839528622696,
114.08205928655)) ;
#176620 = CARTESIAN_POINT('Ctrl Pts',(-26.8176585089322,-13.9168283956105,
114.147060775069)) ;
#176621 = CARTESIAN_POINT('Ctrl Pts',(-26.8914623418963,-13.9168284648869,
114.122829701536)) ;
#176622 = CARTESIAN_POINT('Ctrl Pts',(-26.9652661748605,-13.9168285341632,
114.098598628004)) ;
#176623 = CARTESIAN_POINT('Ctrl Pts',(-26.9439250946234,-13.8839530008224,
114.033597139485)) ;
#176624 = CARTESIAN_POINT('Ctrl Pts',(-26.9610011688202,-13.6058131007772,
114.121164169516)) ;
#176625 = CARTESIAN_POINT('Ctrl Pts',(-26.9377011273381,-13.592308546656,
114.05019600097)) ;
#176626 = CARTESIAN_POINT('Ctrl Pts',(-26.863897288672,-13.5923084632408,
114.074427057136)) ;
#176627 = CARTESIAN_POINT('Ctrl Pts',(-26.790093450006,-13.5923083798256,
114.098658113301)) ;
#176628 = CARTESIAN_POINT('Ctrl Pts',(-26.8133934914881,-13.6058129339469,
114.169626281847)) ;
#176629 = CARTESIAN_POINT('Ctrl Pts',(-26.8366935329702,-13.6193174880682,
114.240594450393)) ;
#176630 = CARTESIAN_POINT('Ctrl Pts',(-26.9104973716362,-13.6193175714834,
114.216363394227)) ;
#176631 = CARTESIAN_POINT('Ctrl Pts',(-26.9843012103023,-13.6193176548985,
114.192132338062)) ;
#176632 = CARTESIAN_POINT('Ctrl Pts',(-26.9610011688202,-13.6058131007772,
114.121164169516)) ;
#176633 = CARTESIAN_POINT('Ctrl Pts',(-26.9541142012214,-13.3154623494247,
114.135571911121)) ;
#176634 = CARTESIAN_POINT('Ctrl Pts',(-26.9305290130074,-13.3222095128514,
114.063735231526)) ;
#176635 = CARTESIAN_POINT('Ctrl Pts',(-26.8567251670928,-13.3222094225439,
114.087966265613)) ;
#176636 = CARTESIAN_POINT('Ctrl Pts',(-26.7829213211782,-13.3222093322365,
114.112197299701)) ;
#176637 = CARTESIAN_POINT('Ctrl Pts',(-26.8065065093922,-13.3154621688099,
114.184033979296)) ;
#176638 = CARTESIAN_POINT('Ctrl Pts',(-26.8300916976061,-13.3087150053832,
114.255870658891)) ;
#176639 = CARTESIAN_POINT('Ctrl Pts',(-26.9038955435208,-13.3087150956907,
114.231639624804)) ;
#176640 = CARTESIAN_POINT('Ctrl Pts',(-26.9776993894353,-13.3087151859981,
114.207408590716)) ;
#176641 = CARTESIAN_POINT('Ctrl Pts',(-26.9541142012214,-13.3154623494247,
114.135571911121)) ;
#176642 = CARTESIAN_POINT('Ctrl Pts',(-26.9227927789619,-13.0305252756843,
114.075814770893)) ;
#176643 = CARTESIAN_POINT('Ctrl Pts',(-26.9006222531828,-13.057175468413,
114.008286924693)) ;
#176644 = CARTESIAN_POINT('Ctrl Pts',(-26.8268183990987,-13.0571753774731,
114.032517933897)) ;
#176645 = CARTESIAN_POINT('Ctrl Pts',(-26.7530145450145,-13.0571752865332,
114.056748943102)) ;
#176646 = CARTESIAN_POINT('Ctrl Pts',(-26.7751850707936,-13.0305250938045,
114.124276789302)) ;
#176647 = CARTESIAN_POINT('Ctrl Pts',(-26.7973555965728,-13.0038749010759,
114.191804635502)) ;
#176648 = CARTESIAN_POINT('Ctrl Pts',(-26.8711594506569,-13.0038749920158,
114.167573626298)) ;
#176649 = CARTESIAN_POINT('Ctrl Pts',(-26.944963304741,-13.0038750829557,
114.143342617093)) ;
#176650 = CARTESIAN_POINT('Ctrl Pts',(-26.9227927789619,-13.0305252756843,
114.075814770893)) ;
#176651 = CARTESIAN_POINT('Ctrl Pts',(-26.8691774398986,-12.7760411077928,
113.947787130553)) ;
#176652 = CARTESIAN_POINT('Ctrl Pts',(-26.8499879959769,-12.8204973460342,
113.889339178628)) ;
#176653 = CARTESIAN_POINT('Ctrl Pts',(-26.7761841340996,-12.8204972646132,
113.913570164095)) ;
#176654 = CARTESIAN_POINT('Ctrl Pts',(-26.7023802722222,-12.8204971831922,
113.937801149563)) ;
#176655 = CARTESIAN_POINT('Ctrl Pts',(-26.721569716144,-12.7760409449508,
113.996249101488)) ;
#176656 = CARTESIAN_POINT('Ctrl Pts',(-26.7407591600657,-12.7315847067095,
114.054697053414)) ;
#176657 = CARTESIAN_POINT('Ctrl Pts',(-26.814563021943,-12.7315847881305,
114.030466067947)) ;
#176658 = CARTESIAN_POINT('Ctrl Pts',(-26.8883668838204,-12.7315848695515,
114.006235082479)) ;
#176659 = CARTESIAN_POINT('Ctrl Pts',(-26.8691774398986,-12.7760411077928,
113.947787130553)) ;
#176660 = CARTESIAN_POINT('Ctrl Pts',(-26.7957043233195,-12.5658693797106,
113.759493744326)) ;
#176661 = CARTESIAN_POINT('Ctrl Pts',(-26.7808818986988,-12.6250641545161,
113.714347028503)) ;
#176662 = CARTESIAN_POINT('Ctrl Pts',(-26.7070780298316,-12.6250640894152,
113.73857799268)) ;
#176663 = CARTESIAN_POINT('Ctrl Pts',(-26.6332741609643,-12.6250640243143,
113.762808956858)) ;
#176664 = CARTESIAN_POINT('Ctrl Pts',(-26.6480965855851,-12.5658692495088,
113.807955672681)) ;
#176665 = CARTESIAN_POINT('Ctrl Pts',(-26.6629190102057,-12.5066744747032,
113.853102388504)) ;
#176666 = CARTESIAN_POINT('Ctrl Pts',(-26.736722879073,-12.5066745398042,
113.828871424327)) ;
#176667 = CARTESIAN_POINT('Ctrl Pts',(-26.8105267479402,-12.506674604905,
113.804640460149)) ;
#176668 = CARTESIAN_POINT('Ctrl Pts',(-26.7957043233195,-12.5658693797106,
113.759493744326)) ;
#176669 = CARTESIAN_POINT('Ctrl Pts',(-26.7071990036801,-12.4170609140262,
113.52535902764)) ;
#176670 = CARTESIAN_POINT('Ctrl Pts',(-26.6978006274313,-12.4867319202062,
113.496733087944)) ;
#176671 = CARTESIAN_POINT('Ctrl Pts',(-26.6239967533843,-12.4867318782286,
113.520964036345)) ;
#176672 = CARTESIAN_POINT('Ctrl Pts',(-26.5501928793373,-12.4867318362511,
113.545194984746)) ;
#176673 = CARTESIAN_POINT('Ctrl Pts',(-26.5595912555861,-12.4170608300712,
113.573820924441)) ;
#176674 = CARTESIAN_POINT('Ctrl Pts',(-26.5689896318348,-12.3473898238912,
113.602446864137)) ;
#176675 = CARTESIAN_POINT('Ctrl Pts',(-26.6427935058819,-12.3473898658687,
113.578215915736)) ;
#176676 = CARTESIAN_POINT('Ctrl Pts',(-26.7165973799289,-12.3473899078463,
113.553984967335)) ;
#176677 = CARTESIAN_POINT('Ctrl Pts',(-26.7071990036801,-12.4170609140262,
113.52535902764)) ;
#176678 = CARTESIAN_POINT('Ctrl Pts',(-26.6088521342578,-12.3396249333132,
113.261367652909)) ;
#176679 = CARTESIAN_POINT('Ctrl Pts',(-26.6055702780408,-12.4148052434578,
113.251371646305)) ;
#176680 = CARTESIAN_POINT('Ctrl Pts',(-26.5317664011453,-12.4148052290128,
113.275602586029)) ;
#176681 = CARTESIAN_POINT('Ctrl Pts',(-26.4579625242497,-12.4148052145678,
113.299833525754)) ;
#176682 = CARTESIAN_POINT('Ctrl Pts',(-26.4612443804668,-12.3396249044232,
113.309829532358)) ;
#176683 = CARTESIAN_POINT('Ctrl Pts',(-26.4645262366838,-12.2644445942785,
113.319825538963)) ;
#176684 = CARTESIAN_POINT('Ctrl Pts',(-26.5383301135793,-12.2644446087235,
113.295594599239)) ;
#176685 = CARTESIAN_POINT('Ctrl Pts',(-26.6121339904748,-12.2644446231686,
113.271363659514)) ;
#176686 = CARTESIAN_POINT('Ctrl Pts',(-26.6088521342578,-12.3396249333132,
113.261367652909)) ;
#176687 = CARTESIAN_POINT('Ctrl Pts',(-26.5073352253782,-12.340046412335,
112.987690769148)) ;
#176688 = CARTESIAN_POINT('Ctrl Pts',(-26.5104009195119,-12.4153088432885,
112.997028376739)) ;
#176689 = CARTESIAN_POINT('Ctrl Pts',(-26.4365970426382,-12.4153088579802,
113.02125931653)) ;
#176690 = CARTESIAN_POINT('Ctrl Pts',(-26.3627931657646,-12.4153088726718,
113.045490256321)) ;
#176691 = CARTESIAN_POINT('Ctrl Pts',(-26.3597274716308,-12.3400464417183,
113.03615264873)) ;
#176692 = CARTESIAN_POINT('Ctrl Pts',(-26.3566617774971,-12.2647840107648,
113.02681504114)) ;
#176693 = CARTESIAN_POINT('Ctrl Pts',(-26.4304656543708,-12.2647839960732,
113.002584101349)) ;
#176694 = CARTESIAN_POINT('Ctrl Pts',(-26.5042695312444,-12.2647839813815,
112.978353161558)) ;
#176695 = CARTESIAN_POINT('Ctrl Pts',(-26.5073352253782,-12.340046412335,
112.987690769148)) ;
#176696 = CARTESIAN_POINT('Ctrl Pts',(-26.4097025231263,-12.4170460254182,
112.725620310096)) ;
#176697 = CARTESIAN_POINT('Ctrl Pts',(-26.4188586939777,-12.4870438442232,
112.753508527089)) ;
#176698 = CARTESIAN_POINT('Ctrl Pts',(-26.3450548197485,-12.487043886487,
112.777739474935)) ;
#176699 = CARTESIAN_POINT('Ctrl Pts',(-26.2712509455193,-12.4870439287509,
112.801970422781)) ;
#176700 = CARTESIAN_POINT('Ctrl Pts',(-26.2620947746679,-12.4170461099459,
112.774082205787)) ;
#176701 = CARTESIAN_POINT('Ctrl Pts',(-26.2529386038164,-12.3470482911409,
112.746193988793)) ;
#176702 = CARTESIAN_POINT('Ctrl Pts',(-26.3267424780456,-12.3470482488771,
112.721963040948)) ;
#176703 = CARTESIAN_POINT('Ctrl Pts',(-26.4005463522748,-12.3470482066133,
112.697732093102)) ;
#176704 = CARTESIAN_POINT('Ctrl Pts',(-26.4097025231263,-12.4170460254182,
112.725620310096)) ;
#176705 = CARTESIAN_POINT('Ctrl Pts',(-26.3209819060534,-12.5662136094611,
112.490921752616)) ;
#176706 = CARTESIAN_POINT('Ctrl Pts',(-26.3356107191864,-12.625901534808,
112.535478755034)) ;
#176707 = CARTESIAN_POINT('Ctrl Pts',(-26.2618068501208,-12.6259016005162,
112.559709718608)) ;
#176708 = CARTESIAN_POINT('Ctrl Pts',(-26.1880029810553,-12.6259016662244,
112.583940682181)) ;
#176709 = CARTESIAN_POINT('Ctrl Pts',(-26.1733741679223,-12.5662137408776,
112.539383679763)) ;
#176710 = CARTESIAN_POINT('Ctrl Pts',(-26.1587453547893,-12.5065258155307,
112.494826677344)) ;
#176711 = CARTESIAN_POINT('Ctrl Pts',(-26.2325492238549,-12.5065257498225,
112.470595713771)) ;
#176712 = CARTESIAN_POINT('Ctrl Pts',(-26.3063530929204,-12.5065256841143,
112.446364750198)) ;
#176713 = CARTESIAN_POINT('Ctrl Pts',(-26.3209819060534,-12.5662136094611,
112.490921752616)) ;
#176714 = CARTESIAN_POINT('Ctrl Pts',(-26.2476333327786,-12.7760199991739,
112.30293791623)) ;
#176715 = CARTESIAN_POINT('Ctrl Pts',(-26.2666719877246,-12.8211489416697,
112.360926585345)) ;
#176716 = CARTESIAN_POINT('Ctrl Pts',(-26.1928681256039,-12.8211490243987,
112.385157570071)) ;
#176717 = CARTESIAN_POINT('Ctrl Pts',(-26.1190642634831,-12.8211491071278,
112.409388554798)) ;
#176718 = CARTESIAN_POINT('Ctrl Pts',(-26.1000256085371,-12.776020164632,
112.351399885683)) ;
#176719 = CARTESIAN_POINT('Ctrl Pts',(-26.0809869535911,-12.7308912221363,
112.293411216568)) ;
#176720 = CARTESIAN_POINT('Ctrl Pts',(-26.1547908157119,-12.7308911394072,
112.269180231842)) ;
#176721 = CARTESIAN_POINT('Ctrl Pts',(-26.2285946778326,-12.7308910566782,
112.244949247116)) ;
#176722 = CARTESIAN_POINT('Ctrl Pts',(-26.2476333327786,-12.7760199991739,
112.30293791623)) ;
#176723 = CARTESIAN_POINT('Ctrl Pts',(-26.1937928662736,-13.0322696653641,
112.174451982578)) ;
#176724 = CARTESIAN_POINT('Ctrl Pts',(-26.2158844526486,-13.0595756323769,
112.241739388323)) ;
#176725 = CARTESIAN_POINT('Ctrl Pts',(-26.1420805985489,-13.059575723918,
112.26597039748)) ;
#176726 = CARTESIAN_POINT('Ctrl Pts',(-26.0682767444492,-13.0595758154591,
112.290201406637)) ;
#176727 = CARTESIAN_POINT('Ctrl Pts',(-26.0461851580742,-13.0322698484462,
112.222914000892)) ;
#176728 = CARTESIAN_POINT('Ctrl Pts',(-26.0240935716991,-13.0049638814334,
112.155626595147)) ;
#176729 = CARTESIAN_POINT('Ctrl Pts',(-26.0978974257988,-13.0049637898923,
112.13139558599)) ;
#176730 = CARTESIAN_POINT('Ctrl Pts',(-26.1717012798985,-13.0049636983512,
112.107164576833)) ;
#176731 = CARTESIAN_POINT('Ctrl Pts',(-26.1937928662736,-13.0322696653641,
112.174451982578)) ;
#176732 = CARTESIAN_POINT('Ctrl Pts',(-26.1627547455184,-13.3151090323585,
112.115281050215)) ;
#176733 = CARTESIAN_POINT('Ctrl Pts',(-26.186314657556,-13.3227086607463,
112.187040739103)) ;
#176734 = CARTESIAN_POINT('Ctrl Pts',(-26.1125108115818,-13.3227087535366,
112.211271773009)) ;
#176735 = CARTESIAN_POINT('Ctrl Pts',(-26.0387069656076,-13.3227088463268,
112.235502806915)) ;
#176736 = CARTESIAN_POINT('Ctrl Pts',(-26.0151470535699,-13.315109217939,
112.163743118026)) ;
#176737 = CARTESIAN_POINT('Ctrl Pts',(-25.9915871415323,-13.3075095895512,
112.091983429138)) ;
#176738 = CARTESIAN_POINT('Ctrl Pts',(-26.0653909875065,-13.307509496761,
112.067752395232)) ;
#176739 = CARTESIAN_POINT('Ctrl Pts',(-26.1391948334808,-13.3075094039707,
112.043521361326)) ;
#176740 = CARTESIAN_POINT('Ctrl Pts',(-26.1627547455184,-13.3151090323585,
112.115281050215)) ;
#176741 = CARTESIAN_POINT('Ctrl Pts',(-26.1558631196965,-13.6075492018493,
112.129940953347)) ;
#176742 = CARTESIAN_POINT('Ctrl Pts',(-26.1792021826536,-13.5947427678056,
112.201027971714)) ;
#176743 = CARTESIAN_POINT('Ctrl Pts',(-26.1053983440989,-13.5947428521219,
112.225259028218)) ;
#176744 = CARTESIAN_POINT('Ctrl Pts',(-26.0315945055442,-13.594742936438,
112.249490084723)) ;
#176745 = CARTESIAN_POINT('Ctrl Pts',(-26.0082554425871,-13.6075493704817,
112.178403066356)) ;
#176746 = CARTESIAN_POINT('Ctrl Pts',(-25.98491637963,-13.6203558045254,112.107316047989)) ;
#176747 = CARTESIAN_POINT('Ctrl Pts',(-26.0587202181847,-13.6203557202092,
112.083084991485)) ;
#176748 = CARTESIAN_POINT('Ctrl Pts',(-26.1325240567394,-13.620355635893,
112.05885393498)) ;
#176749 = CARTESIAN_POINT('Ctrl Pts',(-26.1558631196965,-13.6075492018493,
112.129940953347)) ;
#176750 = CARTESIAN_POINT('Ctrl Pts',(-26.1729300005076,-13.8839937911961,
112.217263774275)) ;
#176751 = CARTESIAN_POINT('Ctrl Pts',(-26.1943813283139,-13.8518669319433,
112.282601056074)) ;
#176752 = CARTESIAN_POINT('Ctrl Pts',(-26.1205774957318,-13.8518670036745,
112.30683213077)) ;
#176753 = CARTESIAN_POINT('Ctrl Pts',(-26.0467736631496,-13.8518670754058,
112.331063205466)) ;
#176754 = CARTESIAN_POINT('Ctrl Pts',(-26.0253223353433,-13.8839939346586,
112.265725923668)) ;
#176755 = CARTESIAN_POINT('Ctrl Pts',(-26.003871007537,-13.9161207939113,
112.200388641869)) ;
#176756 = CARTESIAN_POINT('Ctrl Pts',(-26.0776748401191,-13.9161207221801,
112.176157567173)) ;
#176757 = CARTESIAN_POINT('Ctrl Pts',(-26.1514786727013,-13.9161206504489,
112.151926492477)) ;
#176758 = CARTESIAN_POINT('Ctrl Pts',(-26.1729300005076,-13.8839937911961,
112.217263774275)) ;
#176759 = CARTESIAN_POINT('Ctrl Pts',(-26.2120071941306,-14.1283418739825,
112.371799593747)) ;
#176760 = CARTESIAN_POINT('Ctrl Pts',(-26.2300278122176,-14.0791061363548,
112.426687487438)) ;
#176761 = CARTESIAN_POINT('Ctrl Pts',(-26.1562239835833,-14.079106190233,
112.450918574159)) ;
#176762 = CARTESIAN_POINT('Ctrl Pts',(-26.082420154949,-14.0791062441112,
112.475149660879)) ;
#176763 = CARTESIAN_POINT('Ctrl Pts',(-26.064399536862,-14.1283419817388,
112.420261767188)) ;
#176764 = CARTESIAN_POINT('Ctrl Pts',(-26.046378918775,-14.1775777193664,
112.365373873497)) ;
#176765 = CARTESIAN_POINT('Ctrl Pts',(-26.1201827474093,-14.1775776654883,
112.341142786777)) ;
#176766 = CARTESIAN_POINT('Ctrl Pts',(-26.1939865760436,-14.1775776116101,
112.316911700056)) ;
#176767 = CARTESIAN_POINT('Ctrl Pts',(-26.2120071941306,-14.1283418739825,
112.371799593747)) ;
#176768 = CARTESIAN_POINT('Ctrl Pts',(-26.2693072989749,-14.321085337762,
112.58170002845)) ;
#176769 = CARTESIAN_POINT('Ctrl Pts',(-26.2826224774496,-14.2583178356259,
112.622255912442)) ;
#176770 = CARTESIAN_POINT('Ctrl Pts',(-26.2088186508594,-14.2583178709165,
112.646487005389)) ;
#176771 = CARTESIAN_POINT('Ctrl Pts',(-26.1350148242692,-14.2583179062071,
112.670718098336)) ;
#176772 = CARTESIAN_POINT('Ctrl Pts',(-26.1216996457945,-14.3210854083432,
112.630162214343)) ;
#176773 = CARTESIAN_POINT('Ctrl Pts',(-26.1083844673198,-14.3838529104793,
112.589606330351)) ;
#176774 = CARTESIAN_POINT('Ctrl Pts',(-26.18218829391,-14.3838528751887,112.565375237404)) ;
#176775 = CARTESIAN_POINT('Ctrl Pts',(-26.2559921205002,-14.3838528398981,
112.541144144458)) ;
#176776 = CARTESIAN_POINT('Ctrl Pts',(-26.2693072989749,-14.321085337762,
112.58170002845)) ;
#176777 = CARTESIAN_POINT('Ctrl Pts',(-26.3405926471782,-14.4501544762085,
112.834435287317)) ;
#176778 = CARTESIAN_POINT('Ctrl Pts',(-26.3482140059273,-14.3782797175252,
112.857648715311)) ;
#176779 = CARTESIAN_POINT('Ctrl Pts',(-26.274410178748,-14.378279733915,112.881879806463)) ;
#176780 = CARTESIAN_POINT('Ctrl Pts',(-26.2006063515687,-14.3782797503047,
112.906110897615)) ;
#176781 = CARTESIAN_POINT('Ctrl Pts',(-26.1929849928196,-14.450154508988,
112.882897469621)) ;
#176782 = CARTESIAN_POINT('Ctrl Pts',(-26.1853636340705,-14.5220292676713,
112.859684041627)) ;
#176783 = CARTESIAN_POINT('Ctrl Pts',(-26.2591674612498,-14.5220292512815,
112.835452950475)) ;
#176784 = CARTESIAN_POINT('Ctrl Pts',(-26.3329712884291,-14.5220292348918,
112.811221859322)) ;
#176785 = CARTESIAN_POINT('Ctrl Pts',(-26.3405926471782,-14.4501544762085,
112.834435287317)) ;
#176786 = CARTESIAN_POINT('Ctrl Pts',(-26.4193828840965,-14.504350239421,
113.109906480253)) ;
#176787 = CARTESIAN_POINT('Ctrl Pts',(-26.4207801489466,-14.4285822954382,
113.114162322657)) ;
#176788 = CARTESIAN_POINT('Ctrl Pts',(-26.346976319745,-14.4285822971821,
113.13839340765)) ;
#176789 = CARTESIAN_POINT('Ctrl Pts',(-26.2731724905434,-14.4285822989259,
113.162624492643)) ;
#176790 = CARTESIAN_POINT('Ctrl Pts',(-26.2717752256934,-14.5043502429086,
113.158368650239)) ;
#176791 = CARTESIAN_POINT('Ctrl Pts',(-26.2703779608434,-14.5801181868914,
113.154112807834)) ;
#176792 = CARTESIAN_POINT('Ctrl Pts',(-26.3441817900449,-14.5801181851475,
113.129881722841)) ;
#176793 = CARTESIAN_POINT('Ctrl Pts',(-26.4179856192465,-14.5801181834037,
113.105650637849)) ;
#176794 = CARTESIAN_POINT('Ctrl Pts',(-26.4193828840965,-14.504350239421,
113.109906480253)) ;
#176795 = CARTESIAN_POINT('Ctrl Pts',(-26.4990873137165,-14.4811635345991,
113.387994186648)) ;
#176796 = CARTESIAN_POINT('Ctrl Pts',(-26.4941906716139,-14.4069000332384,
113.373079804133)) ;
#176797 = CARTESIAN_POINT('Ctrl Pts',(-26.4203868398276,-14.4069000243761,
113.397310881253)) ;
#176798 = CARTESIAN_POINT('Ctrl Pts',(-26.3465830080412,-14.4069000155138,
113.421541958373)) ;
#176799 = CARTESIAN_POINT('Ctrl Pts',(-26.3514796501438,-14.4811635168746,
113.436456340888)) ;
#176800 = CARTESIAN_POINT('Ctrl Pts',(-26.3563762922464,-14.5554270182353,
113.451370723402)) ;
#176801 = CARTESIAN_POINT('Ctrl Pts',(-26.4301801240328,-14.5554270270976,
113.427139646282)) ;
#176802 = CARTESIAN_POINT('Ctrl Pts',(-26.5039839558191,-14.5554270359599,
113.402908569162)) ;
#176803 = CARTESIAN_POINT('Ctrl Pts',(-26.4990873137165,-14.4811635345991,
113.387994186648)) ;
#176804 = CARTESIAN_POINT('Ctrl Pts',(-26.5741035318335,-14.3816036851556,
113.652018746242)) ;
#176805 = CARTESIAN_POINT('Ctrl Pts',(-26.5632261840353,-14.3141789361096,
113.61888809934)) ;
#176806 = CARTESIAN_POINT('Ctrl Pts',(-26.4894223485548,-14.3141789218921,
113.643119165208)) ;
#176807 = CARTESIAN_POINT('Ctrl Pts',(-26.4156185130744,-14.3141789076745,
113.667350231076)) ;
#176808 = CARTESIAN_POINT('Ctrl Pts',(-26.4264958608725,-14.3816036567204,
113.700480877978)) ;
#176809 = CARTESIAN_POINT('Ctrl Pts',(-26.4373732086707,-14.4490284057664,
113.73361152488)) ;
#176810 = CARTESIAN_POINT('Ctrl Pts',(-26.5111770441512,-14.449028419984,
113.709380459012)) ;
#176811 = CARTESIAN_POINT('Ctrl Pts',(-26.5849808796317,-14.4490284342016,
113.685149393144)) ;
#176812 = CARTESIAN_POINT('Ctrl Pts',(-26.5741035318335,-14.3816036851556,
113.652018746242)) ;
#176813 = CARTESIAN_POINT('Ctrl Pts',(-26.6376352371572,-14.2132115910195,
113.88096634118)) ;
#176814 = CARTESIAN_POINT('Ctrl Pts',(-26.6215719998171,-14.1574425718006,
113.832040311625)) ;
#176815 = CARTESIAN_POINT('Ctrl Pts',(-26.5477681610995,-14.1574425567691,
113.856271367634)) ;
#176816 = CARTESIAN_POINT('Ctrl Pts',(-26.4739643223819,-14.1574425417376,
113.880502423642)) ;
#176817 = CARTESIAN_POINT('Ctrl Pts',(-26.490027559722,-14.2132115609565,
113.929428453197)) ;
#176818 = CARTESIAN_POINT('Ctrl Pts',(-26.5060907970621,-14.2689805801753,
113.978354482753)) ;
#176819 = CARTESIAN_POINT('Ctrl Pts',(-26.5798946357797,-14.2689805952068,
113.954123426744)) ;
#176820 = CARTESIAN_POINT('Ctrl Pts',(-26.6536984744973,-14.2689806102383,
113.929892370735)) ;
#176821 = CARTESIAN_POINT('Ctrl Pts',(-26.6376352371572,-14.2132115910195,
113.88096634118)) ;
#176822 = CARTESIAN_POINT('Ctrl Pts',(-26.6847308687247,-13.9871283531687,
114.059972839669)) ;
#176823 = CARTESIAN_POINT('Ctrl Pts',(-26.6646189109287,-13.9470611393289,
113.998715061021)) ;
#176824 = CARTESIAN_POINT('Ctrl Pts',(-26.5908150694804,-13.9470611278095,
114.022946108712)) ;
#176825 = CARTESIAN_POINT('Ctrl Pts',(-26.5170112280321,-13.9470611162902,
114.047177156404)) ;
#176826 = CARTESIAN_POINT('Ctrl Pts',(-26.5371231858281,-13.98712833013,114.108434935051)) ;
#176827 = CARTESIAN_POINT('Ctrl Pts',(-26.5572351436241,-14.0271955439699,
114.169692713699)) ;
#176828 = CARTESIAN_POINT('Ctrl Pts',(-26.6310389850724,-14.0271955554892,
114.145461666007)) ;
#176829 = CARTESIAN_POINT('Ctrl Pts',(-26.7048428265207,-14.0271955670085,
114.121230618316)) ;
#176830 = CARTESIAN_POINT('Ctrl Pts',(-26.6847308687247,-13.9871283531687,
114.059972839669)) ;
#176831 = CARTESIAN_POINT('Ctrl Pts',(-26.7108828323385,-13.7209751384546,
114.175063486759)) ;
#176832 = CARTESIAN_POINT('Ctrl Pts',(-26.6881811765791,-13.6994320003675,
114.105917906077)) ;
#176833 = CARTESIAN_POINT('Ctrl Pts',(-26.6143773336532,-13.6994319934453,
114.130148949268)) ;
#176834 = CARTESIAN_POINT('Ctrl Pts',(-26.5405734907274,-13.699431986523,
114.154379992459)) ;
#176835 = CARTESIAN_POINT('Ctrl Pts',(-26.5632751464868,-13.72097512461,114.223525573141)) ;
#176836 = CARTESIAN_POINT('Ctrl Pts',(-26.5859768022463,-13.7425182626971,
114.292671153823)) ;
#176837 = CARTESIAN_POINT('Ctrl Pts',(-26.6597806451721,-13.7425182696194,
114.268440110632)) ;
#176838 = CARTESIAN_POINT('Ctrl Pts',(-26.733584488098,-13.7425182765416,
114.244209067441)) ;
#176839 = CARTESIAN_POINT('Ctrl Pts',(-26.7108828323385,-13.7209751384546,
114.175063486759)) ;
#176840 = CARTESIAN_POINT('Ctrl Pts',(-26.7138425852466,-13.4341833204507,
114.21939759733)) ;
#176841 = CARTESIAN_POINT('Ctrl Pts',(-26.6901693704343,-13.4326332891495,
114.14729280462)) ;
#176842 = CARTESIAN_POINT('Ctrl Pts',(-26.6163655269116,-13.4326332865185,
114.171523845993)) ;
#176843 = CARTESIAN_POINT('Ctrl Pts',(-26.5425616833888,-13.4326332838874,
114.195754887366)) ;
#176844 = CARTESIAN_POINT('Ctrl Pts',(-26.566234898201,-13.4341833151887,
114.267859680076)) ;
#176845 = CARTESIAN_POINT('Ctrl Pts',(-26.5899081130133,-13.4357333464899,
114.339964472785)) ;
#176846 = CARTESIAN_POINT('Ctrl Pts',(-26.663711956536,-13.435733349121,114.315733431413)) ;
#176847 = CARTESIAN_POINT('Ctrl Pts',(-26.7375158000588,-13.435733351752,
114.29150239004)) ;
#176848 = CARTESIAN_POINT('Ctrl Pts',(-26.7138425852466,-13.4341833204507,
114.21939759733)) ;
#176849 = CARTESIAN_POINT('Ctrl Pts',(-26.692396148443,-13.1440226446982,
114.18967350618)) ;
#176850 = CARTESIAN_POINT('Ctrl Pts',(-26.6694482345518,-13.1627318776024,
114.119777863131)) ;
#176851 = CARTESIAN_POINT('Ctrl Pts',(-26.5956443911823,-13.1627318792492,
114.14400890497)) ;
#176852 = CARTESIAN_POINT('Ctrl Pts',(-26.5218405478128,-13.1627318808959,
114.16823994681)) ;
#176853 = CARTESIAN_POINT('Ctrl Pts',(-26.544788461704,-13.1440226479917,
114.238135589859)) ;
#176854 = CARTESIAN_POINT('Ctrl Pts',(-26.5677363755952,-13.1253134150875,
114.308031232908)) ;
#176855 = CARTESIAN_POINT('Ctrl Pts',(-26.6415402189648,-13.1253134134407,
114.283800191069)) ;
#176856 = CARTESIAN_POINT('Ctrl Pts',(-26.7153440623343,-13.125313411794,
114.259569149229)) ;
#176857 = CARTESIAN_POINT('Ctrl Pts',(-26.692396148443,-13.1440226446982,
114.18967350618)) ;
#176858 = CARTESIAN_POINT('Ctrl Pts',(-26.6475602009265,-12.8750223963181,
114.08850476367)) ;
#176859 = CARTESIAN_POINT('Ctrl Pts',(-26.6269765050809,-12.9125432630704,
114.025810147355)) ;
#176860 = CARTESIAN_POINT('Ctrl Pts',(-26.5531726621819,-12.9125432659671,
114.050041190628)) ;
#176861 = CARTESIAN_POINT('Ctrl Pts',(-26.4793688192829,-12.9125432688638,
114.074272233901)) ;
#176862 = CARTESIAN_POINT('Ctrl Pts',(-26.4999525151284,-12.8750224021116,
114.136966850215)) ;
#176863 = CARTESIAN_POINT('Ctrl Pts',(-26.520536210974,-12.8375015353593,
114.19966146653)) ;
#176864 = CARTESIAN_POINT('Ctrl Pts',(-26.594340053873,-12.8375015324626,
114.175430423257)) ;
#176865 = CARTESIAN_POINT('Ctrl Pts',(-26.668143896772,-12.8375015295659,
114.151199379984)) ;
#176866 = CARTESIAN_POINT('Ctrl Pts',(-26.6475602009265,-12.8750223963181,
114.08850476367)) ;
#176867 = CARTESIAN_POINT('Ctrl Pts',(-26.5813161216274,-12.6437154561283,
113.922329063855)) ;
#176868 = CARTESIAN_POINT('Ctrl Pts',(-26.5645911383237,-12.6974444198838,
113.87138746333)) ;
#176869 = CARTESIAN_POINT('Ctrl Pts',(-26.4907872955394,-12.6974444216942,
113.895618506952)) ;
#176870 = CARTESIAN_POINT('Ctrl Pts',(-26.4169834527552,-12.6974444235046,
113.919849550574)) ;
#176871 = CARTESIAN_POINT('Ctrl Pts',(-26.4337084360588,-12.6437154597491,
113.970791151099)) ;
#176872 = CARTESIAN_POINT('Ctrl Pts',(-26.4504334193625,-12.5899864959936,
114.021732751624)) ;
#176873 = CARTESIAN_POINT('Ctrl Pts',(-26.5242372621468,-12.5899864941832,
113.997501708002)) ;
#176874 = CARTESIAN_POINT('Ctrl Pts',(-26.598041104931,-12.5899864923728,
113.973270664379)) ;
#176875 = CARTESIAN_POINT('Ctrl Pts',(-26.5813161216274,-12.6437154561283,
113.922329063855)) ;
#176876 = CARTESIAN_POINT('Ctrl Pts',(-26.4986543480993,-12.4695015573388,
113.705836185377)) ;
#176877 = CARTESIAN_POINT('Ctrl Pts',(-26.4869467016397,-12.5354737259947,
113.670176583294)) ;
#176878 = CARTESIAN_POINT('Ctrl Pts',(-26.413142858443,-12.5354737260558,
113.69440762566)) ;
#176879 = CARTESIAN_POINT('Ctrl Pts',(-26.3393390152463,-12.5354737261168,
113.718638668026)) ;
#176880 = CARTESIAN_POINT('Ctrl Pts',(-26.3510466617059,-12.4695015574609,
113.754298270108)) ;
#176881 = CARTESIAN_POINT('Ctrl Pts',(-26.3627543081655,-12.403529388805,
113.789957872191)) ;
#176882 = CARTESIAN_POINT('Ctrl Pts',(-26.4365581513622,-12.403529388744,
113.765726829825)) ;
#176883 = CARTESIAN_POINT('Ctrl Pts',(-26.5103619945589,-12.4035293886829,
113.741495787459)) ;
#176884 = CARTESIAN_POINT('Ctrl Pts',(-26.4986543480993,-12.4695015573388,
113.705836185377)) ;
#176885 = CARTESIAN_POINT('Ctrl Pts',(-26.40350334832,-12.3618253102505,113.451569423215)) ;
#176886 = CARTESIAN_POINT('Ctrl Pts',(-26.3976869586198,-12.4354130130407,
113.433853638586)) ;
#176887 = CARTESIAN_POINT('Ctrl Pts',(-26.323883114103,-12.4354130116483,
113.458084676931)) ;
#176888 = CARTESIAN_POINT('Ctrl Pts',(-26.2500792695861,-12.4354130102558,
113.482315715276)) ;
#176889 = CARTESIAN_POINT('Ctrl Pts',(-26.2558956592862,-12.3618253074657,
113.500031499905)) ;
#176890 = CARTESIAN_POINT('Ctrl Pts',(-26.2617120489864,-12.2882376046756,
113.517747284534)) ;
#176891 = CARTESIAN_POINT('Ctrl Pts',(-26.3355158935033,-12.288237606068,
113.493516246189)) ;
#176892 = CARTESIAN_POINT('Ctrl Pts',(-26.4093197380202,-12.2882376074604,
113.469285207844)) ;
#176893 = CARTESIAN_POINT('Ctrl Pts',(-26.40350334832,-12.3618253102505,113.451569423215)) ;
#176894 = CARTESIAN_POINT('Ctrl Pts',(-26.3025135279916,-12.3304086987919,
113.179494242336)) ;
#176895 = CARTESIAN_POINT('Ctrl Pts',(-26.3030051536482,-12.406297480682,
113.18099165457)) ;
#176896 = CARTESIAN_POINT('Ctrl Pts',(-26.2292013071264,-12.4062974803833,
113.205222686808)) ;
#176897 = CARTESIAN_POINT('Ctrl Pts',(-26.1553974606047,-12.4062974800845,
113.229453719047)) ;
#176898 = CARTESIAN_POINT('Ctrl Pts',(-26.1549058349481,-12.3304086981944,
113.227956306813)) ;
#176899 = CARTESIAN_POINT('Ctrl Pts',(-26.1544142092914,-12.2545199163043,
113.226458894579)) ;
#176900 = CARTESIAN_POINT('Ctrl Pts',(-26.2282180558132,-12.2545199166031,
113.20222786234)) ;
#176901 = CARTESIAN_POINT('Ctrl Pts',(-26.3020219023349,-12.2545199169019,
113.177996830102)) ;
#176902 = CARTESIAN_POINT('Ctrl Pts',(-26.3025135279916,-12.3304086987919,
113.179494242336)) ;
#176903 = CARTESIAN_POINT('Ctrl Pts',(-26.2025781370336,-12.3767667157857,
112.910488649315)) ;
#176904 = CARTESIAN_POINT('Ctrl Pts',(-26.2093160933167,-12.4495286298161,
112.931011376676)) ;
#176905 = CARTESIAN_POINT('Ctrl Pts',(-26.13551224504,-12.4495286339673,112.95524240357)) ;
#176906 = CARTESIAN_POINT('Ctrl Pts',(-26.0617083967634,-12.4495286381184,
112.979473430463)) ;
#176907 = CARTESIAN_POINT('Ctrl Pts',(-26.0549704404803,-12.376766724088,
112.958950703102)) ;
#176908 = CARTESIAN_POINT('Ctrl Pts',(-26.0482324841972,-12.3040048100576,
112.938427975741)) ;
#176909 = CARTESIAN_POINT('Ctrl Pts',(-26.1220363324738,-12.3040048059064,
112.914196948848)) ;
#176910 = CARTESIAN_POINT('Ctrl Pts',(-26.1958401807505,-12.3040048017553,
112.889965921954)) ;
#176911 = CARTESIAN_POINT('Ctrl Pts',(-26.2025781370336,-12.3767667157857,
112.910488649315)) ;
#176912 = CARTESIAN_POINT('Ctrl Pts',(-26.1095364919782,-12.4973266925111,
112.662514220771)) ;
#176913 = CARTESIAN_POINT('Ctrl Pts',(-26.1220476976156,-12.5617762145597,
112.700621334017)) ;
#176914 = CARTESIAN_POINT('Ctrl Pts',(-26.048243847935,-12.5617762263117,
112.724852356634)) ;
#176915 = CARTESIAN_POINT('Ctrl Pts',(-25.9744399982544,-12.5617762380637,
112.749083379251)) ;
#176916 = CARTESIAN_POINT('Ctrl Pts',(-25.961928792617,-12.497326716015,112.710976266005)) ;
#176917 = CARTESIAN_POINT('Ctrl Pts',(-25.9494175869796,-12.4328771939664,
112.672869152759)) ;
#176918 = CARTESIAN_POINT('Ctrl Pts',(-26.0232214366602,-12.4328771822144,
112.648638130142)) ;
#176919 = CARTESIAN_POINT('Ctrl Pts',(-26.0970252863408,-12.4328771704624,
112.624407107525)) ;
#176920 = CARTESIAN_POINT('Ctrl Pts',(-26.1095364919782,-12.4973266925111,
112.662514220771)) ;
#176921 = CARTESIAN_POINT('Ctrl Pts',(-26.0290482236216,-12.6849702880242,
112.452967860837)) ;
#176922 = CARTESIAN_POINT('Ctrl Pts',(-26.0464605995771,-12.7364118506539,
112.506003147886)) ;
#176923 = CARTESIAN_POINT('Ctrl Pts',(-25.9726567490838,-12.7364118743968,
112.530234168028)) ;
#176924 = CARTESIAN_POINT('Ctrl Pts',(-25.8988528985905,-12.7364118981397,
112.55446518817)) ;
#176925 = CARTESIAN_POINT('Ctrl Pts',(-25.881440522635,-12.68497033551,112.501429901121)) ;
#176926 = CARTESIAN_POINT('Ctrl Pts',(-25.8640281466795,-12.6335287728803,
112.448394614072)) ;
#176927 = CARTESIAN_POINT('Ctrl Pts',(-25.9378319971728,-12.6335287491374,
112.42416359393)) ;
#176928 = CARTESIAN_POINT('Ctrl Pts',(-26.0116358476661,-12.6335287253945,
112.399932573788)) ;
#176929 = CARTESIAN_POINT('Ctrl Pts',(-26.0290482236216,-12.6849702880242,
112.452967860837)) ;
#176930 = CARTESIAN_POINT('Ctrl Pts',(-25.967020193737,-12.9239536141708,
112.299425204879)) ;
#176931 = CARTESIAN_POINT('Ctrl Pts',(-25.9880562807875,-12.958783516276,
112.363497731089)) ;
#176932 = CARTESIAN_POINT('Ctrl Pts',(-25.9142524314298,-12.9587835522301,
112.387728754689)) ;
#176933 = CARTESIAN_POINT('Ctrl Pts',(-25.8404485820722,-12.9587835881843,
112.41195977829)) ;
#176934 = CARTESIAN_POINT('Ctrl Pts',(-25.8194124950216,-12.9239536860792,
112.347887252081)) ;
#176935 = CARTESIAN_POINT('Ctrl Pts',(-25.7983764079711,-12.889123783974,
112.283814725871)) ;
#176936 = CARTESIAN_POINT('Ctrl Pts',(-25.8721802573288,-12.8891237480199,
112.25958370227)) ;
#176937 = CARTESIAN_POINT('Ctrl Pts',(-25.9459841066864,-12.8891237120657,
112.23535267867)) ;
#176938 = CARTESIAN_POINT('Ctrl Pts',(-25.967020193737,-12.9239536141708,
112.299425204879)) ;
#176939 = CARTESIAN_POINT('Ctrl Pts',(-25.9264894675845,-13.198264514804,
112.211386234531)) ;
#176940 = CARTESIAN_POINT('Ctrl Pts',(-25.949652990304,-13.2139924714054,
112.28193858637)) ;
#176941 = CARTESIAN_POINT('Ctrl Pts',(-25.8758491435936,-13.2139925191053,
112.306169618033)) ;
#176942 = CARTESIAN_POINT('Ctrl Pts',(-25.8020452968831,-13.2139925668051,
112.330400649697)) ;
#176943 = CARTESIAN_POINT('Ctrl Pts',(-25.7788817741636,-13.1982646102037,
112.259848297858)) ;
#176944 = CARTESIAN_POINT('Ctrl Pts',(-25.755718251444,-13.1825366536022,
112.189295946019)) ;
#176945 = CARTESIAN_POINT('Ctrl Pts',(-25.8295220981545,-13.1825366059024,
112.165064914356)) ;
#176946 = CARTESIAN_POINT('Ctrl Pts',(-25.9033259448649,-13.1825365582025,
112.140833882692)) ;
#176947 = CARTESIAN_POINT('Ctrl Pts',(-25.9264894675845,-13.198264514804,
112.211386234531)) ;
#176948 = CARTESIAN_POINT('Ctrl Pts',(-25.9096865137876,-13.4887696764051,
112.195672545383)) ;
#176949 = CARTESIAN_POINT('Ctrl Pts',(-25.9333228151172,-13.4842376804655,
112.267664904418)) ;
#176950 = CARTESIAN_POINT('Ctrl Pts',(-25.8595189726337,-13.4842377379434,
112.291895948956)) ;
#176951 = CARTESIAN_POINT('Ctrl Pts',(-25.7857151301502,-13.4842377954214,
112.316126993494)) ;
#176952 = CARTESIAN_POINT('Ctrl Pts',(-25.7620788288205,-13.488769791361,
112.244134634459)) ;
#176953 = CARTESIAN_POINT('Ctrl Pts',(-25.7384425274908,-13.4933017873006,
112.172142275424)) ;
#176954 = CARTESIAN_POINT('Ctrl Pts',(-25.8122463699744,-13.4933017298226,
112.147911230886)) ;
#176955 = CARTESIAN_POINT('Ctrl Pts',(-25.8860502124579,-13.4933016723446,
112.123680186348)) ;
#176956 = CARTESIAN_POINT('Ctrl Pts',(-25.9096865137876,-13.4887696764051,
112.195672545383)) ;
#176957 = CARTESIAN_POINT('Ctrl Pts',(-25.9171975165263,-13.7747050880232,
112.254081199622)) ;
#176958 = CARTESIAN_POINT('Ctrl Pts',(-25.9396084474025,-13.7502030722453,
112.322341277794)) ;
#176959 = CARTESIAN_POINT('Ctrl Pts',(-25.8658046105853,-13.7502031353853,
112.346572339591)) ;
#176960 = CARTESIAN_POINT('Ctrl Pts',(-25.7920007737681,-13.7502031985253,
112.370803401388)) ;
#176961 = CARTESIAN_POINT('Ctrl Pts',(-25.7695898428919,-13.7747052143032,
112.302543323216)) ;
#176962 = CARTESIAN_POINT('Ctrl Pts',(-25.7471789120157,-13.7992072300811,
112.234283245044)) ;
#176963 = CARTESIAN_POINT('Ctrl Pts',(-25.8209827488329,-13.7992071669411,
112.210052183247)) ;
#176964 = CARTESIAN_POINT('Ctrl Pts',(-25.89478658565,-13.7992071038011,112.18582112145)) ;
#176965 = CARTESIAN_POINT('Ctrl Pts',(-25.9171975165263,-13.7747050880232,
112.254081199622)) ;
#176966 = CARTESIAN_POINT('Ctrl Pts',(-25.9477017056163,-14.0346989777519,
112.382474254739)) ;
#176967 = CARTESIAN_POINT('Ctrl Pts',(-25.9672811895643,-13.9920093582588,
112.442110202262)) ;
#176968 = CARTESIAN_POINT('Ctrl Pts',(-25.8934773591914,-13.9920094202152,
112.466341283687)) ;
#176969 = CARTESIAN_POINT('Ctrl Pts',(-25.8196735288186,-13.9920094821717,
112.490572365113)) ;
#176970 = CARTESIAN_POINT('Ctrl Pts',(-25.8000940448706,-14.0346991016648,
112.430936417589)) ;
#176971 = CARTESIAN_POINT('Ctrl Pts',(-25.7805145609227,-14.077388721158,
112.371300470066)) ;
#176972 = CARTESIAN_POINT('Ctrl Pts',(-25.8543183912955,-14.0773886592015,
112.34706938864)) ;
#176973 = CARTESIAN_POINT('Ctrl Pts',(-25.9281222216683,-14.077388597245,
112.322838307215)) ;
#176974 = CARTESIAN_POINT('Ctrl Pts',(-25.9477017056163,-14.0346989777519,
112.382474254739)) ;
#176975 = CARTESIAN_POINT('Ctrl Pts',(-25.9983172672415,-14.2504823475427,
112.572150154809)) ;
#176976 = CARTESIAN_POINT('Ctrl Pts',(-26.0136566144146,-14.1926653559339,
112.618871329711)) ;
#176977 = CARTESIAN_POINT('Ctrl Pts',(-25.9398527905619,-14.192665409366,
112.643102430996)) ;
#176978 = CARTESIAN_POINT('Ctrl Pts',(-25.8660489667091,-14.1926654627981,
112.66733353228)) ;
#176979 = CARTESIAN_POINT('Ctrl Pts',(-25.8507096195361,-14.2504824544068,
112.620612357378)) ;
#176980 = CARTESIAN_POINT('Ctrl Pts',(-25.8353702723631,-14.3082994460156,
112.573891182476)) ;
#176981 = CARTESIAN_POINT('Ctrl Pts',(-25.9091740962158,-14.3082993925835,
112.549660081192)) ;
#176982 = CARTESIAN_POINT('Ctrl Pts',(-25.9829779200685,-14.3082993391515,
112.525428979907)) ;
#176983 = CARTESIAN_POINT('Ctrl Pts',(-25.9983172672415,-14.2504823475427,
112.572150154809)) ;
#176984 = CARTESIAN_POINT('Ctrl Pts',(-26.0642269575703,-14.4061007577842,
112.808231529626)) ;
#176985 = CARTESIAN_POINT('Ctrl Pts',(-26.0742558502766,-14.3373352952271,
112.838777916951)) ;
#176986 = CARTESIAN_POINT('Ctrl Pts',(-26.0004520317635,-14.3373353326338,
112.863009034499)) ;
#176987 = CARTESIAN_POINT('Ctrl Pts',(-25.9266482132503,-14.3373353700405,
112.887240152047)) ;
#176988 = CARTESIAN_POINT('Ctrl Pts',(-25.916619320544,-14.4061008325976,
112.856693764722)) ;
#176989 = CARTESIAN_POINT('Ctrl Pts',(-25.9065904278376,-14.4748662951547,
112.826147377397)) ;
#176990 = CARTESIAN_POINT('Ctrl Pts',(-25.9803942463508,-14.474866257748,
112.80191625985)) ;
#176991 = CARTESIAN_POINT('Ctrl Pts',(-26.0541980648639,-14.4748662203413,
112.777685142302)) ;
#176992 = CARTESIAN_POINT('Ctrl Pts',(-26.0642269575703,-14.4061007577842,
112.808231529626)) ;
#176993 = CARTESIAN_POINT('Ctrl Pts',(-26.141044455505,-14.4917978275685,
113.07789332878)) ;
#176994 = CARTESIAN_POINT('Ctrl Pts',(-26.144986537673,-14.4169485235802,
113.089900273168)) ;
#176995 = CARTESIAN_POINT('Ctrl Pts',(-26.0711827236024,-14.4169485394119,
113.114131404247)) ;
#176996 = CARTESIAN_POINT('Ctrl Pts',(-25.9973789095318,-14.4169485552436,
113.138362535326)) ;
#176997 = CARTESIAN_POINT('Ctrl Pts',(-25.9934368273637,-14.4917978592319,
113.126355590938)) ;
#176998 = CARTESIAN_POINT('Ctrl Pts',(-25.9894947451957,-14.5666471632202,
113.114348646551)) ;
#176999 = CARTESIAN_POINT('Ctrl Pts',(-26.0632985592663,-14.5666471473885,
113.090117515472)) ;
#177000 = CARTESIAN_POINT('Ctrl Pts',(-26.137102373337,-14.5666471315568,
113.065886384393)) ;
#177001 = CARTESIAN_POINT('Ctrl Pts',(-26.141044455505,-14.4917978275685,
113.07789332878)) ;
#177002 = CARTESIAN_POINT('Ctrl Pts',(-26.2209372515167,-14.4998539330622,
113.356520375798)) ;
#177003 = CARTESIAN_POINT('Ctrl Pts',(-26.2185770638367,-14.4243333592347,
113.349331623022)) ;
#177004 = CARTESIAN_POINT('Ctrl Pts',(-26.1447732512048,-14.4243333490761,
113.373562758484)) ;
#177005 = CARTESIAN_POINT('Ctrl Pts',(-26.0709694385729,-14.4243333389175,
113.397793893945)) ;
#177006 = CARTESIAN_POINT('Ctrl Pts',(-26.0733296262529,-14.4998539127449,
113.40498264672)) ;
#177007 = CARTESIAN_POINT('Ctrl Pts',(-26.0756898139329,-14.5753744865724,
113.412171399495)) ;
#177008 = CARTESIAN_POINT('Ctrl Pts',(-26.1494936265649,-14.575374496731,
113.387940264034)) ;
#177009 = CARTESIAN_POINT('Ctrl Pts',(-26.2232974391968,-14.5753745068897,
113.363709128573)) ;
#177010 = CARTESIAN_POINT('Ctrl Pts',(-26.2209372515167,-14.4998539330622,
113.356520375798)) ;
#177011 = CARTESIAN_POINT('Ctrl Pts',(-26.2986502411454,-14.4309092256038,
113.628683576885)) ;
#177012 = CARTESIAN_POINT('Ctrl Pts',(-26.2901272303962,-14.3600915226302,
113.602723859332)) ;
#177013 = CARTESIAN_POINT('Ctrl Pts',(-26.2163234169747,-14.3600914852358,
113.626954992388)) ;
#177014 = CARTESIAN_POINT('Ctrl Pts',(-26.1425196035533,-14.3600914478414,
113.651186125444)) ;
#177015 = CARTESIAN_POINT('Ctrl Pts',(-26.1510426143025,-14.430909150815,
113.677145842998)) ;
#177016 = CARTESIAN_POINT('Ctrl Pts',(-26.1595656250517,-14.5017268537886,
113.703105560551)) ;
#177017 = CARTESIAN_POINT('Ctrl Pts',(-26.2333694384732,-14.501726891183,
113.678874427494)) ;
#177018 = CARTESIAN_POINT('Ctrl Pts',(-26.3071732518947,-14.5017269285774,
113.654643294438)) ;
#177019 = CARTESIAN_POINT('Ctrl Pts',(-26.2986502411454,-14.4309092256038,
113.628683576885)) ;
#177020 = CARTESIAN_POINT('Ctrl Pts',(-26.3674757304941,-14.2894596882656,
113.873752815504)) ;
#177021 = CARTESIAN_POINT('Ctrl Pts',(-26.3534018257283,-14.2284134835687,
113.830885970355)) ;
#177022 = CARTESIAN_POINT('Ctrl Pts',(-26.2795980088395,-14.2284134202247,
113.85511709285)) ;
#177023 = CARTESIAN_POINT('Ctrl Pts',(-26.2057941919506,-14.2284133568807,
113.879348215345)) ;
#177024 = CARTESIAN_POINT('Ctrl Pts',(-26.2198680967164,-14.2894595615776,
113.922215060495)) ;
#177025 = CARTESIAN_POINT('Ctrl Pts',(-26.2339420014822,-14.3505057662746,
113.965081905644)) ;
#177026 = CARTESIAN_POINT('Ctrl Pts',(-26.307745818371,-14.3505058296186,
113.940850783149)) ;
#177027 = CARTESIAN_POINT('Ctrl Pts',(-26.3815496352599,-14.3505058929625,
113.916619660653)) ;
#177028 = CARTESIAN_POINT('Ctrl Pts',(-26.3674757304941,-14.2894596882656,
113.873752815504)) ;
#177029 = CARTESIAN_POINT('Ctrl Pts',(-26.4219359703617,-14.0846391379262,
114.075220353395)) ;
#177030 = CARTESIAN_POINT('Ctrl Pts',(-26.4033026567669,-14.0378023203219,
114.018466284573)) ;
#177031 = CARTESIAN_POINT('Ctrl Pts',(-26.3294988340054,-14.0378022350358,
114.042697389181)) ;
#177032 = CARTESIAN_POINT('Ctrl Pts',(-26.2556950112439,-14.0378021497496,
114.066928493789)) ;
#177033 = CARTESIAN_POINT('Ctrl Pts',(-26.2743283248387,-14.0846389673539,
114.123682562611)) ;
#177034 = CARTESIAN_POINT('Ctrl Pts',(-26.2929616384335,-14.1314757849582,
114.180436631434)) ;
#177035 = CARTESIAN_POINT('Ctrl Pts',(-26.366765461195,-14.1314758702443,
114.156205526826)) ;
#177036 = CARTESIAN_POINT('Ctrl Pts',(-26.4405692839565,-14.1314759555304,
114.131974422218)) ;
#177037 = CARTESIAN_POINT('Ctrl Pts',(-26.4219359703617,-14.0846391379262,
114.075220353395)) ;
#177038 = CARTESIAN_POINT('Ctrl Pts',(-26.4568504724485,-13.833584389583,
114.216907404291)) ;
#177039 = CARTESIAN_POINT('Ctrl Pts',(-26.4350207703579,-13.8042063937381,
114.150417651839)) ;
#177040 = CARTESIAN_POINT('Ctrl Pts',(-26.3612169398539,-13.8042062935713,
114.174648732864)) ;
#177041 = CARTESIAN_POINT('Ctrl Pts',(-26.2874131093499,-13.8042061934045,
114.19887981389)) ;
#177042 = CARTESIAN_POINT('Ctrl Pts',(-26.3092428114404,-13.8335841892493,
114.265369566343)) ;
#177043 = CARTESIAN_POINT('Ctrl Pts',(-26.3310725135309,-13.8629621850941,
114.331859318795)) ;
#177044 = CARTESIAN_POINT('Ctrl Pts',(-26.404876344035,-13.862962285261,114.30762823777)) ;
#177045 = CARTESIAN_POINT('Ctrl Pts',(-26.478680174539,-13.8629623854278,
114.283397156744)) ;
#177046 = CARTESIAN_POINT('Ctrl Pts',(-26.4568504724485,-13.833584389583,
114.216907404291)) ;
#177047 = CARTESIAN_POINT('Ctrl Pts',(-26.469569796329,-13.5522887119168,
114.291086084856)) ;
#177048 = CARTESIAN_POINT('Ctrl Pts',(-26.4460864891027,-13.5425061564868,
114.219559717974)) ;
#177049 = CARTESIAN_POINT('Ctrl Pts',(-26.3722826498022,-13.542506049205,
114.243790772206)) ;
#177050 = CARTESIAN_POINT('Ctrl Pts',(-26.2984788105016,-13.5425059419231,
114.268021826439)) ;
#177051 = CARTESIAN_POINT('Ctrl Pts',(-26.3219621177278,-13.5522884973531,
114.339548193321)) ;
#177052 = CARTESIAN_POINT('Ctrl Pts',(-26.345445424954,-13.5620710527831,
114.411074560204)) ;
#177053 = CARTESIAN_POINT('Ctrl Pts',(-26.4192492642546,-13.5620711600649,
114.386843505971)) ;
#177054 = CARTESIAN_POINT('Ctrl Pts',(-26.4930531035552,-13.5620712673468,
114.362612451738)) ;
#177055 = CARTESIAN_POINT('Ctrl Pts',(-26.469569796329,-13.5522887119168,
114.291086084856)) ;
#177056 = CARTESIAN_POINT('Ctrl Pts',(-26.4579117148728,-13.2592972529684,
114.291267191308)) ;
#177057 = CARTESIAN_POINT('Ctrl Pts',(-26.4344686810137,-13.2699555383047,
114.219863490648)) ;
#177058 = CARTESIAN_POINT('Ctrl Pts',(-26.3606648327152,-13.2699554336479,
114.244094517474)) ;
#177059 = CARTESIAN_POINT('Ctrl Pts',(-26.2868609844167,-13.2699553289911,
114.268325544301)) ;
#177060 = CARTESIAN_POINT('Ctrl Pts',(-26.3103040182758,-13.2592970436547,
114.339729244961)) ;
#177061 = CARTESIAN_POINT('Ctrl Pts',(-26.3337470521349,-13.2486387583184,
114.411132945621)) ;
#177062 = CARTESIAN_POINT('Ctrl Pts',(-26.4075509004334,-13.2486388629752,
114.386901918795)) ;
#177063 = CARTESIAN_POINT('Ctrl Pts',(-26.4813547487319,-13.248638967632,
114.362670891968)) ;
#177064 = CARTESIAN_POINT('Ctrl Pts',(-26.4579117148728,-13.2592972529684,
114.291267191308)) ;
#177065 = CARTESIAN_POINT('Ctrl Pts',(-26.4225035557811,-12.9811038250668,
114.218671706621)) ;
#177066 = CARTESIAN_POINT('Ctrl Pts',(-26.4007684106376,-13.0112007681919,
114.152469959464)) ;
#177067 = CARTESIAN_POINT('Ctrl Pts',(-26.3269645541615,-13.0112006734562,
114.176700961383)) ;
#177068 = CARTESIAN_POINT('Ctrl Pts',(-26.2531606976853,-13.0112005787204,
114.200931963302)) ;
#177069 = CARTESIAN_POINT('Ctrl Pts',(-26.2748958428288,-12.9811036355953,
114.267133710458)) ;
#177070 = CARTESIAN_POINT('Ctrl Pts',(-26.2966309879723,-12.9510066924703,
114.333335457615)) ;
#177071 = CARTESIAN_POINT('Ctrl Pts',(-26.3704348444484,-12.951006787206,
114.309104455696)) ;
#177072 = CARTESIAN_POINT('Ctrl Pts',(-26.4442387009246,-12.9510068819417,
114.284873453778)) ;
#177073 = CARTESIAN_POINT('Ctrl Pts',(-26.4225035557811,-12.9811038250668,
114.218671706621)) ;
#177074 = CARTESIAN_POINT('Ctrl Pts',(-26.3646027960108,-12.7319954339599,
114.077855142364)) ;
#177075 = CARTESIAN_POINT('Ctrl Pts',(-26.3461421281083,-12.7795294847017,
114.021626924628)) ;
#177076 = CARTESIAN_POINT('Ctrl Pts',(-26.2723382650299,-12.7795294077386,
114.045857906437)) ;
#177077 = CARTESIAN_POINT('Ctrl Pts',(-26.1985344019515,-12.7795293307755,
114.070088888246)) ;
#177078 = CARTESIAN_POINT('Ctrl Pts',(-26.2169950698539,-12.7319952800337,
114.126317105982)) ;
#177079 = CARTESIAN_POINT('Ctrl Pts',(-26.2354557377563,-12.6844612292919,
114.182545323718)) ;
#177080 = CARTESIAN_POINT('Ctrl Pts',(-26.3092596008348,-12.684461306255,
114.158314341908)) ;
#177081 = CARTESIAN_POINT('Ctrl Pts',(-26.3830634639132,-12.6844613832181,
114.134083360099)) ;
#177082 = CARTESIAN_POINT('Ctrl Pts',(-26.3646027960108,-12.7319954339599,
114.077855142364)) ;
#177083 = CARTESIAN_POINT('Ctrl Pts',(-26.2880633731457,-12.5329045763516,
113.880121143368)) ;
#177084 = CARTESIAN_POINT('Ctrl Pts',(-26.2741865157817,-12.5944099452727,
113.837854473023)) ;
#177085 = CARTESIAN_POINT('Ctrl Pts',(-26.2003826481654,-12.5944098904592,
113.862085441011)) ;
#177086 = CARTESIAN_POINT('Ctrl Pts',(-26.126578780549,-12.5944098356456,
113.886316408998)) ;
#177087 = CARTESIAN_POINT('Ctrl Pts',(-26.140455637913,-12.5329044667245,
113.928583079342)) ;
#177088 = CARTESIAN_POINT('Ctrl Pts',(-26.1543324952769,-12.4713990978033,
113.970849749687)) ;
#177089 = CARTESIAN_POINT('Ctrl Pts',(-26.2281363628933,-12.4713991526168,
113.946618781699)) ;
#177090 = CARTESIAN_POINT('Ctrl Pts',(-26.3019402305097,-12.4713992074304,
113.922387813712)) ;
#177091 = CARTESIAN_POINT('Ctrl Pts',(-26.2880633731457,-12.5329045763516,
113.880121143368)) ;
#177092 = CARTESIAN_POINT('Ctrl Pts',(-26.1969121836829,-12.3964115152595,
113.638084995048)) ;
#177093 = CARTESIAN_POINT('Ctrl Pts',(-26.1886417973733,-12.467539433598,
113.612894731063)) ;
#177094 = CARTESIAN_POINT('Ctrl Pts',(-26.1148379280184,-12.4675394037743,
113.637125693755)) ;
#177095 = CARTESIAN_POINT('Ctrl Pts',(-26.0410340586634,-12.4675393739507,
113.661356656447)) ;
#177096 = CARTESIAN_POINT('Ctrl Pts',(-26.049304444973,-12.3964114556122,
113.686546920432)) ;
#177097 = CARTESIAN_POINT('Ctrl Pts',(-26.0575748312825,-12.3252835372738,
113.711737184416)) ;
#177098 = CARTESIAN_POINT('Ctrl Pts',(-26.1313787006375,-12.3252835670974,
113.687506221724)) ;
#177099 = CARTESIAN_POINT('Ctrl Pts',(-26.2051825699924,-12.3252835969211,
113.663275259032)) ;
#177100 = CARTESIAN_POINT('Ctrl Pts',(-26.1969121836829,-12.3964115152595,
113.638084995048)) ;
#177101 = CARTESIAN_POINT('Ctrl Pts',(-26.097882878132,-12.3338312624075,
113.371853705732)) ;
#177102 = CARTESIAN_POINT('Ctrl Pts',(-26.0957817313739,-12.4094356003857,
113.365453950137)) ;
#177103 = CARTESIAN_POINT('Ctrl Pts',(-26.0219778624167,-12.409435594184,
113.389684914041)) ;
#177104 = CARTESIAN_POINT('Ctrl Pts',(-25.9481739934595,-12.4094355879822,
113.413915877944)) ;
#177105 = CARTESIAN_POINT('Ctrl Pts',(-25.9502751402177,-12.333831250004,
113.420315633539)) ;
#177106 = CARTESIAN_POINT('Ctrl Pts',(-25.9523762869759,-12.2582269120257,
113.426715389133)) ;
#177107 = CARTESIAN_POINT('Ctrl Pts',(-26.026180155933,-12.2582269182275,
113.40248442523)) ;
#177108 = CARTESIAN_POINT('Ctrl Pts',(-26.0999840248902,-12.2582269244292,
113.378253461326)) ;
#177109 = CARTESIAN_POINT('Ctrl Pts',(-26.097882878132,-12.3338312624075,
113.371853705732)) ;
#177110 = CARTESIAN_POINT('Ctrl Pts',(-25.9966525666846,-12.3486707517994,
113.098994699644)) ;
#177111 = CARTESIAN_POINT('Ctrl Pts',(-26.0008820645952,-12.4233532981751,
113.111877066409)) ;
#177112 = CARTESIAN_POINT('Ctrl Pts',(-25.9270781983048,-12.4233533125853,
113.136108038435)) ;
#177113 = CARTESIAN_POINT('Ctrl Pts',(-25.8532743320144,-12.4233533269956,
113.160339010461)) ;
#177114 = CARTESIAN_POINT('Ctrl Pts',(-25.8490448341037,-12.3486707806198,
113.147456643697)) ;
#177115 = CARTESIAN_POINT('Ctrl Pts',(-25.8448153361931,-12.2739882342441,
113.134574276932)) ;
#177116 = CARTESIAN_POINT('Ctrl Pts',(-25.9186192024836,-12.2739882198339,
113.110343304906)) ;
#177117 = CARTESIAN_POINT('Ctrl Pts',(-25.992423068774,-12.2739882054237,
113.08611233288)) ;
#177118 = CARTESIAN_POINT('Ctrl Pts',(-25.9966525666846,-12.3486707517994,
113.098994699644)) ;
#177119 = CARTESIAN_POINT('Ctrl Pts',(-25.9000472227805,-12.4397941697449,
112.840152077552)) ;
#177120 = CARTESIAN_POINT('Ctrl Pts',(-25.9102955213586,-12.5082273902753,
112.871366740162)) ;
#177121 = CARTESIAN_POINT('Ctrl Pts',(-25.8364916591708,-12.5082274205257,
112.895597724684)) ;
#177122 = CARTESIAN_POINT('Ctrl Pts',(-25.762687796983,-12.508227450776,112.919828709206)) ;
#177123 = CARTESIAN_POINT('Ctrl Pts',(-25.7524394984049,-12.4397942302456,
112.888614046596)) ;
#177124 = CARTESIAN_POINT('Ctrl Pts',(-25.7421911998268,-12.3713610097152,
112.857399383986)) ;
#177125 = CARTESIAN_POINT('Ctrl Pts',(-25.8159950620145,-12.3713609794648,
112.833168399464)) ;
#177126 = CARTESIAN_POINT('Ctrl Pts',(-25.8897989242023,-12.3713609492144,
112.808937414942)) ;
#177127 = CARTESIAN_POINT('Ctrl Pts',(-25.9000472227805,-12.4397941697449,
112.840152077552)) ;
#177128 = CARTESIAN_POINT('Ctrl Pts',(-25.8135929246481,-12.6021170084136,
112.612453782006)) ;
#177129 = CARTESIAN_POINT('Ctrl Pts',(-25.8291558937232,-12.6593209317561,
112.659856073623)) ;
#177130 = CARTESIAN_POINT('Ctrl Pts',(-25.7553520370272,-12.6593209703252,
112.684087074872)) ;
#177131 = CARTESIAN_POINT('Ctrl Pts',(-25.6815481803312,-12.6593210088944,
112.708318076122)) ;
#177132 = CARTESIAN_POINT('Ctrl Pts',(-25.665985211256,-12.6021170855519,
112.660915784504)) ;
#177133 = CARTESIAN_POINT('Ctrl Pts',(-25.6504222421809,-12.5449131622094,
112.613513492887)) ;
#177134 = CARTESIAN_POINT('Ctrl Pts',(-25.7242260988769,-12.5449131236403,
112.589282491638)) ;
#177135 = CARTESIAN_POINT('Ctrl Pts',(-25.7980299555729,-12.5449130850712,
112.565051490389)) ;
#177136 = CARTESIAN_POINT('Ctrl Pts',(-25.8135929246481,-12.6021170084136,
112.612453782006)) ;
#177137 = CARTESIAN_POINT('Ctrl Pts',(-25.7439720862117,-12.8208593941247,
112.435659485376)) ;
#177138 = CARTESIAN_POINT('Ctrl Pts',(-25.7636899177223,-12.862876765698,
112.495716817716)) ;
#177139 = CARTESIAN_POINT('Ctrl Pts',(-25.6898860658087,-12.8628768085356,
112.519947833531)) ;
#177140 = CARTESIAN_POINT('Ctrl Pts',(-25.6160822138952,-12.8628768513732,
112.544178849347)) ;
#177141 = CARTESIAN_POINT('Ctrl Pts',(-25.5963643823846,-12.8208594798,112.484121517008)) ;
#177142 = CARTESIAN_POINT('Ctrl Pts',(-25.576646550874,-12.7788421082267,
112.424064184669)) ;
#177143 = CARTESIAN_POINT('Ctrl Pts',(-25.6504504027875,-12.7788420653891,
112.399833168853)) ;
#177144 = CARTESIAN_POINT('Ctrl Pts',(-25.7242542547011,-12.7788420225515,
112.375602153037)) ;
#177145 = CARTESIAN_POINT('Ctrl Pts',(-25.7439720862117,-12.8208593941247,
112.435659485376)) ;
#177146 = CARTESIAN_POINT('Ctrl Pts',(-25.6940349138125,-13.084370773037,
112.319151955814)) ;
#177147 = CARTESIAN_POINT('Ctrl Pts',(-25.7165329425454,-13.1080532494665,
112.387677320502)) ;
#177148 = CARTESIAN_POINT('Ctrl Pts',(-25.6427290954994,-13.1080532886094,
112.411908351144)) ;
#177149 = CARTESIAN_POINT('Ctrl Pts',(-25.5689252484535,-13.1080533277524,
112.436139381786)) ;
#177150 = CARTESIAN_POINT('Ctrl Pts',(-25.5464272197206,-13.0843708513228,
112.367614017098)) ;
#177151 = CARTESIAN_POINT('Ctrl Pts',(-25.5239291909878,-13.0606883748933,
112.29908865241)) ;
#177152 = CARTESIAN_POINT('Ctrl Pts',(-25.5977330380337,-13.0606883357504,
112.274857621768)) ;
#177153 = CARTESIAN_POINT('Ctrl Pts',(-25.6715368850796,-13.0606882966075,
112.250626591126)) ;
#177154 = CARTESIAN_POINT('Ctrl Pts',(-25.6940349138125,-13.084370773037,
112.319151955814)) ;
#177155 = CARTESIAN_POINT('Ctrl Pts',(-25.6675129647773,-13.3711928765175,
112.273852263887)) ;
#177156 = CARTESIAN_POINT('Ctrl Pts',(-25.6911627416641,-13.3748845002412,
112.345885667787)) ;
#177157 = CARTESIAN_POINT('Ctrl Pts',(-25.6173588980609,-13.3748845322642,
112.370116708915)) ;
#177158 = CARTESIAN_POINT('Ctrl Pts',(-25.5435550544577,-13.3748845642871,
112.394347750043)) ;
#177159 = CARTESIAN_POINT('Ctrl Pts',(-25.5199052775709,-13.3711929405634,
112.322314346143)) ;
#177160 = CARTESIAN_POINT('Ctrl Pts',(-25.4962555006842,-13.3675013168397,
112.250280942242)) ;
#177161 = CARTESIAN_POINT('Ctrl Pts',(-25.5700593442874,-13.3675012848167,
112.226049901115)) ;
#177162 = CARTESIAN_POINT('Ctrl Pts',(-25.6438631878906,-13.3675012527938,
112.201818859987)) ;
#177163 = CARTESIAN_POINT('Ctrl Pts',(-25.6675129647773,-13.3711928765175,
112.273852263887)) ;
#177164 = CARTESIAN_POINT('Ctrl Pts',(-25.6652923171855,-13.6609866789311,
112.302537231817)) ;
#177165 = CARTESIAN_POINT('Ctrl Pts',(-25.6883993942946,-13.644449399206,
112.372917659915)) ;
#177166 = CARTESIAN_POINT('Ctrl Pts',(-25.6145955527509,-13.6444494224757,
112.397148707316)) ;
#177167 = CARTESIAN_POINT('Ctrl Pts',(-25.5407917112072,-13.6444494457453,
112.421379754716)) ;
#177168 = CARTESIAN_POINT('Ctrl Pts',(-25.5176846340981,-13.6609867254704,
112.350999326619)) ;
#177169 = CARTESIAN_POINT('Ctrl Pts',(-25.494577556989,-13.6775240051955,
112.280618898521)) ;
#177170 = CARTESIAN_POINT('Ctrl Pts',(-25.5683813985327,-13.6775239819258,
112.256387851121)) ;
#177171 = CARTESIAN_POINT('Ctrl Pts',(-25.6421852400764,-13.6775239586562,
112.23215680372)) ;
#177172 = CARTESIAN_POINT('Ctrl Pts',(-25.6652923171855,-13.6609866789311,
112.302537231817)) ;
#177173 = CARTESIAN_POINT('Ctrl Pts',(-25.6865853284364,-13.9327616913683,
112.402736133509)) ;
#177174 = CARTESIAN_POINT('Ctrl Pts',(-25.7075091126915,-13.8972231314794,
112.466466603975)) ;
#177175 = CARTESIAN_POINT('Ctrl Pts',(-25.633705272027,-13.8972231463685,
112.490697654054)) ;
#177176 = CARTESIAN_POINT('Ctrl Pts',(-25.5599014313626,-13.8972231612576,
112.514928704133)) ;
#177177 = CARTESIAN_POINT('Ctrl Pts',(-25.5389776471075,-13.9327617211465,
112.451198233666)) ;
#177178 = CARTESIAN_POINT('Ctrl Pts',(-25.5180538628524,-13.9683002810353,
112.3874677632)) ;
#177179 = CARTESIAN_POINT('Ctrl Pts',(-25.5918577035168,-13.9683002661462,
112.363236713121)) ;
#177180 = CARTESIAN_POINT('Ctrl Pts',(-25.6656615441813,-13.9683002512571,
112.339005663042)) ;
#177181 = CARTESIAN_POINT('Ctrl Pts',(-25.6865853284364,-13.9327616913683,
112.402736133509)) ;
#177182 = CARTESIAN_POINT('Ctrl Pts',(-25.7296598130416,-14.1696775509721,
112.569592493143)) ;
#177183 = CARTESIAN_POINT('Ctrl Pts',(-25.7468696670354,-14.117542024341,
112.622010931435)) ;
#177184 = CARTESIAN_POINT('Ctrl Pts',(-25.6730658257034,-14.1175420304562,
112.64624197948)) ;
#177185 = CARTESIAN_POINT('Ctrl Pts',(-25.5992619843714,-14.1175420365713,
112.670473027526)) ;
#177186 = CARTESIAN_POINT('Ctrl Pts',(-25.5820521303776,-14.1696775632024,
112.618054589234)) ;
#177187 = CARTESIAN_POINT('Ctrl Pts',(-25.5648422763838,-14.2218130898334,
112.565636150943)) ;
#177188 = CARTESIAN_POINT('Ctrl Pts',(-25.6386461177158,-14.2218130837183,
112.541405102897)) ;
#177189 = CARTESIAN_POINT('Ctrl Pts',(-25.7124499590478,-14.2218130776032,
112.517174054852)) ;
#177190 = CARTESIAN_POINT('Ctrl Pts',(-25.7296598130416,-14.1696775509721,
112.569592493143)) ;
#177191 = CARTESIAN_POINT('Ctrl Pts',(-25.789817147401,-14.3505522399701,
112.788110084322)) ;
#177192 = CARTESIAN_POINT('Ctrl Pts',(-25.802122003876,-14.2857090044566,
112.825588691676)) ;
#177193 = CARTESIAN_POINT('Ctrl Pts',(-25.7283181617367,-14.2857090064648,
112.849819737262)) ;
#177194 = CARTESIAN_POINT('Ctrl Pts',(-25.6545143195973,-14.285709008473,
112.874050782848)) ;
#177195 = CARTESIAN_POINT('Ctrl Pts',(-25.6422094631223,-14.3505522439865,
112.836572175495)) ;
#177196 = CARTESIAN_POINT('Ctrl Pts',(-25.6299046066472,-14.4153954795,112.799093568141)) ;
#177197 = CARTESIAN_POINT('Ctrl Pts',(-25.7037084487866,-14.4153954774918,
112.774862522554)) ;
#177198 = CARTESIAN_POINT('Ctrl Pts',(-25.7775122909259,-14.4153954754836,
112.750631476968)) ;
#177199 = CARTESIAN_POINT('Ctrl Pts',(-25.789817147401,-14.3505522399701,
112.788110084322)) ;
#177200 = CARTESIAN_POINT('Ctrl Pts',(-25.8627735208457,-14.4659895814683,
113.045823772028)) ;
#177201 = CARTESIAN_POINT('Ctrl Pts',(-25.8692678377504,-14.39298831287,113.065604413469)) ;
#177202 = CARTESIAN_POINT('Ctrl Pts',(-25.7954639943258,-14.392988312459,
113.089835455141)) ;
#177203 = CARTESIAN_POINT('Ctrl Pts',(-25.7216601509012,-14.3929883120481,
113.114066496812)) ;
#177204 = CARTESIAN_POINT('Ctrl Pts',(-25.7151658339964,-14.4659895806463,
113.094285855372)) ;
#177205 = CARTESIAN_POINT('Ctrl Pts',(-25.7086715170917,-14.5389908492445,
113.074505213931)) ;
#177206 = CARTESIAN_POINT('Ctrl Pts',(-25.7824753605163,-14.5389908496555,
113.050274172259)) ;
#177207 = CARTESIAN_POINT('Ctrl Pts',(-25.8562792039409,-14.5389908500665,
113.026043130587)) ;
#177208 = CARTESIAN_POINT('Ctrl Pts',(-25.8627735208457,-14.4659895814683,
113.045823772028)) ;
#177209 = CARTESIAN_POINT('Ctrl Pts',(-25.9424652085819,-14.5060552317741,
113.324112272392)) ;
#177210 = CARTESIAN_POINT('Ctrl Pts',(-25.9426684827821,-14.4301469447621,
113.324731412865)) ;
#177211 = CARTESIAN_POINT('Ctrl Pts',(-25.8688646384337,-14.4301469446393,
113.348962451724)) ;
#177212 = CARTESIAN_POINT('Ctrl Pts',(-25.7950607940854,-14.4301469445164,
113.373193490582)) ;
#177213 = CARTESIAN_POINT('Ctrl Pts',(-25.7948575198852,-14.5060552315285,
113.372574350108)) ;
#177214 = CARTESIAN_POINT('Ctrl Pts',(-25.7946542456851,-14.5819635185405,
113.371955209635)) ;
#177215 = CARTESIAN_POINT('Ctrl Pts',(-25.8684580900334,-14.5819635186633,
113.347724170776)) ;
#177216 = CARTESIAN_POINT('Ctrl Pts',(-25.9422619343817,-14.5819635187861,
113.323493131918)) ;
#177217 = CARTESIAN_POINT('Ctrl Pts',(-25.9424652085819,-14.5060552317741,
113.324112272392)) ;
#177218 = CARTESIAN_POINT('Ctrl Pts',(-26.0220030697392,-14.4677867862301,
113.601843781957)) ;
#177219 = CARTESIAN_POINT('Ctrl Pts',(-26.0159183962998,-14.3944382757636,
113.58331084848)) ;
#177220 = CARTESIAN_POINT('Ctrl Pts',(-25.9421145519418,-14.3944382766233,
113.607541887308)) ;
#177221 = CARTESIAN_POINT('Ctrl Pts',(-25.8683107075837,-14.3944382774829,
113.631772926137)) ;
#177222 = CARTESIAN_POINT('Ctrl Pts',(-25.874395381023,-14.4677867879495,
113.650305859614)) ;
#177223 = CARTESIAN_POINT('Ctrl Pts',(-25.8804800544623,-14.541135298416,
113.668838793091)) ;
#177224 = CARTESIAN_POINT('Ctrl Pts',(-25.9542838988204,-14.5411352975563,
113.644607754262)) ;
#177225 = CARTESIAN_POINT('Ctrl Pts',(-26.0280877431785,-14.5411352966967,
113.620376715434)) ;
#177226 = CARTESIAN_POINT('Ctrl Pts',(-26.0220030697392,-14.4677867862301,
113.601843781957)) ;
#177227 = CARTESIAN_POINT('Ctrl Pts',(-26.094854630819,-14.3553856703914,
113.859024726864)) ;
#177228 = CARTESIAN_POINT('Ctrl Pts',(-26.0829438233281,-14.2897781146532,
113.822746329087)) ;
#177229 = CARTESIAN_POINT('Ctrl Pts',(-26.0091399794359,-14.2897781158864,
113.846977369334)) ;
#177230 = CARTESIAN_POINT('Ctrl Pts',(-25.9353361355436,-14.2897781171196,
113.871208409582)) ;
#177231 = CARTESIAN_POINT('Ctrl Pts',(-25.9472469430345,-14.3553856728579,
113.907486807359)) ;
#177232 = CARTESIAN_POINT('Ctrl Pts',(-25.9591577505255,-14.4209932285961,
113.943765205137)) ;
#177233 = CARTESIAN_POINT('Ctrl Pts',(-26.0329615944177,-14.4209932273629,
113.91953416489)) ;
#177234 = CARTESIAN_POINT('Ctrl Pts',(-26.1067654383099,-14.4209932261297,
113.895303124642)) ;
#177235 = CARTESIAN_POINT('Ctrl Pts',(-26.094854630819,-14.3553856703914,
113.859024726864)) ;
#177236 = CARTESIAN_POINT('Ctrl Pts',(-26.1560900365016,-14.1738642018268,
114.081250316961)) ;
#177237 = CARTESIAN_POINT('Ctrl Pts',(-26.1391465634837,-14.1208352191847,
114.029643231916)) ;
#177238 = CARTESIAN_POINT('Ctrl Pts',(-26.0653427207382,-14.1208352175881,
114.053874275657)) ;
#177239 = CARTESIAN_POINT('Ctrl Pts',(-25.9915388779928,-14.1208352159916,
114.078105319397)) ;
#177240 = CARTESIAN_POINT('Ctrl Pts',(-26.0084823510107,-14.1738641986337,
114.129712404442)) ;
#177241 = CARTESIAN_POINT('Ctrl Pts',(-26.0254258240287,-14.2268931812759,
114.181319489486)) ;
#177242 = CARTESIAN_POINT('Ctrl Pts',(-26.0992296667742,-14.2268931828724,
114.157088445746)) ;
#177243 = CARTESIAN_POINT('Ctrl Pts',(-26.1730335095196,-14.226893184469,
114.132857402005)) ;
#177244 = CARTESIAN_POINT('Ctrl Pts',(-26.1560900365016,-14.1738642018268,
114.081250316961)) ;
#177245 = CARTESIAN_POINT('Ctrl Pts',(-26.1991928753205,-13.9401973275635,
114.247846762684)) ;
#177246 = CARTESIAN_POINT('Ctrl Pts',(-26.1784844305647,-13.9034069013251,
114.184772181116)) ;
#177247 = CARTESIAN_POINT('Ctrl Pts',(-26.1046805883513,-13.9034068952956,
114.209003226477)) ;
#177248 = CARTESIAN_POINT('Ctrl Pts',(-26.0308767461379,-13.903406889266,
114.233234271838)) ;
#177249 = CARTESIAN_POINT('Ctrl Pts',(-26.0515851908937,-13.9401973155044,
114.296308853406)) ;
#177250 = CARTESIAN_POINT('Ctrl Pts',(-26.0722936356495,-13.9769877417428,
114.359383434975)) ;
#177251 = CARTESIAN_POINT('Ctrl Pts',(-26.1460974778628,-13.9769877477723,
114.335152389614)) ;
#177252 = CARTESIAN_POINT('Ctrl Pts',(-26.2199013200762,-13.9769877538019,
114.310921344253)) ;
#177253 = CARTESIAN_POINT('Ctrl Pts',(-26.1991928753205,-13.9401973275635,
114.247846762684)) ;
#177254 = CARTESIAN_POINT('Ctrl Pts',(-26.2212325199795,-13.6684975496401,
114.35043177796)) ;
#177255 = CARTESIAN_POINT('Ctrl Pts',(-26.1982213483443,-13.650624726406,
114.280343461741)) ;
#177256 = CARTESIAN_POINT('Ctrl Pts',(-26.1244175060552,-13.6506247135771,
114.304574506871)) ;
#177257 = CARTESIAN_POINT('Ctrl Pts',(-26.0506136637662,-13.6506247007482,
114.328805552001)) ;
#177258 = CARTESIAN_POINT('Ctrl Pts',(-26.0736248354014,-13.6684975239824,
114.398893868221)) ;
#177259 = CARTESIAN_POINT('Ctrl Pts',(-26.0966360070366,-13.6863703472165,
114.468982184441)) ;
#177260 = CARTESIAN_POINT('Ctrl Pts',(-26.1704398493257,-13.6863703600454,
114.444751139311)) ;
#177261 = CARTESIAN_POINT('Ctrl Pts',(-26.2442436916147,-13.6863703728742,
114.42052009418)) ;
#177262 = CARTESIAN_POINT('Ctrl Pts',(-26.2212325199795,-13.6684975496401,
114.35043177796)) ;
#177263 = CARTESIAN_POINT('Ctrl Pts',(-26.2196857700443,-13.3792258998284,
114.381117503958)) ;
#177264 = CARTESIAN_POINT('Ctrl Pts',(-26.1960167906977,-13.3815248172849,
114.309025611457)) ;
#177265 = CARTESIAN_POINT('Ctrl Pts',(-26.1222129473121,-13.3815247972218,
114.333256653248)) ;
#177266 = CARTESIAN_POINT('Ctrl Pts',(-26.0484091039266,-13.3815247771587,
114.357487695039)) ;
#177267 = CARTESIAN_POINT('Ctrl Pts',(-26.0720780832732,-13.3792258597022,
114.42957958754)) ;
#177268 = CARTESIAN_POINT('Ctrl Pts',(-26.0957470626198,-13.3769269422458,
114.501671480041)) ;
#177269 = CARTESIAN_POINT('Ctrl Pts',(-26.1695509060054,-13.3769269623089,
114.47744043825)) ;
#177270 = CARTESIAN_POINT('Ctrl Pts',(-26.2433547493909,-13.3769269823719,
114.453209396459)) ;
#177271 = CARTESIAN_POINT('Ctrl Pts',(-26.2196857700443,-13.3792258998284,
114.381117503958)) ;
#177272 = CARTESIAN_POINT('Ctrl Pts',(-26.1935600200775,-13.0905267308239,
114.337229266664)) ;
#177273 = CARTESIAN_POINT('Ctrl Pts',(-26.1709422477314,-13.1129867022683,
114.26833918088)) ;
#177274 = CARTESIAN_POINT('Ctrl Pts',(-26.0971384017158,-13.1129866733618,
114.29257021466)) ;
#177275 = CARTESIAN_POINT('Ctrl Pts',(-26.0233345557003,-13.1129866444553,
114.31680124844)) ;
#177276 = CARTESIAN_POINT('Ctrl Pts',(-26.0459523280465,-13.0905266730108,
114.385691334224)) ;
#177277 = CARTESIAN_POINT('Ctrl Pts',(-26.0685701003926,-13.0680667015663,
114.454581420009)) ;
#177278 = CARTESIAN_POINT('Ctrl Pts',(-26.1423739464081,-13.0680667304729,
114.430350386228)) ;
#177279 = CARTESIAN_POINT('Ctrl Pts',(-26.2161777924237,-13.0680667593794,
114.406119352448)) ;
#177280 = CARTESIAN_POINT('Ctrl Pts',(-26.1935600200775,-13.0905267308239,
114.337229266664)) ;
#177281 = CARTESIAN_POINT('Ctrl Pts',(-26.1446708799254,-12.8284630006125,
114.223586216955)) ;
#177282 = CARTESIAN_POINT('Ctrl Pts',(-26.1247043042031,-12.8692525646979,
114.162771248191)) ;
#177283 = CARTESIAN_POINT('Ctrl Pts',(-26.0509004547599,-12.869252533481,
114.187002271531)) ;
#177284 = CARTESIAN_POINT('Ctrl Pts',(-25.9770966053167,-12.869252502264,
114.211233294871)) ;
#177285 = CARTESIAN_POINT('Ctrl Pts',(-25.9970631810391,-12.8284629381786,
114.272048263635)) ;
#177286 = CARTESIAN_POINT('Ctrl Pts',(-26.0170297567614,-12.7876733740933,
114.3328632324)) ;
#177287 = CARTESIAN_POINT('Ctrl Pts',(-26.0908336062046,-12.7876734053102,
114.30863220906)) ;
#177288 = CARTESIAN_POINT('Ctrl Pts',(-26.1646374556478,-12.7876734365271,
114.28440118572)) ;
#177289 = CARTESIAN_POINT('Ctrl Pts',(-26.1446708799254,-12.8284630006125,
114.223586216955)) ;
#177290 = CARTESIAN_POINT('Ctrl Pts',(-26.0750221134765,-12.6065365051644,
114.046995192604)) ;
#177291 = CARTESIAN_POINT('Ctrl Pts',(-26.0591539020257,-12.6628800161341,
113.998663179958)) ;
#177292 = CARTESIAN_POINT('Ctrl Pts',(-25.9853500480458,-12.6628799847594,
114.022894189481)) ;
#177293 = CARTESIAN_POINT('Ctrl Pts',(-25.9115461940659,-12.6628799533848,
114.047125199003)) ;
#177294 = CARTESIAN_POINT('Ctrl Pts',(-25.9274144055167,-12.6065364424151,
114.095457211648)) ;
#177295 = CARTESIAN_POINT('Ctrl Pts',(-25.9432826169676,-12.5501929314454,
114.143789224293)) ;
#177296 = CARTESIAN_POINT('Ctrl Pts',(-26.0170864709474,-12.5501929628201,
114.119558214771)) ;
#177297 = CARTESIAN_POINT('Ctrl Pts',(-26.0908903249274,-12.5501929941947,
114.095327205249)) ;
#177298 = CARTESIAN_POINT('Ctrl Pts',(-26.0750221134765,-12.6065365051644,
114.046995192604)) ;
#177299 = CARTESIAN_POINT('Ctrl Pts',(-25.9893085808254,-12.4434900571409,
113.821371187434)) ;
#177300 = CARTESIAN_POINT('Ctrl Pts',(-25.9786684347472,-12.5112986804866,
113.788963018204)) ;
#177301 = CARTESIAN_POINT('Ctrl Pts',(-25.9048645761478,-12.5112986555149,
113.813194013656)) ;
#177302 = CARTESIAN_POINT('Ctrl Pts',(-25.8310607175484,-12.5112986305432,
113.837425009108)) ;
#177303 = CARTESIAN_POINT('Ctrl Pts',(-25.8417008636267,-12.4434900071976,
113.869833178338)) ;
#177304 = CARTESIAN_POINT('Ctrl Pts',(-25.8523410097049,-12.3756813838519,
113.902241347569)) ;
#177305 = CARTESIAN_POINT('Ctrl Pts',(-25.9261448683043,-12.3756814088236,
113.878010352117)) ;
#177306 = CARTESIAN_POINT('Ctrl Pts',(-25.9999487269037,-12.3756814337953,
113.853779356665)) ;
#177307 = CARTESIAN_POINT('Ctrl Pts',(-25.9893085808254,-12.4434900571409,
113.821371187434)) ;
#177308 = CARTESIAN_POINT('Ctrl Pts',(-25.8927472268414,-12.3500508502058,
113.562734682547)) ;
#177309 = CARTESIAN_POINT('Ctrl Pts',(-25.888099410984,-12.4244812912888,
113.548578184144)) ;
#177310 = CARTESIAN_POINT('Ctrl Pts',(-25.8142955482319,-12.424481278477,
113.572809166948)) ;
#177311 = CARTESIAN_POINT('Ctrl Pts',(-25.7404916854798,-12.4244812656651,
113.597040149751)) ;
#177312 = CARTESIAN_POINT('Ctrl Pts',(-25.7451395013371,-12.3500508245822,
113.611196648154)) ;
#177313 = CARTESIAN_POINT('Ctrl Pts',(-25.7497873171944,-12.2756203834992,
113.625353146556)) ;
#177314 = CARTESIAN_POINT('Ctrl Pts',(-25.8235911799465,-12.275620396311,
113.601122163753)) ;
#177315 = CARTESIAN_POINT('Ctrl Pts',(-25.8973950426987,-12.2756204091229,
113.57689118095)) ;
#177316 = CARTESIAN_POINT('Ctrl Pts',(-25.8927472268414,-12.3500508502058,
113.562734682547)) ;
#177317 = CARTESIAN_POINT('Ctrl Pts',(-25.7915387238206,-12.3331953888952,
113.289941672903)) ;
#177318 = CARTESIAN_POINT('Ctrl Pts',(-25.7932163469713,-12.4089103805945,
113.295051440953)) ;
#177319 = CARTESIAN_POINT('Ctrl Pts',(-25.7194124813001,-12.4089103853774,
113.319282414866)) ;
#177320 = CARTESIAN_POINT('Ctrl Pts',(-25.6456086156289,-12.4089103901604,
113.343513388778)) ;
#177321 = CARTESIAN_POINT('Ctrl Pts',(-25.6439309924783,-12.3331953984611,
113.338403620727)) ;
#177322 = CARTESIAN_POINT('Ctrl Pts',(-25.6422533693277,-12.2574804067618,
113.333293852676)) ;
#177323 = CARTESIAN_POINT('Ctrl Pts',(-25.7160572349988,-12.2574804019789,
113.309062878764)) ;
#177324 = CARTESIAN_POINT('Ctrl Pts',(-25.78986110067,-12.2574803971959,113.284831904852)) ;
#177325 = CARTESIAN_POINT('Ctrl Pts',(-25.7915387238206,-12.3331953888952,
113.289941672903)) ;
#177326 = CARTESIAN_POINT('Ctrl Pts',(-25.6921668349445,-12.3940161187778,
113.022744551192)) ;
#177327 = CARTESIAN_POINT('Ctrl Pts',(-25.7000507376626,-12.4655945537366,
113.046757645277)) ;
#177328 = CARTESIAN_POINT('Ctrl Pts',(-25.626246870914,-12.4655945799172,
113.070988615907)) ;
#177329 = CARTESIAN_POINT('Ctrl Pts',(-25.5524430041654,-12.4655946060978,
113.095219586538)) ;
#177330 = CARTESIAN_POINT('Ctrl Pts',(-25.5445591014473,-12.3940161711391,
113.071206492453)) ;
#177331 = CARTESIAN_POINT('Ctrl Pts',(-25.5366751987291,-12.3224377361804,
113.047193398368)) ;
#177332 = CARTESIAN_POINT('Ctrl Pts',(-25.6104790654777,-12.3224377099997,
113.022962427738)) ;
#177333 = CARTESIAN_POINT('Ctrl Pts',(-25.6842829322263,-12.3224376838191,
112.998731457107)) ;
#177334 = CARTESIAN_POINT('Ctrl Pts',(-25.6921668349445,-12.3940161187778,
113.022744551192)) ;
#177335 = CARTESIAN_POINT('Ctrl Pts',(-25.6010011665108,-12.5284976067023,
112.780567517695)) ;
#177336 = CARTESIAN_POINT('Ctrl Pts',(-25.614526906004,-12.5907910171459,
112.821764736152)) ;
#177337 = CARTESIAN_POINT('Ctrl Pts',(-25.5407230404825,-12.590791066487,
112.84599571052)) ;
#177338 = CARTESIAN_POINT('Ctrl Pts',(-25.4669191749609,-12.5907911158281,
112.870226684888)) ;
#177339 = CARTESIAN_POINT('Ctrl Pts',(-25.4533934354677,-12.5284977053845,
112.829029466431)) ;
#177340 = CARTESIAN_POINT('Ctrl Pts',(-25.4398676959746,-12.466204294941,
112.787832247975)) ;
#177341 = CARTESIAN_POINT('Ctrl Pts',(-25.5136715614961,-12.4662042455999,
112.763601273607)) ;
#177342 = CARTESIAN_POINT('Ctrl Pts',(-25.5874754270177,-12.4662041962588,
112.739370299239)) ;
#177343 = CARTESIAN_POINT('Ctrl Pts',(-25.6010011665108,-12.5284976067023,
112.780567517695)) ;
#177344 = CARTESIAN_POINT('Ctrl Pts',(-25.5241403849889,-12.7253590046235,
112.581767024192)) ;
#177345 = CARTESIAN_POINT('Ctrl Pts',(-25.5423213548809,-12.7739984449888,
112.637143323225)) ;
#177346 = CARTESIAN_POINT('Ctrl Pts',(-25.4685174931494,-12.7739985153053,
112.661374309137)) ;
#177347 = CARTESIAN_POINT('Ctrl Pts',(-25.3947136314178,-12.7739985856217,
112.685605295048)) ;
#177348 = CARTESIAN_POINT('Ctrl Pts',(-25.3765326615258,-12.7253591452565,
112.630228996016)) ;
#177349 = CARTESIAN_POINT('Ctrl Pts',(-25.3583516916337,-12.6767197048912,
112.574852696983)) ;
#177350 = CARTESIAN_POINT('Ctrl Pts',(-25.4321555533653,-12.6767196345747,
112.550621711072)) ;
#177351 = CARTESIAN_POINT('Ctrl Pts',(-25.5059594150968,-12.6767195642582,
112.52639072516)) ;
#177352 = CARTESIAN_POINT('Ctrl Pts',(-25.5241403849889,-12.7253590046235,
112.581767024192)) ;
#177353 = CARTESIAN_POINT('Ctrl Pts',(-25.4653269966594,-12.9750336085797,
112.438402703222)) ;
#177354 = CARTESIAN_POINT('Ctrl Pts',(-25.4869006596714,-13.0063134744705,
112.504112597953)) ;
#177355 = CARTESIAN_POINT('Ctrl Pts',(-25.4130968036294,-13.0063135643594,
112.528343601194)) ;
#177356 = CARTESIAN_POINT('Ctrl Pts',(-25.3392929475873,-13.0063136542484,
112.552574604435)) ;
#177357 = CARTESIAN_POINT('Ctrl Pts',(-25.3177192845753,-12.9750337883576,
112.486864709703)) ;
#177358 = CARTESIAN_POINT('Ctrl Pts',(-25.2961456215632,-12.9437539224668,
112.421154814972)) ;
#177359 = CARTESIAN_POINT('Ctrl Pts',(-25.3699494776053,-12.9437538325779,
112.396923811731)) ;
#177360 = CARTESIAN_POINT('Ctrl Pts',(-25.4437533336474,-12.943753742689,
112.372692808491)) ;
#177361 = CARTESIAN_POINT('Ctrl Pts',(-25.4653269966594,-12.9750336085797,
112.438402703222)) ;
#177362 = CARTESIAN_POINT('Ctrl Pts',(-25.4295219032565,-13.2518773391213,
112.364484091442)) ;
#177363 = CARTESIAN_POINT('Ctrl Pts',(-25.4528995946163,-13.2638740920304,
112.435688765391)) ;
#177364 = CARTESIAN_POINT('Ctrl Pts',(-25.3790957463178,-13.2638741920649,
112.459919792217)) ;
#177365 = CARTESIAN_POINT('Ctrl Pts',(-25.3052918980194,-13.2638742920995,
112.484150819044)) ;
#177366 = CARTESIAN_POINT('Ctrl Pts',(-25.2819142066595,-13.2518775391904,
112.412946145095)) ;
#177367 = CARTESIAN_POINT('Ctrl Pts',(-25.2585365152996,-13.2398807862813,
112.341741471146)) ;
#177368 = CARTESIAN_POINT('Ctrl Pts',(-25.3323403635981,-13.2398806862467,
112.31751044432)) ;
#177369 = CARTESIAN_POINT('Ctrl Pts',(-25.4061442118966,-13.2398805862122,
112.293279417493)) ;
#177370 = CARTESIAN_POINT('Ctrl Pts',(-25.4295219032565,-13.2518773391213,
112.364484091442)) ;
#177371 = CARTESIAN_POINT('Ctrl Pts',(-25.4172132742783,-13.5442043587849,
112.36261312341)) ;
#177372 = CARTESIAN_POINT('Ctrl Pts',(-25.4407477286695,-13.5358098803519,
112.434295272181)) ;
#177373 = CARTESIAN_POINT('Ctrl Pts',(-25.3669438889883,-13.5358099849276,
112.458526325254)) ;
#177374 = CARTESIAN_POINT('Ctrl Pts',(-25.2931400493071,-13.5358100895033,
112.482757378328)) ;
#177375 = CARTESIAN_POINT('Ctrl Pts',(-25.2696055949159,-13.5442045679364,
112.411075229557)) ;
#177376 = CARTESIAN_POINT('Ctrl Pts',(-25.2460711405248,-13.5525990463694,
112.339393080786)) ;
#177377 = CARTESIAN_POINT('Ctrl Pts',(-25.319874980206,-13.5525989417936,
112.315162027713)) ;
#177378 = CARTESIAN_POINT('Ctrl Pts',(-25.3936788198872,-13.5525988372179,
112.290930974639)) ;
#177379 = CARTESIAN_POINT('Ctrl Pts',(-25.4172132742783,-13.5442043587849,
112.36261312341)) ;
#177380 = CARTESIAN_POINT('Ctrl Pts',(-25.4292212348024,-13.8259451748865,
112.434602285511)) ;
#177381 = CARTESIAN_POINT('Ctrl Pts',(-25.4512191540056,-13.7978682383242,
112.50160439598)) ;
#177382 = CARTESIAN_POINT('Ctrl Pts',(-25.37741532312,-13.7978683377893,112.525835475844)) ;
#177383 = CARTESIAN_POINT('Ctrl Pts',(-25.3036114922345,-13.7978684372543,
112.550066555707)) ;
#177384 = CARTESIAN_POINT('Ctrl Pts',(-25.2816135730313,-13.8259453738167,
112.483064445239)) ;
#177385 = CARTESIAN_POINT('Ctrl Pts',(-25.2596156538282,-13.8540223103791,
112.41606233477)) ;
#177386 = CARTESIAN_POINT('Ctrl Pts',(-25.3334194847137,-13.854022210914,
112.391831254906)) ;
#177387 = CARTESIAN_POINT('Ctrl Pts',(-25.4072233155992,-13.8540221114489,
112.367600175042)) ;
#177388 = CARTESIAN_POINT('Ctrl Pts',(-25.4292212348024,-13.8259451748865,
112.434602285511)) ;
#177389 = CARTESIAN_POINT('Ctrl Pts',(-25.4637880029618,-14.0792480619856,
112.575412566812)) ;
#177390 = CARTESIAN_POINT('Ctrl Pts',(-25.4826700787463,-14.0334450409061,
112.632924320946)) ;
#177391 = CARTESIAN_POINT('Ctrl Pts',(-25.4088662558851,-14.0334451269848,
112.65715542525)) ;
#177392 = CARTESIAN_POINT('Ctrl Pts',(-25.3350624330239,-14.0334452130635,
112.681386529554)) ;
#177393 = CARTESIAN_POINT('Ctrl Pts',(-25.3161803572393,-14.079248234143,
112.623874775421)) ;
#177394 = CARTESIAN_POINT('Ctrl Pts',(-25.2972982814547,-14.1250512552225,
112.566363021288)) ;
#177395 = CARTESIAN_POINT('Ctrl Pts',(-25.371102104316,-14.1250511691438,
112.542131916984)) ;
#177396 = CARTESIAN_POINT('Ctrl Pts',(-25.4449059271772,-14.1250510830651,
112.517900812679)) ;
#177397 = CARTESIAN_POINT('Ctrl Pts',(-25.4637880029618,-14.0792480619856,
112.575412566812)) ;
#177398 = CARTESIAN_POINT('Ctrl Pts',(-25.5175967023213,-14.2845087011992,
112.774736681666)) ;
#177399 = CARTESIAN_POINT('Ctrl Pts',(-25.5320168624218,-14.2243072924303,
112.818658160557)) ;
#177400 = CARTESIAN_POINT('Ctrl Pts',(-25.4582130459194,-14.2243073577872,
112.842889284229)) ;
#177401 = CARTESIAN_POINT('Ctrl Pts',(-25.3844092294169,-14.2243074231441,
112.867120407901)) ;
#177402 = CARTESIAN_POINT('Ctrl Pts',(-25.3699890693164,-14.284508831913,
112.823198929011)) ;
#177403 = CARTESIAN_POINT('Ctrl Pts',(-25.3555689092159,-14.3447102406819,
112.77927745012)) ;
#177404 = CARTESIAN_POINT('Ctrl Pts',(-25.4293727257183,-14.344710175325,
112.755046326448)) ;
#177405 = CARTESIAN_POINT('Ctrl Pts',(-25.5031765422207,-14.3447101099681,
112.730815202776)) ;
#177406 = CARTESIAN_POINT('Ctrl Pts',(-25.5175967023213,-14.2845087011992,
112.774736681666)) ;
#177407 = CARTESIAN_POINT('Ctrl Pts',(-25.58604236121,-14.4278905637469,113.018639551001)) ;
#177408 = CARTESIAN_POINT('Ctrl Pts',(-25.5949722174165,-14.3575893614837,
113.045838450109)) ;
#177409 = CARTESIAN_POINT('Ctrl Pts',(-25.5211684050333,-14.3575894011323,
113.070069586328)) ;
#177410 = CARTESIAN_POINT('Ctrl Pts',(-25.4473645926501,-14.3575894407809,
113.094300722547)) ;
#177411 = CARTESIAN_POINT('Ctrl Pts',(-25.4384347364437,-14.4278906430441,
113.067101823439)) ;
#177412 = CARTESIAN_POINT('Ctrl Pts',(-25.4295048802372,-14.4981918453073,
113.03990292433)) ;
#177413 = CARTESIAN_POINT('Ctrl Pts',(-25.5033086926204,-14.4981918056587,
113.015671788111)) ;
#177414 = CARTESIAN_POINT('Ctrl Pts',(-25.5771125050036,-14.4981917660102,
112.991440651893)) ;
#177415 = CARTESIAN_POINT('Ctrl Pts',(-25.58604236121,-14.4278905637469,113.018639551001)) ;
#177416 = CARTESIAN_POINT('Ctrl Pts',(-25.6636620375048,-14.49909499359,113.290546274635)) ;
#177417 = CARTESIAN_POINT('Ctrl Pts',(-25.6664517281903,-14.4237176570017,
113.299043220325)) ;
#177418 = CARTESIAN_POINT('Ctrl Pts',(-25.592647917231,-14.4237176684641,
113.323274360881)) ;
#177419 = CARTESIAN_POINT('Ctrl Pts',(-25.5188441062716,-14.4237176799264,
113.347505501436)) ;
#177420 = CARTESIAN_POINT('Ctrl Pts',(-25.5160544155862,-14.4990950165147,
113.339008555746)) ;
#177421 = CARTESIAN_POINT('Ctrl Pts',(-25.5132647249008,-14.5744723531029,
113.330511610056)) ;
#177422 = CARTESIAN_POINT('Ctrl Pts',(-25.5870685358601,-14.5744723416406,
113.3062804695)) ;
#177423 = CARTESIAN_POINT('Ctrl Pts',(-25.6608723468194,-14.5744723301783,
113.282049328944)) ;
#177424 = CARTESIAN_POINT('Ctrl Pts',(-25.6636620375048,-14.49909499359,113.290546274635)) ;
#177425 = CARTESIAN_POINT('Ctrl Pts',(-25.7439225347513,-14.492829252027,
113.570454450893)) ;
#177426 = CARTESIAN_POINT('Ctrl Pts',(-25.7403793642402,-14.4177767154629,
113.559662523248)) ;
#177427 = CARTESIAN_POINT('Ctrl Pts',(-25.6665755520265,-14.4177766993577,
113.583893659982)) ;
#177428 = CARTESIAN_POINT('Ctrl Pts',(-25.5927717398128,-14.4177766832525,
113.608124796717)) ;
#177429 = CARTESIAN_POINT('Ctrl Pts',(-25.5963149103238,-14.4928292198167,
113.618916724363)) ;
#177430 = CARTESIAN_POINT('Ctrl Pts',(-25.5998580808348,-14.5678817563809,
113.629708652009)) ;
#177431 = CARTESIAN_POINT('Ctrl Pts',(-25.6736618930486,-14.567881772486,
113.605477515274)) ;
#177432 = CARTESIAN_POINT('Ctrl Pts',(-25.7474657052623,-14.5678817885912,
113.581246378539)) ;
#177433 = CARTESIAN_POINT('Ctrl Pts',(-25.7439225347513,-14.492829252027,
113.570454450893)) ;
#177434 = CARTESIAN_POINT('Ctrl Pts',(-25.8206456678488,-14.4093444300335,
113.83969383373)) ;
#177435 = CARTESIAN_POINT('Ctrl Pts',(-25.8110049285776,-14.3400077238797,
113.810329695576)) ;
#177436 = CARTESIAN_POINT('Ctrl Pts',(-25.7372011124802,-14.3400076836513,
113.834560820481)) ;
#177437 = CARTESIAN_POINT('Ctrl Pts',(-25.6633972963827,-14.340007643423,
113.858791945387)) ;
#177438 = CARTESIAN_POINT('Ctrl Pts',(-25.6730380356538,-14.4093443495768,
113.888156083541)) ;
#177439 = CARTESIAN_POINT('Ctrl Pts',(-25.6826787749249,-14.4786810557306,
113.917520221696)) ;
#177440 = CARTESIAN_POINT('Ctrl Pts',(-25.7564825910224,-14.4786810959589,
113.89328909679)) ;
#177441 = CARTESIAN_POINT('Ctrl Pts',(-25.8302864071199,-14.4786811361873,
113.869057971885)) ;
#177442 = CARTESIAN_POINT('Ctrl Pts',(-25.8206456678488,-14.4093444300335,
113.83969383373)) ;
#177443 = CARTESIAN_POINT('Ctrl Pts',(-25.8872186639727,-14.2544052422715,
114.077996994067)) ;
#177444 = CARTESIAN_POINT('Ctrl Pts',(-25.872180153682,-14.1957815883073,
114.032192116431)) ;
#177445 = CARTESIAN_POINT('Ctrl Pts',(-25.7983763318251,-14.1957815301846,
114.056423223795)) ;
#177446 = CARTESIAN_POINT('Ctrl Pts',(-25.7245725099682,-14.1957814720619,
114.080654331158)) ;
#177447 = CARTESIAN_POINT('Ctrl Pts',(-25.739611020259,-14.2544051260261,
114.126459208794)) ;
#177448 = CARTESIAN_POINT('Ctrl Pts',(-25.7546495305497,-14.3130287799903,
114.17226408643)) ;
#177449 = CARTESIAN_POINT('Ctrl Pts',(-25.8284533524066,-14.313028838113,
114.148032979066)) ;
#177450 = CARTESIAN_POINT('Ctrl Pts',(-25.9022571742635,-14.3130288962357,
114.123801871703)) ;
#177451 = CARTESIAN_POINT('Ctrl Pts',(-25.8872186639727,-14.2544052422715,
114.077996994067)) ;
#177452 = CARTESIAN_POINT('Ctrl Pts',(-25.9379469965569,-14.0410991720381,
114.267799990034)) ;
#177453 = CARTESIAN_POINT('Ctrl Pts',(-25.9186138483298,-13.9972803376337,
114.20891433828)) ;
#177454 = CARTESIAN_POINT('Ctrl Pts',(-25.8448100199794,-13.9972802674836,
114.233145425866)) ;
#177455 = CARTESIAN_POINT('Ctrl Pts',(-25.771006191629,-13.9972801973335,
114.257376513451)) ;
#177456 = CARTESIAN_POINT('Ctrl Pts',(-25.790339339856,-14.0410990317379,
114.316262165205)) ;
#177457 = CARTESIAN_POINT('Ctrl Pts',(-25.8096724880831,-14.0849178661423,
114.375147816958)) ;
#177458 = CARTESIAN_POINT('Ctrl Pts',(-25.8834763164336,-14.0849179362924,
114.350916729373)) ;
#177459 = CARTESIAN_POINT('Ctrl Pts',(-25.957280144784,-14.0849180064424,
114.326685641788)) ;
#177460 = CARTESIAN_POINT('Ctrl Pts',(-25.9379469965569,-14.0410991720381,
114.267799990034)) ;
#177461 = CARTESIAN_POINT('Ctrl Pts',(-25.9690716034183,-13.7816895970119,
114.398141043581)) ;
#177462 = CARTESIAN_POINT('Ctrl Pts',(-25.9468006981219,-13.7559161217153,
114.330307457948)) ;
#177463 = CARTESIAN_POINT('Ctrl Pts',(-25.872996862596,-13.7559160484501,
114.354538523678)) ;
#177464 = CARTESIAN_POINT('Ctrl Pts',(-25.7991930270701,-13.7559159751849,
114.378769589408)) ;
#177465 = CARTESIAN_POINT('Ctrl Pts',(-25.8214639323665,-13.7816894504815,
114.446603175041)) ;
#177466 = CARTESIAN_POINT('Ctrl Pts',(-25.843734837663,-13.8074629257781,
114.514436760674)) ;
#177467 = CARTESIAN_POINT('Ctrl Pts',(-25.9175386731889,-13.8074629990433,
114.490205694944)) ;
#177468 = CARTESIAN_POINT('Ctrl Pts',(-25.9913425087147,-13.8074630723084,
114.465974629214)) ;
#177469 = CARTESIAN_POINT('Ctrl Pts',(-25.9690716034183,-13.7816895970119,
114.398141043581)) ;
#177470 = CARTESIAN_POINT('Ctrl Pts',(-25.977202611184,-13.4976199910735,
114.4582556851)) ;
#177471 = CARTESIAN_POINT('Ctrl Pts',(-25.9535989487719,-13.4916413053213,
114.386362736462)) ;
#177472 = CARTESIAN_POINT('Ctrl Pts',(-25.8797951067563,-13.4916412347082,
114.410593782425)) ;
#177473 = CARTESIAN_POINT('Ctrl Pts',(-25.8059912647407,-13.4916411640951,
114.434824828388)) ;
#177474 = CARTESIAN_POINT('Ctrl Pts',(-25.8295949271528,-13.4976198498473,
114.506717777026)) ;
#177475 = CARTESIAN_POINT('Ctrl Pts',(-25.8531985895649,-13.5035985355994,
114.578610725664)) ;
#177476 = CARTESIAN_POINT('Ctrl Pts',(-25.9270024315805,-13.5035986062125,
114.554379679701)) ;
#177477 = CARTESIAN_POINT('Ctrl Pts',(-26.0008062735961,-13.5035986768257,
114.530148633738)) ;
#177478 = CARTESIAN_POINT('Ctrl Pts',(-25.977202611184,-13.4976199910735,
114.4582556851)) ;
#177479 = CARTESIAN_POINT('Ctrl Pts',(-25.9611123344456,-13.2063007087737,
114.444798177741)) ;
#177480 = CARTESIAN_POINT('Ctrl Pts',(-25.9378606125945,-13.2206528794354,
114.37397718344)) ;
#177481 = CARTESIAN_POINT('Ctrl Pts',(-25.864056765183,-13.2206528189828,
114.398208212968)) ;
#177482 = CARTESIAN_POINT('Ctrl Pts',(-25.7902529177715,-13.2206527585302,
114.422439242497)) ;
#177483 = CARTESIAN_POINT('Ctrl Pts',(-25.8135046396226,-13.2063005878686,
114.493260236797)) ;
#177484 = CARTESIAN_POINT('Ctrl Pts',(-25.8367563614737,-13.1919484172069,
114.564081231098)) ;
#177485 = CARTESIAN_POINT('Ctrl Pts',(-25.9105602088852,-13.1919484776594,
114.53985020157)) ;
#177486 = CARTESIAN_POINT('Ctrl Pts',(-25.9843640562967,-13.191948538112,
114.515619172042)) ;
#177487 = CARTESIAN_POINT('Ctrl Pts',(-25.9611123344456,-13.2063007087737,
114.444798177741)) ;
#177488 = CARTESIAN_POINT('Ctrl Pts',(-25.9211552662506,-12.9308185504047,
114.358558160609)) ;
#177489 = CARTESIAN_POINT('Ctrl Pts',(-25.8999242910296,-12.9644269321628,
114.293892034663)) ;
#177490 = CARTESIAN_POINT('Ctrl Pts',(-25.8261204399611,-12.9644268849646,
114.318123053053)) ;
#177491 = CARTESIAN_POINT('Ctrl Pts',(-25.7523165888926,-12.9644268377663,
114.342354071442)) ;
#177492 = CARTESIAN_POINT('Ctrl Pts',(-25.7735475641136,-12.9308184560083,
114.407020197389)) ;
#177493 = CARTESIAN_POINT('Ctrl Pts',(-25.7947785393346,-12.8972100742503,
114.471686323335)) ;
#177494 = CARTESIAN_POINT('Ctrl Pts',(-25.8685823904031,-12.8972101214485,
114.447455304946)) ;
#177495 = CARTESIAN_POINT('Ctrl Pts',(-25.9423862414716,-12.8972101686467,
114.423224286556)) ;
#177496 = CARTESIAN_POINT('Ctrl Pts',(-25.9211552662506,-12.9308185504047,
114.358558160609)) ;
#177497 = CARTESIAN_POINT('Ctrl Pts',(-25.8593713827175,-12.690040453889,
114.205882675566)) ;
#177498 = CARTESIAN_POINT('Ctrl Pts',(-25.8416872490551,-12.7405114660654,
114.152019656903)) ;
#177499 = CARTESIAN_POINT('Ctrl Pts',(-25.7678833962727,-12.7405114337976,
114.176250670072)) ;
#177500 = CARTESIAN_POINT('Ctrl Pts',(-25.6940795434902,-12.7405114015298,
114.200481683241)) ;
#177501 = CARTESIAN_POINT('Ctrl Pts',(-25.7117636771525,-12.6900403893535,
114.254344701904)) ;
#177502 = CARTESIAN_POINT('Ctrl Pts',(-25.7294478108148,-12.6395693771771,
114.308207720567)) ;
#177503 = CARTESIAN_POINT('Ctrl Pts',(-25.8032516635973,-12.6395694094449,
114.283976707398)) ;
#177504 = CARTESIAN_POINT('Ctrl Pts',(-25.8770555163798,-12.6395694417127,
114.259745694229)) ;
#177505 = CARTESIAN_POINT('Ctrl Pts',(-25.8593713827175,-12.690040453889,
114.205882675566)) ;
#177506 = CARTESIAN_POINT('Ctrl Pts',(-25.7799037685495,-12.5021903792694,
113.999176989546)) ;
#177507 = CARTESIAN_POINT('Ctrl Pts',(-25.7670102007119,-12.5658538076965,
113.959905261575)) ;
#177508 = CARTESIAN_POINT('Ctrl Pts',(-25.6932063475663,-12.5658537885695,
113.984136273638)) ;
#177509 = CARTESIAN_POINT('Ctrl Pts',(-25.6194024944207,-12.5658537694425,
114.008367285701)) ;
#177510 = CARTESIAN_POINT('Ctrl Pts',(-25.6322960622582,-12.5021903410154,
114.047639013672)) ;
#177511 = CARTESIAN_POINT('Ctrl Pts',(-25.6451896300958,-12.4385269125883,
114.086910741644)) ;
#177512 = CARTESIAN_POINT('Ctrl Pts',(-25.7189934832414,-12.4385269317153,
114.06267972958)) ;
#177513 = CARTESIAN_POINT('Ctrl Pts',(-25.792797336387,-12.4385269508424,
114.038448717517)) ;
#177514 = CARTESIAN_POINT('Ctrl Pts',(-25.7799037685495,-12.5021903792694,
113.999176989546)) ;
#177515 = CARTESIAN_POINT('Ctrl Pts',(-25.6868876116915,-12.3790435207342,
113.751397700364)) ;
#177516 = CARTESIAN_POINT('Ctrl Pts',(-25.6797338653771,-12.4514021719633,
113.729608542811)) ;
#177517 = CARTESIAN_POINT('Ctrl Pts',(-25.6059300136845,-12.4514021645019,
113.7538395593)) ;
#177518 = CARTESIAN_POINT('Ctrl Pts',(-25.5321261619918,-12.4514021570405,
113.778070575788)) ;
#177519 = CARTESIAN_POINT('Ctrl Pts',(-25.5392799083062,-12.3790435058114,
113.799859733342)) ;
#177520 = CARTESIAN_POINT('Ctrl Pts',(-25.5464336546206,-12.3066848545823,
113.821648890895)) ;
#177521 = CARTESIAN_POINT('Ctrl Pts',(-25.6202375063133,-12.3066848620437,
113.797417874406)) ;
#177522 = CARTESIAN_POINT('Ctrl Pts',(-25.6940413580059,-12.3066848695051,
113.773186857918)) ;
#177523 = CARTESIAN_POINT('Ctrl Pts',(-25.6868876116915,-12.3790435207342,
113.751397700364)) ;
#177524 = CARTESIAN_POINT('Ctrl Pts',(-25.5868978508818,-12.3305042760163,
113.482273898361)) ;
#177525 = CARTESIAN_POINT('Ctrl Pts',(-25.5859817904188,-12.4063616289538,
113.479483725613)) ;
#177526 = CARTESIAN_POINT('Ctrl Pts',(-25.5121779408216,-12.4063616290811,
113.503714748484)) ;
#177527 = CARTESIAN_POINT('Ctrl Pts',(-25.4383740912243,-12.4063616292084,
113.527945771355)) ;
#177528 = CARTESIAN_POINT('Ctrl Pts',(-25.4392901516873,-12.3305042762709,
113.530735944103)) ;
#177529 = CARTESIAN_POINT('Ctrl Pts',(-25.4402062121503,-12.2546469233334,
113.533526116851)) ;
#177530 = CARTESIAN_POINT('Ctrl Pts',(-25.5140100617475,-12.2546469232061,
113.50929509398)) ;
#177531 = CARTESIAN_POINT('Ctrl Pts',(-25.5878139113448,-12.2546469230788,
113.48506407111)) ;
#177532 = CARTESIAN_POINT('Ctrl Pts',(-25.5868978508818,-12.3305042760163,
113.482273898361)) ;
#177533 = CARTESIAN_POINT('Ctrl Pts',(-25.4854179660145,-12.3604684800267,
113.208869990196)) ;
#177534 = CARTESIAN_POINT('Ctrl Pts',(-25.4908479731161,-12.434348796245,
113.225408915486)) ;
#177535 = CARTESIAN_POINT('Ctrl Pts',(-25.4170441264006,-12.4343487994094,
113.249639947135)) ;
#177536 = CARTESIAN_POINT('Ctrl Pts',(-25.3432402796852,-12.4343488025737,
113.273870978783)) ;
#177537 = CARTESIAN_POINT('Ctrl Pts',(-25.3378102725836,-12.3604684863554,
113.257332053493)) ;
#177538 = CARTESIAN_POINT('Ctrl Pts',(-25.332380265482,-12.2865881701371,
113.240793128203)) ;
#177539 = CARTESIAN_POINT('Ctrl Pts',(-25.4061841121974,-12.2865881669728,
113.216562096555)) ;
#177540 = CARTESIAN_POINT('Ctrl Pts',(-25.4799879589129,-12.2865881638084,
113.192331064906)) ;
#177541 = CARTESIAN_POINT('Ctrl Pts',(-25.4854179660145,-12.3604684800267,
113.208869990196)) ;
#177542 = CARTESIAN_POINT('Ctrl Pts',(-25.3908722354269,-12.4650891112354,
112.956114236995)) ;
#177543 = CARTESIAN_POINT('Ctrl Pts',(-25.4021832258839,-12.5317749496589,
112.990565688778)) ;
#177544 = CARTESIAN_POINT('Ctrl Pts',(-25.3283793807559,-12.5317749532163,
113.014796725262)) ;
#177545 = CARTESIAN_POINT('Ctrl Pts',(-25.254575535628,-12.5317749567737,
113.039027761745)) ;
#177546 = CARTESIAN_POINT('Ctrl Pts',(-25.2432645451709,-12.4650891183502,
113.004576309962)) ;
#177547 = CARTESIAN_POINT('Ctrl Pts',(-25.2319535547139,-12.3984032799266,
112.970124858178)) ;
#177548 = CARTESIAN_POINT('Ctrl Pts',(-25.3057573998419,-12.3984032763692,
112.945893821695)) ;
#177549 = CARTESIAN_POINT('Ctrl Pts',(-25.3795612449698,-12.3984032728119,
112.921662785211)) ;
#177550 = CARTESIAN_POINT('Ctrl Pts',(-25.3908722354269,-12.4650891112354,
112.956114236995)) ;
#177551 = CARTESIAN_POINT('Ctrl Pts',(-25.3069218934639,-12.6397680496829,
112.736110244212)) ;
#177552 = CARTESIAN_POINT('Ctrl Pts',(-25.3233734025477,-12.6943569653302,
112.786218886429)) ;
#177553 = CARTESIAN_POINT('Ctrl Pts',(-25.2495695590936,-12.6943569660359,
112.810449928011)) ;
#177554 = CARTESIAN_POINT('Ctrl Pts',(-25.1757657156394,-12.6943569667415,
112.834680969593)) ;
#177555 = CARTESIAN_POINT('Ctrl Pts',(-25.1593142065557,-12.6397680510942,
112.784572327376)) ;
#177556 = CARTESIAN_POINT('Ctrl Pts',(-25.1428626974719,-12.5851791354469,
112.734463685159)) ;
#177557 = CARTESIAN_POINT('Ctrl Pts',(-25.216666540926,-12.5851791347412,
112.710232643577)) ;
#177558 = CARTESIAN_POINT('Ctrl Pts',(-25.2904703843801,-12.5851791340356,
112.686001601995)) ;
#177559 = CARTESIAN_POINT('Ctrl Pts',(-25.3069218934639,-12.6397680496829,
112.736110244212)) ;
#177560 = CARTESIAN_POINT('Ctrl Pts',(-25.2409292762661,-12.8673926753431,
112.570297954244)) ;
#177561 = CARTESIAN_POINT('Ctrl Pts',(-25.2612849273591,-12.9061686393151,
112.632297983135)) ;
#177562 = CARTESIAN_POINT('Ctrl Pts',(-25.1874810842753,-12.9061686378558,
112.656529025845)) ;
#177563 = CARTESIAN_POINT('Ctrl Pts',(-25.1136772411915,-12.9061686363964,
112.680760068555)) ;
#177564 = CARTESIAN_POINT('Ctrl Pts',(-25.0933215900984,-12.8673926724244,
112.618760039664)) ;
#177565 = CARTESIAN_POINT('Ctrl Pts',(-25.0729659390053,-12.8286167084523,
112.556760010772)) ;
#177566 = CARTESIAN_POINT('Ctrl Pts',(-25.1467697820891,-12.8286167099117,
112.532528968062)) ;
#177567 = CARTESIAN_POINT('Ctrl Pts',(-25.220573625173,-12.828616711371,112.508297925353)) ;
#177568 = CARTESIAN_POINT('Ctrl Pts',(-25.2409292762661,-12.8673926753431,
112.570297954244)) ;
#177569 = CARTESIAN_POINT('Ctrl Pts',(-25.1950431269417,-13.138383085188,
112.466309655478)) ;
#177570 = CARTESIAN_POINT('Ctrl Pts',(-25.2178932655646,-13.1582932670834,
112.535907490935)) ;
#177571 = CARTESIAN_POINT('Ctrl Pts',(-25.1440894224487,-13.15829326372,112.560138533547)) ;
#177572 = CARTESIAN_POINT('Ctrl Pts',(-25.0702855793329,-13.1582932603565,
112.58436957616)) ;
#177573 = CARTESIAN_POINT('Ctrl Pts',(-25.04743544071,-13.1383830784611,112.514771740703)) ;
#177574 = CARTESIAN_POINT('Ctrl Pts',(-25.0245853020871,-13.1184728965658,
112.445173905246)) ;
#177575 = CARTESIAN_POINT('Ctrl Pts',(-25.0983891452029,-13.1184728999292,
112.420942862634)) ;
#177576 = CARTESIAN_POINT('Ctrl Pts',(-25.1721929883188,-13.1184729032926,
112.396711820022)) ;
#177577 = CARTESIAN_POINT('Ctrl Pts',(-25.1950431269417,-13.138383085188,
112.466309655478)) ;
#177578 = CARTESIAN_POINT('Ctrl Pts',(-25.1732970592646,-13.4250580301084,
112.435262725168)) ;
#177579 = CARTESIAN_POINT('Ctrl Pts',(-25.1969709139446,-13.4249798616491,
112.507369466809)) ;
#177580 = CARTESIAN_POINT('Ctrl Pts',(-25.123167070483,-13.4249798591319,
112.531600508368)) ;
#177581 = CARTESIAN_POINT('Ctrl Pts',(-25.0493632270214,-13.4249798566146,
112.555831549927)) ;
#177582 = CARTESIAN_POINT('Ctrl Pts',(-25.0256893723414,-13.4250580250739,
112.483724808286)) ;
#177583 = CARTESIAN_POINT('Ctrl Pts',(-25.0020155176614,-13.4251361935332,
112.411618066645)) ;
#177584 = CARTESIAN_POINT('Ctrl Pts',(-25.075819361123,-13.4251361960505,
112.387387025086)) ;
#177585 = CARTESIAN_POINT('Ctrl Pts',(-25.1496232045846,-13.4251361985678,
112.363155983527)) ;
#177586 = CARTESIAN_POINT('Ctrl Pts',(-25.1732970592646,-13.4250580301084,
112.435262725168)) ;
#177587 = CARTESIAN_POINT('Ctrl Pts',(-25.175431424128,-13.713663843469,112.477262712461)) ;
#177588 = CARTESIAN_POINT('Ctrl Pts',(-25.1982564463558,-13.6934329579285,
112.546784047362)) ;
#177589 = CARTESIAN_POINT('Ctrl Pts',(-25.1244526028314,-13.6934329580841,
112.57101508873)) ;
#177590 = CARTESIAN_POINT('Ctrl Pts',(-25.0506487593069,-13.6934329582396,
112.595246130098)) ;
#177591 = CARTESIAN_POINT('Ctrl Pts',(-25.0278237370791,-13.7136638437801,
112.525724795196)) ;
#177592 = CARTESIAN_POINT('Ctrl Pts',(-25.0049987148513,-13.7338947293205,
112.456203460295)) ;
#177593 = CARTESIAN_POINT('Ctrl Pts',(-25.0788025583757,-13.733894729165,
112.431972418927)) ;
#177594 = CARTESIAN_POINT('Ctrl Pts',(-25.1526064019001,-13.7338947290095,
112.407741377559)) ;
#177595 = CARTESIAN_POINT('Ctrl Pts',(-25.175431424128,-13.713663843469,112.477262712461)) ;
#177596 = CARTESIAN_POINT('Ctrl Pts',(-25.2013058612131,-13.9818996954329,
112.591702432285)) ;
#177597 = CARTESIAN_POINT('Ctrl Pts',(-25.2216202953023,-13.9429089187137,
112.653576920689)) ;
#177598 = CARTESIAN_POINT('Ctrl Pts',(-25.147816452688,-13.9429089238121,
112.677807964829)) ;
#177599 = CARTESIAN_POINT('Ctrl Pts',(-25.0740126100738,-13.9429089289105,
112.702039008969)) ;
#177600 = CARTESIAN_POINT('Ctrl Pts',(-25.0536981759845,-13.9818997056297,
112.640164520565)) ;
#177601 = CARTESIAN_POINT('Ctrl Pts',(-25.0333837418953,-14.0208904823489,
112.578290032162)) ;
#177602 = CARTESIAN_POINT('Ctrl Pts',(-25.1071875845096,-14.0208904772505,
112.554058988022)) ;
#177603 = CARTESIAN_POINT('Ctrl Pts',(-25.1809914271238,-14.0208904721521,
112.529827943882)) ;
#177604 = CARTESIAN_POINT('Ctrl Pts',(-25.2013058612131,-13.9818996954329,
112.591702432285)) ;
#177605 = CARTESIAN_POINT('Ctrl Pts',(-25.2475462461254,-14.2073240866329,
112.767809158823)) ;
#177606 = CARTESIAN_POINT('Ctrl Pts',(-25.2639316742078,-14.1525370337597,
112.817716528783)) ;
#177607 = CARTESIAN_POINT('Ctrl Pts',(-25.1901278330324,-14.1525370412397,
112.841947577306)) ;
#177608 = CARTESIAN_POINT('Ctrl Pts',(-25.116323991857,-14.1525370487197,
112.866178625828)) ;
#177609 = CARTESIAN_POINT('Ctrl Pts',(-25.0999385637746,-14.2073241015929,
112.816271255868)) ;
#177610 = CARTESIAN_POINT('Ctrl Pts',(-25.0835531356922,-14.2621111544661,
112.766363885908)) ;
#177611 = CARTESIAN_POINT('Ctrl Pts',(-25.1573569768676,-14.2621111469861,
112.742132837385)) ;
#177612 = CARTESIAN_POINT('Ctrl Pts',(-25.2311608180431,-14.2621111395061,
112.717901788863)) ;
#177613 = CARTESIAN_POINT('Ctrl Pts',(-25.2475462461254,-14.2073240866329,
112.767809158823)) ;
#177614 = CARTESIAN_POINT('Ctrl Pts',(-25.3107801482558,-14.3779496982449,
112.995927736214)) ;
#177615 = CARTESIAN_POINT('Ctrl Pts',(-25.3220392060266,-14.3111692669398,
113.030221009202)) ;
#177616 = CARTESIAN_POINT('Ctrl Pts',(-25.2482353673534,-14.3111692758398,
113.054452065346)) ;
#177617 = CARTESIAN_POINT('Ctrl Pts',(-25.1744315286803,-14.3111692847398,
113.07868312149)) ;
#177618 = CARTESIAN_POINT('Ctrl Pts',(-25.1631724709095,-14.3779497160448,
113.044389848502)) ;
#177619 = CARTESIAN_POINT('Ctrl Pts',(-25.1519134131387,-14.4447301473499,
113.010096575515)) ;
#177620 = CARTESIAN_POINT('Ctrl Pts',(-25.2257172518118,-14.4447301384499,
112.985865519371)) ;
#177621 = CARTESIAN_POINT('Ctrl Pts',(-25.299521090485,-14.4447301295499,
112.961634463227)) ;
#177622 = CARTESIAN_POINT('Ctrl Pts',(-25.3107801482558,-14.3779496982449,
112.995927736214)) ;
#177623 = CARTESIAN_POINT('Ctrl Pts',(-25.3855441089235,-14.4795452062324,
113.25916632019)) ;
#177624 = CARTESIAN_POINT('Ctrl Pts',(-25.390864299521,-14.405574238108,113.27537076184)) ;
#177625 = CARTESIAN_POINT('Ctrl Pts',(-25.3170604639442,-14.4055742445888,
113.299601827415)) ;
#177626 = CARTESIAN_POINT('Ctrl Pts',(-25.2432566283675,-14.4055742510696,
113.32383289299)) ;
#177627 = CARTESIAN_POINT('Ctrl Pts',(-25.23793643777,-14.4795452191939,113.30762845134)) ;
#177628 = CARTESIAN_POINT('Ctrl Pts',(-25.2326162471725,-14.5535161873183,
113.291424009691)) ;
#177629 = CARTESIAN_POINT('Ctrl Pts',(-25.3064200827493,-14.5535161808375,
113.267192944116)) ;
#177630 = CARTESIAN_POINT('Ctrl Pts',(-25.3802239183261,-14.5535161743567,
113.242961878541)) ;
#177631 = CARTESIAN_POINT('Ctrl Pts',(-25.3855441089235,-14.4795452062324,
113.25916632019)) ;
#177632 = CARTESIAN_POINT('Ctrl Pts',(-25.4657056298432,-14.504675613756,
113.538873967324)) ;
#177633 = CARTESIAN_POINT('Ctrl Pts',(-25.4647009460347,-14.4288427645242,
113.53581386187)) ;
#177634 = CARTESIAN_POINT('Ctrl Pts',(-25.3908971135579,-14.4288427635045,
113.560044936887)) ;
#177635 = CARTESIAN_POINT('Ctrl Pts',(-25.3170932810811,-14.4288427624848,
113.584276011904)) ;
#177636 = CARTESIAN_POINT('Ctrl Pts',(-25.3180979648896,-14.5046756117167,
113.587336117358)) ;
#177637 = CARTESIAN_POINT('Ctrl Pts',(-25.3191026486981,-14.5805084609485,
113.590396222811)) ;
#177638 = CARTESIAN_POINT('Ctrl Pts',(-25.3929064811749,-14.5805084619682,
113.566165147794)) ;
#177639 = CARTESIAN_POINT('Ctrl Pts',(-25.4667103136517,-14.5805084629879,
113.541934072777)) ;
#177640 = CARTESIAN_POINT('Ctrl Pts',(-25.4657056298432,-14.504675613756,
113.538873967324)) ;
#177641 = CARTESIAN_POINT('Ctrl Pts',(-25.5441348471131,-14.4524935600785,
113.813035826526)) ;
#177642 = CARTESIAN_POINT('Ctrl Pts',(-25.5369228144404,-14.3801950254555,
113.791069137853)) ;
#177643 = CARTESIAN_POINT('Ctrl Pts',(-25.4631189835325,-14.3801950131856,
113.815300217648)) ;
#177644 = CARTESIAN_POINT('Ctrl Pts',(-25.3893151526246,-14.3801950009157,
113.839531297444)) ;
#177645 = CARTESIAN_POINT('Ctrl Pts',(-25.3965271852974,-14.4524935355387,
113.861497986118)) ;
#177646 = CARTESIAN_POINT('Ctrl Pts',(-25.4037392179702,-14.5247920701618,
113.883464674792)) ;
#177647 = CARTESIAN_POINT('Ctrl Pts',(-25.477543048878,-14.5247920824317,
113.859233594996)) ;
#177648 = CARTESIAN_POINT('Ctrl Pts',(-25.5513468797859,-14.5247920947016,
113.8350025152)) ;
#177649 = CARTESIAN_POINT('Ctrl Pts',(-25.5441348471131,-14.4524935600785,
113.813035826526)) ;
#177650 = CARTESIAN_POINT('Ctrl Pts',(-25.6158038670484,-14.3253673837965,
114.066976143731)) ;
#177651 = CARTESIAN_POINT('Ctrl Pts',(-25.6028398302001,-14.2618396984513,
114.027489778218)) ;
#177652 = CARTESIAN_POINT('Ctrl Pts',(-25.5290360005822,-14.2618396702595,
114.051720861943)) ;
#177653 = CARTESIAN_POINT('Ctrl Pts',(-25.4552321709644,-14.2618396420677,
114.075951945668)) ;
#177654 = CARTESIAN_POINT('Ctrl Pts',(-25.4681962078127,-14.325367327413,
114.115438311181)) ;
#177655 = CARTESIAN_POINT('Ctrl Pts',(-25.481160244661,-14.3888950127582,
114.154924676695)) ;
#177656 = CARTESIAN_POINT('Ctrl Pts',(-25.5549640742788,-14.38889504095,114.13069359297)) ;
#177657 = CARTESIAN_POINT('Ctrl Pts',(-25.6287679038966,-14.3888950691418,
114.106462509245)) ;
#177658 = CARTESIAN_POINT('Ctrl Pts',(-25.6158038670484,-14.3253673837965,
114.066976143731)) ;
#177659 = CARTESIAN_POINT('Ctrl Pts',(-25.6735934060056,-14.1335026343525,
114.278447647152)) ;
#177660 = CARTESIAN_POINT('Ctrl Pts',(-25.6558422293983,-14.0832788793335,
114.224380426171)) ;
#177661 = CARTESIAN_POINT('Ctrl Pts',(-25.5820383986289,-14.0832788338596,
114.248611506388)) ;
#177662 = CARTESIAN_POINT('Ctrl Pts',(-25.5082345678594,-14.0832787883857,
114.272842586606)) ;
#177663 = CARTESIAN_POINT('Ctrl Pts',(-25.5259857444668,-14.1335025434047,
114.326909807587)) ;
#177664 = CARTESIAN_POINT('Ctrl Pts',(-25.5437369210741,-14.1837262984236,
114.380977028568)) ;
#177665 = CARTESIAN_POINT('Ctrl Pts',(-25.6175407518436,-14.1837263438975,
114.356745948351)) ;
#177666 = CARTESIAN_POINT('Ctrl Pts',(-25.691344582613,-14.1837263893715,
114.332514868133)) ;
#177667 = CARTESIAN_POINT('Ctrl Pts',(-25.6735934060056,-14.1335026343525,
114.278447647152)) ;
#177668 = CARTESIAN_POINT('Ctrl Pts',(-25.713031726844,-13.8914689377216,
114.433910815975)) ;
#177669 = CARTESIAN_POINT('Ctrl Pts',(-25.6917702020142,-13.8580710694063,
114.369151640563)) ;
#177670 = CARTESIAN_POINT('Ctrl Pts',(-25.6179663680164,-13.8580710084392,
114.393382710947)) ;
#177671 = CARTESIAN_POINT('Ctrl Pts',(-25.5441625340186,-13.8580709474722,
114.417613781332)) ;
#177672 = CARTESIAN_POINT('Ctrl Pts',(-25.5654240588485,-13.8914688157875,
114.482372956744)) ;
#177673 = CARTESIAN_POINT('Ctrl Pts',(-25.5866855836783,-13.9248666841028,
114.547132132156)) ;
#177674 = CARTESIAN_POINT('Ctrl Pts',(-25.6604894176761,-13.9248667450698,
114.522901061771)) ;
#177675 = CARTESIAN_POINT('Ctrl Pts',(-25.7342932516738,-13.9248668060369,
114.498669991387)) ;
#177676 = CARTESIAN_POINT('Ctrl Pts',(-25.713031726844,-13.8914689377216,
114.433910815975)) ;
#177677 = CARTESIAN_POINT('Ctrl Pts',(-25.7307687812816,-13.6147208150664,
114.523401386807)) ;
#177678 = CARTESIAN_POINT('Ctrl Pts',(-25.7075042451934,-13.6005963890855,
114.452541362134)) ;
#177679 = CARTESIAN_POINT('Ctrl Pts',(-25.6337004062679,-13.6005963145347,
114.476772417509)) ;
#177680 = CARTESIAN_POINT('Ctrl Pts',(-25.5598965673424,-13.600596239984,
114.501003472884)) ;
#177681 = CARTESIAN_POINT('Ctrl Pts',(-25.5831611034306,-13.6147206659649,
114.571863497557)) ;
#177682 = CARTESIAN_POINT('Ctrl Pts',(-25.6064256395188,-13.6288450919457,
114.64272352223)) ;
#177683 = CARTESIAN_POINT('Ctrl Pts',(-25.6802294784443,-13.6288451664965,
114.618492466855)) ;
#177684 = CARTESIAN_POINT('Ctrl Pts',(-25.7540333173698,-13.6288452410473,
114.59426141148)) ;
#177685 = CARTESIAN_POINT('Ctrl Pts',(-25.7307687812816,-13.6147208150664,
114.523401386807)) ;
#177686 = CARTESIAN_POINT('Ctrl Pts',(-25.7245757601632,-13.3237687258409,
114.540012491979)) ;
#177687 = CARTESIAN_POINT('Ctrl Pts',(-25.7009758198009,-13.3299371797537,
114.468130879862)) ;
#177688 = CARTESIAN_POINT('Ctrl Pts',(-25.6271719743241,-13.3299370967314,
114.492361915283)) ;
#177689 = CARTESIAN_POINT('Ctrl Pts',(-25.5533681288474,-13.329937013709,
114.516592950705)) ;
#177690 = CARTESIAN_POINT('Ctrl Pts',(-25.5769680692097,-13.3237685597962,
114.588474562821)) ;
#177691 = CARTESIAN_POINT('Ctrl Pts',(-25.600568009572,-13.3176001058834,
114.660356174938)) ;
#177692 = CARTESIAN_POINT('Ctrl Pts',(-25.6743718550487,-13.3176001889057,
114.636125139517)) ;
#177693 = CARTESIAN_POINT('Ctrl Pts',(-25.7481757005255,-13.3176002719281,
114.611894104095)) ;
#177694 = CARTESIAN_POINT('Ctrl Pts',(-25.7245757601632,-13.3237687258409,
114.540012491979)) ;
#177695 = CARTESIAN_POINT('Ctrl Pts',(-25.6941237439954,-13.0396242352637,
114.482736350999)) ;
#177696 = CARTESIAN_POINT('Ctrl Pts',(-25.671881485573,-13.0656396906541,
114.414990018884)) ;
#177697 = CARTESIAN_POINT('Ctrl Pts',(-25.598077632554,-13.0656396062825,
114.439221031332)) ;
#177698 = CARTESIAN_POINT('Ctrl Pts',(-25.5242737795349,-13.0656395219109,
114.463452043781)) ;
#177699 = CARTESIAN_POINT('Ctrl Pts',(-25.5465160379572,-13.0396240665205,
114.531198375896)) ;
#177700 = CARTESIAN_POINT('Ctrl Pts',(-25.5687582963795,-13.0136086111301,
114.598944708012)) ;
#177701 = CARTESIAN_POINT('Ctrl Pts',(-25.6425621493986,-13.0136086955017,
114.574713695563)) ;
#177702 = CARTESIAN_POINT('Ctrl Pts',(-25.7163660024177,-13.0136087798733,
114.550482683115)) ;
#177703 = CARTESIAN_POINT('Ctrl Pts',(-25.6941237439954,-13.0396242352637,
114.482736350999)) ;
#177704 = CARTESIAN_POINT('Ctrl Pts',(-25.6410851839242,-12.7830678889279,
114.356574719083)) ;
#177705 = CARTESIAN_POINT('Ctrl Pts',(-25.6217813743788,-12.8270330002595,
114.297778428028)) ;
#177706 = CARTESIAN_POINT('Ctrl Pts',(-25.5479775137743,-12.8270329227443,
114.322009417373)) ;
#177707 = CARTESIAN_POINT('Ctrl Pts',(-25.4741736531698,-12.8270328452292,
114.346240406717)) ;
#177708 = CARTESIAN_POINT('Ctrl Pts',(-25.4934774627152,-12.7830677338975,
114.405036697772)) ;
#177709 = CARTESIAN_POINT('Ctrl Pts',(-25.5127812722606,-12.7391026225659,
114.463832988827)) ;
#177710 = CARTESIAN_POINT('Ctrl Pts',(-25.5865851328651,-12.739102700081,
114.439601999483)) ;
#177711 = CARTESIAN_POINT('Ctrl Pts',(-25.6603889934697,-12.7391027775962,
114.415371010139)) ;
#177712 = CARTESIAN_POINT('Ctrl Pts',(-25.6410851839242,-12.7830678889279,
114.356574719083)) ;
#177713 = CARTESIAN_POINT('Ctrl Pts',(-25.5676997033759,-12.5704752635878,
114.168721963641)) ;
#177714 = CARTESIAN_POINT('Ctrl Pts',(-25.5527529624881,-12.6293473017033,
114.123196600596)) ;
#177715 = CARTESIAN_POINT('Ctrl Pts',(-25.4789490946422,-12.6293472382111,
114.147427567884)) ;
#177716 = CARTESIAN_POINT('Ctrl Pts',(-25.4051452267963,-12.6293471747189,
114.171658535172)) ;
#177717 = CARTESIAN_POINT('Ctrl Pts',(-25.4200919676841,-12.5704751366034,
114.217183898218)) ;
#177718 = CARTESIAN_POINT('Ctrl Pts',(-25.4350387085718,-12.5116030984879,
114.262709261263)) ;
#177719 = CARTESIAN_POINT('Ctrl Pts',(-25.5088425764177,-12.5116031619801,
114.238478293975)) ;
#177720 = CARTESIAN_POINT('Ctrl Pts',(-25.5826464442636,-12.5116032254723,
114.214247326686)) ;
#177721 = CARTESIAN_POINT('Ctrl Pts',(-25.5676997033759,-12.5704752635878,
114.168721963641)) ;
#177722 = CARTESIAN_POINT('Ctrl Pts',(-25.4799422590946,-12.4206416986158,
113.936696566694)) ;
#177723 = CARTESIAN_POINT('Ctrl Pts',(-25.4703708909182,-12.490060480766,
113.90754372156)) ;
#177724 = CARTESIAN_POINT('Ctrl Pts',(-25.3965670178971,-12.4900604392227,
113.931774673086)) ;
#177725 = CARTESIAN_POINT('Ctrl Pts',(-25.3227631448761,-12.4900603976793,
113.956005624611)) ;
#177726 = CARTESIAN_POINT('Ctrl Pts',(-25.3323345130525,-12.4206416155292,
113.985158469745)) ;
#177727 = CARTESIAN_POINT('Ctrl Pts',(-25.341905881229,-12.351222833379,114.014311314878)) ;
#177728 = CARTESIAN_POINT('Ctrl Pts',(-25.41570975425,-12.3512228749223,113.990080363353)) ;
#177729 = CARTESIAN_POINT('Ctrl Pts',(-25.4895136272711,-12.3512229164656,
113.965849411827)) ;
#177730 = CARTESIAN_POINT('Ctrl Pts',(-25.4799422590946,-12.4206416986158,
113.936696566694)) ;
#177731 = CARTESIAN_POINT('Ctrl Pts',(-25.381998179666,-12.3408954926335,
113.673866420762)) ;
#177732 = CARTESIAN_POINT('Ctrl Pts',(-25.3785163984105,-12.4159838825569,
113.663261474782)) ;
#177733 = CARTESIAN_POINT('Ctrl Pts',(-25.3047125221132,-12.4159838672949,
113.687492416329)) ;
#177734 = CARTESIAN_POINT('Ctrl Pts',(-25.2309086458159,-12.4159838520328,
113.711723357875)) ;
#177735 = CARTESIAN_POINT('Ctrl Pts',(-25.2343904270714,-12.3408954621094,
113.722328303855)) ;
#177736 = CARTESIAN_POINT('Ctrl Pts',(-25.2378722083269,-12.265807072186,
113.732933249835)) ;
#177737 = CARTESIAN_POINT('Ctrl Pts',(-25.3116760846242,-12.265807087448,
113.708702308288)) ;
#177738 = CARTESIAN_POINT('Ctrl Pts',(-25.3854799609215,-12.26580710271,113.684471366741)) ;
#177739 = CARTESIAN_POINT('Ctrl Pts',(-25.381998179666,-12.3408954926335,
113.673866420762)) ;
#177740 = CARTESIAN_POINT('Ctrl Pts',(-25.2803675767541,-12.3388375024718,
113.399883536457)) ;
#177741 = CARTESIAN_POINT('Ctrl Pts',(-25.2832401365507,-12.4141806587766,
113.408632888022)) ;
#177742 = CARTESIAN_POINT('Ctrl Pts',(-25.2094362596863,-12.414180672439,
113.432863827842)) ;
#177743 = CARTESIAN_POINT('Ctrl Pts',(-25.1356323828219,-12.4141806861015,
113.457094767661)) ;
#177744 = CARTESIAN_POINT('Ctrl Pts',(-25.1327598230253,-12.3388375297967,
113.448345416096)) ;
#177745 = CARTESIAN_POINT('Ctrl Pts',(-25.1298872632288,-12.263494373492,
113.439596064531)) ;
#177746 = CARTESIAN_POINT('Ctrl Pts',(-25.2036911400932,-12.2634943598295,
113.415365124712)) ;
#177747 = CARTESIAN_POINT('Ctrl Pts',(-25.2774950169575,-12.2634943461671,
113.391134184892)) ;
#177748 = CARTESIAN_POINT('Ctrl Pts',(-25.2803675767541,-12.3388375024718,
113.399883536457)) ;
#177749 = CARTESIAN_POINT('Ctrl Pts',(-25.1823213194761,-12.413706142133,
113.136628920894)) ;
#177750 = CARTESIAN_POINT('Ctrl Pts',(-25.1913113188617,-12.4839334398815,
113.164011006395)) ;
#177751 = CARTESIAN_POINT('Ctrl Pts',(-25.1175074442267,-12.4839334817003,
113.188241953004)) ;
#177752 = CARTESIAN_POINT('Ctrl Pts',(-25.0437035695917,-12.4839335235192,
113.212472899614)) ;
#177753 = CARTESIAN_POINT('Ctrl Pts',(-25.0347135702062,-12.4137062257707,
113.185090814114)) ;
#177754 = CARTESIAN_POINT('Ctrl Pts',(-25.0257235708206,-12.3434789280223,
113.157708728613)) ;
#177755 = CARTESIAN_POINT('Ctrl Pts',(-25.0995274454556,-12.3434788862035,
113.133477782003)) ;
#177756 = CARTESIAN_POINT('Ctrl Pts',(-25.1733313200905,-12.3434788443846,
113.109246835393)) ;
#177757 = CARTESIAN_POINT('Ctrl Pts',(-25.1823213194761,-12.413706142133,
113.136628920894)) ;
#177758 = CARTESIAN_POINT('Ctrl Pts',(-25.092980715359,-12.5617183582742,
112.900167957605)) ;
#177759 = CARTESIAN_POINT('Ctrl Pts',(-25.1074837531034,-12.6217168854957,
112.944341868443)) ;
#177760 = CARTESIAN_POINT('Ctrl Pts',(-25.0336798833631,-12.6217169518503,
112.968572829961)) ;
#177761 = CARTESIAN_POINT('Ctrl Pts',(-24.9598760136228,-12.6217170182048,
112.992803791479)) ;
#177762 = CARTESIAN_POINT('Ctrl Pts',(-24.9453729758784,-12.5617184909834,
112.948629880641)) ;
#177763 = CARTESIAN_POINT('Ctrl Pts',(-24.930869938134,-12.501719963762,112.904455969803)) ;
#177764 = CARTESIAN_POINT('Ctrl Pts',(-25.0046738078743,-12.5017198974074,
112.880225008285)) ;
#177765 = CARTESIAN_POINT('Ctrl Pts',(-25.0784776776146,-12.5017198310528,
112.855994046767)) ;
#177766 = CARTESIAN_POINT('Ctrl Pts',(-25.092980715359,-12.5617183582742,
112.900167957605)) ;
#177767 = CARTESIAN_POINT('Ctrl Pts',(-25.0195846393668,-12.7688407831079,
112.711834010416)) ;
#177768 = CARTESIAN_POINT('Ctrl Pts',(-25.0385047320968,-12.8144672602671,
112.76946155808)) ;
#177769 = CARTESIAN_POINT('Ctrl Pts',(-24.964700869039,-12.8144673453734,
112.793692539952)) ;
#177770 = CARTESIAN_POINT('Ctrl Pts',(-24.8908970059813,-12.8144674304797,
112.817923521824)) ;
#177771 = CARTESIAN_POINT('Ctrl Pts',(-24.8719769132512,-12.7688409533206,
112.76029597416)) ;
#177772 = CARTESIAN_POINT('Ctrl Pts',(-24.8530568205212,-12.7232144761614,
112.702668426497)) ;
#177773 = CARTESIAN_POINT('Ctrl Pts',(-24.926860683579,-12.7232143910551,
112.678437444625)) ;
#177774 = CARTESIAN_POINT('Ctrl Pts',(-25.0006645466367,-12.7232143059487,
112.654206462753)) ;
#177775 = CARTESIAN_POINT('Ctrl Pts',(-25.0195846393668,-12.7688407831079,
112.711834010416)) ;
#177776 = CARTESIAN_POINT('Ctrl Pts',(-24.9649866794184,-13.0241117816514,
112.581077125632)) ;
#177777 = CARTESIAN_POINT('Ctrl Pts',(-24.9870115430439,-13.0519843902153,
112.648161304551)) ;
#177778 = CARTESIAN_POINT('Ctrl Pts',(-24.9132076881355,-13.0519844861314,
112.672392311245)) ;
#177779 = CARTESIAN_POINT('Ctrl Pts',(-24.839403833227,-13.0519845820475,
112.696623317938)) ;
#177780 = CARTESIAN_POINT('Ctrl Pts',(-24.8173789696015,-13.0241119734836,
112.629539139019)) ;
#177781 = CARTESIAN_POINT('Ctrl Pts',(-24.795354105976,-12.9962393649197,
112.5624549601)) ;
#177782 = CARTESIAN_POINT('Ctrl Pts',(-24.8691579608845,-12.9962392690036,
112.538223953407)) ;
#177783 = CARTESIAN_POINT('Ctrl Pts',(-24.9429618157929,-12.9962391730874,
112.513992946713)) ;
#177784 = CARTESIAN_POINT('Ctrl Pts',(-24.9649866794184,-13.0241117816514,
112.581077125632)) ;
#177785 = CARTESIAN_POINT('Ctrl Pts',(-24.9332536836434,-13.3070010234793,
112.51985755415)) ;
#177786 = CARTESIAN_POINT('Ctrl Pts',(-24.9567938392213,-13.31516473517,112.591557067941)) ;
#177787 = CARTESIAN_POINT('Ctrl Pts',(-24.8829899928049,-13.3151648334865,
112.6157881005)) ;
#177788 = CARTESIAN_POINT('Ctrl Pts',(-24.8091861463885,-13.315164931803,
112.640019133059)) ;
#177789 = CARTESIAN_POINT('Ctrl Pts',(-24.7856459908106,-13.3070012201123,
112.568319619268)) ;
#177790 = CARTESIAN_POINT('Ctrl Pts',(-24.7621058352326,-13.2988375084216,
112.496620105477)) ;
#177791 = CARTESIAN_POINT('Ctrl Pts',(-24.8359096816491,-13.2988374101051,
112.472389072918)) ;
#177792 = CARTESIAN_POINT('Ctrl Pts',(-24.9097135280655,-13.2988373117886,
112.448158040359)) ;
#177793 = CARTESIAN_POINT('Ctrl Pts',(-24.9332536836434,-13.3070010234793,
112.51985755415)) ;
#177794 = CARTESIAN_POINT('Ctrl Pts',(-24.925629722327,-13.5985554109386,
112.532164471356)) ;
#177795 = CARTESIAN_POINT('Ctrl Pts',(-24.9490024367954,-13.5863758262572,
112.603353986648)) ;
#177796 = CARTESIAN_POINT('Ctrl Pts',(-24.8751985984021,-13.5863759182584,
112.627585043645)) ;
#177797 = CARTESIAN_POINT('Ctrl Pts',(-24.8013947600088,-13.5863760102596,
112.651816100641)) ;
#177798 = CARTESIAN_POINT('Ctrl Pts',(-24.7780220455404,-13.5985555949411,
112.580626585349)) ;
#177799 = CARTESIAN_POINT('Ctrl Pts',(-24.754649331072,-13.6107351796225,
112.509437070056)) ;
#177800 = CARTESIAN_POINT('Ctrl Pts',(-24.8284531694653,-13.6107350876213,
112.48520601306)) ;
#177801 = CARTESIAN_POINT('Ctrl Pts',(-24.9022570078586,-13.6107349956201,
112.460974956064)) ;
#177802 = CARTESIAN_POINT('Ctrl Pts',(-24.925629722327,-13.5985554109386,
112.532164471356)) ;
#177803 = CARTESIAN_POINT('Ctrl Pts',(-24.9421245854702,-13.8770852609277,
112.617931075453)) ;
#177804 = CARTESIAN_POINT('Ctrl Pts',(-24.9636458203389,-13.8454408144546,
112.683481282746)) ;
#177805 = CARTESIAN_POINT('Ctrl Pts',(-24.8898419885264,-13.8454408929621,
112.707712359786)) ;
#177806 = CARTESIAN_POINT('Ctrl Pts',(-24.8160381567138,-13.8454409714697,
112.731943436827)) ;
#177807 = CARTESIAN_POINT('Ctrl Pts',(-24.7945169218452,-13.8770854179428,
112.666393229534)) ;
#177808 = CARTESIAN_POINT('Ctrl Pts',(-24.7729956869765,-13.9087298644159,
112.600843022241)) ;
#177809 = CARTESIAN_POINT('Ctrl Pts',(-24.846799518789,-13.9087297859083,
112.576611945201)) ;
#177810 = CARTESIAN_POINT('Ctrl Pts',(-24.9206033506015,-13.9087297074008,
112.552380868161)) ;
#177811 = CARTESIAN_POINT('Ctrl Pts',(-24.9421245854702,-13.8770852609277,
112.617931075453)) ;
#177812 = CARTESIAN_POINT('Ctrl Pts',(-24.9804514510273,-14.1214182763711,
112.770005884966)) ;
#177813 = CARTESIAN_POINT('Ctrl Pts',(-24.9985978942237,-14.0726671201406,
112.825277021458)) ;
#177814 = CARTESIAN_POINT('Ctrl Pts',(-24.9247940672919,-14.0726671815673,
112.849508113365)) ;
#177815 = CARTESIAN_POINT('Ctrl Pts',(-24.8509902403602,-14.072667242994,
112.873739205271)) ;
#177816 = CARTESIAN_POINT('Ctrl Pts',(-24.8328437971638,-14.1214183992245,
112.818468068778)) ;
#177817 = CARTESIAN_POINT('Ctrl Pts',(-24.8146973539674,-14.170169555455,
112.763196932286)) ;
#177818 = CARTESIAN_POINT('Ctrl Pts',(-24.8885011808991,-14.1701694940283,
112.738965840379)) ;
#177819 = CARTESIAN_POINT('Ctrl Pts',(-24.9623050078308,-14.1701694326015,
112.714734748473)) ;
#177820 = CARTESIAN_POINT('Ctrl Pts',(-24.9804514510273,-14.1214182763711,
112.770005884966)) ;
#177821 = CARTESIAN_POINT('Ctrl Pts',(-25.0373635997591,-14.3164119676812,
112.978804934412)) ;
#177822 = CARTESIAN_POINT('Ctrl Pts',(-25.0508302922444,-14.2539728440819,
113.019822305455)) ;
#177823 = CARTESIAN_POINT('Ctrl Pts',(-24.9770264679556,-14.2539728850066,
113.044053405412)) ;
#177824 = CARTESIAN_POINT('Ctrl Pts',(-24.9032226436669,-14.2539729259314,
113.068284505368)) ;
#177825 = CARTESIAN_POINT('Ctrl Pts',(-24.8897559511816,-14.3164120495308,
113.027267134325)) ;
#177826 = CARTESIAN_POINT('Ctrl Pts',(-24.8762892586964,-14.3788511731302,
112.986249763282)) ;
#177827 = CARTESIAN_POINT('Ctrl Pts',(-24.9500930829851,-14.3788511322054,
112.962018663326)) ;
#177828 = CARTESIAN_POINT('Ctrl Pts',(-25.0238969072739,-14.3788510912806,
112.937787563369)) ;
#177829 = CARTESIAN_POINT('Ctrl Pts',(-25.0373635997591,-14.3164119676812,
112.978804934412)) ;
#177830 = CARTESIAN_POINT('Ctrl Pts',(-25.1082654742619,-14.4472714989735,
113.230330811616)) ;
#177831 = CARTESIAN_POINT('Ctrl Pts',(-25.1160662154225,-14.3756009231922,
113.254090609297)) ;
#177832 = CARTESIAN_POINT('Ctrl Pts',(-25.042262391181,-14.3756009434077,
113.278321709397)) ;
#177833 = CARTESIAN_POINT('Ctrl Pts',(-24.9684585669394,-14.3756009636232,
113.302552809497)) ;
#177834 = CARTESIAN_POINT('Ctrl Pts',(-24.9606578257788,-14.4472715394045,
113.278793011817)) ;
#177835 = CARTESIAN_POINT('Ctrl Pts',(-24.9528570846181,-14.5189421151858,
113.255033214136)) ;
#177836 = CARTESIAN_POINT('Ctrl Pts',(-25.0266609088597,-14.5189420949703,
113.230802114036)) ;
#177837 = CARTESIAN_POINT('Ctrl Pts',(-25.1004647331012,-14.5189420747548,
113.206571013936)) ;
#177838 = CARTESIAN_POINT('Ctrl Pts',(-25.1082654742619,-14.4472714989735,
113.230330811616)) ;
#177839 = CARTESIAN_POINT('Ctrl Pts',(-25.1868459524037,-14.5039655219921,
113.505134344491)) ;
#177840 = CARTESIAN_POINT('Ctrl Pts',(-25.1884382106034,-14.4282278620231,
113.509984104971)) ;
#177841 = CARTESIAN_POINT('Ctrl Pts',(-25.1146343847165,-14.4282278646451,
113.534215200059)) ;
#177842 = CARTESIAN_POINT('Ctrl Pts',(-25.0408305588296,-14.4282278672671,
113.558446295148)) ;
#177843 = CARTESIAN_POINT('Ctrl Pts',(-25.0392383006299,-14.5039655272361,
113.553596534669)) ;
#177844 = CARTESIAN_POINT('Ctrl Pts',(-25.0376460424301,-14.5797031872051,
113.548746774189)) ;
#177845 = CARTESIAN_POINT('Ctrl Pts',(-25.111449868317,-14.5797031845831,
113.5245156791)) ;
#177846 = CARTESIAN_POINT('Ctrl Pts',(-25.1852536942039,-14.5797031819611,
113.500284584012)) ;
#177847 = CARTESIAN_POINT('Ctrl Pts',(-25.1868459524037,-14.5039655219921,
113.505134344491)) ;
#177848 = CARTESIAN_POINT('Ctrl Pts',(-25.267129516287,-14.4826373105238,
113.785223901541)) ;
#177849 = CARTESIAN_POINT('Ctrl Pts',(-25.2623828413335,-14.4082736216989,
113.770766294605)) ;
#177850 = CARTESIAN_POINT('Ctrl Pts',(-25.188579012109,-14.4082736113454,
113.794997379528)) ;
#177851 = CARTESIAN_POINT('Ctrl Pts',(-25.1147751828845,-14.4082736009919,
113.819228464451)) ;
#177852 = CARTESIAN_POINT('Ctrl Pts',(-25.1195218578379,-14.4826372898169,
113.833686071387)) ;
#177853 = CARTESIAN_POINT('Ctrl Pts',(-25.1242685327913,-14.5570009786418,
113.848143678323)) ;
#177854 = CARTESIAN_POINT('Ctrl Pts',(-25.1980723620159,-14.5570009889953,
113.8239125934)) ;
#177855 = CARTESIAN_POINT('Ctrl Pts',(-25.2718761912404,-14.5570009993487,
113.799681508477)) ;
#177856 = CARTESIAN_POINT('Ctrl Pts',(-25.267129516287,-14.4826373105238,
113.785223901541)) ;
#177857 = CARTESIAN_POINT('Ctrl Pts',(-25.3418916496393,-14.3855815012644,
114.048250710986)) ;
#177858 = CARTESIAN_POINT('Ctrl Pts',(-25.3311870097103,-14.3178820902551,
114.015646104187)) ;
#177859 = CARTESIAN_POINT('Ctrl Pts',(-25.2573831771349,-14.3178820716342,
114.039877178904)) ;
#177860 = CARTESIAN_POINT('Ctrl Pts',(-25.1835793445595,-14.3178820530132,
114.064108253621)) ;
#177861 = CARTESIAN_POINT('Ctrl Pts',(-25.1942839844885,-14.3855814640225,
114.096712860419)) ;
#177862 = CARTESIAN_POINT('Ctrl Pts',(-25.2049886244175,-14.4532808750318,
114.129317467217)) ;
#177863 = CARTESIAN_POINT('Ctrl Pts',(-25.2787924569929,-14.4532808936528,
114.105086392501)) ;
#177864 = CARTESIAN_POINT('Ctrl Pts',(-25.3525962895683,-14.4532809122737,
114.080855317784)) ;
#177865 = CARTESIAN_POINT('Ctrl Pts',(-25.3418916496393,-14.3855815012644,
114.048250710986)) ;
#177866 = CARTESIAN_POINT('Ctrl Pts',(-25.4059102519348,-14.2190969785884,
114.278710495903)) ;
#177867 = CARTESIAN_POINT('Ctrl Pts',(-25.3899854352774,-14.1629192872983,
114.230206073229)) ;
#177868 = CARTESIAN_POINT('Ctrl Pts',(-25.3161815987738,-14.1629192658567,
114.254437135981)) ;
#177869 = CARTESIAN_POINT('Ctrl Pts',(-25.2423777622703,-14.1629192444152,
114.278668198734)) ;
#177870 = CARTESIAN_POINT('Ctrl Pts',(-25.2583025789277,-14.2190969357053,
114.327172621408)) ;
#177871 = CARTESIAN_POINT('Ctrl Pts',(-25.2742273955851,-14.2752746269954,
114.375677044082)) ;
#177872 = CARTESIAN_POINT('Ctrl Pts',(-25.3480312320887,-14.275274648437,
114.35144598133)) ;
#177873 = CARTESIAN_POINT('Ctrl Pts',(-25.4218350685922,-14.2752746698786,
114.327214918577)) ;
#177874 = CARTESIAN_POINT('Ctrl Pts',(-25.4059102519348,-14.2190969785884,
114.278710495903)) ;
#177875 = CARTESIAN_POINT('Ctrl Pts',(-25.4534572816173,-13.9949296481822,
114.4590197693)) ;
#177876 = CARTESIAN_POINT('Ctrl Pts',(-25.4334540036049,-13.9543190677503,
114.398093011557)) ;
#177877 = CARTESIAN_POINT('Ctrl Pts',(-25.35965016373,-13.9543190483412,114.42232406404)) ;
#177878 = CARTESIAN_POINT('Ctrl Pts',(-25.285846323855,-13.9543190289321,
114.446555116524)) ;
#177879 = CARTESIAN_POINT('Ctrl Pts',(-25.3058496018674,-13.9949296093639,
114.507481874267)) ;
#177880 = CARTESIAN_POINT('Ctrl Pts',(-25.3258528798797,-14.0355401897957,
114.568408632009)) ;
#177881 = CARTESIAN_POINT('Ctrl Pts',(-25.3996567197547,-14.0355402092049,
114.544177579526)) ;
#177882 = CARTESIAN_POINT('Ctrl Pts',(-25.4734605596297,-14.035540228614,
114.519946527043)) ;
#177883 = CARTESIAN_POINT('Ctrl Pts',(-25.4534572816173,-13.9949296481822,
114.4590197693)) ;
#177884 = CARTESIAN_POINT('Ctrl Pts',(-25.4803949407615,-13.7298783707897,
114.576500255508)) ;
#177885 = CARTESIAN_POINT('Ctrl Pts',(-25.457747280991,-13.7077134495774,
114.507519137741)) ;
#177886 = CARTESIAN_POINT('Ctrl Pts',(-25.3839434387268,-13.7077134348718,
114.531750182947)) ;
#177887 = CARTESIAN_POINT('Ctrl Pts',(-25.3101395964625,-13.7077134201661,
114.555981228153)) ;
#177888 = CARTESIAN_POINT('Ctrl Pts',(-25.332787256233,-13.7298783413784,
114.624962345921)) ;
#177889 = CARTESIAN_POINT('Ctrl Pts',(-25.3554349160035,-13.7520432625907,
114.693943463688)) ;
#177890 = CARTESIAN_POINT('Ctrl Pts',(-25.4292387582677,-13.7520432772964,
114.669712418482)) ;
#177891 = CARTESIAN_POINT('Ctrl Pts',(-25.5030426005319,-13.752043292002,
114.645481373276)) ;
#177892 = CARTESIAN_POINT('Ctrl Pts',(-25.4803949407615,-13.7298783707897,
114.576500255508)) ;
#177893 = CARTESIAN_POINT('Ctrl Pts',(-25.4839639384194,-13.4411780607526,
114.622967439281)) ;
#177894 = CARTESIAN_POINT('Ctrl Pts',(-25.4602961356255,-13.4391385958436,
114.550879130608)) ;
#177895 = CARTESIAN_POINT('Ctrl Pts',(-25.3864922921103,-13.4391385881017,
114.575110172003)) ;
#177896 = CARTESIAN_POINT('Ctrl Pts',(-25.312688448595,-13.4391385803598,
114.599341213399)) ;
#177897 = CARTESIAN_POINT('Ctrl Pts',(-25.336356251389,-13.4411780452688,
114.671429522073)) ;
#177898 = CARTESIAN_POINT('Ctrl Pts',(-25.3600240541829,-13.4432175101778,
114.743517830747)) ;
#177899 = CARTESIAN_POINT('Ctrl Pts',(-25.4338278976981,-13.4432175179197,
114.719286789351)) ;
#177900 = CARTESIAN_POINT('Ctrl Pts',(-25.5076317412133,-13.4432175256616,
114.695055747955)) ;
#177901 = CARTESIAN_POINT('Ctrl Pts',(-25.4839639384194,-13.4411780607526,
114.622967439281)) ;
#177902 = CARTESIAN_POINT('Ctrl Pts',(-25.4634405619125,-13.1535366585443,
114.595704133561)) ;
#177903 = CARTESIAN_POINT('Ctrl Pts',(-25.4404409966477,-13.1715786657878,
114.525651168662)) ;
#177904 = CARTESIAN_POINT('Ctrl Pts',(-25.3666371528437,-13.1715786624699,
114.549882209178)) ;
#177905 = CARTESIAN_POINT('Ctrl Pts',(-25.2928333090395,-13.1715786591521,
114.574113249694)) ;
#177906 = CARTESIAN_POINT('Ctrl Pts',(-25.3158328743043,-13.1535366519086,
114.644166214593)) ;
#177907 = CARTESIAN_POINT('Ctrl Pts',(-25.3388324395691,-13.1354946446651,
114.714219179492)) ;
#177908 = CARTESIAN_POINT('Ctrl Pts',(-25.4126362833732,-13.1354946479829,
114.689988138976)) ;
#177909 = CARTESIAN_POINT('Ctrl Pts',(-25.4864401271773,-13.1354946513008,
114.66575709846)) ;
#177910 = CARTESIAN_POINT('Ctrl Pts',(-25.4634405619125,-13.1535366585443,
114.595704133561)) ;
#177911 = CARTESIAN_POINT('Ctrl Pts',(-25.4188861853407,-12.8812078446008,
114.495722751362)) ;
#177912 = CARTESIAN_POINT('Ctrl Pts',(-25.3982238139182,-12.9182937200929,
114.432788501901)) ;
#177913 = CARTESIAN_POINT('Ctrl Pts',(-25.3244199706641,-12.9182937216163,
114.457019544092)) ;
#177914 = CARTESIAN_POINT('Ctrl Pts',(-25.2506161274099,-12.9182937231397,
114.481250586283)) ;
#177915 = CARTESIAN_POINT('Ctrl Pts',(-25.2712784988323,-12.8812078476476,
114.544184835744)) ;
#177916 = CARTESIAN_POINT('Ctrl Pts',(-25.2919408702547,-12.8441219721555,
114.607119085205)) ;
#177917 = CARTESIAN_POINT('Ctrl Pts',(-25.3657447135089,-12.8441219706321,
114.582888043014)) ;
#177918 = CARTESIAN_POINT('Ctrl Pts',(-25.4395485567631,-12.8441219691087,
114.558657000823)) ;
#177919 = CARTESIAN_POINT('Ctrl Pts',(-25.4188861853407,-12.8812078446008,
114.495722751362)) ;
#177920 = CARTESIAN_POINT('Ctrl Pts',(-25.3535678038264,-12.6502697095916,
114.332121264411)) ;
#177921 = CARTESIAN_POINT('Ctrl Pts',(-25.336704301178,-12.7035365652379,
114.280757756318)) ;
#177922 = CARTESIAN_POINT('Ctrl Pts',(-25.2629004584182,-12.7035365674139,
114.304988800015)) ;
#177923 = CARTESIAN_POINT('Ctrl Pts',(-25.1890966156585,-12.7035365695899,
114.329219843711)) ;
#177924 = CARTESIAN_POINT('Ctrl Pts',(-25.2059601183069,-12.6502697139436,
114.380583351805)) ;
#177925 = CARTESIAN_POINT('Ctrl Pts',(-25.2228236209554,-12.5970028582972,
114.431946859898)) ;
#177926 = CARTESIAN_POINT('Ctrl Pts',(-25.2966274637151,-12.5970028561212,
114.407715816201)) ;
#177927 = CARTESIAN_POINT('Ctrl Pts',(-25.3704313064749,-12.5970028539452,
114.383484772504)) ;
#177928 = CARTESIAN_POINT('Ctrl Pts',(-25.3535678038264,-12.6502697095916,
114.332121264411)) ;
#177929 = CARTESIAN_POINT('Ctrl Pts',(-25.271268624716,-12.4736381112203,
114.116796974903)) ;
#177930 = CARTESIAN_POINT('Ctrl Pts',(-25.2593955331649,-12.5393175291298,
114.080633453818)) ;
#177931 = CARTESIAN_POINT('Ctrl Pts',(-25.1855916906662,-12.5393175306857,
114.10486449831)) ;
#177932 = CARTESIAN_POINT('Ctrl Pts',(-25.1117878481675,-12.5393175322416,
114.129095542802)) ;
#177933 = CARTESIAN_POINT('Ctrl Pts',(-25.1236609397186,-12.473638114332,
114.165259063887)) ;
#177934 = CARTESIAN_POINT('Ctrl Pts',(-25.1355340312698,-12.4079586964224,
114.201422584972)) ;
#177935 = CARTESIAN_POINT('Ctrl Pts',(-25.2093378737685,-12.4079586948666,
114.17719154048)) ;
#177936 = CARTESIAN_POINT('Ctrl Pts',(-25.2831417162671,-12.4079586933107,
114.152960495988)) ;
#177937 = CARTESIAN_POINT('Ctrl Pts',(-25.271268624716,-12.4736381112203,
114.116796974903)) ;
#177938 = CARTESIAN_POINT('Ctrl Pts',(-25.1760059663422,-12.3636957343507,
113.862315910691)) ;
#177939 = CARTESIAN_POINT('Ctrl Pts',(-25.17002920577,-12.4371496799271,113.844111662346)) ;
#177940 = CARTESIAN_POINT('Ctrl Pts',(-25.0962253625595,-12.4371496797509,
113.86834270467)) ;
#177941 = CARTESIAN_POINT('Ctrl Pts',(-25.0224215193491,-12.4371496795748,
113.892573746994)) ;
#177942 = CARTESIAN_POINT('Ctrl Pts',(-25.0283982799213,-12.3636957339984,
113.910777995339)) ;
#177943 = CARTESIAN_POINT('Ctrl Pts',(-25.0343750404935,-12.290241788422,
113.928982243684)) ;
#177944 = CARTESIAN_POINT('Ctrl Pts',(-25.1081788837039,-12.2902417885981,
113.90475120136)) ;
#177945 = CARTESIAN_POINT('Ctrl Pts',(-25.1819827269144,-12.2902417887743,
113.880520159036)) ;
#177946 = CARTESIAN_POINT('Ctrl Pts',(-25.1760059663422,-12.3636957343507,
113.862315910691)) ;
#177947 = CARTESIAN_POINT('Ctrl Pts',(-25.0755208022999,-12.3303161657527,
113.59162885322)) ;
#177948 = CARTESIAN_POINT('Ctrl Pts',(-25.0758197046939,-12.4062080741742,
113.592539261621)) ;
#177949 = CARTESIAN_POINT('Ctrl Pts',(-25.0020158602591,-12.4062080738796,
113.616770300216)) ;
#177950 = CARTESIAN_POINT('Ctrl Pts',(-24.9282120158242,-12.406208073585,
113.64100133881)) ;
#177951 = CARTESIAN_POINT('Ctrl Pts',(-24.9279131134302,-12.3303161651636,
113.64009093041)) ;
#177952 = CARTESIAN_POINT('Ctrl Pts',(-24.9276142110362,-12.2544242567421,
113.639180522009)) ;
#177953 = CARTESIAN_POINT('Ctrl Pts',(-25.0014180554711,-12.2544242570367,
113.614949483414)) ;
#177954 = CARTESIAN_POINT('Ctrl Pts',(-25.0752218999059,-12.2544242573313,
113.590718444819)) ;
#177955 = CARTESIAN_POINT('Ctrl Pts',(-25.0755208022999,-12.3303161657527,
113.59162885322)) ;
#177956 = CARTESIAN_POINT('Ctrl Pts',(-24.975387420301,-12.3741418831008,
113.322042926048)) ;
#177957 = CARTESIAN_POINT('Ctrl Pts',(-24.9819458583715,-12.4470842325009,
113.342018870052)) ;
#177958 = CARTESIAN_POINT('Ctrl Pts',(-24.90814201245,-12.447084234237,113.366249904119)) ;
#177959 = CARTESIAN_POINT('Ctrl Pts',(-24.8343381665285,-12.4470842359731,
113.390480938186)) ;
#177960 = CARTESIAN_POINT('Ctrl Pts',(-24.827779728458,-12.374141886573,113.370504994182)) ;
#177961 = CARTESIAN_POINT('Ctrl Pts',(-24.8212212903875,-12.3011995371729,
113.350529050178)) ;
#177962 = CARTESIAN_POINT('Ctrl Pts',(-24.895025136309,-12.3011995354367,
113.326298016111)) ;
#177963 = CARTESIAN_POINT('Ctrl Pts',(-24.9688289822304,-12.3011995337006,
113.302066982044)) ;
#177964 = CARTESIAN_POINT('Ctrl Pts',(-24.975387420301,-12.3741418831008,
113.322042926048)) ;
#177965 = CARTESIAN_POINT('Ctrl Pts',(-24.8815379026335,-12.4937241519796,
113.071825125992)) ;
#177966 = CARTESIAN_POINT('Ctrl Pts',(-24.893921544422,-12.5584232360499,
113.109543700474)) ;
#177967 = CARTESIAN_POINT('Ctrl Pts',(-24.8201176966158,-12.5584232440279,
113.1337747288)) ;
#177968 = CARTESIAN_POINT('Ctrl Pts',(-24.7463138488095,-12.558423252006,
113.158005757126)) ;
#177969 = CARTESIAN_POINT('Ctrl Pts',(-24.7339302070211,-12.4937241679357,
113.120287182645)) ;
#177970 = CARTESIAN_POINT('Ctrl Pts',(-24.7215465652326,-12.4290250838654,
113.082568608163)) ;
#177971 = CARTESIAN_POINT('Ctrl Pts',(-24.7953504130388,-12.4290250758873,
113.058337579837)) ;
#177972 = CARTESIAN_POINT('Ctrl Pts',(-24.869154260845,-12.4290250679093,
113.034106551511)) ;
#177973 = CARTESIAN_POINT('Ctrl Pts',(-24.8815379026335,-12.4937241519796,
113.071825125992)) ;
#177974 = CARTESIAN_POINT('Ctrl Pts',(-24.8012449463837,-12.6783961032596,
112.862605193765)) ;
#177975 = CARTESIAN_POINT('Ctrl Pts',(-24.8185213903701,-12.7302945007164,
112.915226454164)) ;
#177976 = CARTESIAN_POINT('Ctrl Pts',(-24.7447175419959,-12.7302945169849,
112.93945748076)) ;
#177977 = CARTESIAN_POINT('Ctrl Pts',(-24.6709136936216,-12.7302945332533,
112.963688507356)) ;
#177978 = CARTESIAN_POINT('Ctrl Pts',(-24.6536372496352,-12.6783961357965,
112.911067246957)) ;
#177979 = CARTESIAN_POINT('Ctrl Pts',(-24.6363608056488,-12.6264977383397,
112.858445986558)) ;
#177980 = CARTESIAN_POINT('Ctrl Pts',(-24.7101646540231,-12.6264977220713,
112.834214959962)) ;
#177981 = CARTESIAN_POINT('Ctrl Pts',(-24.7839685023973,-12.6264977058028,
112.809983933366)) ;
#177982 = CARTESIAN_POINT('Ctrl Pts',(-24.8012449463837,-12.6783961032596,
112.862605193765)) ;
#177983 = CARTESIAN_POINT('Ctrl Pts',(-24.738447605087,-12.9163766433386,
112.706791373276)) ;
#177984 = CARTESIAN_POINT('Ctrl Pts',(-24.7593999334311,-12.951734042377,
112.770608784171)) ;
#177985 = CARTESIAN_POINT('Ctrl Pts',(-24.6855960853926,-12.9517340693484,
112.79483981179)) ;
#177986 = CARTESIAN_POINT('Ctrl Pts',(-24.611792237354,-12.9517340963197,
112.819070839409)) ;
#177987 = CARTESIAN_POINT('Ctrl Pts',(-24.5908399090099,-12.9163766972813,
112.755253428513)) ;
#177988 = CARTESIAN_POINT('Ctrl Pts',(-24.5698875806658,-12.8810192982428,
112.691436017618)) ;
#177989 = CARTESIAN_POINT('Ctrl Pts',(-24.6436914287043,-12.8810192712715,
112.667204989999)) ;
#177990 = CARTESIAN_POINT('Ctrl Pts',(-24.7174952767428,-12.8810192443002,
112.642973962381)) ;
#177991 = CARTESIAN_POINT('Ctrl Pts',(-24.738447605087,-12.9163766433386,
112.706791373276)) ;
#177992 = CARTESIAN_POINT('Ctrl Pts',(-24.697217131185,-13.1903758945546,
112.616669578636)) ;
#177993 = CARTESIAN_POINT('Ctrl Pts',(-24.720344718258,-13.2066536724704,
112.687112476478)) ;
#177994 = CARTESIAN_POINT('Ctrl Pts',(-24.6465408720429,-13.206653710727,
112.711343509651)) ;
#177995 = CARTESIAN_POINT('Ctrl Pts',(-24.5727370258278,-13.2066537489837,
112.735574542823)) ;
#177996 = CARTESIAN_POINT('Ctrl Pts',(-24.5496094387548,-13.1903759710679,
112.66513164498)) ;
#177997 = CARTESIAN_POINT('Ctrl Pts',(-24.5264818516818,-13.1740981931521,
112.594688747138)) ;
#177998 = CARTESIAN_POINT('Ctrl Pts',(-24.6002856978969,-13.1740981548955,
112.570457713965)) ;
#177999 = CARTESIAN_POINT('Ctrl Pts',(-24.674089544112,-13.1740981166388,
112.546226680793)) ;
#178000 = CARTESIAN_POINT('Ctrl Pts',(-24.697217131185,-13.1903758945546,
112.616669578636)) ;
#178001 = CARTESIAN_POINT('Ctrl Pts',(-24.679735225327,-13.481432819081,112.598974089601)) ;
#178002 = CARTESIAN_POINT('Ctrl Pts',(-24.7033812444506,-13.4774126955136,
112.670996047636)) ;
#178003 = CARTESIAN_POINT('Ctrl Pts',(-24.62957740167,-13.4774127443564,112.695227091269)) ;
#178004 = CARTESIAN_POINT('Ctrl Pts',(-24.5557735588893,-13.4774127931991,
112.719458134902)) ;
#178005 = CARTESIAN_POINT('Ctrl Pts',(-24.5321275397657,-13.4814329167664,
112.647436176867)) ;
#178006 = CARTESIAN_POINT('Ctrl Pts',(-24.5084815206421,-13.4854530403338,
112.575414218832)) ;
#178007 = CARTESIAN_POINT('Ctrl Pts',(-24.5822853634227,-13.4854529914911,
112.551183175199)) ;
#178008 = CARTESIAN_POINT('Ctrl Pts',(-24.6560892062034,-13.4854529426483,
112.526952131566)) ;
#178009 = CARTESIAN_POINT('Ctrl Pts',(-24.679735225327,-13.481432819081,112.598974089601)) ;
#178010 = CARTESIAN_POINT('Ctrl Pts',(-24.6866566649467,-13.7673558416161,
112.655538950219)) ;
#178011 = CARTESIAN_POINT('Ctrl Pts',(-24.709119400258,-13.7433670881258,
112.723956816513)) ;
#178012 = CARTESIAN_POINT('Ctrl Pts',(-24.6353155624356,-13.7433671429839,
112.748187875248)) ;
#178013 = CARTESIAN_POINT('Ctrl Pts',(-24.5615117246133,-13.7433671978421,
112.772418933983)) ;
#178014 = CARTESIAN_POINT('Ctrl Pts',(-24.5390489893019,-13.7673559513324,
112.704001067689)) ;
#178015 = CARTESIAN_POINT('Ctrl Pts',(-24.5165862539907,-13.7913447048227,
112.635583201395)) ;
#178016 = CARTESIAN_POINT('Ctrl Pts',(-24.590390091813,-13.7913446499646,
112.61135214266)) ;
#178017 = CARTESIAN_POINT('Ctrl Pts',(-24.6641939296354,-13.7913445951064,
112.587121083925)) ;
#178018 = CARTESIAN_POINT('Ctrl Pts',(-24.6866566649467,-13.7673558416161,
112.655538950219)) ;
#178019 = CARTESIAN_POINT('Ctrl Pts',(-24.7163960105244,-14.0271101613543,
112.781439555252)) ;
#178020 = CARTESIAN_POINT('Ctrl Pts',(-24.7360839175633,-13.9849513065541,
112.84140574221)) ;
#178021 = CARTESIAN_POINT('Ctrl Pts',(-24.6622800853002,-13.9849513605373,
112.865636817878)) ;
#178022 = CARTESIAN_POINT('Ctrl Pts',(-24.5884762530371,-13.9849514145205,
112.889867893545)) ;
#178023 = CARTESIAN_POINT('Ctrl Pts',(-24.5687883459981,-14.0271102693206,
112.829901706588)) ;
#178024 = CARTESIAN_POINT('Ctrl Pts',(-24.5491004389591,-14.0692691241208,
112.769935519631)) ;
#178025 = CARTESIAN_POINT('Ctrl Pts',(-24.6229042712222,-14.0692690701376,
112.745704443963)) ;
#178026 = CARTESIAN_POINT('Ctrl Pts',(-24.6967081034854,-14.0692690161544,
112.721473368295)) ;
#178027 = CARTESIAN_POINT('Ctrl Pts',(-24.7163960105244,-14.0271101613543,
112.781439555252)) ;
#178028 = CARTESIAN_POINT('Ctrl Pts',(-24.7663270399,-14.2445027860115,112.968989653976)) ;
#178029 = CARTESIAN_POINT('Ctrl Pts',(-24.7818234876689,-14.187105106811,
113.016189332129)) ;
#178030 = CARTESIAN_POINT('Ctrl Pts',(-24.7080196613805,-14.1871051547693,
113.040420425995)) ;
#178031 = CARTESIAN_POINT('Ctrl Pts',(-24.6342158350921,-14.1871052027276,
113.064651519861)) ;
#178032 = CARTESIAN_POINT('Ctrl Pts',(-24.6187193873233,-14.244502881928,
113.017451841708)) ;
#178033 = CARTESIAN_POINT('Ctrl Pts',(-24.6032229395544,-14.3019005611285,
112.970252163555)) ;
#178034 = CARTESIAN_POINT('Ctrl Pts',(-24.6770267658428,-14.3019005131702,
112.946021069689)) ;
#178035 = CARTESIAN_POINT('Ctrl Pts',(-24.7508305921312,-14.3019004652119,
112.921789975823)) ;
#178036 = CARTESIAN_POINT('Ctrl Pts',(-24.7663270399,-14.2445027860115,112.968989653976)) ;
#178037 = CARTESIAN_POINT('Ctrl Pts',(-24.8322750811479,-14.4028029107363,
113.205401926826)) ;
#178038 = CARTESIAN_POINT('Ctrl Pts',(-24.8424542618704,-14.3342697574314,
113.236406067336)) ;
#178039 = CARTESIAN_POINT('Ctrl Pts',(-24.7686504412644,-14.3342697924112,
113.260637178509)) ;
#178040 = CARTESIAN_POINT('Ctrl Pts',(-24.6948466206583,-14.334269827391,
113.284868289682)) ;
#178041 = CARTESIAN_POINT('Ctrl Pts',(-24.6846674399358,-14.402802980696,
113.253864149172)) ;
#178042 = CARTESIAN_POINT('Ctrl Pts',(-24.6744882592133,-14.471336134001,
113.222860008663)) ;
#178043 = CARTESIAN_POINT('Ctrl Pts',(-24.7482920798194,-14.4713360990211,
113.198628897489)) ;
#178044 = CARTESIAN_POINT('Ctrl Pts',(-24.8220959004254,-14.4713360640413,
113.174397786316)) ;
#178045 = CARTESIAN_POINT('Ctrl Pts',(-24.8322750811479,-14.4028029107363,
113.205401926826)) ;
#178046 = CARTESIAN_POINT('Ctrl Pts',(-24.9082113685337,-14.4900131921161,
113.472067220855)) ;
#178047 = CARTESIAN_POINT('Ctrl Pts',(-24.9123716787017,-14.4152919696491,
113.484738852679)) ;
#178048 = CARTESIAN_POINT('Ctrl Pts',(-24.8385678620488,-14.4152919849729,
113.508969975893)) ;
#178049 = CARTESIAN_POINT('Ctrl Pts',(-24.7647640453958,-14.4152920002968,
113.533201099107)) ;
#178050 = CARTESIAN_POINT('Ctrl Pts',(-24.7606037352279,-14.4900132227638,
113.520529467283)) ;
#178051 = CARTESIAN_POINT('Ctrl Pts',(-24.7564434250599,-14.5647344452309,
113.507857835459)) ;
#178052 = CARTESIAN_POINT('Ctrl Pts',(-24.8302472417128,-14.5647344299071,
113.483626712245)) ;
#178053 = CARTESIAN_POINT('Ctrl Pts',(-24.9040510583658,-14.5647344145832,
113.459395589031)) ;
#178054 = CARTESIAN_POINT('Ctrl Pts',(-24.9082113685337,-14.4900131921161,
113.472067220855)) ;
#178055 = CARTESIAN_POINT('Ctrl Pts',(-24.9884934184206,-14.5009049303826,
113.752069619527)) ;
#178056 = CARTESIAN_POINT('Ctrl Pts',(-24.9863207377421,-14.4253144760394,
113.745451982938)) ;
#178057 = CARTESIAN_POINT('Ctrl Pts',(-24.9125169233169,-14.4253144674804,
113.769683112938)) ;
#178058 = CARTESIAN_POINT('Ctrl Pts',(-24.8387131088918,-14.4253144589214,
113.793914242937)) ;
#178059 = CARTESIAN_POINT('Ctrl Pts',(-24.8408857895702,-14.5009049132646,
113.800531879526)) ;
#178060 = CARTESIAN_POINT('Ctrl Pts',(-24.8430584702487,-14.5764953676079,
113.807149516115)) ;
#178061 = CARTESIAN_POINT('Ctrl Pts',(-24.9168622846738,-14.5764953761669,
113.782918386116)) ;
#178062 = CARTESIAN_POINT('Ctrl Pts',(-24.990666099099,-14.5764953847259,
113.758687256117)) ;
#178063 = CARTESIAN_POINT('Ctrl Pts',(-24.9884934184206,-14.5009049303826,
113.752069619527)) ;
#178064 = CARTESIAN_POINT('Ctrl Pts',(-25.0666037768646,-14.4337694493022,
114.025547084295)) ;
#178065 = CARTESIAN_POINT('Ctrl Pts',(-25.0582386564678,-14.3627554397417,
114.000068275361)) ;
#178066 = CARTESIAN_POINT('Ctrl Pts',(-24.9844348419182,-14.3627554046461,
114.024299404982)) ;
#178067 = CARTESIAN_POINT('Ctrl Pts',(-24.9106310273687,-14.3627553695504,
114.048530534602)) ;
#178068 = CARTESIAN_POINT('Ctrl Pts',(-24.9189961477656,-14.4337693791109,
114.074009343536)) ;
#178069 = CARTESIAN_POINT('Ctrl Pts',(-24.9273612681624,-14.5047833886713,
114.09948815247)) ;
#178070 = CARTESIAN_POINT('Ctrl Pts',(-25.0011650827119,-14.504783423767,
114.075257022849)) ;
#178071 = CARTESIAN_POINT('Ctrl Pts',(-25.0749688972614,-14.5047834588626,
114.051025893229)) ;
#178072 = CARTESIAN_POINT('Ctrl Pts',(-25.0666037768646,-14.4337694493022,
114.025547084295)) ;
#178073 = CARTESIAN_POINT('Ctrl Pts',(-25.1357889459536,-14.2939322119372,
114.271744953977)) ;
#178074 = CARTESIAN_POINT('Ctrl Pts',(-25.1218473907092,-14.232577073239,
114.229281224174)) ;
#178075 = CARTESIAN_POINT('Ctrl Pts',(-25.0480435732121,-14.2325770123608,
114.253512344817)) ;
#178076 = CARTESIAN_POINT('Ctrl Pts',(-24.9742397557151,-14.2325769514826,
114.27774346546)) ;
#178077 = CARTESIAN_POINT('Ctrl Pts',(-24.9881813109595,-14.2939320901808,
114.320207195263)) ;
#178078 = CARTESIAN_POINT('Ctrl Pts',(-25.0021228662039,-14.3552872288789,
114.362670925066)) ;
#178079 = CARTESIAN_POINT('Ctrl Pts',(-25.075926683701,-14.3552872897571,
114.338439804423)) ;
#178080 = CARTESIAN_POINT('Ctrl Pts',(-25.149730501198,-14.3552873506354,
114.31420868378)) ;
#178081 = CARTESIAN_POINT('Ctrl Pts',(-25.1357889459536,-14.2939322119372,
114.271744953977)) ;
#178082 = CARTESIAN_POINT('Ctrl Pts',(-25.1905524181362,-14.0911613446941,
114.474041191823)) ;
#178083 = CARTESIAN_POINT('Ctrl Pts',(-25.1720325424193,-14.0438726639187,
114.417632636512)) ;
#178084 = CARTESIAN_POINT('Ctrl Pts',(-25.0982287195,-14.0438725807802,114.44186374064)) ;
#178085 = CARTESIAN_POINT('Ctrl Pts',(-25.0244248965808,-14.0438724976418,
114.466094844767)) ;
#178086 = CARTESIAN_POINT('Ctrl Pts',(-25.0429447722977,-14.0911611784172,
114.522503400078)) ;
#178087 = CARTESIAN_POINT('Ctrl Pts',(-25.0614646480147,-14.1384498591927,
114.578911955389)) ;
#178088 = CARTESIAN_POINT('Ctrl Pts',(-25.1352684709339,-14.1384499423311,
114.554680851261)) ;
#178089 = CARTESIAN_POINT('Ctrl Pts',(-25.2090722938532,-14.1384500254695,
114.530449747134)) ;
#178090 = CARTESIAN_POINT('Ctrl Pts',(-25.1905524181362,-14.0911613446941,
114.474041191823)) ;
#178091 = CARTESIAN_POINT('Ctrl Pts',(-25.2261345436437,-13.8412394795533,
114.617769466887)) ;
#178092 = CARTESIAN_POINT('Ctrl Pts',(-25.2043717963994,-13.8113299936379,
114.551483648106)) ;
#178093 = CARTESIAN_POINT('Ctrl Pts',(-25.1305679660697,-13.8113298944944,
114.575714729663)) ;
#178094 = CARTESIAN_POINT('Ctrl Pts',(-25.0567641357399,-13.8113297953509,
114.599945811219)) ;
#178095 = CARTESIAN_POINT('Ctrl Pts',(-25.0785268829842,-13.8412392812663,
114.666231629999)) ;
#178096 = CARTESIAN_POINT('Ctrl Pts',(-25.1002896302284,-13.8711487671817,
114.732517448779)) ;
#178097 = CARTESIAN_POINT('Ctrl Pts',(-25.1740934605582,-13.8711488663252,
114.708286367223)) ;
#178098 = CARTESIAN_POINT('Ctrl Pts',(-25.2478972908879,-13.8711489654687,
114.684055285667)) ;
#178099 = CARTESIAN_POINT('Ctrl Pts',(-25.2261345436437,-13.8412394795533,
114.617769466887)) ;
#178100 = CARTESIAN_POINT('Ctrl Pts',(-25.2394283887284,-13.5592605313859,
114.693848406936)) ;
#178101 = CARTESIAN_POINT('Ctrl Pts',(-25.2159688790662,-13.5489932748768,
114.622394523587)) ;
#178102 = CARTESIAN_POINT('Ctrl Pts',(-25.1421650400429,-13.5489931673576,
114.646625578664)) ;
#178103 = CARTESIAN_POINT('Ctrl Pts',(-25.0683612010196,-13.5489930598384,
114.670856633741)) ;
#178104 = CARTESIAN_POINT('Ctrl Pts',(-25.0918207106818,-13.5592603163474,
114.74231051709)) ;
#178105 = CARTESIAN_POINT('Ctrl Pts',(-25.1152802203441,-13.5695275728564,
114.813764400439)) ;
#178106 = CARTESIAN_POINT('Ctrl Pts',(-25.1890840593674,-13.5695276803756,
114.789533345362)) ;
#178107 = CARTESIAN_POINT('Ctrl Pts',(-25.2628878983907,-13.5695277878949,
114.765302290285)) ;
#178108 = CARTESIAN_POINT('Ctrl Pts',(-25.2394283887284,-13.5592605313859,
114.693848406936)) ;
#178109 = CARTESIAN_POINT('Ctrl Pts',(-25.2286664367361,-13.2696223387077,
114.696342245869)) ;
#178110 = CARTESIAN_POINT('Ctrl Pts',(-25.2051938392726,-13.279561631404,
114.624848499195)) ;
#178111 = CARTESIAN_POINT('Ctrl Pts',(-25.1313899912239,-13.2795615243136,
114.649079526783)) ;
#178112 = CARTESIAN_POINT('Ctrl Pts',(-25.0575861431753,-13.2795614172232,
114.67331055437)) ;
#178113 = CARTESIAN_POINT('Ctrl Pts',(-25.0810587406387,-13.2696221245269,
114.744804301044)) ;
#178114 = CARTESIAN_POINT('Ctrl Pts',(-25.1045313381022,-13.2596828318306,
114.816298047717)) ;
#178115 = CARTESIAN_POINT('Ctrl Pts',(-25.1783351861508,-13.259682938921,
114.79206702013)) ;
#178116 = CARTESIAN_POINT('Ctrl Pts',(-25.2521390341995,-13.2596830460114,
114.767835992543)) ;
#178117 = CARTESIAN_POINT('Ctrl Pts',(-25.2286664367361,-13.2696223387077,
114.696342245869)) ;
#178118 = CARTESIAN_POINT('Ctrl Pts',(-25.1937485823441,-12.9883139496615,
114.625551828042)) ;
#178119 = CARTESIAN_POINT('Ctrl Pts',(-25.1719429537545,-13.0179078909162,
114.559135399623)) ;
#178120 = CARTESIAN_POINT('Ctrl Pts',(-25.09813909715,-13.0179077930937,114.583366401151)) ;
#178121 = CARTESIAN_POINT('Ctrl Pts',(-25.0243352405455,-13.0179076952712,
114.607597402679)) ;
#178122 = CARTESIAN_POINT('Ctrl Pts',(-25.0461408691352,-12.9883137540165,
114.674013831097)) ;
#178123 = CARTESIAN_POINT('Ctrl Pts',(-25.0679464977248,-12.9587198127618,
114.740430259516)) ;
#178124 = CARTESIAN_POINT('Ctrl Pts',(-25.1417503543293,-12.9587199105843,
114.716199257988)) ;
#178125 = CARTESIAN_POINT('Ctrl Pts',(-25.2155542109338,-12.9587200084068,
114.69196825646)) ;
#178126 = CARTESIAN_POINT('Ctrl Pts',(-25.1937485823441,-12.9883139496615,
114.625551828042)) ;
#178127 = CARTESIAN_POINT('Ctrl Pts',(-25.1365175245661,-12.7386910562247,
114.486687971447)) ;
#178128 = CARTESIAN_POINT('Ctrl Pts',(-25.1179414901368,-12.7857570655332,
114.430108365799)) ;
#178129 = CARTESIAN_POINT('Ctrl Pts',(-25.0441376264093,-12.7857569845681,
114.454339345632)) ;
#178130 = CARTESIAN_POINT('Ctrl Pts',(-24.9703337626818,-12.785756903603,
114.478570325464)) ;
#178131 = CARTESIAN_POINT('Ctrl Pts',(-24.9889097971111,-12.7386908942945,
114.535149931112)) ;
#178132 = CARTESIAN_POINT('Ctrl Pts',(-25.0074858315404,-12.691624884986,
114.59172953676)) ;
#178133 = CARTESIAN_POINT('Ctrl Pts',(-25.0812896952679,-12.6916249659511,
114.567498556927)) ;
#178134 = CARTESIAN_POINT('Ctrl Pts',(-25.1550935589954,-12.6916250469162,
114.543267577095)) ;
#178135 = CARTESIAN_POINT('Ctrl Pts',(-25.1365175245661,-12.7386910562247,
114.486687971447)) ;
#178136 = CARTESIAN_POINT('Ctrl Pts',(-25.0603010182413,-12.5375785963018,
114.290016712916)) ;
#178137 = CARTESIAN_POINT('Ctrl Pts',(-25.046284425511,-12.5987561417494,
114.247324431092)) ;
#178138 = CARTESIAN_POINT('Ctrl Pts',(-24.9724805567354,-12.5987560832211,
114.271555395549)) ;
#178139 = CARTESIAN_POINT('Ctrl Pts',(-24.8986766879599,-12.5987560246928,
114.295786360006)) ;
#178140 = CARTESIAN_POINT('Ctrl Pts',(-24.9126932806902,-12.5375784792451,
114.33847864183)) ;
#178141 = CARTESIAN_POINT('Ctrl Pts',(-24.9267098734205,-12.4764009337975,
114.381170923654)) ;
#178142 = CARTESIAN_POINT('Ctrl Pts',(-25.0005137421961,-12.4764009923258,
114.356939959197)) ;
#178143 = CARTESIAN_POINT('Ctrl Pts',(-25.0743176109717,-12.4764010508541,
114.33270899474)) ;
#178144 = CARTESIAN_POINT('Ctrl Pts',(-25.0603010182413,-12.5375785963018,
114.290016712916)) ;
#178145 = CARTESIAN_POINT('Ctrl Pts',(-24.9698092052317,-12.3995778757378,
114.049856870399)) ;
#178146 = CARTESIAN_POINT('Ctrl Pts',(-24.9613556898593,-12.4704821067912,
114.024108824699)) ;
#178147 = CARTESIAN_POINT('Ctrl Pts',(-24.88755181852,-12.4704820736808,114.048339781347)) ;
#178148 = CARTESIAN_POINT('Ctrl Pts',(-24.8137479471808,-12.4704820405704,
114.072570737995)) ;
#178149 = CARTESIAN_POINT('Ctrl Pts',(-24.8222014625532,-12.399577809517,
114.098318783695)) ;
#178150 = CARTESIAN_POINT('Ctrl Pts',(-24.8306549779257,-12.3286735784636,
114.124066829395)) ;
#178151 = CARTESIAN_POINT('Ctrl Pts',(-24.9044588492649,-12.328673611574,
114.099835872747)) ;
#178152 = CARTESIAN_POINT('Ctrl Pts',(-24.9782627206042,-12.3286736446844,
114.075604916098)) ;
#178153 = CARTESIAN_POINT('Ctrl Pts',(-24.9698092052317,-12.3995778757378,
114.049856870399)) ;
#178154 = CARTESIAN_POINT('Ctrl Pts',(-24.8707009033833,-12.3345174279643,
113.783475116184)) ;
#178155 = CARTESIAN_POINT('Ctrl Pts',(-24.8684199267263,-12.4100708039264,
113.776527627588)) ;
#178156 = CARTESIAN_POINT('Ctrl Pts',(-24.794616055458,-12.4100707963706,
113.800758584453)) ;
#178157 = CARTESIAN_POINT('Ctrl Pts',(-24.7208121841896,-12.4100707888147,
113.824989541317)) ;
#178158 = CARTESIAN_POINT('Ctrl Pts',(-24.7230931608466,-12.3345174128525,
113.831937029912)) ;
#178159 = CARTESIAN_POINT('Ctrl Pts',(-24.7253741375036,-12.2589640368904,
113.838884518507)) ;
#178160 = CARTESIAN_POINT('Ctrl Pts',(-24.7991780087719,-12.2589640444462,
113.814653561643)) ;
#178161 = CARTESIAN_POINT('Ctrl Pts',(-24.8729818800402,-12.2589640520021,
113.790422604779)) ;
#178162 = CARTESIAN_POINT('Ctrl Pts',(-24.8707009033833,-12.3345174279643,
113.783475116184)) ;
#178163 = CARTESIAN_POINT('Ctrl Pts',(-24.7695605990675,-12.3471393395654,
113.510844338411)) ;
#178164 = CARTESIAN_POINT('Ctrl Pts',(-24.773604630639,-12.4219252940087,
113.523161804465)) ;
#178165 = CARTESIAN_POINT('Ctrl Pts',(-24.6998007616627,-12.4219253092695,
113.54739276831)) ;
#178166 = CARTESIAN_POINT('Ctrl Pts',(-24.6259968926864,-12.4219253245303,
113.571623732156)) ;
#178167 = CARTESIAN_POINT('Ctrl Pts',(-24.621952861115,-12.347139370087,113.559306266102)) ;
#178168 = CARTESIAN_POINT('Ctrl Pts',(-24.6179088295436,-12.2723534156437,
113.546988800049)) ;
#178169 = CARTESIAN_POINT('Ctrl Pts',(-24.6917126985198,-12.272353400383,
113.522757836203)) ;
#178170 = CARTESIAN_POINT('Ctrl Pts',(-24.7655165674961,-12.2723533851222,
113.498526872358)) ;
#178171 = CARTESIAN_POINT('Ctrl Pts',(-24.7695605990675,-12.3471393395654,
113.510844338411)) ;
#178172 = CARTESIAN_POINT('Ctrl Pts',(-24.6727328214046,-12.4360428670471,
113.251326381663)) ;
#178173 = CARTESIAN_POINT('Ctrl Pts',(-24.6828107853567,-12.5047344738789,
113.282022232306)) ;
#178174 = CARTESIAN_POINT('Ctrl Pts',(-24.6090069204631,-12.5047345075886,
113.306253208587)) ;
#178175 = CARTESIAN_POINT('Ctrl Pts',(-24.5352030555695,-12.5047345412984,
113.330484184867)) ;
#178176 = CARTESIAN_POINT('Ctrl Pts',(-24.5251250916174,-12.4360429344666,
113.299788334225)) ;
#178177 = CARTESIAN_POINT('Ctrl Pts',(-24.5150471276653,-12.3673513276347,
113.269092483582)) ;
#178178 = CARTESIAN_POINT('Ctrl Pts',(-24.5888509925589,-12.367351293925,
113.244861507301)) ;
#178179 = CARTESIAN_POINT('Ctrl Pts',(-24.6626548574524,-12.3673512602152,
113.220630531021)) ;
#178180 = CARTESIAN_POINT('Ctrl Pts',(-24.6727328214046,-12.4360428670471,
113.251326381663)) ;
#178181 = CARTESIAN_POINT('Ctrl Pts',(-24.5859199646112,-12.5962612233629,
113.022510647249)) ;
#178182 = CARTESIAN_POINT('Ctrl Pts',(-24.6013377912514,-12.6538708074165,
113.069470858232)) ;
#178183 = CARTESIAN_POINT('Ctrl Pts',(-24.5275339320715,-12.6538708522854,
113.093701851916)) ;
#178184 = CARTESIAN_POINT('Ctrl Pts',(-24.4537300728915,-12.6538708971542,
113.117932845599)) ;
#178185 = CARTESIAN_POINT('Ctrl Pts',(-24.4383122462512,-12.5962613131006,
113.070972634616)) ;
#178186 = CARTESIAN_POINT('Ctrl Pts',(-24.422894419611,-12.538651729047,113.024012423633)) ;
#178187 = CARTESIAN_POINT('Ctrl Pts',(-24.4966982787909,-12.5386516841781,
112.99978142995)) ;
#178188 = CARTESIAN_POINT('Ctrl Pts',(-24.5705021379709,-12.5386516393093,
112.975550436267)) ;
#178189 = CARTESIAN_POINT('Ctrl Pts',(-24.5859199646112,-12.5962612233629,
113.022510647249)) ;
#178190 = CARTESIAN_POINT('Ctrl Pts',(-24.5156431401964,-12.8139558923281,
112.843788818509)) ;
#178191 = CARTESIAN_POINT('Ctrl Pts',(-24.5352599429621,-12.8564528958473,
112.903538433404)) ;
#178192 = CARTESIAN_POINT('Ctrl Pts',(-24.4614560892477,-12.8564529465473,
112.927769443735)) ;
#178193 = CARTESIAN_POINT('Ctrl Pts',(-24.3876522355332,-12.8564529972473,
112.952000454065)) ;
#178194 = CARTESIAN_POINT('Ctrl Pts',(-24.3680354327674,-12.8139559937281,
112.89225083917)) ;
#178195 = CARTESIAN_POINT('Ctrl Pts',(-24.3484186300016,-12.7714589902089,
112.832501224274)) ;
#178196 = CARTESIAN_POINT('Ctrl Pts',(-24.4222224837161,-12.7714589395089,
112.808270213944)) ;
#178197 = CARTESIAN_POINT('Ctrl Pts',(-24.4960263374306,-12.7714588888089,
112.784039203613)) ;
#178198 = CARTESIAN_POINT('Ctrl Pts',(-24.5156431401964,-12.8139558923281,
112.843788818509)) ;
#178199 = CARTESIAN_POINT('Ctrl Pts',(-24.4652008507486,-13.0756188660845,
112.725627916536)) ;
#178200 = CARTESIAN_POINT('Ctrl Pts',(-24.4876351956627,-13.0999108300579,
112.793959310375)) ;
#178201 = CARTESIAN_POINT('Ctrl Pts',(-24.41383134743,-13.0999108795098,112.818190337402)) ;
#178202 = CARTESIAN_POINT('Ctrl Pts',(-24.3400274991972,-13.0999109289618,
112.842421364429)) ;
#178203 = CARTESIAN_POINT('Ctrl Pts',(-24.3175931542831,-13.0756189649884,
112.77408997059)) ;
#178204 = CARTESIAN_POINT('Ctrl Pts',(-24.2951588093689,-13.051327001015,
112.705758576751)) ;
#178205 = CARTESIAN_POINT('Ctrl Pts',(-24.3689626576016,-13.0513269515631,
112.681527549724)) ;
#178206 = CARTESIAN_POINT('Ctrl Pts',(-24.4427665058344,-13.0513269021111,
112.657296522697)) ;
#178207 = CARTESIAN_POINT('Ctrl Pts',(-24.4652008507486,-13.0756188660845,
112.725627916536)) ;
#178208 = CARTESIAN_POINT('Ctrl Pts',(-24.4379052691479,-13.3624251132735,
112.678030789951)) ;
#178209 = CARTESIAN_POINT('Ctrl Pts',(-24.4615441067479,-13.3667285784785,
112.75003087435)) ;
#178210 = CARTESIAN_POINT('Ctrl Pts',(-24.3877402628968,-13.3667286208057,
112.774261914723)) ;
#178211 = CARTESIAN_POINT('Ctrl Pts',(-24.3139364190456,-13.3667286631328,
112.798492955095)) ;
#178212 = CARTESIAN_POINT('Ctrl Pts',(-24.2902975814456,-13.3624251979278,
112.726492870696)) ;
#178213 = CARTESIAN_POINT('Ctrl Pts',(-24.2666587438456,-13.3581217327227,
112.654492786297)) ;
#178214 = CARTESIAN_POINT('Ctrl Pts',(-24.3404625876968,-13.3581216903956,
112.630261745925)) ;
#178215 = CARTESIAN_POINT('Ctrl Pts',(-24.4142664315479,-13.3581216480684,
112.606030705552)) ;
#178216 = CARTESIAN_POINT('Ctrl Pts',(-24.4379052691479,-13.3624251132735,
112.678030789951)) ;
#178217 = CARTESIAN_POINT('Ctrl Pts',(-24.4348796019806,-13.651982180129,
112.704196399724)) ;
#178218 = CARTESIAN_POINT('Ctrl Pts',(-24.4580333293247,-13.6360746304586,
112.774718916708)) ;
#178219 = CARTESIAN_POINT('Ctrl Pts',(-24.3842294884877,-13.6360746639262,
112.798949966261)) ;
#178220 = CARTESIAN_POINT('Ctrl Pts',(-24.3104256476508,-13.6360746973937,
112.823181015814)) ;
#178221 = CARTESIAN_POINT('Ctrl Pts',(-24.2872719203067,-13.651982247064,
112.752658498831)) ;
#178222 = CARTESIAN_POINT('Ctrl Pts',(-24.2641181929626,-13.6678897967344,
112.682135981847)) ;
#178223 = CARTESIAN_POINT('Ctrl Pts',(-24.3379220337996,-13.6678897632668,
112.657904932294)) ;
#178224 = CARTESIAN_POINT('Ctrl Pts',(-24.4117258746365,-13.6678897297993,
112.63367388274)) ;
#178225 = CARTESIAN_POINT('Ctrl Pts',(-24.4348796019806,-13.651982180129,
112.704196399724)) ;
#178226 = CARTESIAN_POINT('Ctrl Pts',(-24.4558001085789,-13.9268736432231,
112.803588355088)) ;
#178227 = CARTESIAN_POINT('Ctrl Pts',(-24.4767901805327,-13.8917477253801,
112.867520727055)) ;
#178228 = CARTESIAN_POINT('Ctrl Pts',(-24.4029863408681,-13.8917477464933,
112.891751780179)) ;
#178229 = CARTESIAN_POINT('Ctrl Pts',(-24.3291825012035,-13.8917477676065,
112.915982833304)) ;
#178230 = CARTESIAN_POINT('Ctrl Pts',(-24.3081924292497,-13.9268736854496,
112.852050461337)) ;
#178231 = CARTESIAN_POINT('Ctrl Pts',(-24.2872023572959,-13.9619996032926,
112.78811808937)) ;
#178232 = CARTESIAN_POINT('Ctrl Pts',(-24.3610061969605,-13.9619995821794,
112.763887036245)) ;
#178233 = CARTESIAN_POINT('Ctrl Pts',(-24.4348100366251,-13.9619995610662,
112.739655983121)) ;
#178234 = CARTESIAN_POINT('Ctrl Pts',(-24.4558001085789,-13.9268736432231,
112.803588355088)) ;
#178235 = CARTESIAN_POINT('Ctrl Pts',(-24.4978634283469,-14.1624927779437,
112.966970517185)) ;
#178236 = CARTESIAN_POINT('Ctrl Pts',(-24.515218335732,-14.1108622061885,
113.019830764522)) ;
#178237 = CARTESIAN_POINT('Ctrl Pts',(-24.4414144963545,-14.1108622190925,
113.044061818521)) ;
#178238 = CARTESIAN_POINT('Ctrl Pts',(-24.367610656977,-14.1108622319965,
113.06829287252)) ;
#178239 = CARTESIAN_POINT('Ctrl Pts',(-24.3502557495919,-14.1624928037518,
113.015432625182)) ;
#178240 = CARTESIAN_POINT('Ctrl Pts',(-24.3329008422068,-14.214123375507,
112.962572377844)) ;
#178241 = CARTESIAN_POINT('Ctrl Pts',(-24.4067046815843,-14.214123362603,
112.938341323845)) ;
#178242 = CARTESIAN_POINT('Ctrl Pts',(-24.4805085209618,-14.214123349699,
112.914110269847)) ;
#178243 = CARTESIAN_POINT('Ctrl Pts',(-24.4978634283469,-14.1624927779437,
112.966970517185)) ;
#178244 = CARTESIAN_POINT('Ctrl Pts',(-24.5579911299017,-14.3467872124729,
113.185684905417)) ;
#178245 = CARTESIAN_POINT('Ctrl Pts',(-24.5704376669349,-14.28220994504,113.223595048778)) ;
#178246 = CARTESIAN_POINT('Ctrl Pts',(-24.496633826401,-14.2822099499131,
113.247826099254)) ;
#178247 = CARTESIAN_POINT('Ctrl Pts',(-24.4228299858672,-14.2822099547862,
113.272057149731)) ;
#178248 = CARTESIAN_POINT('Ctrl Pts',(-24.410383448834,-14.346787222219,113.23414700637)) ;
#178249 = CARTESIAN_POINT('Ctrl Pts',(-24.3979369118009,-14.4113644896518,
113.19623686301)) ;
#178250 = CARTESIAN_POINT('Ctrl Pts',(-24.4717407523347,-14.4113644847787,
113.172005812533)) ;
#178251 = CARTESIAN_POINT('Ctrl Pts',(-24.5455445928685,-14.4113644799057,
113.147774762056)) ;
#178252 = CARTESIAN_POINT('Ctrl Pts',(-24.5579911299017,-14.3467872124729,
113.185684905417)) ;
#178253 = CARTESIAN_POINT('Ctrl Pts',(-24.6305363548121,-14.4636106389172,
113.442047638809)) ;
#178254 = CARTESIAN_POINT('Ctrl Pts',(-24.6372034400423,-14.3907789878482,
113.462354504594)) ;
#178255 = CARTESIAN_POINT('Ctrl Pts',(-24.5633995981574,-14.3907789888133,
113.486585550955)) ;
#178256 = CARTESIAN_POINT('Ctrl Pts',(-24.4895957562725,-14.3907789897784,
113.510816597317)) ;
#178257 = CARTESIAN_POINT('Ctrl Pts',(-24.4829286710424,-14.4636106408474,
113.490509731532)) ;
#178258 = CARTESIAN_POINT('Ctrl Pts',(-24.4762615858122,-14.5364422919164,
113.470202865748)) ;
#178259 = CARTESIAN_POINT('Ctrl Pts',(-24.5500654276971,-14.5364422909513,
113.445971819386)) ;
#178260 = CARTESIAN_POINT('Ctrl Pts',(-24.623869269582,-14.5364422899862,
113.421740773025)) ;
#178261 = CARTESIAN_POINT('Ctrl Pts',(-24.6305363548121,-14.4636106389172,
113.442047638809)) ;
#178262 = CARTESIAN_POINT('Ctrl Pts',(-24.7098618797107,-14.505904926533,
113.719115599711)) ;
#178263 = CARTESIAN_POINT('Ctrl Pts',(-24.710266161591,-14.4300107624531,
113.72034697708)) ;
#178264 = CARTESIAN_POINT('Ctrl Pts',(-24.6364623183247,-14.430010762108,
113.744578019233)) ;
#178265 = CARTESIAN_POINT('Ctrl Pts',(-24.5626584750583,-14.430010761763,
113.768809061387)) ;
#178266 = CARTESIAN_POINT('Ctrl Pts',(-24.562254193178,-14.5059049258428,
113.767577684019)) ;
#178267 = CARTESIAN_POINT('Ctrl Pts',(-24.5618499112976,-14.5817990899227,
113.766346306651)) ;
#178268 = CARTESIAN_POINT('Ctrl Pts',(-24.635653754564,-14.5817990902678,
113.742115264497)) ;
#178269 = CARTESIAN_POINT('Ctrl Pts',(-24.7094575978303,-14.5817990906128,
113.717884222343)) ;
#178270 = CARTESIAN_POINT('Ctrl Pts',(-24.7098618797107,-14.505904926533,
113.719115599711)) ;
#178271 = CARTESIAN_POINT('Ctrl Pts',(-24.789457567232,-14.4703681622542,
113.996992018783)) ;
#178272 = CARTESIAN_POINT('Ctrl Pts',(-24.7835710155258,-14.3968421199682,
113.979062532125)) ;
#178273 = CARTESIAN_POINT('Ctrl Pts',(-24.709767171351,-14.3968421204311,
114.003293571512)) ;
#178274 = CARTESIAN_POINT('Ctrl Pts',(-24.6359633271762,-14.3968421208941,
114.027524610899)) ;
#178275 = CARTESIAN_POINT('Ctrl Pts',(-24.6418498788825,-14.4703681631801,
114.045454097557)) ;
#178276 = CARTESIAN_POINT('Ctrl Pts',(-24.6477364305887,-14.5438942054661,
114.063383584214)) ;
#178277 = CARTESIAN_POINT('Ctrl Pts',(-24.7215402747635,-14.5438942050032,
114.039152544827)) ;
#178278 = CARTESIAN_POINT('Ctrl Pts',(-24.7953441189382,-14.5438942045402,
114.01492150544)) ;
#178279 = CARTESIAN_POINT('Ctrl Pts',(-24.789457567232,-14.4703681622542,
113.996992018783)) ;
#178280 = CARTESIAN_POINT('Ctrl Pts',(-24.8630886166822,-14.359008640194,
114.256813432633)) ;
#178281 = CARTESIAN_POINT('Ctrl Pts',(-24.8513157988554,-14.2931494608221,
114.220955329136)) ;
#178282 = CARTESIAN_POINT('Ctrl Pts',(-24.7775119545306,-14.293149462549,
114.245186368066)) ;
#178283 = CARTESIAN_POINT('Ctrl Pts',(-24.7037081102058,-14.2931494642759,
114.269417406996)) ;
#178284 = CARTESIAN_POINT('Ctrl Pts',(-24.7154809280326,-14.3590086436478,
114.305275510493)) ;
#178285 = CARTESIAN_POINT('Ctrl Pts',(-24.7272537458594,-14.4248678230197,
114.341133613991)) ;
#178286 = CARTESIAN_POINT('Ctrl Pts',(-24.8010575901842,-14.4248678212928,
114.316902575061)) ;
#178287 = CARTESIAN_POINT('Ctrl Pts',(-24.874861434509,-14.4248678195659,
114.292671536131)) ;
#178288 = CARTESIAN_POINT('Ctrl Pts',(-24.8630886166822,-14.359008640194,
114.256813432633)) ;
#178289 = CARTESIAN_POINT('Ctrl Pts',(-24.9242076077781,-14.1808823670753,
114.478358262173)) ;
#178290 = CARTESIAN_POINT('Ctrl Pts',(-24.9074173310337,-14.1273644575797,
114.42721778835)) ;
#178291 = CARTESIAN_POINT('Ctrl Pts',(-24.8336134872222,-14.1273644591981,
114.451448828844)) ;
#178292 = CARTESIAN_POINT('Ctrl Pts',(-24.7598096434107,-14.1273644608165,
114.475679869337)) ;
#178293 = CARTESIAN_POINT('Ctrl Pts',(-24.7765999201551,-14.1808823703121,
114.52682034316)) ;
#178294 = CARTESIAN_POINT('Ctrl Pts',(-24.7933901968995,-14.2344002798077,
114.577960816982)) ;
#178295 = CARTESIAN_POINT('Ctrl Pts',(-24.867194040711,-14.2344002781893,
114.553729776489)) ;
#178296 = CARTESIAN_POINT('Ctrl Pts',(-24.9409978845225,-14.2344002765709,
114.529498735995)) ;
#178297 = CARTESIAN_POINT('Ctrl Pts',(-24.9242076077781,-14.1808823670753,
114.478358262173)) ;
#178298 = CARTESIAN_POINT('Ctrl Pts',(-24.9681883548515,-13.9476582149858,
114.647809634132)) ;
#178299 = CARTESIAN_POINT('Ctrl Pts',(-24.9475678449893,-13.9103470808531,
114.585002888174)) ;
#178300 = CARTESIAN_POINT('Ctrl Pts',(-24.8737640018743,-13.9103470799281,
114.609233930789)) ;
#178301 = CARTESIAN_POINT('Ctrl Pts',(-24.7999601587592,-13.910347079003,
114.633464973403)) ;
#178302 = CARTESIAN_POINT('Ctrl Pts',(-24.8205806686214,-13.9476582131357,
114.696271719361)) ;
#178303 = CARTESIAN_POINT('Ctrl Pts',(-24.8412011784836,-13.9849693472685,
114.759078465319)) ;
#178304 = CARTESIAN_POINT('Ctrl Pts',(-24.9150050215986,-13.9849693481935,
114.734847422704)) ;
#178305 = CARTESIAN_POINT('Ctrl Pts',(-24.9888088647137,-13.9849693491186,
114.71061638009)) ;
#178306 = CARTESIAN_POINT('Ctrl Pts',(-24.9681883548515,-13.9476582149858,
114.647809634132)) ;
#178307 = CARTESIAN_POINT('Ctrl Pts',(-24.9908627448388,-13.6767014389998,
114.75232403868)) ;
#178308 = CARTESIAN_POINT('Ctrl Pts',(-24.9678952272064,-13.6582555044241,
114.682368685648)) ;
#178309 = CARTESIAN_POINT('Ctrl Pts',(-24.8940913843963,-13.6582554985914,
114.706599729192)) ;
#178310 = CARTESIAN_POINT('Ctrl Pts',(-24.8202875415862,-13.6582554927588,
114.730830772735)) ;
#178311 = CARTESIAN_POINT('Ctrl Pts',(-24.8432550592186,-13.6767014273345,
114.800786125767)) ;
#178312 = CARTESIAN_POINT('Ctrl Pts',(-24.866222576851,-13.6951473619102,
114.870741478798)) ;
#178313 = CARTESIAN_POINT('Ctrl Pts',(-24.9400264196611,-13.6951473677429,
114.846510435255)) ;
#178314 = CARTESIAN_POINT('Ctrl Pts',(-25.0138302624712,-13.6951473735755,
114.822279391711)) ;
#178315 = CARTESIAN_POINT('Ctrl Pts',(-24.9908627448388,-13.6767014389998,
114.75232403868)) ;
#178316 = CARTESIAN_POINT('Ctrl Pts',(-24.9899695835005,-13.3872299120028,
114.785058404499)) ;
#178317 = CARTESIAN_POINT('Ctrl Pts',(-24.966297312444,-13.3889692104813,
114.712956486132)) ;
#178318 = CARTESIAN_POINT('Ctrl Pts',(-24.8924934691212,-13.388969198278,
114.737187528114)) ;
#178319 = CARTESIAN_POINT('Ctrl Pts',(-24.8186896257984,-13.3889691860747,
114.761418570096)) ;
#178320 = CARTESIAN_POINT('Ctrl Pts',(-24.8423618968549,-13.3872298875961,
114.833520488463)) ;
#178321 = CARTESIAN_POINT('Ctrl Pts',(-24.8660341679114,-13.3854905891176,
114.90562240683)) ;
#178322 = CARTESIAN_POINT('Ctrl Pts',(-24.9398380112342,-13.385490601321,
114.881391364848)) ;
#178323 = CARTESIAN_POINT('Ctrl Pts',(-25.013641854557,-13.3854906135243,
114.857160322866)) ;
#178324 = CARTESIAN_POINT('Ctrl Pts',(-24.9899695835005,-13.3872299120028,
114.785058404499)) ;
#178325 = CARTESIAN_POINT('Ctrl Pts',(-24.9646913454561,-13.0993467868879,
114.743596413779)) ;
#178326 = CARTESIAN_POINT('Ctrl Pts',(-24.9420143908797,-13.1211895488815,
114.674526068666)) ;
#178327 = CARTESIAN_POINT('Ctrl Pts',(-24.8682105458579,-13.1211895296054,
114.698757105473)) ;
#178328 = CARTESIAN_POINT('Ctrl Pts',(-24.7944067008361,-13.1211895103292,
114.722988142281)) ;
#178329 = CARTESIAN_POINT('Ctrl Pts',(-24.8170836554125,-13.0993467483356,
114.792058487393)) ;
#178330 = CARTESIAN_POINT('Ctrl Pts',(-24.8397606099889,-13.077503986342,
114.861128832505)) ;
#178331 = CARTESIAN_POINT('Ctrl Pts',(-24.9135644550107,-13.0775040056182,
114.836897795698)) ;
#178332 = CARTESIAN_POINT('Ctrl Pts',(-24.9873683000325,-13.0775040248944,
114.812666758891)) ;
#178333 = CARTESIAN_POINT('Ctrl Pts',(-24.9646913454561,-13.0993467868879,
114.743596413779)) ;
#178334 = CARTESIAN_POINT('Ctrl Pts',(-24.9162024965776,-12.8349662721153,
114.631357615901)) ;
#178335 = CARTESIAN_POINT('Ctrl Pts',(-24.8961447139292,-12.8753001510476,
114.570264845728)) ;
#178336 = CARTESIAN_POINT('Ctrl Pts',(-24.8223408660553,-12.8753001272113,
114.594495873848)) ;
#178337 = CARTESIAN_POINT('Ctrl Pts',(-24.7485370181815,-12.875300103375,
114.618726901968)) ;
#178338 = CARTESIAN_POINT('Ctrl Pts',(-24.7685948008298,-12.8349662244428,
114.679819672141)) ;
#178339 = CARTESIAN_POINT('Ctrl Pts',(-24.7886525834782,-12.7946323455105,
114.740912442314)) ;
#178340 = CARTESIAN_POINT('Ctrl Pts',(-24.8624564313521,-12.7946323693468,
114.716681414194)) ;
#178341 = CARTESIAN_POINT('Ctrl Pts',(-24.936260279226,-12.7946323931831,
114.692450386074)) ;
#178342 = CARTESIAN_POINT('Ctrl Pts',(-24.9162024965776,-12.8349662721153,
114.631357615901)) ;
#178343 = CARTESIAN_POINT('Ctrl Pts',(-24.847245455251,-12.6123125745559,
114.45676980248)) ;
#178344 = CARTESIAN_POINT('Ctrl Pts',(-24.8312398686168,-12.6682505751424,
114.408019367388)) ;
#178345 = CARTESIAN_POINT('Ctrl Pts',(-24.7574360170475,-12.6682505503797,
114.432250384252)) ;
#178346 = CARTESIAN_POINT('Ctrl Pts',(-24.6836321654782,-12.6682505256169,
114.456481401117)) ;
#178347 = CARTESIAN_POINT('Ctrl Pts',(-24.6996377521124,-12.6123125250304,
114.505231836208)) ;
#178348 = CARTESIAN_POINT('Ctrl Pts',(-24.7156433387467,-12.5563745244438,
114.5539822713)) ;
#178349 = CARTESIAN_POINT('Ctrl Pts',(-24.7894471903159,-12.5563745492066,
114.529751254436)) ;
#178350 = CARTESIAN_POINT('Ctrl Pts',(-24.8632510418852,-12.5563745739693,
114.505520237572)) ;
#178351 = CARTESIAN_POINT('Ctrl Pts',(-24.847245455251,-12.6123125745559,
114.45676980248)) ;
#178352 = CARTESIAN_POINT('Ctrl Pts',(-24.7618055368288,-12.447065748415,
114.232038687256)) ;
#178353 = CARTESIAN_POINT('Ctrl Pts',(-24.7510075081186,-12.5146221963664,
114.199149633188)) ;
#178354 = CARTESIAN_POINT('Ctrl Pts',(-24.6772036522679,-12.5146221752964,
114.223380637012)) ;
#178355 = CARTESIAN_POINT('Ctrl Pts',(-24.6033997964171,-12.5146221542264,
114.247611640836)) ;
#178356 = CARTESIAN_POINT('Ctrl Pts',(-24.6141978251274,-12.4470657062751,
114.280500694904)) ;
#178357 = CARTESIAN_POINT('Ctrl Pts',(-24.6249958538377,-12.3795092583237,
114.313389748971)) ;
#178358 = CARTESIAN_POINT('Ctrl Pts',(-24.6987997096884,-12.3795092793937,
114.289158745147)) ;
#178359 = CARTESIAN_POINT('Ctrl Pts',(-24.7726035655391,-12.3795093004636,
114.264927741324)) ;
#178360 = CARTESIAN_POINT('Ctrl Pts',(-24.7618055368288,-12.447065748415,
114.232038687256)) ;
#178361 = CARTESIAN_POINT('Ctrl Pts',(-24.6654288827052,-12.3516677675638,
113.973971864171)) ;
#178362 = CARTESIAN_POINT('Ctrl Pts',(-24.6606099935128,-12.4259824807609,
113.959294304173)) ;
#178363 = CARTESIAN_POINT('Ctrl Pts',(-24.5868061336476,-12.4259824693785,
113.983525295769)) ;
#178364 = CARTESIAN_POINT('Ctrl Pts',(-24.5130022737824,-12.425982457996,
114.007756287365)) ;
#178365 = CARTESIAN_POINT('Ctrl Pts',(-24.5178211629749,-12.3516677447989,
114.022433847364)) ;
#178366 = CARTESIAN_POINT('Ctrl Pts',(-24.5226400521673,-12.2773530316018,
114.037111407362)) ;
#178367 = CARTESIAN_POINT('Ctrl Pts',(-24.5964439120325,-12.2773530429843,
114.012880415766)) ;
#178368 = CARTESIAN_POINT('Ctrl Pts',(-24.6702477718977,-12.2773530543667,
113.988649424169)) ;
#178369 = CARTESIAN_POINT('Ctrl Pts',(-24.6654288827052,-12.3516677675638,
113.973971864171)) ;
#178370 = CARTESIAN_POINT('Ctrl Pts',(-24.5645423752006,-12.3325934792249,
113.702063110992)) ;
#178371 = CARTESIAN_POINT('Ctrl Pts',(-24.566028277542,-12.4083470766961,
113.706588928583)) ;
#178372 = CARTESIAN_POINT('Ctrl Pts',(-24.4922244149365,-12.4083470802209,
113.730819911833)) ;
#178373 = CARTESIAN_POINT('Ctrl Pts',(-24.418420552331,-12.4083470837456,
113.755050895082)) ;
#178374 = CARTESIAN_POINT('Ctrl Pts',(-24.4169346499896,-12.3325934862743,
113.750525077491)) ;
#178375 = CARTESIAN_POINT('Ctrl Pts',(-24.4154487476482,-12.256839888803,
113.7459992599)) ;
#178376 = CARTESIAN_POINT('Ctrl Pts',(-24.4892526102537,-12.2568398852783,
113.72176827665)) ;
#178377 = CARTESIAN_POINT('Ctrl Pts',(-24.5630564728592,-12.2568398817536,
113.697537293401)) ;
#178378 = CARTESIAN_POINT('Ctrl Pts',(-24.5645423752006,-12.3325934792249,
113.702063110992)) ;
#178379 = CARTESIAN_POINT('Ctrl Pts',(-24.4649295396859,-12.3910918553195,
113.434163508363)) ;
#178380 = CARTESIAN_POINT('Ctrl Pts',(-24.4726376582911,-12.4628709667284,
113.457641192575)) ;
#178381 = CARTESIAN_POINT('Ctrl Pts',(-24.3988337941039,-12.4628709892207,
113.481872171008)) ;
#178382 = CARTESIAN_POINT('Ctrl Pts',(-24.3250299299166,-12.4628710117129,
113.50610314944)) ;
#178383 = CARTESIAN_POINT('Ctrl Pts',(-24.3173218113114,-12.3910919003041,
113.482625465227)) ;
#178384 = CARTESIAN_POINT('Ctrl Pts',(-24.3096136927062,-12.3193127888952,
113.459147781014)) ;
#178385 = CARTESIAN_POINT('Ctrl Pts',(-24.3834175568935,-12.319312766403,
113.434916802582)) ;
#178386 = CARTESIAN_POINT('Ctrl Pts',(-24.4572214210807,-12.3193127439107,
113.41068582415)) ;
#178387 = CARTESIAN_POINT('Ctrl Pts',(-24.4649295396859,-12.3910918553195,
113.434163508363)) ;
#178388 = CARTESIAN_POINT('Ctrl Pts',(-24.37322692579,-12.5239274893633,113.190432787571)) ;
#178389 = CARTESIAN_POINT('Ctrl Pts',(-24.3866124525482,-12.5865367592055,
113.231202940804)) ;
#178390 = CARTESIAN_POINT('Ctrl Pts',(-24.3128085888032,-12.5865368036991,
113.255433920583)) ;
#178391 = CARTESIAN_POINT('Ctrl Pts',(-24.2390047250582,-12.5865368481928,
113.279664900362)) ;
#178392 = CARTESIAN_POINT('Ctrl Pts',(-24.2256191983,-12.5239275783507,113.238894747129)) ;
#178393 = CARTESIAN_POINT('Ctrl Pts',(-24.2122336715418,-12.4613183085085,
113.198124593896)) ;
#178394 = CARTESIAN_POINT('Ctrl Pts',(-24.2860375352869,-12.4613182640148,
113.173893614117)) ;
#178395 = CARTESIAN_POINT('Ctrl Pts',(-24.3598413990319,-12.4613182195212,
113.149662634338)) ;
#178396 = CARTESIAN_POINT('Ctrl Pts',(-24.37322692579,-12.5239274893633,113.190432787571)) ;
#178397 = CARTESIAN_POINT('Ctrl Pts',(-24.2960054560042,-12.7192927751428,
112.990520520361)) ;
#178398 = CARTESIAN_POINT('Ctrl Pts',(-24.3140714527538,-12.7683526424801,
113.045546629888)) ;
#178399 = CARTESIAN_POINT('Ctrl Pts',(-24.2402675922761,-12.7683527070147,
113.069777619618)) ;
#178400 = CARTESIAN_POINT('Ctrl Pts',(-24.1664637317984,-12.7683527715494,
113.094008609349)) ;
#178401 = CARTESIAN_POINT('Ctrl Pts',(-24.1483977350488,-12.719292904212,
113.038982499823)) ;
#178402 = CARTESIAN_POINT('Ctrl Pts',(-24.1303317382993,-12.6702330368747,
112.983956390296)) ;
#178403 = CARTESIAN_POINT('Ctrl Pts',(-24.2041355987769,-12.67023297234,112.959725400566)) ;
#178404 = CARTESIAN_POINT('Ctrl Pts',(-24.2779394592546,-12.6702329078054,
112.935494410835)) ;
#178405 = CARTESIAN_POINT('Ctrl Pts',(-24.2960054560042,-12.7192927751428,
112.990520520361)) ;
#178406 = CARTESIAN_POINT('Ctrl Pts',(-24.2369143117434,-12.9658343070978,
112.84605739491)) ;
#178407 = CARTESIAN_POINT('Ctrl Pts',(-24.2583972142561,-12.9977530103242,
112.911490847945)) ;
#178408 = CARTESIAN_POINT('Ctrl Pts',(-24.1845933588617,-12.9977530931819,
112.935721853159)) ;
#178409 = CARTESIAN_POINT('Ctrl Pts',(-24.1107895034674,-12.9977531760396,
112.959952858372)) ;
#178410 = CARTESIAN_POINT('Ctrl Pts',(-24.0893066009546,-12.9658344728131,
112.894519405337)) ;
#178411 = CARTESIAN_POINT('Ctrl Pts',(-24.0678236984419,-12.9339157695866,
112.829085952303)) ;
#178412 = CARTESIAN_POINT('Ctrl Pts',(-24.1416275538363,-12.9339156867289,
112.804854947089)) ;
#178413 = CARTESIAN_POINT('Ctrl Pts',(-24.2154314092307,-12.9339156038712,
112.780623941875)) ;
#178414 = CARTESIAN_POINT('Ctrl Pts',(-24.2369143117434,-12.9658343070978,
112.84605739491)) ;
#178415 = CARTESIAN_POINT('Ctrl Pts',(-24.2000431301647,-13.2443245338218,
112.769193829695)) ;
#178416 = CARTESIAN_POINT('Ctrl Pts',(-24.2233982405961,-13.2568466102088,
112.840329725867)) ;
#178417 = CARTESIAN_POINT('Ctrl Pts',(-24.149594392237,-13.2568467056125,
112.864560752509)) ;
#178418 = CARTESIAN_POINT('Ctrl Pts',(-24.0757905438778,-13.2568468010161,
112.888791779151)) ;
#178419 = CARTESIAN_POINT('Ctrl Pts',(-24.0524354334464,-13.2443247246291,
112.817655882979)) ;
#178420 = CARTESIAN_POINT('Ctrl Pts',(-24.029080323015,-13.2318026482422,
112.746519986807)) ;
#178421 = CARTESIAN_POINT('Ctrl Pts',(-24.1028841713741,-13.2318025528385,
112.722288960165)) ;
#178422 = CARTESIAN_POINT('Ctrl Pts',(-24.1766880197333,-13.2318024574349,
112.698057933523)) ;
#178423 = CARTESIAN_POINT('Ctrl Pts',(-24.2000431301647,-13.2443245338218,
112.769193829695)) ;
#178424 = CARTESIAN_POINT('Ctrl Pts',(-24.187186648989,-13.5367809605308,
112.765670474547)) ;
#178425 = CARTESIAN_POINT('Ctrl Pts',(-24.210736331474,-13.5289033830346,
112.8373990057)) ;
#178426 = CARTESIAN_POINT('Ctrl Pts',(-24.1369324914405,-13.5289034843527,
112.8616300577)) ;
#178427 = CARTESIAN_POINT('Ctrl Pts',(-24.063128651407,-13.5289035856708,
112.885861109701)) ;
#178428 = CARTESIAN_POINT('Ctrl Pts',(-24.039578968922,-13.536781163167,112.814132578548)) ;
#178429 = CARTESIAN_POINT('Ctrl Pts',(-24.0160292864371,-13.5446587406632,
112.742404047396)) ;
#178430 = CARTESIAN_POINT('Ctrl Pts',(-24.0898331264706,-13.5446586393451,
112.718172995395)) ;
#178431 = CARTESIAN_POINT('Ctrl Pts',(-24.1636369665041,-13.544658538027,
112.693941943395)) ;
#178432 = CARTESIAN_POINT('Ctrl Pts',(-24.187186648989,-13.5367809605308,
112.765670474547)) ;
#178433 = CARTESIAN_POINT('Ctrl Pts',(-24.198485812454,-13.8179726435299,
112.835367593194)) ;
#178434 = CARTESIAN_POINT('Ctrl Pts',(-24.2205509613614,-13.790451684124,
112.902574474547)) ;
#178435 = CARTESIAN_POINT('Ctrl Pts',(-24.146747129892,-13.7904517814122,
112.926805552632)) ;
#178436 = CARTESIAN_POINT('Ctrl Pts',(-24.0729432984226,-13.7904518787005,
112.951036630717)) ;
#178437 = CARTESIAN_POINT('Ctrl Pts',(-24.0508781495152,-13.8179728381065,
112.883829749365)) ;
#178438 = CARTESIAN_POINT('Ctrl Pts',(-24.0288130006078,-13.8454937975124,
112.816622868012)) ;
#178439 = CARTESIAN_POINT('Ctrl Pts',(-24.1026168320772,-13.8454937002241,
112.792391789926)) ;
#178440 = CARTESIAN_POINT('Ctrl Pts',(-24.1764206635466,-13.8454936029358,
112.768160711841)) ;
#178441 = CARTESIAN_POINT('Ctrl Pts',(-24.198485812454,-13.8179726435299,
112.835367593194)) ;
#178442 = CARTESIAN_POINT('Ctrl Pts',(-24.2324273152291,-14.0724753431544,
112.974281755024)) ;
#178443 = CARTESIAN_POINT('Ctrl Pts',(-24.2514200932839,-14.0271455372004,
113.032130690435)) ;
#178444 = CARTESIAN_POINT('Ctrl Pts',(-24.1776162699435,-14.0271456228523,
113.056361793279)) ;
#178445 = CARTESIAN_POINT('Ctrl Pts',(-24.103812446603,-14.0271457085042,
113.080592896124)) ;
#178446 = CARTESIAN_POINT('Ctrl Pts',(-24.0848196685482,-14.0724755144583,
113.022743960713)) ;
#178447 = CARTESIAN_POINT('Ctrl Pts',(-24.0658268904934,-14.1178053204124,
112.964895025302)) ;
#178448 = CARTESIAN_POINT('Ctrl Pts',(-24.1396307138339,-14.1178052347605,
112.940663922457)) ;
#178449 = CARTESIAN_POINT('Ctrl Pts',(-24.2134345371743,-14.1178051491085,
112.916432819612)) ;
#178450 = CARTESIAN_POINT('Ctrl Pts',(-24.2324273152291,-14.0724753431544,
112.974281755024)) ;
#178451 = CARTESIAN_POINT('Ctrl Pts',(-24.2856593105687,-14.279096140685,
113.171804870744)) ;
#178452 = CARTESIAN_POINT('Ctrl Pts',(-24.3002313758955,-14.2192740208291,
113.216189028444)) ;
#178453 = CARTESIAN_POINT('Ctrl Pts',(-24.2264275591958,-14.219274086963,
113.240420151515)) ;
#178454 = CARTESIAN_POINT('Ctrl Pts',(-24.152623742496,-14.219274153097,113.264651274587)) ;
#178455 = CARTESIAN_POINT('Ctrl Pts',(-24.1380516771692,-14.2790962729529,
113.220267116886)) ;
#178456 = CARTESIAN_POINT('Ctrl Pts',(-24.1234796118424,-14.3389183928089,
113.175882959185)) ;
#178457 = CARTESIAN_POINT('Ctrl Pts',(-24.1972834285421,-14.3389183266749,
113.151651836114)) ;
#178458 = CARTESIAN_POINT('Ctrl Pts',(-24.2710872452418,-14.3389182605409,
113.127420713043)) ;
#178459 = CARTESIAN_POINT('Ctrl Pts',(-24.2856593105687,-14.279096140685,
113.171804870744)) ;
#178460 = CARTESIAN_POINT('Ctrl Pts',(-24.3538376843237,-14.4248617955916,
113.414949069186)) ;
#178461 = CARTESIAN_POINT('Ctrl Pts',(-24.3629371876036,-14.3547743304939,
113.442664685881)) ;
#178462 = CARTESIAN_POINT('Ctrl Pts',(-24.2891333755111,-14.3547743715158,
113.466895822985)) ;
#178463 = CARTESIAN_POINT('Ctrl Pts',(-24.2153295634186,-14.3547744125376,
113.491126960089)) ;
#178464 = CARTESIAN_POINT('Ctrl Pts',(-24.2062300601387,-14.4248618776352,
113.463411343394)) ;
#178465 = CARTESIAN_POINT('Ctrl Pts',(-24.1971305568588,-14.4949493427329,
113.435695726699)) ;
#178466 = CARTESIAN_POINT('Ctrl Pts',(-24.2709343689513,-14.494949301711,
113.411464589595)) ;
#178467 = CARTESIAN_POINT('Ctrl Pts',(-24.3447381810438,-14.4949492606892,
113.387233452491)) ;
#178468 = CARTESIAN_POINT('Ctrl Pts',(-24.3538376843237,-14.4248617955916,
113.414949069186)) ;
#178469 = CARTESIAN_POINT('Ctrl Pts',(-24.4316472822689,-14.4982152843021,
113.687591297354)) ;
#178470 = CARTESIAN_POINT('Ctrl Pts',(-24.4345904335442,-14.4229018669145,
113.696555659197)) ;
#178471 = CARTESIAN_POINT('Ctrl Pts',(-24.3607866232635,-14.4229018794509,
113.720786801819)) ;
#178472 = CARTESIAN_POINT('Ctrl Pts',(-24.2869828129827,-14.4229018919873,
113.745017944441)) ;
#178473 = CARTESIAN_POINT('Ctrl Pts',(-24.2840396617074,-14.4982153093749,
113.736053582599)) ;
#178474 = CARTESIAN_POINT('Ctrl Pts',(-24.2810965104321,-14.5735287267625,
113.727089220757)) ;
#178475 = CARTESIAN_POINT('Ctrl Pts',(-24.3549003207128,-14.5735287142261,
113.702858078135)) ;
#178476 = CARTESIAN_POINT('Ctrl Pts',(-24.4287041309936,-14.5735287016897,
113.678626935512)) ;
#178477 = CARTESIAN_POINT('Ctrl Pts',(-24.4316472822689,-14.4982152843021,
113.687591297354)) ;
#178478 = CARTESIAN_POINT('Ctrl Pts',(-24.511415885813,-14.4941260357652,
113.965774681427)) ;
#178479 = CARTESIAN_POINT('Ctrl Pts',(-24.5080653532222,-14.4189866403318,
113.955569497726)) ;
#178480 = CARTESIAN_POINT('Ctrl Pts',(-24.4342615422946,-14.4189866245763,
113.979800638379)) ;
#178481 = CARTESIAN_POINT('Ctrl Pts',(-24.360457731367,-14.4189866088209,
114.004031779031)) ;
#178482 = CARTESIAN_POINT('Ctrl Pts',(-24.3638082639579,-14.4941260042543,
114.014236962732)) ;
#178483 = CARTESIAN_POINT('Ctrl Pts',(-24.3671587965487,-14.5692653996877,
114.024442146433)) ;
#178484 = CARTESIAN_POINT('Ctrl Pts',(-24.4409626074762,-14.5692654154432,
114.00021100578)) ;
#178485 = CARTESIAN_POINT('Ctrl Pts',(-24.5147664184038,-14.5692654311986,
113.975979865128)) ;
#178486 = CARTESIAN_POINT('Ctrl Pts',(-24.511415885813,-14.4941260357652,
113.965774681427)) ;
#178487 = CARTESIAN_POINT('Ctrl Pts',(-24.588572932717,-14.4126782343137,
114.236447003153)) ;
#178488 = CARTESIAN_POINT('Ctrl Pts',(-24.5790926098734,-14.3431123024057,
114.207571467457)) ;
#178489 = CARTESIAN_POINT('Ctrl Pts',(-24.5052887953129,-14.3431122609052,
114.231802597044)) ;
#178490 = CARTESIAN_POINT('Ctrl Pts',(-24.4314849807525,-14.3431122194047,
114.256033726631)) ;
#178491 = CARTESIAN_POINT('Ctrl Pts',(-24.440965303596,-14.4126781513128,
114.284909262327)) ;
#178492 = CARTESIAN_POINT('Ctrl Pts',(-24.4504456264396,-14.4822440832209,
114.313784798023)) ;
#178493 = CARTESIAN_POINT('Ctrl Pts',(-24.5242494410001,-14.4822441247213,
114.289553668436)) ;
#178494 = CARTESIAN_POINT('Ctrl Pts',(-24.5980532555605,-14.4822441662218,
114.265322538849)) ;
#178495 = CARTESIAN_POINT('Ctrl Pts',(-24.588572932717,-14.4126782343137,
114.236447003153)) ;
#178496 = CARTESIAN_POINT('Ctrl Pts',(-24.6553633361676,-14.2599648668114,
114.475326275185)) ;
#178497 = CARTESIAN_POINT('Ctrl Pts',(-24.6404721795823,-14.2009567428221,
114.429970213033)) ;
#178498 = CARTESIAN_POINT('Ctrl Pts',(-24.5666683594676,-14.2009566811552,
114.454201325703)) ;
#178499 = CARTESIAN_POINT('Ctrl Pts',(-24.492864539353,-14.2009566194882,
114.478432438373)) ;
#178500 = CARTESIAN_POINT('Ctrl Pts',(-24.5077556959384,-14.2599647434775,
114.523788500525)) ;
#178501 = CARTESIAN_POINT('Ctrl Pts',(-24.5226468525237,-14.3189728674668,
114.569144562677)) ;
#178502 = CARTESIAN_POINT('Ctrl Pts',(-24.5964506726383,-14.3189729291337,
114.544913450007)) ;
#178503 = CARTESIAN_POINT('Ctrl Pts',(-24.670254492753,-14.3189729908007,
114.520682337336)) ;
#178504 = CARTESIAN_POINT('Ctrl Pts',(-24.6553633361676,-14.2599648668114,
114.475326275185)) ;
#178505 = CARTESIAN_POINT('Ctrl Pts',(-24.7066777082595,-14.0478524029628,
114.666975267341)) ;
#178506 = CARTESIAN_POINT('Ctrl Pts',(-24.6874500195782,-14.0035651769701,
114.608410828212)) ;
#178507 = CARTESIAN_POINT('Ctrl Pts',(-24.6136461926996,-14.0035651015323,
114.63264192028)) ;
#178508 = CARTESIAN_POINT('Ctrl Pts',(-24.5398423658211,-14.0035650260945,
114.656873012349)) ;
#178509 = CARTESIAN_POINT('Ctrl Pts',(-24.5590700545024,-14.0478522520872,
114.715437451478)) ;
#178510 = CARTESIAN_POINT('Ctrl Pts',(-24.5782977431838,-14.0921394780799,
114.774001890607)) ;
#178511 = CARTESIAN_POINT('Ctrl Pts',(-24.6521015700623,-14.0921395535177,
114.749770798538)) ;
#178512 = CARTESIAN_POINT('Ctrl Pts',(-24.7259053969409,-14.0921396289556,
114.72553970647)) ;
#178513 = CARTESIAN_POINT('Ctrl Pts',(-24.7066777082595,-14.0478524029628,
114.666975267341)) ;
#178514 = CARTESIAN_POINT('Ctrl Pts',(-24.7383886959719,-13.7904112840523,
114.79898244504)) ;
#178515 = CARTESIAN_POINT('Ctrl Pts',(-24.7161851481836,-13.764031497392,
114.731354019336)) ;
#178516 = CARTESIAN_POINT('Ctrl Pts',(-24.6423813137988,-13.7640314159743,
114.755585088541)) ;
#178517 = CARTESIAN_POINT('Ctrl Pts',(-24.5685774794139,-13.7640313345566,
114.779816157747)) ;
#178518 = CARTESIAN_POINT('Ctrl Pts',(-24.5907810272022,-13.7904111212169,
114.84744458345)) ;
#178519 = CARTESIAN_POINT('Ctrl Pts',(-24.6129845749905,-13.8167909078772,
114.915073009154)) ;
#178520 = CARTESIAN_POINT('Ctrl Pts',(-24.6867884093753,-13.8167909892949,
114.890841939949)) ;
#178521 = CARTESIAN_POINT('Ctrl Pts',(-24.7605922437602,-13.8167910707126,
114.866610870743)) ;
#178522 = CARTESIAN_POINT('Ctrl Pts',(-24.7383886959719,-13.7904112840523,
114.79898244504)) ;
#178523 = CARTESIAN_POINT('Ctrl Pts',(-24.7472587412919,-13.5044552055669,
114.861642887694)) ;
#178524 = CARTESIAN_POINT('Ctrl Pts',(-24.7236646551396,-13.4980004286212,
114.789779106659)) ;
#178525 = CARTESIAN_POINT('Ctrl Pts',(-24.6498608134184,-13.498000350832,
114.814010153519)) ;
#178526 = CARTESIAN_POINT('Ctrl Pts',(-24.5760569716972,-13.4980002730428,
114.838241200379)) ;
#178527 = CARTESIAN_POINT('Ctrl Pts',(-24.5996510578494,-13.5044550499884,
114.910104981414)) ;
#178528 = CARTESIAN_POINT('Ctrl Pts',(-24.6232451440017,-13.5109098269341,
114.981968762449)) ;
#178529 = CARTESIAN_POINT('Ctrl Pts',(-24.6970489857229,-13.5109099047233,
114.957737715589)) ;
#178530 = CARTESIAN_POINT('Ctrl Pts',(-24.7708528274441,-13.5109099825126,
114.933506668729)) ;
#178531 = CARTESIAN_POINT('Ctrl Pts',(-24.7472587412919,-13.5044552055669,
114.861642887694)) ;
#178532 = CARTESIAN_POINT('Ctrl Pts',(-24.7317360628477,-13.2137879040768,
114.849818087154)) ;
#178533 = CARTESIAN_POINT('Ctrl Pts',(-24.708456421361,-13.227617723032,114.778912053983)) ;
#178534 = CARTESIAN_POINT('Ctrl Pts',(-24.6346525736394,-13.2276176541368,
114.803143082567)) ;
#178535 = CARTESIAN_POINT('Ctrl Pts',(-24.5608487259178,-13.2276175852417,
114.827374111151)) ;
#178536 = CARTESIAN_POINT('Ctrl Pts',(-24.5841283674045,-13.2137877662865,
114.898280144321)) ;
#178537 = CARTESIAN_POINT('Ctrl Pts',(-24.6074080088912,-13.1999579473313,
114.969186177492)) ;
#178538 = CARTESIAN_POINT('Ctrl Pts',(-24.6812118566128,-13.1999580162265,
114.944955148908)) ;
#178539 = CARTESIAN_POINT('Ctrl Pts',(-24.7550157043344,-13.1999580851216,
114.920724120324)) ;
#178540 = CARTESIAN_POINT('Ctrl Pts',(-24.7317360628477,-13.2137879040768,
114.849818087154)) ;
#178541 = CARTESIAN_POINT('Ctrl Pts',(-24.6925768386914,-12.9385963486889,
114.765886618446)) ;
#178542 = CARTESIAN_POINT('Ctrl Pts',(-24.6712648539298,-12.9716609792406,
114.700973750315)) ;
#178543 = CARTESIAN_POINT('Ctrl Pts',(-24.5974610016299,-12.9716609227663,
114.725204764954)) ;
#178544 = CARTESIAN_POINT('Ctrl Pts',(-24.52365714933,-12.9716608662921,114.749435779593)) ;
#178545 = CARTESIAN_POINT('Ctrl Pts',(-24.5449691340916,-12.9385962357404,
114.814348647724)) ;
#178546 = CARTESIAN_POINT('Ctrl Pts',(-24.5662811188531,-12.9055316051888,
114.879261515854)) ;
#178547 = CARTESIAN_POINT('Ctrl Pts',(-24.640084971153,-12.905531661663,114.855030501215)) ;
#178548 = CARTESIAN_POINT('Ctrl Pts',(-24.7138888234529,-12.9055317181373,
114.830799486576)) ;
#178549 = CARTESIAN_POINT('Ctrl Pts',(-24.6925768386914,-12.9385963486889,
114.765886618446)) ;
#178550 = CARTESIAN_POINT('Ctrl Pts',(-24.6315155721698,-12.6966955833364,
114.615366123145)) ;
#178551 = CARTESIAN_POINT('Ctrl Pts',(-24.613700797823,-12.746700030026,114.561105193829)) ;
#178552 = CARTESIAN_POINT('Ctrl Pts',(-24.539896942895,-12.7466999895666,
114.585336200463)) ;
#178553 = CARTESIAN_POINT('Ctrl Pts',(-24.4660930879669,-12.7466999491071,
114.609567207097)) ;
#178554 = CARTESIAN_POINT('Ctrl Pts',(-24.4839078623137,-12.6966955024176,
114.663828136413)) ;
#178555 = CARTESIAN_POINT('Ctrl Pts',(-24.5017226366605,-12.646691055728,
114.718089065729)) ;
#178556 = CARTESIAN_POINT('Ctrl Pts',(-24.5755264915885,-12.6466910961874,
114.693858059095)) ;
#178557 = CARTESIAN_POINT('Ctrl Pts',(-24.6493303465166,-12.6466911366469,
114.66962705246)) ;
#178558 = CARTESIAN_POINT('Ctrl Pts',(-24.6315155721698,-12.6966955833364,
114.615366123145)) ;
#178559 = CARTESIAN_POINT('Ctrl Pts',(-24.5521621899109,-12.5064217313258,
114.409158146371)) ;
#178560 = CARTESIAN_POINT('Ctrl Pts',(-24.5391265658637,-12.5697873341699,
114.369453737928)) ;
#178561 = CARTESIAN_POINT('Ctrl Pts',(-24.4653227103417,-12.5697873098007,
114.393684742753)) ;
#178562 = CARTESIAN_POINT('Ctrl Pts',(-24.3915188548197,-12.5697872854314,
114.417915747578)) ;
#178563 = CARTESIAN_POINT('Ctrl Pts',(-24.4045544788668,-12.5064216825873,
114.457620156021)) ;
#178564 = CARTESIAN_POINT('Ctrl Pts',(-24.417590102914,-12.4430560797432,
114.497324564464)) ;
#178565 = CARTESIAN_POINT('Ctrl Pts',(-24.491393958436,-12.4430561041124,
114.473093559639)) ;
#178566 = CARTESIAN_POINT('Ctrl Pts',(-24.5651978139581,-12.4430561284817,
114.448862554814)) ;
#178567 = CARTESIAN_POINT('Ctrl Pts',(-24.5521621899109,-12.5064217313258,
114.409158146371)) ;
#178568 = CARTESIAN_POINT('Ctrl Pts',(-24.4595930056771,-12.3814205030376,
114.162674429355)) ;
#178569 = CARTESIAN_POINT('Ctrl Pts',(-24.4522670503864,-12.45361013115,114.140360750861)) ;
#178570 = CARTESIAN_POINT('Ctrl Pts',(-24.3784631958779,-12.4536101207451,
114.164591758773)) ;
#178571 = CARTESIAN_POINT('Ctrl Pts',(-24.3046593413694,-12.4536101103402,
114.188822766685)) ;
#178572 = CARTESIAN_POINT('Ctrl Pts',(-24.3119852966601,-12.3814204822278,
114.211136445179)) ;
#178573 = CARTESIAN_POINT('Ctrl Pts',(-24.3193112519507,-12.3092308541153,
114.233450123673)) ;
#178574 = CARTESIAN_POINT('Ctrl Pts',(-24.3931151064593,-12.3092308645202,
114.209219115761)) ;
#178575 = CARTESIAN_POINT('Ctrl Pts',(-24.4669189609677,-12.3092308749251,
114.184988107849)) ;
#178576 = CARTESIAN_POINT('Ctrl Pts',(-24.4595930056771,-12.3814205030376,
114.162674429355)) ;
#178577 = CARTESIAN_POINT('Ctrl Pts',(-24.3591960058421,-12.3309490204366,
113.892499417778)) ;
#178578 = CARTESIAN_POINT('Ctrl Pts',(-24.3581319519906,-12.4067726596542,
113.889258480905)) ;
#178579 = CARTESIAN_POINT('Ctrl Pts',(-24.2843281000817,-12.4067726592374,
113.913489496735)) ;
#178580 = CARTESIAN_POINT('Ctrl Pts',(-24.2105242481727,-12.4067726588207,
113.937720512564)) ;
#178581 = CARTESIAN_POINT('Ctrl Pts',(-24.2115883020242,-12.330949019603,
113.940961449438)) ;
#178582 = CARTESIAN_POINT('Ctrl Pts',(-24.2126523558756,-12.2551253803854,
113.944202386311)) ;
#178583 = CARTESIAN_POINT('Ctrl Pts',(-24.2864562077845,-12.2551253808022,
113.919971370481)) ;
#178584 = CARTESIAN_POINT('Ctrl Pts',(-24.3602600596935,-12.255125381219,
113.895740354651)) ;
#178585 = CARTESIAN_POINT('Ctrl Pts',(-24.3591960058421,-12.3309490204366,
113.892499417778)) ;
#178586 = CARTESIAN_POINT('Ctrl Pts',(-24.2590492512348,-12.3579787522632,
113.62264874675)) ;
#178587 = CARTESIAN_POINT('Ctrl Pts',(-24.2642481311498,-12.4320290416833,
113.638483695714)) ;
#178588 = CARTESIAN_POINT('Ctrl Pts',(-24.1904442811735,-12.4320290471933,
113.66271471743)) ;
#178589 = CARTESIAN_POINT('Ctrl Pts',(-24.1166404311972,-12.4320290527033,
113.686945739147)) ;
#178590 = CARTESIAN_POINT('Ctrl Pts',(-24.1114415512822,-12.3579787632832,
113.671110790183)) ;
#178591 = CARTESIAN_POINT('Ctrl Pts',(-24.1062426713672,-12.2839284738631,
113.655275841219)) ;
#178592 = CARTESIAN_POINT('Ctrl Pts',(-24.1800465213435,-12.2839284683531,
113.631044819503)) ;
#178593 = CARTESIAN_POINT('Ctrl Pts',(-24.2538503713199,-12.2839284628431,
113.606813797786)) ;
#178594 = CARTESIAN_POINT('Ctrl Pts',(-24.2590492512348,-12.3579787522632,
113.62264874675)) ;
#178595 = CARTESIAN_POINT('Ctrl Pts',(-24.1631094563438,-12.461461206882,
113.36607630111)) ;
#178596 = CARTESIAN_POINT('Ctrl Pts',(-24.1742776481116,-12.5283982631063,
113.400092811004)) ;
#178597 = CARTESIAN_POINT('Ctrl Pts',(-24.1004738012582,-12.5283982698858,
113.424323842232)) ;
#178598 = CARTESIAN_POINT('Ctrl Pts',(-24.0266699544049,-12.5283982766654,
113.44855487346)) ;
#178599 = CARTESIAN_POINT('Ctrl Pts',(-24.0155017626371,-12.4614612204411,
113.414538363566)) ;
#178600 = CARTESIAN_POINT('Ctrl Pts',(-24.0043335708694,-12.3945241642168,
113.380521853673)) ;
#178601 = CARTESIAN_POINT('Ctrl Pts',(-24.0781374177227,-12.3945241574372,
113.356290822444)) ;
#178602 = CARTESIAN_POINT('Ctrl Pts',(-24.1519412645761,-12.3945241506577,
113.332059791216)) ;
#178603 = CARTESIAN_POINT('Ctrl Pts',(-24.1631094563438,-12.461461206882,
113.36607630111)) ;
#178604 = CARTESIAN_POINT('Ctrl Pts',(-24.0794846118896,-12.6327579824641,
113.146729045038)) ;
#178605 = CARTESIAN_POINT('Ctrl Pts',(-24.0957769767799,-12.6878348099754,
113.196352959588)) ;
#178606 = CARTESIAN_POINT('Ctrl Pts',(-24.0219731318251,-12.6878348153818,
113.220583996599)) ;
#178607 = CARTESIAN_POINT('Ctrl Pts',(-23.9481692868703,-12.6878348207882,
113.24481503361)) ;
#178608 = CARTESIAN_POINT('Ctrl Pts',(-23.9318769219801,-12.632757993277,
113.19519111906)) ;
#178609 = CARTESIAN_POINT('Ctrl Pts',(-23.9155845570898,-12.5776811657657,
113.145567204509)) ;
#178610 = CARTESIAN_POINT('Ctrl Pts',(-23.9893884020446,-12.5776811603593,
113.121336167498)) ;
#178611 = CARTESIAN_POINT('Ctrl Pts',(-24.0631922469993,-12.5776811549529,
113.097105130487)) ;
#178612 = CARTESIAN_POINT('Ctrl Pts',(-24.0794846118896,-12.6327579824641,
113.146729045038)) ;
#178613 = CARTESIAN_POINT('Ctrl Pts',(-24.0122990421959,-12.8610649262646,
112.977629767465)) ;
#178614 = CARTESIAN_POINT('Ctrl Pts',(-24.0325718885268,-12.9002826126032,
113.039377586343)) ;
#178615 = CARTESIAN_POINT('Ctrl Pts',(-23.9587680449403,-12.9002826143644,
113.063608627522)) ;
#178616 = CARTESIAN_POINT('Ctrl Pts',(-23.8849642013539,-12.9002826161256,
113.0878396687)) ;
#178617 = CARTESIAN_POINT('Ctrl Pts',(-23.8646913550231,-12.861064929787,
113.026091849823)) ;
#178618 = CARTESIAN_POINT('Ctrl Pts',(-23.8444185086923,-12.8218472434483,
112.964344030946)) ;
#178619 = CARTESIAN_POINT('Ctrl Pts',(-23.9182223522787,-12.8218472416871,
112.940112989767)) ;
#178620 = CARTESIAN_POINT('Ctrl Pts',(-23.9920261958651,-12.8218472399259,
112.915881948588)) ;
#178621 = CARTESIAN_POINT('Ctrl Pts',(-24.0122990421959,-12.8610649262646,
112.977629767465)) ;
#178622 = CARTESIAN_POINT('Ctrl Pts',(-23.9662485633249,-13.1282120035714,
112.872739576532)) ;
#178623 = CARTESIAN_POINT('Ctrl Pts',(-23.9890352233381,-13.1488341330094,
112.942144066345)) ;
#178624 = CARTESIAN_POINT('Ctrl Pts',(-23.9152313801124,-13.1488341316972,
112.966375108623)) ;
#178625 = CARTESIAN_POINT('Ctrl Pts',(-23.8414275368868,-13.148834130385,
112.990606150901)) ;
#178626 = CARTESIAN_POINT('Ctrl Pts',(-23.8186408768736,-13.1282120009471,
112.921201661087)) ;
#178627 = CARTESIAN_POINT('Ctrl Pts',(-23.7958542168604,-13.1075898715092,
112.851797171274)) ;
#178628 = CARTESIAN_POINT('Ctrl Pts',(-23.869658060086,-13.1075898728214,
112.827566128996)) ;
#178629 = CARTESIAN_POINT('Ctrl Pts',(-23.9434619033117,-13.1075898741335,
112.803335086719)) ;
#178630 = CARTESIAN_POINT('Ctrl Pts',(-23.9662485633249,-13.1282120035714,
112.872739576532)) ;
#178631 = CARTESIAN_POINT('Ctrl Pts',(-23.9434524616525,-13.4170777357306,
112.838817161117)) ;
#178632 = CARTESIAN_POINT('Ctrl Pts',(-23.9671300237859,-13.4175593372615,
112.91093519508)) ;
#178633 = CARTESIAN_POINT('Ctrl Pts',(-23.8933261804059,-13.4175593339228,
112.935166236887)) ;
#178634 = CARTESIAN_POINT('Ctrl Pts',(-23.8195223370259,-13.4175593305841,
112.959397278695)) ;
#178635 = CARTESIAN_POINT('Ctrl Pts',(-23.7958447748924,-13.4170777290533,
112.887279244733)) ;
#178636 = CARTESIAN_POINT('Ctrl Pts',(-23.772167212759,-13.4165961275224,
112.81516121077)) ;
#178637 = CARTESIAN_POINT('Ctrl Pts',(-23.845971056139,-13.4165961308611,
112.790930168963)) ;
#178638 = CARTESIAN_POINT('Ctrl Pts',(-23.919774899519,-13.4165961341998,
112.766699127155)) ;
#178639 = CARTESIAN_POINT('Ctrl Pts',(-23.9434524616525,-13.4170777357306,
112.838817161117)) ;
#178640 = CARTESIAN_POINT('Ctrl Pts',(-23.9449981053748,-13.7056413839055,
112.878978183992)) ;
#178641 = CARTESIAN_POINT('Ctrl Pts',(-23.967869039491,-13.6859734009019,
112.948639359155)) ;
#178642 = CARTESIAN_POINT('Ctrl Pts',(-23.8940651957832,-13.6859733981245,
112.972870399964)) ;
#178643 = CARTESIAN_POINT('Ctrl Pts',(-23.8202613520754,-13.6859733953471,
112.997101440773)) ;
#178644 = CARTESIAN_POINT('Ctrl Pts',(-23.7973904179592,-13.7056413783507,
112.92744026561)) ;
#178645 = CARTESIAN_POINT('Ctrl Pts',(-23.7745194838429,-13.7253093613543,
112.857779090447)) ;
#178646 = CARTESIAN_POINT('Ctrl Pts',(-23.8483233275508,-13.7253093641317,
112.833548049638)) ;
#178647 = CARTESIAN_POINT('Ctrl Pts',(-23.9221271712586,-13.725309366909,
112.809317008829)) ;
#178648 = CARTESIAN_POINT('Ctrl Pts',(-23.9449981053748,-13.7056413839055,
112.878978183992)) ;
#178649 = CARTESIAN_POINT('Ctrl Pts',(-23.9701821735012,-13.9747406301587,
112.991309111019)) ;
#178650 = CARTESIAN_POINT('Ctrl Pts',(-23.9905910336019,-13.9362526969778,
113.053471205922)) ;
#178651 = CARTESIAN_POINT('Ctrl Pts',(-23.9167871901567,-13.9362526974253,
113.077702247531)) ;
#178652 = CARTESIAN_POINT('Ctrl Pts',(-23.8429833467115,-13.9362526978728,
113.10193328914)) ;
#178653 = CARTESIAN_POINT('Ctrl Pts',(-23.8225744866109,-13.9747406310537,
113.039771194237)) ;
#178654 = CARTESIAN_POINT('Ctrl Pts',(-23.8021656265102,-14.0132285642346,
112.977609099335)) ;
#178655 = CARTESIAN_POINT('Ctrl Pts',(-23.8759694699554,-14.0132285637871,
112.953378057726)) ;
#178656 = CARTESIAN_POINT('Ctrl Pts',(-23.9497733134006,-14.0132285633396,
112.929147016116)) ;
#178657 = CARTESIAN_POINT('Ctrl Pts',(-23.9701821735012,-13.9747406301587,
112.991309111019)) ;
#178658 = CARTESIAN_POINT('Ctrl Pts',(-24.0160072122531,-14.201974810105,
113.166223946965)) ;
#178659 = CARTESIAN_POINT('Ctrl Pts',(-24.0325147694804,-14.1475641696475,
113.216503302712)) ;
#178660 = CARTESIAN_POINT('Ctrl Pts',(-23.9587109269328,-14.1475641728961,
113.240734347056)) ;
#178661 = CARTESIAN_POINT('Ctrl Pts',(-23.8849070843852,-14.1475641761448,
113.264965391399)) ;
#178662 = CARTESIAN_POINT('Ctrl Pts',(-23.8683995271579,-14.2019748166024,
113.214686035651)) ;
#178663 = CARTESIAN_POINT('Ctrl Pts',(-23.8518919699306,-14.2563854570598,
113.164406679903)) ;
#178664 = CARTESIAN_POINT('Ctrl Pts',(-23.9256958124782,-14.2563854538112,
113.14017563556)) ;
#178665 = CARTESIAN_POINT('Ctrl Pts',(-23.9994996550258,-14.2563854505624,
113.115944591217)) ;
#178666 = CARTESIAN_POINT('Ctrl Pts',(-24.0160072122531,-14.201974810105,
113.166223946965)) ;
#178667 = CARTESIAN_POINT('Ctrl Pts',(-24.0787453413408,-14.3739130003505,
113.392766421991)) ;
#178668 = CARTESIAN_POINT('Ctrl Pts',(-24.0901626436676,-14.3074175885929,
113.427541682514)) ;
#178669 = CARTESIAN_POINT('Ctrl Pts',(-24.0163588028729,-14.3074175937146,
113.451772732196)) ;
#178670 = CARTESIAN_POINT('Ctrl Pts',(-23.9425549620781,-14.3074175988363,
113.476003781877)) ;
#178671 = CARTESIAN_POINT('Ctrl Pts',(-23.9311376597514,-14.3739130105938,
113.441228521355)) ;
#178672 = CARTESIAN_POINT('Ctrl Pts',(-23.9197203574246,-14.4404084223513,
113.406453260833)) ;
#178673 = CARTESIAN_POINT('Ctrl Pts',(-23.9935241982193,-14.4404084172297,
113.382222211151)) ;
#178674 = CARTESIAN_POINT('Ctrl Pts',(-24.067328039014,-14.440408412108,113.357991161469)) ;
#178675 = CARTESIAN_POINT('Ctrl Pts',(-24.0787453413408,-14.3739130003505,
113.392766421991)) ;
#178676 = CARTESIAN_POINT('Ctrl Pts',(-24.153021958778,-14.4775305035498,
113.654416785986)) ;
#178677 = CARTESIAN_POINT('Ctrl Pts',(-24.1585367352309,-14.4037037065639,
113.671213904943)) ;
#178678 = CARTESIAN_POINT('Ctrl Pts',(-24.0847328966993,-14.403703711016,
113.695444961518)) ;
#178679 = CARTESIAN_POINT('Ctrl Pts',(-24.0109290581677,-14.4037037154681,
113.719676018093)) ;
#178680 = CARTESIAN_POINT('Ctrl Pts',(-24.0054142817148,-14.477530512454,
113.702878899137)) ;
#178681 = CARTESIAN_POINT('Ctrl Pts',(-23.999899505262,-14.5513573094398,
113.686081780181)) ;
#178682 = CARTESIAN_POINT('Ctrl Pts',(-24.0737033437936,-14.5513573049878,
113.661850723605)) ;
#178683 = CARTESIAN_POINT('Ctrl Pts',(-24.1475071823252,-14.5513573005357,
113.63761966703)) ;
#178684 = CARTESIAN_POINT('Ctrl Pts',(-24.153021958778,-14.4775305035498,
113.654416785986)) ;
#178685 = CARTESIAN_POINT('Ctrl Pts',(-24.2334081776458,-14.5050608269986,
113.934939965511)) ;
#178686 = CARTESIAN_POINT('Ctrl Pts',(-24.2325798290723,-14.4292041443238,
113.93241694891)) ;
#178687 = CARTESIAN_POINT('Ctrl Pts',(-24.1587759937175,-14.4292041439296,
113.956648015161)) ;
#178688 = CARTESIAN_POINT('Ctrl Pts',(-24.0849721583626,-14.4292041435354,
113.980879081412)) ;
#178689 = CARTESIAN_POINT('Ctrl Pts',(-24.0858005069361,-14.5050608262101,
113.983402098013)) ;
#178690 = CARTESIAN_POINT('Ctrl Pts',(-24.0866288555096,-14.5809175088849,
113.985925114614)) ;
#178691 = CARTESIAN_POINT('Ctrl Pts',(-24.1604326908644,-14.5809175092791,
113.961694048363)) ;
#178692 = CARTESIAN_POINT('Ctrl Pts',(-24.2342365262193,-14.5809175096733,
113.937462982112)) ;
#178693 = CARTESIAN_POINT('Ctrl Pts',(-24.2334081776458,-14.5050608269986,
113.934939965511)) ;
#178694 = CARTESIAN_POINT('Ctrl Pts',(-24.3118138425738,-14.4551363613954,
114.208959708269)) ;
#178695 = CARTESIAN_POINT('Ctrl Pts',(-24.3047814448191,-14.3826564737513,
114.187540158768)) ;
#178696 = CARTESIAN_POINT('Ctrl Pts',(-24.2309776109259,-14.3826564648488,
114.211771229471)) ;
#178697 = CARTESIAN_POINT('Ctrl Pts',(-24.1571737770328,-14.3826564559462,
114.236002300174)) ;
#178698 = CARTESIAN_POINT('Ctrl Pts',(-24.1642061747875,-14.4551363435903,
114.257421849676)) ;
#178699 = CARTESIAN_POINT('Ctrl Pts',(-24.1712385725423,-14.5276162312344,
114.278841399177)) ;
#178700 = CARTESIAN_POINT('Ctrl Pts',(-24.2450424064354,-14.5276162401369,
114.254610328474)) ;
#178701 = CARTESIAN_POINT('Ctrl Pts',(-24.3188462403286,-14.5276162490395,
114.230379257771)) ;
#178702 = CARTESIAN_POINT('Ctrl Pts',(-24.3118138425738,-14.4551363613954,
114.208959708269)) ;
#178703 = CARTESIAN_POINT('Ctrl Pts',(-24.3838624730078,-14.3298705824412,
114.464102745858)) ;
#178704 = CARTESIAN_POINT('Ctrl Pts',(-24.3710507387794,-14.2660313750253,
114.425080269742)) ;
#178705 = CARTESIAN_POINT('Ctrl Pts',(-24.2972469066288,-14.2660313525063,
114.449311345752)) ;
#178706 = CARTESIAN_POINT('Ctrl Pts',(-24.2234430744781,-14.2660313299873,
114.473542421763)) ;
#178707 = CARTESIAN_POINT('Ctrl Pts',(-24.2362548087065,-14.3298705374032,
114.512564897879)) ;
#178708 = CARTESIAN_POINT('Ctrl Pts',(-24.2490665429349,-14.3937097448191,
114.551587373996)) ;
#178709 = CARTESIAN_POINT('Ctrl Pts',(-24.3228703750855,-14.3937097673381,
114.527356297985)) ;
#178710 = CARTESIAN_POINT('Ctrl Pts',(-24.3966742072362,-14.3937097898571,
114.503125221975)) ;
#178711 = CARTESIAN_POINT('Ctrl Pts',(-24.3838624730078,-14.3298705824412,
114.464102745858)) ;
#178712 = CARTESIAN_POINT('Ctrl Pts',(-24.4418657884039,-14.1407879039854,
114.676048055119)) ;
#178713 = CARTESIAN_POINT('Ctrl Pts',(-24.4242559427528,-14.0900585571138,
114.622411305648)) ;
#178714 = CARTESIAN_POINT('Ctrl Pts',(-24.3504521097342,-14.090058520559,
114.646642379015)) ;
#178715 = CARTESIAN_POINT('Ctrl Pts',(-24.2766482767156,-14.0900584840042,
114.670873452382)) ;
#178716 = CARTESIAN_POINT('Ctrl Pts',(-24.2942581223667,-14.1407878308758,
114.724510201853)) ;
#178717 = CARTESIAN_POINT('Ctrl Pts',(-24.3118679680179,-14.1915171777474,
114.778146951323)) ;
#178718 = CARTESIAN_POINT('Ctrl Pts',(-24.3856718010364,-14.1915172143022,
114.753915877957)) ;
#178719 = CARTESIAN_POINT('Ctrl Pts',(-24.459475634055,-14.191517250857,114.72968480459)) ;
#178720 = CARTESIAN_POINT('Ctrl Pts',(-24.4418657884039,-14.1407879039854,
114.676048055119)) ;
#178721 = CARTESIAN_POINT('Ctrl Pts',(-24.4821519623665,-13.8991517087972,
114.83424842299)) ;
#178722 = CARTESIAN_POINT('Ctrl Pts',(-24.460969456234,-13.8652196589451,
114.769729925967)) ;
#178723 = CARTESIAN_POINT('Ctrl Pts',(-24.3871656211141,-13.8652196069501,
114.793960992934)) ;
#178724 = CARTESIAN_POINT('Ctrl Pts',(-24.3133617859942,-13.865219554955,
114.8181920599)) ;
#178725 = CARTESIAN_POINT('Ctrl Pts',(-24.3345442921267,-13.8991516048072,
114.882710556924)) ;
#178726 = CARTESIAN_POINT('Ctrl Pts',(-24.3557267982592,-13.9330836546593,
114.947229053947)) ;
#178727 = CARTESIAN_POINT('Ctrl Pts',(-24.4295306333791,-13.9330837066543,
114.922997986981)) ;
#178728 = CARTESIAN_POINT('Ctrl Pts',(-24.503334468499,-13.9330837586493,
114.898766920014)) ;
#178729 = CARTESIAN_POINT('Ctrl Pts',(-24.4821519623665,-13.8991517087972,
114.83424842299)) ;
#178730 = CARTESIAN_POINT('Ctrl Pts',(-24.5005313129686,-13.622377664187,
114.925775683021)) ;
#178731 = CARTESIAN_POINT('Ctrl Pts',(-24.4772993502077,-13.6077202458349,
114.855014871609)) ;
#178732 = CARTESIAN_POINT('Ctrl Pts',(-24.4034955109649,-13.6077201796241,
114.879245926018)) ;
#178733 = CARTESIAN_POINT('Ctrl Pts',(-24.3296916717221,-13.6077201134133,
114.903476980426)) ;
#178734 = CARTESIAN_POINT('Ctrl Pts',(-24.352923634483,-13.6223775317654,
114.974237791838)) ;
#178735 = CARTESIAN_POINT('Ctrl Pts',(-24.3761555972439,-13.6370349501174,
115.04499860325)) ;
#178736 = CARTESIAN_POINT('Ctrl Pts',(-24.4499594364868,-13.6370350163283,
115.020767548841)) ;
#178737 = CARTESIAN_POINT('Ctrl Pts',(-24.5237632757296,-13.6370350825391,
114.996536494432)) ;
#178738 = CARTESIAN_POINT('Ctrl Pts',(-24.5005313129686,-13.622377664187,
114.925775683021)) ;
#178739 = CARTESIAN_POINT('Ctrl Pts',(-24.49501436777,-13.3324243748073,114.944342617232)) ;
#178740 = CARTESIAN_POINT('Ctrl Pts',(-24.4714021470043,-13.3379896350766,
114.872423601156)) ;
#178741 = CARTESIAN_POINT('Ctrl Pts',(-24.39759830194,-13.3379895606869,114.896654637833)) ;
#178742 = CARTESIAN_POINT('Ctrl Pts',(-24.3237944568757,-13.3379894862972,
114.92088567451)) ;
#178743 = CARTESIAN_POINT('Ctrl Pts',(-24.3474066776414,-13.3324242260279,
114.992804690587)) ;
#178744 = CARTESIAN_POINT('Ctrl Pts',(-24.371018898407,-13.3268589657586,
115.064723706663)) ;
#178745 = CARTESIAN_POINT('Ctrl Pts',(-24.4448227434714,-13.3268590401483,
115.040492669985)) ;
#178746 = CARTESIAN_POINT('Ctrl Pts',(-24.5186265885357,-13.326859114538,
115.016261633308)) ;
#178747 = CARTESIAN_POINT('Ctrl Pts',(-24.49501436777,-13.3324243748073,114.944342617232)) ;
#178748 = CARTESIAN_POINT('Ctrl Pts',(-24.4653775774576,-13.0478498918573,
114.889526808152)) ;
#178749 = CARTESIAN_POINT('Ctrl Pts',(-24.443066690919,-13.0732913047775,
114.821571446019)) ;
#178750 = CARTESIAN_POINT('Ctrl Pts',(-24.3692628390167,-13.073291227464,
114.845802461869)) ;
#178751 = CARTESIAN_POINT('Ctrl Pts',(-24.2954589871145,-13.0732911501505,
114.870033477719)) ;
#178752 = CARTESIAN_POINT('Ctrl Pts',(-24.3177698736531,-13.0478497372302,
114.937988839852)) ;
#178753 = CARTESIAN_POINT('Ctrl Pts',(-24.3400807601917,-13.02240832431,115.005944201984)) ;
#178754 = CARTESIAN_POINT('Ctrl Pts',(-24.413884612094,-13.0224084016235,
114.981713186134)) ;
#178755 = CARTESIAN_POINT('Ctrl Pts',(-24.4876884639962,-13.022408478937,
114.957482170284)) ;
#178756 = CARTESIAN_POINT('Ctrl Pts',(-24.4653775774576,-13.0478498918573,
114.889526808152)) ;
#178757 = CARTESIAN_POINT('Ctrl Pts',(-24.4124318331185,-12.7884262570381,
114.76392923946)) ;
#178758 = CARTESIAN_POINT('Ctrl Pts',(-24.3930468030307,-12.8320168743516,
114.704885563836)) ;
#178759 = CARTESIAN_POINT('Ctrl Pts',(-24.319242943509,-12.8320168006288,
114.729116556479)) ;
#178760 = CARTESIAN_POINT('Ctrl Pts',(-24.2454390839874,-12.8320167269059,
114.753347549122)) ;
#178761 = CARTESIAN_POINT('Ctrl Pts',(-24.2648241140752,-12.7884261095925,
114.812391224746)) ;
#178762 = CARTESIAN_POINT('Ctrl Pts',(-24.284209144163,-12.744835492279,114.87143490037)) ;
#178763 = CARTESIAN_POINT('Ctrl Pts',(-24.3580130036846,-12.7448355660018,
114.847203907727)) ;
#178764 = CARTESIAN_POINT('Ctrl Pts',(-24.4318168632063,-12.7448356397246,
114.822972915085)) ;
#178765 = CARTESIAN_POINT('Ctrl Pts',(-24.4124318331185,-12.7884262570381,
114.76392923946)) ;
#178766 = CARTESIAN_POINT('Ctrl Pts',(-24.3401997969462,-12.5764203972658,
114.57925123095)) ;
#178767 = CARTESIAN_POINT('Ctrl Pts',(-24.3250986174262,-12.6348758868913,
114.533255472867)) ;
#178768 = CARTESIAN_POINT('Ctrl Pts',(-24.2512947512124,-12.6348758265582,
114.557486445126)) ;
#178769 = CARTESIAN_POINT('Ctrl Pts',(-24.1774908849985,-12.6348757662251,
114.581717417385)) ;
#178770 = CARTESIAN_POINT('Ctrl Pts',(-24.1925920645185,-12.5764202765996,
114.627713175469)) ;
#178771 = CARTESIAN_POINT('Ctrl Pts',(-24.2076932440385,-12.517964786974,
114.673708933552)) ;
#178772 = CARTESIAN_POINT('Ctrl Pts',(-24.2814971102523,-12.5179648473072,
114.649477961293)) ;
#178773 = CARTESIAN_POINT('Ctrl Pts',(-24.3553009764662,-12.5179649076403,
114.625246989034)) ;
#178774 = CARTESIAN_POINT('Ctrl Pts',(-24.3401997969462,-12.5764203972658,
114.57925123095)) ;
#178775 = CARTESIAN_POINT('Ctrl Pts',(-24.2523979814976,-12.4236100991773,
114.347280755597)) ;
#178776 = CARTESIAN_POINT('Ctrl Pts',(-24.2426710134567,-12.4928195575656,
114.317653978459)) ;
#178777 = CARTESIAN_POINT('Ctrl Pts',(-24.1688671416776,-12.4928195167555,
114.341884933767)) ;
#178778 = CARTESIAN_POINT('Ctrl Pts',(-24.0950632698985,-12.4928194759453,
114.366115889076)) ;
#178779 = CARTESIAN_POINT('Ctrl Pts',(-24.1047902379394,-12.423610017557,
114.395742666214)) ;
#178780 = CARTESIAN_POINT('Ctrl Pts',(-24.1145172059802,-12.3544005591686,
114.425369443353)) ;
#178781 = CARTESIAN_POINT('Ctrl Pts',(-24.1883210777593,-12.3544005999788,
114.401138488044)) ;
#178782 = CARTESIAN_POINT('Ctrl Pts',(-24.2621249495384,-12.354400640789,
114.376907532736)) ;
#178783 = CARTESIAN_POINT('Ctrl Pts',(-24.2523979814976,-12.4236100991773,
114.347280755597)) ;
#178784 = CARTESIAN_POINT('Ctrl Pts',(-24.1544007543503,-12.3419562515338,
114.084359044048)) ;
#178785 = CARTESIAN_POINT('Ctrl Pts',(-24.1507654132783,-12.4169681280718,
114.073286379695)) ;
#178786 = CARTESIAN_POINT('Ctrl Pts',(-24.0769615378214,-12.4169681124147,
114.097517323801)) ;
#178787 = CARTESIAN_POINT('Ctrl Pts',(-24.0031576623645,-12.4169680967576,
114.121748267908)) ;
#178788 = CARTESIAN_POINT('Ctrl Pts',(-24.0067930034366,-12.3419562202195,
114.132820932261)) ;
#178789 = CARTESIAN_POINT('Ctrl Pts',(-24.0104283445086,-12.2669443436815,
114.143893596615)) ;
#178790 = CARTESIAN_POINT('Ctrl Pts',(-24.0842322199655,-12.2669443593386,
114.119662652508)) ;
#178791 = CARTESIAN_POINT('Ctrl Pts',(-24.1580360954224,-12.2669443749958,
114.095431708402)) ;
#178792 = CARTESIAN_POINT('Ctrl Pts',(-24.1544007543503,-12.3419562515338,
114.084359044048)) ;
#178793 = CARTESIAN_POINT('Ctrl Pts',(-24.0529879307825,-12.3379525743983,
113.810967700911)) ;
#178794 = CARTESIAN_POINT('Ctrl Pts',(-24.0556930383593,-12.4133543694812,
113.819207020064)) ;
#178795 = CARTESIAN_POINT('Ctrl Pts',(-23.9818891619565,-12.4133543821139,
113.843437961289)) ;
#178796 = CARTESIAN_POINT('Ctrl Pts',(-23.9080852855538,-12.4133543947465,
113.867668902515)) ;
#178797 = CARTESIAN_POINT('Ctrl Pts',(-23.905380177977,-12.3379525996635,
113.859429583362)) ;
#178798 = CARTESIAN_POINT('Ctrl Pts',(-23.9026750704002,-12.2625508045805,
113.85119026421)) ;
#178799 = CARTESIAN_POINT('Ctrl Pts',(-23.9764789468029,-12.2625507919479,
113.826959322984)) ;
#178800 = CARTESIAN_POINT('Ctrl Pts',(-24.0502828232057,-12.2625507793153,
113.802728381759)) ;
#178801 = CARTESIAN_POINT('Ctrl Pts',(-24.0529879307825,-12.3379525743983,
113.810967700911)) ;
#178802 = CARTESIAN_POINT('Ctrl Pts',(-23.9551105454002,-12.4104778611719,
113.54810794873)) ;
#178803 = CARTESIAN_POINT('Ctrl Pts',(-23.9639235340744,-12.4809266819483,
113.574950888178)) ;
#178804 = CARTESIAN_POINT('Ctrl Pts',(-23.8901196595169,-12.4809267225878,
113.599181835023)) ;
#178805 = CARTESIAN_POINT('Ctrl Pts',(-23.8163157849594,-12.4809267632273,
113.623412781869)) ;
#178806 = CARTESIAN_POINT('Ctrl Pts',(-23.8075027962851,-12.4104779424509,
113.596569842421)) ;
#178807 = CARTESIAN_POINT('Ctrl Pts',(-23.7986898076108,-12.3400291216744,
113.569726902974)) ;
#178808 = CARTESIAN_POINT('Ctrl Pts',(-23.8724936821683,-12.3400290810349,
113.545495956128)) ;
#178809 = CARTESIAN_POINT('Ctrl Pts',(-23.9462975567259,-12.3400290403954,
113.521265009282)) ;
#178810 = CARTESIAN_POINT('Ctrl Pts',(-23.9551105454002,-12.4104778611719,
113.54810794873)) ;
#178811 = CARTESIAN_POINT('Ctrl Pts',(-23.8656364276719,-12.5557718304403,
113.311130140898)) ;
#178812 = CARTESIAN_POINT('Ctrl Pts',(-23.8799736924216,-12.6161812209366,
113.35479913392)) ;
#178813 = CARTESIAN_POINT('Ctrl Pts',(-23.8061698222053,-12.6161812871028,
113.379030093989)) ;
#178814 = CARTESIAN_POINT('Ctrl Pts',(-23.7323659519891,-12.6161813532691,
113.403261054057)) ;
#178815 = CARTESIAN_POINT('Ctrl Pts',(-23.7180286872394,-12.5557719627728,
113.359592061035)) ;
#178816 = CARTESIAN_POINT('Ctrl Pts',(-23.7036914224898,-12.4953625722765,
113.315923068013)) ;
#178817 = CARTESIAN_POINT('Ctrl Pts',(-23.777495292706,-12.4953625061102,
113.291692107944)) ;
#178818 = CARTESIAN_POINT('Ctrl Pts',(-23.8512991629223,-12.495362439944,
113.267461147876)) ;
#178819 = CARTESIAN_POINT('Ctrl Pts',(-23.8656364276719,-12.5557718304403,
113.311130140898)) ;
#178820 = CARTESIAN_POINT('Ctrl Pts',(-23.7913251487216,-12.7621800376528,
113.120181789862)) ;
#178821 = CARTESIAN_POINT('Ctrl Pts',(-23.810139487679,-12.8082681507132,
113.177487228558)) ;
#178822 = CARTESIAN_POINT('Ctrl Pts',(-23.7363356240177,-12.8082682369313,
113.201718208592)) ;
#178823 = CARTESIAN_POINT('Ctrl Pts',(-23.6625317603564,-12.8082683231495,
113.225949188626)) ;
#178824 = CARTESIAN_POINT('Ctrl Pts',(-23.643717421399,-12.7621802100891,
113.16864374993)) ;
#178825 = CARTESIAN_POINT('Ctrl Pts',(-23.6249030824416,-12.7160920970287,
113.111338311234)) ;
#178826 = CARTESIAN_POINT('Ctrl Pts',(-23.6987069461029,-12.7160920108106,
113.0871073312)) ;
#178827 = CARTESIAN_POINT('Ctrl Pts',(-23.7725108097643,-12.7160919245924,
113.062876351166)) ;
#178828 = CARTESIAN_POINT('Ctrl Pts',(-23.7913251487216,-12.7621800376528,
113.120181789862)) ;
#178829 = CARTESIAN_POINT('Ctrl Pts',(-23.7361036954528,-13.0168738808962,
112.987578292511)) ;
#178830 = CARTESIAN_POINT('Ctrl Pts',(-23.7580650338874,-13.0452490763117,
113.054468983887)) ;
#178831 = CARTESIAN_POINT('Ctrl Pts',(-23.6842611783686,-13.0452491748441,
113.078699988721)) ;
#178832 = CARTESIAN_POINT('Ctrl Pts',(-23.6104573228497,-13.0452492733765,
113.102930993556)) ;
#178833 = CARTESIAN_POINT('Ctrl Pts',(-23.5884959844151,-13.0168740779611,
113.03604030218)) ;
#178834 = CARTESIAN_POINT('Ctrl Pts',(-23.5665346459805,-12.9884988825456,
112.969149610803)) ;
#178835 = CARTESIAN_POINT('Ctrl Pts',(-23.6403385014994,-12.9884987840132,
112.944918605969)) ;
#178836 = CARTESIAN_POINT('Ctrl Pts',(-23.7141423570182,-12.9884986854807,
112.920687601134)) ;
#178837 = CARTESIAN_POINT('Ctrl Pts',(-23.7361036954528,-13.0168738808962,
112.987578292511)) ;
#178838 = CARTESIAN_POINT('Ctrl Pts',(-23.703804074422,-13.2984278863564,
112.924531497575)) ;
#178839 = CARTESIAN_POINT('Ctrl Pts',(-23.7273220652697,-13.3071879031459,
112.996163501084)) ;
#178840 = CARTESIAN_POINT('Ctrl Pts',(-23.6535182184119,-13.3071880059568,
113.020394532299)) ;
#178841 = CARTESIAN_POINT('Ctrl Pts',(-23.579714371554,-13.3071881087676,
113.044625563513)) ;
#178842 = CARTESIAN_POINT('Ctrl Pts',(-23.5561963807064,-13.2984280919781,
112.972993560004)) ;
#178843 = CARTESIAN_POINT('Ctrl Pts',(-23.5326783898587,-13.2896680751886,
112.901361556494)) ;
#178844 = CARTESIAN_POINT('Ctrl Pts',(-23.6064822367166,-13.2896679723777,
112.87713052528)) ;
#178845 = CARTESIAN_POINT('Ctrl Pts',(-23.6802860835744,-13.2896678695669,
112.852899494065)) ;
#178846 = CARTESIAN_POINT('Ctrl Pts',(-23.703804074422,-13.2984278863564,
112.924531497575)) ;
#178847 = CARTESIAN_POINT('Ctrl Pts',(-23.6954444130968,-13.5897265030932,
112.93456078648)) ;
#178848 = CARTESIAN_POINT('Ctrl Pts',(-23.7188468988158,-13.5781620490211,
113.005840980081)) ;
#178849 = CARTESIAN_POINT('Ctrl Pts',(-23.6450430604439,-13.5781621471943,
113.030072037142)) ;
#178850 = CARTESIAN_POINT('Ctrl Pts',(-23.571239222072,-13.5781622453675,
113.054303094203)) ;
#178851 = CARTESIAN_POINT('Ctrl Pts',(-23.547836736353,-13.5897266994396,
112.983022900603)) ;
#178852 = CARTESIAN_POINT('Ctrl Pts',(-23.524434250634,-13.6012911535118,
112.911742707003)) ;
#178853 = CARTESIAN_POINT('Ctrl Pts',(-23.5982380890059,-13.6012910553386,
112.887511649942)) ;
#178854 = CARTESIAN_POINT('Ctrl Pts',(-23.6720419273778,-13.6012909571654,
112.86328059288)) ;
#178855 = CARTESIAN_POINT('Ctrl Pts',(-23.6954444130968,-13.5897265030932,
112.93456078648)) ;
#178856 = CARTESIAN_POINT('Ctrl Pts',(-23.7111888510481,-13.8688372211758,
113.018021310344)) ;
#178857 = CARTESIAN_POINT('Ctrl Pts',(-23.7327926044286,-13.8377685346258,
113.083822855566)) ;
#178858 = CARTESIAN_POINT('Ctrl Pts',(-23.6589887733588,-13.8377686202372,
113.108053934868)) ;
#178859 = CARTESIAN_POINT('Ctrl Pts',(-23.585184942289,-13.8377687058487,
113.13228501417)) ;
#178860 = CARTESIAN_POINT('Ctrl Pts',(-23.5635811889085,-13.8688373923986,
113.066483468949)) ;
#178861 = CARTESIAN_POINT('Ctrl Pts',(-23.5419774355281,-13.8999060789486,
113.000681923728)) ;
#178862 = CARTESIAN_POINT('Ctrl Pts',(-23.6157812665979,-13.8999059933372,
112.976450844425)) ;
#178863 = CARTESIAN_POINT('Ctrl Pts',(-23.6895850976677,-13.8999059077257,
112.952219765123)) ;
#178864 = CARTESIAN_POINT('Ctrl Pts',(-23.7111888510481,-13.8688372211758,
113.018021310344)) ;
#178865 = CARTESIAN_POINT('Ctrl Pts',(-23.7490277618584,-14.1152016754008,
113.168722954981)) ;
#178866 = CARTESIAN_POINT('Ctrl Pts',(-23.7672886351906,-14.0668854985442,
113.224342627059)) ;
#178867 = CARTESIAN_POINT('Ctrl Pts',(-23.6934848096128,-14.0668855661399,
113.248573723089)) ;
#178868 = CARTESIAN_POINT('Ctrl Pts',(-23.6196809840351,-14.0668856337355,
113.272804819119)) ;
#178869 = CARTESIAN_POINT('Ctrl Pts',(-23.6014201107028,-14.1152018105922,
113.217185147041)) ;
#178870 = CARTESIAN_POINT('Ctrl Pts',(-23.5831592373706,-14.1635179874488,
113.161565474963)) ;
#178871 = CARTESIAN_POINT('Ctrl Pts',(-23.6569630629483,-14.1635179198531,
113.137334378933)) ;
#178872 = CARTESIAN_POINT('Ctrl Pts',(-23.7307668885261,-14.1635178522575,
113.113103282903)) ;
#178873 = CARTESIAN_POINT('Ctrl Pts',(-23.7490277618584,-14.1152016754008,
113.168722954981)) ;
#178874 = CARTESIAN_POINT('Ctrl Pts',(-23.8054647064364,-14.3116011164225,
113.376051058603)) ;
#178875 = CARTESIAN_POINT('Ctrl Pts',(-23.8190796168698,-14.2494997572639,
113.417519877438)) ;
#178876 = CARTESIAN_POINT('Ctrl Pts',(-23.7452757946167,-14.249499803588,
113.441750983595)) ;
#178877 = CARTESIAN_POINT('Ctrl Pts',(-23.6714719723636,-14.249499849912,
113.465982089752)) ;
#178878 = CARTESIAN_POINT('Ctrl Pts',(-23.6578570619302,-14.3116012090706,
113.424513270916)) ;
#178879 = CARTESIAN_POINT('Ctrl Pts',(-23.6442421514968,-14.3737025682292,
113.383044452081)) ;
#178880 = CARTESIAN_POINT('Ctrl Pts',(-23.7180459737499,-14.3737025219051,
113.358813345924)) ;
#178881 = CARTESIAN_POINT('Ctrl Pts',(-23.7918497960029,-14.3737024755811,
113.334582239768)) ;
#178882 = CARTESIAN_POINT('Ctrl Pts',(-23.8054647064364,-14.3116011164225,
113.376051058603)) ;
#178883 = CARTESIAN_POINT('Ctrl Pts',(-23.8758475364015,-14.4442909382302,
113.625906113769)) ;
#178884 = CARTESIAN_POINT('Ctrl Pts',(-23.8838347972143,-14.3728313741273,
113.650234020023)) ;
#178885 = CARTESIAN_POINT('Ctrl Pts',(-23.8100309758451,-14.3728313982058,
113.674465128872)) ;
#178886 = CARTESIAN_POINT('Ctrl Pts',(-23.7362271544759,-14.3728314222843,
113.698696237721)) ;
#178887 = CARTESIAN_POINT('Ctrl Pts',(-23.7282398936631,-14.4442909863872,
113.674368331467)) ;
#178888 = CARTESIAN_POINT('Ctrl Pts',(-23.7202526328503,-14.5157505504901,
113.650040425214)) ;
#178889 = CARTESIAN_POINT('Ctrl Pts',(-23.7940564542195,-14.5157505264116,
113.625809316365)) ;
#178890 = CARTESIAN_POINT('Ctrl Pts',(-23.8678602755887,-14.5157505023331,
113.601578207516)) ;
#178891 = CARTESIAN_POINT('Ctrl Pts',(-23.8758475364015,-14.4442909382302,
113.625906113769)) ;
#178892 = CARTESIAN_POINT('Ctrl Pts',(-23.9543884340958,-14.5033545209173,
113.900640311808)) ;
#178893 = CARTESIAN_POINT('Ctrl Pts',(-23.9561692678758,-14.4276627971391,
113.906064442885)) ;
#178894 = CARTESIAN_POINT('Ctrl Pts',(-23.8823654450948,-14.4276628009884,
113.930295547434)) ;
#178895 = CARTESIAN_POINT('Ctrl Pts',(-23.8085616223137,-14.4276628048377,
113.954526651983)) ;
#178896 = CARTESIAN_POINT('Ctrl Pts',(-23.8067807885338,-14.5033545286159,
113.949102520905)) ;
#178897 = CARTESIAN_POINT('Ctrl Pts',(-23.8049999547538,-14.5790462523942,
113.943678389828)) ;
#178898 = CARTESIAN_POINT('Ctrl Pts',(-23.8788037775349,-14.5790462485448,
113.91944728528)) ;
#178899 = CARTESIAN_POINT('Ctrl Pts',(-23.9526076003159,-14.5790462446955,
113.895216180731)) ;
#178900 = CARTESIAN_POINT('Ctrl Pts',(-23.9543884340958,-14.5033545209173,
113.900640311808)) ;
#178901 = CARTESIAN_POINT('Ctrl Pts',(-24.034459322074,-14.4845849990311,
114.179961742102)) ;
#178902 = CARTESIAN_POINT('Ctrl Pts',(-24.0299189346052,-14.4100891125331,
114.166132453338)) ;
#178903 = CARTESIAN_POINT('Ctrl Pts',(-23.9561151089116,-14.4100891003362,
114.190363549015)) ;
#178904 = CARTESIAN_POINT('Ctrl Pts',(-23.8823112832179,-14.4100890881394,
114.214594644693)) ;
#178905 = CARTESIAN_POINT('Ctrl Pts',(-23.8868516706868,-14.4845849746373,
114.228423933456)) ;
#178906 = CARTESIAN_POINT('Ctrl Pts',(-23.8913920581557,-14.5590808611353,
114.24225322222)) ;
#178907 = CARTESIAN_POINT('Ctrl Pts',(-23.9651958838493,-14.5590808733321,
114.218022126543)) ;
#178908 = CARTESIAN_POINT('Ctrl Pts',(-24.0389997095429,-14.559080885529,
114.193791030865)) ;
#178909 = CARTESIAN_POINT('Ctrl Pts',(-24.034459322074,-14.4845849990311,
114.179961742102)) ;
#178910 = CARTESIAN_POINT('Ctrl Pts',(-24.1098198340275,-14.3894948595566,
114.444970199635)) ;
#178911 = CARTESIAN_POINT('Ctrl Pts',(-24.0992767680653,-14.3215252408879,
114.412857720877)) ;
#178912 = CARTESIAN_POINT('Ctrl Pts',(-24.0254729382836,-14.3215252179033,
114.437088804104)) ;
#178913 = CARTESIAN_POINT('Ctrl Pts',(-23.951669108502,-14.3215251949188,
114.46131988733)) ;
#178914 = CARTESIAN_POINT('Ctrl Pts',(-23.9622121744642,-14.3894948135875,
114.493432366087)) ;
#178915 = CARTESIAN_POINT('Ctrl Pts',(-23.9727552404264,-14.4574644322562,
114.525544844844)) ;
#178916 = CARTESIAN_POINT('Ctrl Pts',(-24.0465590702081,-14.4574644552408,
114.501313761618)) ;
#178917 = CARTESIAN_POINT('Ctrl Pts',(-24.1203628999897,-14.4574644782253,
114.477082678392)) ;
#178918 = CARTESIAN_POINT('Ctrl Pts',(-24.1098198340275,-14.3894948595566,
114.444970199635)) ;
#178919 = CARTESIAN_POINT('Ctrl Pts',(-24.1743167962616,-14.2243477865837,
114.676951586264)) ;
#178920 = CARTESIAN_POINT('Ctrl Pts',(-24.1585190622833,-14.1678057740267,
114.628834236749)) ;
#178921 = CARTESIAN_POINT('Ctrl Pts',(-24.0847152279406,-14.1678057466232,
114.653065306083)) ;
#178922 = CARTESIAN_POINT('Ctrl Pts',(-24.0109113935979,-14.1678057192196,
114.677296375417)) ;
#178923 = CARTESIAN_POINT('Ctrl Pts',(-24.0267091275762,-14.2243477317766,
114.725413724931)) ;
#178924 = CARTESIAN_POINT('Ctrl Pts',(-24.0425068615545,-14.2808897443336,
114.773531074446)) ;
#178925 = CARTESIAN_POINT('Ctrl Pts',(-24.1163106958972,-14.2808897717371,
114.749300005113)) ;
#178926 = CARTESIAN_POINT('Ctrl Pts',(-24.1901145302398,-14.2808897991407,
114.725068935779)) ;
#178927 = CARTESIAN_POINT('Ctrl Pts',(-24.1743167962616,-14.2243477865837,
114.676951586264)) ;
#178928 = CARTESIAN_POINT('Ctrl Pts',(-24.222244696456,-14.0022176408066,
114.858320300605)) ;
#178929 = CARTESIAN_POINT('Ctrl Pts',(-24.2023442920191,-13.9610998254784,
114.797706878987)) ;
#178930 = CARTESIAN_POINT('Ctrl Pts',(-24.128540453823,-13.9610997980143,
114.821937936584)) ;
#178931 = CARTESIAN_POINT('Ctrl Pts',(-24.0547366156269,-13.9610997705502,
114.846168994181)) ;
#178932 = CARTESIAN_POINT('Ctrl Pts',(-24.0746370200638,-14.0022175858784,
114.906782415799)) ;
#178933 = CARTESIAN_POINT('Ctrl Pts',(-24.0945374245007,-14.0433354012065,
114.967395837416)) ;
#178934 = CARTESIAN_POINT('Ctrl Pts',(-24.1683412626968,-14.0433354286706,
114.943164779819)) ;
#178935 = CARTESIAN_POINT('Ctrl Pts',(-24.2421451008929,-14.0433354561347,
114.918933722222)) ;
#178936 = CARTESIAN_POINT('Ctrl Pts',(-24.222244696456,-14.0022176408066,
114.858320300605)) ;
#178937 = CARTESIAN_POINT('Ctrl Pts',(-24.249840889695,-13.738467096939,114.977769983769)) ;
#178938 = CARTESIAN_POINT('Ctrl Pts',(-24.2272510577212,-13.7157029540504,
114.90896499996)) ;
#178939 = CARTESIAN_POINT('Ctrl Pts',(-24.1534472163186,-13.7157029304284,
114.933196047791)) ;
#178940 = CARTESIAN_POINT('Ctrl Pts',(-24.0796433749161,-13.7157029068064,
114.957427095621)) ;
#178941 = CARTESIAN_POINT('Ctrl Pts',(-24.1022332068898,-13.7384670496951,
115.02623207943)) ;
#178942 = CARTESIAN_POINT('Ctrl Pts',(-24.1248230388635,-13.7612311925838,
115.09503706324)) ;
#178943 = CARTESIAN_POINT('Ctrl Pts',(-24.1986268802661,-13.7612312162057,
115.070806015409)) ;
#178944 = CARTESIAN_POINT('Ctrl Pts',(-24.2724307216687,-13.7612312398277,
115.046574967579)) ;
#178945 = CARTESIAN_POINT('Ctrl Pts',(-24.249840889695,-13.738467096939,114.977769983769)) ;
#178946 = CARTESIAN_POINT('Ctrl Pts',(-24.2541673118349,-13.4497089979361,
115.026595498721)) ;
#178947 = CARTESIAN_POINT('Ctrl Pts',(-24.2305033326588,-13.4470729422015,
114.954518836024)) ;
#178948 = CARTESIAN_POINT('Ctrl Pts',(-24.1566994891785,-13.4470729268746,
114.978749877526)) ;
#178949 = CARTESIAN_POINT('Ctrl Pts',(-24.0828956456982,-13.4470729115476,
115.002980919029)) ;
#178950 = CARTESIAN_POINT('Ctrl Pts',(-24.1065596248743,-13.4497089672822,
115.075057581726)) ;
#178951 = CARTESIAN_POINT('Ctrl Pts',(-24.1302236040503,-13.4523450230167,
115.147134244423)) ;
#178952 = CARTESIAN_POINT('Ctrl Pts',(-24.2040274475306,-13.4523450383437,
115.122903202921)) ;
#178953 = CARTESIAN_POINT('Ctrl Pts',(-24.2778312910109,-13.4523450536706,
115.098672161419)) ;
#178954 = CARTESIAN_POINT('Ctrl Pts',(-24.2541673118349,-13.4497089979361,
115.026595498721)) ;
#178955 = CARTESIAN_POINT('Ctrl Pts',(-24.2342295189752,-13.1612741016994,
115.001189108722)) ;
#178956 = CARTESIAN_POINT('Ctrl Pts',(-24.2111911927436,-13.1787740076572,
114.931018084053)) ;
#178957 = CARTESIAN_POINT('Ctrl Pts',(-24.1373873484711,-13.1787739983459,
114.955249123143)) ;
#178958 = CARTESIAN_POINT('Ctrl Pts',(-24.0635835041986,-13.1787739890347,
114.979480162232)) ;
#178959 = CARTESIAN_POINT('Ctrl Pts',(-24.0866218304302,-13.161274083077,
115.049651186901)) ;
#178960 = CARTESIAN_POINT('Ctrl Pts',(-24.1096601566617,-13.1437741771192,
115.11982221157)) ;
#178961 = CARTESIAN_POINT('Ctrl Pts',(-24.1834640009343,-13.1437741864305,
115.095591172481)) ;
#178962 = CARTESIAN_POINT('Ctrl Pts',(-24.2572678452068,-13.1437741957417,
115.071360133392)) ;
#178963 = CARTESIAN_POINT('Ctrl Pts',(-24.2342295189752,-13.1612741016994,
115.001189108722)) ;
#178964 = CARTESIAN_POINT('Ctrl Pts',(-24.190640216784,-12.8897094409154,
114.903930822118)) ;
#178965 = CARTESIAN_POINT('Ctrl Pts',(-24.1698760482874,-12.9261981229531,
114.840686515092)) ;
#178966 = CARTESIAN_POINT('Ctrl Pts',(-24.0960722041816,-12.9261981199508,
114.864917554689)) ;
#178967 = CARTESIAN_POINT('Ctrl Pts',(-24.0222683600759,-12.9261981169484,
114.889148594286)) ;
#178968 = CARTESIAN_POINT('Ctrl Pts',(-24.0430325285724,-12.8897094349106,
114.952392901312)) ;
#178969 = CARTESIAN_POINT('Ctrl Pts',(-24.063796697069,-12.8532207528728,
115.015637208338)) ;
#178970 = CARTESIAN_POINT('Ctrl Pts',(-24.1376005411748,-12.8532207558752,
114.991406168741)) ;
#178971 = CARTESIAN_POINT('Ctrl Pts',(-24.2114043852805,-12.8532207588776,
114.967175129144)) ;
#178972 = CARTESIAN_POINT('Ctrl Pts',(-24.190640216784,-12.8897094409154,
114.903930822118)) ;
#178973 = CARTESIAN_POINT('Ctrl Pts',(-24.12571950388,-12.6562456914582,114.741683307062)) ;
#178974 = CARTESIAN_POINT('Ctrl Pts',(-24.1087229981294,-12.7090913672215,
114.689914692932)) ;
#178975 = CARTESIAN_POINT('Ctrl Pts',(-24.0349191547742,-12.7090913678115,
114.714145734815)) ;
#178976 = CARTESIAN_POINT('Ctrl Pts',(-23.9611153114191,-12.7090913684014,
114.738376776699)) ;
#178977 = CARTESIAN_POINT('Ctrl Pts',(-23.9781118171697,-12.6562456926381,
114.790145390829)) ;
#178978 = CARTESIAN_POINT('Ctrl Pts',(-23.9951083229202,-12.6034000168748,
114.841914004959)) ;
#178979 = CARTESIAN_POINT('Ctrl Pts',(-24.0689121662754,-12.6034000162848,
114.817682963075)) ;
#178980 = CARTESIAN_POINT('Ctrl Pts',(-24.1427160096306,-12.6034000156949,
114.793451921192)) ;
#178981 = CARTESIAN_POINT('Ctrl Pts',(-24.12571950388,-12.6562456914582,114.741683307062)) ;
#178982 = CARTESIAN_POINT('Ctrl Pts',(-24.0436220945344,-12.4776727385034,
114.527047044572)) ;
#178983 = CARTESIAN_POINT('Ctrl Pts',(-24.0315999579,-12.5430665367951,114.490429556204)) ;
#178984 = CARTESIAN_POINT('Ctrl Pts',(-23.9577961152497,-12.5430665383516,
114.514660600234)) ;
#178985 = CARTESIAN_POINT('Ctrl Pts',(-23.8839922725995,-12.543066539908,
114.538891644265)) ;
#178986 = CARTESIAN_POINT('Ctrl Pts',(-23.896014409234,-12.4776727416163,
114.575509132633)) ;
#178987 = CARTESIAN_POINT('Ctrl Pts',(-23.9080365458684,-12.4122789433245,
114.612126621002)) ;
#178988 = CARTESIAN_POINT('Ctrl Pts',(-23.9818403885187,-12.4122789417681,
114.587895576971)) ;
#178989 = CARTESIAN_POINT('Ctrl Pts',(-24.0556442311689,-12.4122789402116,
114.563664532941)) ;
#178990 = CARTESIAN_POINT('Ctrl Pts',(-24.0436220945344,-12.4776727385034,
114.527047044572)) ;
#178991 = CARTESIAN_POINT('Ctrl Pts',(-23.949166950014,-12.3662041520314,
114.27482871689)) ;
#178992 = CARTESIAN_POINT('Ctrl Pts',(-23.9429885673847,-12.439478800866,
114.256010360343)) ;
#178993 = CARTESIAN_POINT('Ctrl Pts',(-23.8691847249648,-12.4394788016548,
114.280241405074)) ;
#178994 = CARTESIAN_POINT('Ctrl Pts',(-23.7953808825448,-12.4394788024435,
114.304472449806)) ;
#178995 = CARTESIAN_POINT('Ctrl Pts',(-23.8015592651741,-12.3662041536089,
114.323290806354)) ;
#178996 = CARTESIAN_POINT('Ctrl Pts',(-23.8077376478033,-12.2929295047743,
114.342109162901)) ;
#178997 = CARTESIAN_POINT('Ctrl Pts',(-23.8815414902233,-12.2929295039855,
114.317878118169)) ;
#178998 = CARTESIAN_POINT('Ctrl Pts',(-23.9553453326433,-12.2929295031968,
114.293647073438)) ;
#178999 = CARTESIAN_POINT('Ctrl Pts',(-23.949166950014,-12.3662041520314,
114.27482871689)) ;
#179000 = CARTESIAN_POINT('Ctrl Pts',(-23.8486819494618,-12.3300379060018,
114.004176603024)) ;
#179001 = CARTESIAN_POINT('Ctrl Pts',(-23.8487783311831,-12.4059457816004,
114.004470166228)) ;
#179002 = CARTESIAN_POINT('Ctrl Pts',(-23.7749744882838,-12.405945781314,
114.0287012095)) ;
#179003 = CARTESIAN_POINT('Ctrl Pts',(-23.7011706453844,-12.4059457810276,
114.052932252771)) ;
#179004 = CARTESIAN_POINT('Ctrl Pts',(-23.7010742636631,-12.330037905429,
114.052638689568)) ;
#179005 = CARTESIAN_POINT('Ctrl Pts',(-23.7009778819417,-12.2541300298303,
114.052345126364)) ;
#179006 = CARTESIAN_POINT('Ctrl Pts',(-23.7747817248411,-12.2541300301167,
114.028114083092)) ;
#179007 = CARTESIAN_POINT('Ctrl Pts',(-23.8485855677404,-12.2541300304032,
114.00388303982)) ;
#179008 = CARTESIAN_POINT('Ctrl Pts',(-23.8486819494618,-12.3300379060018,
114.004176603024)) ;
#179009 = CARTESIAN_POINT('Ctrl Pts',(-23.7479716280047,-12.3719948524369,
113.733003975022)) ;
#179010 = CARTESIAN_POINT('Ctrl Pts',(-23.7543642990967,-12.4450845928375,
113.752475019667)) ;
#179011 = CARTESIAN_POINT('Ctrl Pts',(-23.6805604549014,-12.4450845931213,
113.776706058991)) ;
#179012 = CARTESIAN_POINT('Ctrl Pts',(-23.606756610706,-12.4450845934052,
113.800937098315)) ;
#179013 = CARTESIAN_POINT('Ctrl Pts',(-23.600363939614,-12.3719948530046,
113.781466053671)) ;
#179014 = CARTESIAN_POINT('Ctrl Pts',(-23.593971268522,-12.298905112604,113.761995009026)) ;
#179015 = CARTESIAN_POINT('Ctrl Pts',(-23.6677751127173,-12.2989051123201,
113.737763969702)) ;
#179016 = CARTESIAN_POINT('Ctrl Pts',(-23.7415789569127,-12.2989051120363,
113.713532930378)) ;
#179017 = CARTESIAN_POINT('Ctrl Pts',(-23.7479716280047,-12.3719948524369,
113.733003975022)) ;
#179018 = CARTESIAN_POINT('Ctrl Pts',(-23.6544815761993,-12.4886302946211,
113.483633344995)) ;
#179019 = CARTESIAN_POINT('Ctrl Pts',(-23.6666792066729,-12.5536824070631,
113.520785359195)) ;
#179020 = CARTESIAN_POINT('Ctrl Pts',(-23.5928753612354,-12.5536824104958,
113.545016394736)) ;
#179021 = CARTESIAN_POINT('Ctrl Pts',(-23.519071515798,-12.5536824139286,
113.569247430277)) ;
#179022 = CARTESIAN_POINT('Ctrl Pts',(-23.5068738853244,-12.4886303014866,
113.532095416077)) ;
#179023 = CARTESIAN_POINT('Ctrl Pts',(-23.4946762548508,-12.4235781890446,
113.494943401877)) ;
#179024 = CARTESIAN_POINT('Ctrl Pts',(-23.5684801002883,-12.4235781856119,
113.470712366336)) ;
#179025 = CARTESIAN_POINT('Ctrl Pts',(-23.6422839457257,-12.4235781821791,
113.446481330795)) ;
#179026 = CARTESIAN_POINT('Ctrl Pts',(-23.6544815761993,-12.4886302946211,
113.483633344995)) ;
#179027 = CARTESIAN_POINT('Ctrl Pts',(-23.5734119895845,-12.6716133926028,
113.272144861852)) ;
#179028 = CARTESIAN_POINT('Ctrl Pts',(-23.5905546162055,-12.7239835426952,
113.324358536327)) ;
#179029 = CARTESIAN_POINT('Ctrl Pts',(-23.5167507697617,-12.7239835519862,
113.348589568803)) ;
#179030 = CARTESIAN_POINT('Ctrl Pts',(-23.4429469233179,-12.7239835612772,
113.372820601279)) ;
#179031 = CARTESIAN_POINT('Ctrl Pts',(-23.425804296697,-12.6716134111847,
113.320606926803)) ;
#179032 = CARTESIAN_POINT('Ctrl Pts',(-23.408661670076,-12.6192432610923,
113.268393252328)) ;
#179033 = CARTESIAN_POINT('Ctrl Pts',(-23.4824655165198,-12.6192432518013,
113.244162219852)) ;
#179034 = CARTESIAN_POINT('Ctrl Pts',(-23.5562693629636,-12.6192432425104,
113.219931187376)) ;
#179035 = CARTESIAN_POINT('Ctrl Pts',(-23.5734119895845,-12.6716133926028,
113.272144861852)) ;
#179036 = CARTESIAN_POINT('Ctrl Pts',(-23.5097546848615,-12.9096205473869,
113.113892958082)) ;
#179037 = CARTESIAN_POINT('Ctrl Pts',(-23.5306295961467,-12.9454485292725,
113.177474569271)) ;
#179038 = CARTESIAN_POINT('Ctrl Pts',(-23.4568257492868,-12.9454485486713,
113.201705600479)) ;
#179039 = CARTESIAN_POINT('Ctrl Pts',(-23.3830219024269,-12.9454485680701,
113.225936631688)) ;
#179040 = CARTESIAN_POINT('Ctrl Pts',(-23.3621469911418,-12.9096205861845,
113.162355020499)) ;
#179041 = CARTESIAN_POINT('Ctrl Pts',(-23.3412720798566,-12.8737926042989,
113.098773409311)) ;
#179042 = CARTESIAN_POINT('Ctrl Pts',(-23.4150759267165,-12.8737925849001,
113.074542378102)) ;
#179043 = CARTESIAN_POINT('Ctrl Pts',(-23.4888797735763,-12.8737925655013,
113.050311346893)) ;
#179044 = CARTESIAN_POINT('Ctrl Pts',(-23.5097546848615,-12.9096205473869,
113.113892958082)) ;
#179045 = CARTESIAN_POINT('Ctrl Pts',(-23.4680736791357,-13.1819739695916,
113.02227623672)) ;
#179046 = CARTESIAN_POINT('Ctrl Pts',(-23.4911576828605,-13.1988376121803,
113.09258638691)) ;
#179047 = CARTESIAN_POINT('Ctrl Pts',(-23.4173538372792,-13.1988376406376,
113.116817422013)) ;
#179048 = CARTESIAN_POINT('Ctrl Pts',(-23.3435499916979,-13.198837669095,
113.141048457116)) ;
#179049 = CARTESIAN_POINT('Ctrl Pts',(-23.3204659879731,-13.1819740265063,
113.070738306926)) ;
#179050 = CARTESIAN_POINT('Ctrl Pts',(-23.2973819842482,-13.1651103839176,
113.000428156736)) ;
#179051 = CARTESIAN_POINT('Ctrl Pts',(-23.3711858298295,-13.1651103554602,
112.976197121633)) ;
#179052 = CARTESIAN_POINT('Ctrl Pts',(-23.4449896754108,-13.1651103270029,
112.951966086531)) ;
#179053 = CARTESIAN_POINT('Ctrl Pts',(-23.4680736791357,-13.1819739695916,
113.02227623672)) ;
#179054 = CARTESIAN_POINT('Ctrl Pts',(-23.4498548257593,-13.4720244815185,
113.002241777348)) ;
#179055 = CARTESIAN_POINT('Ctrl Pts',(-23.4735105433531,-13.4686610544737,
113.074293275574)) ;
#179056 = CARTESIAN_POINT('Ctrl Pts',(-23.399706700273,-13.4686610921263,
113.098524318295)) ;
#179057 = CARTESIAN_POINT('Ctrl Pts',(-23.3259028571929,-13.4686611297789,
113.122755361017)) ;
#179058 = CARTESIAN_POINT('Ctrl Pts',(-23.3022471395991,-13.4720245568238,
113.05070386279)) ;
#179059 = CARTESIAN_POINT('Ctrl Pts',(-23.2785914220053,-13.4753879838686,
112.978652364563)) ;
#179060 = CARTESIAN_POINT('Ctrl Pts',(-23.3523952650854,-13.475387946216,
112.954421321842)) ;
#179061 = CARTESIAN_POINT('Ctrl Pts',(-23.4261991081655,-13.4753879085634,
112.930190279121)) ;
#179062 = CARTESIAN_POINT('Ctrl Pts',(-23.4498548257593,-13.4720244815185,
113.002241777348)) ;
#179063 = CARTESIAN_POINT('Ctrl Pts',(-23.4559991647249,-13.7591219512168,
113.056520534112)) ;
#179064 = CARTESIAN_POINT('Ctrl Pts',(-23.4785242563665,-13.7357085596368,
113.125128327926)) ;
#179065 = CARTESIAN_POINT('Ctrl Pts',(-23.4047204173389,-13.7357086049052,
113.14935938299)) ;
#179066 = CARTESIAN_POINT('Ctrl Pts',(-23.3309165783112,-13.7357086501736,
113.173590438055)) ;
#179067 = CARTESIAN_POINT('Ctrl Pts',(-23.3083914866696,-13.7591220417536,
113.10498264424)) ;
#179068 = CARTESIAN_POINT('Ctrl Pts',(-23.285866395028,-13.7825354333337,
113.036374850426)) ;
#179069 = CARTESIAN_POINT('Ctrl Pts',(-23.3596702340557,-13.7825353880653,
113.012143795361)) ;
#179070 = CARTESIAN_POINT('Ctrl Pts',(-23.4334740730833,-13.7825353427969,
112.987912740297)) ;
#179071 = CARTESIAN_POINT('Ctrl Pts',(-23.4559991647249,-13.7591219512168,
113.056520534112)) ;
#179072 = CARTESIAN_POINT('Ctrl Pts',(-23.4853259386765,-14.0209982570872,
113.181335126666)) ;
#179073 = CARTESIAN_POINT('Ctrl Pts',(-23.5051016687503,-13.9792670582561,
113.241568808581)) ;
#179074 = CARTESIAN_POINT('Ctrl Pts',(-23.4312978349103,-13.9792671054372,
113.265799879446)) ;
#179075 = CARTESIAN_POINT('Ctrl Pts',(-23.3574940010702,-13.9792671526183,
113.29003095031)) ;
#179076 = CARTESIAN_POINT('Ctrl Pts',(-23.3377182709964,-14.0209983514494,
113.229797268396)) ;
#179077 = CARTESIAN_POINT('Ctrl Pts',(-23.3179425409226,-14.0627295502805,
113.169563586481)) ;
#179078 = CARTESIAN_POINT('Ctrl Pts',(-23.3917463747627,-14.0627295030994,
113.145332515616)) ;
#179079 = CARTESIAN_POINT('Ctrl Pts',(-23.4655502086028,-14.0627294559183,
113.121101444752)) ;
#179080 = CARTESIAN_POINT('Ctrl Pts',(-23.4853259386765,-14.0209982570872,
113.181335126666)) ;
#179081 = CARTESIAN_POINT('Ctrl Pts',(-23.5345041189141,-14.2386408615737,
113.36640397491)) ;
#179082 = CARTESIAN_POINT('Ctrl Pts',(-23.5501447454779,-14.1816542557546,
113.4140427986)) ;
#179083 = CARTESIAN_POINT('Ctrl Pts',(-23.4763409167572,-14.1816542976557,
113.438273885057)) ;
#179084 = CARTESIAN_POINT('Ctrl Pts',(-23.4025370880364,-14.1816543395568,
113.462504971515)) ;
#179085 = CARTESIAN_POINT('Ctrl Pts',(-23.3868964614725,-14.2386409453758,
113.414866147825)) ;
#179086 = CARTESIAN_POINT('Ctrl Pts',(-23.3712558349086,-14.2956275511949,
113.367227324135)) ;
#179087 = CARTESIAN_POINT('Ctrl Pts',(-23.4450596636294,-14.2956275092938,
113.342996237677)) ;
#179088 = CARTESIAN_POINT('Ctrl Pts',(-23.5188634923502,-14.2956274673927,
113.31876515122)) ;
#179089 = CARTESIAN_POINT('Ctrl Pts',(-23.5345041189141,-14.2386408615737,
113.36640397491)) ;
#179090 = CARTESIAN_POINT('Ctrl Pts',(-23.6001054827243,-14.3991847031552,
113.601804261301)) ;
#179091 = CARTESIAN_POINT('Ctrl Pts',(-23.6104522949311,-14.3309065513588,
113.633318980433)) ;
#179092 = CARTESIAN_POINT('Ctrl Pts',(-23.5366484717624,-14.330906583244,
113.657550083801)) ;
#179093 = CARTESIAN_POINT('Ctrl Pts',(-23.4628446485939,-14.3309066151293,
113.68178118717)) ;
#179094 = CARTESIAN_POINT('Ctrl Pts',(-23.4524978363872,-14.3991847669257,
113.650266468038)) ;
#179095 = CARTESIAN_POINT('Ctrl Pts',(-23.4421510241805,-14.4674629187221,
113.618751748905)) ;
#179096 = CARTESIAN_POINT('Ctrl Pts',(-23.515954847349,-14.4674628868368,
113.594520645537)) ;
#179097 = CARTESIAN_POINT('Ctrl Pts',(-23.5897586705176,-14.4674628549516,
113.570289542169)) ;
#179098 = CARTESIAN_POINT('Ctrl Pts',(-23.6001054827243,-14.3991847031552,
113.601804261301)) ;
#179099 = CARTESIAN_POINT('Ctrl Pts',(-23.6758396635348,-14.4885294284138,
113.867853985645)) ;
#179100 = CARTESIAN_POINT('Ctrl Pts',(-23.6801818892424,-14.4139147342441,
113.881079703006)) ;
#179101 = CARTESIAN_POINT('Ctrl Pts',(-23.6063780700887,-14.4139147488746,
113.905310818603)) ;
#179102 = CARTESIAN_POINT('Ctrl Pts',(-23.5325742509351,-14.4139147635052,
113.929541934201)) ;
#179103 = CARTESIAN_POINT('Ctrl Pts',(-23.5282320252275,-14.4885294576749,
113.91631621684)) ;
#179104 = CARTESIAN_POINT('Ctrl Pts',(-23.52388979952,-14.5631441518446,113.903090499479)) ;
#179105 = CARTESIAN_POINT('Ctrl Pts',(-23.5976936186736,-14.563144137214,
113.878859383882)) ;
#179106 = CARTESIAN_POINT('Ctrl Pts',(-23.6714974378272,-14.5631441225835,
113.854628268285)) ;
#179107 = CARTESIAN_POINT('Ctrl Pts',(-23.6758396635348,-14.4885294284138,
113.867853985645)) ;
#179108 = CARTESIAN_POINT('Ctrl Pts',(-23.7560787132041,-14.5016597743674,
114.147723270265)) ;
#179109 = CARTESIAN_POINT('Ctrl Pts',(-23.7540912036683,-14.4260199965907,
114.141669635237)) ;
#179110 = CARTESIAN_POINT('Ctrl Pts',(-23.6802873870442,-14.4260199894703,
114.165900758539)) ;
#179111 = CARTESIAN_POINT('Ctrl Pts',(-23.60648357042,-14.4260199823499,114.19013188184)) ;
#179112 = CARTESIAN_POINT('Ctrl Pts',(-23.6084710799558,-14.5016597601266,
114.196185516868)) ;
#179113 = CARTESIAN_POINT('Ctrl Pts',(-23.6104585894916,-14.5772995379034,
114.202239151896)) ;
#179114 = CARTESIAN_POINT('Ctrl Pts',(-23.6842624061158,-14.5772995450237,
114.178008028595)) ;
#179115 = CARTESIAN_POINT('Ctrl Pts',(-23.7580662227399,-14.5772995521441,
114.153776905293)) ;
#179116 = CARTESIAN_POINT('Ctrl Pts',(-23.7560787132041,-14.5016597743674,
114.147723270265)) ;
#179117 = CARTESIAN_POINT('Ctrl Pts',(-23.8342305464961,-14.437009415365,
114.421263368043)) ;
#179118 = CARTESIAN_POINT('Ctrl Pts',(-23.8260492739451,-14.3657730764766,
114.396344530107)) ;
#179119 = CARTESIAN_POINT('Ctrl Pts',(-23.7522454576535,-14.3657730444813,
114.420575654421)) ;
#179120 = CARTESIAN_POINT('Ctrl Pts',(-23.678441641362,-14.365773012486,114.444806778735)) ;
#179121 = CARTESIAN_POINT('Ctrl Pts',(-23.6866229139129,-14.4370093513744,
114.469725616672)) ;
#179122 = CARTESIAN_POINT('Ctrl Pts',(-23.6948041864639,-14.5082456902627,
114.494644454609)) ;
#179123 = CARTESIAN_POINT('Ctrl Pts',(-23.7686080027555,-14.508245722258,
114.470413330295)) ;
#179124 = CARTESIAN_POINT('Ctrl Pts',(-23.8424118190471,-14.5082457542533,
114.44618220598)) ;
#179125 = CARTESIAN_POINT('Ctrl Pts',(-23.8342305464961,-14.437009415365,
114.421263368043)) ;
#179126 = CARTESIAN_POINT('Ctrl Pts',(-23.9038790142128,-14.2988734246617,
114.668946179201)) ;
#179127 = CARTESIAN_POINT('Ctrl Pts',(-23.8900877080365,-14.2371769971241,
114.626940083908)) ;
#179128 = CARTESIAN_POINT('Ctrl Pts',(-23.8162838894959,-14.237176939765,
114.651171201373)) ;
#179129 = CARTESIAN_POINT('Ctrl Pts',(-23.7424800709552,-14.2371768824059,
114.675402318837)) ;
#179130 = CARTESIAN_POINT('Ctrl Pts',(-23.7562713771315,-14.2988733099436,
114.717408414129)) ;
#179131 = CARTESIAN_POINT('Ctrl Pts',(-23.7700626833078,-14.3605697374812,
114.759414509421)) ;
#179132 = CARTESIAN_POINT('Ctrl Pts',(-23.8438665018485,-14.3605697948403,
114.735183391957)) ;
#179133 = CARTESIAN_POINT('Ctrl Pts',(-23.9176703203892,-14.3605698521993,
114.710952274493)) ;
#179134 = CARTESIAN_POINT('Ctrl Pts',(-23.9038790142128,-14.2988734246617,
114.668946179201)) ;
#179135 = CARTESIAN_POINT('Ctrl Pts',(-23.9589267388881,-14.0989764690058,
114.871924271344)) ;
#179136 = CARTESIAN_POINT('Ctrl Pts',(-23.9405414467477,-14.0511462695814,
114.815925635974)) ;
#179137 = CARTESIAN_POINT('Ctrl Pts',(-23.8667376232761,-14.0511461903864,
114.840156738419)) ;
#179138 = CARTESIAN_POINT('Ctrl Pts',(-23.7929337998045,-14.0511461111915,
114.864387840864)) ;
#179139 = CARTESIAN_POINT('Ctrl Pts',(-23.8113190919448,-14.0989763106159,
114.920386476235)) ;
#179140 = CARTESIAN_POINT('Ctrl Pts',(-23.8297043840852,-14.1468065100403,
114.976385111605)) ;
#179141 = CARTESIAN_POINT('Ctrl Pts',(-23.9035082075568,-14.1468065892353,
114.95215400916)) ;
#179142 = CARTESIAN_POINT('Ctrl Pts',(-23.9773120310284,-14.1468066684302,
114.927922906715)) ;
#179143 = CARTESIAN_POINT('Ctrl Pts',(-23.9589267388881,-14.0989764690058,
114.871924271344)) ;
#179144 = CARTESIAN_POINT('Ctrl Pts',(-23.9954157212117,-13.8484694868484,
115.01867831934)) ;
#179145 = CARTESIAN_POINT('Ctrl Pts',(-23.973718935146,-13.8180580458534,
114.952593407707)) ;
#179146 = CARTESIAN_POINT('Ctrl Pts',(-23.8999151048323,-13.8180579489714,
114.976824489312)) ;
#179147 = CARTESIAN_POINT('Ctrl Pts',(-23.8261112745187,-13.8180578520894,
115.001055570918)) ;
#179148 = CARTESIAN_POINT('Ctrl Pts',(-23.8478080605844,-13.8484692930843,
115.067140482551)) ;
#179149 = CARTESIAN_POINT('Ctrl Pts',(-23.8695048466502,-13.8788807340793,
115.133225394185)) ;
#179150 = CARTESIAN_POINT('Ctrl Pts',(-23.9433086769638,-13.8788808309613,
115.108994312579)) ;
#179151 = CARTESIAN_POINT('Ctrl Pts',(-24.0171125072775,-13.8788809278433,
115.084763230974)) ;
#179152 = CARTESIAN_POINT('Ctrl Pts',(-23.9954157212117,-13.8484694868484,
115.01867831934)) ;
#179153 = CARTESIAN_POINT('Ctrl Pts',(-24.0092992091124,-13.5679794956402,
115.096428165126)) ;
#179154 = CARTESIAN_POINT('Ctrl Pts',(-23.9858673863467,-13.5571060309524,
115.025058611615)) ;
#179155 = CARTESIAN_POINT('Ctrl Pts',(-23.9120635475771,-13.5571059245038,
115.049289667465)) ;
#179156 = CARTESIAN_POINT('Ctrl Pts',(-23.8382597088075,-13.5571058180553,
115.073520723315)) ;
#179157 = CARTESIAN_POINT('Ctrl Pts',(-23.8616915315733,-13.567979282743,
115.144890276826)) ;
#179158 = CARTESIAN_POINT('Ctrl Pts',(-23.885123354339,-13.5788527474308,
115.216259830337)) ;
#179159 = CARTESIAN_POINT('Ctrl Pts',(-23.9589271931086,-13.5788528538794,
115.192028774487)) ;
#179160 = CARTESIAN_POINT('Ctrl Pts',(-24.0327310318782,-13.578852960328,
115.167797718637)) ;
#179161 = CARTESIAN_POINT('Ctrl Pts',(-24.0092992091124,-13.5679794956402,
115.096428165126)) ;
#179162 = CARTESIAN_POINT('Ctrl Pts',(-23.9992431261541,-13.2778704302602,
115.101136556638)) ;
#179163 = CARTESIAN_POINT('Ctrl Pts',(-23.9757477130597,-13.2872353982741,
115.02957331723)) ;
#179164 = CARTESIAN_POINT('Ctrl Pts',(-23.9019438652982,-13.2872352908657,
115.053804345692)) ;
#179165 = CARTESIAN_POINT('Ctrl Pts',(-23.8281400175367,-13.2872351834573,
115.078035374154)) ;
#179166 = CARTESIAN_POINT('Ctrl Pts',(-23.8516354306311,-13.2778702154433,
115.149598613562)) ;
#179167 = CARTESIAN_POINT('Ctrl Pts',(-23.8751308437256,-13.2685052474294,
115.22116185297)) ;
#179168 = CARTESIAN_POINT('Ctrl Pts',(-23.9489346914871,-13.2685053548378,
115.196930824508)) ;
#179169 = CARTESIAN_POINT('Ctrl Pts',(-24.0227385392486,-13.2685054622462,
115.172699796046)) ;
#179170 = CARTESIAN_POINT('Ctrl Pts',(-23.9992431261541,-13.2778704302602,
115.101136556638)) ;
#179171 = CARTESIAN_POINT('Ctrl Pts',(-23.9651195032617,-12.9966579805532,
115.03267001783)) ;
#179172 = CARTESIAN_POINT('Ctrl Pts',(-23.9432377697369,-13.0256699682594,
114.966021786025)) ;
#179173 = CARTESIAN_POINT('Ctrl Pts',(-23.8694339132126,-13.025669868452,
114.990252787797)) ;
#179174 = CARTESIAN_POINT('Ctrl Pts',(-23.7956300566882,-13.0256697686447,
115.014483789568)) ;
#179175 = CARTESIAN_POINT('Ctrl Pts',(-23.817511790213,-12.9966577809386,
115.081132021373)) ;
#179176 = CARTESIAN_POINT('Ctrl Pts',(-23.8393935237377,-12.9676457932324,
115.147780253178)) ;
#179177 = CARTESIAN_POINT('Ctrl Pts',(-23.9131973802621,-12.9676458930398,
115.123549251406)) ;
#179178 = CARTESIAN_POINT('Ctrl Pts',(-23.9870012367865,-12.9676459928471,
115.099318249634)) ;
#179179 = CARTESIAN_POINT('Ctrl Pts',(-23.9651195032617,-12.9966579805532,
115.03267001783)) ;
#179180 = CARTESIAN_POINT('Ctrl Pts',(-23.9083188929157,-12.7449733317735,
114.895243151894)) ;
#179181 = CARTESIAN_POINT('Ctrl Pts',(-23.8896339516894,-12.7916002389954,
114.838331833659)) ;
#179182 = CARTESIAN_POINT('Ctrl Pts',(-23.8158300876213,-12.7916001552318,
114.862562812454)) ;
#179183 = CARTESIAN_POINT('Ctrl Pts',(-23.7420262235532,-12.7916000714681,
114.886793791249)) ;
#179184 = CARTESIAN_POINT('Ctrl Pts',(-23.7607111647796,-12.7449731642463,
114.943705109484)) ;
#179185 = CARTESIAN_POINT('Ctrl Pts',(-23.7793961060059,-12.6983462570244,
115.000616427718)) ;
#179186 = CARTESIAN_POINT('Ctrl Pts',(-23.8531999700739,-12.698346340788,
114.976385448923)) ;
#179187 = CARTESIAN_POINT('Ctrl Pts',(-23.927003834142,-12.6983464245516,
114.952154470128)) ;
#179188 = CARTESIAN_POINT('Ctrl Pts',(-23.9083188929157,-12.7449733317735,
114.895243151894)) ;
#179189 = CARTESIAN_POINT('Ctrl Pts',(-23.8326075291051,-12.5424420519023,
114.700085714252)) ;
#179190 = CARTESIAN_POINT('Ctrl Pts',(-23.81844720302,-12.6032785791417,114.656955643741)) ;
#179191 = CARTESIAN_POINT('Ctrl Pts',(-23.7446433333702,-12.6032785174952,
114.681186605535)) ;
#179192 = CARTESIAN_POINT('Ctrl Pts',(-23.6708394637203,-12.6032784558487,
114.705417567328)) ;
#179193 = CARTESIAN_POINT('Ctrl Pts',(-23.6849997898054,-12.5424419286094,
114.748547637839)) ;
#179194 = CARTESIAN_POINT('Ctrl Pts',(-23.6991601158905,-12.48160540137,114.79167770835)) ;
#179195 = CARTESIAN_POINT('Ctrl Pts',(-23.7729639855403,-12.4816054630165,
114.767446746556)) ;
#179196 = CARTESIAN_POINT('Ctrl Pts',(-23.8467678551901,-12.481605524663,
114.743215784762)) ;
#179197 = CARTESIAN_POINT('Ctrl Pts',(-23.8326075291051,-12.5424420519023,
114.700085714252)) ;
#179198 = CARTESIAN_POINT('Ctrl Pts',(-23.7423558200825,-12.4024494998622,
114.460690641158)) ;
#179199 = CARTESIAN_POINT('Ctrl Pts',(-23.7337409088041,-12.4731509953254,
114.434451009471)) ;
#179200 = CARTESIAN_POINT('Ctrl Pts',(-23.6599370360758,-12.4731509596195,
114.458681961889)) ;
#179201 = CARTESIAN_POINT('Ctrl Pts',(-23.5861331633476,-12.4731509239136,
114.482912914306)) ;
#179202 = CARTESIAN_POINT('Ctrl Pts',(-23.594748074626,-12.4024494284505,
114.509152545993)) ;
#179203 = CARTESIAN_POINT('Ctrl Pts',(-23.6033629859044,-12.3317479329873,
114.535392177679)) ;
#179204 = CARTESIAN_POINT('Ctrl Pts',(-23.6771668586326,-12.3317479686932,
114.511161225262)) ;
#179205 = CARTESIAN_POINT('Ctrl Pts',(-23.7509707313608,-12.331748004399,
114.486930272844)) ;
#179206 = CARTESIAN_POINT('Ctrl Pts',(-23.7423558200825,-12.4024494998622,
114.460690641158)) ;
#179207 = CARTESIAN_POINT('Ctrl Pts',(-23.6437350301605,-12.33540698977,114.195676204108)) ;
#179208 = CARTESIAN_POINT('Ctrl Pts',(-23.6412608759413,-12.4108950254445,
114.188140327696)) ;
#179209 = CARTESIAN_POINT('Ctrl Pts',(-23.5674570025814,-12.4108950163572,
114.212371278189)) ;
#179210 = CARTESIAN_POINT('Ctrl Pts',(-23.4936531292215,-12.4108950072698,
114.236602228683)) ;
#179211 = CARTESIAN_POINT('Ctrl Pts',(-23.4961272834406,-12.3354069715953,
114.244138105095)) ;
#179212 = CARTESIAN_POINT('Ctrl Pts',(-23.4986014376598,-12.2599189359207,
114.251673981507)) ;
#179213 = CARTESIAN_POINT('Ctrl Pts',(-23.5724053110197,-12.2599189450081,
114.227443031014)) ;
#179214 = CARTESIAN_POINT('Ctrl Pts',(-23.6462091843796,-12.2599189540954,
114.20321208052)) ;
#179215 = CARTESIAN_POINT('Ctrl Pts',(-23.6437350301605,-12.33540698977,114.195676204108)) ;
#179216 = CARTESIAN_POINT('Ctrl Pts',(-23.54230497616,-12.3455818235887,113.922252265825)) ;
#179217 = CARTESIAN_POINT('Ctrl Pts',(-23.5461738202571,-12.4204731523851,
113.934036138957)) ;
#179218 = CARTESIAN_POINT('Ctrl Pts',(-23.4723699490057,-12.4204731683141,
113.958267095873)) ;
#179219 = CARTESIAN_POINT('Ctrl Pts',(-23.3985660777543,-12.4204731842432,
113.982498052789)) ;
#179220 = CARTESIAN_POINT('Ctrl Pts',(-23.3946972336572,-12.3455818554468,
113.970714179657)) ;
#179221 = CARTESIAN_POINT('Ctrl Pts',(-23.3908283895601,-12.2706905266504,
113.958930306525)) ;
#179222 = CARTESIAN_POINT('Ctrl Pts',(-23.4646322608115,-12.2706905107213,
113.934699349609)) ;
#179223 = CARTESIAN_POINT('Ctrl Pts',(-23.5384361320628,-12.2706904947923,
113.910468392693)) ;
#179224 = CARTESIAN_POINT('Ctrl Pts',(-23.54230497616,-12.3455818235887,113.922252265825)) ;
#179225 = CARTESIAN_POINT('Ctrl Pts',(-23.4449159493085,-12.433061741337,
113.661165866049)) ;
#179226 = CARTESIAN_POINT('Ctrl Pts',(-23.4548546920134,-12.5019585481824,
113.691437671103)) ;
#179227 = CARTESIAN_POINT('Ctrl Pts',(-23.3810508250872,-12.5019585842902,
113.715668641192)) ;
#179228 = CARTESIAN_POINT('Ctrl Pts',(-23.307246958161,-12.501958620398,113.739899611282)) ;
#179229 = CARTESIAN_POINT('Ctrl Pts',(-23.2973082154561,-12.4330618135526,
113.709627806229)) ;
#179230 = CARTESIAN_POINT('Ctrl Pts',(-23.2873694727513,-12.3641650067072,
113.679356001175)) ;
#179231 = CARTESIAN_POINT('Ctrl Pts',(-23.3611733396774,-12.3641649705994,
113.655125031086)) ;
#179232 = CARTESIAN_POINT('Ctrl Pts',(-23.4349772066036,-12.3641649344917,
113.630894060996)) ;
#179233 = CARTESIAN_POINT('Ctrl Pts',(-23.4449159493085,-12.433061741337,
113.661165866049)) ;
#179234 = CARTESIAN_POINT('Ctrl Pts',(-23.3581859160956,-12.5907670484714,
113.432424558756)) ;
#179235 = CARTESIAN_POINT('Ctrl Pts',(-23.3734620758896,-12.6487569748398,
113.478953275208)) ;
#179236 = CARTESIAN_POINT('Ctrl Pts',(-23.2996582144225,-12.6487570251188,
113.503184261925)) ;
#179237 = CARTESIAN_POINT('Ctrl Pts',(-23.2258543529553,-12.6487570753977,
113.527415248642)) ;
#179238 = CARTESIAN_POINT('Ctrl Pts',(-23.2105781931613,-12.5907671490293,
113.48088653219)) ;
#179239 = CARTESIAN_POINT('Ctrl Pts',(-23.1953020333673,-12.5327772226608,
113.434357815739)) ;
#179240 = CARTESIAN_POINT('Ctrl Pts',(-23.2691058948344,-12.5327771723819,
113.410126829022)) ;
#179241 = CARTESIAN_POINT('Ctrl Pts',(-23.3429097563016,-12.5327771221029,
113.385895842305)) ;
#179242 = CARTESIAN_POINT('Ctrl Pts',(-23.3581859160956,-12.5907670484714,
113.432424558756)) ;
#179243 = CARTESIAN_POINT('Ctrl Pts',(-23.2872506370322,-12.8072730343164,
113.25175834982)) ;
#179244 = CARTESIAN_POINT('Ctrl Pts',(-23.3067702142274,-12.8502341493777,
113.31121183114)) ;
#179245 = CARTESIAN_POINT('Ctrl Pts',(-23.2329663588169,-12.8502342073388,
113.335442836304)) ;
#179246 = CARTESIAN_POINT('Ctrl Pts',(-23.1591625034065,-12.8502342652999,
113.359673841469)) ;
#179247 = CARTESIAN_POINT('Ctrl Pts',(-23.1396429262112,-12.8072731502386,
113.300220360149)) ;
#179248 = CARTESIAN_POINT('Ctrl Pts',(-23.120123349016,-12.7643120351774,
113.240766878829)) ;
#179249 = CARTESIAN_POINT('Ctrl Pts',(-23.1939272044265,-12.7643119772163,
113.216535873664)) ;
#179250 = CARTESIAN_POINT('Ctrl Pts',(-23.267731059837,-12.7643119192552,
113.192304868499)) ;
#179251 = CARTESIAN_POINT('Ctrl Pts',(-23.2872506370322,-12.8072730343164,
113.25175834982)) ;
#179252 = CARTESIAN_POINT('Ctrl Pts',(-23.2361882931638,-13.0681776762317,
113.131728504028)) ;
#179253 = CARTESIAN_POINT('Ctrl Pts',(-23.2585681123116,-13.0929875781858,
113.199893821003)) ;
#179254 = CARTESIAN_POINT('Ctrl Pts',(-23.1847642630524,-13.0929876362341,
113.224124844904)) ;
#179255 = CARTESIAN_POINT('Ctrl Pts',(-23.1109604137933,-13.0929876942824,
113.248355868804)) ;
#179256 = CARTESIAN_POINT('Ctrl Pts',(-23.0885805946455,-13.0681777923284,
113.18019055183)) ;
#179257 = CARTESIAN_POINT('Ctrl Pts',(-23.0662007754978,-13.0433678903743,
113.112025234855)) ;
#179258 = CARTESIAN_POINT('Ctrl Pts',(-23.1400046247569,-13.043367832326,
113.087794210954)) ;
#179259 = CARTESIAN_POINT('Ctrl Pts',(-23.2138084740161,-13.0433677742776,
113.063563187054)) ;
#179260 = CARTESIAN_POINT('Ctrl Pts',(-23.2361882931638,-13.0681776762317,
113.131728504028)) ;
#179261 = CARTESIAN_POINT('Ctrl Pts',(-23.2082374843446,-13.3550287065478,
113.082188386664)) ;
#179262 = CARTESIAN_POINT('Ctrl Pts',(-23.2318663981751,-13.3598480286535,
113.154158244693)) ;
#179263 = CARTESIAN_POINT('Ctrl Pts',(-23.1580625540699,-13.3598480797462,
113.178389284292)) ;
#179264 = CARTESIAN_POINT('Ctrl Pts',(-23.0842587099647,-13.3598481308389,
113.202620323891)) ;
#179265 = CARTESIAN_POINT('Ctrl Pts',(-23.0606297961342,-13.3550288087332,
113.130650465862)) ;
#179266 = CARTESIAN_POINT('Ctrl Pts',(-23.0370008823037,-13.3502094866275,
113.058680607834)) ;
#179267 = CARTESIAN_POINT('Ctrl Pts',(-23.1108047264089,-13.3502094355348,
113.034449568235)) ;
#179268 = CARTESIAN_POINT('Ctrl Pts',(-23.1846085705141,-13.3502093844422,
113.010218528636)) ;
#179269 = CARTESIAN_POINT('Ctrl Pts',(-23.2082374843446,-13.3550287065478,
113.082188386664)) ;
#179270 = CARTESIAN_POINT('Ctrl Pts',(-23.2046137347424,-13.6436167217993,
113.106398539743)) ;
#179271 = CARTESIAN_POINT('Ctrl Pts',(-23.2278019241114,-13.6282936387258,
113.177026022299)) ;
#179272 = CARTESIAN_POINT('Ctrl Pts',(-23.1539980837884,-13.6282936821549,
113.201257073418)) ;
#179273 = CARTESIAN_POINT('Ctrl Pts',(-23.0801942434654,-13.6282937255841,
113.225488124537)) ;
#179274 = CARTESIAN_POINT('Ctrl Pts',(-23.0570060540965,-13.6436168086577,
113.154860641981)) ;
#179275 = CARTESIAN_POINT('Ctrl Pts',(-23.0338178647275,-13.6589398917312,
113.084233159425)) ;
#179276 = CARTESIAN_POINT('Ctrl Pts',(-23.1076217050505,-13.6589398483021,
113.060002108306)) ;
#179277 = CARTESIAN_POINT('Ctrl Pts',(-23.1814255453735,-13.6589398048729,
113.035771057187)) ;
#179278 = CARTESIAN_POINT('Ctrl Pts',(-23.2046137347424,-13.6436167217993,
113.106398539743)) ;
#179279 = CARTESIAN_POINT('Ctrl Pts',(-23.2246473462219,-13.9180811572707,
113.202915786182)) ;
#179280 = CARTESIAN_POINT('Ctrl Pts',(-23.2457373765754,-13.8835710604602,
113.267152615087)) ;
#179281 = CARTESIAN_POINT('Ctrl Pts',(-23.1719335384956,-13.8835710916854,
113.291383673039)) ;
#179282 = CARTESIAN_POINT('Ctrl Pts',(-23.0981297004159,-13.8835711229105,
113.31561473099)) ;
#179283 = CARTESIAN_POINT('Ctrl Pts',(-23.0770396700624,-13.918081219721,
113.251377902085)) ;
#179284 = CARTESIAN_POINT('Ctrl Pts',(-23.055949639709,-13.9525913165315,
113.187141073179)) ;
#179285 = CARTESIAN_POINT('Ctrl Pts',(-23.1297534777888,-13.9525912853064,
113.162910015228)) ;
#179286 = CARTESIAN_POINT('Ctrl Pts',(-23.2035573158685,-13.9525912540812,
113.138678957277)) ;
#179287 = CARTESIAN_POINT('Ctrl Pts',(-23.2246473462219,-13.9180811572707,
113.202915786182)) ;
#179288 = CARTESIAN_POINT('Ctrl Pts',(-23.2663198478807,-14.156549136634,
113.365316344901)) ;
#179289 = CARTESIAN_POINT('Ctrl Pts',(-23.2837980929174,-14.1053360637856,
113.418552258655)) ;
#179290 = CARTESIAN_POINT('Ctrl Pts',(-23.2099942554152,-14.1053360831036,
113.442783318366)) ;
#179291 = CARTESIAN_POINT('Ctrl Pts',(-23.1361904179131,-14.1053361024216,
113.467014378076)) ;
#179292 = CARTESIAN_POINT('Ctrl Pts',(-23.1187121728764,-14.1565491752701,
113.413778464322)) ;
#179293 = CARTESIAN_POINT('Ctrl Pts',(-23.1012339278397,-14.2077622481185,
113.360542550568)) ;
#179294 = CARTESIAN_POINT('Ctrl Pts',(-23.1750377653419,-14.2077622288005,
113.336311490857)) ;
#179295 = CARTESIAN_POINT('Ctrl Pts',(-23.248841602844,-14.2077622094825,
113.312080431146)) ;
#179296 = CARTESIAN_POINT('Ctrl Pts',(-23.2663198478807,-14.156549136634,
113.365316344901)) ;
#179297 = CARTESIAN_POINT('Ctrl Pts',(-23.3260277991125,-14.3423727651068,
113.58274099428)) ;
#179298 = CARTESIAN_POINT('Ctrl Pts',(-23.3386275164003,-14.2781068691163,
113.621117699827)) ;
#179299 = CARTESIAN_POINT('Ctrl Pts',(-23.2648236779677,-14.2781068782219,
113.645348756703)) ;
#179300 = CARTESIAN_POINT('Ctrl Pts',(-23.191019839535,-14.2781068873274,
113.66957981358)) ;
#179301 = CARTESIAN_POINT('Ctrl Pts',(-23.1784201222473,-14.342372783318,
113.631203108033)) ;
#179302 = CARTESIAN_POINT('Ctrl Pts',(-23.1658204049595,-14.4066386793085,
113.592826402486)) ;
#179303 = CARTESIAN_POINT('Ctrl Pts',(-23.2396242433921,-14.406638670203,
113.568595345609)) ;
#179304 = CARTESIAN_POINT('Ctrl Pts',(-23.3134280818248,-14.4066386610974,
113.544364288733)) ;
#179305 = CARTESIAN_POINT('Ctrl Pts',(-23.3260277991125,-14.3423727651068,
113.58274099428)) ;
#179306 = CARTESIAN_POINT('Ctrl Pts',(-23.3982430302962,-14.4613427108393,
113.838084052962)) ;
#179307 = CARTESIAN_POINT('Ctrl Pts',(-23.4050870415736,-14.3886728717829,
113.858929806808)) ;
#179308 = CARTESIAN_POINT('Ctrl Pts',(-23.3312832017508,-14.3886728745372,
113.88316085945)) ;
#179309 = CARTESIAN_POINT('Ctrl Pts',(-23.2574793619279,-14.3886728772916,
113.907391912092)) ;
#179310 = CARTESIAN_POINT('Ctrl Pts',(-23.2506353506505,-14.461342716348,
113.886546158247)) ;
#179311 = CARTESIAN_POINT('Ctrl Pts',(-23.243791339373,-14.5340125554044,
113.865700404401)) ;
#179312 = CARTESIAN_POINT('Ctrl Pts',(-23.3175951791959,-14.5340125526501,
113.841469351759)) ;
#179313 = CARTESIAN_POINT('Ctrl Pts',(-23.3913990190187,-14.5340125498957,
113.817238299117)) ;
#179314 = CARTESIAN_POINT('Ctrl Pts',(-23.3982430302962,-14.4613427108393,
113.838084052962)) ;
#179315 = CARTESIAN_POINT('Ctrl Pts',(-23.4778308247352,-14.5057889124528,
114.116110858595)) ;
#179316 = CARTESIAN_POINT('Ctrl Pts',(-23.4783907365172,-14.4299056340327,
114.117816259447)) ;
#179317 = CARTESIAN_POINT('Ctrl Pts',(-23.4045868946325,-14.4299056336396,
114.142047305809)) ;
#179318 = CARTESIAN_POINT('Ctrl Pts',(-23.3307830527477,-14.4299056332465,
114.166278352171)) ;
#179319 = CARTESIAN_POINT('Ctrl Pts',(-23.3302231409656,-14.5057889116665,
114.164572951319)) ;
#179320 = CARTESIAN_POINT('Ctrl Pts',(-23.3296632291836,-14.5816721900866,
114.162867550466)) ;
#179321 = CARTESIAN_POINT('Ctrl Pts',(-23.4034670710684,-14.5816721904797,
114.138636504104)) ;
#179322 = CARTESIAN_POINT('Ctrl Pts',(-23.4772709129532,-14.5816721908728,
114.114405457742)) ;
#179323 = CARTESIAN_POINT('Ctrl Pts',(-23.4778308247352,-14.5057889124528,
114.116110858595)) ;
#179324 = CARTESIAN_POINT('Ctrl Pts',(-23.5571252249388,-14.4724226584541,
114.392900262027)) ;
#179325 = CARTESIAN_POINT('Ctrl Pts',(-23.5514192768126,-14.3987559090156,
114.375520864663)) ;
#179326 = CARTESIAN_POINT('Ctrl Pts',(-23.4776154337327,-14.3987559084173,
114.399751907385)) ;
#179327 = CARTESIAN_POINT('Ctrl Pts',(-23.4038115906528,-14.3987559078189,
114.423982950107)) ;
#179328 = CARTESIAN_POINT('Ctrl Pts',(-23.4095175387789,-14.4724226572574,
114.44136234747)) ;
#179329 = CARTESIAN_POINT('Ctrl Pts',(-23.4152234869051,-14.5460894066958,
114.458741744834)) ;
#179330 = CARTESIAN_POINT('Ctrl Pts',(-23.489027329985,-14.5460894072942,
114.434510702113)) ;
#179331 = CARTESIAN_POINT('Ctrl Pts',(-23.5628311730649,-14.5460894078926,
114.410279659391)) ;
#179332 = CARTESIAN_POINT('Ctrl Pts',(-23.5571252249388,-14.4724226584541,
114.392900262027)) ;
#179333 = CARTESIAN_POINT('Ctrl Pts',(-23.6311473330998,-14.3630839653471,
114.653969620511)) ;
#179334 = CARTESIAN_POINT('Ctrl Pts',(-23.6195269569882,-14.2969416918189,
114.618575829864)) ;
#179335 = CARTESIAN_POINT('Ctrl Pts',(-23.5457231128652,-14.2969416928651,
114.642806869409)) ;
#179336 = CARTESIAN_POINT('Ctrl Pts',(-23.4719192687422,-14.2969416939113,
114.667037908954)) ;
#179337 = CARTESIAN_POINT('Ctrl Pts',(-23.4835396448539,-14.3630839674395,
114.702431699601)) ;
#179338 = CARTESIAN_POINT('Ctrl Pts',(-23.4951600209655,-14.4292262409677,
114.737825490247)) ;
#179339 = CARTESIAN_POINT('Ctrl Pts',(-23.5689638650885,-14.4292262399216,
114.713594450703)) ;
#179340 = CARTESIAN_POINT('Ctrl Pts',(-23.6427677092115,-14.4292262388754,
114.689363411158)) ;
#179341 = CARTESIAN_POINT('Ctrl Pts',(-23.6311473330998,-14.3630839653471,
114.653969620511)) ;
#179342 = CARTESIAN_POINT('Ctrl Pts',(-23.6926670750486,-14.1865023299291,
114.87674421223)) ;
#179343 = CARTESIAN_POINT('Ctrl Pts',(-23.6760010931989,-14.132592518795,
114.825982320627)) ;
#179344 = CARTESIAN_POINT('Ctrl Pts',(-23.6021972490565,-14.1325925211688,
114.850213360112)) ;
#179345 = CARTESIAN_POINT('Ctrl Pts',(-23.528393404914,-14.1325925235426,
114.874444399598)) ;
#179346 = CARTESIAN_POINT('Ctrl Pts',(-23.5450593867637,-14.1865023346767,
114.925206291201)) ;
#179347 = CARTESIAN_POINT('Ctrl Pts',(-23.5617253686134,-14.2404121458108,
114.975968182805)) ;
#179348 = CARTESIAN_POINT('Ctrl Pts',(-23.6355292127559,-14.240412143437,
114.95173714332)) ;
#179349 = CARTESIAN_POINT('Ctrl Pts',(-23.7093330568983,-14.2404121410632,
114.927506103834)) ;
#179350 = CARTESIAN_POINT('Ctrl Pts',(-23.6926670750486,-14.1865023299291,
114.87674421223)) ;
#179351 = CARTESIAN_POINT('Ctrl Pts',(-23.737109657086,-13.9552367476643,
115.047514669265)) ;
#179352 = CARTESIAN_POINT('Ctrl Pts',(-23.7165830285528,-13.91739633188,114.98499387076)) ;
#179353 = CARTESIAN_POINT('Ctrl Pts',(-23.6427791848163,-13.917396334111,
115.009224911482)) ;
#179354 = CARTESIAN_POINT('Ctrl Pts',(-23.5689753410797,-13.9173963363419,
115.033455952203)) ;
#179355 = CARTESIAN_POINT('Ctrl Pts',(-23.5895019696129,-13.9552367521262,
115.095976750709)) ;
#179356 = CARTESIAN_POINT('Ctrl Pts',(-23.6100285981462,-13.9930771679105,
115.158497549214)) ;
#179357 = CARTESIAN_POINT('Ctrl Pts',(-23.6838324418827,-13.9930771656796,
115.134266508492)) ;
#179358 = CARTESIAN_POINT('Ctrl Pts',(-23.7576362856192,-13.9930771634486,
115.110035467771)) ;
#179359 = CARTESIAN_POINT('Ctrl Pts',(-23.737109657086,-13.9552367476643,
115.047514669265)) ;
#179360 = CARTESIAN_POINT('Ctrl Pts',(-23.7605010634612,-13.6844063432408,
115.1543055001)) ;
#179361 = CARTESIAN_POINT('Ctrl Pts',(-23.7375752646493,-13.6654217630373,
115.084477215966)) ;
#179362 = CARTESIAN_POINT('Ctrl Pts',(-23.6637714214189,-13.6654217622708,
115.10870825823)) ;
#179363 = CARTESIAN_POINT('Ctrl Pts',(-23.5899675781886,-13.6654217615044,
115.132939300493)) ;
#179364 = CARTESIAN_POINT('Ctrl Pts',(-23.6128933770005,-13.6844063417079,
115.202767584627)) ;
#179365 = CARTESIAN_POINT('Ctrl Pts',(-23.6358191758124,-13.7033909219114,
115.272595868762)) ;
#179366 = CARTESIAN_POINT('Ctrl Pts',(-23.7096230190428,-13.7033909226779,
115.248364826498)) ;
#179367 = CARTESIAN_POINT('Ctrl Pts',(-23.7834268622731,-13.7033909234443,
115.224133784235)) ;
#179368 = CARTESIAN_POINT('Ctrl Pts',(-23.7605010634612,-13.6844063432408,
115.1543055001)) ;
#179369 = CARTESIAN_POINT('Ctrl Pts',(-23.760236922336,-13.395616216205,115.188901213406)) ;
#179370 = CARTESIAN_POINT('Ctrl Pts',(-23.7365635501868,-13.3967687826649,
115.116795941421)) ;
#179371 = CARTESIAN_POINT('Ctrl Pts',(-23.6627597068722,-13.3967687773501,
115.141026983428)) ;
#179372 = CARTESIAN_POINT('Ctrl Pts',(-23.5889558635576,-13.3967687720353,
115.165258025435)) ;
#179373 = CARTESIAN_POINT('Ctrl Pts',(-23.6126292357068,-13.3956162055754,
115.23736329742)) ;
#179374 = CARTESIAN_POINT('Ctrl Pts',(-23.6363026078559,-13.3944636391155,
115.309468569405)) ;
#179375 = CARTESIAN_POINT('Ctrl Pts',(-23.7101064511705,-13.3944636444303,
115.285237527398)) ;
#179376 = CARTESIAN_POINT('Ctrl Pts',(-23.7839102944851,-13.3944636497451,
115.261006485391)) ;
#179377 = CARTESIAN_POINT('Ctrl Pts',(-23.760236922336,-13.395616216205,115.188901213406)) ;
#179378 = CARTESIAN_POINT('Ctrl Pts',(-23.7358042656124,-13.1080920804484,
115.149918807693)) ;
#179379 = CARTESIAN_POINT('Ctrl Pts',(-23.7130691272017,-13.1293224287734,
115.080671244182)) ;
#179380 = CARTESIAN_POINT('Ctrl Pts',(-23.6392652830181,-13.1293224180304,
115.104902283542)) ;
#179381 = CARTESIAN_POINT('Ctrl Pts',(-23.5654614388346,-13.1293224072874,
115.129133322903)) ;
#179382 = CARTESIAN_POINT('Ctrl Pts',(-23.5881965772453,-13.1080920589624,
115.198380886413)) ;
#179383 = CARTESIAN_POINT('Ctrl Pts',(-23.610931715656,-13.0868617106374,
115.267628449924)) ;
#179384 = CARTESIAN_POINT('Ctrl Pts',(-23.6847355598396,-13.0868617213805,
115.243397410564)) ;
#179385 = CARTESIAN_POINT('Ctrl Pts',(-23.7585394040231,-13.0868617321235,
115.219166371203)) ;
#179386 = CARTESIAN_POINT('Ctrl Pts',(-23.7358042656124,-13.1080920804484,
115.149918807693)) ;
#179387 = CARTESIAN_POINT('Ctrl Pts',(-23.6876957397051,-12.8414911099526,
115.039017564153)) ;
#179388 = CARTESIAN_POINT('Ctrl Pts',(-23.6675492663887,-12.8813675737048,
114.977654656676)) ;
#179389 = CARTESIAN_POINT('Ctrl Pts',(-23.5937454199294,-12.8813675568765,
115.001885689105)) ;
#179390 = CARTESIAN_POINT('Ctrl Pts',(-23.5199415734701,-12.8813675400482,
115.026116721534)) ;
#179391 = CARTESIAN_POINT('Ctrl Pts',(-23.5400880467865,-12.8414910762961,
115.08747962901)) ;
#179392 = CARTESIAN_POINT('Ctrl Pts',(-23.5602345201028,-12.8016146125439,
115.148842536487)) ;
#179393 = CARTESIAN_POINT('Ctrl Pts',(-23.6340383665621,-12.8016146293722,
115.124611504058)) ;
#179394 = CARTESIAN_POINT('Ctrl Pts',(-23.7078422130214,-12.8016146462005,
115.10038047163)) ;
#179395 = CARTESIAN_POINT('Ctrl Pts',(-23.6876957397051,-12.8414911099526,
115.039017564153)) ;
#179396 = CARTESIAN_POINT('Ctrl Pts',(-23.6196197911873,-12.6185827250958,
114.866926329754)) ;
#179397 = CARTESIAN_POINT('Ctrl Pts',(-23.6034678707082,-12.6740802978787,
114.817730185585)) ;
#179398 = CARTESIAN_POINT('Ctrl Pts',(-23.5296640215903,-12.6740802801009,
114.841961209916)) ;
#179399 = CARTESIAN_POINT('Ctrl Pts',(-23.4558601724725,-12.674080262323,
114.866192234247)) ;
#179400 = CARTESIAN_POINT('Ctrl Pts',(-23.4720120929516,-12.6185826895401,
114.915388378416)) ;
#179401 = CARTESIAN_POINT('Ctrl Pts',(-23.4881640134308,-12.5630851167572,
114.964584522586)) ;
#179402 = CARTESIAN_POINT('Ctrl Pts',(-23.5619678625486,-12.563085134535,
114.940353498254)) ;
#179403 = CARTESIAN_POINT('Ctrl Pts',(-23.6357717116664,-12.5630851523128,
114.916122473923)) ;
#179404 = CARTESIAN_POINT('Ctrl Pts',(-23.6196197911873,-12.6185827250958,
114.866926329754)) ;
#179405 = CARTESIAN_POINT('Ctrl Pts',(-23.5344644232555,-12.4509854490646,
114.643132785995)) ;
#179406 = CARTESIAN_POINT('Ctrl Pts',(-23.5234985411404,-12.518265407944,
114.609732477738)) ;
#179407 = CARTESIAN_POINT('Ctrl Pts',(-23.4496946881903,-12.5182653912533,
114.633963490396)) ;
#179408 = CARTESIAN_POINT('Ctrl Pts',(-23.3758908352401,-12.5182653745627,
114.658194503055)) ;
#179409 = CARTESIAN_POINT('Ctrl Pts',(-23.3868567173552,-12.4509854156833,
114.691594811312)) ;
#179410 = CARTESIAN_POINT('Ctrl Pts',(-23.3978225994702,-12.383705456804,
114.72499511957)) ;
#179411 = CARTESIAN_POINT('Ctrl Pts',(-23.4716264524203,-12.3837054734946,
114.700764106911)) ;
#179412 = CARTESIAN_POINT('Ctrl Pts',(-23.5454303053705,-12.3837054901852,
114.676533094252)) ;
#179413 = CARTESIAN_POINT('Ctrl Pts',(-23.5344644232555,-12.4509854490646,
114.643132785995)) ;
#179414 = CARTESIAN_POINT('Ctrl Pts',(-23.4384531446303,-12.3534810644787,
114.386130027561)) ;
#179415 = CARTESIAN_POINT('Ctrl Pts',(-23.4334417543044,-12.427665920119,
114.370866140378)) ;
#179416 = CARTESIAN_POINT('Ctrl Pts',(-23.3596378977513,-12.4276659104835,
114.395097142063)) ;
#179417 = CARTESIAN_POINT('Ctrl Pts',(-23.2858340411983,-12.4276659008479,
114.419328143747)) ;
#179418 = CARTESIAN_POINT('Ctrl Pts',(-23.2908454315242,-12.3534810452076,
114.43459203093)) ;
#179419 = CARTESIAN_POINT('Ctrl Pts',(-23.2958568218501,-12.2792961895673,
114.449855918113)) ;
#179420 = CARTESIAN_POINT('Ctrl Pts',(-23.3696606784032,-12.2792961992029,
114.425624916429)) ;
#179421 = CARTESIAN_POINT('Ctrl Pts',(-23.4434645349562,-12.2792962088384,
114.401393914744)) ;
#179422 = CARTESIAN_POINT('Ctrl Pts',(-23.4384531446303,-12.3534810644787,
114.386130027561)) ;
#179423 = CARTESIAN_POINT('Ctrl Pts',(-23.3373005505562,-12.3320089256095,
114.113522831925)) ;
#179424 = CARTESIAN_POINT('Ctrl Pts',(-23.3386099896682,-12.407800207037,
114.117511171175)) ;
#179425 = CARTESIAN_POINT('Ctrl Pts',(-23.2648061300108,-12.407800209429,
114.141742163405)) ;
#179426 = CARTESIAN_POINT('Ctrl Pts',(-23.1910022703534,-12.4078002118209,
114.165973155634)) ;
#179427 = CARTESIAN_POINT('Ctrl Pts',(-23.1896928312415,-12.3320089303934,
114.161984816384)) ;
#179428 = CARTESIAN_POINT('Ctrl Pts',(-23.1883833921295,-12.2562176489658,
114.157996477134)) ;
#179429 = CARTESIAN_POINT('Ctrl Pts',(-23.2621872517869,-12.2562176465738,
114.133765484905)) ;
#179430 = CARTESIAN_POINT('Ctrl Pts',(-23.3359911114443,-12.2562176441819,
114.109534492675)) ;
#179431 = CARTESIAN_POINT('Ctrl Pts',(-23.3373005505562,-12.3320089256095,
114.113522831925)) ;
#179432 = CARTESIAN_POINT('Ctrl Pts',(-23.2376722572993,-12.3884256006082,
113.845536510079)) ;
#179433 = CARTESIAN_POINT('Ctrl Pts',(-23.2452056301701,-12.4603875127443,
113.868481947164)) ;
#179434 = CARTESIAN_POINT('Ctrl Pts',(-23.1714017687528,-12.4603875316984,
113.892712934033)) ;
#179435 = CARTESIAN_POINT('Ctrl Pts',(-23.0975979073355,-12.4603875506525,
113.916943920902)) ;
#179436 = CARTESIAN_POINT('Ctrl Pts',(-23.0900645344648,-12.3884256385165,
113.893998483817)) ;
#179437 = CARTESIAN_POINT('Ctrl Pts',(-23.0825311615941,-12.3164637263805,
113.871053046732)) ;
#179438 = CARTESIAN_POINT('Ctrl Pts',(-23.1563350230114,-12.3164637074263,
113.846822059863)) ;
#179439 = CARTESIAN_POINT('Ctrl Pts',(-23.2301388844286,-12.3164636884722,
113.822591072994)) ;
#179440 = CARTESIAN_POINT('Ctrl Pts',(-23.2376722572993,-12.3884256006082,
113.845536510079)) ;
#179441 = CARTESIAN_POINT('Ctrl Pts',(-23.1459449956219,-12.5185566369419,
113.601605269859)) ;
#179442 = CARTESIAN_POINT('Ctrl Pts',(-23.1591598321752,-12.5815371501028,
113.641855528462)) ;
#179443 = CARTESIAN_POINT('Ctrl Pts',(-23.0853559708827,-12.5815371883386,
113.666086515711)) ;
#179444 = CARTESIAN_POINT('Ctrl Pts',(-23.0115521095902,-12.5815372265744,
113.69031750296)) ;
#179445 = CARTESIAN_POINT('Ctrl Pts',(-22.9983372730369,-12.5185567134136,
113.650067244357)) ;
#179446 = CARTESIAN_POINT('Ctrl Pts',(-22.9851224364836,-12.4555762002527,
113.609816985754)) ;
#179447 = CARTESIAN_POINT('Ctrl Pts',(-23.0589262977762,-12.4555761620169,
113.585585998505)) ;
#179448 = CARTESIAN_POINT('Ctrl Pts',(-23.1327301590687,-12.4555761237811,
113.561355011256)) ;
#179449 = CARTESIAN_POINT('Ctrl Pts',(-23.1459449956219,-12.5185566369419,
113.601605269859)) ;
#179450 = CARTESIAN_POINT('Ctrl Pts',(-23.0678884204578,-12.7128146761132,
113.399287149443)) ;
#179451 = CARTESIAN_POINT('Ctrl Pts',(-23.0858389718743,-12.7623237651114,
113.453961631268)) ;
#179452 = CARTESIAN_POINT('Ctrl Pts',(-23.0120351128278,-12.7623238229043,
113.478192625358)) ;
#179453 = CARTESIAN_POINT('Ctrl Pts',(-22.9382312537813,-12.7623238806971,
113.502423619448)) ;
#179454 = CARTESIAN_POINT('Ctrl Pts',(-22.9202807023649,-12.7128147916989,
113.447749137622)) ;
#179455 = CARTESIAN_POINT('Ctrl Pts',(-22.9023301509484,-12.6633057027007,
113.393074655797)) ;
#179456 = CARTESIAN_POINT('Ctrl Pts',(-22.9761340099949,-12.6633056449079,
113.368843661707)) ;
#179457 = CARTESIAN_POINT('Ctrl Pts',(-23.0499378690414,-12.663305587115,
113.344612667617)) ;
#179458 = CARTESIAN_POINT('Ctrl Pts',(-23.0678884204578,-12.7128146761132,
113.399287149443)) ;
#179459 = CARTESIAN_POINT('Ctrl Pts',(-23.0080726213499,-12.9591843124397,
113.25274040277)) ;
#179460 = CARTESIAN_POINT('Ctrl Pts',(-23.0294880013055,-12.9915649142031,
113.317968193112)) ;
#179461 = CARTESIAN_POINT('Ctrl Pts',(-22.9556841465484,-12.9915649910661,
113.342199200267)) ;
#179462 = CARTESIAN_POINT('Ctrl Pts',(-22.8818802917913,-12.9915650679292,
113.366430207422)) ;
#179463 = CARTESIAN_POINT('Ctrl Pts',(-22.8604649118357,-12.9591844661657,
113.30120241708)) ;
#179464 = CARTESIAN_POINT('Ctrl Pts',(-22.8390495318801,-12.9268038644023,
113.235974626737)) ;
#179465 = CARTESIAN_POINT('Ctrl Pts',(-22.9128533866372,-12.9268037875393,
113.211743619582)) ;
#179466 = CARTESIAN_POINT('Ctrl Pts',(-22.9866572413943,-12.9268037106763,
113.187512612428)) ;
#179467 = CARTESIAN_POINT('Ctrl Pts',(-23.0080726213499,-12.9591843124397,
113.25274040277)) ;
#179468 = CARTESIAN_POINT('Ctrl Pts',(-22.9707781839292,-13.2359003760254,
113.174438606138)) ;
#179469 = CARTESIAN_POINT('Ctrl Pts',(-22.9940981173892,-13.2490083473187,
113.245467359058)) ;
#179470 = CARTESIAN_POINT('Ctrl Pts',(-22.9202942691491,-13.24900843612,113.269698386062)) ;
#179471 = CARTESIAN_POINT('Ctrl Pts',(-22.8464904209091,-13.2490085249213,
113.293929413067)) ;
#179472 = CARTESIAN_POINT('Ctrl Pts',(-22.8231704874491,-13.235900553628,
113.222900660147)) ;
#179473 = CARTESIAN_POINT('Ctrl Pts',(-22.7998505539891,-13.2227925823347,
113.151871907227)) ;
#179474 = CARTESIAN_POINT('Ctrl Pts',(-22.8736544022292,-13.2227924935334,
113.127640880223)) ;
#179475 = CARTESIAN_POINT('Ctrl Pts',(-22.9474582504692,-13.2227924047321,
113.103409853218)) ;
#179476 = CARTESIAN_POINT('Ctrl Pts',(-22.9707781839292,-13.2359003760254,
113.174438606138)) ;
#179477 = CARTESIAN_POINT('Ctrl Pts',(-22.9571487392571,-13.5269168879405,
113.168395654949)) ;
#179478 = CARTESIAN_POINT('Ctrl Pts',(-22.9807202921007,-13.5197262961672,
113.240190799802)) ;
#179479 = CARTESIAN_POINT('Ctrl Pts',(-22.9069164515481,-13.5197263915446,
113.264421850221)) ;
#179480 = CARTESIAN_POINT('Ctrl Pts',(-22.8331126109954,-13.5197264869221,
113.28865290064)) ;
#179481 = CARTESIAN_POINT('Ctrl Pts',(-22.8095410581518,-13.5269170786954,
113.216857755787)) ;
#179482 = CARTESIAN_POINT('Ctrl Pts',(-22.7859695053082,-13.5341076704686,
113.145062610933)) ;
#179483 = CARTESIAN_POINT('Ctrl Pts',(-22.8597733458609,-13.5341075750912,
113.120831560514)) ;
#179484 = CARTESIAN_POINT('Ctrl Pts',(-22.9335771864135,-13.5341074797137,
113.096600510095)) ;
#179485 = CARTESIAN_POINT('Ctrl Pts',(-22.9571487392571,-13.5269168879405,
113.168395654949)) ;
#179486 = CARTESIAN_POINT('Ctrl Pts',(-22.9677330810903,-13.8100818853549,
113.236088284649)) ;
#179487 = CARTESIAN_POINT('Ctrl Pts',(-22.9898665157146,-13.7831112951298,
113.303503153356)) ;
#179488 = CARTESIAN_POINT('Ctrl Pts',(-22.9160626835003,-13.7831113889682,
113.327734229173)) ;
#179489 = CARTESIAN_POINT('Ctrl Pts',(-22.8422588512859,-13.7831114828066,
113.351965304989)) ;
#179490 = CARTESIAN_POINT('Ctrl Pts',(-22.8201254166616,-13.8100820730318,
113.284550436281)) ;
#179491 = CARTESIAN_POINT('Ctrl Pts',(-22.7979919820373,-13.837052663257,
113.217135567573)) ;
#179492 = CARTESIAN_POINT('Ctrl Pts',(-22.8717958142516,-13.8370525694185,
113.192904491757)) ;
#179493 = CARTESIAN_POINT('Ctrl Pts',(-22.945599646466,-13.8370524755801,
113.168673415941)) ;
#179494 = CARTESIAN_POINT('Ctrl Pts',(-22.9677330810903,-13.8100818853549,
113.236088284649)) ;
#179495 = CARTESIAN_POINT('Ctrl Pts',(-23.0011086677166,-14.0658493622321,
113.373303697314)) ;
#179496 = CARTESIAN_POINT('Ctrl Pts',(-23.0202087390422,-14.0209825335161,
113.431479430768)) ;
#179497 = CARTESIAN_POINT('Ctrl Pts',(-22.9464049149718,-14.0209826175788,
113.455710531389)) ;
#179498 = CARTESIAN_POINT('Ctrl Pts',(-22.8726010909013,-14.0209827016415,
113.479941632011)) ;
#179499 = CARTESIAN_POINT('Ctrl Pts',(-22.8535010195757,-14.0658495303575,
113.421765898557)) ;
#179500 = CARTESIAN_POINT('Ctrl Pts',(-22.8344009482501,-14.1107163590735,
113.363590165103)) ;
#179501 = CARTESIAN_POINT('Ctrl Pts',(-22.9082047723206,-14.1107162750108,
113.339359064481)) ;
#179502 = CARTESIAN_POINT('Ctrl Pts',(-22.982008596391,-14.1107161909481,
113.31512796386)) ;
#179503 = CARTESIAN_POINT('Ctrl Pts',(-23.0011086677166,-14.0658493622321,
113.373303697314)) ;
#179504 = CARTESIAN_POINT('Ctrl Pts',(-23.0539725203832,-14.2744004374724,
113.569778136137)) ;
#179505 = CARTESIAN_POINT('Ctrl Pts',(-23.0686762202321,-14.2149073780421,
113.614563231378)) ;
#179506 = CARTESIAN_POINT('Ctrl Pts',(-22.9948724030358,-14.2149074440193,
113.638794352937)) ;
#179507 = CARTESIAN_POINT('Ctrl Pts',(-22.9210685858396,-14.2149075099964,
113.663025474496)) ;
#179508 = CARTESIAN_POINT('Ctrl Pts',(-22.9063648859907,-14.2744005694268,
113.618240379255)) ;
#179509 = CARTESIAN_POINT('Ctrl Pts',(-22.8916611861419,-14.3338936288571,
113.573455284013)) ;
#179510 = CARTESIAN_POINT('Ctrl Pts',(-22.9654650033381,-14.3338935628799,
113.549224162454)) ;
#179511 = CARTESIAN_POINT('Ctrl Pts',(-23.0392688205343,-14.3338934969028,
113.524993040895)) ;
#179512 = CARTESIAN_POINT('Ctrl Pts',(-23.0539725203832,-14.2744004374724,
113.569778136137)) ;
#179513 = CARTESIAN_POINT('Ctrl Pts',(-23.1216893204055,-14.4215076088756,
113.811439149396)) ;
#179514 = CARTESIAN_POINT('Ctrl Pts',(-23.1309543238125,-14.3516564443396,
113.839658852781)) ;
#179515 = CARTESIAN_POINT('Ctrl Pts',(-23.0571505115092,-14.3516564861261,
113.863889989243)) ;
#179516 = CARTESIAN_POINT('Ctrl Pts',(-22.9833466992058,-14.3516565279127,
113.888121125705)) ;
#179517 = CARTESIAN_POINT('Ctrl Pts',(-22.9740816957989,-14.4215076924487,
113.85990142232)) ;
#179518 = CARTESIAN_POINT('Ctrl Pts',(-22.9648166923919,-14.4913588569847,
113.831681718935)) ;
#179519 = CARTESIAN_POINT('Ctrl Pts',(-23.0386205046952,-14.4913588151982,
113.807450582473)) ;
#179520 = CARTESIAN_POINT('Ctrl Pts',(-23.1124243169985,-14.4913587734116,
113.783219446011)) ;
#179521 = CARTESIAN_POINT('Ctrl Pts',(-23.1216893204055,-14.4215076088756,
113.811439149396)) ;
#179522 = CARTESIAN_POINT('Ctrl Pts',(-23.1988440710271,-14.4970287487176,
114.081882466236)) ;
#179523 = CARTESIAN_POINT('Ctrl Pts',(-23.2020027620207,-14.421801684016,
114.091503327255)) ;
#179524 = CARTESIAN_POINT('Ctrl Pts',(-23.1281989521545,-14.42180169783,114.11573447114)) ;
#179525 = CARTESIAN_POINT('Ctrl Pts',(-23.0543951422883,-14.421801711644,
114.139965615025)) ;
#179526 = CARTESIAN_POINT('Ctrl Pts',(-23.0512364512947,-14.4970287763456,
114.130344754007)) ;
#179527 = CARTESIAN_POINT('Ctrl Pts',(-23.0480777603011,-14.5722558410471,
114.120723892988)) ;
#179528 = CARTESIAN_POINT('Ctrl Pts',(-23.1218815701673,-14.5722558272332,
114.096492749103)) ;
#179529 = CARTESIAN_POINT('Ctrl Pts',(-23.1956853800335,-14.5722558134192,
114.072261605218)) ;
#179530 = CARTESIAN_POINT('Ctrl Pts',(-23.1988440710271,-14.4970287487176,
114.081882466236)) ;
#179531 = CARTESIAN_POINT('Ctrl Pts',(-23.2792349709217,-14.495364180026,
114.362233916425)) ;
#179532 = CARTESIAN_POINT('Ctrl Pts',(-23.2760513537556,-14.420141562785,
114.352537130133)) ;
#179533 = CARTESIAN_POINT('Ctrl Pts',(-23.202247543564,-14.4201415475385,
114.376768273027)) ;
#179534 = CARTESIAN_POINT('Ctrl Pts',(-23.1284437333723,-14.420141532292,
114.400999415921)) ;
#179535 = CARTESIAN_POINT('Ctrl Pts',(-23.1316273505383,-14.495364149533,
114.410696202213)) ;
#179536 = CARTESIAN_POINT('Ctrl Pts',(-23.1348109677044,-14.570586766774,
114.420392988505)) ;
#179537 = CARTESIAN_POINT('Ctrl Pts',(-23.2086147778961,-14.5705867820204,
114.396161845611)) ;
#179538 = CARTESIAN_POINT('Ctrl Pts',(-23.2824185880877,-14.5705867972669,
114.371930702717)) ;
#179539 = CARTESIAN_POINT('Ctrl Pts',(-23.2792349709217,-14.495364180026,
114.362233916425)) ;
#179540 = CARTESIAN_POINT('Ctrl Pts',(-23.3563637359517,-14.4159600881982,
114.632728072821)) ;
#179541 = CARTESIAN_POINT('Ctrl Pts',(-23.3470544555899,-14.3461687677575,
114.604373504854)) ;
#179542 = CARTESIAN_POINT('Ctrl Pts',(-23.2732506422362,-14.346168725633,
114.628604638116)) ;
#179543 = CARTESIAN_POINT('Ctrl Pts',(-23.1994468288825,-14.3461686835086,
114.652835771379)) ;
#179544 = CARTESIAN_POINT('Ctrl Pts',(-23.2087561092442,-14.4159600039494,
114.681190339346)) ;
#179545 = CARTESIAN_POINT('Ctrl Pts',(-23.2180653896059,-14.4857513243901,
114.709544907314)) ;
#179546 = CARTESIAN_POINT('Ctrl Pts',(-23.2918692029597,-14.4857513665145,
114.685313774051)) ;
#179547 = CARTESIAN_POINT('Ctrl Pts',(-23.3656730163134,-14.485751408639,
114.661082640788)) ;
#179548 = CARTESIAN_POINT('Ctrl Pts',(-23.3563637359517,-14.4159600881982,
114.632728072821)) ;
#179549 = CARTESIAN_POINT('Ctrl Pts',(-23.4233024681412,-14.2660479877099,
114.871922390373)) ;
#179550 = CARTESIAN_POINT('Ctrl Pts',(-23.4085752084141,-14.2066193411526,
114.827065531498)) ;
#179551 = CARTESIAN_POINT('Ctrl Pts',(-23.3347713898697,-14.206619276698,
114.85129664895)) ;
#179552 = CARTESIAN_POINT('Ctrl Pts',(-23.2609675713253,-14.2066192122434,
114.875527766403)) ;
#179553 = CARTESIAN_POINT('Ctrl Pts',(-23.2756948310523,-14.2660478588008,
114.920384625278)) ;
#179554 = CARTESIAN_POINT('Ctrl Pts',(-23.2904220907793,-14.3254765053581,
114.965241484154)) ;
#179555 = CARTESIAN_POINT('Ctrl Pts',(-23.3642259093238,-14.3254765698126,
114.941010366701)) ;
#179556 = CARTESIAN_POINT('Ctrl Pts',(-23.4380297278682,-14.3254766342672,
114.916779249248)) ;
#179557 = CARTESIAN_POINT('Ctrl Pts',(-23.4233024681412,-14.2660479877099,
114.871922390373)) ;
#179558 = CARTESIAN_POINT('Ctrl Pts',(-23.4754105644669,-14.0549162780305,
115.066119893745)) ;
#179559 = CARTESIAN_POINT('Ctrl Pts',(-23.4562889637978,-14.010139153776,
115.007878581465)) ;
#179560 = CARTESIAN_POINT('Ctrl Pts',(-23.3824851382236,-14.0101390737133,
115.032109677506)) ;
#179561 = CARTESIAN_POINT('Ctrl Pts',(-23.3086813126494,-14.0101389936507,
115.056340773547)) ;
#179562 = CARTESIAN_POINT('Ctrl Pts',(-23.3278029133185,-14.0549161179053,
115.114582085827)) ;
#179563 = CARTESIAN_POINT('Ctrl Pts',(-23.3469245139876,-14.0996932421598,
115.172823398108)) ;
#179564 = CARTESIAN_POINT('Ctrl Pts',(-23.4207283395618,-14.0996933222224,
115.148592302067)) ;
#179565 = CARTESIAN_POINT('Ctrl Pts',(-23.494532165136,-14.0996934022851,
115.124361206026)) ;
#179566 = CARTESIAN_POINT('Ctrl Pts',(-23.4754105644669,-14.0549162780305,
115.066119893745)) ;
#179567 = CARTESIAN_POINT('Ctrl Pts',(-23.5077572471595,-13.7973888984154,
115.200198351239)) ;
#179568 = CARTESIAN_POINT('Ctrl Pts',(-23.4856127499084,-13.7705242930268,
115.132749783824)) ;
#179569 = CARTESIAN_POINT('Ctrl Pts',(-23.4118089164229,-13.7705242060614,
115.156980855769)) ;
#179570 = CARTESIAN_POINT('Ctrl Pts',(-23.3380050829375,-13.770524119096,
115.181211927714)) ;
#179571 = CARTESIAN_POINT('Ctrl Pts',(-23.3601495801886,-13.7973887244846,
115.248660495129)) ;
#179572 = CARTESIAN_POINT('Ctrl Pts',(-23.3822940774398,-13.8242533298732,
115.316109062544)) ;
#179573 = CARTESIAN_POINT('Ctrl Pts',(-23.4560979109252,-13.8242534168386,
115.291877990599)) ;
#179574 = CARTESIAN_POINT('Ctrl Pts',(-23.5299017444107,-13.824253503804,
115.267646918654)) ;
#179575 = CARTESIAN_POINT('Ctrl Pts',(-23.5077572471595,-13.7973888984154,
115.200198351239)) ;
#179576 = CARTESIAN_POINT('Ctrl Pts',(-23.5172572061641,-13.5143192821472,
115.264479052943)) ;
#179577 = CARTESIAN_POINT('Ctrl Pts',(-23.4936848178715,-13.5071778533561,
115.192681359907)) ;
#179578 = CARTESIAN_POINT('Ctrl Pts',(-23.4198809766881,-13.507177766311,
115.216912408405)) ;
#179579 = CARTESIAN_POINT('Ctrl Pts',(-23.3460771355048,-13.5071776792659,
115.241143456903)) ;
#179580 = CARTESIAN_POINT('Ctrl Pts',(-23.3696495237974,-13.514319108057,
115.312941149939)) ;
#179581 = CARTESIAN_POINT('Ctrl Pts',(-23.39322191209,-13.5214605368481,115.384738842976)) ;
#179582 = CARTESIAN_POINT('Ctrl Pts',(-23.4670257532734,-13.5214606238932,
115.360507794478)) ;
#179583 = CARTESIAN_POINT('Ctrl Pts',(-23.5408295944568,-13.5214607109383,
115.33627674598)) ;
#179584 = CARTESIAN_POINT('Ctrl Pts',(-23.5172572061641,-13.5143192821472,
115.264479052943)) ;
#179585 = CARTESIAN_POINT('Ctrl Pts',(-23.5025567461663,-13.2228141005811,
115.255249135668)) ;
#179586 = CARTESIAN_POINT('Ctrl Pts',(-23.4792395565044,-13.236014362639,
115.184228736629)) ;
#179587 = CARTESIAN_POINT('Ctrl Pts',(-23.4054357084178,-13.2360142841561,
115.208459764101)) ;
#179588 = CARTESIAN_POINT('Ctrl Pts',(-23.3316318603313,-13.2360142056732,
115.232690791573)) ;
#179589 = CARTESIAN_POINT('Ctrl Pts',(-23.3549490499933,-13.2228139436153,
115.303711190613)) ;
#179590 = CARTESIAN_POINT('Ctrl Pts',(-23.3782662396552,-13.2096136815574,
115.374731589652)) ;
#179591 = CARTESIAN_POINT('Ctrl Pts',(-23.4520700877417,-13.2096137600403,
115.35050056218)) ;
#179592 = CARTESIAN_POINT('Ctrl Pts',(-23.5258739358282,-13.2096138385232,
115.326269534708)) ;
#179593 = CARTESIAN_POINT('Ctrl Pts',(-23.5025567461663,-13.2228141005811,
115.255249135668)) ;
#179594 = CARTESIAN_POINT('Ctrl Pts',(-23.4640229788602,-12.9463122499942,
115.173287772294)) ;
#179595 = CARTESIAN_POINT('Ctrl Pts',(-23.4426283410456,-12.9788376519378,
115.108123156115)) ;
#179596 = CARTESIAN_POINT('Ctrl Pts',(-23.3688244875743,-12.978837586653,
115.132354167186)) ;
#179597 = CARTESIAN_POINT('Ctrl Pts',(-23.295020634103,-12.9788375213682,
115.156585178257)) ;
#179598 = CARTESIAN_POINT('Ctrl Pts',(-23.3164152719176,-12.9463121194246,
115.221749794436)) ;
#179599 = CARTESIAN_POINT('Ctrl Pts',(-23.3378099097322,-12.913786717481,
115.286914410615)) ;
#179600 = CARTESIAN_POINT('Ctrl Pts',(-23.4116137632035,-12.9137867827658,
115.262683399543)) ;
#179601 = CARTESIAN_POINT('Ctrl Pts',(-23.4854176166749,-12.9137868480506,
115.238452388472)) ;
#179602 = CARTESIAN_POINT('Ctrl Pts',(-23.4640229788602,-12.9463122499942,
115.173287772294)) ;
#179603 = CARTESIAN_POINT('Ctrl Pts',(-23.4033068584606,-12.7025112775513,
115.023933887441)) ;
#179604 = CARTESIAN_POINT('Ctrl Pts',(-23.38538272599,-12.7521082971811,114.969339870752)) ;
#179605 = CARTESIAN_POINT('Ctrl Pts',(-23.3115788693362,-12.7521082496802,
114.99357087213)) ;
#179606 = CARTESIAN_POINT('Ctrl Pts',(-23.2377750126825,-12.7521082021794,
115.017801873508)) ;
#179607 = CARTESIAN_POINT('Ctrl Pts',(-23.2556991451531,-12.7025111825496,
115.072395890197)) ;
#179608 = CARTESIAN_POINT('Ctrl Pts',(-23.2736232776238,-12.6529141629198,
115.126989906885)) ;
#179609 = CARTESIAN_POINT('Ctrl Pts',(-23.3474271342775,-12.6529142104206,
115.102758905507)) ;
#179610 = CARTESIAN_POINT('Ctrl Pts',(-23.4212309909313,-12.6529142579215,
115.078527904129)) ;
#179611 = CARTESIAN_POINT('Ctrl Pts',(-23.4033068584606,-12.7025112775513,
115.023933887441)) ;
#179612 = CARTESIAN_POINT('Ctrl Pts',(-23.3247469439269,-12.5113386435153,
114.819989036996)) ;
#179613 = CARTESIAN_POINT('Ctrl Pts',(-23.3115496393032,-12.5743584257443,
114.779792175398)) ;
#179614 = CARTESIAN_POINT('Ctrl Pts',(-23.2377457810958,-12.5743583951879,
114.804023172044)) ;
#179615 = CARTESIAN_POINT('Ctrl Pts',(-23.1639419228884,-12.5743583646314,
114.82825416869)) ;
#179616 = CARTESIAN_POINT('Ctrl Pts',(-23.1771392275121,-12.5113385824024,
114.868451030287)) ;
#179617 = CARTESIAN_POINT('Ctrl Pts',(-23.1903365321358,-12.4483188001733,
114.908647891885)) ;
#179618 = CARTESIAN_POINT('Ctrl Pts',(-23.2641403903432,-12.4483188307298,
114.884416895239)) ;
#179619 = CARTESIAN_POINT('Ctrl Pts',(-23.3379442485506,-12.4483188612862,
114.860185898593)) ;
#179620 = CARTESIAN_POINT('Ctrl Pts',(-23.3247469439269,-12.5113386435153,
114.819989036996)) ;
#179621 = CARTESIAN_POINT('Ctrl Pts',(-23.2322554152184,-12.3839986409936,
114.573835678973)) ;
#179622 = CARTESIAN_POINT('Ctrl Pts',(-23.2247600633501,-12.45600534241,114.551006045648)) ;
#179623 = CARTESIAN_POINT('Ctrl Pts',(-23.1509562059776,-12.4560053286552,
114.575237044837)) ;
#179624 = CARTESIAN_POINT('Ctrl Pts',(-23.0771523486052,-12.4560053149005,
114.599468044026)) ;
#179625 = CARTESIAN_POINT('Ctrl Pts',(-23.0846477004735,-12.3839986134842,
114.622297677351)) ;
#179626 = CARTESIAN_POINT('Ctrl Pts',(-23.0921430523418,-12.3119919120679,
114.645127310676)) ;
#179627 = CARTESIAN_POINT('Ctrl Pts',(-23.1659469097142,-12.3119919258226,
114.620896311487)) ;
#179628 = CARTESIAN_POINT('Ctrl Pts',(-23.2397507670867,-12.3119919395773,
114.596665312298)) ;
#179629 = CARTESIAN_POINT('Ctrl Pts',(-23.2322554152184,-12.3839986409936,
114.573835678973)) ;
#179630 = CARTESIAN_POINT('Ctrl Pts',(-23.1325124738357,-12.3313598679509,
114.305463729675)) ;
#179631 = CARTESIAN_POINT('Ctrl Pts',(-23.1312369108758,-12.4071510797427,
114.301578569967)) ;
#179632 = CARTESIAN_POINT('Ctrl Pts',(-23.0574330554719,-12.4071510785913,
114.325809575152)) ;
#179633 = CARTESIAN_POINT('Ctrl Pts',(-22.983629200068,-12.4071510774399,
114.350040580336)) ;
#179634 = CARTESIAN_POINT('Ctrl Pts',(-22.9849047630278,-12.3313598656482,
114.353925740044)) ;
#179635 = CARTESIAN_POINT('Ctrl Pts',(-22.9861803259877,-12.2555686538564,
114.357810899752)) ;
#179636 = CARTESIAN_POINT('Ctrl Pts',(-23.0599841813916,-12.2555686550078,
114.333579894567)) ;
#179637 = CARTESIAN_POINT('Ctrl Pts',(-23.1337880367955,-12.2555686561592,
114.309348889382)) ;
#179638 = CARTESIAN_POINT('Ctrl Pts',(-23.1325124738357,-12.3313598679509,
114.305463729675)) ;
#179639 = CARTESIAN_POINT('Ctrl Pts',(-23.0315695868954,-12.3561484752169,
114.033447032347)) ;
#179640 = CARTESIAN_POINT('Ctrl Pts',(-23.0366068410836,-12.4303237529548,
114.048789695264)) ;
#179641 = CARTESIAN_POINT('Ctrl Pts',(-22.9628029885546,-12.4303237603732,
114.073020709205)) ;
#179642 = CARTESIAN_POINT('Ctrl Pts',(-22.8889991360256,-12.4303237677915,
114.097251723146)) ;
#179643 = CARTESIAN_POINT('Ctrl Pts',(-22.8839618818374,-12.3561484900536,
114.08190906023)) ;
#179644 = CARTESIAN_POINT('Ctrl Pts',(-22.8789246276492,-12.2819732123158,
114.066566397313)) ;
#179645 = CARTESIAN_POINT('Ctrl Pts',(-22.9527284801782,-12.2819732048974,
114.042335383372)) ;
#179646 = CARTESIAN_POINT('Ctrl Pts',(-23.0265323327071,-12.2819731974791,
114.018104369431)) ;
#179647 = CARTESIAN_POINT('Ctrl Pts',(-23.0315695868954,-12.3561484752169,
114.033447032347)) ;
#179648 = CARTESIAN_POINT('Ctrl Pts',(-22.9354487583315,-12.4578681360596,
113.776309520322)) ;
#179649 = CARTESIAN_POINT('Ctrl Pts',(-22.9464679447324,-12.5250537220818,
113.809872183762)) ;
#179650 = CARTESIAN_POINT('Ctrl Pts',(-22.8726640957551,-12.5250537323896,
113.834103208521)) ;
#179651 = CARTESIAN_POINT('Ctrl Pts',(-22.7988602467779,-12.5250537426973,
113.85833423328)) ;
#179652 = CARTESIAN_POINT('Ctrl Pts',(-22.787841060377,-12.4578681566752,
113.82477156984)) ;
#179653 = CARTESIAN_POINT('Ctrl Pts',(-22.7768218739761,-12.390682570653,
113.7912089064)) ;
#179654 = CARTESIAN_POINT('Ctrl Pts',(-22.8506257229533,-12.3906825603452,
113.766977881641)) ;
#179655 = CARTESIAN_POINT('Ctrl Pts',(-22.9244295719306,-12.3906825500374,
113.742746856882)) ;
#179656 = CARTESIAN_POINT('Ctrl Pts',(-22.9354487583315,-12.4578681360596,
113.776309520322)) ;
#179657 = CARTESIAN_POINT('Ctrl Pts',(-22.8516194022014,-12.6270814220524,
113.556268256684)) ;
#179658 = CARTESIAN_POINT('Ctrl Pts',(-22.8677782073947,-12.6825528988753,
113.605485369805)) ;
#179659 = CARTESIAN_POINT('Ctrl Pts',(-22.7939743607582,-12.6825529093536,
113.629716401694)) ;
#179660 = CARTESIAN_POINT('Ctrl Pts',(-22.7201705141217,-12.6825529198319,
113.653947433583)) ;
#179661 = CARTESIAN_POINT('Ctrl Pts',(-22.7040117089284,-12.627081443009,
113.604730320462)) ;
#179662 = CARTESIAN_POINT('Ctrl Pts',(-22.6878529037351,-12.5716099661861,
113.555513207342)) ;
#179663 = CARTESIAN_POINT('Ctrl Pts',(-22.7616567503716,-12.5716099557078,
113.531282175453)) ;
#179664 = CARTESIAN_POINT('Ctrl Pts',(-22.8354605970081,-12.5716099452296,
113.507051143564)) ;
#179665 = CARTESIAN_POINT('Ctrl Pts',(-22.8516194022014,-12.6270814220524,
113.556268256684)) ;
#179666 = CARTESIAN_POINT('Ctrl Pts',(-22.7839838450555,-12.8533401319523,
113.385716322209)) ;
#179667 = CARTESIAN_POINT('Ctrl Pts',(-22.8041559831465,-12.8930967028274,
113.447157399914)) ;
#179668 = CARTESIAN_POINT('Ctrl Pts',(-22.7303521385785,-12.8930967101103,
113.471388438103)) ;
#179669 = CARTESIAN_POINT('Ctrl Pts',(-22.6565482940104,-12.8930967173931,
113.495619476292)) ;
#179670 = CARTESIAN_POINT('Ctrl Pts',(-22.6363761559194,-12.853340146518,
113.434178398587)) ;
#179671 = CARTESIAN_POINT('Ctrl Pts',(-22.6162040178284,-12.8135835756429,
113.372737320882)) ;
#179672 = CARTESIAN_POINT('Ctrl Pts',(-22.6900078623964,-12.8135835683601,
113.348506282693)) ;
#179673 = CARTESIAN_POINT('Ctrl Pts',(-22.7638117069645,-12.8135835610772,
113.324275244504)) ;
#179674 = CARTESIAN_POINT('Ctrl Pts',(-22.7839838450555,-12.8533401319523,
113.385716322209)) ;
#179675 = CARTESIAN_POINT('Ctrl Pts',(-22.737057523416,-13.1210491167834,
113.278349913962)) ;
#179676 = CARTESIAN_POINT('Ctrl Pts',(-22.7598008408309,-13.1421721692445,
113.347622389144)) ;
#179677 = CARTESIAN_POINT('Ctrl Pts',(-22.6859969973566,-13.1421721715333,
113.371853430664)) ;
#179678 = CARTESIAN_POINT('Ctrl Pts',(-22.6121931538823,-13.1421721738222,
113.396084472184)) ;
#179679 = CARTESIAN_POINT('Ctrl Pts',(-22.5894498364674,-13.121049121361,
113.326811997003)) ;
#179680 = CARTESIAN_POINT('Ctrl Pts',(-22.5667065190524,-13.0999260688999,
113.257539521822)) ;
#179681 = CARTESIAN_POINT('Ctrl Pts',(-22.6405103625268,-13.0999260666111,
113.233308480301)) ;
#179682 = CARTESIAN_POINT('Ctrl Pts',(-22.7143142060011,-13.0999260643223,
113.209077438781)) ;
#179683 = CARTESIAN_POINT('Ctrl Pts',(-22.737057523416,-13.1210491167834,
113.278349913962)) ;
#179684 = CARTESIAN_POINT('Ctrl Pts',(-22.7137114782824,-13.40900770729,113.242669521787)) ;
#179685 = CARTESIAN_POINT('Ctrl Pts',(-22.7373858208915,-13.410054885097,
113.314777749557)) ;
#179686 = CARTESIAN_POINT('Ctrl Pts',(-22.663581977556,-13.4100548838608,
113.339008791501)) ;
#179687 = CARTESIAN_POINT('Ctrl Pts',(-22.5897781342205,-13.4100548826247,
113.363239833444)) ;
#179688 = CARTESIAN_POINT('Ctrl Pts',(-22.5661037916114,-13.4090077048177,
113.291131605674)) ;
#179689 = CARTESIAN_POINT('Ctrl Pts',(-22.5424294490023,-13.4079605270107,
113.219023377904)) ;
#179690 = CARTESIAN_POINT('Ctrl Pts',(-22.6162332923378,-13.4079605282469,
113.19479233596)) ;
#179691 = CARTESIAN_POINT('Ctrl Pts',(-22.6900371356733,-13.407960529483,
113.170561294017)) ;
#179692 = CARTESIAN_POINT('Ctrl Pts',(-22.7137114782824,-13.40900770729,113.242669521787)) ;
#179693 = CARTESIAN_POINT('Ctrl Pts',(-22.7145790475153,-13.6972694862933,
113.280702081642)) ;
#179694 = CARTESIAN_POINT('Ctrl Pts',(-22.7374956175448,-13.6781895282422,
113.350502256437)) ;
#179695 = CARTESIAN_POINT('Ctrl Pts',(-22.6636917739189,-13.6781895252059,
113.374733297496)) ;
#179696 = CARTESIAN_POINT('Ctrl Pts',(-22.5898879302931,-13.6781895221696,
113.398964338555)) ;
#179697 = CARTESIAN_POINT('Ctrl Pts',(-22.5669713602635,-13.6972694802207,
113.32916416376)) ;
#179698 = CARTESIAN_POINT('Ctrl Pts',(-22.544054790234,-13.7163494382719,
113.259363988965)) ;
#179699 = CARTESIAN_POINT('Ctrl Pts',(-22.6178586338598,-13.7163494413082,
113.235132947906)) ;
#179700 = CARTESIAN_POINT('Ctrl Pts',(-22.6916624774857,-13.7163494443445,
113.210901906847)) ;
#179701 = CARTESIAN_POINT('Ctrl Pts',(-22.7145790475153,-13.6972694862933,
113.280702081642)) ;
#179702 = CARTESIAN_POINT('Ctrl Pts',(-22.73888971428,-13.9663054532962,113.390221067271)) ;
#179703 = CARTESIAN_POINT('Ctrl Pts',(-22.7594085131034,-13.9284104742122,
113.452718017853)) ;
#179704 = CARTESIAN_POINT('Ctrl Pts',(-22.6856046691513,-13.9284104715145,
113.476949057918)) ;
#179705 = CARTESIAN_POINT('Ctrl Pts',(-22.6118008251992,-13.9284104688168,
113.501180097983)) ;
#179706 = CARTESIAN_POINT('Ctrl Pts',(-22.5912820263757,-13.9663054479008,
113.438683147401)) ;
#179707 = CARTESIAN_POINT('Ctrl Pts',(-22.5707632275523,-14.0042004269848,
113.376186196819)) ;
#179708 = CARTESIAN_POINT('Ctrl Pts',(-22.6445670715044,-14.0042004296825,
113.351955156754)) ;
#179709 = CARTESIAN_POINT('Ctrl Pts',(-22.7183709154566,-14.0042004323802,
113.327724116689)) ;
#179710 = CARTESIAN_POINT('Ctrl Pts',(-22.73888971428,-13.9663054532962,113.390221067271)) ;
#179711 = CARTESIAN_POINT('Ctrl Pts',(-22.7845308373615,-14.1969043333081,
113.564878486232)) ;
#179712 = CARTESIAN_POINT('Ctrl Pts',(-22.8011552397315,-14.1428507400375,
113.615513733517)) ;
#179713 = CARTESIAN_POINT('Ctrl Pts',(-22.7273513962051,-14.1428507401224,
113.639744774879)) ;
#179714 = CARTESIAN_POINT('Ctrl Pts',(-22.6535475526786,-14.1428507402074,
113.663975816241)) ;
#179715 = CARTESIAN_POINT('Ctrl Pts',(-22.6369231503086,-14.196904333478,
113.613340568955)) ;
#179716 = CARTESIAN_POINT('Ctrl Pts',(-22.6202987479386,-14.2509579267487,
113.56270532167)) ;
#179717 = CARTESIAN_POINT('Ctrl Pts',(-22.6941025914651,-14.2509579266637,
113.538474280308)) ;
#179718 = CARTESIAN_POINT('Ctrl Pts',(-22.7679064349915,-14.2509579265788,
113.514243238946)) ;
#179719 = CARTESIAN_POINT('Ctrl Pts',(-22.7845308373615,-14.1969043333081,
113.564878486232)) ;
#179720 = CARTESIAN_POINT('Ctrl Pts',(-22.8467313080852,-14.3698914257013,
113.789672047739)) ;
#179721 = CARTESIAN_POINT('Ctrl Pts',(-22.8583054400605,-14.3036801668695,
113.824924986188)) ;
#179722 = CARTESIAN_POINT('Ctrl Pts',(-22.7845015975603,-14.3036801689092,
113.849156030675)) ;
#179723 = CARTESIAN_POINT('Ctrl Pts',(-22.71069775506,-14.303680170949,113.873387075162)) ;
#179724 = CARTESIAN_POINT('Ctrl Pts',(-22.6991236230846,-14.3698914297808,
113.838134136713)) ;
#179725 = CARTESIAN_POINT('Ctrl Pts',(-22.6875494911093,-14.4361026886127,
113.802881198264)) ;
#179726 = CARTESIAN_POINT('Ctrl Pts',(-22.7613533336096,-14.4361026865729,
113.778650153777)) ;
#179727 = CARTESIAN_POINT('Ctrl Pts',(-22.8351571761099,-14.4361026845332,
113.75441910929)) ;
#179728 = CARTESIAN_POINT('Ctrl Pts',(-22.8467313080852,-14.3698914257013,
113.789672047739)) ;
#179729 = CARTESIAN_POINT('Ctrl Pts',(-22.9207425971933,-14.4755193866787,
114.050515802976)) ;
#179730 = CARTESIAN_POINT('Ctrl Pts',(-22.9264328703088,-14.4018362726686,
114.067847456596)) ;
#179731 = CARTESIAN_POINT('Ctrl Pts',(-22.8526290294858,-14.4018362752404,
114.092078506192)) ;
#179732 = CARTESIAN_POINT('Ctrl Pts',(-22.7788251886628,-14.4018362778122,
114.116309555787)) ;
#179733 = CARTESIAN_POINT('Ctrl Pts',(-22.7731349155474,-14.4755193918222,
114.098977902168)) ;
#179734 = CARTESIAN_POINT('Ctrl Pts',(-22.7674446424319,-14.5492025058322,
114.081646248548)) ;
#179735 = CARTESIAN_POINT('Ctrl Pts',(-22.8412484832549,-14.5492025032605,
114.057415198952)) ;
#179736 = CARTESIAN_POINT('Ctrl Pts',(-22.9150523240779,-14.5492025006887,
114.033184149356)) ;
#179737 = CARTESIAN_POINT('Ctrl Pts',(-22.9207425971933,-14.4755193866787,
114.050515802976)) ;
#179738 = CARTESIAN_POINT('Ctrl Pts',(-23.0006816978968,-14.5054697818126,
114.329505017033)) ;
#179739 = CARTESIAN_POINT('Ctrl Pts',(-23.0000638124603,-14.4295881889502,
114.327623037386)) ;
#179740 = CARTESIAN_POINT('Ctrl Pts',(-22.9262599739428,-14.4295881891086,
114.351854094004)) ;
#179741 = CARTESIAN_POINT('Ctrl Pts',(-22.8524561354252,-14.429588189267,
114.376085150622)) ;
#179742 = CARTESIAN_POINT('Ctrl Pts',(-22.8530740208617,-14.5054697821294,
114.377967130269)) ;
#179743 = CARTESIAN_POINT('Ctrl Pts',(-22.8536919062982,-14.5813513749918,
114.379849109916)) ;
#179744 = CARTESIAN_POINT('Ctrl Pts',(-22.9274957448158,-14.5813513748333,
114.355618053298)) ;
#179745 = CARTESIAN_POINT('Ctrl Pts',(-23.0012995833333,-14.5813513746749,
114.33138699668)) ;
#179746 = CARTESIAN_POINT('Ctrl Pts',(-23.0006816978968,-14.5054697818126,
114.329505017033)) ;
#179747 = CARTESIAN_POINT('Ctrl Pts',(-23.0797492263395,-14.4574393177702,
114.6057916227)) ;
#179748 = CARTESIAN_POINT('Ctrl Pts',(-23.0728759886018,-14.384801335134,
114.584856849095)) ;
#179749 = CARTESIAN_POINT('Ctrl Pts',(-22.9990721521764,-14.384801328945,
114.609087912085)) ;
#179750 = CARTESIAN_POINT('Ctrl Pts',(-22.9252683157509,-14.384801322756,
114.633318975075)) ;
#179751 = CARTESIAN_POINT('Ctrl Pts',(-22.9321415534886,-14.4574393053923,
114.65425374868)) ;
#179752 = CARTESIAN_POINT('Ctrl Pts',(-22.9390147912263,-14.5300772880285,
114.675188522285)) ;
#179753 = CARTESIAN_POINT('Ctrl Pts',(-23.0128186276518,-14.5300772942175,
114.650957459295)) ;
#179754 = CARTESIAN_POINT('Ctrl Pts',(-23.0866224640773,-14.5300773004065,
114.626726396305)) ;
#179755 = CARTESIAN_POINT('Ctrl Pts',(-23.0797492263395,-14.4574393177702,
114.6057916227)) ;
#179756 = CARTESIAN_POINT('Ctrl Pts',(-23.1516520346911,-14.3349211938034,
114.860267274073)) ;
#179757 = CARTESIAN_POINT('Ctrl Pts',(-23.1390144923335,-14.2707324518497,
114.821775358504)) ;
#179758 = CARTESIAN_POINT('Ctrl Pts',(-23.0652106573152,-14.2707324355109,
114.84600642578)) ;
#179759 = CARTESIAN_POINT('Ctrl Pts',(-22.9914068222969,-14.2707324191721,
114.870237493056)) ;
#179760 = CARTESIAN_POINT('Ctrl Pts',(-23.0040443646544,-14.3349211611258,
114.908729408625)) ;
#179761 = CARTESIAN_POINT('Ctrl Pts',(-23.0166819070119,-14.3991099030794,
114.947221324195)) ;
#179762 = CARTESIAN_POINT('Ctrl Pts',(-23.0904857420302,-14.3991099194182,
114.922990256919)) ;
#179763 = CARTESIAN_POINT('Ctrl Pts',(-23.1642895770486,-14.399109935757,
114.898759189643)) ;
#179764 = CARTESIAN_POINT('Ctrl Pts',(-23.1516520346911,-14.3349211938034,
114.860267274073)) ;
#179765 = CARTESIAN_POINT('Ctrl Pts',(-23.2103873638468,-14.1470800055845,
115.074578542204)) ;
#179766 = CARTESIAN_POINT('Ctrl Pts',(-23.1928978798013,-14.0959137214437,
115.021308394955)) ;
#179767 = CARTESIAN_POINT('Ctrl Pts',(-23.1190940448238,-14.0959136926008,
115.045539462355)) ;
#179768 = CARTESIAN_POINT('Ctrl Pts',(-23.0452902098462,-14.095913663758,
115.069770529756)) ;
#179769 = CARTESIAN_POINT('Ctrl Pts',(-23.0627796938917,-14.1470799478988,
115.123040677004)) ;
#179770 = CARTESIAN_POINT('Ctrl Pts',(-23.0802691779372,-14.1982462320397,
115.176310824253)) ;
#179771 = CARTESIAN_POINT('Ctrl Pts',(-23.1540730129147,-14.1982462608825,
115.152079756853)) ;
#179772 = CARTESIAN_POINT('Ctrl Pts',(-23.2278768478922,-14.1982462897254,
115.127848689452)) ;
#179773 = CARTESIAN_POINT('Ctrl Pts',(-23.2103873638468,-14.1470800055845,
115.074578542204)) ;
#179774 = CARTESIAN_POINT('Ctrl Pts',(-23.2512289756988,-13.9065331674936,
115.234478316148)) ;
#179775 = CARTESIAN_POINT('Ctrl Pts',(-23.2301280118323,-13.8720877275132,
115.170208183899)) ;
#179776 = CARTESIAN_POINT('Ctrl Pts',(-23.1563241754642,-13.8720876844338,
115.194439247064)) ;
#179777 = CARTESIAN_POINT('Ctrl Pts',(-23.0825203390961,-13.8720876413544,
115.218670310229)) ;
#179778 = CARTESIAN_POINT('Ctrl Pts',(-23.1036213029626,-13.9065330813348,
115.282940442478)) ;
#179779 = CARTESIAN_POINT('Ctrl Pts',(-23.1247222668291,-13.9409785213152,
115.347210574727)) ;
#179780 = CARTESIAN_POINT('Ctrl Pts',(-23.1985261031972,-13.9409785643945,
115.322979511562)) ;
#179781 = CARTESIAN_POINT('Ctrl Pts',(-23.2723299395653,-13.9409786074739,
115.298748448398)) ;
#179782 = CARTESIAN_POINT('Ctrl Pts',(-23.2512289756988,-13.9065331674936,
115.234478316148)) ;
#179783 = CARTESIAN_POINT('Ctrl Pts',(-23.2702582801817,-13.630738678715,
115.327956236279)) ;
#179784 = CARTESIAN_POINT('Ctrl Pts',(-23.2470632296834,-13.6154990346672,
115.257307853852)) ;
#179785 = CARTESIAN_POINT('Ctrl Pts',(-23.1732593900141,-13.6154989781254,
115.281538906962)) ;
#179786 = CARTESIAN_POINT('Ctrl Pts',(-23.0994555503449,-13.6154989215836,
115.305769960072)) ;
#179787 = CARTESIAN_POINT('Ctrl Pts',(-23.1226506008432,-13.6307385656315,
115.376418342499)) ;
#179788 = CARTESIAN_POINT('Ctrl Pts',(-23.1458456513416,-13.6459782096793,
115.447066724927)) ;
#179789 = CARTESIAN_POINT('Ctrl Pts',(-23.2196494910108,-13.6459782662211,
115.422835671817)) ;
#179790 = CARTESIAN_POINT('Ctrl Pts',(-23.29345333068,-13.6459783227629,115.398604618707)) ;
#179791 = CARTESIAN_POINT('Ctrl Pts',(-23.2702582801817,-13.630738678715,
115.327956236279)) ;
#179792 = CARTESIAN_POINT('Ctrl Pts',(-23.2654718156878,-13.3408270196336,
115.34875619149)) ;
#179793 = CARTESIAN_POINT('Ctrl Pts',(-23.2418454296788,-13.3458064636332,
115.276794030546)) ;
#179794 = CARTESIAN_POINT('Ctrl Pts',(-23.1680415850337,-13.3458063983403,
115.301025068501)) ;
#179795 = CARTESIAN_POINT('Ctrl Pts',(-23.0942377403886,-13.3458063330474,
115.325256106455)) ;
#179796 = CARTESIAN_POINT('Ctrl Pts',(-23.1178641263977,-13.3408268890478,
115.397218267399)) ;
#179797 = CARTESIAN_POINT('Ctrl Pts',(-23.1414905124067,-13.3358474450482,
115.469180428343)) ;
#179798 = CARTESIAN_POINT('Ctrl Pts',(-23.2152943570518,-13.3358475103411,
115.444949390389)) ;
#179799 = CARTESIAN_POINT('Ctrl Pts',(-23.2890982016969,-13.335847575634,
115.420718352435)) ;
#179800 = CARTESIAN_POINT('Ctrl Pts',(-23.2654718156878,-13.3408270196336,
115.34875619149)) ;
#179801 = CARTESIAN_POINT('Ctrl Pts',(-23.2364052797184,-13.0553492265632,
115.295741122605)) ;
#179802 = CARTESIAN_POINT('Ctrl Pts',(-23.2140390795287,-13.0802672240232,
115.227617284172)) ;
#179803 = CARTESIAN_POINT('Ctrl Pts',(-23.1402352286369,-13.0802671541192,
115.2518483031)) ;
#179804 = CARTESIAN_POINT('Ctrl Pts',(-23.066431377745,-13.0802670842153,
115.276079322027)) ;
#179805 = CARTESIAN_POINT('Ctrl Pts',(-23.0887975779347,-13.0553490867554,
115.34420316046)) ;
#179806 = CARTESIAN_POINT('Ctrl Pts',(-23.1111637781244,-13.0304310892955,
115.412326998893)) ;
#179807 = CARTESIAN_POINT('Ctrl Pts',(-23.1849676290162,-13.0304311591994,
115.388095979966)) ;
#179808 = CARTESIAN_POINT('Ctrl Pts',(-23.2587714799081,-13.0304312291033,
115.363864961038)) ;
#179809 = CARTESIAN_POINT('Ctrl Pts',(-23.2364052797184,-13.0553492265632,
115.295741122605)) ;
#179810 = CARTESIAN_POINT('Ctrl Pts',(-23.184450119502,-12.7963986353394,
115.172941175961)) ;
#179811 = CARTESIAN_POINT('Ctrl Pts',(-23.1649453982512,-12.8394319369363,
115.113532940537)) ;
#179812 = CARTESIAN_POINT('Ctrl Pts',(-23.0911415405192,-12.8394318699613,
115.137763938631)) ;
#179813 = CARTESIAN_POINT('Ctrl Pts',(-23.0173376827871,-12.8394318029862,
115.161994936724)) ;
#179814 = CARTESIAN_POINT('Ctrl Pts',(-23.0368424040378,-12.7963985013893,
115.221403172148)) ;
#179815 = CARTESIAN_POINT('Ctrl Pts',(-23.0563471252886,-12.7533651997924,
115.280811407572)) ;
#179816 = CARTESIAN_POINT('Ctrl Pts',(-23.1301509830206,-12.7533652667675,
115.256580409478)) ;
#179817 = CARTESIAN_POINT('Ctrl Pts',(-23.2039548407527,-12.7533653337425,
115.232349411385)) ;
#179818 = CARTESIAN_POINT('Ctrl Pts',(-23.184450119502,-12.7963986353394,
115.172941175961)) ;
#179819 = CARTESIAN_POINT('Ctrl Pts',(-23.112508885965,-12.581755675213,114.98929825524)) ;
#179820 = CARTESIAN_POINT('Ctrl Pts',(-23.097264403479,-12.6398371824031,
114.942866019574)) ;
#179821 = CARTESIAN_POINT('Ctrl Pts',(-23.0234605390643,-12.6398371256695,
114.967096997313)) ;
#179822 = CARTESIAN_POINT('Ctrl Pts',(-22.9496566746497,-12.639837068936,
114.991327975052)) ;
#179823 = CARTESIAN_POINT('Ctrl Pts',(-22.9649011571356,-12.581755561746,
115.037760210718)) ;
#179824 = CARTESIAN_POINT('Ctrl Pts',(-22.9801456396215,-12.5236740545559,
115.084192446384)) ;
#179825 = CARTESIAN_POINT('Ctrl Pts',(-23.0539495040362,-12.5236741112895,
115.059961468645)) ;
#179826 = CARTESIAN_POINT('Ctrl Pts',(-23.1277533684509,-12.523674168023,
115.035730490905)) ;
#179827 = CARTESIAN_POINT('Ctrl Pts',(-23.112508885965,-12.581755675213,114.98929825524)) ;
#179828 = CARTESIAN_POINT('Ctrl Pts',(-23.0250710503237,-12.4271874700909,
114.758426315697)) ;
#179829 = CARTESIAN_POINT('Ctrl Pts',(-23.0151754699224,-12.4961449438695,
114.728285972627)) ;
#179830 = CARTESIAN_POINT('Ctrl Pts',(-22.9413715999022,-12.4961449047111,
114.752516933292)) ;
#179831 = CARTESIAN_POINT('Ctrl Pts',(-22.8675677298821,-12.4961448655528,
114.776747893958)) ;
#179832 = CARTESIAN_POINT('Ctrl Pts',(-22.8774633102834,-12.4271873917741,
114.806888237029)) ;
#179833 = CARTESIAN_POINT('Ctrl Pts',(-22.8873588906847,-12.3582299179955,
114.837028580099)) ;
#179834 = CARTESIAN_POINT('Ctrl Pts',(-22.9611627607048,-12.3582299571538,
114.812797619433)) ;
#179835 = CARTESIAN_POINT('Ctrl Pts',(-23.034966630725,-12.3582299963122,
114.788566658768)) ;
#179836 = CARTESIAN_POINT('Ctrl Pts',(-23.0250710503237,-12.4271874700909,
114.758426315697)) ;
#179837 = CARTESIAN_POINT('Ctrl Pts',(-22.9276247608224,-12.3434882644401,
114.49706508371)) ;
#179838 = CARTESIAN_POINT('Ctrl Pts',(-22.9237846766469,-12.4183899253302,
114.485368804997)) ;
#179839 = CARTESIAN_POINT('Ctrl Pts',(-22.8499808028187,-12.4183899094731,
114.509599754064)) ;
#179840 = CARTESIAN_POINT('Ctrl Pts',(-22.7761769289905,-12.418389893616,
114.533830703132)) ;
#179841 = CARTESIAN_POINT('Ctrl Pts',(-22.780017013166,-12.3434882327259,
114.545526981844)) ;
#179842 = CARTESIAN_POINT('Ctrl Pts',(-22.7838570973414,-12.2685865718357,
114.557223260557)) ;
#179843 = CARTESIAN_POINT('Ctrl Pts',(-22.8576609711696,-12.2685865876929,
114.53299231149)) ;
#179844 = CARTESIAN_POINT('Ctrl Pts',(-22.9314648449978,-12.26858660355,114.508761362422)) ;
#179845 = CARTESIAN_POINT('Ctrl Pts',(-22.9276247608224,-12.3434882644401,
114.49706508371)) ;
#179846 = CARTESIAN_POINT('Ctrl Pts',(-22.826190770514,-12.3367187774922,
114.223618478407)) ;
#179847 = CARTESIAN_POINT('Ctrl Pts',(-22.8286921174986,-12.412202858538,
114.23123717574)) ;
#179848 = CARTESIAN_POINT('Ctrl Pts',(-22.7548882421407,-12.4122028696992,
114.255468120148)) ;
#179849 = CARTESIAN_POINT('Ctrl Pts',(-22.6810843667827,-12.4122028808603,
114.279699064556)) ;
#179850 = CARTESIAN_POINT('Ctrl Pts',(-22.678583019798,-12.3367187998145,
114.272080367222)) ;
#179851 = CARTESIAN_POINT('Ctrl Pts',(-22.6760816728134,-12.2612347187686,
114.264461669889)) ;
#179852 = CARTESIAN_POINT('Ctrl Pts',(-22.7498855481713,-12.2612347076075,
114.240230725481)) ;
#179853 = CARTESIAN_POINT('Ctrl Pts',(-22.8236894235293,-12.2612346964463,
114.215999781074)) ;
#179854 = CARTESIAN_POINT('Ctrl Pts',(-22.826190770514,-12.3367187774922,
114.223618478407)) ;
#179855 = CARTESIAN_POINT('Ctrl Pts',(-22.7275355764204,-12.4076100218016,
113.958611864948)) ;
#179856 = CARTESIAN_POINT('Ctrl Pts',(-22.7361941637396,-12.478255694811,
113.984984522816)) ;
#179857 = CARTESIAN_POINT('Ctrl Pts',(-22.662390289618,-12.4782557339545,
114.00921547099)) ;
#179858 = CARTESIAN_POINT('Ctrl Pts',(-22.5885864154965,-12.4782557730979,
114.033446419164)) ;
#179859 = CARTESIAN_POINT('Ctrl Pts',(-22.5799278281774,-12.4076101000885,
114.007073761295)) ;
#179860 = CARTESIAN_POINT('Ctrl Pts',(-22.5712692408582,-12.3369644270791,
113.980701103427)) ;
#179861 = CARTESIAN_POINT('Ctrl Pts',(-22.6450731149797,-12.3369643879356,
113.956470155253)) ;
#179862 = CARTESIAN_POINT('Ctrl Pts',(-22.7188769891013,-12.3369643487922,
113.93223920708)) ;
#179863 = CARTESIAN_POINT('Ctrl Pts',(-22.7275355764204,-12.4076100218016,
113.958611864948)) ;
#179864 = CARTESIAN_POINT('Ctrl Pts',(-22.6381489586998,-12.5503272886106,
113.721728947846)) ;
#179865 = CARTESIAN_POINT('Ctrl Pts',(-22.6523289736193,-12.6111127645847,
113.764918983274)) ;
#179866 = CARTESIAN_POINT('Ctrl Pts',(-22.5785251034211,-12.6111128294537,
113.789149943397)) ;
#179867 = CARTESIAN_POINT('Ctrl Pts',(-22.5047212332228,-12.6111128943226,
113.81338090352)) ;
#179868 = CARTESIAN_POINT('Ctrl Pts',(-22.4905412183032,-12.5503274183485,
113.770190868092)) ;
#179869 = CARTESIAN_POINT('Ctrl Pts',(-22.4763612033837,-12.4895419423743,
113.727000832665)) ;
#179870 = CARTESIAN_POINT('Ctrl Pts',(-22.550165073582,-12.4895418775054,
113.702769872541)) ;
#179871 = CARTESIAN_POINT('Ctrl Pts',(-22.6239689437803,-12.4895418126364,
113.678538912418)) ;
#179872 = CARTESIAN_POINT('Ctrl Pts',(-22.6381489586998,-12.5503272886106,
113.721728947846)) ;
#179873 = CARTESIAN_POINT('Ctrl Pts',(-22.5630668542689,-12.7556871760659,
113.528549608634)) ;
#179874 = CARTESIAN_POINT('Ctrl Pts',(-22.5817750440793,-12.8022252144536,
113.585531734144)) ;
#179875 = CARTESIAN_POINT('Ctrl Pts',(-22.5079711800751,-12.8022253005655,
113.609762713133)) ;
#179876 = CARTESIAN_POINT('Ctrl Pts',(-22.434167316071,-12.8022253866775,
113.633993692123)) ;
#179877 = CARTESIAN_POINT('Ctrl Pts',(-22.4154591262606,-12.7556873482899,
113.577011566613)) ;
#179878 = CARTESIAN_POINT('Ctrl Pts',(-22.3967509364503,-12.7091493099022,
113.520029441103)) ;
#179879 = CARTESIAN_POINT('Ctrl Pts',(-22.4705548004545,-12.7091492237902,
113.495798462113)) ;
#179880 = CARTESIAN_POINT('Ctrl Pts',(-22.5443586644586,-12.7091491376783,
113.471567483124)) ;
#179881 = CARTESIAN_POINT('Ctrl Pts',(-22.5630668542689,-12.7556871760659,
113.528549608634)) ;
#179882 = CARTESIAN_POINT('Ctrl Pts',(-22.5073121196337,-13.0091921750313,
113.394296840887)) ;
#179883 = CARTESIAN_POINT('Ctrl Pts',(-22.5292047849245,-13.038100701856,
113.460978364909)) ;
#179884 = CARTESIAN_POINT('Ctrl Pts',(-22.4554009289081,-13.03810080188,113.485209368228)) ;
#179885 = CARTESIAN_POINT('Ctrl Pts',(-22.3815970728916,-13.038100901904,
113.509440371547)) ;
#179886 = CARTESIAN_POINT('Ctrl Pts',(-22.3597044076008,-13.0091923750794,
113.442758847525)) ;
#179887 = CARTESIAN_POINT('Ctrl Pts',(-22.3378117423101,-12.9802838482547,
113.376077323502)) ;
#179888 = CARTESIAN_POINT('Ctrl Pts',(-22.4116155983265,-12.9802837482307,
113.351846320183)) ;
#179889 = CARTESIAN_POINT('Ctrl Pts',(-22.4854194543429,-12.9802836482067,
113.327615316865)) ;
#179890 = CARTESIAN_POINT('Ctrl Pts',(-22.5073121196337,-13.0091921750313,
113.394296840887)) ;
#179891 = CARTESIAN_POINT('Ctrl Pts',(-22.4743110003687,-13.2902503547293,
113.32912295841)) ;
#179892 = CARTESIAN_POINT('Ctrl Pts',(-22.497808872614,-13.2995791016308,
113.400693683843)) ;
#179893 = CARTESIAN_POINT('Ctrl Pts',(-22.424005025375,-13.2995792074157,
113.424924713897)) ;
#179894 = CARTESIAN_POINT('Ctrl Pts',(-22.3502011781361,-13.2995793132006,
113.449155743951)) ;
#179895 = CARTESIAN_POINT('Ctrl Pts',(-22.3267033058907,-13.2902505662991,
113.377585018517)) ;
#179896 = CARTESIAN_POINT('Ctrl Pts',(-22.3032054336454,-13.2809218193976,
113.306014293084)) ;
#179897 = CARTESIAN_POINT('Ctrl Pts',(-22.3770092808844,-13.2809217136127,
113.28178326303)) ;
#179898 = CARTESIAN_POINT('Ctrl Pts',(-22.4508131281233,-13.2809216078278,
113.257552232976)) ;
#179899 = CARTESIAN_POINT('Ctrl Pts',(-22.4743110003687,-13.2902503547293,
113.32912295841)) ;
#179900 = CARTESIAN_POINT('Ctrl Pts',(-22.4652747457874,-13.5823834440121,
113.337185548665)) ;
#179901 = CARTESIAN_POINT('Ctrl Pts',(-22.4887023578516,-13.5713305139235,
113.408542272981)) ;
#179902 = CARTESIAN_POINT('Ctrl Pts',(-22.4148985194354,-13.5713306161393,
113.432773329908)) ;
#179903 = CARTESIAN_POINT('Ctrl Pts',(-22.3410946810191,-13.5713307183552,
113.457004386834)) ;
#179904 = CARTESIAN_POINT('Ctrl Pts',(-22.317667068955,-13.5823836484438,
113.385647662517)) ;
#179905 = CARTESIAN_POINT('Ctrl Pts',(-22.2942394568908,-13.5934365785324,
113.3142909382)) ;
#179906 = CARTESIAN_POINT('Ctrl Pts',(-22.368043295307,-13.5934364763166,
113.290059881274)) ;
#179907 = CARTESIAN_POINT('Ctrl Pts',(-22.4418471337233,-13.5934363741007,
113.265828824348)) ;
#179908 = CARTESIAN_POINT('Ctrl Pts',(-22.4652747457874,-13.5823834440121,
113.337185548665)) ;
#179909 = CARTESIAN_POINT('Ctrl Pts',(-22.4804477896373,-13.8618181146796,
113.418880666887)) ;
#179910 = CARTESIAN_POINT('Ctrl Pts',(-22.5021170027006,-13.8312391943693,
113.484881591642)) ;
#179911 = CARTESIAN_POINT('Ctrl Pts',(-22.428313172045,-13.8312392849538,
113.509112672206)) ;
#179912 = CARTESIAN_POINT('Ctrl Pts',(-22.3545093413895,-13.8312393755383,
113.53334375277)) ;
#179913 = CARTESIAN_POINT('Ctrl Pts',(-22.3328401283261,-13.8618182958485,
113.467342828015)) ;
#179914 = CARTESIAN_POINT('Ctrl Pts',(-22.3111709152628,-13.8923972161587,
113.401341903259)) ;
#179915 = CARTESIAN_POINT('Ctrl Pts',(-22.3849747459184,-13.8923971255743,
113.377110822695)) ;
#179916 = CARTESIAN_POINT('Ctrl Pts',(-22.4587785765739,-13.8923970349898,
113.352879742131)) ;
#179917 = CARTESIAN_POINT('Ctrl Pts',(-22.4804477896373,-13.8618181146796,
113.418880666887)) ;
#179918 = CARTESIAN_POINT('Ctrl Pts',(-22.517518476082,-14.1083106024044,
113.567088552821)) ;
#179919 = CARTESIAN_POINT('Ctrl Pts',(-22.5359014970355,-14.0604763693046,
113.623080266709)) ;
#179920 = CARTESIAN_POINT('Ctrl Pts',(-22.4620976726408,-14.0604764428427,
113.647311366343)) ;
#179921 = CARTESIAN_POINT('Ctrl Pts',(-22.3882938482461,-14.0604765163808,
113.671542465977)) ;
#179922 = CARTESIAN_POINT('Ctrl Pts',(-22.3699108272926,-14.1083107494807,
113.615550752088)) ;
#179923 = CARTESIAN_POINT('Ctrl Pts',(-22.3515278063391,-14.1561449825805,
113.559559038199)) ;
#179924 = CARTESIAN_POINT('Ctrl Pts',(-22.4253316307338,-14.1561449090424,
113.535327938566)) ;
#179925 = CARTESIAN_POINT('Ctrl Pts',(-22.4991354551285,-14.1561448355042,
113.511096838932)) ;
#179926 = CARTESIAN_POINT('Ctrl Pts',(-22.517518476082,-14.1083106024044,
113.567088552821)) ;
#179927 = CARTESIAN_POINT('Ctrl Pts',(-22.5736052210533,-14.3070623418306,
113.773452298608)) ;
#179928 = CARTESIAN_POINT('Ctrl Pts',(-22.5873648692715,-14.2452796350311,
113.81536196524)) ;
#179929 = CARTESIAN_POINT('Ctrl Pts',(-22.5135610487874,-14.2452796860699,
113.839593076785)) ;
#179930 = CARTESIAN_POINT('Ctrl Pts',(-22.4397572283033,-14.2452797371086,
113.86382418833)) ;
#179931 = CARTESIAN_POINT('Ctrl Pts',(-22.4259975800851,-14.3070624439081,
113.821914521697)) ;
#179932 = CARTESIAN_POINT('Ctrl Pts',(-22.412237931867,-14.3688451507076,
113.780004855065)) ;
#179933 = CARTESIAN_POINT('Ctrl Pts',(-22.4860417523511,-14.3688450996689,
113.75577374352)) ;
#179934 = CARTESIAN_POINT('Ctrl Pts',(-22.5598455728352,-14.3688450486301,
113.731542631975)) ;
#179935 = CARTESIAN_POINT('Ctrl Pts',(-22.5736052210533,-14.3070623418306,
113.773452298608)) ;
#179936 = CARTESIAN_POINT('Ctrl Pts',(-22.6439238545744,-14.4418892785907,
114.023216814566)) ;
#179937 = CARTESIAN_POINT('Ctrl Pts',(-22.652058457175,-14.370599628049,114.047993499991)) ;
#179938 = CARTESIAN_POINT('Ctrl Pts',(-22.57825463788,-14.3705996550827,114.072224615158)) ;
#179939 = CARTESIAN_POINT('Ctrl Pts',(-22.504450818585,-14.3705996821164,
114.096455730324)) ;
#179940 = CARTESIAN_POINT('Ctrl Pts',(-22.4963162159844,-14.4418893326581,
114.071679044899)) ;
#179941 = CARTESIAN_POINT('Ctrl Pts',(-22.4881816133838,-14.5131789831999,
114.046902359473)) ;
#179942 = CARTESIAN_POINT('Ctrl Pts',(-22.5619854326788,-14.5131789561661,
114.022671244307)) ;
#179943 = CARTESIAN_POINT('Ctrl Pts',(-22.6357892519738,-14.5131789291324,
113.99844012914)) ;
#179944 = CARTESIAN_POINT('Ctrl Pts',(-22.6439238545744,-14.4418892785907,
114.023216814566)) ;
#179945 = CARTESIAN_POINT('Ctrl Pts',(-22.7221906575843,-14.502692884587,
114.29704932502)) ;
#179946 = CARTESIAN_POINT('Ctrl Pts',(-22.7241395691929,-14.4270502382033,
114.302985393882)) ;
#179947 = CARTESIAN_POINT('Ctrl Pts',(-22.6503357490113,-14.4270502433144,
114.327216506348)) ;
#179948 = CARTESIAN_POINT('Ctrl Pts',(-22.5765319288297,-14.4270502484255,
114.351447618814)) ;
#179949 = CARTESIAN_POINT('Ctrl Pts',(-22.5745830172211,-14.5026928948091,
114.345511549952)) ;
#179950 = CARTESIAN_POINT('Ctrl Pts',(-22.5726341056125,-14.5783355411928,
114.339575481091)) ;
#179951 = CARTESIAN_POINT('Ctrl Pts',(-22.6464379257941,-14.5783355360817,
114.315344368625)) ;
#179952 = CARTESIAN_POINT('Ctrl Pts',(-22.7202417459757,-14.5783355309706,
114.291113256159)) ;
#179953 = CARTESIAN_POINT('Ctrl Pts',(-22.7221906575843,-14.502692884587,
114.29704932502)) ;
#179954 = CARTESIAN_POINT('Ctrl Pts',(-22.8020413108005,-14.4862255258319,
114.575584821507)) ;
#179955 = CARTESIAN_POINT('Ctrl Pts',(-22.7976870656786,-14.4116185668452,
114.562322492106)) ;
#179956 = CARTESIAN_POINT('Ctrl Pts',(-22.7238832430576,-14.4116185533067,
114.586553597142)) ;
#179957 = CARTESIAN_POINT('Ctrl Pts',(-22.6500794204367,-14.4116185397681,
114.610784702179)) ;
#179958 = CARTESIAN_POINT('Ctrl Pts',(-22.6544336655587,-14.4862254987549,
114.62404703158)) ;
#179959 = CARTESIAN_POINT('Ctrl Pts',(-22.6587879106807,-14.5608324577416,
114.637309360981)) ;
#179960 = CARTESIAN_POINT('Ctrl Pts',(-22.7325917333016,-14.5608324712802,
114.613078255944)) ;
#179961 = CARTESIAN_POINT('Ctrl Pts',(-22.8063955559225,-14.5608324848187,
114.588847150908)) ;
#179962 = CARTESIAN_POINT('Ctrl Pts',(-22.8020413108005,-14.4862255258319,
114.575584821507)) ;
#179963 = CARTESIAN_POINT('Ctrl Pts',(-22.877609829832,-14.3934141564473,
114.841215988645)) ;
#179964 = CARTESIAN_POINT('Ctrl Pts',(-22.867238975887,-14.3251742595679,
114.809628039706)) ;
#179965 = CARTESIAN_POINT('Ctrl Pts',(-22.7934351490755,-14.325174232371,
114.833859131978)) ;
#179966 = CARTESIAN_POINT('Ctrl Pts',(-22.719631322264,-14.3251742051741,
114.858090224251)) ;
#179967 = CARTESIAN_POINT('Ctrl Pts',(-22.730002176209,-14.3934141020535,
114.889678173191)) ;
#179968 = CARTESIAN_POINT('Ctrl Pts',(-22.7403730301541,-14.4616539989329,
114.921266122131)) ;
#179969 = CARTESIAN_POINT('Ctrl Pts',(-22.8141768569656,-14.4616540261298,
114.897035029858)) ;
#179970 = CARTESIAN_POINT('Ctrl Pts',(-22.8879806837771,-14.4616540533267,
114.872803937585)) ;
#179971 = CARTESIAN_POINT('Ctrl Pts',(-22.877609829832,-14.3934141564473,
114.841215988645)) ;
#179972 = CARTESIAN_POINT('Ctrl Pts',(-22.9425681516689,-14.2302607448999,
115.074611405796)) ;
#179973 = CARTESIAN_POINT('Ctrl Pts',(-22.9269105859837,-14.1733086335148,
115.026920986085)) ;
#179974 = CARTESIAN_POINT('Ctrl Pts',(-22.8531067540947,-14.1733085993244,
115.051152062893)) ;
#179975 = CARTESIAN_POINT('Ctrl Pts',(-22.7793029222056,-14.173308565134,
115.0753831397)) ;
#179976 = CARTESIAN_POINT('Ctrl Pts',(-22.7949604878908,-14.2302606765191,
115.123073559411)) ;
#179977 = CARTESIAN_POINT('Ctrl Pts',(-22.810618053576,-14.2872127879042,
115.170763979122)) ;
#179978 = CARTESIAN_POINT('Ctrl Pts',(-22.884421885465,-14.2872128220946,
115.146532902315)) ;
#179979 = CARTESIAN_POINT('Ctrl Pts',(-22.9582257173541,-14.287212856285,
115.122301825507)) ;
#179980 = CARTESIAN_POINT('Ctrl Pts',(-22.9425681516689,-14.2302607448999,
115.074611405796)) ;
#179981 = CARTESIAN_POINT('Ctrl Pts',(-22.9912511714667,-14.0081666908763,
115.258483536822)) ;
#179982 = CARTESIAN_POINT('Ctrl Pts',(-22.9714340856062,-13.9666350467411,
115.198123889987)) ;
#179983 = CARTESIAN_POINT('Ctrl Pts',(-22.8976302488478,-13.9666350124539,
115.222354951962)) ;
#179984 = CARTESIAN_POINT('Ctrl Pts',(-22.8238264120893,-13.9666349781666,
115.246586013938)) ;
#179985 = CARTESIAN_POINT('Ctrl Pts',(-22.8436434979498,-14.0081666223018,
115.306945660774)) ;
#179986 = CARTESIAN_POINT('Ctrl Pts',(-22.8634605838102,-14.0496982664369,
115.36730530761)) ;
#179987 = CARTESIAN_POINT('Ctrl Pts',(-22.9372644205687,-14.0496983007242,
115.343074245634)) ;
#179988 = CARTESIAN_POINT('Ctrl Pts',(-23.0110682573271,-14.0496983350115,
115.318843183658)) ;
#179989 = CARTESIAN_POINT('Ctrl Pts',(-22.9912511714667,-14.0081666908763,
115.258483536822)) ;
#179990 = CARTESIAN_POINT('Ctrl Pts',(-23.0192337790016,-13.7466548362381,
115.378918754356)) ;
#179991 = CARTESIAN_POINT('Ctrl Pts',(-22.9967045463713,-13.7233199580348,
115.31029834618)) ;
#179992 = CARTESIAN_POINT('Ctrl Pts',(-22.9229007059932,-13.7233199251522,
115.334529397131)) ;
#179993 = CARTESIAN_POINT('Ctrl Pts',(-22.849096865615,-13.7233198922696,
115.358760448081)) ;
#179994 = CARTESIAN_POINT('Ctrl Pts',(-22.8716260982453,-13.7466547704729,
115.427380856258)) ;
#179995 = CARTESIAN_POINT('Ctrl Pts',(-22.8941553308756,-13.7699896486762,
115.496001264434)) ;
#179996 = CARTESIAN_POINT('Ctrl Pts',(-22.9679591712538,-13.7699896815587,
115.471770213484)) ;
#179997 = CARTESIAN_POINT('Ctrl Pts',(-23.041763011632,-13.7699897144413,
115.447539162533)) ;
#179998 = CARTESIAN_POINT('Ctrl Pts',(-23.0192337790016,-13.7466548362381,
115.378918754356)) ;
#179999 = CARTESIAN_POINT('Ctrl Pts',(-23.0243744063994,-13.4587847124533,
115.430169417964)) ;
#180000 = CARTESIAN_POINT('Ctrl Pts',(-23.0007154115326,-13.4555144548359,
115.358107936487)) ;
#180001 = CARTESIAN_POINT('Ctrl Pts',(-22.9269115681353,-13.4555144300918,
115.382338978242)) ;
#180002 = CARTESIAN_POINT('Ctrl Pts',(-22.8531077247379,-13.4555144053477,
115.406570019997)) ;
#180003 = CARTESIAN_POINT('Ctrl Pts',(-22.8767667196047,-13.4587846629652,
115.478631501474)) ;
#180004 = CARTESIAN_POINT('Ctrl Pts',(-22.9004257144714,-13.4620549205826,
115.550692982951)) ;
#180005 = CARTESIAN_POINT('Ctrl Pts',(-22.9742295578688,-13.4620549453267,
115.526461941196)) ;
#180006 = CARTESIAN_POINT('Ctrl Pts',(-23.0480334012661,-13.4620549700708,
115.502230899441)) ;
#180007 = CARTESIAN_POINT('Ctrl Pts',(-23.0243744063994,-13.4587847124533,
115.430169417964)) ;
#180008 = CARTESIAN_POINT('Ctrl Pts',(-23.0049652251957,-13.1685102080527,
115.4065743669)) ;
#180009 = CARTESIAN_POINT('Ctrl Pts',(-22.9818905294018,-13.1855034690251,
115.336292566279)) ;
#180010 = CARTESIAN_POINT('Ctrl Pts',(-22.908086684634,-13.1855034529917,
115.36052360386)) ;
#180011 = CARTESIAN_POINT('Ctrl Pts',(-22.8342828398661,-13.1855034369582,
115.38475464144)) ;
#180012 = CARTESIAN_POINT('Ctrl Pts',(-22.85735753566,-13.1685101759858,115.455036442061)) ;
#180013 = CARTESIAN_POINT('Ctrl Pts',(-22.8804322314538,-13.1515169150133,
115.525318242682)) ;
#180014 = CARTESIAN_POINT('Ctrl Pts',(-22.9542360762216,-13.1515169310468,
115.501087205101)) ;
#180015 = CARTESIAN_POINT('Ctrl Pts',(-23.0280399209895,-13.1515169470802,
115.476856167521)) ;
#180016 = CARTESIAN_POINT('Ctrl Pts',(-23.0049652251957,-13.1685102080527,
115.4065743669)) ;
#180017 = CARTESIAN_POINT('Ctrl Pts',(-22.9622751071858,-12.8978336872395,
115.311834565575)) ;
#180018 = CARTESIAN_POINT('Ctrl Pts',(-22.9414163104123,-12.9337522455578,
115.248302035944)) ;
#180019 = CARTESIAN_POINT('Ctrl Pts',(-22.8676124651999,-12.9337522361366,
115.272533072171)) ;
#180020 = CARTESIAN_POINT('Ctrl Pts',(-22.7938086199876,-12.9337522267154,
115.296764108397)) ;
#180021 = CARTESIAN_POINT('Ctrl Pts',(-22.814667416761,-12.897833668397,115.360296638028)) ;
#180022 = CARTESIAN_POINT('Ctrl Pts',(-22.8355262135344,-12.8619151100786,
115.423829167659)) ;
#180023 = CARTESIAN_POINT('Ctrl Pts',(-22.9093300587468,-12.8619151194999,
115.399598131433)) ;
#180024 = CARTESIAN_POINT('Ctrl Pts',(-22.9831339039592,-12.8619151289211,
115.375367095206)) ;
#180025 = CARTESIAN_POINT('Ctrl Pts',(-22.9622751071858,-12.8978336872395,
115.311834565575)) ;
#180026 = CARTESIAN_POINT('Ctrl Pts',(-22.8977448880343,-12.6619537350285,
115.150913911777)) ;
#180027 = CARTESIAN_POINT('Ctrl Pts',(-22.8806231861635,-12.7143974709413,
115.098763970377)) ;
#180028 = CARTESIAN_POINT('Ctrl Pts',(-22.8068193417578,-12.714397468419,
115.12299500906)) ;
#180029 = CARTESIAN_POINT('Ctrl Pts',(-22.7330154973522,-12.7143974658967,
115.147226047744)) ;
#180030 = CARTESIAN_POINT('Ctrl Pts',(-22.750137199223,-12.6619537299839,
115.199375989144)) ;
#180031 = CARTESIAN_POINT('Ctrl Pts',(-22.7672589010938,-12.6095099940711,
115.251525930544)) ;
#180032 = CARTESIAN_POINT('Ctrl Pts',(-22.8410627454994,-12.6095099965934,
115.22729489186)) ;
#180033 = CARTESIAN_POINT('Ctrl Pts',(-22.9148665899051,-12.6095099991157,
115.203063853177)) ;
#180034 = CARTESIAN_POINT('Ctrl Pts',(-22.8977448880343,-12.6619537350285,
115.150913911777)) ;
#180035 = CARTESIAN_POINT('Ctrl Pts',(-22.8158701194052,-12.4816257056073,
114.937014037923)) ;
#180036 = CARTESIAN_POINT('Ctrl Pts',(-22.803705693731,-12.5467399887244,
114.899963160045)) ;
#180037 = CARTESIAN_POINT('Ctrl Pts',(-22.7299018503216,-12.5467399890346,
114.924194201763)) ;
#180038 = CARTESIAN_POINT('Ctrl Pts',(-22.6560980069122,-12.5467399893448,
114.948425243481)) ;
#180039 = CARTESIAN_POINT('Ctrl Pts',(-22.6682624325864,-12.4816257062277,
114.985476121359)) ;
#180040 = CARTESIAN_POINT('Ctrl Pts',(-22.6804268582606,-12.4165114231106,
115.022526999237)) ;
#180041 = CARTESIAN_POINT('Ctrl Pts',(-22.75423070167,-12.4165114228005,114.998295957519)) ;
#180042 = CARTESIAN_POINT('Ctrl Pts',(-22.8280345450794,-12.4165114224903,
114.974064915801)) ;
#180043 = CARTESIAN_POINT('Ctrl Pts',(-22.8158701194052,-12.4816257056073,
114.937014037923)) ;
#180044 = CARTESIAN_POINT('Ctrl Pts',(-22.7221314995921,-12.3684889471066,
114.686813418536)) ;
#180045 = CARTESIAN_POINT('Ctrl Pts',(-22.7157636589691,-12.441600008621,
114.667418003494)) ;
#180046 = CARTESIAN_POINT('Ctrl Pts',(-22.6419598163146,-12.441600009445,
114.691649047512)) ;
#180047 = CARTESIAN_POINT('Ctrl Pts',(-22.5681559736601,-12.4416000102689,
114.715880091529)) ;
#180048 = CARTESIAN_POINT('Ctrl Pts',(-22.5745238142832,-12.3684889487544,
114.735275506571)) ;
#180049 = CARTESIAN_POINT('Ctrl Pts',(-22.5808916549062,-12.2953778872399,
114.754670921612)) ;
#180050 = CARTESIAN_POINT('Ctrl Pts',(-22.6546954975606,-12.295377886416,
114.730439877594)) ;
#180051 = CARTESIAN_POINT('Ctrl Pts',(-22.7284993402151,-12.2953778855921,
114.706208833577)) ;
#180052 = CARTESIAN_POINT('Ctrl Pts',(-22.7221314995921,-12.3684889471066,
114.686813418536)) ;
#180053 = CARTESIAN_POINT('Ctrl Pts',(-22.6211642213523,-12.3299903879882,
114.414896154153)) ;
#180054 = CARTESIAN_POINT('Ctrl Pts',(-22.6211005272298,-12.4058988295515,
114.414702152198)) ;
#180055 = CARTESIAN_POINT('Ctrl Pts',(-22.547296684874,-12.4058988295036,
114.438933197125)) ;
#180056 = CARTESIAN_POINT('Ctrl Pts',(-22.4734928425182,-12.4058988294557,
114.463164242052)) ;
#180057 = CARTESIAN_POINT('Ctrl Pts',(-22.4735565366407,-12.3299903878923,
114.463358244007)) ;
#180058 = CARTESIAN_POINT('Ctrl Pts',(-22.4736202307632,-12.254081946329,
114.463552245962)) ;
#180059 = CARTESIAN_POINT('Ctrl Pts',(-22.547424073119,-12.2540819463769,
114.439321201035)) ;
#180060 = CARTESIAN_POINT('Ctrl Pts',(-22.6212279154748,-12.2540819464249,
114.415090156108)) ;
#180061 = CARTESIAN_POINT('Ctrl Pts',(-22.6211642213523,-12.3299903879882,
114.414896154153)) ;
#180062 = CARTESIAN_POINT('Ctrl Pts',(-22.5210459323926,-12.3696139932957,
114.145284395622)) ;
#180063 = CARTESIAN_POINT('Ctrl Pts',(-22.5272419402638,-12.4428670872802,
114.164156435911)) ;
#180064 = CARTESIAN_POINT('Ctrl Pts',(-22.4534380974035,-12.4428670865975,
114.188387479302)) ;
#180065 = CARTESIAN_POINT('Ctrl Pts',(-22.3796342545432,-12.4428670859149,
114.212618522693)) ;
#180066 = CARTESIAN_POINT('Ctrl Pts',(-22.373438246672,-12.3696139919303,
114.193746482403)) ;
#180067 = CARTESIAN_POINT('Ctrl Pts',(-22.3672422388009,-12.2963608979458,
114.174874442114)) ;
#180068 = CARTESIAN_POINT('Ctrl Pts',(-22.4410460816612,-12.2963608986285,
114.150643398723)) ;
#180069 = CARTESIAN_POINT('Ctrl Pts',(-22.5148499245215,-12.2963608993112,
114.126412355333)) ;
#180070 = CARTESIAN_POINT('Ctrl Pts',(-22.5210459323926,-12.3696139932957,
114.145284395622)) ;
#180071 = CARTESIAN_POINT('Ctrl Pts',(-22.4270329126327,-12.4839372794238,
113.894388923213)) ;
#180072 = CARTESIAN_POINT('Ctrl Pts',(-22.4390689464251,-12.5493150647165,
113.931048740115)) ;
#180073 = CARTESIAN_POINT('Ctrl Pts',(-22.3652651026278,-12.5493150649477,
113.955279780652)) ;
#180074 = CARTESIAN_POINT('Ctrl Pts',(-22.2914612588304,-12.549315065179,
113.979510821188)) ;
#180075 = CARTESIAN_POINT('Ctrl Pts',(-22.279425225038,-12.4839372798862,
113.942851004286)) ;
#180076 = CARTESIAN_POINT('Ctrl Pts',(-22.2673891912455,-12.4185594945934,
113.906191187384)) ;
#180077 = CARTESIAN_POINT('Ctrl Pts',(-22.3411930350429,-12.4185594943622,
113.881960146848)) ;
#180078 = CARTESIAN_POINT('Ctrl Pts',(-22.4149968788402,-12.418559494131,
113.857729106311)) ;
#180079 = CARTESIAN_POINT('Ctrl Pts',(-22.4270329126327,-12.4839372794238,
113.894388923213)) ;
#180080 = CARTESIAN_POINT('Ctrl Pts',(-22.3450439580957,-12.6667316342934,
113.680343028654)) ;
#180081 = CARTESIAN_POINT('Ctrl Pts',(-22.3620843484137,-12.7194414647668,
113.73224530796)) ;
#180082 = CARTESIAN_POINT('Ctrl Pts',(-22.2882805032508,-12.7194414698136,
113.756476344337)) ;
#180083 = CARTESIAN_POINT('Ctrl Pts',(-22.2144766580878,-12.7194414748605,
113.780707380714)) ;
#180084 = CARTESIAN_POINT('Ctrl Pts',(-22.1974362677697,-12.6667316443871,
113.728805101408)) ;
#180085 = CARTESIAN_POINT('Ctrl Pts',(-22.1803958774517,-12.6140218139138,
113.676902822102)) ;
#180086 = CARTESIAN_POINT('Ctrl Pts',(-22.2541997226147,-12.6140218088669,
113.652671785725)) ;
#180087 = CARTESIAN_POINT('Ctrl Pts',(-22.3280035677777,-12.6140218038201,
113.628440749348)) ;
#180088 = CARTESIAN_POINT('Ctrl Pts',(-22.3450439580957,-12.6667316342934,
113.680343028654)) ;
#180089 = CARTESIAN_POINT('Ctrl Pts',(-22.2812994602008,-12.9020313562946,
113.521591306162)) ;
#180090 = CARTESIAN_POINT('Ctrl Pts',(-22.3020828222175,-12.9383882322268,
113.584894073218)) ;
#180091 = CARTESIAN_POINT('Ctrl Pts',(-22.2282789766405,-12.9383882439588,
113.609125108335)) ;
#180092 = CARTESIAN_POINT('Ctrl Pts',(-22.1544751310636,-12.9383882556908,
113.633356143451)) ;
#180093 = CARTESIAN_POINT('Ctrl Pts',(-22.133691769047,-12.9020313797586,
113.570053376394)) ;
#180094 = CARTESIAN_POINT('Ctrl Pts',(-22.1129084070303,-12.8656745038264,
113.506750609338)) ;
#180095 = CARTESIAN_POINT('Ctrl Pts',(-22.1867122526073,-12.8656744920944,
113.482519574222)) ;
#180096 = CARTESIAN_POINT('Ctrl Pts',(-22.2605160981842,-12.8656744803624,
113.458288539106)) ;
#180097 = CARTESIAN_POINT('Ctrl Pts',(-22.2812994602008,-12.9020313562946,
113.521591306162)) ;
#180098 = CARTESIAN_POINT('Ctrl Pts',(-22.2388473261469,-13.1740426154344,
113.427694180976)) ;
#180099 = CARTESIAN_POINT('Ctrl Pts',(-22.2618922493966,-13.1914596717363,
113.497885298515)) ;
#180100 = CARTESIAN_POINT('Ctrl Pts',(-22.1880884043741,-13.1914596914773,
113.52211633532)) ;
#180101 = CARTESIAN_POINT('Ctrl Pts',(-22.1142845593517,-13.1914597112182,
113.546347372125)) ;
#180102 = CARTESIAN_POINT('Ctrl Pts',(-22.091239636102,-13.1740426549163,
113.476156254586)) ;
#180103 = CARTESIAN_POINT('Ctrl Pts',(-22.0681947128524,-13.1566255986144,
113.405965137047)) ;
#180104 = CARTESIAN_POINT('Ctrl Pts',(-22.1419985578748,-13.1566255788734,
113.381734100242)) ;
#180105 = CARTESIAN_POINT('Ctrl Pts',(-22.2158024028973,-13.1566255591325,
113.357503063437)) ;
#180106 = CARTESIAN_POINT('Ctrl Pts',(-22.2388473261469,-13.1740426154344,
113.427694180976)) ;
#180107 = CARTESIAN_POINT('Ctrl Pts',(-22.2199943655419,-13.4634545824485,
113.40566955685)) ;
#180108 = CARTESIAN_POINT('Ctrl Pts',(-22.243656437071,-13.4606896668886,
113.47774040833)) ;
#180109 = CARTESIAN_POINT('Ctrl Pts',(-22.1698525937983,-13.4606896946661,
113.501971450465)) ;
#180110 = CARTESIAN_POINT('Ctrl Pts',(-22.0960487505255,-13.4606897224437,
113.526202492599)) ;
#180111 = CARTESIAN_POINT('Ctrl Pts',(-22.0723866789964,-13.4634546380036,
113.454131641119)) ;
#180112 = CARTESIAN_POINT('Ctrl Pts',(-22.0487246074673,-13.4662195535635,
113.382060789639)) ;
#180113 = CARTESIAN_POINT('Ctrl Pts',(-22.12252845074,-13.466219525786,113.357829747505)) ;
#180114 = CARTESIAN_POINT('Ctrl Pts',(-22.1963322940127,-13.4662194980085,
113.33359870537)) ;
#180115 = CARTESIAN_POINT('Ctrl Pts',(-22.2199943655419,-13.4634545824485,
113.40566955685)) ;
#180116 = CARTESIAN_POINT('Ctrl Pts',(-22.2254048356507,-13.7505708131454,
113.45766775839)) ;
#180117 = CARTESIAN_POINT('Ctrl Pts',(-22.2479884314305,-13.7277551955946,
113.526453746576)) ;
#180118 = CARTESIAN_POINT('Ctrl Pts',(-22.1741845912889,-13.7277552307989,
113.550684798247)) ;
#180119 = CARTESIAN_POINT('Ctrl Pts',(-22.1003807511473,-13.7277552660031,
113.574915849919)) ;
#180120 = CARTESIAN_POINT('Ctrl Pts',(-22.0777971553675,-13.7505708835539,
113.506129861733)) ;
#180121 = CARTESIAN_POINT('Ctrl Pts',(-22.0552135595877,-13.7733865011047,
113.437343873547)) ;
#180122 = CARTESIAN_POINT('Ctrl Pts',(-22.1290173997293,-13.7733864659004,
113.413112821876)) ;
#180123 = CARTESIAN_POINT('Ctrl Pts',(-22.2028212398709,-13.7733864306961,
113.388881770204)) ;
#180124 = CARTESIAN_POINT('Ctrl Pts',(-22.2254048356507,-13.7505708131454,
113.45766775839)) ;
#180125 = CARTESIAN_POINT('Ctrl Pts',(-22.253988225315,-14.0133363300327,
113.580184190739)) ;
#180126 = CARTESIAN_POINT('Ctrl Pts',(-22.2738750852953,-13.9721415095329,
113.64075635663)) ;
#180127 = CARTESIAN_POINT('Ctrl Pts',(-22.2000712494337,-13.9721415478717,
113.664987421337)) ;
#180128 = CARTESIAN_POINT('Ctrl Pts',(-22.126267413572,-13.9721415862106,
113.689218486045)) ;
#180129 = CARTESIAN_POINT('Ctrl Pts',(-22.1063805535917,-14.0133364067105,
113.628646320154)) ;
#180130 = CARTESIAN_POINT('Ctrl Pts',(-22.0864936936113,-14.0545312272103,
113.568074154263)) ;
#180131 = CARTESIAN_POINT('Ctrl Pts',(-22.160297529473,-14.0545311888715,
113.543843089555)) ;
#180132 = CARTESIAN_POINT('Ctrl Pts',(-22.2341013653346,-14.0545311505326,
113.519612024848)) ;
#180133 = CARTESIAN_POINT('Ctrl Pts',(-22.253988225315,-14.0133363300327,
113.580184190739)) ;
#180134 = CARTESIAN_POINT('Ctrl Pts',(-22.302884463881,-14.2335678065818,
113.764575325811)) ;
#180135 = CARTESIAN_POINT('Ctrl Pts',(-22.3186524020933,-14.1769371406859,
113.812601920414)) ;
#180136 = CARTESIAN_POINT('Ctrl Pts',(-22.2448485711463,-14.1769371770333,
113.836833000091)) ;
#180137 = CARTESIAN_POINT('Ctrl Pts',(-22.1710447401993,-14.1769372133807,
113.861064079767)) ;
#180138 = CARTESIAN_POINT('Ctrl Pts',(-22.155276801987,-14.2335678792767,
113.813037485163)) ;
#180139 = CARTESIAN_POINT('Ctrl Pts',(-22.1395088637747,-14.2901985451726,
113.76501089056)) ;
#180140 = CARTESIAN_POINT('Ctrl Pts',(-22.2133126947217,-14.2901985088252,
113.740779810884)) ;
#180141 = CARTESIAN_POINT('Ctrl Pts',(-22.2871165256687,-14.2901984724778,
113.716548731207)) ;
#180142 = CARTESIAN_POINT('Ctrl Pts',(-22.302884463881,-14.2335678065818,
113.764575325811)) ;
#180143 = CARTESIAN_POINT('Ctrl Pts',(-22.3681132301931,-14.3958087768564,
113.998825699408)) ;
#180144 = CARTESIAN_POINT('Ctrl Pts',(-22.3786137764085,-14.3277685970779,
114.030808667693)) ;
#180145 = CARTESIAN_POINT('Ctrl Pts',(-22.304809950723,-14.3277686257104,
114.055039763396)) ;
#180146 = CARTESIAN_POINT('Ctrl Pts',(-22.2310061250376,-14.327768654343,
114.079270859098)) ;
#180147 = CARTESIAN_POINT('Ctrl Pts',(-22.2205055788222,-14.3958088341215,
114.047287890812)) ;
#180148 = CARTESIAN_POINT('Ctrl Pts',(-22.2100050326069,-14.4638490139001,
114.015304922527)) ;
#180149 = CARTESIAN_POINT('Ctrl Pts',(-22.2838088582923,-14.4638489852675,
113.991073826824)) ;
#180150 = CARTESIAN_POINT('Ctrl Pts',(-22.3576126839778,-14.463848956635,
113.966842731122)) ;
#180151 = CARTESIAN_POINT('Ctrl Pts',(-22.3681132301931,-14.3958087768564,
113.998825699408)) ;
#180152 = CARTESIAN_POINT('Ctrl Pts',(-22.443875331704,-14.4872051600084,
114.265066140511)) ;
#180153 = CARTESIAN_POINT('Ctrl Pts',(-22.4483673589723,-14.4126853477426,
114.278748129396)) ;
#180154 = CARTESIAN_POINT('Ctrl Pts',(-22.3745635375518,-14.4126853615341,
114.302979238089)) ;
#180155 = CARTESIAN_POINT('Ctrl Pts',(-22.3007597161312,-14.4126853753255,
114.327210346781)) ;
#180156 = CARTESIAN_POINT('Ctrl Pts',(-22.2962676888629,-14.4872051875913,
114.313528357897)) ;
#180157 = CARTESIAN_POINT('Ctrl Pts',(-22.2917756615946,-14.561724999857,
114.299846369012)) ;
#180158 = CARTESIAN_POINT('Ctrl Pts',(-22.3655794830151,-14.5617249860656,
114.275615260319)) ;
#180159 = CARTESIAN_POINT('Ctrl Pts',(-22.4393833044357,-14.5617249722742,
114.251384151627)) ;
#180160 = CARTESIAN_POINT('Ctrl Pts',(-22.443875331704,-14.4872051600084,
114.265066140511)) ;
#180161 = CARTESIAN_POINT('Ctrl Pts',(-22.5236867142171,-14.5023836342265,
114.543451391417)) ;
#180162 = CARTESIAN_POINT('Ctrl Pts',(-22.5218827377138,-14.4266966491582,
114.53795676855)) ;
#180163 = CARTESIAN_POINT('Ctrl Pts',(-22.4480789185891,-14.4266966434283,
114.562187884235)) ;
#180164 = CARTESIAN_POINT('Ctrl Pts',(-22.3742750994644,-14.4266966376984,
114.586418999921)) ;
#180165 = CARTESIAN_POINT('Ctrl Pts',(-22.3760790759678,-14.5023836227667,
114.591913622788)) ;
#180166 = CARTESIAN_POINT('Ctrl Pts',(-22.3778830524711,-14.5780706078349,
114.597408245655)) ;
#180167 = CARTESIAN_POINT('Ctrl Pts',(-22.4516868715958,-14.5780706135648,
114.573177129969)) ;
#180168 = CARTESIAN_POINT('Ctrl Pts',(-22.5254906907205,-14.5780706192947,
114.548946014284)) ;
#180169 = CARTESIAN_POINT('Ctrl Pts',(-22.5236867142171,-14.5023836342265,
114.543451391417)) ;
#180170 = CARTESIAN_POINT('Ctrl Pts',(-22.6023114828813,-14.4395233841403,
114.8185888207)) ;
#180171 = CARTESIAN_POINT('Ctrl Pts',(-22.5942777325874,-14.3681145695168,
114.794119311872)) ;
#180172 = CARTESIAN_POINT('Ctrl Pts',(-22.5204739146049,-14.3681145402781,
114.818350431036)) ;
#180173 = CARTESIAN_POINT('Ctrl Pts',(-22.4466700966224,-14.3681145110395,
114.8425815502)) ;
#180174 = CARTESIAN_POINT('Ctrl Pts',(-22.4547038469163,-14.4395233256629,
114.867051059028)) ;
#180175 = CARTESIAN_POINT('Ctrl Pts',(-22.4627375972102,-14.5109321402864,
114.891520567857)) ;
#180176 = CARTESIAN_POINT('Ctrl Pts',(-22.5365414151927,-14.510932169525,
114.867289448692)) ;
#180177 = CARTESIAN_POINT('Ctrl Pts',(-22.6103452331752,-14.5109321987637,
114.843058329528)) ;
#180178 = CARTESIAN_POINT('Ctrl Pts',(-22.6023114828813,-14.4395233841403,
114.8185888207)) ;
#180179 = CARTESIAN_POINT('Ctrl Pts',(-22.6719122092473,-14.3038981389521,
115.065942143316)) ;
#180180 = CARTESIAN_POINT('Ctrl Pts',(-22.6582758145708,-14.2418546197311,
115.024407883578)) ;
#180181 = CARTESIAN_POINT('Ctrl Pts',(-22.5844719945869,-14.2418545666607,
115.048638996647)) ;
#180182 = CARTESIAN_POINT('Ctrl Pts',(-22.5106681746031,-14.2418545135903,
115.072870109715)) ;
#180183 = CARTESIAN_POINT('Ctrl Pts',(-22.5243045692795,-14.3038980328113,
115.114404369452)) ;
#180184 = CARTESIAN_POINT('Ctrl Pts',(-22.5379409639559,-14.3659415520323,
115.15593862919)) ;
#180185 = CARTESIAN_POINT('Ctrl Pts',(-22.6117447839398,-14.3659416051027,
115.131707516122)) ;
#180186 = CARTESIAN_POINT('Ctrl Pts',(-22.6855486039237,-14.3659416581731,
115.107476403053)) ;
#180187 = CARTESIAN_POINT('Ctrl Pts',(-22.6719122092473,-14.3038981389521,
115.065942143316)) ;
#180188 = CARTESIAN_POINT('Ctrl Pts',(-22.7275755368524,-14.1052991872385,
115.270872462987)) ;
#180189 = CARTESIAN_POINT('Ctrl Pts',(-22.7093008428281,-14.057030828904,
115.215210691726)) ;
#180190 = CARTESIAN_POINT('Ctrl Pts',(-22.6354970186199,-14.0570307540221,
115.239441791928)) ;
#180191 = CARTESIAN_POINT('Ctrl Pts',(-22.5616931944116,-14.0570306791401,
115.263672892129)) ;
#180192 = CARTESIAN_POINT('Ctrl Pts',(-22.5799678884359,-14.1052990374745,
115.31933466339)) ;
#180193 = CARTESIAN_POINT('Ctrl Pts',(-22.5982425824603,-14.1535673958089,
115.37499643465)) ;
#180194 = CARTESIAN_POINT('Ctrl Pts',(-22.6720464066685,-14.1535674706909,
115.350765334449)) ;
#180195 = CARTESIAN_POINT('Ctrl Pts',(-22.7458502308768,-14.1535675455729,
115.326534234247)) ;
#180196 = CARTESIAN_POINT('Ctrl Pts',(-22.7275755368524,-14.1052991872385,
115.270872462987)) ;
#180197 = CARTESIAN_POINT('Ctrl Pts',(-22.7645650054977,-13.8563431079666,
115.419085314818)) ;
#180198 = CARTESIAN_POINT('Ctrl Pts',(-22.742945507972,-13.8253850611036,
115.353235811681)) ;
#180199 = CARTESIAN_POINT('Ctrl Pts',(-22.6691416774397,-13.8253849680989,
115.377466892621)) ;
#180200 = CARTESIAN_POINT('Ctrl Pts',(-22.5953378469074,-13.8253848750942,
115.40169797356)) ;
#180201 = CARTESIAN_POINT('Ctrl Pts',(-22.616957344433,-13.8563429219572,
115.467547476697)) ;
#180202 = CARTESIAN_POINT('Ctrl Pts',(-22.6385768419586,-13.8873009688202,
115.533396979833)) ;
#180203 = CARTESIAN_POINT('Ctrl Pts',(-22.712380672491,-13.8873010618249,
115.509165898894)) ;
#180204 = CARTESIAN_POINT('Ctrl Pts',(-22.7861845030233,-13.8873011548297,
115.484934817954)) ;
#180205 = CARTESIAN_POINT('Ctrl Pts',(-22.7645650054977,-13.8563431079666,
115.419085314818)) ;
#180206 = CARTESIAN_POINT('Ctrl Pts',(-22.7791798044281,-13.5768529523028,
115.499023031472)) ;
#180207 = CARTESIAN_POINT('Ctrl Pts',(-22.7557753098736,-13.5653624857166,
115.427736715333)) ;
#180208 = CARTESIAN_POINT('Ctrl Pts',(-22.6819714713014,-13.56536238196,115.451967771784)) ;
#180209 = CARTESIAN_POINT('Ctrl Pts',(-22.6081676327291,-13.5653622782034,
115.476198828235)) ;
#180210 = CARTESIAN_POINT('Ctrl Pts',(-22.6315721272836,-13.5768527447896,
115.547485144374)) ;
#180211 = CARTESIAN_POINT('Ctrl Pts',(-22.6549766218381,-13.5883432113757,
115.618771460513)) ;
#180212 = CARTESIAN_POINT('Ctrl Pts',(-22.7287804604104,-13.5883433151323,
115.594540404062)) ;
#180213 = CARTESIAN_POINT('Ctrl Pts',(-22.8025842989826,-13.5883434188889,
115.570309347611)) ;
#180214 = CARTESIAN_POINT('Ctrl Pts',(-22.7791798044281,-13.5768529523028,
115.499023031472)) ;
#180215 = CARTESIAN_POINT('Ctrl Pts',(-22.7697827423378,-13.2855121533732,
115.505888509514)) ;
#180216 = CARTESIAN_POINT('Ctrl Pts',(-22.7462655648333,-13.2943449974089,
115.434258979246)) ;
#180217 = CARTESIAN_POINT('Ctrl Pts',(-22.6724617173834,-13.2943448909631,
115.458490008657)) ;
#180218 = CARTESIAN_POINT('Ctrl Pts',(-22.5986578699334,-13.2943447845173,
115.482721038068)) ;
#180219 = CARTESIAN_POINT('Ctrl Pts',(-22.6221750474379,-13.2855119404815,
115.554350568336)) ;
#180220 = CARTESIAN_POINT('Ctrl Pts',(-22.6456922249424,-13.2766790964458,
115.625980098605)) ;
#180221 = CARTESIAN_POINT('Ctrl Pts',(-22.7194960723924,-13.2766792028916,
115.601749069194)) ;
#180222 = CARTESIAN_POINT('Ctrl Pts',(-22.7932999198423,-13.2766793093374,
115.577518039783)) ;
#180223 = CARTESIAN_POINT('Ctrl Pts',(-22.7697827423378,-13.2855121533732,
115.505888509514)) ;
#180224 = CARTESIAN_POINT('Ctrl Pts',(-22.736267599059,-13.0041275578471,
115.439237761638)) ;
#180225 = CARTESIAN_POINT('Ctrl Pts',(-22.714322517485,-13.0326186796293,
115.372396581896)) ;
#180226 = CARTESIAN_POINT('Ctrl Pts',(-22.6405186612293,-13.0326185795002,
115.396627584487)) ;
#180227 = CARTESIAN_POINT('Ctrl Pts',(-22.5667148049737,-13.0326184793711,
115.420858587077)) ;
#180228 = CARTESIAN_POINT('Ctrl Pts',(-22.5886598865477,-13.0041273575889,
115.487699766818)) ;
#180229 = CARTESIAN_POINT('Ctrl Pts',(-22.6106049681218,-12.9756362358068,
115.554540946559)) ;
#180230 = CARTESIAN_POINT('Ctrl Pts',(-22.6844088243775,-12.9756363359359,
115.530309943969)) ;
#180231 = CARTESIAN_POINT('Ctrl Pts',(-22.7582126806331,-12.975636436065,
115.506078941379)) ;
#180232 = CARTESIAN_POINT('Ctrl Pts',(-22.736267599059,-13.0041275578471,
115.439237761638)) ;
#180233 = CARTESIAN_POINT('Ctrl Pts',(-22.6804050530378,-12.7524010633512,
115.304496989377)) ;
#180234 = CARTESIAN_POINT('Ctrl Pts',(-22.6615950142437,-12.798508919761,
115.247204644104)) ;
#180235 = CARTESIAN_POINT('Ctrl Pts',(-22.5877911501292,-12.798508834093,
115.271435622758)) ;
#180236 = CARTESIAN_POINT('Ctrl Pts',(-22.5139872860148,-12.7985087484251,
115.295666601412)) ;
#180237 = CARTESIAN_POINT('Ctrl Pts',(-22.5327973248089,-12.7524008920153,
115.352958946684)) ;
#180238 = CARTESIAN_POINT('Ctrl Pts',(-22.551607363603,-12.7062930356055,
115.410251291957)) ;
#180239 = CARTESIAN_POINT('Ctrl Pts',(-22.6254112277175,-12.7062931212734,
115.386020313304)) ;
#180240 = CARTESIAN_POINT('Ctrl Pts',(-22.6992150918319,-12.7062932069414,
115.36178933465)) ;
#180241 = CARTESIAN_POINT('Ctrl Pts',(-22.6804050530378,-12.7524010633512,
115.304496989377)) ;
#180242 = CARTESIAN_POINT('Ctrl Pts',(-22.6049368462365,-12.5474082659178,
115.110214285938)) ;
#180243 = CARTESIAN_POINT('Ctrl Pts',(-22.5906314344715,-12.6078966446447,
115.066642307803)) ;
#180244 = CARTESIAN_POINT('Ctrl Pts',(-22.5168275643,-12.6078965805878,115.090873268007)) ;
#180245 = CARTESIAN_POINT('Ctrl Pts',(-22.4430236941285,-12.6078965165309,
115.115104228212)) ;
#180246 = CARTESIAN_POINT('Ctrl Pts',(-22.4573291058934,-12.5474081378039,
115.158676206348)) ;
#180247 = CARTESIAN_POINT('Ctrl Pts',(-22.4716345176584,-12.4869197590769,
115.202248184483)) ;
#180248 = CARTESIAN_POINT('Ctrl Pts',(-22.5454383878299,-12.4869198231338,
115.178017224278)) ;
#180249 = CARTESIAN_POINT('Ctrl Pts',(-22.6192422580014,-12.4869198871908,
115.153786264074)) ;
#180250 = CARTESIAN_POINT('Ctrl Pts',(-22.6049368462365,-12.5474082659178,
115.110214285938)) ;
#180251 = CARTESIAN_POINT('Ctrl Pts',(-22.5152721436028,-12.4057612857423,
114.872509443197)) ;
#180252 = CARTESIAN_POINT('Ctrl Pts',(-22.506473096668,-12.4762290506085,
114.845708963927)) ;
#180253 = CARTESIAN_POINT('Ctrl Pts',(-22.432669222784,-12.4762290124344,
114.869939912825)) ;
#180254 = CARTESIAN_POINT('Ctrl Pts',(-22.3588653489,-12.4762289742604,114.894170861722)) ;
#180255 = CARTESIAN_POINT('Ctrl Pts',(-22.3676643958349,-12.4057612093942,
114.920971340992)) ;
#180256 = CARTESIAN_POINT('Ctrl Pts',(-22.3764634427698,-12.3352934445281,
114.947771820262)) ;
#180257 = CARTESIAN_POINT('Ctrl Pts',(-22.4502673166537,-12.3352934827021,
114.923540871364)) ;
#180258 = CARTESIAN_POINT('Ctrl Pts',(-22.5240711905377,-12.3352935208762,
114.899309922467)) ;
#180259 = CARTESIAN_POINT('Ctrl Pts',(-22.5152721436028,-12.4057612857423,
114.872509443197)) ;
#180260 = CARTESIAN_POINT('Ctrl Pts',(-22.416477982246,-12.3361751661113,
114.607093665793)) ;
#180261 = CARTESIAN_POINT('Ctrl Pts',(-22.413828814936,-12.4116066467127,
114.599024727648)) ;
#180262 = CARTESIAN_POINT('Ctrl Pts',(-22.3400249400517,-12.4116066363173,
114.623255673499)) ;
#180263 = CARTESIAN_POINT('Ctrl Pts',(-22.2662210651673,-12.4116066259219,
114.647486619349)) ;
#180264 = CARTESIAN_POINT('Ctrl Pts',(-22.2688702324773,-12.3361751453206,
114.655555557494)) ;
#180265 = CARTESIAN_POINT('Ctrl Pts',(-22.2715193997872,-12.2607436647193,
114.663624495639)) ;
#180266 = CARTESIAN_POINT('Ctrl Pts',(-22.3453232746716,-12.2607436751146,
114.639393549788)) ;
#180267 = CARTESIAN_POINT('Ctrl Pts',(-22.4191271495559,-12.26074368551,114.615162603938)) ;
#180268 = CARTESIAN_POINT('Ctrl Pts',(-22.416477982246,-12.3361751661113,
114.607093665793)) ;
#180269 = CARTESIAN_POINT('Ctrl Pts',(-22.3151654199719,-12.3442704255669,
114.333978009921)) ;
#180270 = CARTESIAN_POINT('Ctrl Pts',(-22.318851814107,-12.4192498359007,
114.345206169785)) ;
#180271 = CARTESIAN_POINT('Ctrl Pts',(-22.2450479408706,-12.4192498519891,
114.369437120655)) ;
#180272 = CARTESIAN_POINT('Ctrl Pts',(-22.1712440676341,-12.4192498680774,
114.393668071524)) ;
#180273 = CARTESIAN_POINT('Ctrl Pts',(-22.1675576734989,-12.3442704577436,
114.38243991166)) ;
#180274 = CARTESIAN_POINT('Ctrl Pts',(-22.1638712793637,-12.2692910474097,
114.371211751796)) ;
#180275 = CARTESIAN_POINT('Ctrl Pts',(-22.2376751526002,-12.2692910313214,
114.346980800926)) ;
#180276 = CARTESIAN_POINT('Ctrl Pts',(-22.3114790258367,-12.269291015233,
114.322749850057)) ;
#180277 = CARTESIAN_POINT('Ctrl Pts',(-22.3151654199719,-12.3442704255669,
114.333978009921)) ;
#180278 = CARTESIAN_POINT('Ctrl Pts',(-22.2178317346334,-12.4291570429794,
114.072959782331)) ;
#180279 = CARTESIAN_POINT('Ctrl Pts',(-22.2275858904983,-12.4983225025168,
114.102669365496)) ;
#180280 = CARTESIAN_POINT('Ctrl Pts',(-22.1537820211615,-12.4983225412537,
114.126900328243)) ;
#180281 = CARTESIAN_POINT('Ctrl Pts',(-22.0799781518247,-12.4983225799905,
114.15113129099)) ;
#180282 = CARTESIAN_POINT('Ctrl Pts',(-22.0702239959598,-12.429157120453,
114.121421707825)) ;
#180283 = CARTESIAN_POINT('Ctrl Pts',(-22.0604698400949,-12.3599916609156,
114.09171212466)) ;
#180284 = CARTESIAN_POINT('Ctrl Pts',(-22.1342737094317,-12.3599916221787,
114.067481161913)) ;
#180285 = CARTESIAN_POINT('Ctrl Pts',(-22.2080775787685,-12.3599915834419,
114.043250199166)) ;
#180286 = CARTESIAN_POINT('Ctrl Pts',(-22.2178317346334,-12.4291570429794,
114.072959782331)) ;
#180287 = CARTESIAN_POINT('Ctrl Pts',(-22.1305576720065,-12.5849331529663,
113.842608904662)) ;
#180288 = CARTESIAN_POINT('Ctrl Pts',(-22.1456858757499,-12.6433268351206,
113.888686970688)) ;
#180289 = CARTESIAN_POINT('Ctrl Pts',(-22.0718820120717,-12.6433268905322,
113.91291795067)) ;
#180290 = CARTESIAN_POINT('Ctrl Pts',(-21.9980781483935,-12.6433269459438,
113.937148930652)) ;
#180291 = CARTESIAN_POINT('Ctrl Pts',(-21.98294994465,-12.5849332637895,113.891070864627)) ;
#180292 = CARTESIAN_POINT('Ctrl Pts',(-21.9678217409065,-12.5265395816352,
113.844992798601)) ;
#180293 = CARTESIAN_POINT('Ctrl Pts',(-22.0416256045847,-12.5265395262236,
113.820761818619)) ;
#180294 = CARTESIAN_POINT('Ctrl Pts',(-22.115429468263,-12.526539470812,113.796530838636)) ;
#180295 = CARTESIAN_POINT('Ctrl Pts',(-22.1305576720065,-12.5849331529663,
113.842608904662)) ;
#180296 = CARTESIAN_POINT('Ctrl Pts',(-22.0589049961337,-12.8005108515807,
113.659850775532)) ;
#180297 = CARTESIAN_POINT('Ctrl Pts',(-22.0783245226493,-12.8439413739947,
113.718999518458)) ;
#180298 = CARTESIAN_POINT('Ctrl Pts',(-22.0045206655792,-12.8439414387627,
113.743230518568)) ;
#180299 = CARTESIAN_POINT('Ctrl Pts',(-21.9307168085092,-12.8439415035308,
113.767461518678)) ;
#180300 = CARTESIAN_POINT('Ctrl Pts',(-21.9112972819936,-12.8005109811168,
113.708312775751)) ;
#180301 = CARTESIAN_POINT('Ctrl Pts',(-21.8918777554779,-12.7570804587029,
113.649164032825)) ;
#180302 = CARTESIAN_POINT('Ctrl Pts',(-21.965681612548,-12.7570803939349,
113.624933032715)) ;
#180303 = CARTESIAN_POINT('Ctrl Pts',(-22.039485469618,-12.7570803291668,
113.600702032605)) ;
#180304 = CARTESIAN_POINT('Ctrl Pts',(-22.0589049961337,-12.8005108515807,
113.659850775532)) ;
#180305 = CARTESIAN_POINT('Ctrl Pts',(-22.0073169664416,-13.060269126664,
113.538192775077)) ;
#180306 = CARTESIAN_POINT('Ctrl Pts',(-22.0296337589836,-13.0856291470037,
113.606166122998)) ;
#180307 = CARTESIAN_POINT('Ctrl Pts',(-21.9558299085615,-13.0856292137402,
113.630397143356)) ;
#180308 = CARTESIAN_POINT('Ctrl Pts',(-21.8820260581393,-13.0856292804768,
113.654628163715)) ;
#180309 = CARTESIAN_POINT('Ctrl Pts',(-21.8597092655973,-13.0602692601371,
113.586654815794)) ;
#180310 = CARTESIAN_POINT('Ctrl Pts',(-21.8373924730553,-13.0349092397974,
113.518681467873)) ;
#180311 = CARTESIAN_POINT('Ctrl Pts',(-21.9111963234774,-13.0349091730608,
113.494450447515)) ;
#180312 = CARTESIAN_POINT('Ctrl Pts',(-21.9850001738996,-13.0349091063243,
113.470219427156)) ;
#180313 = CARTESIAN_POINT('Ctrl Pts',(-22.0073169664416,-13.060269126664,
113.538192775077)) ;
#180314 = CARTESIAN_POINT('Ctrl Pts',(-21.978691089474,-13.3453693583979,
113.486439374298)) ;
#180315 = CARTESIAN_POINT('Ctrl Pts',(-22.0023070600683,-13.3508620232142,
113.558369809098)) ;
#180316 = CARTESIAN_POINT('Ctrl Pts',(-21.9285032156018,-13.3508620856039,
113.582600847596)) ;
#180317 = CARTESIAN_POINT('Ctrl Pts',(-21.8546993711354,-13.3508621479936,
113.606831886095)) ;
#180318 = CARTESIAN_POINT('Ctrl Pts',(-21.8310834005412,-13.3453694831773,
113.534901451295)) ;
#180319 = CARTESIAN_POINT('Ctrl Pts',(-21.8074674299469,-13.3398768183609,
113.462971016496)) ;
#180320 = CARTESIAN_POINT('Ctrl Pts',(-21.8812712744133,-13.3398767559712,
113.438739977997)) ;
#180321 = CARTESIAN_POINT('Ctrl Pts',(-21.9550751188797,-13.3398766935815,
113.414508939498)) ;
#180322 = CARTESIAN_POINT('Ctrl Pts',(-21.978691089474,-13.3453693583979,
113.486439374298)) ;
#180323 = CARTESIAN_POINT('Ctrl Pts',(-21.9743140972656,-13.6361640667827,
113.508607131723)) ;
#180324 = CARTESIAN_POINT('Ctrl Pts',(-21.9975369390037,-13.6213614987656,
113.57934015963)) ;
#180325 = CARTESIAN_POINT('Ctrl Pts',(-21.9237330991818,-13.6213615511211,
113.603571212275)) ;
#180326 = CARTESIAN_POINT('Ctrl Pts',(-21.84992925936,-13.6213616034766,113.62780226492)) ;
#180327 = CARTESIAN_POINT('Ctrl Pts',(-21.8267064176218,-13.6361641714938,
113.557069237013)) ;
#180328 = CARTESIAN_POINT('Ctrl Pts',(-21.8034835758837,-13.6509667395109,
113.486336209106)) ;
#180329 = CARTESIAN_POINT('Ctrl Pts',(-21.8772874157056,-13.6509666871554,
113.462105156461)) ;
#180330 = CARTESIAN_POINT('Ctrl Pts',(-21.9510912555274,-13.6509666347999,
113.437874103816)) ;
#180331 = CARTESIAN_POINT('Ctrl Pts',(-21.9743140972656,-13.6361640667827,
113.508607131723)) ;
#180332 = CARTESIAN_POINT('Ctrl Pts',(-21.9936997725589,-13.9104324089111,
113.603035067072)) ;
#180333 = CARTESIAN_POINT('Ctrl Pts',(-22.0148720614655,-13.8764575771015,
113.667522442062)) ;
#180334 = CARTESIAN_POINT('Ctrl Pts',(-21.9410682247111,-13.8764576175232,
113.69175350405)) ;
#180335 = CARTESIAN_POINT('Ctrl Pts',(-21.8672643879568,-13.8764576579448,
113.715984566039)) ;
#180336 = CARTESIAN_POINT('Ctrl Pts',(-21.8460920990502,-13.9104324897545,
113.651497191049)) ;
#180337 = CARTESIAN_POINT('Ctrl Pts',(-21.8249198101436,-13.9444073215641,
113.587009816059)) ;
#180338 = CARTESIAN_POINT('Ctrl Pts',(-21.8987236468979,-13.9444072811424,
113.56277875407)) ;
#180339 = CARTESIAN_POINT('Ctrl Pts',(-21.9725274836523,-13.9444072407208,
113.538547692082)) ;
#180340 = CARTESIAN_POINT('Ctrl Pts',(-21.9936997725589,-13.9104324089111,
113.603035067072)) ;
#180341 = CARTESIAN_POINT('Ctrl Pts',(-22.0347431039267,-14.1501784561149,
113.763511943349)) ;
#180342 = CARTESIAN_POINT('Ctrl Pts',(-22.0523478858651,-14.0994124816197,
113.817133267897)) ;
#180343 = CARTESIAN_POINT('Ctrl Pts',(-21.9785440504179,-14.0994125084155,
113.841364333867)) ;
#180344 = CARTESIAN_POINT('Ctrl Pts',(-21.9047402149707,-14.0994125352114,
113.865595399836)) ;
#180345 = CARTESIAN_POINT('Ctrl Pts',(-21.8871354330323,-14.1501785097066,
113.811974075288)) ;
#180346 = CARTESIAN_POINT('Ctrl Pts',(-21.8695306510939,-14.2009444842018,
113.75835275074)) ;
#180347 = CARTESIAN_POINT('Ctrl Pts',(-21.9433344865411,-14.200944457406,
113.73412168477)) ;
#180348 = CARTESIAN_POINT('Ctrl Pts',(-22.0171383219884,-14.2009444306102,
113.709890618801)) ;
#180349 = CARTESIAN_POINT('Ctrl Pts',(-22.0347431039267,-14.1501784561149,
113.763511943349)) ;
#180350 = CARTESIAN_POINT('Ctrl Pts',(-22.0939751521265,-14.3377944456025,
113.979478469494)) ;
#180351 = CARTESIAN_POINT('Ctrl Pts',(-22.1067351330108,-14.273851283079,
114.018343311917)) ;
#180352 = CARTESIAN_POINT('Ctrl Pts',(-22.0329312970307,-14.2738512972119,
114.042574376263)) ;
#180353 = CARTESIAN_POINT('Ctrl Pts',(-21.9591274610505,-14.2738513113447,
114.06680544061)) ;
#180354 = CARTESIAN_POINT('Ctrl Pts',(-21.9463674801662,-14.3377944738682,
114.027940598186)) ;
#180355 = CARTESIAN_POINT('Ctrl Pts',(-21.9336074992819,-14.4017376363917,
113.989075755763)) ;
#180356 = CARTESIAN_POINT('Ctrl Pts',(-22.0074113352621,-14.4017376222589,
113.964844691417)) ;
#180357 = CARTESIAN_POINT('Ctrl Pts',(-22.0812151712422,-14.4017376081261,
113.94061362707)) ;
#180358 = CARTESIAN_POINT('Ctrl Pts',(-22.0939751521265,-14.3377944456025,
113.979478469494)) ;
#180359 = CARTESIAN_POINT('Ctrl Pts',(-22.1659929301065,-14.4588735568458,
114.234265903067)) ;
#180360 = CARTESIAN_POINT('Ctrl Pts',(-22.1730103976931,-14.3863794182977,
114.255639976685)) ;
#180361 = CARTESIAN_POINT('Ctrl Pts',(-22.0992065603188,-14.3863794234914,
114.279871036785)) ;
#180362 = CARTESIAN_POINT('Ctrl Pts',(-22.0254027229444,-14.3863794286851,
114.304102096885)) ;
#180363 = CARTESIAN_POINT('Ctrl Pts',(-22.0183852553577,-14.4588735672332,
114.282728023267)) ;
#180364 = CARTESIAN_POINT('Ctrl Pts',(-22.011367787771,-14.5313677057812,
114.261353949649)) ;
#180365 = CARTESIAN_POINT('Ctrl Pts',(-22.0851716251454,-14.5313677005875,
114.237122889549)) ;
#180366 = CARTESIAN_POINT('Ctrl Pts',(-22.1589754625198,-14.5313676953939,
114.212891829449)) ;
#180367 = CARTESIAN_POINT('Ctrl Pts',(-22.1659929301065,-14.4588735568458,
114.234265903067)) ;
#180368 = CARTESIAN_POINT('Ctrl Pts',(-22.2451385688619,-14.5056122473976,
114.510797193633)) ;
#180369 = CARTESIAN_POINT('Ctrl Pts',(-22.2459063570101,-14.4297450127553,
114.513135752203)) ;
#180370 = CARTESIAN_POINT('Ctrl Pts',(-22.1721025175833,-14.4297450124761,
114.537366806052)) ;
#180371 = CARTESIAN_POINT('Ctrl Pts',(-22.0982986781565,-14.4297450121969,
114.5615978599)) ;
#180372 = CARTESIAN_POINT('Ctrl Pts',(-22.0975308900083,-14.5056122468393,
114.55925930133)) ;
#180373 = CARTESIAN_POINT('Ctrl Pts',(-22.0967631018602,-14.5814794814817,
114.556920742759)) ;
#180374 = CARTESIAN_POINT('Ctrl Pts',(-22.170566941287,-14.5814794817608,
114.532689688911)) ;
#180375 = CARTESIAN_POINT('Ctrl Pts',(-22.2443707807138,-14.58147948204,114.508458635062)) ;
#180376 = CARTESIAN_POINT('Ctrl Pts',(-22.2451385688619,-14.5056122473976,
114.510797193633)) ;
#180377 = CARTESIAN_POINT('Ctrl Pts',(-22.324940686415,-14.4743736272664,
114.789329071983)) ;
#180378 = CARTESIAN_POINT('Ctrl Pts',(-22.3194033900936,-14.4005733067483,
114.772463360702)) ;
#180379 = CARTESIAN_POINT('Ctrl Pts',(-22.2455995486149,-14.4005733047048,
114.7966944083)) ;
#180380 = CARTESIAN_POINT('Ctrl Pts',(-22.1717957071361,-14.4005733026613,
114.820925455899)) ;
#180381 = CARTESIAN_POINT('Ctrl Pts',(-22.1773330034575,-14.4743736231794,
114.83779116718)) ;
#180382 = CARTESIAN_POINT('Ctrl Pts',(-22.1828702997789,-14.5481739436975,
114.854656878461)) ;
#180383 = CARTESIAN_POINT('Ctrl Pts',(-22.2566741412577,-14.548173945741,
114.830425830863)) ;
#180384 = CARTESIAN_POINT('Ctrl Pts',(-22.3304779827364,-14.5481739477846,
114.806194783264)) ;
#180385 = CARTESIAN_POINT('Ctrl Pts',(-22.324940686415,-14.4743736272664,
114.789329071983)) ;
#180386 = CARTESIAN_POINT('Ctrl Pts',(-22.3988824387203,-14.3676054099568,
115.049984802301)) ;
#180387 = CARTESIAN_POINT('Ctrl Pts',(-22.3874402811753,-14.3011495694392,
115.015133836573)) ;
#180388 = CARTESIAN_POINT('Ctrl Pts',(-22.3136364381479,-14.3011495683314,
115.039364879455)) ;
#180389 = CARTESIAN_POINT('Ctrl Pts',(-22.2398325951206,-14.3011495672236,
115.063595922336)) ;
#180390 = CARTESIAN_POINT('Ctrl Pts',(-22.2512747526657,-14.3676054077411,
115.098446888065)) ;
#180391 = CARTESIAN_POINT('Ctrl Pts',(-22.2627169102107,-14.4340612482587,
115.133297853793)) ;
#180392 = CARTESIAN_POINT('Ctrl Pts',(-22.3365207532381,-14.4340612493665,
115.109066810911)) ;
#180393 = CARTESIAN_POINT('Ctrl Pts',(-22.4103245962654,-14.4340612504743,
115.084835768029)) ;
#180394 = CARTESIAN_POINT('Ctrl Pts',(-22.3988824387203,-14.3676054099568,
115.049984802301)) ;
#180395 = CARTESIAN_POINT('Ctrl Pts',(-22.4609934584054,-14.1926642104704,
115.274637530722)) ;
#180396 = CARTESIAN_POINT('Ctrl Pts',(-22.4444629941387,-14.1383247775165,
115.22428840378)) ;
#180397 = CARTESIAN_POINT('Ctrl Pts',(-22.3706591502841,-14.1383247785838,
115.248519444142)) ;
#180398 = CARTESIAN_POINT('Ctrl Pts',(-22.2968553064295,-14.1383247796511,
115.272750484504)) ;
#180399 = CARTESIAN_POINT('Ctrl Pts',(-22.3133857706962,-14.192664212605,
115.323099611446)) ;
#180400 = CARTESIAN_POINT('Ctrl Pts',(-22.3299162349628,-14.2470036455589,
115.373448738388)) ;
#180401 = CARTESIAN_POINT('Ctrl Pts',(-22.4037200788174,-14.2470036444916,
115.349217698026)) ;
#180402 = CARTESIAN_POINT('Ctrl Pts',(-22.477523922672,-14.2470036434243,
115.324986657664)) ;
#180403 = CARTESIAN_POINT('Ctrl Pts',(-22.4609934584054,-14.1926642104704,
115.274637530722)) ;
#180404 = CARTESIAN_POINT('Ctrl Pts',(-22.5060098471497,-13.9629645552833,
115.447132030502)) ;
#180405 = CARTESIAN_POINT('Ctrl Pts',(-22.485579189812,-13.9245838600997,
115.384903544793)) ;
#180406 = CARTESIAN_POINT('Ctrl Pts',(-22.411775345856,-13.9245838630912,
115.409134584846)) ;
#180407 = CARTESIAN_POINT('Ctrl Pts',(-22.3379715019,-13.9245838660827,115.433365624899)) ;
#180408 = CARTESIAN_POINT('Ctrl Pts',(-22.3584021592378,-13.9629645612662,
115.495594110609)) ;
#180409 = CARTESIAN_POINT('Ctrl Pts',(-22.3788328165755,-14.0013452564497,
115.557822596318)) ;
#180410 = CARTESIAN_POINT('Ctrl Pts',(-22.4526366605315,-14.0013452534583,
115.533591556265)) ;
#180411 = CARTESIAN_POINT('Ctrl Pts',(-22.5264405044875,-14.0013452504668,
115.509360516212)) ;
#180412 = CARTESIAN_POINT('Ctrl Pts',(-22.5060098471497,-13.9629645552833,
115.447132030502)) ;
#180413 = CARTESIAN_POINT('Ctrl Pts',(-22.5301282053753,-13.6916669453695,
115.556308146258)) ;
#180414 = CARTESIAN_POINT('Ctrl Pts',(-22.5072437313959,-13.6721744570857,
115.486605730959)) ;
#180415 = CARTESIAN_POINT('Ctrl Pts',(-22.4334398878541,-13.6721744593942,
115.510836772273)) ;
#180416 = CARTESIAN_POINT('Ctrl Pts',(-22.3596360443124,-13.6721744617026,
115.535067813588)) ;
#180417 = CARTESIAN_POINT('Ctrl Pts',(-22.3825205182917,-13.6916669499864,
115.604770228888)) ;
#180418 = CARTESIAN_POINT('Ctrl Pts',(-22.4054049922711,-13.7111594382702,
115.674472644188)) ;
#180419 = CARTESIAN_POINT('Ctrl Pts',(-22.4792088358129,-13.7111594359618,
115.650241602873)) ;
#180420 = CARTESIAN_POINT('Ctrl Pts',(-22.5530126793547,-13.7111594336534,
115.626010561558)) ;
#180421 = CARTESIAN_POINT('Ctrl Pts',(-22.5301282053753,-13.6916669453695,
115.556308146258)) ;
#180422 = CARTESIAN_POINT('Ctrl Pts',(-22.5305152960144,-13.4042886281479,
115.592739547311)) ;
#180423 = CARTESIAN_POINT('Ctrl Pts',(-22.5068408787418,-13.4048339669214,
115.520631092151)) ;
#180424 = CARTESIAN_POINT('Ctrl Pts',(-22.4330370354201,-13.4048339668837,
115.544862134136)) ;
#180425 = CARTESIAN_POINT('Ctrl Pts',(-22.3592331920984,-13.404833966846,
115.569093176121)) ;
#180426 = CARTESIAN_POINT('Ctrl Pts',(-22.382907609371,-13.4042886280725,
115.641201631281)) ;
#180427 = CARTESIAN_POINT('Ctrl Pts',(-22.4065820266436,-13.403743289299,
115.713310086441)) ;
#180428 = CARTESIAN_POINT('Ctrl Pts',(-22.4803858699653,-13.4037432893367,
115.689079044456)) ;
#180429 = CARTESIAN_POINT('Ctrl Pts',(-22.554189713287,-13.4037432893744,
115.664848002471)) ;
#180430 = CARTESIAN_POINT('Ctrl Pts',(-22.5305152960144,-13.4042886281479,
115.592739547311)) ;
#180431 = CARTESIAN_POINT('Ctrl Pts',(-22.5067605017534,-13.1160881842174,
115.55586845108)) ;
#180432 = CARTESIAN_POINT('Ctrl Pts',(-22.4839758365331,-13.1367582104912,
115.486470037027)) ;
#180433 = CARTESIAN_POINT('Ctrl Pts',(-22.4101719928964,-13.1367582061789,
115.510701078053)) ;
#180434 = CARTESIAN_POINT('Ctrl Pts',(-22.3363681492598,-13.1367582018666,
115.534932119079)) ;
#180435 = CARTESIAN_POINT('Ctrl Pts',(-22.3591528144801,-13.1160881755929,
115.604330533131)) ;
#180436 = CARTESIAN_POINT('Ctrl Pts',(-22.3819374797004,-13.0954181493191,
115.673728947184)) ;
#180437 = CARTESIAN_POINT('Ctrl Pts',(-22.455741323337,-13.0954181536314,
115.649497906158)) ;
#180438 = CARTESIAN_POINT('Ctrl Pts',(-22.5295451669737,-13.0954181579436,
115.625266865132)) ;
#180439 = CARTESIAN_POINT('Ctrl Pts',(-22.5067605017534,-13.1160881842174,
115.55586845108)) ;
#180440 = CARTESIAN_POINT('Ctrl Pts',(-22.4595154178549,-12.8495738757798,
115.447455103037)) ;
#180441 = CARTESIAN_POINT('Ctrl Pts',(-22.4392620419425,-12.8888833461409,
115.385766587677)) ;
#180442 = CARTESIAN_POINT('Ctrl Pts',(-22.365458196973,-12.8888833370438,
115.409997624643)) ;
#180443 = CARTESIAN_POINT('Ctrl Pts',(-22.2916543520035,-12.8888833279467,
115.434228661609)) ;
#180444 = CARTESIAN_POINT('Ctrl Pts',(-22.311907727916,-12.8495738575856,
115.495917176969)) ;
#180445 = CARTESIAN_POINT('Ctrl Pts',(-22.3321611038284,-12.8102643872246,
115.557605692329)) ;
#180446 = CARTESIAN_POINT('Ctrl Pts',(-22.4059649487979,-12.8102643963217,
115.533374655363)) ;
#180447 = CARTESIAN_POINT('Ctrl Pts',(-22.4797687937674,-12.8102644054188,
115.509143618397)) ;
#180448 = CARTESIAN_POINT('Ctrl Pts',(-22.4595154178549,-12.8495738757798,
115.447455103037)) ;
#180449 = CARTESIAN_POINT('Ctrl Pts',(-22.3918481625051,-12.6242652876755,
115.276723191289)) ;
#180450 = CARTESIAN_POINT('Ctrl Pts',(-22.3755581859856,-12.6793633695142,
115.22710655087)) ;
#180451 = CARTESIAN_POINT('Ctrl Pts',(-22.3017543389936,-12.6793633576824,
115.251337581676)) ;
#180452 = CARTESIAN_POINT('Ctrl Pts',(-22.2279504920016,-12.6793633458506,
115.275568612482)) ;
#180453 = CARTESIAN_POINT('Ctrl Pts',(-22.244240468521,-12.6242652640119,
115.325185252901)) ;
#180454 = CARTESIAN_POINT('Ctrl Pts',(-22.2605304450405,-12.5691671821732,
115.374801893319)) ;
#180455 = CARTESIAN_POINT('Ctrl Pts',(-22.3343342920325,-12.569167194005,
115.350570862513)) ;
#180456 = CARTESIAN_POINT('Ctrl Pts',(-22.4081381390246,-12.5691672058369,
115.326339831707)) ;
#180457 = CARTESIAN_POINT('Ctrl Pts',(-22.3918481625051,-12.6242652876755,
115.276723191289)) ;
#180458 = CARTESIAN_POINT('Ctrl Pts',(-22.3066463098264,-12.4543477917217,
115.052950743928)) ;
#180459 = CARTESIAN_POINT('Ctrl Pts',(-22.2955420650032,-12.5213905408383,
115.019129005345)) ;
#180460 = CARTESIAN_POINT('Ctrl Pts',(-22.2217382143452,-12.5213905278412,
115.043360024985)) ;
#180461 = CARTESIAN_POINT('Ctrl Pts',(-22.1479343636872,-12.521390514844,
115.067591044625)) ;
#180462 = CARTESIAN_POINT('Ctrl Pts',(-22.1590386085103,-12.4543477657274,
115.101412783208)) ;
#180463 = CARTESIAN_POINT('Ctrl Pts',(-22.1701428533335,-12.3873050166108,
115.135234521791)) ;
#180464 = CARTESIAN_POINT('Ctrl Pts',(-22.2439467039915,-12.387305029608,
115.111003502151)) ;
#180465 = CARTESIAN_POINT('Ctrl Pts',(-22.3177505546495,-12.3873050426051,
115.086772482511)) ;
#180466 = CARTESIAN_POINT('Ctrl Pts',(-22.3066463098264,-12.4543477917217,
115.052950743928)) ;
#180467 = CARTESIAN_POINT('Ctrl Pts',(-22.2113534668614,-12.3553371823295,
114.797951573092)) ;
#180468 = CARTESIAN_POINT('Ctrl Pts',(-22.2061572714321,-12.4293892510952,
114.78212479958)) ;
#180469 = CARTESIAN_POINT('Ctrl Pts',(-22.1323534180165,-12.4293892433542,
114.806355810821)) ;
#180470 = CARTESIAN_POINT('Ctrl Pts',(-22.058549564601,-12.4293892356132,
114.830586822062)) ;
#180471 = CARTESIAN_POINT('Ctrl Pts',(-22.0637457600304,-12.3553371668475,
114.846413595574)) ;
#180472 = CARTESIAN_POINT('Ctrl Pts',(-22.0689419554598,-12.2812850980819,
114.862240369086)) ;
#180473 = CARTESIAN_POINT('Ctrl Pts',(-22.1427458088753,-12.2812851058229,
114.838009357845)) ;
#180474 = CARTESIAN_POINT('Ctrl Pts',(-22.2165496622908,-12.2812851135639,
114.813778346604)) ;
#180475 = CARTESIAN_POINT('Ctrl Pts',(-22.2113534668614,-12.3553371823295,
114.797951573092)) ;
#180476 = CARTESIAN_POINT('Ctrl Pts',(-22.1099317335009,-12.3315537600446,
114.524642057895)) ;
#180477 = CARTESIAN_POINT('Ctrl Pts',(-22.1110725413318,-12.4073738615737,
114.52811677365)) ;
#180478 = CARTESIAN_POINT('Ctrl Pts',(-22.0372686845444,-12.4073738630853,
114.552347774621)) ;
#180479 = CARTESIAN_POINT('Ctrl Pts',(-21.963464827757,-12.4073738645969,
114.576578775592)) ;
#180480 = CARTESIAN_POINT('Ctrl Pts',(-21.9623240199261,-12.3315537630678,
114.573104059837)) ;
#180481 = CARTESIAN_POINT('Ctrl Pts',(-21.9611832120952,-12.2557336615386,
114.569629344082)) ;
#180482 = CARTESIAN_POINT('Ctrl Pts',(-22.0349870688826,-12.255733660027,
114.545398343111)) ;
#180483 = CARTESIAN_POINT('Ctrl Pts',(-22.1087909256699,-12.2557336585155,
114.521167342141)) ;
#180484 = CARTESIAN_POINT('Ctrl Pts',(-22.1099317335009,-12.3315537600446,
114.524642057895)) ;
#180485 = CARTESIAN_POINT('Ctrl Pts',(-22.010593220664,-12.3856473127391,
114.257389293014)) ;
#180486 = CARTESIAN_POINT('Ctrl Pts',(-22.0179406256113,-12.4577997306566,
114.279768302014)) ;
#180487 = CARTESIAN_POINT('Ctrl Pts',(-21.9441367672794,-12.4577997458788,
114.30399929828)) ;
#180488 = CARTESIAN_POINT('Ctrl Pts',(-21.8703329089475,-12.457799761101,
114.328230294547)) ;
#180489 = CARTESIAN_POINT('Ctrl Pts',(-21.8629855040001,-12.3856473431835,
114.305851285547)) ;
#180490 = CARTESIAN_POINT('Ctrl Pts',(-21.8556380990528,-12.3134949252661,
114.283472276546)) ;
#180491 = CARTESIAN_POINT('Ctrl Pts',(-21.9294419573847,-12.3134949100439,
114.25924128028)) ;
#180492 = CARTESIAN_POINT('Ctrl Pts',(-22.0032458157166,-12.3134948948217,
114.235010284013)) ;
#180493 = CARTESIAN_POINT('Ctrl Pts',(-22.010593220664,-12.3856473127391,
114.257389293014)) ;
#180494 = CARTESIAN_POINT('Ctrl Pts',(-21.9183564548921,-12.513656004823,
114.011961870334)) ;
#180495 = CARTESIAN_POINT('Ctrl Pts',(-21.9314195210671,-12.5769754722421,
114.051749861039)) ;
#180496 = CARTESIAN_POINT('Ctrl Pts',(-21.8576156621307,-12.5769755044901,
114.075980855464)) ;
#180497 = CARTESIAN_POINT('Ctrl Pts',(-21.7838118031943,-12.576975536738,
114.10021184989)) ;
#180498 = CARTESIAN_POINT('Ctrl Pts',(-21.7707487370193,-12.5136560693188,
114.060423859185)) ;
#180499 = CARTESIAN_POINT('Ctrl Pts',(-21.7576856708444,-12.4503366018996,
114.02063586848)) ;
#180500 = CARTESIAN_POINT('Ctrl Pts',(-21.8314895297808,-12.4503365696517,
113.996404874054)) ;
#180501 = CARTESIAN_POINT('Ctrl Pts',(-21.9052933887172,-12.4503365374038,
113.972173879629)) ;
#180502 = CARTESIAN_POINT('Ctrl Pts',(-21.9183564548921,-12.513656004823,
114.011961870334)) ;
#180503 = CARTESIAN_POINT('Ctrl Pts',(-21.839571054505,-12.707439556573,113.807586885716)) ;
#180504 = CARTESIAN_POINT('Ctrl Pts',(-21.8574172488463,-12.7573213774984,
113.861943512876)) ;
#180505 = CARTESIAN_POINT('Ctrl Pts',(-21.7836133912687,-12.7573214291752,
113.88617451144)) ;
#180506 = CARTESIAN_POINT('Ctrl Pts',(-21.709809533691,-12.7573214808521,
113.910405510004)) ;
#180507 = CARTESIAN_POINT('Ctrl Pts',(-21.6919633393498,-12.7074396599266,
113.856048882843)) ;
#180508 = CARTESIAN_POINT('Ctrl Pts',(-21.6741171450086,-12.6575578390012,
113.801692255683)) ;
#180509 = CARTESIAN_POINT('Ctrl Pts',(-21.7479210025862,-12.6575577873243,
113.777461257119)) ;
#180510 = CARTESIAN_POINT('Ctrl Pts',(-21.8217248601638,-12.6575577356475,
113.753230258555)) ;
#180511 = CARTESIAN_POINT('Ctrl Pts',(-21.839571054505,-12.707439556573,113.807586885716)) ;
#180512 = CARTESIAN_POINT('Ctrl Pts',(-21.7797609837458,-12.9500051005904,
113.660688819678)) ;
#180513 = CARTESIAN_POINT('Ctrl Pts',(-21.8010788020931,-12.9830234168188,
113.725619453298)) ;
#180514 = CARTESIAN_POINT('Ctrl Pts',(-21.7272749484766,-12.9830234842415,
113.749850463927)) ;
#180515 = CARTESIAN_POINT('Ctrl Pts',(-21.65347109486,-12.9830235516642,113.774081474556)) ;
#180516 = CARTESIAN_POINT('Ctrl Pts',(-21.6321532765127,-12.9500052354358,
113.709150840935)) ;
#180517 = CARTESIAN_POINT('Ctrl Pts',(-21.6108354581654,-12.9169869192073,
113.644220207315)) ;
#180518 = CARTESIAN_POINT('Ctrl Pts',(-21.6846393117819,-12.9169868517846,
113.619989196687)) ;
#180519 = CARTESIAN_POINT('Ctrl Pts',(-21.7584431653985,-12.9169867843619,
113.595758186058)) ;
#180520 = CARTESIAN_POINT('Ctrl Pts',(-21.7797609837458,-12.9500051005904,
113.660688819678)) ;
#180521 = CARTESIAN_POINT('Ctrl Pts',(-21.741415490494,-13.2274462581565,
113.579389468672)) ;
#180522 = CARTESIAN_POINT('Ctrl Pts',(-21.7647069644902,-13.2411424706592,
113.650331538803)) ;
#180523 = CARTESIAN_POINT('Ctrl Pts',(-21.6909031163578,-13.2411425518727,
113.674562566135)) ;
#180524 = CARTESIAN_POINT('Ctrl Pts',(-21.6170992682254,-13.2411426330862,
113.698793593467)) ;
#180525 = CARTESIAN_POINT('Ctrl Pts',(-21.5938077942292,-13.2274464205834,
113.627851523337)) ;
#180526 = CARTESIAN_POINT('Ctrl Pts',(-21.570516320233,-13.2137502080807,
113.556909453206)) ;
#180527 = CARTESIAN_POINT('Ctrl Pts',(-21.6443201683654,-13.2137501268672,
113.532678425874)) ;
#180528 = CARTESIAN_POINT('Ctrl Pts',(-21.7181240164978,-13.2137500456537,
113.508447398542)) ;
#180529 = CARTESIAN_POINT('Ctrl Pts',(-21.741415490494,-13.2274462581565,
113.579389468672)) ;
#180530 = CARTESIAN_POINT('Ctrl Pts',(-21.7271451352815,-13.5192262317475,
113.571491516801)) ;
#180531 = CARTESIAN_POINT('Ctrl Pts',(-21.750730941216,-13.5125713400262,
113.643330074385)) ;
#180532 = CARTESIAN_POINT('Ctrl Pts',(-21.6769271002671,-13.5125714295465,
113.667561123597)) ;
#180533 = CARTESIAN_POINT('Ctrl Pts',(-21.6031232593182,-13.5125715190667,
113.691792172809)) ;
#180534 = CARTESIAN_POINT('Ctrl Pts',(-21.5795374533838,-13.519226410788,
113.619953615225)) ;
#180535 = CARTESIAN_POINT('Ctrl Pts',(-21.5559516474493,-13.5258813025093,
113.548115057642)) ;
#180536 = CARTESIAN_POINT('Ctrl Pts',(-21.6297554883982,-13.525881212989,
113.523884008429)) ;
#180537 = CARTESIAN_POINT('Ctrl Pts',(-21.7035593293471,-13.5258811234688,
113.499652959217)) ;
#180538 = CARTESIAN_POINT('Ctrl Pts',(-21.7271451352815,-13.5192262317475,
113.571491516801)) ;
#180539 = CARTESIAN_POINT('Ctrl Pts',(-21.7370271436767,-13.8018769048648,
113.636919707644)) ;
#180540 = CARTESIAN_POINT('Ctrl Pts',(-21.7592262395528,-13.7754786172954,
113.704534570041)) ;
#180541 = CARTESIAN_POINT('Ctrl Pts',(-21.6854224064523,-13.7754787060709,
113.728765643158)) ;
#180542 = CARTESIAN_POINT('Ctrl Pts',(-21.6116185733517,-13.7754787948464,
113.752996716275)) ;
#180543 = CARTESIAN_POINT('Ctrl Pts',(-21.5894194774756,-13.8018770824157,
113.685381853878)) ;
#180544 = CARTESIAN_POINT('Ctrl Pts',(-21.5672203815995,-13.8282753699851,
113.617766991481)) ;
#180545 = CARTESIAN_POINT('Ctrl Pts',(-21.6410242147001,-13.8282752812096,
113.593535918364)) ;
#180546 = CARTESIAN_POINT('Ctrl Pts',(-21.7148280478006,-13.8282751924341,
113.569304845247)) ;
#180547 = CARTESIAN_POINT('Ctrl Pts',(-21.7370271436767,-13.8018769048648,
113.636919707644)) ;
#180548 = CARTESIAN_POINT('Ctrl Pts',(-21.7697376558309,-14.058784271986,
113.772109441117)) ;
#180549 = CARTESIAN_POINT('Ctrl Pts',(-21.7889497969748,-14.0144111213973,
113.830626521239)) ;
#180550 = CARTESIAN_POINT('Ctrl Pts',(-21.7151459718567,-14.0144112025132,
113.854857618669)) ;
#180551 = CARTESIAN_POINT('Ctrl Pts',(-21.6413421467386,-14.014411283629,
113.879088716099)) ;
#180552 = CARTESIAN_POINT('Ctrl Pts',(-21.6221300055947,-14.0587844342176,
113.820571635977)) ;
#180553 = CARTESIAN_POINT('Ctrl Pts',(-21.6029178644509,-14.1031575848063,
113.762054555855)) ;
#180554 = CARTESIAN_POINT('Ctrl Pts',(-21.676721689569,-14.1031575036904,
113.737823458425)) ;
#180555 = CARTESIAN_POINT('Ctrl Pts',(-21.7505255146871,-14.1031574225746,
113.713592360994)) ;
#180556 = CARTESIAN_POINT('Ctrl Pts',(-21.7697376558309,-14.058784271986,
113.772109441117)) ;
#180557 = CARTESIAN_POINT('Ctrl Pts',(-21.8220819037483,-14.2690401451517,
113.967006518844)) ;
#180558 = CARTESIAN_POINT('Ctrl Pts',(-21.8369339115327,-14.2099227100526,
114.012243336187)) ;
#180559 = CARTESIAN_POINT('Ctrl Pts',(-21.7631300934121,-14.2099227749143,
114.03647445493)) ;
#180560 = CARTESIAN_POINT('Ctrl Pts',(-21.6893262752916,-14.209922839776,
114.060705573674)) ;
#180561 = CARTESIAN_POINT('Ctrl Pts',(-21.6744742675071,-14.2690402748751,
114.015468756331)) ;
#180562 = CARTESIAN_POINT('Ctrl Pts',(-21.6596222597227,-14.3281577099741,
113.970231938989)) ;
#180563 = CARTESIAN_POINT('Ctrl Pts',(-21.7334260778433,-14.3281576451124,
113.946000820246)) ;
#180564 = CARTESIAN_POINT('Ctrl Pts',(-21.8072298959639,-14.3281575802507,
113.921769701502)) ;
#180565 = CARTESIAN_POINT('Ctrl Pts',(-21.8220819037483,-14.2690401451517,
113.967006518844)) ;
#180566 = CARTESIAN_POINT('Ctrl Pts',(-21.8895943124559,-14.418345814643,
114.208124022186)) ;
#180567 = CARTESIAN_POINT('Ctrl Pts',(-21.8990204669094,-14.3487174926443,
114.236834565689)) ;
#180568 = CARTESIAN_POINT('Ctrl Pts',(-21.8252166540276,-14.3487175346435,
114.261065700389)) ;
#180569 = CARTESIAN_POINT('Ctrl Pts',(-21.7514128411458,-14.3487175766427,
114.285296835089)) ;
#180570 = CARTESIAN_POINT('Ctrl Pts',(-21.7419866866923,-14.4183458986414,
114.256586291586)) ;
#180571 = CARTESIAN_POINT('Ctrl Pts',(-21.7325605322388,-14.48797422064,114.227875748084)) ;
#180572 = CARTESIAN_POINT('Ctrl Pts',(-21.8063643451206,-14.4879741786408,
114.203644613384)) ;
#180573 = CARTESIAN_POINT('Ctrl Pts',(-21.8801681580024,-14.4879741366417,
114.179413478684)) ;
#180574 = CARTESIAN_POINT('Ctrl Pts',(-21.8895943124559,-14.418345814643,
114.208124022186)) ;
#180575 = CARTESIAN_POINT('Ctrl Pts',(-21.966477791396,-14.4960013207205,
114.477695371654)) ;
#180576 = CARTESIAN_POINT('Ctrl Pts',(-21.9698176997642,-14.4208489309484,
114.487868191563)) ;
#180577 = CARTESIAN_POINT('Ctrl Pts',(-21.8960138897414,-14.4208489456351,
114.512099334971)) ;
#180578 = CARTESIAN_POINT('Ctrl Pts',(-21.8222100797186,-14.4208489603219,
114.536330478379)) ;
#180579 = CARTESIAN_POINT('Ctrl Pts',(-21.8188701713504,-14.496001350094,
114.52615765847)) ;
#180580 = CARTESIAN_POINT('Ctrl Pts',(-21.8155302629822,-14.5711537398661,
114.51598483856)) ;
#180581 = CARTESIAN_POINT('Ctrl Pts',(-21.889334073005,-14.5711537251794,
114.491753695152)) ;
#180582 = CARTESIAN_POINT('Ctrl Pts',(-21.9631378830277,-14.5711537104926,
114.467522551744)) ;
#180583 = CARTESIAN_POINT('Ctrl Pts',(-21.966477791396,-14.4960013207205,
114.477695371654)) ;
#180584 = CARTESIAN_POINT('Ctrl Pts',(-22.0471672488081,-14.4962457299704,
114.759096539096)) ;
#180585 = CARTESIAN_POINT('Ctrl Pts',(-22.0441414094765,-14.4209645456079,
114.749880318615)) ;
#180586 = CARTESIAN_POINT('Ctrl Pts',(-21.9703375995745,-14.4209645311187,
114.774111462391)) ;
#180587 = CARTESIAN_POINT('Ctrl Pts',(-21.8965337896726,-14.4209645166296,
114.798342606167)) ;
#180588 = CARTESIAN_POINT('Ctrl Pts',(-21.8995596290041,-14.4962457009921,
114.807558826648)) ;
#180589 = CARTESIAN_POINT('Ctrl Pts',(-21.9025854683358,-14.5715268853546,
114.81677504713)) ;
#180590 = CARTESIAN_POINT('Ctrl Pts',(-21.9763892782377,-14.5715268998438,
114.792543903354)) ;
#180591 = CARTESIAN_POINT('Ctrl Pts',(-22.0501930881397,-14.5715269143329,
114.768312759578)) ;
#180592 = CARTESIAN_POINT('Ctrl Pts',(-22.0471672488081,-14.4962457299704,
114.759096539096)) ;
#180593 = CARTESIAN_POINT('Ctrl Pts',(-22.1237856140213,-14.4198799151553,
115.027702043525)) ;
#180594 = CARTESIAN_POINT('Ctrl Pts',(-22.1146768854847,-14.3498193552219,
114.999958324006)) ;
#180595 = CARTESIAN_POINT('Ctrl Pts',(-22.0408730730278,-14.3498193130492,
115.02418946)) ;
#180596 = CARTESIAN_POINT('Ctrl Pts',(-21.967069260571,-14.3498192708765,
115.048420595995)) ;
#180597 = CARTESIAN_POINT('Ctrl Pts',(-21.9761779891077,-14.4198798308098,
115.076164315514)) ;
#180598 = CARTESIAN_POINT('Ctrl Pts',(-21.9852867176444,-14.4899403907432,
115.103908035032)) ;
#180599 = CARTESIAN_POINT('Ctrl Pts',(-22.0590905301012,-14.4899404329159,
115.079676899038)) ;
#180600 = CARTESIAN_POINT('Ctrl Pts',(-22.132894342558,-14.4899404750886,
115.055445763043)) ;
#180601 = CARTESIAN_POINT('Ctrl Pts',(-22.1237856140213,-14.4198799151553,
115.027702043525)) ;
#180602 = CARTESIAN_POINT('Ctrl Pts',(-22.1916978524243,-14.2709014086462,
115.270163302908)) ;
#180603 = CARTESIAN_POINT('Ctrl Pts',(-22.1770973048726,-14.2111372247694,
115.225692388811)) ;
#180604 = CARTESIAN_POINT('Ctrl Pts',(-22.1032934872705,-14.2111371588843,
115.249923509134)) ;
#180605 = CARTESIAN_POINT('Ctrl Pts',(-22.0294896696684,-14.2111370929992,
115.274154629457)) ;
#180606 = CARTESIAN_POINT('Ctrl Pts',(-22.0440902172201,-14.270901276876,
115.318625543554)) ;
#180607 = CARTESIAN_POINT('Ctrl Pts',(-22.0586907647718,-14.3306654607528,
115.36309645765)) ;
#180608 = CARTESIAN_POINT('Ctrl Pts',(-22.1324945823739,-14.3306655266379,
115.338865337328)) ;
#180609 = CARTESIAN_POINT('Ctrl Pts',(-22.206298399976,-14.330665592523,115.314634217005)) ;
#180610 = CARTESIAN_POINT('Ctrl Pts',(-22.1916978524243,-14.2709014086462,
115.270163302908)) ;
#180611 = CARTESIAN_POINT('Ctrl Pts',(-22.244095479827,-14.0614284920593,
115.465166551261)) ;
#180612 = CARTESIAN_POINT('Ctrl Pts',(-22.2250822225662,-14.016200017183,
115.407255235435)) ;
#180613 = CARTESIAN_POINT('Ctrl Pts',(-22.1512783980525,-14.01619993407,115.431486334706)) ;
#180614 = CARTESIAN_POINT('Ctrl Pts',(-22.0774745735387,-14.016199850957,
115.455717433977)) ;
#180615 = CARTESIAN_POINT('Ctrl Pts',(-22.0964878307995,-14.0614283258333,
115.513628749803)) ;
#180616 = CARTESIAN_POINT('Ctrl Pts',(-22.1155010880602,-14.1066568007097,
115.571540065629)) ;
#180617 = CARTESIAN_POINT('Ctrl Pts',(-22.189304912574,-14.1066568838226,
115.547308966358)) ;
#180618 = CARTESIAN_POINT('Ctrl Pts',(-22.2631087370878,-14.1066569669356,
115.523077867087)) ;
#180619 = CARTESIAN_POINT('Ctrl Pts',(-22.244095479827,-14.0614284920593,
115.465166551261)) ;
#180620 = CARTESIAN_POINT('Ctrl Pts',(-22.2770600984898,-13.8059370930909,
115.601015529285)) ;
#180621 = CARTESIAN_POINT('Ctrl Pts',(-22.2549834954965,-13.778478597832,
115.5337737567)) ;
#180622 = CARTESIAN_POINT('Ctrl Pts',(-22.1811796629507,-13.7784785051367,
115.558004831507)) ;
#180623 = CARTESIAN_POINT('Ctrl Pts',(-22.1073758304049,-13.7784784124414,
115.582235906314)) ;
#180624 = CARTESIAN_POINT('Ctrl Pts',(-22.1294524333982,-13.8059369077003,
115.649477678899)) ;
#180625 = CARTESIAN_POINT('Ctrl Pts',(-22.1515290363916,-13.8333954029592,
115.716719451483)) ;
#180626 = CARTESIAN_POINT('Ctrl Pts',(-22.2253328689374,-13.8333954956545,
115.692488376677)) ;
#180627 = CARTESIAN_POINT('Ctrl Pts',(-22.2991367014832,-13.8333955883498,
115.66825730187)) ;
#180628 = CARTESIAN_POINT('Ctrl Pts',(-22.2770600984898,-13.8059370930909,
115.601015529285)) ;
#180629 = CARTESIAN_POINT('Ctrl Pts',(-22.2872367367097,-13.5211628984478,
115.667631143365)) ;
#180630 = CARTESIAN_POINT('Ctrl Pts',(-22.2636792886074,-13.5135452087457,
115.595878955628)) ;
#180631 = CARTESIAN_POINT('Ctrl Pts',(-22.1898754477952,-13.5135451161284,
115.620110005257)) ;
#180632 = CARTESIAN_POINT('Ctrl Pts',(-22.116071606983,-13.513545023511,115.644341054886)) ;
#180633 = CARTESIAN_POINT('Ctrl Pts',(-22.1396290550854,-13.5211627132132,
115.716093242622)) ;
#180634 = CARTESIAN_POINT('Ctrl Pts',(-22.1631865031877,-13.5287804029153,
115.787845430359)) ;
#180635 = CARTESIAN_POINT('Ctrl Pts',(-22.2369903439999,-13.5287804955326,
115.76361438073)) ;
#180636 = CARTESIAN_POINT('Ctrl Pts',(-22.3107941848121,-13.52878058815,115.739383331101)) ;
#180637 = CARTESIAN_POINT('Ctrl Pts',(-22.2872367367097,-13.5211628984478,
115.667631143365)) ;
#180638 = CARTESIAN_POINT('Ctrl Pts',(-22.2733014770103,-13.2317212421624,
115.660460390471)) ;
#180639 = CARTESIAN_POINT('Ctrl Pts',(-22.2499517872738,-13.244300576159,
115.589341001286)) ;
#180640 = CARTESIAN_POINT('Ctrl Pts',(-22.1761479389709,-13.2443004892996,
115.613572028099)) ;
#180641 = CARTESIAN_POINT('Ctrl Pts',(-22.102344090668,-13.2443004024403,
115.637803054912)) ;
#180642 = CARTESIAN_POINT('Ctrl Pts',(-22.1256937804045,-13.2317210684437,
115.708922444097)) ;
#180643 = CARTESIAN_POINT('Ctrl Pts',(-22.1490434701409,-13.2191417344471,
115.780041833282)) ;
#180644 = CARTESIAN_POINT('Ctrl Pts',(-22.2228473184438,-13.2191418213064,
115.755810806469)) ;
#180645 = CARTESIAN_POINT('Ctrl Pts',(-22.2966511667467,-13.2191419081658,
115.731579779656)) ;
#180646 = CARTESIAN_POINT('Ctrl Pts',(-22.2733014770103,-13.2317212421624,
115.660460390471)) ;
#180647 = CARTESIAN_POINT('Ctrl Pts',(-22.2352493339622,-12.953209842425,
115.580148172852)) ;
#180648 = CARTESIAN_POINT('Ctrl Pts',(-22.2137846357895,-12.9852534588735,
115.514770163977)) ;
#180649 = CARTESIAN_POINT('Ctrl Pts',(-22.1399807814508,-12.9852533862488,
115.539001172406)) ;
#180650 = CARTESIAN_POINT('Ctrl Pts',(-22.0661769271121,-12.9852533136241,
115.563232180835)) ;
#180651 = CARTESIAN_POINT('Ctrl Pts',(-22.0876416252848,-12.9532096971755,
115.62861018971)) ;
#180652 = CARTESIAN_POINT('Ctrl Pts',(-22.1091063234574,-12.921166080727,
115.693988198586)) ;
#180653 = CARTESIAN_POINT('Ctrl Pts',(-22.1829101777961,-12.9211661533517,
115.669757190157)) ;
#180654 = CARTESIAN_POINT('Ctrl Pts',(-22.2567140321349,-12.9211662259765,
115.645526181728)) ;
#180655 = CARTESIAN_POINT('Ctrl Pts',(-22.2352493339622,-12.953209842425,
115.580148172852)) ;
#180656 = CARTESIAN_POINT('Ctrl Pts',(-22.1754856836276,-12.7094642616823,
115.433485637688)) ;
#180657 = CARTESIAN_POINT('Ctrl Pts',(-22.1574294209425,-12.7585743721417,
115.378489173487)) ;
#180658 = CARTESIAN_POINT('Ctrl Pts',(-22.0836255623272,-12.7585743165694,
115.402720168891)) ;
#180659 = CARTESIAN_POINT('Ctrl Pts',(-22.009821703712,-12.7585742609971,
115.426951164294)) ;
#180660 = CARTESIAN_POINT('Ctrl Pts',(-22.027877966397,-12.7094641505378,
115.481947628495)) ;
#180661 = CARTESIAN_POINT('Ctrl Pts',(-22.0459342290821,-12.6603540400784,
115.536944092696)) ;
#180662 = CARTESIAN_POINT('Ctrl Pts',(-22.1197380876974,-12.6603540956507,
115.512713097292)) ;
#180663 = CARTESIAN_POINT('Ctrl Pts',(-22.1935419463127,-12.660354151223,
115.488482101889)) ;
#180664 = CARTESIAN_POINT('Ctrl Pts',(-22.1754856836276,-12.7094642616823,
115.433485637688)) ;
#180665 = CARTESIAN_POINT('Ctrl Pts',(-22.0966448910796,-12.5150572905195,
115.22901210739)) ;
#180666 = CARTESIAN_POINT('Ctrl Pts',(-22.0833278506864,-12.5778156836835,
115.18845054981)) ;
#180667 = CARTESIAN_POINT('Ctrl Pts',(-22.0095239905601,-12.5778156484991,
115.212681540611)) ;
#180668 = CARTESIAN_POINT('Ctrl Pts',(-21.9357201304339,-12.5778156133148,
115.236912531413)) ;
#180669 = CARTESIAN_POINT('Ctrl Pts',(-21.9490371708272,-12.5150572201508,
115.277474088992)) ;
#180670 = CARTESIAN_POINT('Ctrl Pts',(-21.9623542112205,-12.4522988269869,
115.318035646572)) ;
#180671 = CARTESIAN_POINT('Ctrl Pts',(-22.0361580713467,-12.4522988621712,
115.293804655771)) ;
#180672 = CARTESIAN_POINT('Ctrl Pts',(-22.1099619314729,-12.4522988973556,
115.269573664969)) ;
#180673 = CARTESIAN_POINT('Ctrl Pts',(-22.0966448910796,-12.5150572905195,
115.22901210739)) ;
#180674 = CARTESIAN_POINT('Ctrl Pts',(-22.0054187277231,-12.3871819681861,
114.986327553014)) ;
#180675 = CARTESIAN_POINT('Ctrl Pts',(-21.997723242732,-12.4589631112732,
114.962888346264)) ;
#180676 = CARTESIAN_POINT('Ctrl Pts',(-21.9239193820062,-12.4589630933021,
114.987119335239)) ;
#180677 = CARTESIAN_POINT('Ctrl Pts',(-21.8501155212804,-12.458963075331,
115.011350324214)) ;
#180678 = CARTESIAN_POINT('Ctrl Pts',(-21.8578110062715,-12.3871819322439,
115.034789530964)) ;
#180679 = CARTESIAN_POINT('Ctrl Pts',(-21.8655064912626,-12.3154007891568,
115.058228737713)) ;
#180680 = CARTESIAN_POINT('Ctrl Pts',(-21.9393103519884,-12.3154008071279,
115.033997748738)) ;
#180681 = CARTESIAN_POINT('Ctrl Pts',(-22.0131142127142,-12.315400825099,
115.009766759763)) ;
#180682 = CARTESIAN_POINT('Ctrl Pts',(-22.0054187277231,-12.3871819681861,
114.986327553014)) ;
#180683 = CARTESIAN_POINT('Ctrl Pts',(-21.905263733452,-12.3316884564228,
114.716909806915)) ;
#180684 = CARTESIAN_POINT('Ctrl Pts',(-21.9038120156515,-12.4074536121107,
114.7124881078)) ;
#180685 = CARTESIAN_POINT('Ctrl Pts',(-21.8300081572495,-12.4074536102533,
114.736719103853)) ;
#180686 = CARTESIAN_POINT('Ctrl Pts',(-21.7562042988474,-12.407453608396,
114.760950099906)) ;
#180687 = CARTESIAN_POINT('Ctrl Pts',(-21.7576560166478,-12.3316884527082,
114.765371799021)) ;
#180688 = CARTESIAN_POINT('Ctrl Pts',(-21.7591077344482,-12.2559232970203,
114.769793498135)) ;
#180689 = CARTESIAN_POINT('Ctrl Pts',(-21.8329115928503,-12.2559232988777,
114.745562502083)) ;
#180690 = CARTESIAN_POINT('Ctrl Pts',(-21.9067154512524,-12.255923300735,
114.72133150603)) ;
#180691 = CARTESIAN_POINT('Ctrl Pts',(-21.905263733452,-12.3316884564228,
114.716909806915)) ;
#180692 = CARTESIAN_POINT('Ctrl Pts',(-21.8045903005962,-12.3542922095437,
114.445593550072)) ;
#180693 = CARTESIAN_POINT('Ctrl Pts',(-21.809434740059,-12.4285936621951,
114.46034893024)) ;
#180694 = CARTESIAN_POINT('Ctrl Pts',(-21.7356308842862,-12.428593671534,
114.484579934302)) ;
#180695 = CARTESIAN_POINT('Ctrl Pts',(-21.6618270285135,-12.428593680873,
114.508810938363)) ;
#180696 = CARTESIAN_POINT('Ctrl Pts',(-21.6569825890507,-12.3542922282216,
114.494055558194)) ;
#180697 = CARTESIAN_POINT('Ctrl Pts',(-21.6521381495879,-12.2799907755701,
114.479300178026)) ;
#180698 = CARTESIAN_POINT('Ctrl Pts',(-21.7259420053606,-12.2799907662312,
114.455069173964)) ;
#180699 = CARTESIAN_POINT('Ctrl Pts',(-21.7997458611334,-12.2799907568923,
114.430838169903)) ;
#180700 = CARTESIAN_POINT('Ctrl Pts',(-21.8045903005962,-12.3542922095437,
114.445593550072)) ;
#180701 = CARTESIAN_POINT('Ctrl Pts',(-21.7081146500002,-12.4537268763868,
114.187411168182)) ;
#180702 = CARTESIAN_POINT('Ctrl Pts',(-21.7189646587714,-12.5211987643482,
114.220458543672)) ;
#180703 = CARTESIAN_POINT('Ctrl Pts',(-21.6451608071161,-12.5211987790939,
114.244689560275)) ;
#180704 = CARTESIAN_POINT('Ctrl Pts',(-21.5713569554607,-12.5211987938395,
114.268920576877)) ;
#180705 = CARTESIAN_POINT('Ctrl Pts',(-21.5605069466895,-12.4537269058781,
114.235873201386)) ;
#180706 = CARTESIAN_POINT('Ctrl Pts',(-21.5496569379183,-12.3862550179166,
114.202825825896)) ;
#180707 = CARTESIAN_POINT('Ctrl Pts',(-21.6234607895737,-12.386255003171,
114.178594809294)) ;
#180708 = CARTESIAN_POINT('Ctrl Pts',(-21.697264641229,-12.3862549884253,
114.154363792692)) ;
#180709 = CARTESIAN_POINT('Ctrl Pts',(-21.7081146500002,-12.4537268763868,
114.187411168182)) ;
#180710 = CARTESIAN_POINT('Ctrl Pts',(-21.6237862011861,-12.6212675456056,
113.965882774821)) ;
#180711 = CARTESIAN_POINT('Ctrl Pts',(-21.6398097461159,-12.6771429779521,
114.014687906835)) ;
#180712 = CARTESIAN_POINT('Ctrl Pts',(-21.5660058974906,-12.6771429943205,
114.038918932666)) ;
#180713 = CARTESIAN_POINT('Ctrl Pts',(-21.4922020488653,-12.6771430106889,
114.063149958497)) ;
#180714 = CARTESIAN_POINT('Ctrl Pts',(-21.4761785039354,-12.6212675783423,
114.014344826483)) ;
#180715 = CARTESIAN_POINT('Ctrl Pts',(-21.4601549590056,-12.5653921459958,
113.965539694469)) ;
#180716 = CARTESIAN_POINT('Ctrl Pts',(-21.5339588076309,-12.5653921296274,
113.941308668638)) ;
#180717 = CARTESIAN_POINT('Ctrl Pts',(-21.6077626562563,-12.565392113259,
113.917077642806)) ;
#180718 = CARTESIAN_POINT('Ctrl Pts',(-21.6237862011861,-12.6212675456056,
113.965882774821)) ;
#180719 = CARTESIAN_POINT('Ctrl Pts',(-21.5556046478956,-12.846192059173,
113.793679096726)) ;
#180720 = CARTESIAN_POINT('Ctrl Pts',(-21.5756792298815,-12.8864467914097,
113.854823034128)) ;
#180721 = CARTESIAN_POINT('Ctrl Pts',(-21.5018753840635,-12.8864468052169,
113.87905406851)) ;
#180722 = CARTESIAN_POINT('Ctrl Pts',(-21.4280715382456,-12.8864468190241,
113.903285102892)) ;
#180723 = CARTESIAN_POINT('Ctrl Pts',(-21.4079969562597,-12.8461920867874,
113.84214116549)) ;
#180724 = CARTESIAN_POINT('Ctrl Pts',(-21.3879223742738,-12.8059373545508,
113.780997228088)) ;
#180725 = CARTESIAN_POINT('Ctrl Pts',(-21.4617262200917,-12.8059373407436,
113.756766193706)) ;
#180726 = CARTESIAN_POINT('Ctrl Pts',(-21.5355300659097,-12.8059373269364,
113.732535159324)) ;
#180727 = CARTESIAN_POINT('Ctrl Pts',(-21.5556046478956,-12.846192059173,
113.793679096726)) ;
#180728 = CARTESIAN_POINT('Ctrl Pts',(-21.5080827888729,-13.1124184461725,
113.684427311798)) ;
#180729 = CARTESIAN_POINT('Ctrl Pts',(-21.5307714606436,-13.1341445509028,
113.753533345037)) ;
#180730 = CARTESIAN_POINT('Ctrl Pts',(-21.4569676166366,-13.1341445595333,
113.777764384935)) ;
#180731 = CARTESIAN_POINT('Ctrl Pts',(-21.3831637726296,-13.1341445681639,
113.801995424833)) ;
#180732 = CARTESIAN_POINT('Ctrl Pts',(-21.3604751008589,-13.1124184634336,
113.732889391594)) ;
#180733 = CARTESIAN_POINT('Ctrl Pts',(-21.3377864290883,-13.0906923587033,
113.663783358355)) ;
#180734 = CARTESIAN_POINT('Ctrl Pts',(-21.4115902730953,-13.0906923500727,
113.639552318457)) ;
#180735 = CARTESIAN_POINT('Ctrl Pts',(-21.4853941171023,-13.0906923414422,
113.615321278559)) ;
#180736 = CARTESIAN_POINT('Ctrl Pts',(-21.5080827888729,-13.1124184461725,
113.684427311798)) ;
#180737 = CARTESIAN_POINT('Ctrl Pts',(-21.483971454148,-13.400879749144,113.646523677771)) ;
#180738 = CARTESIAN_POINT('Ctrl Pts',(-21.5076425326459,-13.4024961126535,
113.718621963503)) ;
#180739 = CARTESIAN_POINT('Ctrl Pts',(-21.4338386893524,-13.4024961156936,
113.742853005574)) ;
#180740 = CARTESIAN_POINT('Ctrl Pts',(-21.360034846059,-13.4024961187337,
113.767084047645)) ;
#180741 = CARTESIAN_POINT('Ctrl Pts',(-21.3363637675611,-13.4008797552242,
113.694985761914)) ;
#180742 = CARTESIAN_POINT('Ctrl Pts',(-21.3126926890632,-13.3992633917147,
113.622887476182)) ;
#180743 = CARTESIAN_POINT('Ctrl Pts',(-21.3864965323567,-13.3992633886746,
113.598656434111)) ;
#180744 = CARTESIAN_POINT('Ctrl Pts',(-21.4603003756501,-13.3992633856344,
113.57442539204)) ;
#180745 = CARTESIAN_POINT('Ctrl Pts',(-21.483971454148,-13.400879749144,113.646523677771)) ;
#180746 = CARTESIAN_POINT('Ctrl Pts',(-21.4841119720974,-13.6891262166377,
113.682294540054)) ;
#180747 = CARTESIAN_POINT('Ctrl Pts',(-21.5070772034444,-13.6706178186388,
113.752242929323)) ;
#180748 = CARTESIAN_POINT('Ctrl Pts',(-21.4332733600708,-13.6706178179427,
113.77647397115)) ;
#180749 = CARTESIAN_POINT('Ctrl Pts',(-21.3594695166973,-13.6706178172465,
113.800705012978)) ;
#180750 = CARTESIAN_POINT('Ctrl Pts',(-21.3365042853503,-13.6891262152454,
113.730756623709)) ;
#180751 = CARTESIAN_POINT('Ctrl Pts',(-21.3135390540032,-13.7076346132443,
113.66080823444)) ;
#180752 = CARTESIAN_POINT('Ctrl Pts',(-21.3873428973768,-13.7076346139405,
113.636577192613)) ;
#180753 = CARTESIAN_POINT('Ctrl Pts',(-21.4611467407504,-13.7076346146366,
113.612346150785)) ;
#180754 = CARTESIAN_POINT('Ctrl Pts',(-21.4841119720974,-13.6891262166377,
113.682294540054)) ;
#180755 = CARTESIAN_POINT('Ctrl Pts',(-21.5080695511385,-13.9605413879786,
113.790974309993)) ;
#180756 = CARTESIAN_POINT('Ctrl Pts',(-21.5286572198407,-13.9230519796462,
113.853681027115)) ;
#180757 = CARTESIAN_POINT('Ctrl Pts',(-21.4548533759605,-13.9230519767635,
113.877912067399)) ;
#180758 = CARTESIAN_POINT('Ctrl Pts',(-21.3810495320804,-13.9230519738809,
113.902143107683)) ;
#180759 = CARTESIAN_POINT('Ctrl Pts',(-21.3604618633781,-13.9605413822133,
113.839436390562)) ;
#180760 = CARTESIAN_POINT('Ctrl Pts',(-21.3398741946759,-13.9980307905457,
113.77672967344)) ;
#180761 = CARTESIAN_POINT('Ctrl Pts',(-21.413678038556,-13.9980307934284,
113.752498633156)) ;
#180762 = CARTESIAN_POINT('Ctrl Pts',(-21.4874818824362,-13.9980307963111,
113.728267592871)) ;
#180763 = CARTESIAN_POINT('Ctrl Pts',(-21.5080695511385,-13.9605413879786,
113.790974309993)) ;
#180764 = CARTESIAN_POINT('Ctrl Pts',(-21.5525393505442,-14.1894540736428,
113.961580396736)) ;
#180765 = CARTESIAN_POINT('Ctrl Pts',(-21.569324495808,-14.1359254038344,
114.012705240998)) ;
#180766 = CARTESIAN_POINT('Ctrl Pts',(-21.4955206516589,-14.1359254016367,
114.036936280463)) ;
#180767 = CARTESIAN_POINT('Ctrl Pts',(-21.4217168075098,-14.135925399439,
114.061167319929)) ;
#180768 = CARTESIAN_POINT('Ctrl Pts',(-21.404931662246,-14.1894540692474,
114.010042475666)) ;
#180769 = CARTESIAN_POINT('Ctrl Pts',(-21.3881465169822,-14.2429827390558,
113.958917631403)) ;
#180770 = CARTESIAN_POINT('Ctrl Pts',(-21.4619503611313,-14.2429827412535,
113.934686591938)) ;
#180771 = CARTESIAN_POINT('Ctrl Pts',(-21.5357542052804,-14.2429827434512,
113.910455552473)) ;
#180772 = CARTESIAN_POINT('Ctrl Pts',(-21.5525393505442,-14.1894540736428,
113.961580396736)) ;
#180773 = CARTESIAN_POINT('Ctrl Pts',(-21.6146814088062,-14.3660067048925,
114.186472926776)) ;
#180774 = CARTESIAN_POINT('Ctrl Pts',(-21.6264149208127,-14.3000702425711,
114.222211311175)) ;
#180775 = CARTESIAN_POINT('Ctrl Pts',(-21.5526110770569,-14.3000702422313,
114.246442351837)) ;
#180776 = CARTESIAN_POINT('Ctrl Pts',(-21.478807233301,-14.3000702418915,
114.2706733925)) ;
#180777 = CARTESIAN_POINT('Ctrl Pts',(-21.4670737212945,-14.3660067042129,
114.234935008102)) ;
#180778 = CARTESIAN_POINT('Ctrl Pts',(-21.4553402092879,-14.4319431665342,
114.199196623703)) ;
#180779 = CARTESIAN_POINT('Ctrl Pts',(-21.5291440530438,-14.431943166874,
114.174965583041)) ;
#180780 = CARTESIAN_POINT('Ctrl Pts',(-21.6029478967997,-14.4319431672138,
114.150734542378)) ;
#180781 = CARTESIAN_POINT('Ctrl Pts',(-21.6146814088062,-14.3660067048925,
114.186472926776)) ;
#180782 = CARTESIAN_POINT('Ctrl Pts',(-21.6884351663154,-14.4734792612079,
114.446508526122)) ;
#180783 = CARTESIAN_POINT('Ctrl Pts',(-21.6943034555198,-14.3999420243742,
114.464382388145)) ;
#180784 = CARTESIAN_POINT('Ctrl Pts',(-21.6204996128377,-14.3999420254069,
114.488613432078)) ;
#180785 = CARTESIAN_POINT('Ctrl Pts',(-21.5466957701556,-14.3999420264397,
114.512844476011)) ;
#180786 = CARTESIAN_POINT('Ctrl Pts',(-21.5408274809512,-14.4734792632734,
114.494970613988)) ;
#180787 = CARTESIAN_POINT('Ctrl Pts',(-21.5349591917469,-14.5470165001072,
114.477096751966)) ;
#180788 = CARTESIAN_POINT('Ctrl Pts',(-21.608763034429,-14.5470164990744,
114.452865708032)) ;
#180789 = CARTESIAN_POINT('Ctrl Pts',(-21.6825668771111,-14.5470164980416,
114.428634664099)) ;
#180790 = CARTESIAN_POINT('Ctrl Pts',(-21.6884351663154,-14.4734792612079,
114.446508526122)) ;
#180791 = CARTESIAN_POINT('Ctrl Pts',(-21.7683784809354,-14.5056975632985,
114.725551946228)) ;
#180792 = CARTESIAN_POINT('Ctrl Pts',(-21.7679376011022,-14.4298031115965,
114.724209097231)) ;
#180793 = CARTESIAN_POINT('Ctrl Pts',(-21.6941337602889,-14.4298031119292,
114.748440146856)) ;
#180794 = CARTESIAN_POINT('Ctrl Pts',(-21.6203299194757,-14.4298031122619,
114.772671196482)) ;
#180795 = CARTESIAN_POINT('Ctrl Pts',(-21.6207707993088,-14.5056975639639,
114.774014045479)) ;
#180796 = CARTESIAN_POINT('Ctrl Pts',(-21.621211679142,-14.5815920156659,
114.775356894476)) ;
#180797 = CARTESIAN_POINT('Ctrl Pts',(-21.6950155199553,-14.5815920153332,
114.75112584485)) ;
#180798 = CARTESIAN_POINT('Ctrl Pts',(-21.7688193607686,-14.5815920150005,
114.726894795225)) ;
#180799 = CARTESIAN_POINT('Ctrl Pts',(-21.7683784809354,-14.5056975632985,
114.725551946228)) ;
#180800 = CARTESIAN_POINT('Ctrl Pts',(-21.8474157178673,-14.4599236721213,
115.001679784935)) ;
#180801 = CARTESIAN_POINT('Ctrl Pts',(-21.8407231446936,-14.387115192455,
114.981295286612)) ;
#180802 = CARTESIAN_POINT('Ctrl Pts',(-21.7669193056391,-14.3871151888849,
115.005526341595)) ;
#180803 = CARTESIAN_POINT('Ctrl Pts',(-21.6931154665847,-14.3871151853148,
115.029757396577)) ;
#180804 = CARTESIAN_POINT('Ctrl Pts',(-21.6998080397583,-14.4599236649811,
115.0501418949)) ;
#180805 = CARTESIAN_POINT('Ctrl Pts',(-21.706500612932,-14.5327321446473,
115.070526393222)) ;
#180806 = CARTESIAN_POINT('Ctrl Pts',(-21.7803044519865,-14.5327321482174,
115.04629533824)) ;
#180807 = CARTESIAN_POINT('Ctrl Pts',(-21.854108291041,-14.5327321517875,
115.022064283257)) ;
#180808 = CARTESIAN_POINT('Ctrl Pts',(-21.8474157178673,-14.4599236721213,
115.001679784935)) ;
#180809 = CARTESIAN_POINT('Ctrl Pts',(-21.9195991566158,-14.3395761921465,
115.257002682461)) ;
#180810 = CARTESIAN_POINT('Ctrl Pts',(-21.9071229816857,-14.27506508821,115.219002266226)) ;
#180811 = CARTESIAN_POINT('Ctrl Pts',(-21.8333191441344,-14.2750650771765,
115.243233325787)) ;
#180812 = CARTESIAN_POINT('Ctrl Pts',(-21.7595153065832,-14.2750650661431,
115.267464385348)) ;
#180813 = CARTESIAN_POINT('Ctrl Pts',(-21.7719914815133,-14.3395761700796,
115.305464801583)) ;
#180814 = CARTESIAN_POINT('Ctrl Pts',(-21.7844676564434,-14.4040872740161,
115.343465217818)) ;
#180815 = CARTESIAN_POINT('Ctrl Pts',(-21.8582714939946,-14.4040872850496,
115.319234158257)) ;
#180816 = CARTESIAN_POINT('Ctrl Pts',(-21.9320753315458,-14.404087296083,
115.295003098696)) ;
#180817 = CARTESIAN_POINT('Ctrl Pts',(-21.9195991566158,-14.3395761921465,
115.257002682461)) ;
#180818 = CARTESIAN_POINT('Ctrl Pts',(-21.9788462429372,-14.1535350418836,
115.472880057577)) ;
#180819 = CARTESIAN_POINT('Ctrl Pts',(-21.9614823731304,-14.101920284912,
115.419992511226)) ;
#180820 = CARTESIAN_POINT('Ctrl Pts',(-21.8876785361283,-14.1019202637606,
115.44422357246)) ;
#180821 = CARTESIAN_POINT('Ctrl Pts',(-21.8138746991261,-14.1019202426092,
115.468454633693)) ;
#180822 = CARTESIAN_POINT('Ctrl Pts',(-21.8312385689329,-14.1535349995808,
115.521342180044)) ;
#180823 = CARTESIAN_POINT('Ctrl Pts',(-21.8486024387397,-14.2051497565524,
115.574229726395)) ;
#180824 = CARTESIAN_POINT('Ctrl Pts',(-21.9224062757418,-14.2051497777038,
115.549998665161)) ;
#180825 = CARTESIAN_POINT('Ctrl Pts',(-21.996210112744,-14.2051497988552,
115.525767603927)) ;
#180826 = CARTESIAN_POINT('Ctrl Pts',(-21.9788462429372,-14.1535350418836,
115.472880057577)) ;
#180827 = CARTESIAN_POINT('Ctrl Pts',(-22.0203775008148,-13.9130985111844,
115.635036561647)) ;
#180828 = CARTESIAN_POINT('Ctrl Pts',(-21.99935074439,-13.8781962453412,115.570992453461)) ;
#180829 = CARTESIAN_POINT('Ctrl Pts',(-21.9255469068525,-13.8781962102056,
115.595223513064)) ;
#180830 = CARTESIAN_POINT('Ctrl Pts',(-21.851743069315,-13.87819617507,115.619454572667)) ;
#180831 = CARTESIAN_POINT('Ctrl Pts',(-21.8727698257398,-13.9130984409133,
115.683498680853)) ;
#180832 = CARTESIAN_POINT('Ctrl Pts',(-21.8937965821645,-13.9480007067565,
115.747542789039)) ;
#180833 = CARTESIAN_POINT('Ctrl Pts',(-21.967600419702,-13.9480007418921,
115.723311729436)) ;
#180834 = CARTESIAN_POINT('Ctrl Pts',(-22.0414042572395,-13.9480007770277,
115.699080669833)) ;
#180835 = CARTESIAN_POINT('Ctrl Pts',(-22.0203775008148,-13.9130985111844,
115.635036561647)) ;
#180836 = CARTESIAN_POINT('Ctrl Pts',(-22.0399483640035,-13.6395736822347,
115.72995984664)) ;
#180837 = CARTESIAN_POINT('Ctrl Pts',(-22.0167942098363,-13.6237185301076,
115.659436028045)) ;
#180838 = CARTESIAN_POINT('Ctrl Pts',(-21.9429903696287,-13.6237184841126,
115.683667079515)) ;
#180839 = CARTESIAN_POINT('Ctrl Pts',(-21.8691865294211,-13.6237184381175,
115.707898130985)) ;
#180840 = CARTESIAN_POINT('Ctrl Pts',(-21.8923406835883,-13.6395735902447,
115.77842194958)) ;
#180841 = CARTESIAN_POINT('Ctrl Pts',(-21.9154948377555,-13.6554287423718,
115.848945768175)) ;
#180842 = CARTESIAN_POINT('Ctrl Pts',(-21.9892986779631,-13.6554287883668,
115.824714716705)) ;
#180843 = CARTESIAN_POINT('Ctrl Pts',(-22.0631025181708,-13.6554288343619,
115.800483665235)) ;
#180844 = CARTESIAN_POINT('Ctrl Pts',(-22.0399483640035,-13.6395736822347,
115.72995984664)) ;
#180845 = CARTESIAN_POINT('Ctrl Pts',(-22.0358686869632,-13.3487006076146,
115.75305462755)) ;
#180846 = CARTESIAN_POINT('Ctrl Pts',(-22.0122308536401,-13.3531309210736,
115.68105760011)) ;
#180847 = CARTESIAN_POINT('Ctrl Pts',(-21.9384270093491,-13.3531308648212,
115.705288639143)) ;
#180848 = CARTESIAN_POINT('Ctrl Pts',(-21.8646231650582,-13.3531308085687,
115.729519678176)) ;
#180849 = CARTESIAN_POINT('Ctrl Pts',(-21.8882609983813,-13.3487004951098,
115.801516705617)) ;
#180850 = CARTESIAN_POINT('Ctrl Pts',(-21.9118988317044,-13.3442701816508,
115.873513733057)) ;
#180851 = CARTESIAN_POINT('Ctrl Pts',(-21.9857026759953,-13.3442702379032,
115.849282694024)) ;
#180852 = CARTESIAN_POINT('Ctrl Pts',(-22.0595065202863,-13.3442702941557,
115.825051654991)) ;
#180853 = CARTESIAN_POINT('Ctrl Pts',(-22.0358686869632,-13.3487006076146,
115.75305462755)) ;
#180854 = CARTESIAN_POINT('Ctrl Pts',(-22.0075438310689,-13.0636371844073,
115.70218883906)) ;
#180855 = CARTESIAN_POINT('Ctrl Pts',(-21.9851168187077,-13.0879765100876,
115.633879776751)) ;
#180856 = CARTESIAN_POINT('Ctrl Pts',(-21.9113129689696,-13.0879764491053,
115.658110799193)) ;
#180857 = CARTESIAN_POINT('Ctrl Pts',(-21.8375091192314,-13.0879763881229,
115.682341821635)) ;
#180858 = CARTESIAN_POINT('Ctrl Pts',(-21.8599361315927,-13.0636370624426,
115.750650883944)) ;
#180859 = CARTESIAN_POINT('Ctrl Pts',(-21.882363143954,-13.0392977367622,
115.818959946253)) ;
#180860 = CARTESIAN_POINT('Ctrl Pts',(-21.9561669936921,-13.0392977977446,
115.794728923811)) ;
#180861 = CARTESIAN_POINT('Ctrl Pts',(-22.0299708434302,-13.0392978587269,
115.77049790137)) ;
#180862 = CARTESIAN_POINT('Ctrl Pts',(-22.0075438310689,-13.0636371844073,
115.70218883906)) ;
#180863 = CARTESIAN_POINT('Ctrl Pts',(-21.9561819767785,-12.803286823163,
115.581244291729)) ;
#180864 = CARTESIAN_POINT('Ctrl Pts',(-21.9365739681163,-12.8458384350668,
115.521521459681)) ;
#180865 = CARTESIAN_POINT('Ctrl Pts',(-21.8627701120826,-12.8458383747554,
115.545752462947)) ;
#180866 = CARTESIAN_POINT('Ctrl Pts',(-21.788966256049,-12.8458383144439,
115.569983466214)) ;
#180867 = CARTESIAN_POINT('Ctrl Pts',(-21.8085742647111,-12.8032867025401,
115.629706298262)) ;
#180868 = CARTESIAN_POINT('Ctrl Pts',(-21.8281822733732,-12.7607350906363,
115.68942913031)) ;
#180869 = CARTESIAN_POINT('Ctrl Pts',(-21.9019861294069,-12.7607351509478,
115.665198127044)) ;
#180870 = CARTESIAN_POINT('Ctrl Pts',(-21.9757899854406,-12.7607352112592,
115.640967123777)) ;
#180871 = CARTESIAN_POINT('Ctrl Pts',(-21.9561819767785,-12.803286823163,
115.581244291729)) ;
#180872 = CARTESIAN_POINT('Ctrl Pts',(-21.8847933182746,-12.5872505028287,
115.399264233317)) ;
#180873 = CARTESIAN_POINT('Ctrl Pts',(-21.8694073476483,-12.644946835435,
115.352401047758)) ;
#180874 = CARTESIAN_POINT('Ctrl Pts',(-21.7956034852775,-12.6449467832351,
115.376632031723)) ;
#180875 = CARTESIAN_POINT('Ctrl Pts',(-21.7217996229066,-12.6449467310352,
115.400863015687)) ;
#180876 = CARTESIAN_POINT('Ctrl Pts',(-21.7371855935328,-12.5872503984288,
115.447726201246)) ;
#180877 = CARTESIAN_POINT('Ctrl Pts',(-21.752571564159,-12.5295540658224,
115.494589386805)) ;
#180878 = CARTESIAN_POINT('Ctrl Pts',(-21.8263754265299,-12.5295541180224,
115.47035840284)) ;
#180879 = CARTESIAN_POINT('Ctrl Pts',(-21.9001792889008,-12.5295541702223,
115.446127418876)) ;
#180880 = CARTESIAN_POINT('Ctrl Pts',(-21.8847933182746,-12.5872505028287,
115.399264233317)) ;
#180881 = CARTESIAN_POINT('Ctrl Pts',(-21.7976012004924,-12.4304809457012,
115.169196272267)) ;
#180882 = CARTESIAN_POINT('Ctrl Pts',(-21.7875456541485,-12.4992062995871,
115.138568698872)) ;
#180883 = CARTESIAN_POINT('Ctrl Pts',(-21.7137417860944,-12.4992062624081,
115.162799665526)) ;
#180884 = CARTESIAN_POINT('Ctrl Pts',(-21.6399379180403,-12.4992062252292,
115.187030632181)) ;
#180885 = CARTESIAN_POINT('Ctrl Pts',(-21.6499934643842,-12.4304808713433,
115.217658205575)) ;
#180886 = CARTESIAN_POINT('Ctrl Pts',(-21.6600490107281,-12.3617555174574,
115.24828577897)) ;
#180887 = CARTESIAN_POINT('Ctrl Pts',(-21.7338528787822,-12.3617555546364,
115.224054812315)) ;
#180888 = CARTESIAN_POINT('Ctrl Pts',(-21.8076567468363,-12.3617555918153,
115.199823845661)) ;
#180889 = CARTESIAN_POINT('Ctrl Pts',(-21.7976012004924,-12.4304809457012,
115.169196272267)) ;
#180890 = CARTESIAN_POINT('Ctrl Pts',(-21.700169966331,-12.3447676693836,
114.907940821846)) ;
#180891 = CARTESIAN_POINT('Ctrl Pts',(-21.6961674254043,-12.4195774199376,
114.895749726183)) ;
#180892 = CARTESIAN_POINT('Ctrl Pts',(-21.6223635532352,-12.4195774042201,
114.919980680304)) ;
#180893 = CARTESIAN_POINT('Ctrl Pts',(-21.548559681066,-12.4195773885026,
114.944211634424)) ;
#180894 = CARTESIAN_POINT('Ctrl Pts',(-21.5525622219927,-12.3447676379485,
114.956402730087)) ;
#180895 = CARTESIAN_POINT('Ctrl Pts',(-21.5565647629194,-12.2699578873945,
114.96859382575)) ;
#180896 = CARTESIAN_POINT('Ctrl Pts',(-21.6303686350885,-12.269957903112,
114.944362871629)) ;
#180897 = CARTESIAN_POINT('Ctrl Pts',(-21.7041725072576,-12.2699579188295,
114.920131917509)) ;
#180898 = CARTESIAN_POINT('Ctrl Pts',(-21.700169966331,-12.3447676693836,
114.907940821846)) ;
#180899 = CARTESIAN_POINT('Ctrl Pts',(-21.5992738440407,-12.3358385329225,
114.635951321801)) ;
#180900 = CARTESIAN_POINT('Ctrl Pts',(-21.6015788063553,-12.4113804397121,
114.642971863216)) ;
#180901 = CARTESIAN_POINT('Ctrl Pts',(-21.5277749325704,-12.4113804494303,
114.667202812415)) ;
#180902 = CARTESIAN_POINT('Ctrl Pts',(-21.4539710587855,-12.4113804591485,
114.691433761613)) ;
#180903 = CARTESIAN_POINT('Ctrl Pts',(-21.4516660964708,-12.335838552359,
114.684413220199)) ;
#180904 = CARTESIAN_POINT('Ctrl Pts',(-21.4493611341561,-12.2602966455695,
114.677392678784)) ;
#180905 = CARTESIAN_POINT('Ctrl Pts',(-21.523165007941,-12.2602966358513,
114.653161729585)) ;
#180906 = CARTESIAN_POINT('Ctrl Pts',(-21.596968881726,-12.260296626133,114.628930780386)) ;
#180907 = CARTESIAN_POINT('Ctrl Pts',(-21.5992738440407,-12.3358385329225,
114.635951321801)) ;
#180908 = CARTESIAN_POINT('Ctrl Pts',(-21.5003785782672,-12.4042599768703,
114.370232214751)) ;
#180909 = CARTESIAN_POINT('Ctrl Pts',(-21.5088568368988,-12.4751356263476,
114.396055620604)) ;
#180910 = CARTESIAN_POINT('Ctrl Pts',(-21.4350529637228,-12.4751356632063,
114.420286571658)) ;
#180911 = CARTESIAN_POINT('Ctrl Pts',(-21.3612490905468,-12.4751357000651,
114.444517522711)) ;
#180912 = CARTESIAN_POINT('Ctrl Pts',(-21.3527708319152,-12.4042600505878,
114.418694116858)) ;
#180913 = CARTESIAN_POINT('Ctrl Pts',(-21.3442925732836,-12.3333844011106,
114.392870711006)) ;
#180914 = CARTESIAN_POINT('Ctrl Pts',(-21.4180964464596,-12.3333843642518,
114.368639759952)) ;
#180915 = CARTESIAN_POINT('Ctrl Pts',(-21.4919003196355,-12.3333843273931,
114.344408808898)) ;
#180916 = CARTESIAN_POINT('Ctrl Pts',(-21.5003785782672,-12.4042599768703,
114.370232214751)) ;
#180917 = CARTESIAN_POINT('Ctrl Pts',(-21.4104042015346,-12.5454038835963,
114.131652978612)) ;
#180918 = CARTESIAN_POINT('Ctrl Pts',(-21.4244426778221,-12.6065294802411,
114.174411910246)) ;
#180919 = CARTESIAN_POINT('Ctrl Pts',(-21.3506388079976,-12.6065295430782,
114.198642871508)) ;
#180920 = CARTESIAN_POINT('Ctrl Pts',(-21.2768349381732,-12.6065296059152,
114.22287383277)) ;
#180921 = CARTESIAN_POINT('Ctrl Pts',(-21.2627964618856,-12.5454040092703,
114.180114901136)) ;
#180922 = CARTESIAN_POINT('Ctrl Pts',(-21.2487579855981,-12.4842784126255,
114.137355969502)) ;
#180923 = CARTESIAN_POINT('Ctrl Pts',(-21.3225618554226,-12.4842783497885,
114.11312500824)) ;
#180924 = CARTESIAN_POINT('Ctrl Pts',(-21.3963657252471,-12.4842782869515,
114.088894046978)) ;
#180925 = CARTESIAN_POINT('Ctrl Pts',(-21.4104042015346,-12.5454038835963,
114.131652978612)) ;
#180926 = CARTESIAN_POINT('Ctrl Pts',(-21.3349456169578,-12.7490645526663,
113.9372922249)) ;
#180927 = CARTESIAN_POINT('Ctrl Pts',(-21.3535389852584,-12.796061398436,
113.993924622637)) ;
#180928 = CARTESIAN_POINT('Ctrl Pts',(-21.2797351212098,-12.7960614831609,
114.018155601491)) ;
#180929 = CARTESIAN_POINT('Ctrl Pts',(-21.2059312571613,-12.7960615678859,
114.042386580345)) ;
#180930 = CARTESIAN_POINT('Ctrl Pts',(-21.1873378888607,-12.7490647221162,
113.985754182609)) ;
#180931 = CARTESIAN_POINT('Ctrl Pts',(-21.1687445205602,-12.7020678763465,
113.929121784872)) ;
#180932 = CARTESIAN_POINT('Ctrl Pts',(-21.2425483846087,-12.7020677916216,
113.904890806017)) ;
#180933 = CARTESIAN_POINT('Ctrl Pts',(-21.3163522486572,-12.7020677068967,
113.880659827163)) ;
#180934 = CARTESIAN_POINT('Ctrl Pts',(-21.3349456169578,-12.7490645526663,
113.9372922249)) ;
#180935 = CARTESIAN_POINT('Ctrl Pts',(-21.278705237238,-13.0004109945635,
113.801433245637)) ;
#180936 = CARTESIAN_POINT('Ctrl Pts',(-21.300519235436,-13.0299291555683,
113.867875162378)) ;
#180937 = CARTESIAN_POINT('Ctrl Pts',(-21.2267153790532,-13.0299292556675,
113.892106164581)) ;
#180938 = CARTESIAN_POINT('Ctrl Pts',(-21.1529115226705,-13.0299293557667,
113.916337166784)) ;
#180939 = CARTESIAN_POINT('Ctrl Pts',(-21.1310975244725,-13.0004111947619,
113.849895250044)) ;
#180940 = CARTESIAN_POINT('Ctrl Pts',(-21.1092835262744,-12.9708930337571,
113.783453333303)) ;
#180941 = CARTESIAN_POINT('Ctrl Pts',(-21.1830873826572,-12.9708929336578,
113.7592223311)) ;
#180942 = CARTESIAN_POINT('Ctrl Pts',(-21.25689123904,-12.9708928335586,113.734991328897)) ;
#180943 = CARTESIAN_POINT('Ctrl Pts',(-21.278705237238,-13.0004109945635,
113.801433245637)) ;
#180944 = CARTESIAN_POINT('Ctrl Pts',(-21.2448570719353,-13.281956740539,
113.733818494743)) ;
#180945 = CARTESIAN_POINT('Ctrl Pts',(-21.2683324030269,-13.2918622013087,
113.805320563426)) ;
#180946 = CARTESIAN_POINT('Ctrl Pts',(-21.1945285554331,-13.2918623086419,
113.8295515924)) ;
#180947 = CARTESIAN_POINT('Ctrl Pts',(-21.1207247078394,-13.2918624159751,
113.853782621373)) ;
#180948 = CARTESIAN_POINT('Ctrl Pts',(-21.0972493767479,-13.2819569552054,
113.782280552689)) ;
#180949 = CARTESIAN_POINT('Ctrl Pts',(-21.0737740456563,-13.2720514944356,
113.710778484005)) ;
#180950 = CARTESIAN_POINT('Ctrl Pts',(-21.14757789325,-13.2720513871025,113.686547455032)) ;
#180951 = CARTESIAN_POINT('Ctrl Pts',(-21.2213817408438,-13.2720512797693,
113.662316426059)) ;
#180952 = CARTESIAN_POINT('Ctrl Pts',(-21.2448570719353,-13.281956740539,
113.733818494743)) ;
#180953 = CARTESIAN_POINT('Ctrl Pts',(-21.2351498447256,-13.573019683806,
113.739702682927)) ;
#180954 = CARTESIAN_POINT('Ctrl Pts',(-21.2586042557794,-13.5626188486144,
113.811141032577)) ;
#180955 = CARTESIAN_POINT('Ctrl Pts',(-21.1848004171839,-13.5626189543087,
113.835372088957)) ;
#180956 = CARTESIAN_POINT('Ctrl Pts',(-21.1109965785883,-13.5626190600031,
113.859603145337)) ;
#180957 = CARTESIAN_POINT('Ctrl Pts',(-21.0875421675344,-13.5730198951947,
113.788164795687)) ;
#180958 = CARTESIAN_POINT('Ctrl Pts',(-21.0640877564806,-13.5834207303863,
113.716726446036)) ;
#180959 = CARTESIAN_POINT('Ctrl Pts',(-21.1378915950762,-13.583420624692,
113.692495389656)) ;
#180960 = CARTESIAN_POINT('Ctrl Pts',(-21.2116954336718,-13.5834205189976,
113.668264333277)) ;
#180961 = CARTESIAN_POINT('Ctrl Pts',(-21.2351498447256,-13.573019683806,
113.739702682927)) ;
#180962 = CARTESIAN_POINT('Ctrl Pts',(-21.2495046916565,-13.8532505028034,
113.818910957215)) ;
#180963 = CARTESIAN_POINT('Ctrl Pts',(-21.2712576372625,-13.823269355178,
113.885166917691)) ;
#180964 = CARTESIAN_POINT('Ctrl Pts',(-21.1974538069553,-13.823269450611,
113.909397999316)) ;
#180965 = CARTESIAN_POINT('Ctrl Pts',(-21.1236499766481,-13.8232695460439,
113.933629080941)) ;
#180966 = CARTESIAN_POINT('Ctrl Pts',(-21.101897031042,-13.8532506936693,
113.867373120465)) ;
#180967 = CARTESIAN_POINT('Ctrl Pts',(-21.080144085436,-13.8832318412947,
113.801117159989)) ;
#180968 = CARTESIAN_POINT('Ctrl Pts',(-21.1539479157432,-13.8832317458617,
113.776886078364)) ;
#180969 = CARTESIAN_POINT('Ctrl Pts',(-21.2277517460505,-13.8832316504288,
113.752654996739)) ;
#180970 = CARTESIAN_POINT('Ctrl Pts',(-21.2495046916565,-13.8532505028034,
113.818910957215)) ;
#180971 = CARTESIAN_POINT('Ctrl Pts',(-21.2861585371864,-14.1021597581384,
113.966023254985)) ;
#180972 = CARTESIAN_POINT('Ctrl Pts',(-21.3046510157037,-14.0547556097992,
114.022348358853)) ;
#180973 = CARTESIAN_POINT('Ctrl Pts',(-21.2308471921295,-14.0547556877835,
114.046579460986)) ;
#180974 = CARTESIAN_POINT('Ctrl Pts',(-21.1570433685553,-14.0547557657678,
114.070810563118)) ;
#180975 = CARTESIAN_POINT('Ctrl Pts',(-21.138550890038,-14.102159914107,114.01448545925)) ;
#180976 = CARTESIAN_POINT('Ctrl Pts',(-21.1200584115207,-14.1495640624461,
113.958160355381)) ;
#180977 = CARTESIAN_POINT('Ctrl Pts',(-21.1938622350949,-14.1495639844619,
113.933929253249)) ;
#180978 = CARTESIAN_POINT('Ctrl Pts',(-21.2676660586691,-14.1495639064776,
113.909698151116)) ;
#180979 = CARTESIAN_POINT('Ctrl Pts',(-21.2861585371864,-14.1021597581384,
113.966023254985)) ;
#180980 = CARTESIAN_POINT('Ctrl Pts',(-21.3416525533176,-14.3018608409922,
114.170484973414)) ;
#180981 = CARTESIAN_POINT('Ctrl Pts',(-21.3555650519419,-14.240442969134,
114.212860197592)) ;
#180982 = CARTESIAN_POINT('Ctrl Pts',(-21.2817612329827,-14.2404430248273,
114.237091313781)) ;
#180983 = CARTESIAN_POINT('Ctrl Pts',(-21.2079574140235,-14.2404430805207,
114.261322429971)) ;
#180984 = CARTESIAN_POINT('Ctrl Pts',(-21.1940449153992,-14.3018609523788,
114.218947205793)) ;
#180985 = CARTESIAN_POINT('Ctrl Pts',(-21.1801324167749,-14.3632788242369,
114.176571981615)) ;
#180986 = CARTESIAN_POINT('Ctrl Pts',(-21.2539362357341,-14.3632787685436,
114.152340865426)) ;
#180987 = CARTESIAN_POINT('Ctrl Pts',(-21.3277400546933,-14.3632787128503,
114.128109749236)) ;
#180988 = CARTESIAN_POINT('Ctrl Pts',(-21.3416525533176,-14.3018608409922,
114.170484973414)) ;
#180989 = CARTESIAN_POINT('Ctrl Pts',(-21.411315277641,-14.4384983198451,
114.418115610093)) ;
#180990 = CARTESIAN_POINT('Ctrl Pts',(-21.4196514727048,-14.3674483770308,
114.443506313464)) ;
#180991 = CARTESIAN_POINT('Ctrl Pts',(-21.3458476559104,-14.3674484079295,
114.467737436247)) ;
#180992 = CARTESIAN_POINT('Ctrl Pts',(-21.2720438391161,-14.3674484388281,
114.49196855903)) ;
#180993 = CARTESIAN_POINT('Ctrl Pts',(-21.2637076440523,-14.4384983816424,
114.466577855659)) ;
#180994 = CARTESIAN_POINT('Ctrl Pts',(-21.2553714489885,-14.5095483244567,
114.441187152289)) ;
#180995 = CARTESIAN_POINT('Ctrl Pts',(-21.3291752657829,-14.509548293558,
114.416956029506)) ;
#180996 = CARTESIAN_POINT('Ctrl Pts',(-21.4029790825773,-14.5095482626594,
114.392724906723)) ;
#180997 = CARTESIAN_POINT('Ctrl Pts',(-21.411315277641,-14.4384983198451,
114.418115610093)) ;
#180998 = CARTESIAN_POINT('Ctrl Pts',(-21.4896790967479,-14.5020770602936,
114.692365991293)) ;
#180999 = CARTESIAN_POINT('Ctrl Pts',(-21.4918207117146,-14.4264807176174,
114.698889003319)) ;
#181000 = CARTESIAN_POINT('Ctrl Pts',(-21.4180168942886,-14.4264807240547,
114.723120124178)) ;
#181001 = CARTESIAN_POINT('Ctrl Pts',(-21.3442130768625,-14.426480730492,
114.747351245037)) ;
#181002 = CARTESIAN_POINT('Ctrl Pts',(-21.3420714618958,-14.5020770731682,
114.740828233011)) ;
#181003 = CARTESIAN_POINT('Ctrl Pts',(-21.339929846929,-14.5776734158445,
114.734305220985)) ;
#181004 = CARTESIAN_POINT('Ctrl Pts',(-21.4137336643551,-14.5776734094072,
114.710074100126)) ;
#181005 = CARTESIAN_POINT('Ctrl Pts',(-21.4875374817811,-14.5776734029699,
114.685842979267)) ;
#181006 = CARTESIAN_POINT('Ctrl Pts',(-21.4896790967479,-14.5020770602936,
114.692365991293)) ;
#181007 = CARTESIAN_POINT('Ctrl Pts',(-21.5697542529171,-14.48777877411,114.971664919752)) ;
#181008 = CARTESIAN_POINT('Ctrl Pts',(-21.5655757371925,-14.4130666847603,
114.958937833571)) ;
#181009 = CARTESIAN_POINT('Ctrl Pts',(-21.4917719173005,-14.413066670136,
114.98316894692)) ;
#181010 = CARTESIAN_POINT('Ctrl Pts',(-21.4179680974086,-14.4130666555116,
115.007400060268)) ;
#181011 = CARTESIAN_POINT('Ctrl Pts',(-21.4221466131332,-14.4877787448612,
115.020127146449)) ;
#181012 = CARTESIAN_POINT('Ctrl Pts',(-21.4263251288578,-14.5624908342109,
115.032854232629)) ;
#181013 = CARTESIAN_POINT('Ctrl Pts',(-21.5001289487497,-14.5624908488352,
115.008623119281)) ;
#181014 = CARTESIAN_POINT('Ctrl Pts',(-21.5739327686417,-14.5624908634596,
114.984392005932)) ;
#181015 = CARTESIAN_POINT('Ctrl Pts',(-21.5697542529171,-14.48777877411,114.971664919752)) ;
#181016 = CARTESIAN_POINT('Ctrl Pts',(-21.6455150626232,-14.3970097456745,
115.237875186916)) ;
#181017 = CARTESIAN_POINT('Ctrl Pts',(-21.6353069764491,-14.3285220925645,
115.206783002163)) ;
#181018 = CARTESIAN_POINT('Ctrl Pts',(-21.5615031523443,-14.3285220617789,
115.231014102679)) ;
#181019 = CARTESIAN_POINT('Ctrl Pts',(-21.4876993282394,-14.3285220309933,
115.255245203196)) ;
#181020 = CARTESIAN_POINT('Ctrl Pts',(-21.4979074144135,-14.3970096841033,
115.286337387949)) ;
#181021 = CARTESIAN_POINT('Ctrl Pts',(-21.5081155005876,-14.4654973372134,
115.317429572702)) ;
#181022 = CARTESIAN_POINT('Ctrl Pts',(-21.5819193246924,-14.465497367999,
115.293198472186)) ;
#181023 = CARTESIAN_POINT('Ctrl Pts',(-21.6557231487973,-14.4654973987846,
115.268967371669)) ;
#181024 = CARTESIAN_POINT('Ctrl Pts',(-21.6455150626232,-14.3970097456745,
115.237875186916)) ;
#181025 = CARTESIAN_POINT('Ctrl Pts',(-21.7106846353234,-14.2362612997962,
115.471811422078)) ;
#181026 = CARTESIAN_POINT('Ctrl Pts',(-21.6951775844478,-14.1788934065685,
115.424579445984)) ;
#181027 = CARTESIAN_POINT('Ctrl Pts',(-21.6213737551867,-14.1788933656858,
115.448810530796)) ;
#181028 = CARTESIAN_POINT('Ctrl Pts',(-21.5475699259256,-14.178893324803,
115.473041615607)) ;
#181029 = CARTESIAN_POINT('Ctrl Pts',(-21.5630769768012,-14.2362612180308,
115.520273591701)) ;
#181030 = CARTESIAN_POINT('Ctrl Pts',(-21.5785840276768,-14.2936291112585,
115.567505567795)) ;
#181031 = CARTESIAN_POINT('Ctrl Pts',(-21.6523878569379,-14.2936291521412,
115.543274482984)) ;
#181032 = CARTESIAN_POINT('Ctrl Pts',(-21.726191686199,-14.293629193024,115.519043398172)) ;
#181033 = CARTESIAN_POINT('Ctrl Pts',(-21.7106846353234,-14.2362612997962,
115.471811422078)) ;
#181034 = CARTESIAN_POINT('Ctrl Pts',(-21.7599663610644,-14.0159101115065,
115.65749922043)) ;
#181035 = CARTESIAN_POINT('Ctrl Pts',(-21.740258470966,-13.973840125215,115.597472166055)) ;
#181036 = CARTESIAN_POINT('Ctrl Pts',(-21.666454636156,-13.97384008191,115.621703233965)) ;
#181037 = CARTESIAN_POINT('Ctrl Pts',(-21.592650801346,-13.973840038605,115.645934301876)) ;
#181038 = CARTESIAN_POINT('Ctrl Pts',(-21.6123586914444,-14.0159100248966,
115.705961356251)) ;
#181039 = CARTESIAN_POINT('Ctrl Pts',(-21.6320665815428,-14.0579800111881,
115.765988410626)) ;
#181040 = CARTESIAN_POINT('Ctrl Pts',(-21.7058704163528,-14.0579800544931,
115.741757342715)) ;
#181041 = CARTESIAN_POINT('Ctrl Pts',(-21.7796742511628,-14.0579800977981,
115.717526274805)) ;
#181042 = CARTESIAN_POINT('Ctrl Pts',(-21.7599663610644,-14.0159101115065,
115.65749922043)) ;
#181043 = CARTESIAN_POINT('Ctrl Pts',(-21.7887254354454,-13.7543350935969,
115.7804395058)) ;
#181044 = CARTESIAN_POINT('Ctrl Pts',(-21.7662483401476,-13.7304650573216,
115.711977899343)) ;
#181045 = CARTESIAN_POINT('Ctrl Pts',(-21.6924445007129,-13.730465015473,
115.736208953168)) ;
#181046 = CARTESIAN_POINT('Ctrl Pts',(-21.6186406612782,-13.7304649736245,
115.760440006992)) ;
#181047 = CARTESIAN_POINT('Ctrl Pts',(-21.6411177565759,-13.7543350098997,
115.828901613449)) ;
#181048 = CARTESIAN_POINT('Ctrl Pts',(-21.6635948518736,-13.778205046175,
115.897363219905)) ;
#181049 = CARTESIAN_POINT('Ctrl Pts',(-21.7373986913083,-13.7782050880236,
115.873132166081)) ;
#181050 = CARTESIAN_POINT('Ctrl Pts',(-21.8112025307431,-13.7782051298721,
115.848901112257)) ;
#181051 = CARTESIAN_POINT('Ctrl Pts',(-21.7887254354454,-13.7543350935969,
115.7804395058)) ;
#181052 = CARTESIAN_POINT('Ctrl Pts',(-21.7944517107035,-13.4665595551094,
115.833506874945)) ;
#181053 = CARTESIAN_POINT('Ctrl Pts',(-21.7708033171206,-13.4627465020412,
115.761477683097)) ;
#181054 = CARTESIAN_POINT('Ctrl Pts',(-21.6969994739287,-13.4627464684725,
115.785708725478)) ;
#181055 = CARTESIAN_POINT('Ctrl Pts',(-21.6231956307368,-13.4627464349037,
115.809939767858)) ;
#181056 = CARTESIAN_POINT('Ctrl Pts',(-21.6468440243196,-13.4665594879718,
115.881968959706)) ;
#181057 = CARTESIAN_POINT('Ctrl Pts',(-21.6704924179025,-13.4703725410399,
115.953998151553)) ;
#181058 = CARTESIAN_POINT('Ctrl Pts',(-21.7442962610944,-13.4703725746087,
115.929767109173)) ;
#181059 = CARTESIAN_POINT('Ctrl Pts',(-21.8181001042863,-13.4703726081775,
115.905536066792)) ;
#181060 = CARTESIAN_POINT('Ctrl Pts',(-21.7944517107035,-13.4665595551094,
115.833506874945)) ;
#181061 = CARTESIAN_POINT('Ctrl Pts',(-21.7759076496093,-13.1776643244991,
115.812347038779)) ;
#181062 = CARTESIAN_POINT('Ctrl Pts',(-21.7527874084242,-13.1940170948714,
115.741926514053)) ;
#181063 = CARTESIAN_POINT('Ctrl Pts',(-21.6789835629887,-13.1940170691323,
115.7661575496)) ;
#181064 = CARTESIAN_POINT('Ctrl Pts',(-21.6051797175531,-13.1940170433932,
115.790388585147)) ;
#181065 = CARTESIAN_POINT('Ctrl Pts',(-21.6282999587382,-13.1776642730209,
115.860809109873)) ;
#181066 = CARTESIAN_POINT('Ctrl Pts',(-21.6514201999233,-13.1613115026485,
115.931229634599)) ;
#181067 = CARTESIAN_POINT('Ctrl Pts',(-21.7252240453588,-13.1613115283877,
115.906998599052)) ;
#181068 = CARTESIAN_POINT('Ctrl Pts',(-21.7990278907943,-13.1613115541268,
115.882767563505)) ;
#181069 = CARTESIAN_POINT('Ctrl Pts',(-21.7759076496093,-13.1776643244991,
115.812347038779)) ;
#181070 = CARTESIAN_POINT('Ctrl Pts',(-21.7336480522878,-12.90467088677,115.719119626664)) ;
#181071 = CARTESIAN_POINT('Ctrl Pts',(-21.7127091437857,-12.9401099840166,
115.655343089489)) ;
#181072 = CARTESIAN_POINT('Ctrl Pts',(-21.6389052974629,-12.9401099680248,
115.679574122334)) ;
#181073 = CARTESIAN_POINT('Ctrl Pts',(-21.5651014511401,-12.9401099520331,
115.703805155178)) ;
#181074 = CARTESIAN_POINT('Ctrl Pts',(-21.5860403596422,-12.9046708547865,
115.767581692352)) ;
#181075 = CARTESIAN_POINT('Ctrl Pts',(-21.6069792681442,-12.86923175754,115.831358229527)) ;
#181076 = CARTESIAN_POINT('Ctrl Pts',(-21.680783114467,-12.8692317735317,
115.807127196682)) ;
#181077 = CARTESIAN_POINT('Ctrl Pts',(-21.7545869607898,-12.8692317895235,
115.782896163838)) ;
#181078 = CARTESIAN_POINT('Ctrl Pts',(-21.7336480522878,-12.90467088677,115.719119626664)) ;
#181079 = CARTESIAN_POINT('Ctrl Pts',(-21.670032619818,-12.6688603640825,
115.560779753081)) ;
#181080 = CARTESIAN_POINT('Ctrl Pts',(-21.6527710229661,-12.7208184006723,
115.508203713992)) ;
#181081 = CARTESIAN_POINT('Ctrl Pts',(-21.5789671769035,-12.7208183925847,
115.532434747629)) ;
#181082 = CARTESIAN_POINT('Ctrl Pts',(-21.505163330841,-12.7208183844972,
115.556665781266)) ;
#181083 = CARTESIAN_POINT('Ctrl Pts',(-21.5224249276929,-12.6688603479075,
115.609241820356)) ;
#181084 = CARTESIAN_POINT('Ctrl Pts',(-21.5396865245448,-12.6169023113178,
115.661817859445)) ;
#181085 = CARTESIAN_POINT('Ctrl Pts',(-21.6134903706073,-12.6169023194053,
115.637586825808)) ;
#181086 = CARTESIAN_POINT('Ctrl Pts',(-21.6872942166699,-12.6169023274928,
115.613355792171)) ;
#181087 = CARTESIAN_POINT('Ctrl Pts',(-21.670032619818,-12.6688603640825,
115.560779753081)) ;
#181088 = CARTESIAN_POINT('Ctrl Pts',(-21.5885287279957,-12.48602188738,115.348081223403)) ;
#181089 = CARTESIAN_POINT('Ctrl Pts',(-21.5761965323051,-12.5508253721629,
115.310519345023)) ;
#181090 = CARTESIAN_POINT('Ctrl Pts',(-21.5023926874474,-12.5508253699932,
115.33475038233)) ;
#181091 = CARTESIAN_POINT('Ctrl Pts',(-21.4285888425897,-12.5508253678235,
115.358981419637)) ;
#181092 = CARTESIAN_POINT('Ctrl Pts',(-21.4409210382802,-12.4860218830405,
115.396543298016)) ;
#181093 = CARTESIAN_POINT('Ctrl Pts',(-21.4532532339708,-12.4212183982575,
115.434105176396)) ;
#181094 = CARTESIAN_POINT('Ctrl Pts',(-21.5270570788285,-12.4212184004273,
115.409874139089)) ;
#181095 = CARTESIAN_POINT('Ctrl Pts',(-21.6008609236862,-12.421218402597,
115.385643101782)) ;
#181096 = CARTESIAN_POINT('Ctrl Pts',(-21.5885287279957,-12.48602188738,115.348081223403)) ;
#181097 = CARTESIAN_POINT('Ctrl Pts',(-21.4945267923872,-12.3704601308902,
115.097266800152)) ;
#181098 = CARTESIAN_POINT('Ctrl Pts',(-21.4880053381033,-12.4434303508523,
115.077403502628)) ;
#181099 = CARTESIAN_POINT('Ctrl Pts',(-21.4142014945595,-12.4434303510562,
115.101634543937)) ;
#181100 = CARTESIAN_POINT('Ctrl Pts',(-21.3403976510158,-12.4434303512601,
115.125865585246)) ;
#181101 = CARTESIAN_POINT('Ctrl Pts',(-21.3469191052998,-12.370460131298,
115.14572888277)) ;
#181102 = CARTESIAN_POINT('Ctrl Pts',(-21.3534405595837,-12.297489911336,
115.165592180293)) ;
#181103 = CARTESIAN_POINT('Ctrl Pts',(-21.4272444031274,-12.2974899111321,
115.141361138984)) ;
#181104 = CARTESIAN_POINT('Ctrl Pts',(-21.5010482466712,-12.2974899109282,
115.117130097675)) ;
#181105 = CARTESIAN_POINT('Ctrl Pts',(-21.4945267923872,-12.3704601308902,
115.097266800152)) ;
#181106 = CARTESIAN_POINT('Ctrl Pts',(-21.3942570657881,-12.3301504850153,
114.827261741778)) ;
#181107 = CARTESIAN_POINT('Ctrl Pts',(-21.3939948822089,-12.406044193393,
114.826463172943)) ;
#181108 = CARTESIAN_POINT('Ctrl Pts',(-21.3201910395033,-12.4060441935951,
114.850694216804)) ;
#181109 = CARTESIAN_POINT('Ctrl Pts',(-21.2463871967976,-12.4060441937972,
114.874925260666)) ;
#181110 = CARTESIAN_POINT('Ctrl Pts',(-21.2466493803768,-12.3301504854195,
114.875723829501)) ;
#181111 = CARTESIAN_POINT('Ctrl Pts',(-21.2469115639559,-12.2542567770418,
114.876522398337)) ;
#181112 = CARTESIAN_POINT('Ctrl Pts',(-21.3207154066615,-12.2542567768397,
114.852291354475)) ;
#181113 = CARTESIAN_POINT('Ctrl Pts',(-21.3945192493672,-12.2542567766376,
114.828060310614)) ;
#181114 = CARTESIAN_POINT('Ctrl Pts',(-21.3942570657881,-12.3301504850153,
114.827261741778)) ;
#181115 = CARTESIAN_POINT('Ctrl Pts',(-21.2939223840727,-12.3670848663884,
114.557023720825)) ;
#181116 = CARTESIAN_POINT('Ctrl Pts',(-21.299934115299,-12.440512077599,114.57533448422)) ;
#181117 = CARTESIAN_POINT('Ctrl Pts',(-21.2261302729601,-12.4405120766493,
114.599565529198)) ;
#181118 = CARTESIAN_POINT('Ctrl Pts',(-21.1523264306211,-12.4405120756996,
114.623796574177)) ;
#181119 = CARTESIAN_POINT('Ctrl Pts',(-21.1463146993948,-12.367084864489,
114.605485810782)) ;
#181120 = CARTESIAN_POINT('Ctrl Pts',(-21.1403029681685,-12.2936576532783,
114.587175047387)) ;
#181121 = CARTESIAN_POINT('Ctrl Pts',(-21.2141068105074,-12.293657654228,
114.562944002409)) ;
#181122 = CARTESIAN_POINT('Ctrl Pts',(-21.2879106528464,-12.2936576551777,
114.53871295743)) ;
#181123 = CARTESIAN_POINT('Ctrl Pts',(-21.2939223840727,-12.3670848663884,
114.557023720825)) ;
#181124 = CARTESIAN_POINT('Ctrl Pts',(-21.1989536269659,-12.4806961242678,
114.303499956068)) ;
#181125 = CARTESIAN_POINT('Ctrl Pts',(-21.2108665545281,-12.5462988180666,
114.339784811313)) ;
#181126 = CARTESIAN_POINT('Ctrl Pts',(-21.1370627115663,-12.5462988169735,
114.364015854394)) ;
#181127 = CARTESIAN_POINT('Ctrl Pts',(-21.0632588686045,-12.5462988158804,
114.388246897476)) ;
#181128 = CARTESIAN_POINT('Ctrl Pts',(-21.0513459410423,-12.4806961220815,
114.351962042231)) ;
#181129 = CARTESIAN_POINT('Ctrl Pts',(-21.0394330134802,-12.4150934282827,
114.315677186986)) ;
#181130 = CARTESIAN_POINT('Ctrl Pts',(-21.113236856442,-12.4150934293758,
114.291446143904)) ;
#181131 = CARTESIAN_POINT('Ctrl Pts',(-21.1870406994037,-12.415093430469,
114.267215100823)) ;
#181132 = CARTESIAN_POINT('Ctrl Pts',(-21.1989536269659,-12.4806961242678,
114.303499956068)) ;
#181133 = CARTESIAN_POINT('Ctrl Pts',(-21.1174616220678,-12.659847054779,
114.090572179847)) ;
#181134 = CARTESIAN_POINT('Ctrl Pts',(-21.1343519658611,-12.7130362017687,
114.142017441774)) ;
#181135 = CARTESIAN_POINT('Ctrl Pts',(-21.0605481221497,-12.7130362022566,
114.166248482573)) ;
#181136 = CARTESIAN_POINT('Ctrl Pts',(-20.9867442784384,-12.7130362027444,
114.190479523371)) ;
#181137 = CARTESIAN_POINT('Ctrl Pts',(-20.9698539346452,-12.6598470557547,
114.139034261444)) ;
#181138 = CARTESIAN_POINT('Ctrl Pts',(-20.9529635908519,-12.606657908765,
114.087588999516)) ;
#181139 = CARTESIAN_POINT('Ctrl Pts',(-21.0267674345633,-12.6066579082772,
114.063357958718)) ;
#181140 = CARTESIAN_POINT('Ctrl Pts',(-21.1005712782746,-12.6066579077893,
114.039126917919)) ;
#181141 = CARTESIAN_POINT('Ctrl Pts',(-21.1174616220678,-12.659847054779,
114.090572179847)) ;
#181142 = CARTESIAN_POINT('Ctrl Pts',(-21.0527943299023,-12.8944266812495,
113.929149642183)) ;
#181143 = CARTESIAN_POINT('Ctrl Pts',(-21.0734893261191,-12.9313139586903,
113.992183261414)) ;
#181144 = CARTESIAN_POINT('Ctrl Pts',(-20.9996854816442,-12.9313139638645,
114.016414299887)) ;
#181145 = CARTESIAN_POINT('Ctrl Pts',(-20.9258816371693,-12.9313139690387,
114.04064533836)) ;
#181146 = CARTESIAN_POINT('Ctrl Pts',(-20.9051866409525,-12.8944266915978,
113.977611719129)) ;
#181147 = CARTESIAN_POINT('Ctrl Pts',(-20.8844916447358,-12.8575394141569,
113.914578099897)) ;
#181148 = CARTESIAN_POINT('Ctrl Pts',(-20.9582954892107,-12.8575394089827,
113.890347061425)) ;
#181149 = CARTESIAN_POINT('Ctrl Pts',(-21.0320993336856,-12.8575394038086,
113.866116022952)) ;
#181150 = CARTESIAN_POINT('Ctrl Pts',(-21.0527943299023,-12.8944266812495,
113.929149642183)) ;
#181151 = CARTESIAN_POINT('Ctrl Pts',(-21.009715412858,-13.1656332510844,
113.833333116255)) ;
#181152 = CARTESIAN_POINT('Ctrl Pts',(-21.0327159486317,-13.183637429578,
113.903389036868)) ;
#181153 = CARTESIAN_POINT('Ctrl Pts',(-20.9589121041979,-13.1836374410536,
113.927620075466)) ;
#181154 = CARTESIAN_POINT('Ctrl Pts',(-20.885108259764,-13.1836374525291,
113.951851114064)) ;
#181155 = CARTESIAN_POINT('Ctrl Pts',(-20.8621077239903,-13.1656332740355,
113.88179519345)) ;
#181156 = CARTESIAN_POINT('Ctrl Pts',(-20.8391071882165,-13.1476290955419,
113.811739272837)) ;
#181157 = CARTESIAN_POINT('Ctrl Pts',(-20.9129110326504,-13.1476290840664,
113.787508234239)) ;
#181158 = CARTESIAN_POINT('Ctrl Pts',(-20.9867148770842,-13.1476290725908,
113.763277195641)) ;
#181159 = CARTESIAN_POINT('Ctrl Pts',(-21.009715412858,-13.1656332510844,
113.833333116255)) ;
#181160 = CARTESIAN_POINT('Ctrl Pts',(-20.9901169836703,-13.455130793988,
113.809077738093)) ;
#181161 = CARTESIAN_POINT('Ctrl Pts',(-21.0137859653004,-13.4529475727115,
113.8811696368)) ;
#181162 = CARTESIAN_POINT('Ctrl Pts',(-20.9399821218703,-13.452947591497,
113.905400678454)) ;
#181163 = CARTESIAN_POINT('Ctrl Pts',(-20.8661782784401,-13.4529476102826,
113.929631720109)) ;
#181164 = CARTESIAN_POINT('Ctrl Pts',(-20.84250929681,-13.4551308315591,113.857539821403)) ;
#181165 = CARTESIAN_POINT('Ctrl Pts',(-20.8188403151799,-13.4573140528355,
113.785447922696)) ;
#181166 = CARTESIAN_POINT('Ctrl Pts',(-20.89264415861,-13.45731403405,113.761216881042)) ;
#181167 = CARTESIAN_POINT('Ctrl Pts',(-20.9664480020402,-13.4573140152645,
113.736985839387)) ;
#181168 = CARTESIAN_POINT('Ctrl Pts',(-20.9901169836703,-13.455130793988,
113.809077738093)) ;
#181169 = CARTESIAN_POINT('Ctrl Pts',(-20.9948751859287,-13.7427936624919,
113.859110662264)) ;
#181170 = CARTESIAN_POINT('Ctrl Pts',(-21.0175108531374,-13.7205220170914,
113.928055251801)) ;
#181171 = CARTESIAN_POINT('Ctrl Pts',(-20.9437070120615,-13.7205220434154,
113.952286300627)) ;
#181172 = CARTESIAN_POINT('Ctrl Pts',(-20.8699031709856,-13.7205220697394,
113.976517349452)) ;
#181173 = CARTESIAN_POINT('Ctrl Pts',(-20.847267503777,-13.7427937151399,
113.907572759915)) ;
#181174 = CARTESIAN_POINT('Ctrl Pts',(-20.8246318365683,-13.7650653605404,
113.838628170377)) ;
#181175 = CARTESIAN_POINT('Ctrl Pts',(-20.8984356776442,-13.7650653342164,
113.814397121552)) ;
#181176 = CARTESIAN_POINT('Ctrl Pts',(-20.9722395187201,-13.7650653078924,
113.790166072726)) ;
#181177 = CARTESIAN_POINT('Ctrl Pts',(-20.9948751859287,-13.7427936624919,
113.859110662264)) ;
#181178 = CARTESIAN_POINT('Ctrl Pts',(-21.0227622802631,-14.0059776158613,
113.979433797495)) ;
#181179 = CARTESIAN_POINT('Ctrl Pts',(-21.0427513300967,-13.9652981717702,
114.040317217391)) ;
#181180 = CARTESIAN_POINT('Ctrl Pts',(-20.9689474924063,-13.9652982015733,
114.064548276528)) ;
#181181 = CARTESIAN_POINT('Ctrl Pts',(-20.895143654716,-13.9652982313764,
114.088779335666)) ;
#181182 = CARTESIAN_POINT('Ctrl Pts',(-20.8751546048824,-14.0059776754674,
114.02789591577)) ;
#181183 = CARTESIAN_POINT('Ctrl Pts',(-20.8551655550488,-14.0466571195585,
113.967012495875)) ;
#181184 = CARTESIAN_POINT('Ctrl Pts',(-20.9289693927392,-14.0466570897554,
113.942781436737)) ;
#181185 = CARTESIAN_POINT('Ctrl Pts',(-21.0027732304295,-14.0466570599524,
113.9185503776)) ;
#181186 = CARTESIAN_POINT('Ctrl Pts',(-21.0227622802631,-14.0059776158613,
113.979433797495)) ;
#181187 = CARTESIAN_POINT('Ctrl Pts',(-21.0711237055155,-14.2279037819529,
114.162216793604)) ;
#181188 = CARTESIAN_POINT('Ctrl Pts',(-21.0870308603311,-14.1716706622332,
114.210667419716)) ;
#181189 = CARTESIAN_POINT('Ctrl Pts',(-21.0132270269163,-14.1716706921349,
114.234898491876)) ;
#181190 = CARTESIAN_POINT('Ctrl Pts',(-20.9394231935014,-14.1716707220365,
114.259129564036)) ;
#181191 = CARTESIAN_POINT('Ctrl Pts',(-20.9235160386858,-14.2279038417561,
114.210678937924)) ;
#181192 = CARTESIAN_POINT('Ctrl Pts',(-20.9076088838701,-14.2841369614758,
114.162228311812)) ;
#181193 = CARTESIAN_POINT('Ctrl Pts',(-20.981412717285,-14.2841369315741,
114.137997239652)) ;
#181194 = CARTESIAN_POINT('Ctrl Pts',(-21.0552165506998,-14.2841369016725,
114.113766167492)) ;
#181195 = CARTESIAN_POINT('Ctrl Pts',(-21.0711237055155,-14.2279037819529,
114.162216793604)) ;
#181196 = CARTESIAN_POINT('Ctrl Pts',(-21.1359737665809,-14.3919406672911,
114.39531754647)) ;
#181197 = CARTESIAN_POINT('Ctrl Pts',(-21.1466400020903,-14.3241730854154,
114.427805177804)) ;
#181198 = CARTESIAN_POINT('Ctrl Pts',(-21.0728361735549,-14.3241731099825,
114.452036264826)) ;
#181199 = CARTESIAN_POINT('Ctrl Pts',(-20.9990323450195,-14.3241731345496,
114.476267351848)) ;
#181200 = CARTESIAN_POINT('Ctrl Pts',(-20.98836610951,-14.3919407164252,114.443779720514)) ;
#181201 = CARTESIAN_POINT('Ctrl Pts',(-20.9776998740006,-14.4597082983009,
114.41129208918)) ;
#181202 = CARTESIAN_POINT('Ctrl Pts',(-21.051503702536,-14.4597082737338,
114.387061002158)) ;
#181203 = CARTESIAN_POINT('Ctrl Pts',(-21.1253075310714,-14.4597082491667,
114.362829915136)) ;
#181204 = CARTESIAN_POINT('Ctrl Pts',(-21.1359737665809,-14.3919406672911,
114.39531754647)) ;
#181205 = CARTESIAN_POINT('Ctrl Pts',(-21.211254131552,-14.4855253459423,
114.659978503316)) ;
#181206 = CARTESIAN_POINT('Ctrl Pts',(-21.215947932786,-14.4111261442654,
114.674275063348)) ;
#181207 = CARTESIAN_POINT('Ctrl Pts',(-21.142144108098,-14.4111261567896,
114.698506162089)) ;
#181208 = CARTESIAN_POINT('Ctrl Pts',(-21.0683402834099,-14.4111261693137,
114.722737260829)) ;
#181209 = CARTESIAN_POINT('Ctrl Pts',(-21.0636464821759,-14.4855253709906,
114.708440700797)) ;
#181210 = CARTESIAN_POINT('Ctrl Pts',(-21.058952680942,-14.5599245726675,
114.694144140765)) ;
#181211 = CARTESIAN_POINT('Ctrl Pts',(-21.13275650563,-14.5599245601434,114.669913042024)) ;
#181212 = CARTESIAN_POINT('Ctrl Pts',(-21.206560330318,-14.5599245476192,
114.645681943284)) ;
#181213 = CARTESIAN_POINT('Ctrl Pts',(-21.211254131552,-14.4855253459423,
114.659978503316)) ;
#181214 = CARTESIAN_POINT('Ctrl Pts',(-21.2915339470349,-14.5029122651219,
114.940022641269)) ;
#181215 = CARTESIAN_POINT('Ctrl Pts',(-21.2898945125984,-14.4271913157213,
114.935029187143)) ;
#181216 = CARTESIAN_POINT('Ctrl Pts',(-21.2160906909928,-14.4271913111352,
114.959260295272)) ;
#181217 = CARTESIAN_POINT('Ctrl Pts',(-21.1422868693872,-14.427191306549,
114.983491403401)) ;
#181218 = CARTESIAN_POINT('Ctrl Pts',(-21.1439263038237,-14.5029122559496,
114.988484857527)) ;
#181219 = CARTESIAN_POINT('Ctrl Pts',(-21.1455657382602,-14.5786332053501,
114.993478311653)) ;
#181220 = CARTESIAN_POINT('Ctrl Pts',(-21.2193695598658,-14.5786332099363,
114.969247203524)) ;
#181221 = CARTESIAN_POINT('Ctrl Pts',(-21.2931733814714,-14.5786332145224,
114.945016095395)) ;
#181222 = CARTESIAN_POINT('Ctrl Pts',(-21.2915339470349,-14.5029122651219,
114.940022641269)) ;
#181223 = CARTESIAN_POINT('Ctrl Pts',(-21.3695938610987,-14.4429567945224,
115.213104290298)) ;
#181224 = CARTESIAN_POINT('Ctrl Pts',(-21.3617712091174,-14.3713125211074,
115.189277753062)) ;
#181225 = CARTESIAN_POINT('Ctrl Pts',(-21.2879673882971,-14.3713124959872,
115.213508863583)) ;
#181226 = CARTESIAN_POINT('Ctrl Pts',(-21.2141635674768,-14.371312470867,
115.237739974103)) ;
#181227 = CARTESIAN_POINT('Ctrl Pts',(-21.2219862194581,-14.4429567442819,
115.261566511339)) ;
#181228 = CARTESIAN_POINT('Ctrl Pts',(-21.2298088714394,-14.5146010176969,
115.285393048575)) ;
#181229 = CARTESIAN_POINT('Ctrl Pts',(-21.3036126922597,-14.5146010428171,
115.261161938054)) ;
#181230 = CARTESIAN_POINT('Ctrl Pts',(-21.37741651308,-14.5146010679373,115.236930827533)) ;
#181231 = CARTESIAN_POINT('Ctrl Pts',(-21.3695938610987,-14.4429567945224,
115.213104290298)) ;
#181232 = CARTESIAN_POINT('Ctrl Pts',(-21.4400444498509,-14.3088313127917,
115.463288416723)) ;
#181233 = CARTESIAN_POINT('Ctrl Pts',(-21.4265550909516,-14.2464468463962,
115.422202004376)) ;
#181234 = CARTESIAN_POINT('Ctrl Pts',(-21.352751269324,-14.2464467981566,
115.446433112437)) ;
#181235 = CARTESIAN_POINT('Ctrl Pts',(-21.2789474476964,-14.2464467499169,
115.470664220499)) ;
#181236 = CARTESIAN_POINT('Ctrl Pts',(-21.2924368065957,-14.3088312163124,
115.511750632847)) ;
#181237 = CARTESIAN_POINT('Ctrl Pts',(-21.3059261654949,-14.3712156827079,
115.552837045195)) ;
#181238 = CARTESIAN_POINT('Ctrl Pts',(-21.3797299871225,-14.3712157309476,
115.528605937133)) ;
#181239 = CARTESIAN_POINT('Ctrl Pts',(-21.4535338087501,-14.3712157791872,
115.504374829071)) ;
#181240 = CARTESIAN_POINT('Ctrl Pts',(-21.4400444498509,-14.3088313127917,
115.463288416723)) ;
#181241 = CARTESIAN_POINT('Ctrl Pts',(-21.4961500025639,-14.1118280044828,
115.669548634659)) ;
#181242 = CARTESIAN_POINT('Ctrl Pts',(-21.4779920712133,-14.0631071534286,
115.614242503785)) ;
#181243 = CARTESIAN_POINT('Ctrl Pts',(-21.4041882459561,-14.0631070839309,
115.638473600791)) ;
#181244 = CARTESIAN_POINT('Ctrl Pts',(-21.3303844206988,-14.0631070144332,
115.662704697798)) ;
#181245 = CARTESIAN_POINT('Ctrl Pts',(-21.3485423520494,-14.1118278654874,
115.718010828672)) ;
#181246 = CARTESIAN_POINT('Ctrl Pts',(-21.3667002834,-14.1605487165416,115.773316959545)) ;
#181247 = CARTESIAN_POINT('Ctrl Pts',(-21.4405041086572,-14.1605487860393,
115.749085862539)) ;
#181248 = CARTESIAN_POINT('Ctrl Pts',(-21.5143079339144,-14.160548855537,
115.724854765532)) ;
#181249 = CARTESIAN_POINT('Ctrl Pts',(-21.4961500025639,-14.1118280044828,
115.669548634659)) ;
#181250 = CARTESIAN_POINT('Ctrl Pts',(-21.5338004050003,-13.8633524569287,
115.819871913818)) ;
#181251 = CARTESIAN_POINT('Ctrl Pts',(-21.5122496905878,-13.8319077248758,
115.754231913034)) ;
#181252 = CARTESIAN_POINT('Ctrl Pts',(-21.4384458597035,-13.8319076363894,
115.778462992901)) ;
#181253 = CARTESIAN_POINT('Ctrl Pts',(-21.3646420288192,-13.8319075479029,
115.802694072769)) ;
#181254 = CARTESIAN_POINT('Ctrl Pts',(-21.3861927432316,-13.8633522799557,
115.868334073552)) ;
#181255 = CARTESIAN_POINT('Ctrl Pts',(-21.407743457644,-13.8947970120086,
115.933974074336)) ;
#181256 = CARTESIAN_POINT('Ctrl Pts',(-21.4815472885284,-13.894797100495,
115.909742994468)) ;
#181257 = CARTESIAN_POINT('Ctrl Pts',(-21.5553511194127,-13.8947971889815,
115.885511914601)) ;
#181258 = CARTESIAN_POINT('Ctrl Pts',(-21.5338004050003,-13.8633524569287,
115.819871913818)) ;
#181259 = CARTESIAN_POINT('Ctrl Pts',(-21.5489972331909,-13.5856086171591,
115.901434129162)) ;
#181260 = CARTESIAN_POINT('Ctrl Pts',(-21.5256242740484,-13.5735093381459,
115.830243864882)) ;
#181261 = CARTESIAN_POINT('Ctrl Pts',(-21.4518204355535,-13.5735092387167,
115.854474921568)) ;
#181262 = CARTESIAN_POINT('Ctrl Pts',(-21.3780165970586,-13.5735091392875,
115.878705978255)) ;
#181263 = CARTESIAN_POINT('Ctrl Pts',(-21.401389556201,-13.5856084183006,
115.949896242535)) ;
#181264 = CARTESIAN_POINT('Ctrl Pts',(-21.4247625153435,-13.5977076973138,
116.021086506816)) ;
#181265 = CARTESIAN_POINT('Ctrl Pts',(-21.4985663538384,-13.597707796743,
115.996855450129)) ;
#181266 = CARTESIAN_POINT('Ctrl Pts',(-21.5723701923333,-13.5977078961722,
115.972624393442)) ;
#181267 = CARTESIAN_POINT('Ctrl Pts',(-21.5489972331909,-13.5856086171591,
115.901434129162)) ;
#181268 = CARTESIAN_POINT('Ctrl Pts',(-21.540363783719,-13.29429050433,115.910632149051)) ;
#181269 = CARTESIAN_POINT('Ctrl Pts',(-21.5168248652678,-13.3025120940468,
115.838936399422)) ;
#181270 = CARTESIAN_POINT('Ctrl Pts',(-21.4430210182317,-13.3025119902988,
115.863167430093)) ;
#181271 = CARTESIAN_POINT('Ctrl Pts',(-21.3692171711956,-13.3025118865508,
115.887398460765)) ;
#181272 = CARTESIAN_POINT('Ctrl Pts',(-21.3927560896468,-13.294290296834,
115.959094210394)) ;
#181273 = CARTESIAN_POINT('Ctrl Pts',(-21.4162950080979,-13.2860687071171,
116.030789960024)) ;
#181274 = CARTESIAN_POINT('Ctrl Pts',(-21.4900988551341,-13.2860688108651,
116.006558929353)) ;
#181275 = CARTESIAN_POINT('Ctrl Pts',(-21.5639027021702,-13.2860689146131,
115.982327898681)) ;
#181276 = CARTESIAN_POINT('Ctrl Pts',(-21.540363783719,-13.29429050433,115.910632149051)) ;
#181277 = CARTESIAN_POINT('Ctrl Pts',(-21.5075688559681,-13.0122145331766,
115.846182232389)) ;
#181278 = CARTESIAN_POINT('Ctrl Pts',(-21.4855516918688,-13.0401416634717,
115.779121500935)) ;
#181279 = CARTESIAN_POINT('Ctrl Pts',(-21.4117478360689,-13.0401415643198,
115.803352504913)) ;
#181280 = CARTESIAN_POINT('Ctrl Pts',(-21.3379439802689,-13.0401414651678,
115.827583508891)) ;
#181281 = CARTESIAN_POINT('Ctrl Pts',(-21.3599611443683,-13.0122143348728,
115.894644240346)) ;
#181282 = CARTESIAN_POINT('Ctrl Pts',(-21.3819783084676,-12.9842872045777,
115.9617049718)) ;
#181283 = CARTESIAN_POINT('Ctrl Pts',(-21.4557821642676,-12.9842873037296,
115.937473967822)) ;
#181284 = CARTESIAN_POINT('Ctrl Pts',(-21.5295860200675,-12.9842874028816,
115.913242963844)) ;
#181285 = CARTESIAN_POINT('Ctrl Pts',(-21.5075688559681,-13.0122145331766,
115.846182232389)) ;
#181286 = CARTESIAN_POINT('Ctrl Pts',(-21.4520578760768,-12.7583429519339,
115.712662082996)) ;
#181287 = CARTESIAN_POINT('Ctrl Pts',(-21.4331479501616,-12.8040356004971,
115.65506549767)) ;
#181288 = CARTESIAN_POINT('Ctrl Pts',(-21.3593440862728,-12.8040355143443,
115.679296477011)) ;
#181289 = CARTESIAN_POINT('Ctrl Pts',(-21.2855402223839,-12.8040354281915,
115.703527456352)) ;
#181290 = CARTESIAN_POINT('Ctrl Pts',(-21.3044501482991,-12.7583427796283,
115.761124041677)) ;
#181291 = CARTESIAN_POINT('Ctrl Pts',(-21.3233600742142,-12.7126501310651,
115.818720627003)) ;
#181292 = CARTESIAN_POINT('Ctrl Pts',(-21.3971639381031,-12.7126502172179,
115.794489647662)) ;
#181293 = CARTESIAN_POINT('Ctrl Pts',(-21.4709678019919,-12.7126503033707,
115.770258668321)) ;
#181294 = CARTESIAN_POINT('Ctrl Pts',(-21.4520578760768,-12.7583429519339,
115.712662082996)) ;
#181295 = CARTESIAN_POINT('Ctrl Pts',(-21.377127791228,-12.5522896132778,
115.51996437081)) ;
#181296 = CARTESIAN_POINT('Ctrl Pts',(-21.3626860354123,-12.6124359304363,
115.475977110671)) ;
#181297 = CARTESIAN_POINT('Ctrl Pts',(-21.2888821651091,-12.6124358649261,
115.500208070475)) ;
#181298 = CARTESIAN_POINT('Ctrl Pts',(-21.2150782948059,-12.6124357994159,
115.524439030279)) ;
#181299 = CARTESIAN_POINT('Ctrl Pts',(-21.2295200506216,-12.5522894822574,
115.568426290417)) ;
#181300 = CARTESIAN_POINT('Ctrl Pts',(-21.2439618064373,-12.4921431650989,
115.612413550556)) ;
#181301 = CARTESIAN_POINT('Ctrl Pts',(-21.3177656767405,-12.4921432306091,
115.588182590752)) ;
#181302 = CARTESIAN_POINT('Ctrl Pts',(-21.3915695470436,-12.4921432961193,
115.563951630948)) ;
#181303 = CARTESIAN_POINT('Ctrl Pts',(-21.377127791228,-12.5522896132778,
115.51996437081)) ;
#181304 = CARTESIAN_POINT('Ctrl Pts',(-21.2880636112646,-12.4090180636989,
115.283992249369)) ;
#181305 = CARTESIAN_POINT('Ctrl Pts',(-21.2790882199127,-12.4792560944464,
115.256654653408)) ;
#181306 = CARTESIAN_POINT('Ctrl Pts',(-21.2052843453941,-12.4792560544209,
115.280885600373)) ;
#181307 = CARTESIAN_POINT('Ctrl Pts',(-21.1314804708756,-12.4792560143955,
115.305116547337)) ;
#181308 = CARTESIAN_POINT('Ctrl Pts',(-21.1404558622274,-12.409017983648,
115.332454143298)) ;
#181309 = CARTESIAN_POINT('Ctrl Pts',(-21.1494312535792,-12.3387799529005,
115.359791739258)) ;
#181310 = CARTESIAN_POINT('Ctrl Pts',(-21.2232351280978,-12.3387799929259,
115.335560792294)) ;
#181311 = CARTESIAN_POINT('Ctrl Pts',(-21.2970390026164,-12.3387800329514,
115.31132984533)) ;
#181312 = CARTESIAN_POINT('Ctrl Pts',(-21.2880636112646,-12.4090180636989,
115.283992249369)) ;
#181313 = CARTESIAN_POINT('Ctrl Pts',(-21.1893528871873,-12.3371174607651,
115.018865437518)) ;
#181314 = CARTESIAN_POINT('Ctrl Pts',(-21.1865205563104,-12.4124801362831,
115.010238612627)) ;
#181315 = CARTESIAN_POINT('Ctrl Pts',(-21.1127166802678,-12.4124801245382,
115.03446955495)) ;
#181316 = CARTESIAN_POINT('Ctrl Pts',(-21.0389128042251,-12.4124801127933,
115.058700497272)) ;
#181317 = CARTESIAN_POINT('Ctrl Pts',(-21.041745135102,-12.3371174372753,
115.067327322162)) ;
#181318 = CARTESIAN_POINT('Ctrl Pts',(-21.0445774659788,-12.2617547617574,
115.075954147053)) ;
#181319 = CARTESIAN_POINT('Ctrl Pts',(-21.1183813420215,-12.2617547735023,
115.05172320473)) ;
#181320 = CARTESIAN_POINT('Ctrl Pts',(-21.1921852180641,-12.2617547852472,
115.027492262408)) ;
#181321 = CARTESIAN_POINT('Ctrl Pts',(-21.1893528871873,-12.3371174607651,
115.018865437518)) ;
#181322 = CARTESIAN_POINT('Ctrl Pts',(-21.0881345102603,-12.3428658905722,
114.745994676073)) ;
#181323 = CARTESIAN_POINT('Ctrl Pts',(-21.0916317451865,-12.4179397314328,
114.756646687407)) ;
#181324 = CARTESIAN_POINT('Ctrl Pts',(-21.0178278702962,-12.4179397474679,
114.780877633239)) ;
#181325 = CARTESIAN_POINT('Ctrl Pts',(-20.9440239954059,-12.4179397635031,
114.805108579071)) ;
#181326 = CARTESIAN_POINT('Ctrl Pts',(-20.9405267604797,-12.3428659226425,
114.794456567738)) ;
#181327 = CARTESIAN_POINT('Ctrl Pts',(-20.9370295255536,-12.267792081782,
114.783804556404)) ;
#181328 = CARTESIAN_POINT('Ctrl Pts',(-21.0108334004439,-12.2677920657468,
114.759573610572)) ;
#181329 = CARTESIAN_POINT('Ctrl Pts',(-21.0846372753342,-12.2677920497116,
114.73534266474)) ;
#181330 = CARTESIAN_POINT('Ctrl Pts',(-21.0881345102603,-12.3428658905722,
114.745994676073)) ;
#181331 = CARTESIAN_POINT('Ctrl Pts',(-20.9904482281693,-12.4257351119528,
114.483961462618)) ;
#181332 = CARTESIAN_POINT('Ctrl Pts',(-21.000036278797,-12.4951358678153,
114.513165115915)) ;
#181333 = CARTESIAN_POINT('Ctrl Pts',(-20.9262324076312,-12.4951359082695,
114.537396073091)) ;
#181334 = CARTESIAN_POINT('Ctrl Pts',(-20.8524285364653,-12.4951359487237,
114.561627030267)) ;
#181335 = CARTESIAN_POINT('Ctrl Pts',(-20.8428404858377,-12.4257351928613,
114.532423376971)) ;
#181336 = CARTESIAN_POINT('Ctrl Pts',(-20.8332524352101,-12.3563344369988,
114.503219723674)) ;
#181337 = CARTESIAN_POINT('Ctrl Pts',(-20.9070563063759,-12.3563343965446,
114.478988766498)) ;
#181338 = CARTESIAN_POINT('Ctrl Pts',(-20.9808601775417,-12.3563343560904,
114.454757809322)) ;
#181339 = CARTESIAN_POINT('Ctrl Pts',(-20.9904482281693,-12.4257351119528,
114.483961462618)) ;
#181340 = CARTESIAN_POINT('Ctrl Pts',(-20.9030223342738,-12.5790185234623,
114.253042471409)) ;
#181341 = CARTESIAN_POINT('Ctrl Pts',(-20.9179968510548,-12.6378213476739,
114.298652431594)) ;
#181342 = CARTESIAN_POINT('Ctrl Pts',(-20.8441929853562,-12.6378214074388,
114.322883405423)) ;
#181343 = CARTESIAN_POINT('Ctrl Pts',(-20.7703891196576,-12.6378214672038,
114.347114379252)) ;
#181344 = CARTESIAN_POINT('Ctrl Pts',(-20.7554146028766,-12.5790186429921,
114.301504419066)) ;
#181345 = CARTESIAN_POINT('Ctrl Pts',(-20.7404400860955,-12.5202158187805,
114.255894458881)) ;
#181346 = CARTESIAN_POINT('Ctrl Pts',(-20.8142439517941,-12.5202157590156,
114.231663485053)) ;
#181347 = CARTESIAN_POINT('Ctrl Pts',(-20.8880478174927,-12.5202156992507,
114.207432511224)) ;
#181348 = CARTESIAN_POINT('Ctrl Pts',(-20.9030223342738,-12.5790185234623,
114.253042471409)) ;
#181349 = CARTESIAN_POINT('Ctrl Pts',(-20.8305192061514,-12.7940406828703,
114.067860324909)) ;
#181350 = CARTESIAN_POINT('Ctrl Pts',(-20.8498407335462,-12.837920143464,
114.12671057818)) ;
#181351 = CARTESIAN_POINT('Ctrl Pts',(-20.7760368749615,-12.8379202140664,
114.150941573677)) ;
#181352 = CARTESIAN_POINT('Ctrl Pts',(-20.7022330163768,-12.8379202846688,
114.175172569173)) ;
#181353 = CARTESIAN_POINT('Ctrl Pts',(-20.6829114889821,-12.7940408240752,
114.116322315902)) ;
#181354 = CARTESIAN_POINT('Ctrl Pts',(-20.6635899615873,-12.7501613634815,
114.057472062632)) ;
#181355 = CARTESIAN_POINT('Ctrl Pts',(-20.7373938201719,-12.7501612928791,
114.033241067135)) ;
#181356 = CARTESIAN_POINT('Ctrl Pts',(-20.8111976787566,-12.7501612222767,
114.009010071638)) ;
#181357 = CARTESIAN_POINT('Ctrl Pts',(-20.8305192061514,-12.7940406828703,
114.067860324909)) ;
#181358 = CARTESIAN_POINT('Ctrl Pts',(-20.7785061884323,-13.0518842131347,
113.944776920917)) ;
#181359 = CARTESIAN_POINT('Ctrl Pts',(-20.8007570400159,-13.0778272755866,
114.012549423138)) ;
#181360 = CARTESIAN_POINT('Ctrl Pts',(-20.7269531884297,-13.0778273508396,
114.036780439951)) ;
#181361 = CARTESIAN_POINT('Ctrl Pts',(-20.6531493368435,-13.0778274260925,
114.061011456764)) ;
#181362 = CARTESIAN_POINT('Ctrl Pts',(-20.6308984852599,-13.0518843636406,
113.993238954542)) ;
#181363 = CARTESIAN_POINT('Ctrl Pts',(-20.6086476336763,-13.0259413011886,
113.92546645232)) ;
#181364 = CARTESIAN_POINT('Ctrl Pts',(-20.6824514852625,-13.0259412259357,
113.901235435508)) ;
#181365 = CARTESIAN_POINT('Ctrl Pts',(-20.7562553368487,-13.0259411506828,
113.877004418695)) ;
#181366 = CARTESIAN_POINT('Ctrl Pts',(-20.7785061884323,-13.0518842131347,
113.944776920917)) ;
#181367 = CARTESIAN_POINT('Ctrl Pts',(-20.74911735469,-13.3370763555055,113.890776267983)) ;
#181368 = CARTESIAN_POINT('Ctrl Pts',(-20.7727189618692,-13.343146769627,
113.96266295396)) ;
#181369 = CARTESIAN_POINT('Ctrl Pts',(-20.698915117013,-13.3431468412151,
113.986893991271)) ;
#181370 = CARTESIAN_POINT('Ctrl Pts',(-20.6251112721567,-13.3431469128033,
114.011125028582)) ;
#181371 = CARTESIAN_POINT('Ctrl Pts',(-20.6015096649775,-13.3370764986818,
113.939238342606)) ;
#181372 = CARTESIAN_POINT('Ctrl Pts',(-20.5779080577983,-13.3310060845603,
113.867351656629)) ;
#181373 = CARTESIAN_POINT('Ctrl Pts',(-20.6517119026545,-13.3310060129721,
113.843120619318)) ;
#181374 = CARTESIAN_POINT('Ctrl Pts',(-20.7255157475108,-13.3310059413839,
113.818889582007)) ;
#181375 = CARTESIAN_POINT('Ctrl Pts',(-20.74911735469,-13.3370763555055,113.890776267983)) ;
#181376 = CARTESIAN_POINT('Ctrl Pts',(-20.7440079729999,-13.6270297095458,
113.910587476447)) ;
#181377 = CARTESIAN_POINT('Ctrl Pts',(-20.767270009811,-13.6128647269904,
113.981439886012)) ;
#181378 = CARTESIAN_POINT('Ctrl Pts',(-20.6934661705013,-13.6128647900771,
114.005670940217)) ;
#181379 = CARTESIAN_POINT('Ctrl Pts',(-20.6196623311916,-13.6128648531639,
114.029901994422)) ;
#181380 = CARTESIAN_POINT('Ctrl Pts',(-20.5964002943804,-13.6270298357193,
113.959049584857)) ;
#181381 = CARTESIAN_POINT('Ctrl Pts',(-20.5731382575693,-13.6411948182747,
113.888197175291)) ;
#181382 = CARTESIAN_POINT('Ctrl Pts',(-20.646942096879,-13.6411947551879,
113.863966121086)) ;
#181383 = CARTESIAN_POINT('Ctrl Pts',(-20.7207459361887,-13.6411946921012,
113.839735066881)) ;
#181384 = CARTESIAN_POINT('Ctrl Pts',(-20.7440079729999,-13.6270297095458,
113.910587476447)) ;
#181385 = CARTESIAN_POINT('Ctrl Pts',(-20.7628136407268,-13.9038567932623,
114.003478096107)) ;
#181386 = CARTESIAN_POINT('Ctrl Pts',(-20.7840611677085,-13.8703419963818,
114.068194633963)) ;
#181387 = CARTESIAN_POINT('Ctrl Pts',(-20.7102573321534,-13.8703420447739,
114.092425699604)) ;
#181388 = CARTESIAN_POINT('Ctrl Pts',(-20.6364534965982,-13.8703420931661,
114.116656765245)) ;
#181389 = CARTESIAN_POINT('Ctrl Pts',(-20.6152059696165,-13.9038568900467,
114.051940227388)) ;
#181390 = CARTESIAN_POINT('Ctrl Pts',(-20.5939584426348,-13.9373716869272,
113.987223689532)) ;
#181391 = CARTESIAN_POINT('Ctrl Pts',(-20.66776227819,-13.9373716385351,113.962992623891)) ;
#181392 = CARTESIAN_POINT('Ctrl Pts',(-20.7415661137451,-13.9373715901429,
113.93876155825)) ;
#181393 = CARTESIAN_POINT('Ctrl Pts',(-20.7628136407268,-13.9038567932623,
114.003478096107)) ;
#181394 = CARTESIAN_POINT('Ctrl Pts',(-20.8034569028155,-14.1447030861545,
114.162759758855)) ;
#181395 = CARTESIAN_POINT('Ctrl Pts',(-20.821164521826,-14.0943210410225,
114.216694308367)) ;
#181396 = CARTESIAN_POINT('Ctrl Pts',(-20.7473606880735,-14.0943210744769,
114.240925379498)) ;
#181397 = CARTESIAN_POINT('Ctrl Pts',(-20.673556854321,-14.0943211079313,
114.26515645063)) ;
#181398 = CARTESIAN_POINT('Ctrl Pts',(-20.6558492353105,-14.1447031530633,
114.211221901118)) ;
#181399 = CARTESIAN_POINT('Ctrl Pts',(-20.6381416163,-14.1950851981953,114.157287351607)) ;
#181400 = CARTESIAN_POINT('Ctrl Pts',(-20.7119454500525,-14.1950851647409,
114.133056280476)) ;
#181401 = CARTESIAN_POINT('Ctrl Pts',(-20.785749283805,-14.1950851312865,
114.108825209344)) ;
#181402 = CARTESIAN_POINT('Ctrl Pts',(-20.8034569028155,-14.1447030861545,
114.162759758855)) ;
#181403 = CARTESIAN_POINT('Ctrl Pts',(-20.8618372427062,-14.332817774621,
114.375897727997)) ;
#181404 = CARTESIAN_POINT('Ctrl Pts',(-20.8747644917741,-14.2692250612684,
114.415272042114)) ;
#181405 = CARTESIAN_POINT('Ctrl Pts',(-20.8009606585353,-14.2692250813647,
114.43950311481)) ;
#181406 = CARTESIAN_POINT('Ctrl Pts',(-20.7271568252965,-14.269225101461,
114.463734187506)) ;
#181407 = CARTESIAN_POINT('Ctrl Pts',(-20.7142295762286,-14.3328178148136,
114.424359873389)) ;
#181408 = CARTESIAN_POINT('Ctrl Pts',(-20.7013023271606,-14.3964105281663,
114.384985559272)) ;
#181409 = CARTESIAN_POINT('Ctrl Pts',(-20.7751061603994,-14.3964105080699,
114.360754486576)) ;
#181410 = CARTESIAN_POINT('Ctrl Pts',(-20.8489099936382,-14.3964104879736,
114.33652341388)) ;
#181411 = CARTESIAN_POINT('Ctrl Pts',(-20.8618372427062,-14.332817774621,
114.375897727997)) ;
#181412 = CARTESIAN_POINT('Ctrl Pts',(-20.9337388829321,-14.45646682902,114.630435787986)) ;
#181413 = CARTESIAN_POINT('Ctrl Pts',(-20.9409299779606,-14.3841439170352,
114.652338702601)) ;
#181414 = CARTESIAN_POINT('Ctrl Pts',(-20.8671261432927,-14.3841439249686,
114.676569770944)) ;
#181415 = CARTESIAN_POINT('Ctrl Pts',(-20.7933223086247,-14.3841439329019,
114.700800839287)) ;
#181416 = CARTESIAN_POINT('Ctrl Pts',(-20.7861312135962,-14.4564668448866,
114.678897924672)) ;
#181417 = CARTESIAN_POINT('Ctrl Pts',(-20.7789401185677,-14.5287897568713,
114.656995010056)) ;
#181418 = CARTESIAN_POINT('Ctrl Pts',(-20.8527439532357,-14.528789748938,
114.632763941713)) ;
#181419 = CARTESIAN_POINT('Ctrl Pts',(-20.9265477879036,-14.5287897410047,
114.60853287337)) ;
#181420 = CARTESIAN_POINT('Ctrl Pts',(-20.9337388829321,-14.45646682902,114.630435787986)) ;
#181421 = CARTESIAN_POINT('Ctrl Pts',(-21.0127215247643,-14.5053560860543,
114.906444434635)) ;
#181422 = CARTESIAN_POINT('Ctrl Pts',(-21.0136752367889,-14.4295100560536,
114.90934928717)) ;
#181423 = CARTESIAN_POINT('Ctrl Pts',(-20.9398714000126,-14.4295100560703,
114.933580349091)) ;
#181424 = CARTESIAN_POINT('Ctrl Pts',(-20.8660675632364,-14.429510056087,
114.957811411013)) ;
#181425 = CARTESIAN_POINT('Ctrl Pts',(-20.8651138512118,-14.5053560860877,
114.954906558478)) ;
#181426 = CARTESIAN_POINT('Ctrl Pts',(-20.8641601391871,-14.5812021160883,
114.952001705943)) ;
#181427 = CARTESIAN_POINT('Ctrl Pts',(-20.9379639759634,-14.5812021160717,
114.927770644021)) ;
#181428 = CARTESIAN_POINT('Ctrl Pts',(-21.0117678127397,-14.581202116055,
114.903539582099)) ;
#181429 = CARTESIAN_POINT('Ctrl Pts',(-21.0127215247643,-14.5053560860543,
114.906444434635)) ;
#181430 = CARTESIAN_POINT('Ctrl Pts',(-21.0928080257603,-14.4762759602464,
115.185935827809)) ;
#181431 = CARTESIAN_POINT('Ctrl Pts',(-21.0874352126605,-14.4023454887856,
115.169571105754)) ;
#181432 = CARTESIAN_POINT('Ctrl Pts',(-21.0136313731792,-14.4023454850915,
115.193802159437)) ;
#181433 = CARTESIAN_POINT('Ctrl Pts',(-20.9398275336979,-14.4023454813974,
115.218033213119)) ;
#181434 = CARTESIAN_POINT('Ctrl Pts',(-20.9452003467976,-14.4762759528582,
115.234397935174)) ;
#181435 = CARTESIAN_POINT('Ctrl Pts',(-20.9505731598973,-14.5502064243191,
115.250762657229)) ;
#181436 = CARTESIAN_POINT('Ctrl Pts',(-21.0243769993787,-14.5502064280132,
115.226531603546)) ;
#181437 = CARTESIAN_POINT('Ctrl Pts',(-21.09818083886,-14.5502064317073,115.202300549864)) ;
#181438 = CARTESIAN_POINT('Ctrl Pts',(-21.0928080257603,-14.4762759602464,
115.185935827809)) ;
#181439 = CARTESIAN_POINT('Ctrl Pts',(-21.166945453464,-14.3712943997113,
115.44718234613)) ;
#181440 = CARTESIAN_POINT('Ctrl Pts',(-21.1556545074881,-14.3045830394382,
115.412791946338)) ;
#181441 = CARTESIAN_POINT('Ctrl Pts',(-21.0818506659481,-14.3045830356426,
115.43702299375)) ;
#181442 = CARTESIAN_POINT('Ctrl Pts',(-21.008046824408,-14.3045830318471,
115.461254041162)) ;
#181443 = CARTESIAN_POINT('Ctrl Pts',(-21.0193377703839,-14.3712943921201,
115.495644440954)) ;
#181444 = CARTESIAN_POINT('Ctrl Pts',(-21.0306287163597,-14.4380057523932,
115.530034840746)) ;
#181445 = CARTESIAN_POINT('Ctrl Pts',(-21.1044325578998,-14.4380057561888,
115.505803793334)) ;
#181446 = CARTESIAN_POINT('Ctrl Pts',(-21.1782363994398,-14.4380057599843,
115.481572745922)) ;
#181447 = CARTESIAN_POINT('Ctrl Pts',(-21.166945453464,-14.3712943997113,
115.44718234613)) ;
#181448 = CARTESIAN_POINT('Ctrl Pts',(-21.22925533612,-14.1990455522355,115.672287786187)) ;
#181449 = CARTESIAN_POINT('Ctrl Pts',(-21.2128657588445,-14.1442616573657,
115.622367778204)) ;
#181450 = CARTESIAN_POINT('Ctrl Pts',(-21.1390619159356,-14.1442616552479,
115.646598821446)) ;
#181451 = CARTESIAN_POINT('Ctrl Pts',(-21.0652580730266,-14.1442616531301,
115.670829864688)) ;
#181452 = CARTESIAN_POINT('Ctrl Pts',(-21.0816476503021,-14.1990455479999,
115.720749872672)) ;
#181453 = CARTESIAN_POINT('Ctrl Pts',(-21.0980372275776,-14.2538294428697,
115.770669880655)) ;
#181454 = CARTESIAN_POINT('Ctrl Pts',(-21.1718410704865,-14.2538294449875,
115.746438837413)) ;
#181455 = CARTESIAN_POINT('Ctrl Pts',(-21.2456449133955,-14.2538294471053,
115.722207794171)) ;
#181456 = CARTESIAN_POINT('Ctrl Pts',(-21.22925533612,-14.1990455522355,115.672287786187)) ;
#181457 = CARTESIAN_POINT('Ctrl Pts',(-21.275036309889,-13.969268231171,115.847326008971)) ;
#181458 = CARTESIAN_POINT('Ctrl Pts',(-21.2546885946839,-13.9304471194496,
115.785350151579)) ;
#181459 = CARTESIAN_POINT('Ctrl Pts',(-21.1808847509395,-13.9304471207081,
115.809581192277)) ;
#181460 = CARTESIAN_POINT('Ctrl Pts',(-21.107080907195,-13.9304471219666,
115.833812232975)) ;
#181461 = CARTESIAN_POINT('Ctrl Pts',(-21.1274286224002,-13.9692682336881,
115.895788090367)) ;
#181462 = CARTESIAN_POINT('Ctrl Pts',(-21.1477763376053,-14.0080893454095,
115.957763947758)) ;
#181463 = CARTESIAN_POINT('Ctrl Pts',(-21.2215801813498,-14.008089344151,
115.933532907061)) ;
#181464 = CARTESIAN_POINT('Ctrl Pts',(-21.2953840250942,-14.0080893428925,
115.909301866363)) ;
#181465 = CARTESIAN_POINT('Ctrl Pts',(-21.275036309889,-13.969268231171,115.847326008971)) ;
#181466 = CARTESIAN_POINT('Ctrl Pts',(-21.2996282826531,-13.7012052922517,
115.957629225369)) ;
#181467 = CARTESIAN_POINT('Ctrl Pts',(-21.2768004959632,-13.6810448607135,
115.888099470425)) ;
#181468 = CARTESIAN_POINT('Ctrl Pts',(-21.2029966522746,-13.6810448639026,
115.912330511293)) ;
#181469 = CARTESIAN_POINT('Ctrl Pts',(-21.1291928085861,-13.6810448670916,
115.936561552161)) ;
#181470 = CARTESIAN_POINT('Ctrl Pts',(-21.152020595276,-13.7012052986298,
116.006091307105)) ;
#181471 = CARTESIAN_POINT('Ctrl Pts',(-21.174848381966,-13.7213657301679,
116.075621062049)) ;
#181472 = CARTESIAN_POINT('Ctrl Pts',(-21.2486522256545,-13.7213657269789,
116.051390021181)) ;
#181473 = CARTESIAN_POINT('Ctrl Pts',(-21.3224560693431,-13.7213657237898,
116.027158980313)) ;
#181474 = CARTESIAN_POINT('Ctrl Pts',(-21.2996282826531,-13.7012052922517,
115.957629225369)) ;
#181475 = CARTESIAN_POINT('Ctrl Pts',(-21.300776790549,-13.4115854195081,
115.996699140416)) ;
#181476 = CARTESIAN_POINT('Ctrl Pts',(-21.2770987495347,-13.4116194662379,
115.924579647977)) ;
#181477 = CARTESIAN_POINT('Ctrl Pts',(-21.20329490617,-13.4116194689939,115.948810689832)) ;
#181478 = CARTESIAN_POINT('Ctrl Pts',(-21.1294910628053,-13.41161947175,115.973041731686)) ;
#181479 = CARTESIAN_POINT('Ctrl Pts',(-21.1531691038196,-13.4115854250202,
116.045161224125)) ;
#181480 = CARTESIAN_POINT('Ctrl Pts',(-21.176847144834,-13.4115513782904,
116.117280716563)) ;
#181481 = CARTESIAN_POINT('Ctrl Pts',(-21.2506509881987,-13.4115513755344,
116.093049674709)) ;
#181482 = CARTESIAN_POINT('Ctrl Pts',(-21.3244548315633,-13.4115513727784,
116.068818632855)) ;
#181483 = CARTESIAN_POINT('Ctrl Pts',(-21.300776790549,-13.4115854195081,
115.996699140416)) ;
#181484 = CARTESIAN_POINT('Ctrl Pts',(-21.2776657782434,-13.1240520278943,
115.961667884177)) ;
#181485 = CARTESIAN_POINT('Ctrl Pts',(-21.2548350128594,-13.1441635924048,
115.892129056556)) ;
#181486 = CARTESIAN_POINT('Ctrl Pts',(-21.1810311695779,-13.144163592711,
115.916360098664)) ;
#181487 = CARTESIAN_POINT('Ctrl Pts',(-21.1072273262965,-13.1441635930171,
115.940591140771)) ;
#181488 = CARTESIAN_POINT('Ctrl Pts',(-21.1300580916804,-13.1240520285066,
116.010129968393)) ;
#181489 = CARTESIAN_POINT('Ctrl Pts',(-21.1528888570643,-13.103940463996,
116.079668796014)) ;
#181490 = CARTESIAN_POINT('Ctrl Pts',(-21.2266927003458,-13.1039404636899,
116.055437753906)) ;
#181491 = CARTESIAN_POINT('Ctrl Pts',(-21.3004965436273,-13.1039404633837,
116.031206711798)) ;
#181492 = CARTESIAN_POINT('Ctrl Pts',(-21.2776657782434,-13.1240520278943,
115.961667884177)) ;
#181493 = CARTESIAN_POINT('Ctrl Pts',(-21.2310997495999,-12.8565945311091,
115.85532524094)) ;
#181494 = CARTESIAN_POINT('Ctrl Pts',(-21.2107526317274,-12.895411134357,
115.79335120282)) ;
#181495 = CARTESIAN_POINT('Ctrl Pts',(-21.1369487878002,-12.8954111308149,
115.817582242961)) ;
#181496 = CARTESIAN_POINT('Ctrl Pts',(-21.0631449438729,-12.8954111272728,
115.841813283102)) ;
#181497 = CARTESIAN_POINT('Ctrl Pts',(-21.0834920617454,-12.8565945240249,
115.903787321221)) ;
#181498 = CARTESIAN_POINT('Ctrl Pts',(-21.1038391796179,-12.817777920777,
115.965761359341)) ;
#181499 = CARTESIAN_POINT('Ctrl Pts',(-21.1776430235452,-12.8177779243191,
115.9415303192)) ;
#181500 = CARTESIAN_POINT('Ctrl Pts',(-21.2514468674724,-12.8177779278612,
115.917299279059)) ;
#181501 = CARTESIAN_POINT('Ctrl Pts',(-21.2310997495999,-12.8565945311091,
115.85532524094)) ;
#181502 = CARTESIAN_POINT('Ctrl Pts',(-21.1639038965067,-12.6299321000607,
115.686042104693)) ;
#181503 = CARTESIAN_POINT('Ctrl Pts',(-21.1474868349835,-12.6846316848106,
115.636038384002)) ;
#181504 = CARTESIAN_POINT('Ctrl Pts',(-21.0736829896652,-12.6846316781894,
115.660269419906)) ;
#181505 = CARTESIAN_POINT('Ctrl Pts',(-20.9998791443469,-12.6846316715683,
115.68450045581)) ;
#181506 = CARTESIAN_POINT('Ctrl Pts',(-21.0162962058702,-12.6299320868185,
115.7345041765)) ;
#181507 = CARTESIAN_POINT('Ctrl Pts',(-21.0327132673934,-12.5752325020687,
115.784507897191)) ;
#181508 = CARTESIAN_POINT('Ctrl Pts',(-21.1065171127117,-12.5752325086898,
115.760276861287)) ;
#181509 = CARTESIAN_POINT('Ctrl Pts',(-21.18032095803,-12.5752325153109,115.736045825383)) ;
#181510 = CARTESIAN_POINT('Ctrl Pts',(-21.1639038965067,-12.6299321000607,
115.686042104693)) ;
#181511 = CARTESIAN_POINT('Ctrl Pts',(-21.0795308737286,-12.458754218581,
115.464633703423)) ;
#181512 = CARTESIAN_POINT('Ctrl Pts',(-21.0682449006004,-12.5254858902144,
115.430258449939)) ;
#181513 = CARTESIAN_POINT('Ctrl Pts',(-20.9944410527263,-12.5254858817945,
115.454489478058)) ;
#181514 = CARTESIAN_POINT('Ctrl Pts',(-20.9206372048521,-12.5254858733746,
115.478720506177)) ;
#181515 = CARTESIAN_POINT('Ctrl Pts',(-20.9319231779803,-12.4587542017412,
115.513095759661)) ;
#181516 = CARTESIAN_POINT('Ctrl Pts',(-20.9432091511085,-12.3920225301078,
115.547471013146)) ;
#181517 = CARTESIAN_POINT('Ctrl Pts',(-21.0170129989826,-12.3920225385277,
115.523239985027)) ;
#181518 = CARTESIAN_POINT('Ctrl Pts',(-21.0908168468568,-12.3920225469476,
115.499008956907)) ;
#181519 = CARTESIAN_POINT('Ctrl Pts',(-21.0795308737286,-12.458754218581,
115.464633703423)) ;
#181520 = CARTESIAN_POINT('Ctrl Pts',(-20.9840008114821,-12.3569969390507,
115.209096703892)) ;
#181521 = CARTESIAN_POINT('Ctrl Pts',(-20.978635400475,-12.4309301429408,
115.192754527206)) ;
#181522 = CARTESIAN_POINT('Ctrl Pts',(-20.9048315498076,-12.4309301369064,
115.216985546818)) ;
#181523 = CARTESIAN_POINT('Ctrl Pts',(-20.8310276991402,-12.430930130872,
115.241216566429)) ;
#181524 = CARTESIAN_POINT('Ctrl Pts',(-20.8363931101473,-12.356996926982,
115.257558743115)) ;
#181525 = CARTESIAN_POINT('Ctrl Pts',(-20.8417585211544,-12.283063723092,
115.273900919801)) ;
#181526 = CARTESIAN_POINT('Ctrl Pts',(-20.9155623718218,-12.2830637291264,
115.249669900189)) ;
#181527 = CARTESIAN_POINT('Ctrl Pts',(-20.9893662224891,-12.2830637351607,
115.225438880578)) ;
#181528 = CARTESIAN_POINT('Ctrl Pts',(-20.9840008114821,-12.3569969390507,
115.209096703892)) ;
#181529 = CARTESIAN_POINT('Ctrl Pts',(-20.8827940549326,-12.3311725454961,
114.936383442419)) ;
#181530 = CARTESIAN_POINT('Ctrl Pts',(-20.8837517075036,-12.4070160661621,
114.939300296995)) ;
#181531 = CARTESIAN_POINT('Ctrl Pts',(-20.8099478537991,-12.4070160669481,
114.963531307356)) ;
#181532 = CARTESIAN_POINT('Ctrl Pts',(-20.7361440000946,-12.4070160677341,
114.987762317717)) ;
#181533 = CARTESIAN_POINT('Ctrl Pts',(-20.7351863475235,-12.3311725470681,
114.984845463141)) ;
#181534 = CARTESIAN_POINT('Ctrl Pts',(-20.7342286949525,-12.2553290264021,
114.981928608564)) ;
#181535 = CARTESIAN_POINT('Ctrl Pts',(-20.808032548657,-12.2553290256161,
114.957697598203)) ;
#181536 = CARTESIAN_POINT('Ctrl Pts',(-20.8818364023615,-12.2553290248301,
114.933466587842)) ;
#181537 = CARTESIAN_POINT('Ctrl Pts',(-20.8827940549326,-12.3311725454961,
114.936383442419)) ;
#181538 = CARTESIAN_POINT('Ctrl Pts',(-20.7831194155453,-12.3830921654557,
114.668177530527)) ;
#181539 = CARTESIAN_POINT('Ctrl Pts',(-20.7903054822259,-12.4554200435771,
114.690065129378)) ;
#181540 = CARTESIAN_POINT('Ctrl Pts',(-20.716501626603,-12.4554200554495,
114.714296133896)) ;
#181541 = CARTESIAN_POINT('Ctrl Pts',(-20.6426977709801,-12.4554200673219,
114.738527138414)) ;
#181542 = CARTESIAN_POINT('Ctrl Pts',(-20.6355117042995,-12.3830921892004,
114.716639539563)) ;
#181543 = CARTESIAN_POINT('Ctrl Pts',(-20.6283256376189,-12.310764311079,
114.694751940711)) ;
#181544 = CARTESIAN_POINT('Ctrl Pts',(-20.7021294932418,-12.3107642992066,
114.670520936193)) ;
#181545 = CARTESIAN_POINT('Ctrl Pts',(-20.7759333488647,-12.3107642873342,
114.646289931676)) ;
#181546 = CARTESIAN_POINT('Ctrl Pts',(-20.7831194155453,-12.3830921654557,
114.668177530527)) ;
#181547 = CARTESIAN_POINT('Ctrl Pts',(-20.6905057252182,-12.5097082549453,
114.421659452315)) ;
#181548 = CARTESIAN_POINT('Ctrl Pts',(-20.7034324595095,-12.5733006688363,
114.461032198267)) ;
#181549 = CARTESIAN_POINT('Ctrl Pts',(-20.6296286028042,-12.5733006960963,
114.485263199488)) ;
#181550 = CARTESIAN_POINT('Ctrl Pts',(-20.555824746099,-12.5733007233563,
114.509494200709)) ;
#181551 = CARTESIAN_POINT('Ctrl Pts',(-20.5428980118077,-12.5097083094653,
114.470121454757)) ;
#181552 = CARTESIAN_POINT('Ctrl Pts',(-20.5299712775163,-12.4461158955744,
114.430748708805)) ;
#181553 = CARTESIAN_POINT('Ctrl Pts',(-20.6037751342216,-12.4461158683144,
114.406517707584)) ;
#181554 = CARTESIAN_POINT('Ctrl Pts',(-20.6775789909268,-12.4461158410544,
114.382286706363)) ;
#181555 = CARTESIAN_POINT('Ctrl Pts',(-20.6905057252182,-12.5097082549453,
114.421659452315)) ;
#181556 = CARTESIAN_POINT('Ctrl Pts',(-20.611889484645,-12.6999655173835,
114.217488910924)) ;
#181557 = CARTESIAN_POINT('Ctrl Pts',(-20.6295936140436,-12.7503658770991,
114.271412831411)) ;
#181558 = CARTESIAN_POINT('Ctrl Pts',(-20.5557897586328,-12.7503659198469,
114.295643836575)) ;
#181559 = CARTESIAN_POINT('Ctrl Pts',(-20.481985903222,-12.7503659625947,
114.319874841739)) ;
#181560 = CARTESIAN_POINT('Ctrl Pts',(-20.4642817738234,-12.699965602879,
114.265950921252)) ;
#181561 = CARTESIAN_POINT('Ctrl Pts',(-20.4465776444248,-12.6495652431633,
114.212027000766)) ;
#181562 = CARTESIAN_POINT('Ctrl Pts',(-20.5203814998356,-12.6495652004156,
114.187795995602)) ;
#181563 = CARTESIAN_POINT('Ctrl Pts',(-20.5941853552464,-12.6495651576678,
114.163564990438)) ;
#181564 = CARTESIAN_POINT('Ctrl Pts',(-20.611889484645,-12.6999655173835,
114.217488910924)) ;
#181565 = CARTESIAN_POINT('Ctrl Pts',(-20.5509672408573,-12.9431519741363,
114.067493771152)) ;
#181566 = CARTESIAN_POINT('Ctrl Pts',(-20.5722146237278,-12.9766466266446,
114.132209869832)) ;
#181567 = CARTESIAN_POINT('Ctrl Pts',(-20.4984107710343,-12.9766466864281,
114.156440883272)) ;
#181568 = CARTESIAN_POINT('Ctrl Pts',(-20.4246069183407,-12.9766467462115,
114.180671896712)) ;
#181569 = CARTESIAN_POINT('Ctrl Pts',(-20.4033595354702,-12.9431520937032,
114.115955798032)) ;
#181570 = CARTESIAN_POINT('Ctrl Pts',(-20.3821121525996,-12.9096574411949,
114.051239699352)) ;
#181571 = CARTESIAN_POINT('Ctrl Pts',(-20.4559160052932,-12.9096573814114,
114.027008685912)) ;
#181572 = CARTESIAN_POINT('Ctrl Pts',(-20.5297198579867,-12.9096573216279,
114.002777672472)) ;
#181573 = CARTESIAN_POINT('Ctrl Pts',(-20.5509672408573,-12.9431519741363,
114.067493771152)) ;
#181574 = CARTESIAN_POINT('Ctrl Pts',(-20.5121852559406,-13.2187420743147,
113.984700488241)) ;
#181575 = CARTESIAN_POINT('Ctrl Pts',(-20.535439895788,-13.233044020348,114.055530367671)) ;
#181576 = CARTESIAN_POINT('Ctrl Pts',(-20.4616360479609,-13.2330440926295,
114.079761395933)) ;
#181577 = CARTESIAN_POINT('Ctrl Pts',(-20.3878322001338,-13.2330441649111,
114.103992424196)) ;
#181578 = CARTESIAN_POINT('Ctrl Pts',(-20.3645775602864,-13.2187422188778,
114.033162544766)) ;
#181579 = CARTESIAN_POINT('Ctrl Pts',(-20.341322920439,-13.2044402728445,
113.962332665335)) ;
#181580 = CARTESIAN_POINT('Ctrl Pts',(-20.4151267682661,-13.204440200563,
113.938101637073)) ;
#181581 = CARTESIAN_POINT('Ctrl Pts',(-20.4889306160931,-13.2044401282814,
113.913870608811)) ;
#181582 = CARTESIAN_POINT('Ctrl Pts',(-20.5121852559406,-13.2187420743147,
113.984700488241)) ;
#181583 = CARTESIAN_POINT('Ctrl Pts',(-20.4971344280026,-13.5111774969548,
113.974526122815)) ;
#181584 = CARTESIAN_POINT('Ctrl Pts',(-20.5207357628537,-13.505083397222,
114.046411979112)) ;
#181585 = CARTESIAN_POINT('Ctrl Pts',(-20.4469319214645,-13.5050834796266,
114.070643026983)) ;
#181586 = CARTESIAN_POINT('Ctrl Pts',(-20.3731280800753,-13.5050835620312,
114.094874074854)) ;
#181587 = CARTESIAN_POINT('Ctrl Pts',(-20.3495267452242,-13.511177661764,
114.022988218557)) ;
#181588 = CARTESIAN_POINT('Ctrl Pts',(-20.3259254103731,-13.5172717614969,
113.95110236226)) ;
#181589 = CARTESIAN_POINT('Ctrl Pts',(-20.3997292517623,-13.5172716790923,
113.926871314389)) ;
#181590 = CARTESIAN_POINT('Ctrl Pts',(-20.4735330931515,-13.5172715966877,
113.902640266518)) ;
#181591 = CARTESIAN_POINT('Ctrl Pts',(-20.4971344280026,-13.5111774969548,
113.974526122815)) ;
#181592 = CARTESIAN_POINT('Ctrl Pts',(-20.5063387268511,-13.7940494918521,
114.037849430853)) ;
#181593 = CARTESIAN_POINT('Ctrl Pts',(-20.5286013967457,-13.7681973144643,
114.105657929582)) ;
#181594 = CARTESIAN_POINT('Ctrl Pts',(-20.4547975626805,-13.7681973972875,
114.129888999761)) ;
#181595 = CARTESIAN_POINT('Ctrl Pts',(-20.3809937286154,-13.7681974801107,
114.15412006994)) ;
#181596 = CARTESIAN_POINT('Ctrl Pts',(-20.3587310587208,-13.7940496574985,
114.086311571211)) ;
#181597 = CARTESIAN_POINT('Ctrl Pts',(-20.3364683888263,-13.8199018348862,
114.018503072482)) ;
#181598 = CARTESIAN_POINT('Ctrl Pts',(-20.4102722228914,-13.819901752063,
113.994272002303)) ;
#181599 = CARTESIAN_POINT('Ctrl Pts',(-20.4840760569565,-13.8199016692398,
113.970040932124)) ;
#181600 = CARTESIAN_POINT('Ctrl Pts',(-20.5063387268511,-13.7940494918521,
114.037849430853)) ;
#181601 = CARTESIAN_POINT('Ctrl Pts',(-20.5386101711866,-14.0529110285333,
114.171842551174)) ;
#181602 = CARTESIAN_POINT('Ctrl Pts',(-20.5579137638,-14.0089483158053,114.230638177808)) ;
#181603 = CARTESIAN_POINT('Ctrl Pts',(-20.4841099376321,-14.0089483935527,
114.25486927204)) ;
#181604 = CARTESIAN_POINT('Ctrl Pts',(-20.4103061114642,-14.0089484713001,
114.279100366273)) ;
#181605 = CARTESIAN_POINT('Ctrl Pts',(-20.3910025188508,-14.0529111840282,
114.22030473964)) ;
#181606 = CARTESIAN_POINT('Ctrl Pts',(-20.3716989262374,-14.0968738967562,
114.161509113006)) ;
#181607 = CARTESIAN_POINT('Ctrl Pts',(-20.4455027524053,-14.0968738190088,
114.137278018774)) ;
#181608 = CARTESIAN_POINT('Ctrl Pts',(-20.5193065785732,-14.0968737412614,
114.113046924541)) ;
#181609 = CARTESIAN_POINT('Ctrl Pts',(-20.5386101711866,-14.0529110285333,
114.171842551174)) ;
#181610 = CARTESIAN_POINT('Ctrl Pts',(-20.5902344604345,-14.2634870650102,
114.364365229605)) ;
#181611 = CARTESIAN_POINT('Ctrl Pts',(-20.6052317953266,-14.2047586746315,
114.410044689958)) ;
#181612 = CARTESIAN_POINT('Ctrl Pts',(-20.531427975912,-14.2047587372463,
114.43427580476)) ;
#181613 = CARTESIAN_POINT('Ctrl Pts',(-20.4576241564973,-14.204758799861,
114.458506919562)) ;
#181614 = CARTESIAN_POINT('Ctrl Pts',(-20.4426268216052,-14.2634871902397,
114.412827459209)) ;
#181615 = CARTESIAN_POINT('Ctrl Pts',(-20.4276294867131,-14.3222155806184,
114.367147998855)) ;
#181616 = CARTESIAN_POINT('Ctrl Pts',(-20.5014333061278,-14.3222155180036,
114.342916884053)) ;
#181617 = CARTESIAN_POINT('Ctrl Pts',(-20.5752371255424,-14.3222154553889,
114.318685769251)) ;
#181618 = CARTESIAN_POINT('Ctrl Pts',(-20.5902344604345,-14.2634870650102,
114.364365229605)) ;
#181619 = CARTESIAN_POINT('Ctrl Pts',(-20.6572920468694,-14.4148461022599,
114.60407461122)) ;
#181620 = CARTESIAN_POINT('Ctrl Pts',(-20.6668958738474,-14.3454644446965,
114.633326316629)) ;
#181621 = CARTESIAN_POINT('Ctrl Pts',(-20.5930920598847,-14.3454644862781,
114.657557448037)) ;
#181622 = CARTESIAN_POINT('Ctrl Pts',(-20.519288245922,-14.3454645278597,
114.681788579445)) ;
#181623 = CARTESIAN_POINT('Ctrl Pts',(-20.509684418944,-14.414846185423,114.652536874035)) ;
#181624 = CARTESIAN_POINT('Ctrl Pts',(-20.500080591966,-14.4842278429864,
114.623285168626)) ;
#181625 = CARTESIAN_POINT('Ctrl Pts',(-20.5738844059287,-14.4842278014048,
114.599054037218)) ;
#181626 = CARTESIAN_POINT('Ctrl Pts',(-20.6476882198914,-14.4842277598232,
114.57482290581)) ;
#181627 = CARTESIAN_POINT('Ctrl Pts',(-20.6572920468694,-14.4148461022599,
114.60407461122)) ;
#181628 = CARTESIAN_POINT('Ctrl Pts',(-20.7340710302273,-14.494780073978,
114.873368689738)) ;
#181629 = CARTESIAN_POINT('Ctrl Pts',(-20.7375952932734,-14.4197159016166,
114.88410302429)) ;
#181630 = CARTESIAN_POINT('Ctrl Pts',(-20.6637914825865,-14.4197159169921,
114.908334165676)) ;
#181631 = CARTESIAN_POINT('Ctrl Pts',(-20.5899876718997,-14.4197159323676,
114.932565307061)) ;
#181632 = CARTESIAN_POINT('Ctrl Pts',(-20.5864634088536,-14.4947801047291,
114.921830972509)) ;
#181633 = CARTESIAN_POINT('Ctrl Pts',(-20.5829391458075,-14.5698442770905,
114.911096637957)) ;
#181634 = CARTESIAN_POINT('Ctrl Pts',(-20.6567429564944,-14.5698442617149,
114.886865496572)) ;
#181635 = CARTESIAN_POINT('Ctrl Pts',(-20.7305467671812,-14.5698442463394,
114.862634355187)) ;
#181636 = CARTESIAN_POINT('Ctrl Pts',(-20.7340710302273,-14.494780073978,
114.873368689738)) ;
#181637 = CARTESIAN_POINT('Ctrl Pts',(-20.814667921946,-14.4974507314962,
115.154444310866)) ;
#181638 = CARTESIAN_POINT('Ctrl Pts',(-20.8118340578012,-14.4220890720825,
115.145812815837)) ;
#181639 = CARTESIAN_POINT('Ctrl Pts',(-20.7380302478058,-14.4220890586317,
115.170043959328)) ;
#181640 = CARTESIAN_POINT('Ctrl Pts',(-20.6642264378103,-14.4220890451809,
115.194275102819)) ;
#181641 = CARTESIAN_POINT('Ctrl Pts',(-20.6670603019551,-14.4974507045946,
115.202906597848)) ;
#181642 = CARTESIAN_POINT('Ctrl Pts',(-20.6698941660999,-14.5728123640084,
115.211538092878)) ;
#181643 = CARTESIAN_POINT('Ctrl Pts',(-20.7436979760954,-14.5728123774592,
115.187306949387)) ;
#181644 = CARTESIAN_POINT('Ctrl Pts',(-20.8175017860908,-14.57281239091,115.163075805895)) ;
#181645 = CARTESIAN_POINT('Ctrl Pts',(-20.814667921946,-14.4974507314962,
115.154444310866)) ;
#181646 = CARTESIAN_POINT('Ctrl Pts',(-20.8916746371351,-14.4229495346006,
115.424337435555)) ;
#181647 = CARTESIAN_POINT('Ctrl Pts',(-20.8827289243665,-14.3526782474262,
115.397090235752)) ;
#181648 = CARTESIAN_POINT('Ctrl Pts',(-20.8089251121826,-14.3526782058987,
115.421321372578)) ;
#181649 = CARTESIAN_POINT('Ctrl Pts',(-20.7351212999988,-14.3526781643712,
115.445552509404)) ;
#181650 = CARTESIAN_POINT('Ctrl Pts',(-20.7440670127673,-14.4229494515456,
115.472799709206)) ;
#181651 = CARTESIAN_POINT('Ctrl Pts',(-20.7530127255359,-14.49322073872,115.500046909008)) ;
#181652 = CARTESIAN_POINT('Ctrl Pts',(-20.8268165377198,-14.4932207802475,
115.475815772183)) ;
#181653 = CARTESIAN_POINT('Ctrl Pts',(-20.9006203499037,-14.493220821775,
115.451584635357)) ;
#181654 = CARTESIAN_POINT('Ctrl Pts',(-20.8916746371351,-14.4229495346006,
115.424337435555)) ;
#181655 = CARTESIAN_POINT('Ctrl Pts',(-20.9596595247132,-14.2768020033666,
115.6668461103)) ;
#181656 = CARTESIAN_POINT('Ctrl Pts',(-20.9452208674078,-14.2166300695752,
115.622868287728)) ;
#181657 = CARTESIAN_POINT('Ctrl Pts',(-20.8714170505769,-14.2166300030693,
115.647099410399)) ;
#181658 = CARTESIAN_POINT('Ctrl Pts',(-20.7976132337459,-14.2166299365633,
115.671330533071)) ;
#181659 = CARTESIAN_POINT('Ctrl Pts',(-20.8120518910512,-14.2768018703547,
115.715308355643)) ;
#181660 = CARTESIAN_POINT('Ctrl Pts',(-20.8264905483566,-14.336973804146,
115.759286178215)) ;
#181661 = CARTESIAN_POINT('Ctrl Pts',(-20.9002943651876,-14.336973870652,
115.735055055544)) ;
#181662 = CARTESIAN_POINT('Ctrl Pts',(-20.9740981820186,-14.3369739371579,
115.710823932872)) ;
#181663 = CARTESIAN_POINT('Ctrl Pts',(-20.9596595247132,-14.2768020033666,
115.6668461103)) ;
#181664 = CARTESIAN_POINT('Ctrl Pts',(-21.012974127338,-14.0672719747909,
115.864923528027)) ;
#181665 = CARTESIAN_POINT('Ctrl Pts',(-20.9940531582264,-14.0216384576254,
115.807293306955)) ;
#181666 = CARTESIAN_POINT('Ctrl Pts',(-20.9202493344567,-14.0216383725684,
115.831524408492)) ;
#181667 = CARTESIAN_POINT('Ctrl Pts',(-20.8464455106869,-14.0216382875114,
115.855755510029)) ;
#181668 = CARTESIAN_POINT('Ctrl Pts',(-20.8653664797985,-14.067271804677,
115.913385731101)) ;
#181669 = CARTESIAN_POINT('Ctrl Pts',(-20.88428744891,-14.1129053218425,115.971015952173)) ;
#181670 = CARTESIAN_POINT('Ctrl Pts',(-20.9580912726798,-14.1129054068995,
115.946784850636)) ;
#181671 = CARTESIAN_POINT('Ctrl Pts',(-21.0318950964495,-14.1129054919565,
115.922553749099)) ;
#181672 = CARTESIAN_POINT('Ctrl Pts',(-21.012974127338,-14.0672719747909,
115.864923528027)) ;
#181673 = CARTESIAN_POINT('Ctrl Pts',(-21.0462752479574,-13.8140437794069,
116.001605423442)) ;
#181674 = CARTESIAN_POINT('Ctrl Pts',(-21.0242717527116,-13.786022349902,
115.934586325172)) ;
#181675 = CARTESIAN_POINT('Ctrl Pts',(-20.9504679209727,-13.7860222533108,
115.958817402436)) ;
#181676 = CARTESIAN_POINT('Ctrl Pts',(-20.8766640892339,-13.7860221567197,
115.983048479701)) ;
#181677 = CARTESIAN_POINT('Ctrl Pts',(-20.8986675844797,-13.8140435862246,
116.050067577971)) ;
#181678 = CARTESIAN_POINT('Ctrl Pts',(-20.9206710797256,-13.8420650157295,
116.117086676241)) ;
#181679 = CARTESIAN_POINT('Ctrl Pts',(-20.9944749114644,-13.8420651123206,
116.092855598977)) ;
#181680 = CARTESIAN_POINT('Ctrl Pts',(-21.0682787432033,-13.8420652089118,
116.068624521712)) ;
#181681 = CARTESIAN_POINT('Ctrl Pts',(-21.0462752479574,-13.8140437794069,
116.001605423442)) ;
#181682 = CARTESIAN_POINT('Ctrl Pts',(-21.057235818105,-13.5305545368903,
116.070529359299)) ;
#181683 = CARTESIAN_POINT('Ctrl Pts',(-21.0336987141124,-13.5222834200997,
115.998839136312)) ;
#181684 = CARTESIAN_POINT('Ctrl Pts',(-20.9598948737852,-13.5222833210965,
116.023070187418)) ;
#181685 = CARTESIAN_POINT('Ctrl Pts',(-20.8860910334581,-13.5222832220932,
116.047301238524)) ;
#181686 = CARTESIAN_POINT('Ctrl Pts',(-20.9096281374507,-13.5305543388838,
116.11899146151)) ;
#181687 = CARTESIAN_POINT('Ctrl Pts',(-20.9331652414433,-13.5388254556744,
116.190681684497)) ;
#181688 = CARTESIAN_POINT('Ctrl Pts',(-21.0069690817705,-13.5388255546776,
116.166450633391)) ;
#181689 = CARTESIAN_POINT('Ctrl Pts',(-21.0807729220976,-13.5388256536809,
116.142219582285)) ;
#181690 = CARTESIAN_POINT('Ctrl Pts',(-21.057235818105,-13.5305545368903,
116.070529359299)) ;
#181691 = CARTESIAN_POINT('Ctrl Pts',(-21.0439982208835,-13.2400469135056,
116.065602507524)) ;
#181692 = CARTESIAN_POINT('Ctrl Pts',(-21.0206177244586,-13.2520460162367,
115.994389286006)) ;
#181693 = CARTESIAN_POINT('Ctrl Pts',(-20.9468138760363,-13.2520459225966,
116.018620312456)) ;
#181694 = CARTESIAN_POINT('Ctrl Pts',(-20.873010027614,-13.2520458289565,
116.042851338905)) ;
#181695 = CARTESIAN_POINT('Ctrl Pts',(-20.8963905240389,-13.2400467262255,
116.114064560423)) ;
#181696 = CARTESIAN_POINT('Ctrl Pts',(-20.9197710204638,-13.2280476234944,
116.18527778194)) ;
#181697 = CARTESIAN_POINT('Ctrl Pts',(-20.9935748688861,-13.2280477171344,
116.161046755491)) ;
#181698 = CARTESIAN_POINT('Ctrl Pts',(-21.0673787173084,-13.2280478107745,
116.136815729041)) ;
#181699 = CARTESIAN_POINT('Ctrl Pts',(-21.0439982208835,-13.2400469135056,
116.065602507524)) ;
#181700 = CARTESIAN_POINT('Ctrl Pts',(-21.0066020047252,-12.9607801917685,
115.987295334548)) ;
#181701 = CARTESIAN_POINT('Ctrl Pts',(-20.9850605701347,-12.9922952069383,
115.921683598776)) ;
#181702 = CARTESIAN_POINT('Ctrl Pts',(-20.911256714969,-12.9922951270176,
115.945914604686)) ;
#181703 = CARTESIAN_POINT('Ctrl Pts',(-20.8374528598033,-12.9922950470968,
115.970145610596)) ;
#181704 = CARTESIAN_POINT('Ctrl Pts',(-20.8589942943938,-12.960780031927,
116.035757346369)) ;
#181705 = CARTESIAN_POINT('Ctrl Pts',(-20.8805357289843,-12.9292650167572,
116.101369082141)) ;
#181706 = CARTESIAN_POINT('Ctrl Pts',(-20.95433958415,-12.929265096678,116.077138076231)) ;
#181707 = CARTESIAN_POINT('Ctrl Pts',(-21.0281434393157,-12.9292651765987,
116.052907070321)) ;
#181708 = CARTESIAN_POINT('Ctrl Pts',(-21.0066020047252,-12.9607801917685,
115.987295334548)) ;
#181709 = CARTESIAN_POINT('Ctrl Pts',(-20.9473443980316,-12.7157522020321,
115.842202222821)) ;
#181710 = CARTESIAN_POINT('Ctrl Pts',(-20.929175396646,-12.7644222769748,
115.786862374571)) ;
#181711 = CARTESIAN_POINT('Ctrl Pts',(-20.8553715365486,-12.7644222146516,
115.81109336546)) ;
#181712 = CARTESIAN_POINT('Ctrl Pts',(-20.7815676764512,-12.7644221523283,
115.835324356349)) ;
#181713 = CARTESIAN_POINT('Ctrl Pts',(-20.7997366778369,-12.7157520773856,
115.8906642046)) ;
#181714 = CARTESIAN_POINT('Ctrl Pts',(-20.8179056792225,-12.6670820024428,
115.946004052851)) ;
#181715 = CARTESIAN_POINT('Ctrl Pts',(-20.8917095393199,-12.6670820647661,
115.921773061961)) ;
#181716 = CARTESIAN_POINT('Ctrl Pts',(-20.9655133994172,-12.6670821270893,
115.897542071072)) ;
#181717 = CARTESIAN_POINT('Ctrl Pts',(-20.9473443980316,-12.7157522020321,
115.842202222821)) ;
#181718 = CARTESIAN_POINT('Ctrl Pts',(-20.8694399766873,-12.5205021117526,
115.640390114338)) ;
#181719 = CARTESIAN_POINT('Ctrl Pts',(-20.8559487341846,-12.5828779756765,
115.599297965034)) ;
#181720 = CARTESIAN_POINT('Ctrl Pts',(-20.7821448714235,-12.5828779339693,
115.62352894781)) ;
#181721 = CARTESIAN_POINT('Ctrl Pts',(-20.7083410086625,-12.582877892262,
115.647759930586)) ;
#181722 = CARTESIAN_POINT('Ctrl Pts',(-20.7218322511651,-12.5205020283381,
115.688852079889)) ;
#181723 = CARTESIAN_POINT('Ctrl Pts',(-20.7353234936678,-12.4581261644142,
115.729944229193)) ;
#181724 = CARTESIAN_POINT('Ctrl Pts',(-20.8091273564289,-12.4581262061215,
115.705713246417)) ;
#181725 = CARTESIAN_POINT('Ctrl Pts',(-20.88293121919,-12.4581262478287,115.681482263641)) ;
#181726 = CARTESIAN_POINT('Ctrl Pts',(-20.8694399766873,-12.5205021117526,
115.640390114338)) ;
#181727 = CARTESIAN_POINT('Ctrl Pts',(-20.7779765651367,-12.3896091910669,
115.397208988666)) ;
#181728 = CARTESIAN_POINT('Ctrl Pts',(-20.7701183297895,-12.4612182427459,
115.373274070417)) ;
#181729 = CARTESIAN_POINT('Ctrl Pts',(-20.6963144664325,-12.4612182215385,
115.397505051378)) ;
#181730 = CARTESIAN_POINT('Ctrl Pts',(-20.6225106030756,-12.461218200331,
115.421736032339)) ;
#181731 = CARTESIAN_POINT('Ctrl Pts',(-20.6303688384228,-12.389609148652,
115.445670950587)) ;
#181732 = CARTESIAN_POINT('Ctrl Pts',(-20.6382270737699,-12.318000096973,
115.469605868836)) ;
#181733 = CARTESIAN_POINT('Ctrl Pts',(-20.7120309371269,-12.3180001181804,
115.445374887875)) ;
#181734 = CARTESIAN_POINT('Ctrl Pts',(-20.7858348004839,-12.3180001393879,
115.421143906914)) ;
#181735 = CARTESIAN_POINT('Ctrl Pts',(-20.7779765651367,-12.3896091910669,
115.397208988666)) ;
#181736 = CARTESIAN_POINT('Ctrl Pts',(-20.6779561212234,-12.3322116649338,
115.128190401515)) ;
#181737 = CARTESIAN_POINT('Ctrl Pts',(-20.6763321849345,-12.4079372852091,
115.123244152491)) ;
#181738 = CARTESIAN_POINT('Ctrl Pts',(-20.6025283236232,-12.4079372823359,
115.147475139682)) ;
#181739 = CARTESIAN_POINT('Ctrl Pts',(-20.5287244623119,-12.4079372794628,
115.171706126874)) ;
#181740 = CARTESIAN_POINT('Ctrl Pts',(-20.5303483986008,-12.3322116591875,
115.176652375899)) ;
#181741 = CARTESIAN_POINT('Ctrl Pts',(-20.5319723348897,-12.2564860389122,
115.181598624924)) ;
#181742 = CARTESIAN_POINT('Ctrl Pts',(-20.605776196201,-12.2564860417854,
115.157367637732)) ;
#181743 = CARTESIAN_POINT('Ctrl Pts',(-20.6795800575123,-12.2564860446585,
115.13313665054)) ;
#181744 = CARTESIAN_POINT('Ctrl Pts',(-20.6779561212234,-12.3322116649338,
115.128190401515)) ;
#181745 = CARTESIAN_POINT('Ctrl Pts',(-20.5774147689211,-12.3526193896652,
114.857217210318)) ;
#181746 = CARTESIAN_POINT('Ctrl Pts',(-20.582078673644,-12.4270343562084,
114.871422710604)) ;
#181747 = CARTESIAN_POINT('Ctrl Pts',(-20.5082748147709,-12.4270343671983,
114.895653705222)) ;
#181748 = CARTESIAN_POINT('Ctrl Pts',(-20.4344709558978,-12.4270343781882,
114.919884699841)) ;
#181749 = CARTESIAN_POINT('Ctrl Pts',(-20.4298070511749,-12.352619411645,
114.905679199554)) ;
#181750 = CARTESIAN_POINT('Ctrl Pts',(-20.4251431464519,-12.2782044451017,
114.891473699268)) ;
#181751 = CARTESIAN_POINT('Ctrl Pts',(-20.498947005325,-12.2782044341118,
114.86724270465)) ;
#181752 = CARTESIAN_POINT('Ctrl Pts',(-20.5727508641981,-12.2782044231219,
114.843011710032)) ;
#181753 = CARTESIAN_POINT('Ctrl Pts',(-20.5774147689211,-12.3526193896652,
114.857217210318)) ;
#181754 = CARTESIAN_POINT('Ctrl Pts',(-20.480876963674,-12.4495335034968,
114.598771665885)) ;
#181755 = CARTESIAN_POINT('Ctrl Pts',(-20.4915518909879,-12.5172950398371,
114.631285771301)) ;
#181756 = CARTESIAN_POINT('Ctrl Pts',(-20.4177480363705,-12.517295059255,
114.655516778881)) ;
#181757 = CARTESIAN_POINT('Ctrl Pts',(-20.343944181753,-12.5172950786729,
114.679747786462)) ;
#181758 = CARTESIAN_POINT('Ctrl Pts',(-20.333269254439,-12.4495335423326,
114.647233681045)) ;
#181759 = CARTESIAN_POINT('Ctrl Pts',(-20.3225943271251,-12.3817720059923,
114.614719575629)) ;
#181760 = CARTESIAN_POINT('Ctrl Pts',(-20.3963981817425,-12.3817719865744,
114.590488568049)) ;
#181761 = CARTESIAN_POINT('Ctrl Pts',(-20.47020203636,-12.3817719671566,114.566257560468)) ;
#181762 = CARTESIAN_POINT('Ctrl Pts',(-20.480876963674,-12.4495335034968,
114.598771665885)) ;
#181763 = CARTESIAN_POINT('Ctrl Pts',(-20.3957540886572,-12.6159519111974,
114.374983031782)) ;
#181764 = CARTESIAN_POINT('Ctrl Pts',(-20.411654514387,-12.6721964554001,
114.423413162412)) ;
#181765 = CARTESIAN_POINT('Ctrl Pts',(-20.337850663774,-12.6721964775936,
114.447644182189)) ;
#181766 = CARTESIAN_POINT('Ctrl Pts',(-20.264046813161,-12.6721964997871,
114.471875201966)) ;
#181767 = CARTESIAN_POINT('Ctrl Pts',(-20.2481463874312,-12.6159519555843,
114.423445071337)) ;
#181768 = CARTESIAN_POINT('Ctrl Pts',(-20.2322459617013,-12.5597074113816,
114.375014940707)) ;
#181769 = CARTESIAN_POINT('Ctrl Pts',(-20.3060498123144,-12.5597073891882,
114.35078392093)) ;
#181770 = CARTESIAN_POINT('Ctrl Pts',(-20.3798536629274,-12.5597073669947,
114.326552901153)) ;
#181771 = CARTESIAN_POINT('Ctrl Pts',(-20.3957540886572,-12.6159519111974,
114.374983031782)) ;
#181772 = CARTESIAN_POINT('Ctrl Pts',(-20.3271536623197,-12.8395609374739,
114.201485817632)) ;
#181773 = CARTESIAN_POINT('Ctrl Pts',(-20.3471345416621,-12.8802774256323,
114.262344351742)) ;
#181774 = CARTESIAN_POINT('Ctrl Pts',(-20.2733306944363,-12.8802774463099,
114.286575381836)) ;
#181775 = CARTESIAN_POINT('Ctrl Pts',(-20.1995268472104,-12.8802774669874,
114.31080641193)) ;
#181776 = CARTESIAN_POINT('Ctrl Pts',(-20.179545967868,-12.839560978829,114.24994787782)) ;
#181777 = CARTESIAN_POINT('Ctrl Pts',(-20.1595650885256,-12.7988444906705,
114.189089343709)) ;
#181778 = CARTESIAN_POINT('Ctrl Pts',(-20.2333689357514,-12.798844469993,
114.164858313616)) ;
#181779 = CARTESIAN_POINT('Ctrl Pts',(-20.3071727829772,-12.7988444493154,
114.140627283522)) ;
#181780 = CARTESIAN_POINT('Ctrl Pts',(-20.3271536623197,-12.8395609374739,
114.201485817632)) ;
#181781 = CARTESIAN_POINT('Ctrl Pts',(-20.2791583118047,-13.1036924153161,
114.090643871318)) ;
#181782 = CARTESIAN_POINT('Ctrl Pts',(-20.3017891444804,-13.126027690226,
114.159573735842)) ;
#181783 = CARTESIAN_POINT('Ctrl Pts',(-20.2279852997255,-13.1260277069746,
114.183804773462)) ;
#181784 = CARTESIAN_POINT('Ctrl Pts',(-20.1541814549706,-13.1260277237232,
114.208035811082)) ;
#181785 = CARTESIAN_POINT('Ctrl Pts',(-20.1315506222949,-13.1036924488133,
114.139105946557)) ;
#181786 = CARTESIAN_POINT('Ctrl Pts',(-20.1089197896193,-13.0813571739034,
114.070176082033)) ;
#181787 = CARTESIAN_POINT('Ctrl Pts',(-20.1827236343742,-13.0813571571548,
114.045945044413)) ;
#181788 = CARTESIAN_POINT('Ctrl Pts',(-20.2565274791291,-13.0813571404062,
114.021714006793)) ;
#181789 = CARTESIAN_POINT('Ctrl Pts',(-20.2791583118047,-13.1036924153161,
114.090643871318)) ;
#181790 = CARTESIAN_POINT('Ctrl Pts',(-20.2542197759365,-13.3927905140901,
114.05034234162)) ;
#181791 = CARTESIAN_POINT('Ctrl Pts',(-20.277888414452,-13.3949729390862,
114.122433195443)) ;
#181792 = CARTESIAN_POINT('Ctrl Pts',(-20.204084571161,-13.3949729481192,
114.146664237522)) ;
#181793 = CARTESIAN_POINT('Ctrl Pts',(-20.1302807278701,-13.3949729571521,
114.170895279601)) ;
#181794 = CARTESIAN_POINT('Ctrl Pts',(-20.1066120893547,-13.392790532156,
114.098804425778)) ;
#181795 = CARTESIAN_POINT('Ctrl Pts',(-20.0829434508393,-13.3906081071599,
114.026713571955)) ;
#181796 = CARTESIAN_POINT('Ctrl Pts',(-20.1567472941302,-13.390608098127,
114.002482529876)) ;
#181797 = CARTESIAN_POINT('Ctrl Pts',(-20.2305511374211,-13.3906080890941,
113.978251487797)) ;
#181798 = CARTESIAN_POINT('Ctrl Pts',(-20.2542197759365,-13.3927905140901,
114.05034234162)) ;
#181799 = CARTESIAN_POINT('Ctrl Pts',(-20.2537651631048,-13.6807940128297,
114.084250210379)) ;
#181800 = CARTESIAN_POINT('Ctrl Pts',(-20.2767706334503,-13.6628697332101,
114.154321161045)) ;
#181801 = CARTESIAN_POINT('Ctrl Pts',(-20.2029667904965,-13.6628697375112,
114.178552204151)) ;
#181802 = CARTESIAN_POINT('Ctrl Pts',(-20.1291629475428,-13.6628697418123,
114.202783247257)) ;
#181803 = CARTESIAN_POINT('Ctrl Pts',(-20.1061574771973,-13.680794021432,
114.132712296591)) ;
#181804 = CARTESIAN_POINT('Ctrl Pts',(-20.0831520068518,-13.6987183010517,
114.062641345926)) ;
#181805 = CARTESIAN_POINT('Ctrl Pts',(-20.1569558498055,-13.6987182967505,
114.03841030282)) ;
#181806 = CARTESIAN_POINT('Ctrl Pts',(-20.2307596927593,-13.6987182924494,
114.014179259714)) ;
#181807 = CARTESIAN_POINT('Ctrl Pts',(-20.2537651631048,-13.6807940128297,
114.084250210379)) ;
#181808 = CARTESIAN_POINT('Ctrl Pts',(-20.2767369580529,-13.9516407801447,
114.189702183706)) ;
#181809 = CARTESIAN_POINT('Ctrl Pts',(-20.2974385928997,-13.9147771638665,
114.252756023256)) ;
#181810 = CARTESIAN_POINT('Ctrl Pts',(-20.2236347495658,-13.9147771635359,
114.276987065204)) ;
#181811 = CARTESIAN_POINT('Ctrl Pts',(-20.1498309062319,-13.9147771632054,
114.301218107152)) ;
#181812 = CARTESIAN_POINT('Ctrl Pts',(-20.1291292713852,-13.9516407794836,
114.238164267602)) ;
#181813 = CARTESIAN_POINT('Ctrl Pts',(-20.1084276365384,-13.9885043957617,
114.175110428052)) ;
#181814 = CARTESIAN_POINT('Ctrl Pts',(-20.1822314798723,-13.9885043960923,
114.150879386104)) ;
#181815 = CARTESIAN_POINT('Ctrl Pts',(-20.2560353232062,-13.9885043964229,
114.126648344155)) ;
#181816 = CARTESIAN_POINT('Ctrl Pts',(-20.2767369580529,-13.9516407801447,
114.189702183706)) ;
#181817 = CARTESIAN_POINT('Ctrl Pts',(-20.3212515827195,-14.1848191645832,
114.360909549778)) ;
#181818 = CARTESIAN_POINT('Ctrl Pts',(-20.3381385223981,-14.1316174193291,
114.412344443398)) ;
#181819 = CARTESIAN_POINT('Ctrl Pts',(-20.2643346783687,-14.1316174171336,
114.436575483228)) ;
#181820 = CARTESIAN_POINT('Ctrl Pts',(-20.1905308343394,-14.1316174149382,
114.460806523058)) ;
#181821 = CARTESIAN_POINT('Ctrl Pts',(-20.1736438946608,-14.1848191601922,
114.409371629438)) ;
#181822 = CARTESIAN_POINT('Ctrl Pts',(-20.1567569549822,-14.2380209054463,
114.357936735817)) ;
#181823 = CARTESIAN_POINT('Ctrl Pts',(-20.2305607990116,-14.2380209076418,
114.333705695988)) ;
#181824 = CARTESIAN_POINT('Ctrl Pts',(-20.304364643041,-14.2380209098372,
114.309474656158)) ;
#181825 = CARTESIAN_POINT('Ctrl Pts',(-20.3212515827195,-14.1848191645832,
114.360909549778)) ;
#181826 = CARTESIAN_POINT('Ctrl Pts',(-20.3823727653949,-14.3611535147467,
114.582313485388)) ;
#181827 = CARTESIAN_POINT('Ctrl Pts',(-20.3942874125168,-14.2955603830771,
114.618603578166)) ;
#181828 = CARTESIAN_POINT('Ctrl Pts',(-20.3204835681855,-14.2955603814556,
114.642834617076)) ;
#181829 = CARTESIAN_POINT('Ctrl Pts',(-20.2466797238541,-14.2955603798341,
114.667065655986)) ;
#181830 = CARTESIAN_POINT('Ctrl Pts',(-20.2347650767322,-14.3611535115037,
114.630775563208)) ;
#181831 = CARTESIAN_POINT('Ctrl Pts',(-20.2228504296103,-14.4267466431733,
114.594485470431)) ;
#181832 = CARTESIAN_POINT('Ctrl Pts',(-20.2966542739417,-14.4267466447948,
114.570254431521)) ;
#181833 = CARTESIAN_POINT('Ctrl Pts',(-20.370458118273,-14.4267466464163,
114.546023392611)) ;
#181834 = CARTESIAN_POINT('Ctrl Pts',(-20.3823727653949,-14.3611535147467,
114.582313485388)) ;
#181835 = CARTESIAN_POINT('Ctrl Pts',(-20.4563210601665,-14.4717132500286,
114.843190270097)) ;
#181836 = CARTESIAN_POINT('Ctrl Pts',(-20.4623519080848,-14.3983025037114,
114.861559259812)) ;
#181837 = CARTESIAN_POINT('Ctrl Pts',(-20.3885480641969,-14.3983025035885,
114.885790300072)) ;
#181838 = CARTESIAN_POINT('Ctrl Pts',(-20.314744220309,-14.3983025034657,
114.910021340333)) ;
#181839 = CARTESIAN_POINT('Ctrl Pts',(-20.3087133723907,-14.4717132497829,
114.891652350619)) ;
#181840 = CARTESIAN_POINT('Ctrl Pts',(-20.3026825244725,-14.5451239961002,
114.873283360904)) ;
#181841 = CARTESIAN_POINT('Ctrl Pts',(-20.3764863683604,-14.545123996223,
114.849052320643)) ;
#181842 = CARTESIAN_POINT('Ctrl Pts',(-20.4502902122482,-14.5451239963458,
114.824821280383)) ;
#181843 = CARTESIAN_POINT('Ctrl Pts',(-20.4563210601665,-14.4717132500286,
114.843190270097)) ;
#181844 = CARTESIAN_POINT('Ctrl Pts',(-20.5359913410577,-14.5058049610956,
115.121300978399)) ;
#181845 = CARTESIAN_POINT('Ctrl Pts',(-20.5357343387305,-14.4299061959812,
115.120518190733)) ;
#181846 = CARTESIAN_POINT('Ctrl Pts',(-20.4619304960325,-14.4299061963414,
115.144749234618)) ;
#181847 = CARTESIAN_POINT('Ctrl Pts',(-20.3881266533344,-14.4299061967016,
115.168980278503)) ;
#181848 = CARTESIAN_POINT('Ctrl Pts',(-20.3883836556616,-14.505804961816,
115.169763066168)) ;
#181849 = CARTESIAN_POINT('Ctrl Pts',(-20.3886406579888,-14.5817037269304,
115.170545853834)) ;
#181850 = CARTESIAN_POINT('Ctrl Pts',(-20.4624445006868,-14.5817037265702,
115.146314809949)) ;
#181851 = CARTESIAN_POINT('Ctrl Pts',(-20.5362483433849,-14.58170372621,115.122083766064)) ;
#181852 = CARTESIAN_POINT('Ctrl Pts',(-20.5359913410577,-14.5058049610956,
115.121300978399)) ;
#181853 = CARTESIAN_POINT('Ctrl Pts',(-20.6152285993297,-14.4622432474708,
115.398086166475)) ;
#181854 = CARTESIAN_POINT('Ctrl Pts',(-20.6087050569855,-14.389275462024,
115.378216508923)) ;
#181855 = CARTESIAN_POINT('Ctrl Pts',(-20.5349012157987,-14.3892754604599,
115.402447557411)) ;
#181856 = CARTESIAN_POINT('Ctrl Pts',(-20.4610973746118,-14.3892754588959,
115.426678605899)) ;
#181857 = CARTESIAN_POINT('Ctrl Pts',(-20.4676209169561,-14.4622432443427,
115.44654826345)) ;
#181858 = CARTESIAN_POINT('Ctrl Pts',(-20.4741444593003,-14.5352110297894,
115.466417921002)) ;
#181859 = CARTESIAN_POINT('Ctrl Pts',(-20.5479483004871,-14.5352110313535,
115.442186872514)) ;
#181860 = CARTESIAN_POINT('Ctrl Pts',(-20.621752141674,-14.5352110329176,
115.417955824026)) ;
#181861 = CARTESIAN_POINT('Ctrl Pts',(-20.6152285993297,-14.4622432474708,
115.398086166475)) ;
#181862 = CARTESIAN_POINT('Ctrl Pts',(-20.6876764922037,-14.343914063795,
115.654200032397)) ;
#181863 = CARTESIAN_POINT('Ctrl Pts',(-20.6753512998401,-14.2791023763225,
115.616659484858)) ;
#181864 = CARTESIAN_POINT('Ctrl Pts',(-20.6015474601322,-14.2791023697226,
115.64089053785)) ;
#181865 = CARTESIAN_POINT('Ctrl Pts',(-20.5277436204242,-14.2791023631227,
115.665121590843)) ;
#181866 = CARTESIAN_POINT('Ctrl Pts',(-20.5400688127878,-14.3439140505953,
115.702662138382)) ;
#181867 = CARTESIAN_POINT('Ctrl Pts',(-20.5523940051514,-14.4087257380679,
115.740202685921)) ;
#181868 = CARTESIAN_POINT('Ctrl Pts',(-20.6261978448593,-14.4087257446678,
115.715971632929)) ;
#181869 = CARTESIAN_POINT('Ctrl Pts',(-20.7000016845672,-14.4087257512676,
115.691740579936)) ;
#181870 = CARTESIAN_POINT('Ctrl Pts',(-20.6876764922037,-14.343914063795,
115.654200032397)) ;
#181871 = CARTESIAN_POINT('Ctrl Pts',(-20.7473748229597,-14.1592285094383,
115.871492526232)) ;
#181872 = CARTESIAN_POINT('Ctrl Pts',(-20.7301296462246,-14.1072180552491,
115.818966499993)) ;
#181873 = CARTESIAN_POINT('Ctrl Pts',(-20.6563258073989,-14.1072180404113,
115.843197555672)) ;
#181874 = CARTESIAN_POINT('Ctrl Pts',(-20.5825219685731,-14.1072180255735,
115.867428611351)) ;
#181875 = CARTESIAN_POINT('Ctrl Pts',(-20.5997671453082,-14.1592284797627,
115.91995463759)) ;
#181876 = CARTESIAN_POINT('Ctrl Pts',(-20.6170123220432,-14.2112389339519,
115.97248066383)) ;
#181877 = CARTESIAN_POINT('Ctrl Pts',(-20.690816160869,-14.2112389487897,
115.948249608151)) ;
#181878 = CARTESIAN_POINT('Ctrl Pts',(-20.7646199996947,-14.2112389636275,
115.924018552472)) ;
#181879 = CARTESIAN_POINT('Ctrl Pts',(-20.7473748229597,-14.1592285094383,
115.871492526232)) ;
#181880 = CARTESIAN_POINT('Ctrl Pts',(-20.7892502687807,-13.9218383285055,
116.034450676081)) ;
#181881 = CARTESIAN_POINT('Ctrl Pts',(-20.7683235711504,-13.8863275964736,
115.97071133106)) ;
#181882 = CARTESIAN_POINT('Ctrl Pts',(-20.6945197320421,-13.8863275716233,
115.994942385878)) ;
#181883 = CARTESIAN_POINT('Ctrl Pts',(-20.6207158929338,-13.886327546773,
116.019173440697)) ;
#181884 = CARTESIAN_POINT('Ctrl Pts',(-20.6416425905641,-13.9218382788049,
116.082912785718)) ;
#181885 = CARTESIAN_POINT('Ctrl Pts',(-20.6625692881944,-13.9573490108368,
116.146652130738)) ;
#181886 = CARTESIAN_POINT('Ctrl Pts',(-20.7363731273027,-13.9573490356871,
116.12242107592)) ;
#181887 = CARTESIAN_POINT('Ctrl Pts',(-20.810176966411,-13.9573490605374,
116.098190021101)) ;
#181888 = CARTESIAN_POINT('Ctrl Pts',(-20.7892502687807,-13.9218383285055,
116.034450676081)) ;
#181889 = CARTESIAN_POINT('Ctrl Pts',(-20.8096697160064,-13.6477929587425,
116.132141353103)) ;
#181890 = CARTESIAN_POINT('Ctrl Pts',(-20.7865525111925,-13.6313648712608,
116.061730076469)) ;
#181891 = CARTESIAN_POINT('Ctrl Pts',(-20.7127486704703,-13.6313648350965,
116.085961126372)) ;
#181892 = CARTESIAN_POINT('Ctrl Pts',(-20.638944829748,-13.6313647989322,
116.110192176274)) ;
#181893 = CARTESIAN_POINT('Ctrl Pts',(-20.6620620345618,-13.6477928864138,
116.180603452908)) ;
#181894 = CARTESIAN_POINT('Ctrl Pts',(-20.6851792393755,-13.6642209738955,
116.251014729542)) ;
#181895 = CARTESIAN_POINT('Ctrl Pts',(-20.7589830800978,-13.6642210100599,
116.22678367964)) ;
#181896 = CARTESIAN_POINT('Ctrl Pts',(-20.8327869208201,-13.6642210462242,
116.202552629737)) ;
#181897 = CARTESIAN_POINT('Ctrl Pts',(-20.8096697160064,-13.6477929587425,
116.132141353103)) ;
#181898 = CARTESIAN_POINT('Ctrl Pts',(-20.8062757150026,-13.3573882946602,
116.157281504951)) ;
#181899 = CARTESIAN_POINT('Ctrl Pts',(-20.7826279371143,-13.3612124494826,
116.085254188169)) ;
#181900 = CARTESIAN_POINT('Ctrl Pts',(-20.7088240931421,-13.3612124035114,
116.109485228173)) ;
#181901 = CARTESIAN_POINT('Ctrl Pts',(-20.6350202491699,-13.3612123575402,
116.133716268177)) ;
#181902 = CARTESIAN_POINT('Ctrl Pts',(-20.6586680270582,-13.3573882027177,
116.205743584959)) ;
#181903 = CARTESIAN_POINT('Ctrl Pts',(-20.6823158049464,-13.3535640478952,
116.277770901741)) ;
#181904 = CARTESIAN_POINT('Ctrl Pts',(-20.7561196489186,-13.3535640938664,
116.253539861737)) ;
#181905 = CARTESIAN_POINT('Ctrl Pts',(-20.8299234928908,-13.3535641398377,
116.229308821733)) ;
#181906 = CARTESIAN_POINT('Ctrl Pts',(-20.8062757150026,-13.3573882946602,
116.157281504951)) ;
#181907 = CARTESIAN_POINT('Ctrl Pts',(-20.7786075112858,-13.0713760146383,
116.108481462324)) ;
#181908 = CARTESIAN_POINT('Ctrl Pts',(-20.7561233059056,-13.0951747720227,
116.03999819949)) ;
#181909 = CARTESIAN_POINT('Ctrl Pts',(-20.682319457276,-13.0951747198527,
116.064229225309)) ;
#181910 = CARTESIAN_POINT('Ctrl Pts',(-20.6085156086464,-13.0951746676827,
116.088460251127)) ;
#181911 = CARTESIAN_POINT('Ctrl Pts',(-20.6309998140267,-13.0713759102982,
116.156943513961)) ;
#181912 = CARTESIAN_POINT('Ctrl Pts',(-20.6534840194069,-13.0475771529138,
116.225426776795)) ;
#181913 = CARTESIAN_POINT('Ctrl Pts',(-20.7272878680365,-13.0475772050838,
116.201195750976)) ;
#181914 = CARTESIAN_POINT('Ctrl Pts',(-20.8010917166661,-13.0475772572539,
116.176964725158)) ;
#181915 = CARTESIAN_POINT('Ctrl Pts',(-20.7786075112858,-13.0713760146383,
116.108481462324)) ;
#181916 = CARTESIAN_POINT('Ctrl Pts',(-20.727862298227,-12.8101300373193,
115.989403245096)) ;
#181917 = CARTESIAN_POINT('Ctrl Pts',(-20.7081542834235,-12.852202961782,
115.929375810654)) ;
#181918 = CARTESIAN_POINT('Ctrl Pts',(-20.634350429137,-12.8522029087301,
115.953606819242)) ;
#181919 = CARTESIAN_POINT('Ctrl Pts',(-20.5605465748504,-12.8522028556782,
115.97783782783)) ;
#181920 = CARTESIAN_POINT('Ctrl Pts',(-20.5802545896539,-12.8101299312156,
116.037865262272)) ;
#181921 = CARTESIAN_POINT('Ctrl Pts',(-20.5999626044573,-12.7680570067529,
116.097892696714)) ;
#181922 = CARTESIAN_POINT('Ctrl Pts',(-20.6737664587439,-12.7680570598048,
116.073661688126)) ;
#181923 = CARTESIAN_POINT('Ctrl Pts',(-20.7475703130304,-12.7680571128567,
116.049430679538)) ;
#181924 = CARTESIAN_POINT('Ctrl Pts',(-20.727862298227,-12.8101300373193,
115.989403245096)) ;
#181925 = CARTESIAN_POINT('Ctrl Pts',(-20.6569850715304,-12.5926203368979,
115.808983189136)) ;
#181926 = CARTESIAN_POINT('Ctrl Pts',(-20.6414632766714,-12.6499401722223,
115.761706305044)) ;
#181927 = CARTESIAN_POINT('Ctrl Pts',(-20.5676594164585,-12.6499401250942,
115.785937295581)) ;
#181928 = CARTESIAN_POINT('Ctrl Pts',(-20.4938555562457,-12.6499400779661,
115.810168286119)) ;
#181929 = CARTESIAN_POINT('Ctrl Pts',(-20.5093773511048,-12.5926202426416,
115.857445170211)) ;
#181930 = CARTESIAN_POINT('Ctrl Pts',(-20.5248991459638,-12.5353004073172,
115.904722054302)) ;
#181931 = CARTESIAN_POINT('Ctrl Pts',(-20.5987030061767,-12.5353004544453,
115.880491063765)) ;
#181932 = CARTESIAN_POINT('Ctrl Pts',(-20.6725068663895,-12.5353005015734,
115.856260073227)) ;
#181933 = CARTESIAN_POINT('Ctrl Pts',(-20.6569850715304,-12.5926203368979,
115.808983189136)) ;
#181934 = CARTESIAN_POINT('Ctrl Pts',(-20.5702654370651,-12.4341144288436,
115.580315447972)) ;
#181935 = CARTESIAN_POINT('Ctrl Pts',(-20.5600417992635,-12.5025837722115,
115.549175895275)) ;
#181936 = CARTESIAN_POINT('Ctrl Pts',(-20.4862379335849,-12.5025837377898,
115.573406869165)) ;
#181937 = CARTESIAN_POINT('Ctrl Pts',(-20.4124340679063,-12.502583703368,
115.597637843054)) ;
#181938 = CARTESIAN_POINT('Ctrl Pts',(-20.4226577057078,-12.4341143600001,
115.628777395751)) ;
#181939 = CARTESIAN_POINT('Ctrl Pts',(-20.4328813435093,-12.3656450166321,
115.659916948448)) ;
#181940 = CARTESIAN_POINT('Ctrl Pts',(-20.506685209188,-12.3656450510539,
115.635685974559)) ;
#181941 = CARTESIAN_POINT('Ctrl Pts',(-20.5804890748666,-12.3656450854756,
115.611455000669)) ;
#181942 = CARTESIAN_POINT('Ctrl Pts',(-20.5702654370651,-12.4341144288436,
115.580315447972)) ;
#181943 = CARTESIAN_POINT('Ctrl Pts',(-20.4730652679923,-12.346259851331,
115.319760267267)) ;
#181944 = CARTESIAN_POINT('Ctrl Pts',(-20.4688784108342,-12.4209624752005,
115.30700777424)) ;
#181945 = CARTESIAN_POINT('Ctrl Pts',(-20.3950745409072,-12.4209624599237,
115.33123873519)) ;
#181946 = CARTESIAN_POINT('Ctrl Pts',(-20.3212706709801,-12.4209624446469,
115.355469696139)) ;
#181947 = CARTESIAN_POINT('Ctrl Pts',(-20.3254575281383,-12.3462598207773,
115.368222189166)) ;
#181948 = CARTESIAN_POINT('Ctrl Pts',(-20.3296443852964,-12.2715571969078,
115.380974682192)) ;
#181949 = CARTESIAN_POINT('Ctrl Pts',(-20.4034482552235,-12.2715572121846,
115.356743721243)) ;
#181950 = CARTESIAN_POINT('Ctrl Pts',(-20.4772521251505,-12.2715572274614,
115.332512760293)) ;
#181951 = CARTESIAN_POINT('Ctrl Pts',(-20.4730652679923,-12.346259851331,
115.319760267267)) ;
#181952 = CARTESIAN_POINT('Ctrl Pts',(-20.372232841033,-12.3348158852733,
115.047945482228)) ;
#181953 = CARTESIAN_POINT('Ctrl Pts',(-20.3743491903962,-12.4104256805368,
115.054391539147)) ;
#181954 = CARTESIAN_POINT('Ctrl Pts',(-20.3005453185203,-12.4104256886821,
115.078622494161)) ;
#181955 = CARTESIAN_POINT('Ctrl Pts',(-20.2267414466445,-12.4104256968275,
115.102853449174)) ;
#181956 = CARTESIAN_POINT('Ctrl Pts',(-20.2246250972813,-12.334815901564,
115.096407392256)) ;
#181957 = CARTESIAN_POINT('Ctrl Pts',(-20.2225087479182,-12.2592061063006,
115.089961335338)) ;
#181958 = CARTESIAN_POINT('Ctrl Pts',(-20.296312619794,-12.2592060981552,
115.065730380324)) ;
#181959 = CARTESIAN_POINT('Ctrl Pts',(-20.3701164916698,-12.2592060900098,
115.04149942531)) ;
#181960 = CARTESIAN_POINT('Ctrl Pts',(-20.372232841033,-12.3348158852733,
115.047945482228)) ;
#181961 = CARTESIAN_POINT('Ctrl Pts',(-20.272459099619,-12.4019396871859,
114.779822675992)) ;
#181962 = CARTESIAN_POINT('Ctrl Pts',(-20.2808041605409,-12.4729745049504,
114.805240383184)) ;
#181963 = CARTESIAN_POINT('Ctrl Pts',(-20.2070002883668,-12.4729745398318,
114.829471337289)) ;
#181964 = CARTESIAN_POINT('Ctrl Pts',(-20.1331964161927,-12.4729745747131,
114.853702291394)) ;
#181965 = CARTESIAN_POINT('Ctrl Pts',(-20.1248513552708,-12.4019397569486,
114.828284584203)) ;
#181966 = CARTESIAN_POINT('Ctrl Pts',(-20.1165062943488,-12.330904939184,
114.802866877011)) ;
#181967 = CARTESIAN_POINT('Ctrl Pts',(-20.1903101665229,-12.3309049043027,
114.778635922906)) ;
#181968 = CARTESIAN_POINT('Ctrl Pts',(-20.2641140386971,-12.3309048694214,
114.7544049688)) ;
#181969 = CARTESIAN_POINT('Ctrl Pts',(-20.272459099619,-12.4019396871859,
114.779822675992)) ;
#181970 = CARTESIAN_POINT('Ctrl Pts',(-20.1830070427554,-12.5400212389952,
114.542504031555)) ;
#181971 = CARTESIAN_POINT('Ctrl Pts',(-20.1968824352242,-12.6015185806479,
114.584766236272)) ;
#181972 = CARTESIAN_POINT('Ctrl Pts',(-20.1230785662842,-12.6015186402617,
114.608997200228)) ;
#181973 = CARTESIAN_POINT('Ctrl Pts',(-20.0492746973443,-12.6015186998755,
114.633228164184)) ;
#181974 = CARTESIAN_POINT('Ctrl Pts',(-20.0353993048755,-12.5400213582228,
114.590965959467)) ;
#181975 = CARTESIAN_POINT('Ctrl Pts',(-20.0215239124067,-12.4785240165702,
114.54870375475)) ;
#181976 = CARTESIAN_POINT('Ctrl Pts',(-20.0953277813467,-12.4785239569564,
114.524472790794)) ;
#181977 = CARTESIAN_POINT('Ctrl Pts',(-20.1691316502866,-12.4785238973426,
114.500241826838)) ;
#181978 = CARTESIAN_POINT('Ctrl Pts',(-20.1830070427554,-12.5400212389952,
114.542504031555)) ;
#181979 = CARTESIAN_POINT('Ctrl Pts',(-20.1067029971044,-12.7426569389483,
114.345713360105)) ;
#181980 = CARTESIAN_POINT('Ctrl Pts',(-20.1251890157944,-12.790097789664,
114.402018788292)) ;
#181981 = CARTESIAN_POINT('Ctrl Pts',(-20.0513851519428,-12.7900978720305,
114.426249767746)) ;
#181982 = CARTESIAN_POINT('Ctrl Pts',(-19.9775812880912,-12.790097954397,
114.450480747201)) ;
#181983 = CARTESIAN_POINT('Ctrl Pts',(-19.9590952694012,-12.7426571036813,
114.394175319013)) ;
#181984 = CARTESIAN_POINT('Ctrl Pts',(-19.9406092507112,-12.6952162529655,
114.337869890826)) ;
#181985 = CARTESIAN_POINT('Ctrl Pts',(-20.0144131145628,-12.695216170599,
114.313638911372)) ;
#181986 = CARTESIAN_POINT('Ctrl Pts',(-20.0882169784144,-12.6952160882325,
114.289407931918)) ;
#181987 = CARTESIAN_POINT('Ctrl Pts',(-20.1067029971044,-12.7426569389483,
114.345713360105)) ;
#181988 = CARTESIAN_POINT('Ctrl Pts',(-20.0499392060894,-12.9928209893326,
114.208234860581)) ;
#181989 = CARTESIAN_POINT('Ctrl Pts',(-20.0716826594989,-13.0228660525859,
114.2744619093)) ;
#181990 = CARTESIAN_POINT('Ctrl Pts',(-19.9978788029917,-13.0228661512881,
114.298692911124)) ;
#181991 = CARTESIAN_POINT('Ctrl Pts',(-19.9240749464844,-13.0228662499903,
114.322923912948)) ;
#181992 = CARTESIAN_POINT('Ctrl Pts',(-19.9023314930749,-12.992821186737,
114.256696864229)) ;
#181993 = CARTESIAN_POINT('Ctrl Pts',(-19.8805880396653,-12.9627761234838,
114.190469815509)) ;
#181994 = CARTESIAN_POINT('Ctrl Pts',(-19.9543918961725,-12.9627760247816,
114.166238813685)) ;
#181995 = CARTESIAN_POINT('Ctrl Pts',(-20.0281957526798,-12.9627759260794,
114.142007811862)) ;
#181996 = CARTESIAN_POINT('Ctrl Pts',(-20.0499392060894,-12.9928209893326,
114.208234860581)) ;
#181997 = CARTESIAN_POINT('Ctrl Pts',(-20.0153853295519,-13.274121349933,
114.138514811439)) ;
#181998 = CARTESIAN_POINT('Ctrl Pts',(-20.0388382801524,-13.2845716251807,
114.209948712753)) ;
#181999 = CARTESIAN_POINT('Ctrl Pts',(-19.9650344322706,-13.2845717326201,
114.234179740849)) ;
#182000 = CARTESIAN_POINT('Ctrl Pts',(-19.8912305843888,-13.2845718400594,
114.258410768945)) ;
#182001 = CARTESIAN_POINT('Ctrl Pts',(-19.8677776337882,-13.2741215648117,
114.18697686763)) ;
#182002 = CARTESIAN_POINT('Ctrl Pts',(-19.8443246831877,-13.263671289564,
114.115542966315)) ;
#182003 = CARTESIAN_POINT('Ctrl Pts',(-19.9181285310695,-13.2636711821247,
114.09131193822)) ;
#182004 = CARTESIAN_POINT('Ctrl Pts',(-19.9919323789513,-13.2636710746853,
114.067080910124)) ;
#182005 = CARTESIAN_POINT('Ctrl Pts',(-20.0153853295519,-13.274121349933,
114.138514811439)) ;
#182006 = CARTESIAN_POINT('Ctrl Pts',(-20.0050410507883,-13.5650423075934,
114.142439305779)) ;
#182007 = CARTESIAN_POINT('Ctrl Pts',(-20.0285177894748,-13.5551969668732,
114.213945661769)) ;
#182008 = CARTESIAN_POINT('Ctrl Pts',(-19.95471395066,-13.555197074088,114.238176717481)) ;
#182009 = CARTESIAN_POINT('Ctrl Pts',(-19.8809101118452,-13.5551971813029,
114.262407773194)) ;
#182010 = CARTESIAN_POINT('Ctrl Pts',(-19.8574333731587,-13.5650425220231,
114.190901417204)) ;
#182011 = CARTESIAN_POINT('Ctrl Pts',(-19.8339566344721,-13.5748878627432,
114.119395061214)) ;
#182012 = CARTESIAN_POINT('Ctrl Pts',(-19.9077604732869,-13.5748877555284,
114.095164005502)) ;
#182013 = CARTESIAN_POINT('Ctrl Pts',(-19.9815643121017,-13.5748876483136,
114.070932949789)) ;
#182014 = CARTESIAN_POINT('Ctrl Pts',(-20.0050410507883,-13.5650423075934,
114.142439305779)) ;
#182015 = CARTESIAN_POINT('Ctrl Pts',(-20.0186971571549,-13.8454220244642,
114.219462038445)) ;
#182016 = CARTESIAN_POINT('Ctrl Pts',(-20.0405222537569,-13.8159869229919,
114.285937759159)) ;
#182017 = CARTESIAN_POINT('Ctrl Pts',(-19.9667184235267,-13.8159870213789,
114.310168841019)) ;
#182018 = CARTESIAN_POINT('Ctrl Pts',(-19.8929145932964,-13.8159871197658,
114.334399922878)) ;
#182019 = CARTESIAN_POINT('Ctrl Pts',(-19.8710894966944,-13.8454222212381,
114.267924202164)) ;
#182020 = CARTESIAN_POINT('Ctrl Pts',(-19.8492644000924,-13.8748573227103,
114.20144848145)) ;
#182021 = CARTESIAN_POINT('Ctrl Pts',(-19.9230682303227,-13.8748572243234,
114.177217399591)) ;
#182022 = CARTESIAN_POINT('Ctrl Pts',(-19.9968720605529,-13.8748571259364,
114.152986317731)) ;
#182023 = CARTESIAN_POINT('Ctrl Pts',(-20.0186971571549,-13.8454220244642,
114.219462038445)) ;
#182024 = CARTESIAN_POINT('Ctrl Pts',(-20.0547596385372,-14.095635489283,
114.36479225159)) ;
#182025 = CARTESIAN_POINT('Ctrl Pts',(-20.0733651925667,-14.0486874017416,
114.421461765146)) ;
#182026 = CARTESIAN_POINT('Ctrl Pts',(-19.9995613695628,-14.0486874834364,
114.445692869016)) ;
#182027 = CARTESIAN_POINT('Ctrl Pts',(-19.9257575465589,-14.0486875651311,
114.469923972886)) ;
#182028 = CARTESIAN_POINT('Ctrl Pts',(-19.9071519925294,-14.0956356526725,
114.41325445933)) ;
#182029 = CARTESIAN_POINT('Ctrl Pts',(-19.8885464384999,-14.1425837402138,
114.356584945773)) ;
#182030 = CARTESIAN_POINT('Ctrl Pts',(-19.9623502615038,-14.1425836585191,
114.332353841904)) ;
#182031 = CARTESIAN_POINT('Ctrl Pts',(-20.0361540845077,-14.1425835768243,
114.308122738034)) ;
#182032 = CARTESIAN_POINT('Ctrl Pts',(-20.0547596385372,-14.095635489283,
114.36479225159)) ;
#182033 = CARTESIAN_POINT('Ctrl Pts',(-20.1097879472539,-14.2970558104585,
114.56784725279)) ;
#182034 = CARTESIAN_POINT('Ctrl Pts',(-20.1238459167263,-14.2359749683573,
114.6106655576)) ;
#182035 = CARTESIAN_POINT('Ctrl Pts',(-20.0500420989193,-14.2359750277231,
114.634896677298)) ;
#182036 = CARTESIAN_POINT('Ctrl Pts',(-19.9762382811122,-14.2359750870889,
114.659127796997)) ;
#182037 = CARTESIAN_POINT('Ctrl Pts',(-19.9621803116398,-14.2970559291901,
114.616309492187)) ;
#182038 = CARTESIAN_POINT('Ctrl Pts',(-19.9481223421674,-14.3581367712912,
114.573491187376)) ;
#182039 = CARTESIAN_POINT('Ctrl Pts',(-20.0219261599745,-14.3581367119255,
114.549260067678)) ;
#182040 = CARTESIAN_POINT('Ctrl Pts',(-20.0957299777816,-14.3581366525597,
114.525028947979)) ;
#182041 = CARTESIAN_POINT('Ctrl Pts',(-20.1097879472539,-14.2970558104585,
114.56784725279)) ;
#182042 = CARTESIAN_POINT('Ctrl Pts',(-20.1793472667708,-14.4359480747077,
114.815266815336)) ;
#182043 = CARTESIAN_POINT('Ctrl Pts',(-20.1878342866457,-14.3650783452255,
114.841116906637)) ;
#182044 = CARTESIAN_POINT('Ctrl Pts',(-20.114030471417,-14.3650783787337,
114.865348034189)) ;
#182045 = CARTESIAN_POINT('Ctrl Pts',(-20.0402266561884,-14.3650784122419,
114.889579161741)) ;
#182046 = CARTESIAN_POINT('Ctrl Pts',(-20.0317396363136,-14.4359481417242,
114.86372907044)) ;
#182047 = CARTESIAN_POINT('Ctrl Pts',(-20.0232526164387,-14.5068178712064,
114.837878979139)) ;
#182048 = CARTESIAN_POINT('Ctrl Pts',(-20.0970564316673,-14.5068178376981,
114.813647851587)) ;
#182049 = CARTESIAN_POINT('Ctrl Pts',(-20.1708602468959,-14.5068178041899,
114.789416724035)) ;
#182050 = CARTESIAN_POINT('Ctrl Pts',(-20.1793472667708,-14.4359480747077,
114.815266815336)) ;
#182051 = CARTESIAN_POINT('Ctrl Pts',(-20.2575026754292,-14.501304829004,
115.088848135438)) ;
#182052 = CARTESIAN_POINT('Ctrl Pts',(-20.2598105850978,-14.4257651981435,
115.095877654163)) ;
#182053 = CARTESIAN_POINT('Ctrl Pts',(-20.1860067697474,-14.4257652059426,
115.120108781345)) ;
#182054 = CARTESIAN_POINT('Ctrl Pts',(-20.112202954397,-14.4257652137418,
115.144339908526)) ;
#182055 = CARTESIAN_POINT('Ctrl Pts',(-20.1098950447284,-14.5013048446024,
115.1373103898)) ;
#182056 = CARTESIAN_POINT('Ctrl Pts',(-20.1075871350598,-14.576844475463,
115.130280871074)) ;
#182057 = CARTESIAN_POINT('Ctrl Pts',(-20.1813909504102,-14.5768444676638,
115.106049743893)) ;
#182058 = CARTESIAN_POINT('Ctrl Pts',(-20.2551947657606,-14.5768444598646,
115.081818616712)) ;
#182059 = CARTESIAN_POINT('Ctrl Pts',(-20.2575026754292,-14.501304829004,
115.088848135438)) ;
#182060 = CARTESIAN_POINT('Ctrl Pts',(-20.3373604074522,-14.4893139259723,
115.367374582084)) ;
#182061 = CARTESIAN_POINT('Ctrl Pts',(-20.3333659245991,-14.4144981524163,
115.355208030175)) ;
#182062 = CARTESIAN_POINT('Ctrl Pts',(-20.2595621073134,-14.4144981369881,
115.379439151462)) ;
#182063 = CARTESIAN_POINT('Ctrl Pts',(-20.1857582900276,-14.4144981215599,
115.403670272748)) ;
#182064 = CARTESIAN_POINT('Ctrl Pts',(-20.1897527728807,-14.4893138951159,
115.415836824657)) ;
#182065 = CARTESIAN_POINT('Ctrl Pts',(-20.1937472557339,-14.564129668672,
115.428003376567)) ;
#182066 = CARTESIAN_POINT('Ctrl Pts',(-20.2675510730196,-14.5641296841002,
115.40377225528)) ;
#182067 = CARTESIAN_POINT('Ctrl Pts',(-20.3413548903053,-14.5641296995284,
115.379541133994)) ;
#182068 = CARTESIAN_POINT('Ctrl Pts',(-20.3373604074522,-14.4893139259723,
115.367374582084)) ;
#182069 = CARTESIAN_POINT('Ctrl Pts',(-20.4135150495728,-14.4004454436412,
115.63486985746)) ;
#182070 = CARTESIAN_POINT('Ctrl Pts',(-20.4034620789504,-14.3317211347541,
115.604250129488)) ;
#182071 = CARTESIAN_POINT('Ctrl Pts',(-20.3296582572807,-14.331721100851,
115.628481237421)) ;
#182072 = CARTESIAN_POINT('Ctrl Pts',(-20.255854435611,-14.331721066948,115.652712345355)) ;
#182073 = CARTESIAN_POINT('Ctrl Pts',(-20.2659074062333,-14.4004453758351,
115.683332073327)) ;
#182074 = CARTESIAN_POINT('Ctrl Pts',(-20.2759603768557,-14.4691696847222,
115.713951801299)) ;
#182075 = CARTESIAN_POINT('Ctrl Pts',(-20.3497641985254,-14.4691697186253,
115.689720693366)) ;
#182076 = CARTESIAN_POINT('Ctrl Pts',(-20.4235680201952,-14.4691697525284,
115.665489585432)) ;
#182077 = CARTESIAN_POINT('Ctrl Pts',(-20.4135150495728,-14.4004454436412,
115.63486985746)) ;
#182078 = CARTESIAN_POINT('Ctrl Pts',(-20.4788768821726,-14.2418718140722,
115.86930035727)) ;
#182079 = CARTESIAN_POINT('Ctrl Pts',(-20.4635137429904,-14.1841154082224,
115.822506712786)) ;
#182080 = CARTESIAN_POINT('Ctrl Pts',(-20.3897099161486,-14.1841153614757,
115.846737804967)) ;
#182081 = CARTESIAN_POINT('Ctrl Pts',(-20.3159060893068,-14.1841153147289,
115.870968897147)) ;
#182082 = CARTESIAN_POINT('Ctrl Pts',(-20.3312692284891,-14.2418717205788,
115.917762541631)) ;
#182083 = CARTESIAN_POINT('Ctrl Pts',(-20.3466323676714,-14.2996281264286,
115.964556186114)) ;
#182084 = CARTESIAN_POINT('Ctrl Pts',(-20.4204361945131,-14.2996281731753,
115.940325093934)) ;
#182085 = CARTESIAN_POINT('Ctrl Pts',(-20.4942400213549,-14.299628219922,
115.916094001753)) ;
#182086 = CARTESIAN_POINT('Ctrl Pts',(-20.4788768821726,-14.2418718140722,
115.86930035727)) ;
#182087 = CARTESIAN_POINT('Ctrl Pts',(-20.5287019786929,-14.0233785235775,
116.056610441429)) ;
#182088 = CARTESIAN_POINT('Ctrl Pts',(-20.5091010771396,-13.9807896305814,
115.996909256697)) ;
#182089 = CARTESIAN_POINT('Ctrl Pts',(-20.4352972442419,-13.9807895787785,
116.021140330432)) ;
#182090 = CARTESIAN_POINT('Ctrl Pts',(-20.3614934113443,-13.9807895269757,
116.045371404168)) ;
#182091 = CARTESIAN_POINT('Ctrl Pts',(-20.3810943128976,-14.0233784199718,
116.105072588899)) ;
#182092 = CARTESIAN_POINT('Ctrl Pts',(-20.4006952144509,-14.0659673129679,
116.16477377363)) ;
#182093 = CARTESIAN_POINT('Ctrl Pts',(-20.4744990473485,-14.0659673647708,
116.140542699895)) ;
#182094 = CARTESIAN_POINT('Ctrl Pts',(-20.5483028802461,-14.0659674165736,
116.11631162616)) ;
#182095 = CARTESIAN_POINT('Ctrl Pts',(-20.5287019786929,-14.0233785235775,
116.056610441429)) ;
#182096 = CARTESIAN_POINT('Ctrl Pts',(-20.5581714230433,-13.7618917263419,
116.181832379666)) ;
#182097 = CARTESIAN_POINT('Ctrl Pts',(-20.5357493769413,-13.7374955038548,
116.113538443995)) ;
#182098 = CARTESIAN_POINT('Ctrl Pts',(-20.4619455385341,-13.7374954531261,
116.137769500949)) ;
#182099 = CARTESIAN_POINT('Ctrl Pts',(-20.3881417001269,-13.7374954023974,
116.162000557903)) ;
#182100 = CARTESIAN_POINT('Ctrl Pts',(-20.4105637462289,-13.7618916248845,
116.230294493574)) ;
#182101 = CARTESIAN_POINT('Ctrl Pts',(-20.4329857923308,-13.7862878473716,
116.298588429245)) ;
#182102 = CARTESIAN_POINT('Ctrl Pts',(-20.506789630738,-13.7862878981003,
116.274357372291)) ;
#182103 = CARTESIAN_POINT('Ctrl Pts',(-20.5805934691452,-13.786287948829,
116.250126315337)) ;
#182104 = CARTESIAN_POINT('Ctrl Pts',(-20.5581714230433,-13.7618917263419,
116.181832379666)) ;
#182105 = CARTESIAN_POINT('Ctrl Pts',(-20.5645519553757,-13.4754623735639,
116.236774706755)) ;
#182106 = CARTESIAN_POINT('Ctrl Pts',(-20.5409155733802,-13.471028133492,
116.164782100062)) ;
#182107 = CARTESIAN_POINT('Ctrl Pts',(-20.4671117304669,-13.4710280894286,
116.189013143291)) ;
#182108 = CARTESIAN_POINT('Ctrl Pts',(-20.3933078875535,-13.4710280453652,
116.213244186519)) ;
#182109 = CARTESIAN_POINT('Ctrl Pts',(-20.4169442695489,-13.4754622854371,
116.285236793213)) ;
#182110 = CARTESIAN_POINT('Ctrl Pts',(-20.4405806515443,-13.479896525509,
116.357229399907)) ;
#182111 = CARTESIAN_POINT('Ctrl Pts',(-20.5143844944577,-13.4798965695724,
116.332998356678)) ;
#182112 = CARTESIAN_POINT('Ctrl Pts',(-20.5881883373711,-13.4798966136358,
116.308767313449)) ;
#182113 = CARTESIAN_POINT('Ctrl Pts',(-20.5645519553757,-13.4754623735639,
116.236774706755)) ;
#182114 = CARTESIAN_POINT('Ctrl Pts',(-20.5467688213249,-13.1862230579374,
116.217949995558)) ;
#182115 = CARTESIAN_POINT('Ctrl Pts',(-20.523607060582,-13.2019774295457,
116.147403008764)) ;
#182116 = CARTESIAN_POINT('Ctrl Pts',(-20.4498032145121,-13.2019773939464,
116.171634042378)) ;
#182117 = CARTESIAN_POINT('Ctrl Pts',(-20.3759993684423,-13.2019773583471,
116.195865075993)) ;
#182118 = CARTESIAN_POINT('Ctrl Pts',(-20.3991611291852,-13.1862229867387,
116.266412062787)) ;
#182119 = CARTESIAN_POINT('Ctrl Pts',(-20.4223228899281,-13.1704686151304,
116.336959049582)) ;
#182120 = CARTESIAN_POINT('Ctrl Pts',(-20.4961267359979,-13.1704686507297,
116.312728015967)) ;
#182121 = CARTESIAN_POINT('Ctrl Pts',(-20.5699305820678,-13.170468686329,
116.288496982352)) ;
#182122 = CARTESIAN_POINT('Ctrl Pts',(-20.5467688213249,-13.1862230579374,
116.217949995558)) ;
#182123 = CARTESIAN_POINT('Ctrl Pts',(-20.5051147908571,-12.9121173454345,
116.12661145186)) ;
#182124 = CARTESIAN_POINT('Ctrl Pts',(-20.4840909773503,-12.9470346448942,
116.062576307566)) ;
#182125 = CARTESIAN_POINT('Ctrl Pts',(-20.4102871297331,-12.947034620835,
116.086807336468)) ;
#182126 = CARTESIAN_POINT('Ctrl Pts',(-20.3364832821159,-12.9470345967758,
116.111038365369)) ;
#182127 = CARTESIAN_POINT('Ctrl Pts',(-20.3575070956226,-12.9121172973162,
116.175073509663)) ;
#182128 = CARTESIAN_POINT('Ctrl Pts',(-20.3785309091293,-12.8771999978565,
116.239108653958)) ;
#182129 = CARTESIAN_POINT('Ctrl Pts',(-20.4523347567466,-12.8772000219157,
116.214877625056)) ;
#182130 = CARTESIAN_POINT('Ctrl Pts',(-20.5261386043638,-12.8772000459749,
116.190646596154)) ;
#182131 = CARTESIAN_POINT('Ctrl Pts',(-20.5051147908571,-12.9121173454345,
116.12661145186)) ;
#182132 = CARTESIAN_POINT('Ctrl Pts',(-20.4420769531017,-12.6748571224349,
115.970037261179)) ;
#182133 = CARTESIAN_POINT('Ctrl Pts',(-20.4246897099179,-12.7263936809792,
115.917078523479)) ;
#182134 = CARTESIAN_POINT('Ctrl Pts',(-20.350885862107,-12.7263936670357,
115.941309551791)) ;
#182135 = CARTESIAN_POINT('Ctrl Pts',(-20.2770820142961,-12.7263936530922,
115.965540580103)) ;
#182136 = CARTESIAN_POINT('Ctrl Pts',(-20.2944692574799,-12.6748570945479,
116.018499317803)) ;
#182137 = CARTESIAN_POINT('Ctrl Pts',(-20.3118565006636,-12.6233205360036,
116.071458055503)) ;
#182138 = CARTESIAN_POINT('Ctrl Pts',(-20.3856603484746,-12.6233205499471,
116.047227027191)) ;
#182139 = CARTESIAN_POINT('Ctrl Pts',(-20.4594641962855,-12.6233205638906,
116.02299599888)) ;
#182140 = CARTESIAN_POINT('Ctrl Pts',(-20.4420769531017,-12.6748571224349,
115.970037261179)) ;
#182141 = CARTESIAN_POINT('Ctrl Pts',(-20.3606399883835,-12.4898752939566,
115.757680794649)) ;
#182142 = CARTESIAN_POINT('Ctrl Pts',(-20.3481742578633,-12.5544068109691,
115.71971219061)) ;
#182143 = CARTESIAN_POINT('Ctrl Pts',(-20.274370411419,-12.5544068057079,
115.743943223084)) ;
#182144 = CARTESIAN_POINT('Ctrl Pts',(-20.2005665649747,-12.5544068004467,
115.768174255558)) ;
#182145 = CARTESIAN_POINT('Ctrl Pts',(-20.2130322954949,-12.4898752834342,
115.806142859598)) ;
#182146 = CARTESIAN_POINT('Ctrl Pts',(-20.2254980260151,-12.4253437664217,
115.844111463637)) ;
#182147 = CARTESIAN_POINT('Ctrl Pts',(-20.2993018724594,-12.4253437716829,
115.819880431163)) ;
#182148 = CARTESIAN_POINT('Ctrl Pts',(-20.3731057189037,-12.4253437769441,
115.795649398689)) ;
#182149 = CARTESIAN_POINT('Ctrl Pts',(-20.3606399883835,-12.4898752939566,
115.757680794649)) ;
#182150 = CARTESIAN_POINT('Ctrl Pts',(-20.267669228754,-12.3730682967797,
115.5097223699)) ;
#182151 = CARTESIAN_POINT('Ctrl Pts',(-20.2609477177173,-12.4458523869168,
115.489249731667)) ;
#182152 = CARTESIAN_POINT('Ctrl Pts',(-20.1871438723082,-12.4458523855329,
115.513480767294)) ;
#182153 = CARTESIAN_POINT('Ctrl Pts',(-20.113340026899,-12.445852384149,115.537711802922)) ;
#182154 = CARTESIAN_POINT('Ctrl Pts',(-20.1200615379358,-12.3730682940119,
115.558184441155)) ;
#182155 = CARTESIAN_POINT('Ctrl Pts',(-20.1267830489725,-12.3002842038747,
115.578657079388)) ;
#182156 = CARTESIAN_POINT('Ctrl Pts',(-20.2005868943816,-12.3002842052586,
115.55442604376)) ;
#182157 = CARTESIAN_POINT('Ctrl Pts',(-20.2743907397907,-12.3002842066425,
115.530195008133)) ;
#182158 = CARTESIAN_POINT('Ctrl Pts',(-20.267669228754,-12.3730682967797,
115.5097223699)) ;
#182159 = CARTESIAN_POINT('Ctrl Pts',(-20.166688706548,-12.330125354393,115.237846370994)) ;
#182160 = CARTESIAN_POINT('Ctrl Pts',(-20.1662696956355,-12.4060180175289,
115.236570131351)) ;
#182161 = CARTESIAN_POINT('Ctrl Pts',(-20.092465852039,-12.4060180179283,
115.260801172499)) ;
#182162 = CARTESIAN_POINT('Ctrl Pts',(-20.0186620084424,-12.4060180183277,
115.285032213647)) ;
#182163 = CARTESIAN_POINT('Ctrl Pts',(-20.0190810193549,-12.3301253551918,
115.286308453291)) ;
#182164 = CARTESIAN_POINT('Ctrl Pts',(-20.0195000302674,-12.2542326920559,
115.287584692934)) ;
#182165 = CARTESIAN_POINT('Ctrl Pts',(-20.0933038738639,-12.2542326916565,
115.263353651786)) ;
#182166 = CARTESIAN_POINT('Ctrl Pts',(-20.1671077174604,-12.2542326912571,
115.239122610638)) ;
#182167 = CARTESIAN_POINT('Ctrl Pts',(-20.166688706548,-12.330125354393,115.237846370994)) ;
#182168 = CARTESIAN_POINT('Ctrl Pts',(-20.0667473533349,-12.3650026478225,
114.968634787347)) ;
#182169 = CARTESIAN_POINT('Ctrl Pts',(-20.0725778668182,-12.4385726507877,
114.986393590701)) ;
#182170 = CARTESIAN_POINT('Ctrl Pts',(-19.9987740239603,-12.4385726504867,
115.010624634099)) ;
#182171 = CARTESIAN_POINT('Ctrl Pts',(-19.9249701811023,-12.4385726501857,
115.034855677496)) ;
#182172 = CARTESIAN_POINT('Ctrl Pts',(-19.9191396676191,-12.3650026472205,
115.017096874142)) ;
#182173 = CARTESIAN_POINT('Ctrl Pts',(-19.9133091541358,-12.2914326442552,
114.999338070788)) ;
#182174 = CARTESIAN_POINT('Ctrl Pts',(-19.9871129969937,-12.2914326445563,
114.97510702739)) ;
#182175 = CARTESIAN_POINT('Ctrl Pts',(-20.0609168398517,-12.2914326448573,
114.950875983992)) ;
#182176 = CARTESIAN_POINT('Ctrl Pts',(-20.0667473533349,-12.3650026478225,
114.968634787347)) ;
#182177 = CARTESIAN_POINT('Ctrl Pts',(-19.9714448335891,-12.4764750890778,
114.714120708034)) ;
#182178 = CARTESIAN_POINT('Ctrl Pts',(-19.9831991431023,-12.5423709931459,
114.749922438328)) ;
#182179 = CARTESIAN_POINT('Ctrl Pts',(-19.9093953006452,-12.5423709914641,
114.774153482947)) ;
#182180 = CARTESIAN_POINT('Ctrl Pts',(-19.8355914581881,-12.5423709897823,
114.798384527565)) ;
#182181 = CARTESIAN_POINT('Ctrl Pts',(-19.8238371486749,-12.4764750857142,
114.762582797271)) ;
#182182 = CARTESIAN_POINT('Ctrl Pts',(-19.8120828391616,-12.410579181646,
114.726781066978)) ;
#182183 = CARTESIAN_POINT('Ctrl Pts',(-19.8858866816187,-12.4105791833278,
114.702550022359)) ;
#182184 = CARTESIAN_POINT('Ctrl Pts',(-19.9596905240758,-12.4105791850096,
114.67831897774)) ;
#182185 = CARTESIAN_POINT('Ctrl Pts',(-19.9714448335891,-12.4764750890778,
114.714120708034)) ;
#182186 = CARTESIAN_POINT('Ctrl Pts',(-19.8896127307638,-12.6535586984017,
114.500104289073)) ;
#182187 = CARTESIAN_POINT('Ctrl Pts',(-19.9063692751628,-12.7071860625279,
114.551142019704)) ;
#182188 = CARTESIAN_POINT('Ctrl Pts',(-19.8325654322624,-12.7071860605199,
114.575373062973)) ;
#182189 = CARTESIAN_POINT('Ctrl Pts',(-19.758761589362,-12.7071860585118,
114.599604106241)) ;
#182190 = CARTESIAN_POINT('Ctrl Pts',(-19.742005044963,-12.6535586943856,
114.54856637561)) ;
#182191 = CARTESIAN_POINT('Ctrl Pts',(-19.7252485005639,-12.5999313302593,
114.497528644979)) ;
#182192 = CARTESIAN_POINT('Ctrl Pts',(-19.7990523434643,-12.5999313322674,
114.473297601711)) ;
#182193 = CARTESIAN_POINT('Ctrl Pts',(-19.8728561863647,-12.5999313342754,
114.449066558443)) ;
#182194 = CARTESIAN_POINT('Ctrl Pts',(-19.8896127307638,-12.6535586984017,
114.500104289073)) ;
#182195 = CARTESIAN_POINT('Ctrl Pts',(-19.8242138693162,-12.8875907025722,
114.33656955619)) ;
#182196 = CARTESIAN_POINT('Ctrl Pts',(-19.8448239027325,-12.9249550568961,
114.399344392539)) ;
#182197 = CARTESIAN_POINT('Ctrl Pts',(-19.7710200590923,-12.9249550576415,
114.423575433555)) ;
#182198 = CARTESIAN_POINT('Ctrl Pts',(-19.6972162154521,-12.9249550583868,
114.44780647457)) ;
#182199 = CARTESIAN_POINT('Ctrl Pts',(-19.6766061820359,-12.887590704063,
114.385031638221)) ;
#182200 = CARTESIAN_POINT('Ctrl Pts',(-19.6559961486197,-12.8502263497391,
114.322256801871)) ;
#182201 = CARTESIAN_POINT('Ctrl Pts',(-19.7297999922599,-12.8502263489938,
114.298025760856)) ;
#182202 = CARTESIAN_POINT('Ctrl Pts',(-19.8036038359,-12.8502263482484,114.273794719841)) ;
#182203 = CARTESIAN_POINT('Ctrl Pts',(-19.8242138693162,-12.8875907025722,
114.33656955619)) ;
#182204 = CARTESIAN_POINT('Ctrl Pts',(-19.7806786916706,-13.1564738506933,
114.239166113218)) ;
#182205 = CARTESIAN_POINT('Ctrl Pts',(-19.8036300452104,-13.1751180004759,
114.30907223283)) ;
#182206 = CARTESIAN_POINT('Ctrl Pts',(-19.7298262013386,-13.1751180045343,
114.333303273139)) ;
#182207 = CARTESIAN_POINT('Ctrl Pts',(-19.6560223574667,-13.1751180085928,
114.357534313449)) ;
#182208 = CARTESIAN_POINT('Ctrl Pts',(-19.633071003927,-13.1564738588101,
114.287628193837)) ;
#182209 = CARTESIAN_POINT('Ctrl Pts',(-19.6101196503872,-13.1378297090275,
114.217722074225)) ;
#182210 = CARTESIAN_POINT('Ctrl Pts',(-19.6839234942591,-13.1378297049691,
114.193491033915)) ;
#182211 = CARTESIAN_POINT('Ctrl Pts',(-19.7577273381309,-13.1378297009107,
114.169259993606)) ;
#182212 = CARTESIAN_POINT('Ctrl Pts',(-19.7806786916706,-13.1564738506933,
114.239166113218)) ;
#182213 = CARTESIAN_POINT('Ctrl Pts',(-19.7602296026469,-13.4476180482474,
114.212556713675)) ;
#182214 = CARTESIAN_POINT('Ctrl Pts',(-19.7839041995415,-13.4459601626287,
114.284665715712)) ;
#182215 = CARTESIAN_POINT('Ctrl Pts',(-19.7101003560251,-13.4459601740975,
114.308896757104)) ;
#182216 = CARTESIAN_POINT('Ctrl Pts',(-19.6362965125087,-13.4459601855664,
114.333127798496)) ;
#182217 = CARTESIAN_POINT('Ctrl Pts',(-19.6126219156141,-13.4476180711851,
114.261018796459)) ;
#182218 = CARTESIAN_POINT('Ctrl Pts',(-19.5889473187195,-13.4492759568038,
114.188909794422)) ;
#182219 = CARTESIAN_POINT('Ctrl Pts',(-19.6627511622359,-13.4492759453349,
114.16467875303)) ;
#182220 = CARTESIAN_POINT('Ctrl Pts',(-19.7365550057523,-13.4492759338661,
114.140447711637)) ;
#182221 = CARTESIAN_POINT('Ctrl Pts',(-19.7602296026469,-13.4476180482474,
114.212556713675)) ;
#182222 = CARTESIAN_POINT('Ctrl Pts',(-19.7643490688689,-13.7346448783816,
114.260518004658)) ;
#182223 = CARTESIAN_POINT('Ctrl Pts',(-19.7870375076896,-13.7129435340765,
114.329623328187)) ;
#182224 = CARTESIAN_POINT('Ctrl Pts',(-19.713233665749,-13.7129435517169,
114.353854374379)) ;
#182225 = CARTESIAN_POINT('Ctrl Pts',(-19.6394298238083,-13.7129435693573,
114.378085420571)) ;
#182226 = CARTESIAN_POINT('Ctrl Pts',(-19.6167413849876,-13.7346449136625,
114.308980097041)) ;
#182227 = CARTESIAN_POINT('Ctrl Pts',(-19.5940529461669,-13.7563462579677,
114.239874773512)) ;
#182228 = CARTESIAN_POINT('Ctrl Pts',(-19.6678567881075,-13.7563462403272,
114.21564372732)) ;
#182229 = CARTESIAN_POINT('Ctrl Pts',(-19.7416606300482,-13.7563462226868,
114.191412681128)) ;
#182230 = CARTESIAN_POINT('Ctrl Pts',(-19.7643490688689,-13.7346448783816,
114.260518004658)) ;
#182231 = CARTESIAN_POINT('Ctrl Pts',(-19.7916546783398,-13.9993799399049,
114.37915348673)) ;
#182232 = CARTESIAN_POINT('Ctrl Pts',(-19.811735534808,-13.9591628378215,
114.440316534995)) ;
#182233 = CARTESIAN_POINT('Ctrl Pts',(-19.7379316955588,-13.9591628601971,
114.464547589384)) ;
#182234 = CARTESIAN_POINT('Ctrl Pts',(-19.6641278563097,-13.9591628825727,
114.488778643774)) ;
#182235 = CARTESIAN_POINT('Ctrl Pts',(-19.6440469998415,-13.9993799846561,
114.427615595509)) ;
#182236 = CARTESIAN_POINT('Ctrl Pts',(-19.6239661433733,-14.0395970867396,
114.366452547245)) ;
#182237 = CARTESIAN_POINT('Ctrl Pts',(-19.6977699826225,-14.0395970643639,
114.342221492855)) ;
#182238 = CARTESIAN_POINT('Ctrl Pts',(-19.7715738218716,-14.0395970419883,
114.317990438466)) ;
#182239 = CARTESIAN_POINT('Ctrl Pts',(-19.7916546783398,-13.9993799399049,
114.37915348673)) ;
#182240 = CARTESIAN_POINT('Ctrl Pts',(-19.8393939276307,-14.2219559568416,
114.559939768172)) ;
#182241 = CARTESIAN_POINT('Ctrl Pts',(-19.8554384541888,-14.1661403968853,
114.608808806644)) ;
#182242 = CARTESIAN_POINT('Ctrl Pts',(-19.7816346183794,-14.1661404199882,
114.63303987151)) ;
#182243 = CARTESIAN_POINT('Ctrl Pts',(-19.7078307825699,-14.166140443091,
114.657270936377)) ;
#182244 = CARTESIAN_POINT('Ctrl Pts',(-19.6917862560118,-14.2219560030472,
114.608401897904)) ;
#182245 = CARTESIAN_POINT('Ctrl Pts',(-19.6757417294536,-14.2777715630035,
114.559532859432)) ;
#182246 = CARTESIAN_POINT('Ctrl Pts',(-19.7495455652631,-14.2777715399007,
114.535301794566)) ;
#182247 = CARTESIAN_POINT('Ctrl Pts',(-19.8233494010725,-14.2777715167979,
114.511070729699)) ;
#182248 = CARTESIAN_POINT('Ctrl Pts',(-19.8393939276307,-14.2219559568416,
114.559939768172)) ;
#182249 = CARTESIAN_POINT('Ctrl Pts',(-19.9035549276073,-14.3877271051732,
114.790823935463)) ;
#182250 = CARTESIAN_POINT('Ctrl Pts',(-19.9144091659851,-14.3202567503196,
114.823884193423)) ;
#182251 = CARTESIAN_POINT('Ctrl Pts',(-19.8406053341715,-14.3202567702551,
114.84811527046)) ;
#182252 = CARTESIAN_POINT('Ctrl Pts',(-19.7668015023578,-14.3202567901906,
114.872346347496)) ;
#182253 = CARTESIAN_POINT('Ctrl Pts',(-19.75594726398,-14.3877271450442,114.839286089537)) ;
#182254 = CARTESIAN_POINT('Ctrl Pts',(-19.7450930256021,-14.4551974998978,
114.806225831578)) ;
#182255 = CARTESIAN_POINT('Ctrl Pts',(-19.8188968574157,-14.4551974799623,
114.781994754541)) ;
#182256 = CARTESIAN_POINT('Ctrl Pts',(-19.8927006892294,-14.4551974600268,
114.757763677504)) ;
#182257 = CARTESIAN_POINT('Ctrl Pts',(-19.9035549276073,-14.3877271051732,
114.790823935463)) ;
#182258 = CARTESIAN_POINT('Ctrl Pts',(-19.9791956729631,-14.4840522417127,
115.05686055136)) ;
#182259 = CARTESIAN_POINT('Ctrl Pts',(-19.9840468444247,-14.4097585017527,
115.07163643588)) ;
#182260 = CARTESIAN_POINT('Ctrl Pts',(-19.9102430170675,-14.4097585129656,
115.095867526491)) ;
#182261 = CARTESIAN_POINT('Ctrl Pts',(-19.8364391897103,-14.4097585241785,
115.120098617101)) ;
#182262 = CARTESIAN_POINT('Ctrl Pts',(-19.8315880182487,-14.4840522641385,
115.105322732581)) ;
#182263 = CARTESIAN_POINT('Ctrl Pts',(-19.8267368467871,-14.5583460040984,
115.090546848061)) ;
#182264 = CARTESIAN_POINT('Ctrl Pts',(-19.9005406741443,-14.5583459928856,
115.06631575745)) ;
#182265 = CARTESIAN_POINT('Ctrl Pts',(-19.9743445015015,-14.5583459816727,
115.04208466684)) ;
#182266 = CARTESIAN_POINT('Ctrl Pts',(-19.9791956729631,-14.4840522417127,
115.05686055136)) ;
#182267 = CARTESIAN_POINT('Ctrl Pts',(-20.0588167420593,-14.5035551456864,
115.334617178698)) ;
#182268 = CARTESIAN_POINT('Ctrl Pts',(-20.057386595992,-14.4277930448145,
115.330261183388)) ;
#182269 = CARTESIAN_POINT('Ctrl Pts',(-19.9835827710018,-14.4277930415592,
115.354492281207)) ;
#182270 = CARTESIAN_POINT('Ctrl Pts',(-19.9097789460115,-14.427793038304,
115.378723379027)) ;
#182271 = CARTESIAN_POINT('Ctrl Pts',(-19.9112090920788,-14.503555139176,
115.383079374337)) ;
#182272 = CARTESIAN_POINT('Ctrl Pts',(-19.912639238146,-14.579317240048,115.387435369648)) ;
#182273 = CARTESIAN_POINT('Ctrl Pts',(-19.9864430631363,-14.5793172433032,
115.363204271828)) ;
#182274 = CARTESIAN_POINT('Ctrl Pts',(-20.0602468881266,-14.5793172465584,
115.338973174008)) ;
#182275 = CARTESIAN_POINT('Ctrl Pts',(-20.0588167420593,-14.5035551456864,
115.334617178698)) ;
#182276 = CARTESIAN_POINT('Ctrl Pts',(-20.1375552337769,-14.4455933724693,
115.610012047624)) ;
#182277 = CARTESIAN_POINT('Ctrl Pts',(-20.1298896565059,-14.3737681183539,
115.58666393477)) ;
#182278 = CARTESIAN_POINT('Ctrl Pts',(-20.0560858333493,-14.3737680965987,
115.610895038174)) ;
#182279 = CARTESIAN_POINT('Ctrl Pts',(-19.9822820101926,-14.3737680748436,
115.635126141579)) ;
#182280 = CARTESIAN_POINT('Ctrl Pts',(-19.9899475874636,-14.445593328959,
115.658474254434)) ;
#182281 = CARTESIAN_POINT('Ctrl Pts',(-19.9976131647346,-14.5174185830743,
115.681822367288)) ;
#182282 = CARTESIAN_POINT('Ctrl Pts',(-20.0714169878912,-14.5174186048295,
115.657591263883)) ;
#182283 = CARTESIAN_POINT('Ctrl Pts',(-20.1452208110478,-14.5174186265847,
115.633360160479)) ;
#182284 = CARTESIAN_POINT('Ctrl Pts',(-20.1375552337769,-14.4455933724693,
115.610012047624)) ;
#182285 = CARTESIAN_POINT('Ctrl Pts',(-20.2080701569904,-14.3137077173971,
115.860269168483)) ;
#182286 = CARTESIAN_POINT('Ctrl Pts',(-20.1947361462872,-14.2509862906075,
115.819655921839)) ;
#182287 = CARTESIAN_POINT('Ctrl Pts',(-20.1209323226071,-14.2509862477117,
115.843887023649)) ;
#182288 = CARTESIAN_POINT('Ctrl Pts',(-20.0471284989271,-14.2509862048158,
115.86811812546)) ;
#182289 = CARTESIAN_POINT('Ctrl Pts',(-20.0604625096304,-14.3137076316054,
115.908731372104)) ;
#182290 = CARTESIAN_POINT('Ctrl Pts',(-20.0737965203336,-14.3764290583951,
115.949344618748)) ;
#182291 = CARTESIAN_POINT('Ctrl Pts',(-20.1476003440137,-14.3764291012909,
115.925113516938)) ;
#182292 = CARTESIAN_POINT('Ctrl Pts',(-20.2214041676937,-14.3764291441867,
115.900882415128)) ;
#182293 = CARTESIAN_POINT('Ctrl Pts',(-20.2080701569904,-14.3137077173971,
115.860269168483)) ;
#182294 = CARTESIAN_POINT('Ctrl Pts',(-20.2646911851614,-14.118290994482,
116.068126903514)) ;
#182295 = CARTESIAN_POINT('Ctrl Pts',(-20.2466522852371,-14.0691221426053,
116.013183323304)) ;
#182296 = CARTESIAN_POINT('Ctrl Pts',(-20.1728484586584,-14.0691220793387,
116.037414416285)) ;
#182297 = CARTESIAN_POINT('Ctrl Pts',(-20.0990446320796,-14.0691220160722,
116.061645509267)) ;
#182298 = CARTESIAN_POINT('Ctrl Pts',(-20.1170835320039,-14.1182908679489,
116.116589089477)) ;
#182299 = CARTESIAN_POINT('Ctrl Pts',(-20.1351224319283,-14.1674597198256,
116.171532669688)) ;
#182300 = CARTESIAN_POINT('Ctrl Pts',(-20.208926258507,-14.1674597830921,
116.147301576706)) ;
#182301 = CARTESIAN_POINT('Ctrl Pts',(-20.2827300850857,-14.1674598463587,
116.123070483725)) ;
#182302 = CARTESIAN_POINT('Ctrl Pts',(-20.2646911851614,-14.118290994482,
116.068126903514)) ;
#182303 = CARTESIAN_POINT('Ctrl Pts',(-20.3028224443455,-13.8721339097932,
116.21976440383)) ;
#182304 = CARTESIAN_POINT('Ctrl Pts',(-20.2813606322499,-13.840079359465,
116.1543951853)) ;
#182305 = CARTESIAN_POINT('Ctrl Pts',(-20.2075568006751,-13.8400792780125,
116.178626263064)) ;
#182306 = CARTESIAN_POINT('Ctrl Pts',(-20.1337529691003,-13.8400791965599,
116.202857340829)) ;
#182307 = CARTESIAN_POINT('Ctrl Pts',(-20.1552147811959,-13.872133746888,
116.268226559358)) ;
#182308 = CARTESIAN_POINT('Ctrl Pts',(-20.1766765932915,-13.9041882972162,
116.333595777888)) ;
#182309 = CARTESIAN_POINT('Ctrl Pts',(-20.2504804248663,-13.9041883786687,
116.309364700123)) ;
#182310 = CARTESIAN_POINT('Ctrl Pts',(-20.3242842564411,-13.9041884601213,
116.285133622359)) ;
#182311 = CARTESIAN_POINT('Ctrl Pts',(-20.3028224443455,-13.8721339097932,
116.21976440383)) ;
#182312 = CARTESIAN_POINT('Ctrl Pts',(-20.3188675383437,-13.5943341067766,
116.304015063102)) ;
#182313 = CARTESIAN_POINT('Ctrl Pts',(-20.2955222534172,-13.5816279445403,
116.232909090126)) ;
#182314 = CARTESIAN_POINT('Ctrl Pts',(-20.2217184149583,-13.5816278507647,
116.257140146922)) ;
#182315 = CARTESIAN_POINT('Ctrl Pts',(-20.1479145764994,-13.5816277569891,
116.281371203719)) ;
#182316 = CARTESIAN_POINT('Ctrl Pts',(-20.1712598614258,-13.5943339192254,
116.352477176694)) ;
#182317 = CARTESIAN_POINT('Ctrl Pts',(-20.1946051463523,-13.6070400814617,
116.42358314967)) ;
#182318 = CARTESIAN_POINT('Ctrl Pts',(-20.2684089848112,-13.6070401752373,
116.399352092874)) ;
#182319 = CARTESIAN_POINT('Ctrl Pts',(-20.3422128232701,-13.6070402690129,
116.375121036078)) ;
#182320 = CARTESIAN_POINT('Ctrl Pts',(-20.3188675383437,-13.5943341067766,
116.304015063102)) ;
#182321 = CARTESIAN_POINT('Ctrl Pts',(-20.310817084727,-13.3016132059809,
116.315163697483)) ;
#182322 = CARTESIAN_POINT('Ctrl Pts',(-20.2872614887352,-13.309324862532,
116.243417150824)) ;
#182323 = CARTESIAN_POINT('Ctrl Pts',(-20.2134576420664,-13.3093247622356,
116.267648182615)) ;
#182324 = CARTESIAN_POINT('Ctrl Pts',(-20.1396537953975,-13.3093246619392,
116.291879214405)) ;
#182325 = CARTESIAN_POINT('Ctrl Pts',(-20.1632093913893,-13.3016130053881,
116.363625761064)) ;
#182326 = CARTESIAN_POINT('Ctrl Pts',(-20.1867649873811,-13.293901348837,
116.435372307722)) ;
#182327 = CARTESIAN_POINT('Ctrl Pts',(-20.2605688340499,-13.2939014491334,
116.411141275932)) ;
#182328 = CARTESIAN_POINT('Ctrl Pts',(-20.3343726807187,-13.2939015494298,
116.386910244142)) ;
#182329 = CARTESIAN_POINT('Ctrl Pts',(-20.310817084727,-13.3016132059809,
116.315163697483)) ;
#182330 = CARTESIAN_POINT('Ctrl Pts',(-20.2787910861107,-13.0203974601351,
116.252886906067)) ;
#182331 = CARTESIAN_POINT('Ctrl Pts',(-20.2567073240818,-13.0477539673653,
116.185623328126)) ;
#182332 = CARTESIAN_POINT('Ctrl Pts',(-20.182903468911,-13.0477538708474,
116.209854334021)) ;
#182333 = CARTESIAN_POINT('Ctrl Pts',(-20.1090996137403,-13.0477537743296,
116.234085339916)) ;
#182334 = CARTESIAN_POINT('Ctrl Pts',(-20.1311833757692,-13.0203972670994,
116.301348917857)) ;
#182335 = CARTESIAN_POINT('Ctrl Pts',(-20.1532671377981,-12.9930407598692,
116.368612495798)) ;
#182336 = CARTESIAN_POINT('Ctrl Pts',(-20.2270709929689,-12.9930408563871,
116.344381489903)) ;
#182337 = CARTESIAN_POINT('Ctrl Pts',(-20.3008748481397,-12.9930409529049,
116.320150484008)) ;
#182338 = CARTESIAN_POINT('Ctrl Pts',(-20.2787910861107,-13.0203974601351,
116.252886906067)) ;
#182339 = CARTESIAN_POINT('Ctrl Pts',(-20.2240804356435,-12.7657619407627,
116.121738912419)) ;
#182340 = CARTESIAN_POINT('Ctrl Pts',(-20.2050494897071,-12.8109362194434,
116.06377371967)) ;
#182341 = CARTESIAN_POINT('Ctrl Pts',(-20.1312456264214,-12.8109361340697,
116.088004700848)) ;
#182342 = CARTESIAN_POINT('Ctrl Pts',(-20.0574417631357,-12.810936048696,
116.112235682026)) ;
#182343 = CARTESIAN_POINT('Ctrl Pts',(-20.076472709072,-12.7657617700153,
116.170200874775)) ;
#182344 = CARTESIAN_POINT('Ctrl Pts',(-20.0955036550083,-12.7205874913346,
116.228166067524)) ;
#182345 = CARTESIAN_POINT('Ctrl Pts',(-20.1693075182941,-12.7205875767083,
116.203935086346)) ;
#182346 = CARTESIAN_POINT('Ctrl Pts',(-20.2431113815798,-12.720587662082,
116.179704105168)) ;
#182347 = CARTESIAN_POINT('Ctrl Pts',(-20.2240804356435,-12.7657619407627,
116.121738912419)) ;
#182348 = CARTESIAN_POINT('Ctrl Pts',(-20.149613612166,-12.5577255499837,
115.930492489718)) ;
#182349 = CARTESIAN_POINT('Ctrl Pts',(-20.1350175403921,-12.6174909098253,
115.886035208073)) ;
#182350 = CARTESIAN_POINT('Ctrl Pts',(-20.0612136703226,-12.6174908436088,
115.910266168589)) ;
#182351 = CARTESIAN_POINT('Ctrl Pts',(-19.9874098002531,-12.6174907773923,
115.934497129104)) ;
#182352 = CARTESIAN_POINT('Ctrl Pts',(-20.002005872027,-12.5577254175507,
115.97895441075)) ;
#182353 = CARTESIAN_POINT('Ctrl Pts',(-20.0166019438008,-12.497960057709,
116.023411692395)) ;
#182354 = CARTESIAN_POINT('Ctrl Pts',(-20.0904058138703,-12.4979601239256,
115.999180731879)) ;
#182355 = CARTESIAN_POINT('Ctrl Pts',(-20.1642096839398,-12.4979601901421,
115.974949771364)) ;
#182356 = CARTESIAN_POINT('Ctrl Pts',(-20.149613612166,-12.5577255499837,
115.930492489718)) ;
#182357 = CARTESIAN_POINT('Ctrl Pts',(-20.0607208453583,-12.4120606642955,
115.695117936638)) ;
#182358 = CARTESIAN_POINT('Ctrl Pts',(-20.0515773677667,-12.4820840248362,
115.667268377092)) ;
#182359 = CARTESIAN_POINT('Ctrl Pts',(-19.9777734930595,-12.482083983576,
115.691499323482)) ;
#182360 = CARTESIAN_POINT('Ctrl Pts',(-19.9039696183523,-12.4820839423157,
115.715730269872)) ;
#182361 = CARTESIAN_POINT('Ctrl Pts',(-19.913113095944,-12.412060581775,115.743579829418)) ;
#182362 = CARTESIAN_POINT('Ctrl Pts',(-19.9222565735356,-12.3420372212343,
115.771429388964)) ;
#182363 = CARTESIAN_POINT('Ctrl Pts',(-19.9960604482428,-12.3420372624946,
115.747198442574)) ;
#182364 = CARTESIAN_POINT('Ctrl Pts',(-20.06986432295,-12.3420373037548,115.722967496184)) ;
#182365 = CARTESIAN_POINT('Ctrl Pts',(-20.0607208453583,-12.4120606642955,
115.695117936638)) ;
#182366 = CARTESIAN_POINT('Ctrl Pts',(-19.9618159399851,-12.3380220880362,
115.429525652929)) ;
#182367 = CARTESIAN_POINT('Ctrl Pts',(-19.9588261722604,-12.4133190427032,
115.420419300761)) ;
#182368 = CARTESIAN_POINT('Ctrl Pts',(-19.8850222955982,-12.4133190298849,
115.444650241197)) ;
#182369 = CARTESIAN_POINT('Ctrl Pts',(-19.811218418936,-12.4133190170666,
115.468881181632)) ;
#182370 = CARTESIAN_POINT('Ctrl Pts',(-19.8142081866607,-12.3380220623996,
115.477987533799)) ;
#182371 = CARTESIAN_POINT('Ctrl Pts',(-19.8171979543855,-12.2627251077326,
115.487093885967)) ;
#182372 = CARTESIAN_POINT('Ctrl Pts',(-19.8910018310476,-12.2627251205509,
115.462862945531)) ;
#182373 = CARTESIAN_POINT('Ctrl Pts',(-19.9648057077098,-12.2627251333692,
115.438632005096)) ;
#182374 = CARTESIAN_POINT('Ctrl Pts',(-19.9618159399851,-12.3380220880362,
115.429525652929)) ;
#182375 = CARTESIAN_POINT('Ctrl Pts',(-19.8611741252131,-12.3416277493325,
115.158205582033)) ;
#182376 = CARTESIAN_POINT('Ctrl Pts',(-19.8644777699935,-12.4167843477481,
115.168267948947)) ;
#182377 = CARTESIAN_POINT('Ctrl Pts',(-19.7906738939163,-12.4167843633384,
115.192498891164)) ;
#182378 = CARTESIAN_POINT('Ctrl Pts',(-19.7168700178391,-12.4167843789286,
115.216729833381)) ;
#182379 = CARTESIAN_POINT('Ctrl Pts',(-19.7135663730587,-12.3416277805131,
115.206667466468)) ;
#182380 = CARTESIAN_POINT('Ctrl Pts',(-19.7102627282783,-12.2664711820975,
115.196605099554)) ;
#182381 = CARTESIAN_POINT('Ctrl Pts',(-19.7840666043555,-12.2664711665072,
115.172374157337)) ;
#182382 = CARTESIAN_POINT('Ctrl Pts',(-19.8578704804326,-12.266471150917,
115.14814321512)) ;
#182383 = CARTESIAN_POINT('Ctrl Pts',(-19.8611741252131,-12.3416277493325,
115.158205582033)) ;
#182384 = CARTESIAN_POINT('Ctrl Pts',(-19.7631652821149,-12.4221117178776,
114.895226151352)) ;
#182385 = CARTESIAN_POINT('Ctrl Pts',(-19.7725811313252,-12.4917616411482,
114.923905306819)) ;
#182386 = CARTESIAN_POINT('Ctrl Pts',(-19.6987772586223,-12.4917616828604,
114.948136259314)) ;
#182387 = CARTESIAN_POINT('Ctrl Pts',(-19.6249733859194,-12.4917617245726,
114.972367211809)) ;
#182388 = CARTESIAN_POINT('Ctrl Pts',(-19.6155575367091,-12.422111801302,
114.943688056342)) ;
#182389 = CARTESIAN_POINT('Ctrl Pts',(-19.6061416874989,-12.3524618780314,
114.915008900874)) ;
#182390 = CARTESIAN_POINT('Ctrl Pts',(-19.6799455602017,-12.3524618363192,
114.89077794838)) ;
#182391 = CARTESIAN_POINT('Ctrl Pts',(-19.7537494329046,-12.3524617946069,
114.866546995885)) ;
#182392 = CARTESIAN_POINT('Ctrl Pts',(-19.7631652821149,-12.4221117178776,
114.895226151352)) ;
#182393 = CARTESIAN_POINT('Ctrl Pts',(-19.6752313663645,-12.5739000669618,
114.662827645649)) ;
#182394 = CARTESIAN_POINT('Ctrl Pts',(-19.6900674408757,-12.6330567654726,
114.708015932909)) ;
#182395 = CARTESIAN_POINT('Ctrl Pts',(-19.6162635736451,-12.6330568281404,
114.732246902071)) ;
#182396 = CARTESIAN_POINT('Ctrl Pts',(-19.5424597064145,-12.6330568908083,
114.756477871234)) ;
#182397 = CARTESIAN_POINT('Ctrl Pts',(-19.5276236319032,-12.5739001922976,
114.711289583973)) ;
#182398 = CARTESIAN_POINT('Ctrl Pts',(-19.5127875573919,-12.5147434937868,
114.666101296713)) ;
#182399 = CARTESIAN_POINT('Ctrl Pts',(-19.5865914246226,-12.5147434311189,
114.641870327551)) ;
#182400 = CARTESIAN_POINT('Ctrl Pts',(-19.6603952918532,-12.5147433684511,
114.617639358388)) ;
#182401 = CARTESIAN_POINT('Ctrl Pts',(-19.6752313663645,-12.5739000669618,
114.662827645649)) ;
#182402 = CARTESIAN_POINT('Ctrl Pts',(-19.6024167491396,-12.7865530350162,
114.47657434342)) ;
#182403 = CARTESIAN_POINT('Ctrl Pts',(-19.62162373082,-12.830951855475,114.535075708779)) ;
#182404 = CARTESIAN_POINT('Ctrl Pts',(-19.5478198706535,-12.8309519318751,
114.559306699458)) ;
#182405 = CARTESIAN_POINT('Ctrl Pts',(-19.4740160104871,-12.8309520082752,
114.583537690136)) ;
#182406 = CARTESIAN_POINT('Ctrl Pts',(-19.4548090288067,-12.7865531878164,
114.525036324778)) ;
#182407 = CARTESIAN_POINT('Ctrl Pts',(-19.4356020471263,-12.7421543673576,
114.466534959419)) ;
#182408 = CARTESIAN_POINT('Ctrl Pts',(-19.5094059072927,-12.7421542909575,
114.44230396874)) ;
#182409 = CARTESIAN_POINT('Ctrl Pts',(-19.5832097674592,-12.7421542145574,
114.418072978062)) ;
#182410 = CARTESIAN_POINT('Ctrl Pts',(-19.6024167491396,-12.7865530350162,
114.47657434342)) ;
#182411 = CARTESIAN_POINT('Ctrl Pts',(-19.5495231103684,-13.044698151263,
114.350994766483)) ;
#182412 = CARTESIAN_POINT('Ctrl Pts',(-19.5717169142585,-13.071140713464,
114.418593510497)) ;
#182413 = CARTESIAN_POINT('Ctrl Pts',(-19.4979130617208,-13.0711407952517,
114.442824524411)) ;
#182414 = CARTESIAN_POINT('Ctrl Pts',(-19.4241092091832,-13.0711408770393,
114.467055538326)) ;
#182415 = CARTESIAN_POINT('Ctrl Pts',(-19.4019154052932,-13.0446983148383,
114.399456794313)) ;
#182416 = CARTESIAN_POINT('Ctrl Pts',(-19.3797216014032,-13.0182557526373,
114.3318580503)) ;
#182417 = CARTESIAN_POINT('Ctrl Pts',(-19.4535254539408,-13.0182556708497,
114.307627036385)) ;
#182418 = CARTESIAN_POINT('Ctrl Pts',(-19.5273293064784,-13.018255589062,
114.28339602247)) ;
#182419 = CARTESIAN_POINT('Ctrl Pts',(-19.5495231103684,-13.044698151263,
114.350994766483)) ;
#182420 = CARTESIAN_POINT('Ctrl Pts',(-19.5196225512715,-13.328059924083,
114.29525984895)) ;
#182421 = CARTESIAN_POINT('Ctrl Pts',(-19.5432061536921,-13.33475818736,114.367091695157)) ;
#182422 = CARTESIAN_POINT('Ctrl Pts',(-19.4694023083734,-13.3347582681445,
114.39132273106)) ;
#182423 = CARTESIAN_POINT('Ctrl Pts',(-19.3955984630547,-13.334758348929,
114.415553766962)) ;
#182424 = CARTESIAN_POINT('Ctrl Pts',(-19.3720148606341,-13.328060085652,
114.343721920755)) ;
#182425 = CARTESIAN_POINT('Ctrl Pts',(-19.3484312582135,-13.321361822375,
114.271890074548)) ;
#182426 = CARTESIAN_POINT('Ctrl Pts',(-19.4222351035322,-13.3213617415905,
114.247659038646)) ;
#182427 = CARTESIAN_POINT('Ctrl Pts',(-19.4960389488509,-13.321361660806,
114.223428002743)) ;
#182428 = CARTESIAN_POINT('Ctrl Pts',(-19.5196225512715,-13.328059924083,
114.29525984895)) ;
#182429 = CARTESIAN_POINT('Ctrl Pts',(-19.5137354281578,-13.6187777866059,
114.312782448992)) ;
#182430 = CARTESIAN_POINT('Ctrl Pts',(-19.5370320865056,-13.6051885128316,
114.383740309993)) ;
#182431 = CARTESIAN_POINT('Ctrl Pts',(-19.4632282475792,-13.6051885851199,
114.407971365366)) ;
#182432 = CARTESIAN_POINT('Ctrl Pts',(-19.3894244086527,-13.6051886574082,
114.432202420738)) ;
#182433 = CARTESIAN_POINT('Ctrl Pts',(-19.3661277503048,-13.6187779311824,
114.361244559737)) ;
#182434 = CARTESIAN_POINT('Ctrl Pts',(-19.3428310919569,-13.6323672049567,
114.290286698735)) ;
#182435 = CARTESIAN_POINT('Ctrl Pts',(-19.4166349308834,-13.6323671326684,
114.266055643363)) ;
#182436 = CARTESIAN_POINT('Ctrl Pts',(-19.4904387698099,-13.6323670603802,
114.241824587991)) ;
#182437 = CARTESIAN_POINT('Ctrl Pts',(-19.5137354281578,-13.6187777866059,
114.312782448992)) ;
#182438 = CARTESIAN_POINT('Ctrl Pts',(-19.5318785681101,-13.8959727795492,
114.403613733301)) ;
#182439 = CARTESIAN_POINT('Ctrl Pts',(-19.5532078201559,-13.863009115872,
114.468579192321)) ;
#182440 = CARTESIAN_POINT('Ctrl Pts',(-19.4794039858328,-13.8630091736306,
114.492810261715)) ;
#182441 = CARTESIAN_POINT('Ctrl Pts',(-19.4056001515098,-13.8630092313891,
114.517041331108)) ;
#182442 = CARTESIAN_POINT('Ctrl Pts',(-19.3842708994639,-13.8959728950663,
114.452075872088)) ;
#182443 = CARTESIAN_POINT('Ctrl Pts',(-19.3629416474181,-13.9289365587434,
114.387110413069)) ;
#182444 = CARTESIAN_POINT('Ctrl Pts',(-19.4367454817412,-13.9289365009848,
114.362879343675)) ;
#182445 = CARTESIAN_POINT('Ctrl Pts',(-19.5105493160643,-13.9289364432263,
114.338648274282)) ;
#182446 = CARTESIAN_POINT('Ctrl Pts',(-19.5318785681101,-13.8959727795492,
114.403613733301)) ;
#182447 = CARTESIAN_POINT('Ctrl Pts',(-19.5718247752165,-14.1380897314584,
114.560743510385)) ;
#182448 = CARTESIAN_POINT('Ctrl Pts',(-19.5896635278032,-14.0881713161907,
114.615077471405)) ;
#182449 = CARTESIAN_POINT('Ctrl Pts',(-19.5158596961997,-14.0881713577831,
114.639308549082)) ;
#182450 = CARTESIAN_POINT('Ctrl Pts',(-19.4420558645962,-14.0881713993755,
114.663539626758)) ;
#182451 = CARTESIAN_POINT('Ctrl Pts',(-19.4242171120094,-14.1380898146432,
114.609205665738)) ;
#182452 = CARTESIAN_POINT('Ctrl Pts',(-19.4063783594226,-14.1880082299108,
114.554871704718)) ;
#182453 = CARTESIAN_POINT('Ctrl Pts',(-19.4801821910262,-14.1880081883184,
114.530640627041)) ;
#182454 = CARTESIAN_POINT('Ctrl Pts',(-19.5539860226297,-14.188008146726,
114.506409549364)) ;
#182455 = CARTESIAN_POINT('Ctrl Pts',(-19.5718247752165,-14.1380897314584,
114.560743510385)) ;
#182456 = CARTESIAN_POINT('Ctrl Pts',(-19.6301836363791,-14.3289912800735,
114.774053959867)) ;
#182457 = CARTESIAN_POINT('Ctrl Pts',(-19.6432389873474,-14.2656678675504,
114.813818451542)) ;
#182458 = CARTESIAN_POINT('Ctrl Pts',(-19.5694351562483,-14.2656678924027,
114.838049530756)) ;
#182459 = CARTESIAN_POINT('Ctrl Pts',(-19.4956313251491,-14.2656679172549,
114.862280609969)) ;
#182460 = CARTESIAN_POINT('Ctrl Pts',(-19.4825759741808,-14.3289913297781,
114.822516118294)) ;
#182461 = CARTESIAN_POINT('Ctrl Pts',(-19.4695206232126,-14.3923147423012,
114.782751626618)) ;
#182462 = CARTESIAN_POINT('Ctrl Pts',(-19.5433244543117,-14.3923147174489,
114.758520547405)) ;
#182463 = CARTESIAN_POINT('Ctrl Pts',(-19.6171282854108,-14.3923146925966,
114.734289468192)) ;
#182464 = CARTESIAN_POINT('Ctrl Pts',(-19.6301836363791,-14.3289912800735,
114.774053959867)) ;
#182465 = CARTESIAN_POINT('Ctrl Pts',(-19.7013725695596,-14.4536834307714,
115.026197380429)) ;
#182466 = CARTESIAN_POINT('Ctrl Pts',(-19.7087463412497,-14.3815580790825,
115.048656698481)) ;
#182467 = CARTESIAN_POINT('Ctrl Pts',(-19.6349425096067,-14.381558090492,
115.072887776038)) ;
#182468 = CARTESIAN_POINT('Ctrl Pts',(-19.5611386779637,-14.3815581019016,
115.097118853595)) ;
#182469 = CARTESIAN_POINT('Ctrl Pts',(-19.5537649062736,-14.4536834535906,
115.074659535542)) ;
#182470 = CARTESIAN_POINT('Ctrl Pts',(-19.5463911345834,-14.5258088052795,
115.052200217489)) ;
#182471 = CARTESIAN_POINT('Ctrl Pts',(-19.6201949662265,-14.52580879387,115.027969139933)) ;
#182472 = CARTESIAN_POINT('Ctrl Pts',(-19.6939987978695,-14.5258087824604,
115.003738062376)) ;
#182473 = CARTESIAN_POINT('Ctrl Pts',(-19.7013725695596,-14.4536834307714,
115.026197380429)) ;
#182474 = CARTESIAN_POINT('Ctrl Pts',(-19.7802758537962,-14.5050447602448,
115.301993496295)) ;
#182475 = CARTESIAN_POINT('Ctrl Pts',(-19.7814175815001,-14.4292238155188,
115.305471014069)) ;
#182476 = CARTESIAN_POINT('Ctrl Pts',(-19.7076137477033,-14.4292238160263,
115.329702085066)) ;
#182477 = CARTESIAN_POINT('Ctrl Pts',(-19.6338099139064,-14.4292238165338,
115.353933156062)) ;
#182478 = CARTESIAN_POINT('Ctrl Pts',(-19.6326681862024,-14.5050447612597,
115.350455638288)) ;
#182479 = CARTESIAN_POINT('Ctrl Pts',(-19.6315264584984,-14.5808657059856,
115.346978120514)) ;
#182480 = CARTESIAN_POINT('Ctrl Pts',(-19.7053302922953,-14.5808657054781,
115.322747049518)) ;
#182481 = CARTESIAN_POINT('Ctrl Pts',(-19.7791341260922,-14.5808657049707,
115.298515978521)) ;
#182482 = CARTESIAN_POINT('Ctrl Pts',(-19.7802758537962,-14.5050447602448,
115.301993496295)) ;
#182483 = CARTESIAN_POINT('Ctrl Pts',(-19.8602648502565,-14.4782940097224,
115.581115798134)) ;
#182484 = CARTESIAN_POINT('Ctrl Pts',(-19.8550887574373,-14.4042259752822,
115.565350254132)) ;
#182485 = CARTESIAN_POINT('Ctrl Pts',(-19.781284920809,-14.4042259695799,
115.589581316504)) ;
#182486 = CARTESIAN_POINT('Ctrl Pts',(-19.7074810841807,-14.4042259638776,
115.613812378877)) ;
#182487 = CARTESIAN_POINT('Ctrl Pts',(-19.712657177,-14.4782939983178,115.629577922879)) ;
#182488 = CARTESIAN_POINT('Ctrl Pts',(-19.7178332698193,-14.552362032758,
115.645343466881)) ;
#182489 = CARTESIAN_POINT('Ctrl Pts',(-19.7916371064475,-14.5523620384603,
115.621112404509)) ;
#182490 = CARTESIAN_POINT('Ctrl Pts',(-19.8654409430758,-14.5523620441626,
115.596881342136)) ;
#182491 = CARTESIAN_POINT('Ctrl Pts',(-19.8602648502565,-14.4782940097224,
115.581115798134)) ;
#182492 = CARTESIAN_POINT('Ctrl Pts',(-19.9347147614836,-14.3758709565101,
115.843310818207)) ;
#182493 = CARTESIAN_POINT('Ctrl Pts',(-19.923599187215,-14.3088425929799,
115.809454572183)) ;
#182494 = CARTESIAN_POINT('Ctrl Pts',(-19.8497953478602,-14.3088425851836,
115.83368562625)) ;
#182495 = CARTESIAN_POINT('Ctrl Pts',(-19.7759915085054,-14.3088425773873,
115.857916680318)) ;
#182496 = CARTESIAN_POINT('Ctrl Pts',(-19.787107082774,-14.3758709409175,
115.891772926342)) ;
#182497 = CARTESIAN_POINT('Ctrl Pts',(-19.7982226570426,-14.4428993044478,
115.925629172366)) ;
#182498 = CARTESIAN_POINT('Ctrl Pts',(-19.8720264963974,-14.442899312244,
115.901398118298)) ;
#182499 = CARTESIAN_POINT('Ctrl Pts',(-19.9458303357523,-14.4428993200403,
115.87716706423)) ;
#182500 = CARTESIAN_POINT('Ctrl Pts',(-19.9347147614836,-14.3758709565101,
115.843310818207)) ;
#182501 = CARTESIAN_POINT('Ctrl Pts',(-19.9978520690189,-14.2038414128419,
116.071213910054)) ;
#182502 = CARTESIAN_POINT('Ctrl Pts',(-19.9815743341015,-14.1487238719563,
116.021634555749)) ;
#182503 = CARTESIAN_POINT('Ctrl Pts',(-19.9077704923257,-14.1487238662438,
116.045865602443)) ;
#182504 = CARTESIAN_POINT('Ctrl Pts',(-19.8339666505498,-14.1487238605313,
116.070096649137)) ;
#182505 = CARTESIAN_POINT('Ctrl Pts',(-19.8502443854672,-14.2038414014169,
116.119676003441)) ;
#182506 = CARTESIAN_POINT('Ctrl Pts',(-19.8665221203846,-14.2589589423024,
116.169255357746)) ;
#182507 = CARTESIAN_POINT('Ctrl Pts',(-19.9403259621604,-14.2589589480149,
116.145024311053)) ;
#182508 = CARTESIAN_POINT('Ctrl Pts',(-20.0141298039363,-14.2589589537274,
116.120793264359)) ;
#182509 = CARTESIAN_POINT('Ctrl Pts',(-19.9978520690189,-14.2038414128419,
116.071213910054)) ;
#182510 = CARTESIAN_POINT('Ctrl Pts',(-20.0437608055394,-13.9777022974474,
116.246290431743)) ;
#182511 = CARTESIAN_POINT('Ctrl Pts',(-20.0235237807075,-13.9382924680263,
116.184651719268)) ;
#182512 = CARTESIAN_POINT('Ctrl Pts',(-19.9497199377517,-13.9382924647888,
116.208882762368)) ;
#182513 = CARTESIAN_POINT('Ctrl Pts',(-19.8759160947959,-13.9382924615514,
116.233113805468)) ;
#182514 = CARTESIAN_POINT('Ctrl Pts',(-19.8961531196278,-13.9777022909725,
116.294752517942)) ;
#182515 = CARTESIAN_POINT('Ctrl Pts',(-19.9163901444597,-14.0171121203935,
116.356391230417)) ;
#182516 = CARTESIAN_POINT('Ctrl Pts',(-19.9901939874155,-14.017112123631,
116.332160187317)) ;
#182517 = CARTESIAN_POINT('Ctrl Pts',(-20.0639978303713,-14.0171121268685,
116.307929144217)) ;
#182518 = CARTESIAN_POINT('Ctrl Pts',(-20.0437608055394,-13.9777022974474,
116.246290431743)) ;
#182519 = CARTESIAN_POINT('Ctrl Pts',(-20.0692545667737,-13.7081471730545,
116.359670607939)) ;
#182520 = CARTESIAN_POINT('Ctrl Pts',(-20.046467328162,-13.6875008672276,
116.290264355866)) ;
#182521 = CARTESIAN_POINT('Ctrl Pts',(-19.9726634845246,-13.6875008686463,
116.314495396889)) ;
#182522 = CARTESIAN_POINT('Ctrl Pts',(-19.8988596408872,-13.687500870065,
116.338726437913)) ;
#182523 = CARTESIAN_POINT('Ctrl Pts',(-19.9216468794989,-13.7081471758919,
116.408132689987)) ;
#182524 = CARTESIAN_POINT('Ctrl Pts',(-19.9444341181106,-13.7287934817188,
116.47753894206)) ;
#182525 = CARTESIAN_POINT('Ctrl Pts',(-20.018237961748,-13.7287934803001,
116.453307901037)) ;
#182526 = CARTESIAN_POINT('Ctrl Pts',(-20.0920418053854,-13.7287934788814,
116.429076860013)) ;
#182527 = CARTESIAN_POINT('Ctrl Pts',(-20.0692545667737,-13.7081471730545,
116.359670607939)) ;
#182528 = CARTESIAN_POINT('Ctrl Pts',(-20.0710088126816,-13.4207218926891,
116.400338260626)) ;
#182529 = CARTESIAN_POINT('Ctrl Pts',(-20.0473342388488,-13.4201152017274,
116.328229328668)) ;
#182530 = CARTESIAN_POINT('Ctrl Pts',(-19.9735303954241,-13.4201152047761,
116.35246037034)) ;
#182531 = CARTESIAN_POINT('Ctrl Pts',(-19.8997265519995,-13.4201152078248,
116.376691412012)) ;
#182532 = CARTESIAN_POINT('Ctrl Pts',(-19.9234011258323,-13.4207218987865,
116.44880034397)) ;
#182533 = CARTESIAN_POINT('Ctrl Pts',(-19.9470756996652,-13.4213285897482,
116.520909275928)) ;
#182534 = CARTESIAN_POINT('Ctrl Pts',(-20.0208795430899,-13.4213285866995,
116.496678234256)) ;
#182535 = CARTESIAN_POINT('Ctrl Pts',(-20.0946833865145,-13.4213285836508,
116.472447192584)) ;
#182536 = CARTESIAN_POINT('Ctrl Pts',(-20.0710088126816,-13.4207218926891,
116.400338260626)) ;
#182537 = CARTESIAN_POINT('Ctrl Pts',(-20.0486389329938,-13.1323473586493,
116.367635760185)) ;
#182538 = CARTESIAN_POINT('Ctrl Pts',(-20.0257581006651,-13.1518767361785,
116.297944436781)) ;
#182539 = CARTESIAN_POINT('Ctrl Pts',(-19.9519542575344,-13.1518767392038,
116.322175479348)) ;
#182540 = CARTESIAN_POINT('Ctrl Pts',(-19.8781504144038,-13.1518767422291,
116.346406521915)) ;
#182541 = CARTESIAN_POINT('Ctrl Pts',(-19.9010312467325,-13.1323473646999,
116.416097845319)) ;
#182542 = CARTESIAN_POINT('Ctrl Pts',(-19.9239120790612,-13.1128179871707,
116.485789168723)) ;
#182543 = CARTESIAN_POINT('Ctrl Pts',(-19.9977159221919,-13.1128179841454,
116.461558126156)) ;
#182544 = CARTESIAN_POINT('Ctrl Pts',(-20.0715197653226,-13.1128179811201,
116.437327083588)) ;
#182545 = CARTESIAN_POINT('Ctrl Pts',(-20.0486389329938,-13.1323473586493,
116.367635760185)) ;
#182546 = CARTESIAN_POINT('Ctrl Pts',(-20.0027585392029,-12.8640039527127,
116.26336619867)) ;
#182547 = CARTESIAN_POINT('Ctrl Pts',(-19.9823136010525,-12.9022999989721,
116.201094215862)) ;
#182548 = CARTESIAN_POINT('Ctrl Pts',(-19.9085097578917,-12.9022999996752,
116.225325258337)) ;
#182549 = CARTESIAN_POINT('Ctrl Pts',(-19.8347059147309,-12.9023000003783,
116.249556300812)) ;
#182550 = CARTESIAN_POINT('Ctrl Pts',(-19.8551508528813,-12.8640039541189,
116.31182828362)) ;
#182551 = CARTESIAN_POINT('Ctrl Pts',(-19.8755957910317,-12.8257079078595,
116.374100266428)) ;
#182552 = CARTESIAN_POINT('Ctrl Pts',(-19.9493996341925,-12.8257079071564,
116.349869223953)) ;
#182553 = CARTESIAN_POINT('Ctrl Pts',(-20.0232034773534,-12.8257079064533,
116.325638181478)) ;
#182554 = CARTESIAN_POINT('Ctrl Pts',(-20.0027585392029,-12.8640039527127,
116.26336619867)) ;
#182555 = CARTESIAN_POINT('Ctrl Pts',(-19.935788026807,-12.6351955964259,
116.094916391057)) ;
#182556 = CARTESIAN_POINT('Ctrl Pts',(-19.9192541332925,-12.6895248162975,
116.044556819081)) ;
#182557 = CARTESIAN_POINT('Ctrl Pts',(-19.8454502892082,-12.6895248136964,
116.068787858743)) ;
#182558 = CARTESIAN_POINT('Ctrl Pts',(-19.7716464451238,-12.6895248110954,
116.093018898405)) ;
#182559 = CARTESIAN_POINT('Ctrl Pts',(-19.7881803386382,-12.6351955912238,
116.143378470382)) ;
#182560 = CARTESIAN_POINT('Ctrl Pts',(-19.8047142321527,-12.5808663713523,
116.193738042358)) ;
#182561 = CARTESIAN_POINT('Ctrl Pts',(-19.8785180762371,-12.5808663739533,
116.169507002696)) ;
#182562 = CARTESIAN_POINT('Ctrl Pts',(-19.9523219203215,-12.5808663765543,
116.145275963034)) ;
#182563 = CARTESIAN_POINT('Ctrl Pts',(-19.935788026807,-12.6351955964259,
116.094916391057)) ;
#182564 = CARTESIAN_POINT('Ctrl Pts',(-19.8524350019228,-12.4633049543151,
115.876360547653)) ;
#182565 = CARTESIAN_POINT('Ctrl Pts',(-19.8409661307527,-12.5297151872054,
115.841428216412)) ;
#182566 = CARTESIAN_POINT('Ctrl Pts',(-19.7671622852702,-12.5297151829142,
115.865659251816)) ;
#182567 = CARTESIAN_POINT('Ctrl Pts',(-19.6933584397878,-12.529715178623,
115.88989028722)) ;
#182568 = CARTESIAN_POINT('Ctrl Pts',(-19.7048273109579,-12.4633049457328,
115.924822618461)) ;
#182569 = CARTESIAN_POINT('Ctrl Pts',(-19.7162961821279,-12.3968947128425,
115.959754949702)) ;
#182570 = CARTESIAN_POINT('Ctrl Pts',(-19.7901000276104,-12.3968947171337,
115.935523914298)) ;
#182571 = CARTESIAN_POINT('Ctrl Pts',(-19.8639038730929,-12.3968947214249,
115.911292878894)) ;
#182572 = CARTESIAN_POINT('Ctrl Pts',(-19.8524350019228,-12.4633049543151,
115.876360547653)) ;
#182573 = CARTESIAN_POINT('Ctrl Pts',(-19.7565552164464,-12.3586842738095,
115.619991906947)) ;
#182574 = CARTESIAN_POINT('Ctrl Pts',(-19.7510262973849,-12.4324967253125,
115.603151711264)) ;
#182575 = CARTESIAN_POINT('Ctrl Pts',(-19.6772224491687,-12.432496720994,
115.627382738341)) ;
#182576 = CARTESIAN_POINT('Ctrl Pts',(-19.6034186009525,-12.4324967166755,
115.651613765419)) ;
#182577 = CARTESIAN_POINT('Ctrl Pts',(-19.6089475200141,-12.3586842651726,
115.668453961102)) ;
#182578 = CARTESIAN_POINT('Ctrl Pts',(-19.6144764390756,-12.2848718136696,
115.685294156784)) ;
#182579 = CARTESIAN_POINT('Ctrl Pts',(-19.6882802872918,-12.284871817988,
115.661063129707)) ;
#182580 = CARTESIAN_POINT('Ctrl Pts',(-19.762084135508,-12.2848718223065,
115.63683210263)) ;
#182581 = CARTESIAN_POINT('Ctrl Pts',(-19.7565552164464,-12.3586842738095,
115.619991906947)) ;
#182582 = CARTESIAN_POINT('Ctrl Pts',(-19.6559368636795,-12.3308701665295,
115.348879090383)) ;
#182583 = CARTESIAN_POINT('Ctrl Pts',(-19.6566937304098,-12.4067313032611,
115.351184383885)) ;
#182584 = CARTESIAN_POINT('Ctrl Pts',(-19.5828898799169,-12.4067313035056,
115.375415404028)) ;
#182585 = CARTESIAN_POINT('Ctrl Pts',(-19.5090860294241,-12.4067313037501,
115.399646424171)) ;
#182586 = CARTESIAN_POINT('Ctrl Pts',(-19.5083291626938,-12.3308701670186,
115.39734113067)) ;
#182587 = CARTESIAN_POINT('Ctrl Pts',(-19.5075722959635,-12.2550090302871,
115.395035837168)) ;
#182588 = CARTESIAN_POINT('Ctrl Pts',(-19.5813761464564,-12.2550090300425,
115.370804817025)) ;
#182589 = CARTESIAN_POINT('Ctrl Pts',(-19.6551799969492,-12.255009029798,
115.346573796882)) ;
#182590 = CARTESIAN_POINT('Ctrl Pts',(-19.6559368636795,-12.3308701665295,
115.348879090383)) ;
#182591 = CARTESIAN_POINT('Ctrl Pts',(-19.5559630364021,-12.3804185210795,
115.079826490949)) ;
#182592 = CARTESIAN_POINT('Ctrl Pts',(-19.5629676944445,-12.4529298980233,
115.101161548555)) ;
#182593 = CARTESIAN_POINT('Ctrl Pts',(-19.4891638418352,-12.452929906521,
115.125392562252)) ;
#182594 = CARTESIAN_POINT('Ctrl Pts',(-19.415359989226,-12.4529299150187,
115.149623575949)) ;
#182595 = CARTESIAN_POINT('Ctrl Pts',(-19.4083553311837,-12.380418538075,
115.128288518343)) ;
#182596 = CARTESIAN_POINT('Ctrl Pts',(-19.4013506731413,-12.3079071611312,
115.106953460736)) ;
#182597 = CARTESIAN_POINT('Ctrl Pts',(-19.4751545257505,-12.3079071526335,
115.082722447039)) ;
#182598 = CARTESIAN_POINT('Ctrl Pts',(-19.5489583783597,-12.3079071441357,
115.058491433342)) ;
#182599 = CARTESIAN_POINT('Ctrl Pts',(-19.5559630364021,-12.3804185210795,
115.079826490949)) ;
#182600 = CARTESIAN_POINT('Ctrl Pts',(-19.4632285523152,-12.5045865657479,
114.832858816864)) ;
#182601 = CARTESIAN_POINT('Ctrl Pts',(-19.4759837989463,-12.5685333529208,
114.871709239288)) ;
#182602 = CARTESIAN_POINT('Ctrl Pts',(-19.4021799450906,-12.5685333737573,
114.895940249188)) ;
#182603 = CARTESIAN_POINT('Ctrl Pts',(-19.3283760912348,-12.5685333945939,
114.920171259088)) ;
#182604 = CARTESIAN_POINT('Ctrl Pts',(-19.3156208446037,-12.504586607421,
114.881320836664)) ;
#182605 = CARTESIAN_POINT('Ctrl Pts',(-19.3028655979726,-12.4406398202481,
114.84247041424)) ;
#182606 = CARTESIAN_POINT('Ctrl Pts',(-19.3766694518284,-12.4406397994116,
114.81823940434)) ;
#182607 = CARTESIAN_POINT('Ctrl Pts',(-19.4504733056841,-12.440639778575,
114.794008394439)) ;
#182608 = CARTESIAN_POINT('Ctrl Pts',(-19.4632285523152,-12.5045865657479,
114.832858816864)) ;
#182609 = CARTESIAN_POINT('Ctrl Pts',(-19.3838405577288,-12.6936012415773,
114.626458033077)) ;
#182610 = CARTESIAN_POINT('Ctrl Pts',(-19.4014244618248,-12.7444433865652,
114.680015766882)) ;
#182611 = CARTESIAN_POINT('Ctrl Pts',(-19.3276206083385,-12.7444434214993,
114.704246777907)) ;
#182612 = CARTESIAN_POINT('Ctrl Pts',(-19.2538167548521,-12.7444434564334,
114.728477788932)) ;
#182613 = CARTESIAN_POINT('Ctrl Pts',(-19.2362328507561,-12.6936013114455,
114.674920055127)) ;
#182614 = CARTESIAN_POINT('Ctrl Pts',(-19.2186489466601,-12.6427591664577,
114.621362321322)) ;
#182615 = CARTESIAN_POINT('Ctrl Pts',(-19.2924528001464,-12.6427591315236,
114.597131310297)) ;
#182616 = CARTESIAN_POINT('Ctrl Pts',(-19.3662566536328,-12.6427590965895,
114.572900299272)) ;
#182617 = CARTESIAN_POINT('Ctrl Pts',(-19.3838405577288,-12.6936012415773,
114.626458033077)) ;
#182618 = CARTESIAN_POINT('Ctrl Pts',(-19.3222105618298,-12.9362801376937,
114.474398641739)) ;
#182619 = CARTESIAN_POINT('Ctrl Pts',(-19.3433851628242,-12.9702525737982,
114.538893058736)) ;
#182620 = CARTESIAN_POINT('Ctrl Pts',(-19.2695813111783,-12.9702526255318,
114.563124075367)) ;
#182621 = CARTESIAN_POINT('Ctrl Pts',(-19.1957774595324,-12.9702526772653,
114.587355091998)) ;
#182622 = CARTESIAN_POINT('Ctrl Pts',(-19.1746028585379,-12.9362802411607,
114.522860675001)) ;
#182623 = CARTESIAN_POINT('Ctrl Pts',(-19.1534282575434,-12.9023078050562,
114.458366258004)) ;
#182624 = CARTESIAN_POINT('Ctrl Pts',(-19.2272321091894,-12.9023077533226,
114.434135241373)) ;
#182625 = CARTESIAN_POINT('Ctrl Pts',(-19.3010359608353,-12.9023077015891,
114.409904224742)) ;
#182626 = CARTESIAN_POINT('Ctrl Pts',(-19.3222105618298,-12.9362801376937,
114.474398641739)) ;
#182627 = CARTESIAN_POINT('Ctrl Pts',(-19.2828604657008,-13.2112926431605,
114.389881775346)) ;
#182628 = CARTESIAN_POINT('Ctrl Pts',(-19.3060817289072,-13.2261131719055,
114.460609995074)) ;
#182629 = CARTESIAN_POINT('Ctrl Pts',(-19.2322778814261,-13.2261132359039,
114.48484102439)) ;
#182630 = CARTESIAN_POINT('Ctrl Pts',(-19.1584740339449,-13.2261132999022,
114.509072053706)) ;
#182631 = CARTESIAN_POINT('Ctrl Pts',(-19.1352527707385,-13.2112927711572,
114.438343833979)) ;
#182632 = CARTESIAN_POINT('Ctrl Pts',(-19.1120315075321,-13.1964722424121,
114.367615614251)) ;
#182633 = CARTESIAN_POINT('Ctrl Pts',(-19.1858353550133,-13.1964721784138,
114.343384584935)) ;
#182634 = CARTESIAN_POINT('Ctrl Pts',(-19.2596392024944,-13.1964721144154,
114.319153555619)) ;
#182635 = CARTESIAN_POINT('Ctrl Pts',(-19.2828604657008,-13.2112926431605,
114.389881775346)) ;
#182636 = CARTESIAN_POINT('Ctrl Pts',(-19.2671542279157,-13.5026318637497,
114.377588421652)) ;
#182637 = CARTESIAN_POINT('Ctrl Pts',(-19.2907702583407,-13.4971333433814,
114.449519038463)) ;
#182638 = CARTESIAN_POINT('Ctrl Pts',(-19.2169664165159,-13.4971334172492,
114.473750085008)) ;
#182639 = CARTESIAN_POINT('Ctrl Pts',(-19.1431625746911,-13.4971334911169,
114.497981131552)) ;
#182640 = CARTESIAN_POINT('Ctrl Pts',(-19.119546544266,-13.5026320114853,
114.426050514741)) ;
#182641 = CARTESIAN_POINT('Ctrl Pts',(-19.0959305138409,-13.5081305318536,
114.35411989793)) ;
#182642 = CARTESIAN_POINT('Ctrl Pts',(-19.1697343556658,-13.5081304579859,
114.329888851385)) ;
#182643 = CARTESIAN_POINT('Ctrl Pts',(-19.2435381974906,-13.5081303841181,
114.305657804841)) ;
#182644 = CARTESIAN_POINT('Ctrl Pts',(-19.2671542279157,-13.5026318637497,
114.377588421652)) ;
#182645 = CARTESIAN_POINT('Ctrl Pts',(-19.2757419733594,-13.7865927515763,
114.439120363259)) ;
#182646 = CARTESIAN_POINT('Ctrl Pts',(-19.2980606185593,-13.7612608950297,
114.507099353878)) ;
#182647 = CARTESIAN_POINT('Ctrl Pts',(-19.2242567835297,-13.7612609711619,
114.531330421119)) ;
#182648 = CARTESIAN_POINT('Ctrl Pts',(-19.1504529485,-13.7612610472941,114.55556148836)) ;
#182649 = CARTESIAN_POINT('Ctrl Pts',(-19.1281343033001,-13.7865929038406,
114.487582497741)) ;
#182650 = CARTESIAN_POINT('Ctrl Pts',(-19.1058156581001,-13.8119247603871,
114.419603507123)) ;
#182651 = CARTESIAN_POINT('Ctrl Pts',(-19.1796194931298,-13.811924684255,
114.395372439881)) ;
#182652 = CARTESIAN_POINT('Ctrl Pts',(-19.2534233281594,-13.8119246081228,
114.37114137264)) ;
#182653 = CARTESIAN_POINT('Ctrl Pts',(-19.2757419733594,-13.7865927515763,
114.439120363259)) ;
#182654 = CARTESIAN_POINT('Ctrl Pts',(-19.3070927419327,-14.0445932154009,
114.570030945766)) ;
#182655 = CARTESIAN_POINT('Ctrl Pts',(-19.3265220349553,-14.0012118501805,
114.629209435722)) ;
#182656 = CARTESIAN_POINT('Ctrl Pts',(-19.2527182070799,-14.001211921774,
114.653440524754)) ;
#182657 = CARTESIAN_POINT('Ctrl Pts',(-19.1789143792045,-14.0012119933675,
114.677671613786)) ;
#182658 = CARTESIAN_POINT('Ctrl Pts',(-19.159485086182,-14.0445933585879,
114.61849312383)) ;
#182659 = CARTESIAN_POINT('Ctrl Pts',(-19.1400557931594,-14.0879747238084,
114.559314633874)) ;
#182660 = CARTESIAN_POINT('Ctrl Pts',(-19.2138596210347,-14.0879746522149,
114.535083544842)) ;
#182661 = CARTESIAN_POINT('Ctrl Pts',(-19.2876634489101,-14.0879745806213,
114.510852455809)) ;
#182662 = CARTESIAN_POINT('Ctrl Pts',(-19.3070927419327,-14.0445932154009,
114.570030945766)) ;
#182663 = CARTESIAN_POINT('Ctrl Pts',(-19.358347515694,-14.2581092551482,
114.761608730446)) ;
#182664 = CARTESIAN_POINT('Ctrl Pts',(-19.3734928699903,-14.199757820622,
114.807739034136)) ;
#182665 = CARTESIAN_POINT('Ctrl Pts',(-19.2996890489537,-14.199757880284,
114.831970143998)) ;
#182666 = CARTESIAN_POINT('Ctrl Pts',(-19.2258852279171,-14.199757939946,
114.85620125386)) ;
#182667 = CARTESIAN_POINT('Ctrl Pts',(-19.2107398736208,-14.2581093744722,
114.81007095017)) ;
#182668 = CARTESIAN_POINT('Ctrl Pts',(-19.1955945193246,-14.3164608089984,
114.763940646481)) ;
#182669 = CARTESIAN_POINT('Ctrl Pts',(-19.2693983403611,-14.3164607493364,
114.739709536619)) ;
#182670 = CARTESIAN_POINT('Ctrl Pts',(-19.3432021613977,-14.3164606896743,
114.715478426757)) ;
#182671 = CARTESIAN_POINT('Ctrl Pts',(-19.358347515694,-14.2581092551482,
114.761608730446)) ;
#182672 = CARTESIAN_POINT('Ctrl Pts',(-19.4252783091883,-14.4117380229187,
115.001038317045)) ;
#182673 = CARTESIAN_POINT('Ctrl Pts',(-19.4350370294147,-14.3425754066096,
115.030761802378)) ;
#182674 = CARTESIAN_POINT('Ctrl Pts',(-19.3612332141478,-14.3425754472621,
115.054992929814)) ;
#182675 = CARTESIAN_POINT('Ctrl Pts',(-19.287429398881,-14.3425754879145,
115.079224057249)) ;
#182676 = CARTESIAN_POINT('Ctrl Pts',(-19.2776706786545,-14.4117381042236,
115.049500571916)) ;
#182677 = CARTESIAN_POINT('Ctrl Pts',(-19.2679119584281,-14.4809007205327,
115.019777086582)) ;
#182678 = CARTESIAN_POINT('Ctrl Pts',(-19.3417157736949,-14.4809006798802,
114.995545959146)) ;
#182679 = CARTESIAN_POINT('Ctrl Pts',(-19.4155195889618,-14.4809006392278,
114.971314831711)) ;
#182680 = CARTESIAN_POINT('Ctrl Pts',(-19.4252783091883,-14.4117380229187,
115.001038317045)) ;
#182681 = CARTESIAN_POINT('Ctrl Pts',(-19.5019526631148,-14.4936441507055,
115.270046158408)) ;
#182682 = CARTESIAN_POINT('Ctrl Pts',(-19.5056386466896,-14.4186618661927,
115.281273067656)) ;
#182683 = CARTESIAN_POINT('Ctrl Pts',(-19.4318348350287,-14.4186618819305,
115.305504206074)) ;
#182684 = CARTESIAN_POINT('Ctrl Pts',(-19.3580310233677,-14.4186618976683,
115.329735344493)) ;
#182685 = CARTESIAN_POINT('Ctrl Pts',(-19.3543450397929,-14.4936441821811,
115.318508435245)) ;
#182686 = CARTESIAN_POINT('Ctrl Pts',(-19.350659056218,-14.5686264666939,
115.307281525998)) ;
#182687 = CARTESIAN_POINT('Ctrl Pts',(-19.424462867879,-14.5686264509561,
115.283050387579)) ;
#182688 = CARTESIAN_POINT('Ctrl Pts',(-19.49826667954,-14.5686264352184,115.258819249161)) ;
#182689 = CARTESIAN_POINT('Ctrl Pts',(-19.5019526631148,-14.4936441507055,
115.270046158408)) ;
#182690 = CARTESIAN_POINT('Ctrl Pts',(-19.5823198515389,-14.4983888239063,
115.550327419762)) ;
#182691 = CARTESIAN_POINT('Ctrl Pts',(-19.5796658758239,-14.422965043811,
115.542243835903)) ;
#182692 = CARTESIAN_POINT('Ctrl Pts',(-19.505862065243,-14.4229650315207,
115.566474977611)) ;
#182693 = CARTESIAN_POINT('Ctrl Pts',(-19.4320582546622,-14.4229650192305,
115.59070611932)) ;
#182694 = CARTESIAN_POINT('Ctrl Pts',(-19.4347122303772,-14.4983887993257,
115.598789703178)) ;
#182695 = CARTESIAN_POINT('Ctrl Pts',(-19.4373662060922,-14.573812579421,
115.606873287037)) ;
#182696 = CARTESIAN_POINT('Ctrl Pts',(-19.511170016673,-14.5738125917113,
115.582642145328)) ;
#182697 = CARTESIAN_POINT('Ctrl Pts',(-19.5849738272539,-14.5738126040015,
115.55841100362)) ;
#182698 = CARTESIAN_POINT('Ctrl Pts',(-19.5823198515389,-14.4983888239063,
115.550327419762)) ;
#182699 = CARTESIAN_POINT('Ctrl Pts',(-19.6595477418913,-14.426207251784,
115.82090191206)) ;
#182700 = CARTESIAN_POINT('Ctrl Pts',(-19.6507666379267,-14.3557121733631,
115.79415608413)) ;
#182701 = CARTESIAN_POINT('Ctrl Pts',(-19.5769628256401,-14.355712132954,
115.818387220643)) ;
#182702 = CARTESIAN_POINT('Ctrl Pts',(-19.5031590133536,-14.3557120925449,
115.842618357156)) ;
#182703 = CARTESIAN_POINT('Ctrl Pts',(-19.5119401173182,-14.4262071709657,
115.869364185087)) ;
#182704 = CARTESIAN_POINT('Ctrl Pts',(-19.5207212212828,-14.4967022493866,
115.896110013017)) ;
#182705 = CARTESIAN_POINT('Ctrl Pts',(-19.5945250335694,-14.4967022897957,
115.871878876504)) ;
#182706 = CARTESIAN_POINT('Ctrl Pts',(-19.6683288458559,-14.4967023302048,
115.847647739991)) ;
#182707 = CARTESIAN_POINT('Ctrl Pts',(-19.6595477418913,-14.426207251784,
115.82090191206)) ;
#182708 = CARTESIAN_POINT('Ctrl Pts',(-19.7280764038109,-14.2809809264381,
116.065217208955)) ;
#182709 = CARTESIAN_POINT('Ctrl Pts',(-19.7137615271889,-14.2205203869784,
116.021616402365)) ;
#182710 = CARTESIAN_POINT('Ctrl Pts',(-19.6399577106063,-14.2205203209335,
116.045847525793)) ;
#182711 = CARTESIAN_POINT('Ctrl Pts',(-19.5661538940236,-14.2205202548886,
116.070078649221)) ;
#182712 = CARTESIAN_POINT('Ctrl Pts',(-19.5804687706457,-14.2809807943484,
116.113679455811)) ;
#182713 = CARTESIAN_POINT('Ctrl Pts',(-19.5947836472677,-14.3414413338082,
116.157280262401)) ;
#182714 = CARTESIAN_POINT('Ctrl Pts',(-19.6685874638503,-14.3414413998531,
116.133049138973)) ;
#182715 = CARTESIAN_POINT('Ctrl Pts',(-19.7423912804329,-14.3414414658979,
116.108818015545)) ;
#182716 = CARTESIAN_POINT('Ctrl Pts',(-19.7280764038109,-14.2809809264381,
116.065217208955)) ;
#182717 = CARTESIAN_POINT('Ctrl Pts',(-19.7813206021368,-14.0755731076895,
116.262663449883)) ;
#182718 = CARTESIAN_POINT('Ctrl Pts',(-19.7625374017033,-14.0293643773253,
116.205452849931)) ;
#182719 = CARTESIAN_POINT('Ctrl Pts',(-19.6887335786472,-14.0293642911148,
116.229683953641)) ;
#182720 = CARTESIAN_POINT('Ctrl Pts',(-19.614929755591,-14.0293642049043,
116.253915057352)) ;
#182721 = CARTESIAN_POINT('Ctrl Pts',(-19.6337129560244,-14.0755729352685,
116.311125657304)) ;
#182722 = CARTESIAN_POINT('Ctrl Pts',(-19.6524961564578,-14.1217816656326,
116.368336257255)) ;
#182723 = CARTESIAN_POINT('Ctrl Pts',(-19.726299979514,-14.1217817518431,
116.344105153545)) ;
#182724 = CARTESIAN_POINT('Ctrl Pts',(-19.8001038025702,-14.1217818380536,
116.319874049834)) ;
#182725 = CARTESIAN_POINT('Ctrl Pts',(-19.7813206021368,-14.0755731076895,
116.262663449883)) ;
#182726 = CARTESIAN_POINT('Ctrl Pts',(-19.8156285654698,-13.8214647968314,
116.402723704513)) ;
#182727 = CARTESIAN_POINT('Ctrl Pts',(-19.7936862540445,-13.7929280082953,
116.33589096223)) ;
#182728 = CARTESIAN_POINT('Ctrl Pts',(-19.7198824228961,-13.7929279092314,
116.360122041293)) ;
#182729 = CARTESIAN_POINT('Ctrl Pts',(-19.6460785917477,-13.7929278101675,
116.384353120356)) ;
#182730 = CARTESIAN_POINT('Ctrl Pts',(-19.668020903173,-13.8214645987035,
116.451185862638)) ;
#182731 = CARTESIAN_POINT('Ctrl Pts',(-19.6899632145983,-13.8500013872396,
116.518018604921)) ;
#182732 = CARTESIAN_POINT('Ctrl Pts',(-19.7637670457467,-13.8500014863035,
116.493787525858)) ;
#182733 = CARTESIAN_POINT('Ctrl Pts',(-19.8375708768951,-13.8500015853674,
116.469556446795)) ;
#182734 = CARTESIAN_POINT('Ctrl Pts',(-19.8156285654698,-13.8214647968314,
116.402723704513)) ;
#182735 = CARTESIAN_POINT('Ctrl Pts',(-19.8271835709341,-13.5390721929965,
116.473371097639)) ;
#182736 = CARTESIAN_POINT('Ctrl Pts',(-19.8036682136408,-13.5302086359891,
116.401747111505)) ;
#182737 = CARTESIAN_POINT('Ctrl Pts',(-19.7298643737381,-13.5302085326853,
116.425978163903)) ;
#182738 = CARTESIAN_POINT('Ctrl Pts',(-19.6560605338353,-13.5302084293816,
116.450209216302)) ;
#182739 = CARTESIAN_POINT('Ctrl Pts',(-19.6795758911286,-13.539071986389,
116.521833202437)) ;
#182740 = CARTESIAN_POINT('Ctrl Pts',(-19.7030912484218,-13.5479355433964,
116.593457188571)) ;
#182741 = CARTESIAN_POINT('Ctrl Pts',(-19.7768950883246,-13.5479356467002,
116.569226136173)) ;
#182742 = CARTESIAN_POINT('Ctrl Pts',(-19.8506989282273,-13.5479357500039,
116.544995083774)) ;
#182743 = CARTESIAN_POINT('Ctrl Pts',(-19.8271835709341,-13.5390721929965,
116.473371097639)) ;
#182744 = CARTESIAN_POINT('Ctrl Pts',(-19.8146134378266,-13.2479213210197,
116.470556422711)) ;
#182745 = CARTESIAN_POINT('Ctrl Pts',(-19.7912065222546,-13.2593718199025,
116.399262732634)) ;
#182746 = CARTESIAN_POINT('Ctrl Pts',(-19.7174026738327,-13.2593717210079,
116.423493759085)) ;
#182747 = CARTESIAN_POINT('Ctrl Pts',(-19.6435988254109,-13.2593716221134,
116.447724785536)) ;
#182748 = CARTESIAN_POINT('Ctrl Pts',(-19.667005740983,-13.2479211232306,
116.519018475613)) ;
#182749 = CARTESIAN_POINT('Ctrl Pts',(-19.690412656555,-13.2364706243478,
116.59031216569)) ;
#182750 = CARTESIAN_POINT('Ctrl Pts',(-19.7642165049769,-13.2364707232423,
116.566081139239)) ;
#182751 = CARTESIAN_POINT('Ctrl Pts',(-19.8380203533987,-13.2364708221369,
116.541850112788)) ;
#182752 = CARTESIAN_POINT('Ctrl Pts',(-19.8146134378266,-13.2479213210197,
116.470556422711)) ;
#182753 = CARTESIAN_POINT('Ctrl Pts',(-19.7780274303114,-12.9689956696526,
116.394584966036)) ;
#182754 = CARTESIAN_POINT('Ctrl Pts',(-19.7564059267676,-12.9999372691398,
116.328729353013)) ;
#182755 = CARTESIAN_POINT('Ctrl Pts',(-19.6826020709247,-12.9999371823959,
116.352960356861)) ;
#182756 = CARTESIAN_POINT('Ctrl Pts',(-19.6087982150818,-12.9999370956519,
116.377191360708)) ;
#182757 = CARTESIAN_POINT('Ctrl Pts',(-19.6304197186256,-12.9689954961647,
116.443046973731)) ;
#182758 = CARTESIAN_POINT('Ctrl Pts',(-19.6520412221694,-12.9380538966775,
116.508902586753)) ;
#182759 = CARTESIAN_POINT('Ctrl Pts',(-19.7258450780123,-12.9380539834215,
116.484671582906)) ;
#182760 = CARTESIAN_POINT('Ctrl Pts',(-19.7996489338551,-12.9380540701654,
116.460440579058)) ;
#182761 = CARTESIAN_POINT('Ctrl Pts',(-19.7780274303114,-12.9689956696526,
116.394584966036)) ;
#182762 = CARTESIAN_POINT('Ctrl Pts',(-19.7192534733058,-12.7220961737177,
116.251055118297)) ;
#182763 = CARTESIAN_POINT('Ctrl Pts',(-19.7009686186426,-12.7703223930981,
116.195362399511)) ;
#182764 = CARTESIAN_POINT('Ctrl Pts',(-19.6271647572106,-12.7703223245763,
116.219593386335)) ;
#182765 = CARTESIAN_POINT('Ctrl Pts',(-19.5533608957786,-12.7703222560545,
116.243824373159)) ;
#182766 = CARTESIAN_POINT('Ctrl Pts',(-19.5716457504418,-12.7220960366741,
116.299517091945)) ;
#182767 = CARTESIAN_POINT('Ctrl Pts',(-19.589930605105,-12.6738698172937,
116.355209810731)) ;
#182768 = CARTESIAN_POINT('Ctrl Pts',(-19.663734466537,-12.6738698858155,
116.330978823907)) ;
#182769 = CARTESIAN_POINT('Ctrl Pts',(-19.737538327969,-12.6738699543374,
116.306747837083)) ;
#182770 = CARTESIAN_POINT('Ctrl Pts',(-19.7192534733058,-12.7220961737177,
116.251055118297)) ;
#182771 = CARTESIAN_POINT('Ctrl Pts',(-19.6419060205883,-12.5254520180373,
116.050893527524)) ;
#182772 = CARTESIAN_POINT('Ctrl Pts',(-19.6282608755407,-12.5874803484278,
116.009332615734)) ;
#182773 = CARTESIAN_POINT('Ctrl Pts',(-19.5544570106936,-12.5874803012304,
116.033563592156)) ;
#182774 = CARTESIAN_POINT('Ctrl Pts',(-19.4806531458465,-12.5874802540331,
116.057794568578)) ;
#182775 = CARTESIAN_POINT('Ctrl Pts',(-19.4942982908941,-12.5254519236426,
116.099355480369)) ;
#182776 = CARTESIAN_POINT('Ctrl Pts',(-19.5079434359418,-12.463423593252,
116.140916392159)) ;
#182777 = CARTESIAN_POINT('Ctrl Pts',(-19.5817473007888,-12.4634236404494,
116.116685415737)) ;
#182778 = CARTESIAN_POINT('Ctrl Pts',(-19.6555511656359,-12.4634236876467,
116.092454439314)) ;
#182779 = CARTESIAN_POINT('Ctrl Pts',(-19.6419060205883,-12.5254520180373,
116.050893527524)) ;
#182780 = CARTESIAN_POINT('Ctrl Pts',(-19.5507750838464,-12.3924871288094,
115.808727229059)) ;
#182781 = CARTESIAN_POINT('Ctrl Pts',(-19.5427394409189,-12.4638924990082,
115.784251955766)) ;
#182782 = CARTESIAN_POINT('Ctrl Pts',(-19.4689355748862,-12.4638924741093,
115.808482928577)) ;
#182783 = CARTESIAN_POINT('Ctrl Pts',(-19.3951317088534,-12.4638924492103,
115.832713901388)) ;
#182784 = CARTESIAN_POINT('Ctrl Pts',(-19.4031673517809,-12.3924870790115,
115.857189174681)) ;
#182785 = CARTESIAN_POINT('Ctrl Pts',(-19.4112029947084,-12.3210817088127,
115.881664447974)) ;
#182786 = CARTESIAN_POINT('Ctrl Pts',(-19.4850068607412,-12.3210817337116,
115.857433475163)) ;
#182787 = CARTESIAN_POINT('Ctrl Pts',(-19.5588107267739,-12.3210817586106,
115.833202502352)) ;
#182788 = CARTESIAN_POINT('Ctrl Pts',(-19.5507750838464,-12.3924871288094,
115.808727229059)) ;
#182789 = CARTESIAN_POINT('Ctrl Pts',(-19.4509678272437,-12.3327720085306,
115.540332649395)) ;
#182790 = CARTESIAN_POINT('Ctrl Pts',(-19.4491517888012,-12.4084551705648,
115.534801288009)) ;
#182791 = CARTESIAN_POINT('Ctrl Pts',(-19.3753479243441,-12.4084551665108,
115.55903226562)) ;
#182792 = CARTESIAN_POINT('Ctrl Pts',(-19.3015440598871,-12.4084551624567,
115.58326324323)) ;
#182793 = CARTESIAN_POINT('Ctrl Pts',(-19.3033600983296,-12.3327720004226,
115.588794604616)) ;
#182794 = CARTESIAN_POINT('Ctrl Pts',(-19.3051761367722,-12.2570888383885,
115.594325966001)) ;
#182795 = CARTESIAN_POINT('Ctrl Pts',(-19.3789800012292,-12.2570888424425,
115.570094988391)) ;
#182796 = CARTESIAN_POINT('Ctrl Pts',(-19.4527838656863,-12.2570888464965,
115.54586401078)) ;
#182797 = CARTESIAN_POINT('Ctrl Pts',(-19.4509678272437,-12.3327720085306,
115.540332649395)) ;
#182798 = CARTESIAN_POINT('Ctrl Pts',(-19.3501879158993,-12.3509988977752,
115.268703339782)) ;
#182799 = CARTESIAN_POINT('Ctrl Pts',(-19.35467457357,-12.4255237330698,115.282368973957)) ;
#182800 = CARTESIAN_POINT('Ctrl Pts',(-19.280870711689,-12.4255237455323,
115.306599959414)) ;
#182801 = CARTESIAN_POINT('Ctrl Pts',(-19.2070668498081,-12.4255237579948,
115.330830944871)) ;
#182802 = CARTESIAN_POINT('Ctrl Pts',(-19.2025801921374,-12.3509989227002,
115.317165310695)) ;
#182803 = CARTESIAN_POINT('Ctrl Pts',(-19.1980935344667,-12.2764740874057,
115.303499676519)) ;
#182804 = CARTESIAN_POINT('Ctrl Pts',(-19.2718973963476,-12.2764740749432,
115.279268691063)) ;
#182805 = CARTESIAN_POINT('Ctrl Pts',(-19.3457012582286,-12.2764740624807,
115.255037705606)) ;
#182806 = CARTESIAN_POINT('Ctrl Pts',(-19.3501879158993,-12.3509988977752,
115.268703339782)) ;
#182807 = CARTESIAN_POINT('Ctrl Pts',(-19.2537109950385,-12.4453838611795,
115.010328377215)) ;
#182808 = CARTESIAN_POINT('Ctrl Pts',(-19.2642064131177,-12.5134317382336,
115.042295726253)) ;
#182809 = CARTESIAN_POINT('Ctrl Pts',(-19.1904025553865,-12.5134317622461,
115.066526724349)) ;
#182810 = CARTESIAN_POINT('Ctrl Pts',(-19.1165986976553,-12.5134317862586,
115.090757722445)) ;
#182811 = CARTESIAN_POINT('Ctrl Pts',(-19.1061032795761,-12.4453839092044,
115.058790373407)) ;
#182812 = CARTESIAN_POINT('Ctrl Pts',(-19.0956078614969,-12.3773360321503,
115.026823024368)) ;
#182813 = CARTESIAN_POINT('Ctrl Pts',(-19.1694117192281,-12.3773360081379,
115.002592026272)) ;
#182814 = CARTESIAN_POINT('Ctrl Pts',(-19.2432155769593,-12.3773359841254,
114.978361028176)) ;
#182815 = CARTESIAN_POINT('Ctrl Pts',(-19.2537109950385,-12.4453838611795,
115.010328377215)) ;
#182816 = CARTESIAN_POINT('Ctrl Pts',(-19.1680396764701,-12.6100760699984,
114.78492817834)) ;
#182817 = CARTESIAN_POINT('Ctrl Pts',(-19.1837973550642,-12.6667282433853,
114.832923524027)) ;
#182818 = CARTESIAN_POINT('Ctrl Pts',(-19.109993502002,-12.6667282722992,
114.857154536344)) ;
#182819 = CARTESIAN_POINT('Ctrl Pts',(-19.0361896489399,-12.6667283012131,
114.881385548662)) ;
#182820 = CARTESIAN_POINT('Ctrl Pts',(-19.0204319703459,-12.6100761278262,
114.833390202975)) ;
#182821 = CARTESIAN_POINT('Ctrl Pts',(-19.0046742917518,-12.5534239544393,
114.785394857287)) ;
#182822 = CARTESIAN_POINT('Ctrl Pts',(-19.078478144814,-12.5534239255254,
114.76116384497)) ;
#182823 = CARTESIAN_POINT('Ctrl Pts',(-19.1522819978761,-12.5534238966115,
114.736932832653)) ;
#182824 = CARTESIAN_POINT('Ctrl Pts',(-19.1680396764701,-12.6100760699984,
114.78492817834)) ;
#182825 = CARTESIAN_POINT('Ctrl Pts',(-19.0989285208918,-12.8316470477012,
114.609808039742)) ;
#182826 = CARTESIAN_POINT('Ctrl Pts',(-19.1188033970976,-12.8729143960197,
114.670343705199)) ;
#182827 = CARTESIAN_POINT('Ctrl Pts',(-19.0449995481209,-12.8729144255077,
114.694574729961)) ;
#182828 = CARTESIAN_POINT('Ctrl Pts',(-18.9711956991442,-12.8729144549957,
114.718805754722)) ;
#182829 = CARTESIAN_POINT('Ctrl Pts',(-18.9513208229384,-12.8316471066773,
114.658270089265)) ;
#182830 = CARTESIAN_POINT('Ctrl Pts',(-18.9314459467326,-12.7903797583588,
114.597734423807)) ;
#182831 = CARTESIAN_POINT('Ctrl Pts',(-19.0052497957093,-12.7903797288708,
114.573503399046)) ;
#182832 = CARTESIAN_POINT('Ctrl Pts',(-19.079053644686,-12.7903796993828,
114.549272374285)) ;
#182833 = CARTESIAN_POINT('Ctrl Pts',(-19.0989285208918,-12.8316470477012,
114.609808039742)) ;
#182834 = CARTESIAN_POINT('Ctrl Pts',(-19.0499531759888,-13.0973555362981,
114.496308559562)) ;
#182835 = CARTESIAN_POINT('Ctrl Pts',(-19.0725398327684,-13.1201328482756,
114.5651038713)) ;
#182836 = CARTESIAN_POINT('Ctrl Pts',(-18.9987359873466,-13.1201328716907,
114.589334906889)) ;
#182837 = CARTESIAN_POINT('Ctrl Pts',(-18.9249321419248,-13.1201328951058,
114.613565942478)) ;
#182838 = CARTESIAN_POINT('Ctrl Pts',(-18.9023454851452,-13.0973555831283,
114.54477063074)) ;
#182839 = CARTESIAN_POINT('Ctrl Pts',(-18.8797588283656,-13.0745782711508,
114.475975319001)) ;
#182840 = CARTESIAN_POINT('Ctrl Pts',(-18.9535626737874,-13.0745782477357,
114.451744283413)) ;
#182841 = CARTESIAN_POINT('Ctrl Pts',(-19.0273665192092,-13.0745782243206,
114.427513247824)) ;
#182842 = CARTESIAN_POINT('Ctrl Pts',(-19.0499531759888,-13.0973555362981,
114.496308559562)) ;
#182843 = CARTESIAN_POINT('Ctrl Pts',(-19.0246223482772,-13.3829827267331,
114.454418834067)) ;
#182844 = CARTESIAN_POINT('Ctrl Pts',(-19.0482819521427,-13.3858507921175,
114.526482169625)) ;
#182845 = CARTESIAN_POINT('Ctrl Pts',(-18.9744781087354,-13.3858508103817,
114.55071321135)) ;
#182846 = CARTESIAN_POINT('Ctrl Pts',(-18.9006742653281,-13.3858508286459,
114.574944253074)) ;
#182847 = CARTESIAN_POINT('Ctrl Pts',(-18.8770146614626,-13.3829827632615,
114.502880917516)) ;
#182848 = CARTESIAN_POINT('Ctrl Pts',(-18.8533550575971,-13.380114697877,
114.430817581958)) ;
#182849 = CARTESIAN_POINT('Ctrl Pts',(-18.9271589010044,-13.3801146796128,
114.406586540234)) ;
#182850 = CARTESIAN_POINT('Ctrl Pts',(-19.0009627444117,-13.3801146613487,
114.382355498509)) ;
#182851 = CARTESIAN_POINT('Ctrl Pts',(-19.0246223482772,-13.3829827267331,
114.454418834067)) ;
#182852 = CARTESIAN_POINT('Ctrl Pts',(-19.0233599186535,-13.6735145155205,
114.486149491012)) ;
#182853 = CARTESIAN_POINT('Ctrl Pts',(-19.0464072958713,-13.6561003398034,
114.556348083136)) ;
#182854 = CARTESIAN_POINT('Ctrl Pts',(-18.9726034534189,-13.6561003497692,
114.580579127769)) ;
#182855 = CARTESIAN_POINT('Ctrl Pts',(-18.8987996109665,-13.656100359735,
114.604810172402)) ;
#182856 = CARTESIAN_POINT('Ctrl Pts',(-18.8757522337487,-13.673514535452,
114.534611580278)) ;
#182857 = CARTESIAN_POINT('Ctrl Pts',(-18.8527048565308,-13.690928711169,
114.464412988154)) ;
#182858 = CARTESIAN_POINT('Ctrl Pts',(-18.9265086989832,-13.6909287012033,
114.440181943521)) ;
#182859 = CARTESIAN_POINT('Ctrl Pts',(-19.0003125414356,-13.6909286912375,
114.415950898888)) ;
#182860 = CARTESIAN_POINT('Ctrl Pts',(-19.0233599186535,-13.6735145155205,
114.486149491012)) ;
#182861 = CARTESIAN_POINT('Ctrl Pts',(-19.0457709783456,-13.9443960540442,
114.589809022558)) ;
#182862 = CARTESIAN_POINT('Ctrl Pts',(-19.0665555634341,-13.9080411308625,
114.65311551506)) ;
#182863 = CARTESIAN_POINT('Ctrl Pts',(-18.9927517208893,-13.9080411350017,
114.677346559412)) ;
#182864 = CARTESIAN_POINT('Ctrl Pts',(-18.9189478783444,-13.9080411391408,
114.701577603763)) ;
#182865 = CARTESIAN_POINT('Ctrl Pts',(-18.898163293256,-13.9443960623225,
114.638271111261)) ;
#182866 = CARTESIAN_POINT('Ctrl Pts',(-18.8773787081675,-13.9807509855041,
114.574964618758)) ;
#182867 = CARTESIAN_POINT('Ctrl Pts',(-18.9511825507123,-13.980750981365,
114.550733574406)) ;
#182868 = CARTESIAN_POINT('Ctrl Pts',(-19.0249863932572,-13.9807509772258,
114.526502530055)) ;
#182869 = CARTESIAN_POINT('Ctrl Pts',(-19.0457709783456,-13.9443960540442,
114.589809022558)) ;
#182870 = CARTESIAN_POINT('Ctrl Pts',(-19.0894428117511,-14.1780473237906,
114.75829138369)) ;
#182871 = CARTESIAN_POINT('Ctrl Pts',(-19.1064751505177,-14.125322660068,
114.810169139406)) ;
#182872 = CARTESIAN_POINT('Ctrl Pts',(-19.0326713072854,-14.12532266015,114.834400181664)) ;
#182873 = CARTESIAN_POINT('Ctrl Pts',(-18.9588674640532,-14.1253226602321,
114.858631223921)) ;
#182874 = CARTESIAN_POINT('Ctrl Pts',(-18.9418351252866,-14.1780473239547,
114.806753468205)) ;
#182875 = CARTESIAN_POINT('Ctrl Pts',(-18.9248027865201,-14.2307719876773,
114.754875712489)) ;
#182876 = CARTESIAN_POINT('Ctrl Pts',(-18.9986066297524,-14.2307719875953,
114.730644670231)) ;
#182877 = CARTESIAN_POINT('Ctrl Pts',(-19.0724104729846,-14.2307719875132,
114.706413627973)) ;
#182878 = CARTESIAN_POINT('Ctrl Pts',(-19.0894428117511,-14.1780473237906,
114.75829138369)) ;
#182879 = CARTESIAN_POINT('Ctrl Pts',(-19.1503829732197,-14.3571729772058,
114.97930953691)) ;
#182880 = CARTESIAN_POINT('Ctrl Pts',(-19.1624527588711,-14.2918617658065,
115.016072156599)) ;
#182881 = CARTESIAN_POINT('Ctrl Pts',(-19.088648914819,-14.2918617643923,
115.04030319636)) ;
#182882 = CARTESIAN_POINT('Ctrl Pts',(-19.0148450707669,-14.291861762978,
115.064534236121)) ;
#182883 = CARTESIAN_POINT('Ctrl Pts',(-19.0027752851155,-14.3571729743773,
115.027771616431)) ;
#182884 = CARTESIAN_POINT('Ctrl Pts',(-18.9907054994641,-14.4224841857766,
114.991008996742)) ;
#182885 = CARTESIAN_POINT('Ctrl Pts',(-19.0645093435162,-14.4224841871909,
114.966777956981)) ;
#182886 = CARTESIAN_POINT('Ctrl Pts',(-19.1383131875683,-14.4224841886051,
114.942546917221)) ;
#182887 = CARTESIAN_POINT('Ctrl Pts',(-19.1503829732197,-14.3571729772058,
114.97930953691)) ;
#182888 = CARTESIAN_POINT('Ctrl Pts',(-19.2242001392869,-14.4697035049953,
115.239834214336)) ;
#182889 = CARTESIAN_POINT('Ctrl Pts',(-19.2303944994986,-14.3964364704153,
115.258701236151)) ;
#182890 = CARTESIAN_POINT('Ctrl Pts',(-19.1565906550596,-14.3964364695808,
115.282932274733)) ;
#182891 = CARTESIAN_POINT('Ctrl Pts',(-19.0827868106205,-14.3964364687462,
115.307163313314)) ;
#182892 = CARTESIAN_POINT('Ctrl Pts',(-19.0765924504088,-14.4697035033262,
115.2882962915)) ;
#182893 = CARTESIAN_POINT('Ctrl Pts',(-19.0703980901972,-14.5429705379062,
115.269429269686)) ;
#182894 = CARTESIAN_POINT('Ctrl Pts',(-19.1442019346362,-14.5429705387408,
115.245198231104)) ;
#182895 = CARTESIAN_POINT('Ctrl Pts',(-19.2180057790753,-14.5429705395753,
115.220967192522)) ;
#182896 = CARTESIAN_POINT('Ctrl Pts',(-19.2242001392869,-14.4697035049953,
115.239834214336)) ;
#182897 = CARTESIAN_POINT('Ctrl Pts',(-19.3035102564175,-14.5058316151569,
115.516726782394)) ;
#182898 = CARTESIAN_POINT('Ctrl Pts',(-19.3034446215456,-14.4299343068103,
115.5165268692)) ;
#182899 = CARTESIAN_POINT('Ctrl Pts',(-19.2296407775637,-14.4299343070279,
115.540757909174)) ;
#182900 = CARTESIAN_POINT('Ctrl Pts',(-19.1558369335817,-14.4299343072455,
115.564988949148)) ;
#182901 = CARTESIAN_POINT('Ctrl Pts',(-19.1559025684536,-14.5058316155922,
115.565188862343)) ;
#182902 = CARTESIAN_POINT('Ctrl Pts',(-19.1559682033254,-14.5817289239388,
115.565388775537)) ;
#182903 = CARTESIAN_POINT('Ctrl Pts',(-19.2297720473073,-14.5817289237212,
115.541157735563)) ;
#182904 = CARTESIAN_POINT('Ctrl Pts',(-19.3035758912893,-14.5817289235035,
115.516926695588)) ;
#182905 = CARTESIAN_POINT('Ctrl Pts',(-19.3035102564175,-14.5058316151569,
115.516726782394)) ;
#182906 = CARTESIAN_POINT('Ctrl Pts',(-19.3827642308923,-14.4647781183691,
115.793520482864)) ;
#182907 = CARTESIAN_POINT('Ctrl Pts',(-19.3764319338488,-14.3916362177671,
115.774233327761)) ;
#182908 = CARTESIAN_POINT('Ctrl Pts',(-19.3026280907892,-14.3916362178144,
115.798464370545)) ;
#182909 = CARTESIAN_POINT('Ctrl Pts',(-19.2288242477297,-14.3916362178617,
115.822695413328)) ;
#182910 = CARTESIAN_POINT('Ctrl Pts',(-19.2351565447731,-14.4647781184637,
115.841982568431)) ;
#182911 = CARTESIAN_POINT('Ctrl Pts',(-19.2414888418166,-14.5379200190658,
115.861269723533)) ;
#182912 = CARTESIAN_POINT('Ctrl Pts',(-19.3152926848761,-14.5379200190184,
115.83703868075)) ;
#182913 = CARTESIAN_POINT('Ctrl Pts',(-19.3890965279357,-14.5379200189711,
115.812807637966)) ;
#182914 = CARTESIAN_POINT('Ctrl Pts',(-19.3827642308923,-14.4647781183691,
115.793520482864)) ;
#182915 = CARTESIAN_POINT('Ctrl Pts',(-19.4555982839664,-14.3484987257117,
116.050853216229)) ;
#182916 = CARTESIAN_POINT('Ctrl Pts',(-19.4434365510196,-14.2833691759875,
116.013810539845)) ;
#182917 = CARTESIAN_POINT('Ctrl Pts',(-19.3696327093056,-14.2833691732841,
116.038041586727)) ;
#182918 = CARTESIAN_POINT('Ctrl Pts',(-19.2958288675915,-14.2833691705807,
116.062272633608)) ;
#182919 = CARTESIAN_POINT('Ctrl Pts',(-19.3079906005384,-14.3484987203049,
116.099315309993)) ;
#182920 = CARTESIAN_POINT('Ctrl Pts',(-19.3201523334852,-14.4136282700291,
116.136357986378)) ;
#182921 = CARTESIAN_POINT('Ctrl Pts',(-19.3939561751992,-14.4136282727325,
116.112126939496)) ;
#182922 = CARTESIAN_POINT('Ctrl Pts',(-19.4677600169133,-14.4136282754358,
116.087895892614)) ;
#182923 = CARTESIAN_POINT('Ctrl Pts',(-19.4555982839664,-14.3484987257117,
116.050853216229)) ;
#182924 = CARTESIAN_POINT('Ctrl Pts',(-19.5158156777424,-14.1655053892491,
116.26975198964)) ;
#182925 = CARTESIAN_POINT('Ctrl Pts',(-19.4986972476325,-14.1130583565086,
116.217612013334)) ;
#182926 = CARTESIAN_POINT('Ctrl Pts',(-19.4248934070266,-14.1130583479537,
116.241843063591)) ;
#182927 = CARTESIAN_POINT('Ctrl Pts',(-19.3510895664207,-14.1130583393988,
116.266074113848)) ;
#182928 = CARTESIAN_POINT('Ctrl Pts',(-19.3682079965306,-14.1655053721393,
116.318214090154)) ;
#182929 = CARTESIAN_POINT('Ctrl Pts',(-19.3853264266405,-14.2179524048798,
116.370354066459)) ;
#182930 = CARTESIAN_POINT('Ctrl Pts',(-19.4591302672464,-14.2179524134347,
116.346123016202)) ;
#182931 = CARTESIAN_POINT('Ctrl Pts',(-19.5329341078523,-14.2179524219896,
116.321891965945)) ;
#182932 = CARTESIAN_POINT('Ctrl Pts',(-19.5158156777424,-14.1655053892491,
116.26975198964)) ;
#182933 = CARTESIAN_POINT('Ctrl Pts',(-19.5583308176863,-13.9286208259661,
116.434763630565)) ;
#182934 = CARTESIAN_POINT('Ctrl Pts',(-19.537483987011,-13.8926376196403,
116.371267547564)) ;
#182935 = CARTESIAN_POINT('Ctrl Pts',(-19.4636801467042,-13.8926376022121,
116.395498598732)) ;
#182936 = CARTESIAN_POINT('Ctrl Pts',(-19.3898763063974,-13.8926375847838,
116.4197296499)) ;
#182937 = CARTESIAN_POINT('Ctrl Pts',(-19.4107231370728,-13.9286207911095,
116.483225732902)) ;
#182938 = CARTESIAN_POINT('Ctrl Pts',(-19.4315699677482,-13.9646039974353,
116.546721815903)) ;
#182939 = CARTESIAN_POINT('Ctrl Pts',(-19.5053738080549,-13.9646040148635,
116.522490764735)) ;
#182940 = CARTESIAN_POINT('Ctrl Pts',(-19.5791776483617,-13.9646040322918,
116.498259713567)) ;
#182941 = CARTESIAN_POINT('Ctrl Pts',(-19.5583308176863,-13.9286208259661,
116.434763630565)) ;
#182942 = CARTESIAN_POINT('Ctrl Pts',(-19.5793222342617,-13.6565946963034,
116.5340328038)) ;
#182943 = CARTESIAN_POINT('Ctrl Pts',(-19.5562485424584,-13.6395527561257,
116.463754060976)) ;
#182944 = CARTESIAN_POINT('Ctrl Pts',(-19.4824447011078,-13.6395527301396,
116.487985108965)) ;
#182945 = CARTESIAN_POINT('Ctrl Pts',(-19.4086408597573,-13.6395527041535,
116.512216156954)) ;
#182946 = CARTESIAN_POINT('Ctrl Pts',(-19.4317145515606,-13.6565946443312,
116.582494899778)) ;
#182947 = CARTESIAN_POINT('Ctrl Pts',(-19.4547882433639,-13.6736365845089,
116.652773642602)) ;
#182948 = CARTESIAN_POINT('Ctrl Pts',(-19.5285920847144,-13.673636610495,
116.628542594613)) ;
#182949 = CARTESIAN_POINT('Ctrl Pts',(-19.6023959260649,-13.6736366364811,
116.604311546624)) ;
#182950 = CARTESIAN_POINT('Ctrl Pts',(-19.5793222342617,-13.6565946963034,
116.5340328038)) ;
#182951 = CARTESIAN_POINT('Ctrl Pts',(-19.5766443908906,-13.3650274692435,
116.561521687916)) ;
#182952 = CARTESIAN_POINT('Ctrl Pts',(-19.5529865212982,-13.3683183370286,
116.489463633607)) ;
#182953 = CARTESIAN_POINT('Ctrl Pts',(-19.4791826776011,-13.368318300107,
116.513694674449)) ;
#182954 = CARTESIAN_POINT('Ctrl Pts',(-19.4053788339039,-13.3683182631854,
116.537925715291)) ;
#182955 = CARTESIAN_POINT('Ctrl Pts',(-19.4290367034963,-13.3650273954003,
116.6099837696)) ;
#182956 = CARTESIAN_POINT('Ctrl Pts',(-19.4526945730887,-13.3617365276153,
116.682041823909)) ;
#182957 = CARTESIAN_POINT('Ctrl Pts',(-19.5264984167859,-13.3617365645369,
116.657810783067)) ;
#182958 = CARTESIAN_POINT('Ctrl Pts',(-19.6003022604831,-13.3617366014585,
116.633579742225)) ;
#182959 = CARTESIAN_POINT('Ctrl Pts',(-19.5766443908906,-13.3650274692435,
116.561521687916)) ;
#182960 = CARTESIAN_POINT('Ctrl Pts',(-19.5495669925005,-13.0788343995772,
116.514498473725)) ;
#182961 = CARTESIAN_POINT('Ctrl Pts',(-19.5270319383932,-13.1021119946019,
116.445860334053)) ;
#182962 = CARTESIAN_POINT('Ctrl Pts',(-19.4532280907541,-13.1021119511676,
116.470091362888)) ;
#182963 = CARTESIAN_POINT('Ctrl Pts',(-19.379424243115,-13.1021119077334,
116.494322391723)) ;
#182964 = CARTESIAN_POINT('Ctrl Pts',(-19.4019592972223,-13.0788343127088,
116.562960531395)) ;
#182965 = CARTESIAN_POINT('Ctrl Pts',(-19.4244943513295,-13.0555567176841,
116.631598671068)) ;
#182966 = CARTESIAN_POINT('Ctrl Pts',(-19.4982981989686,-13.0555567611183,
116.607367642232)) ;
#182967 = CARTESIAN_POINT('Ctrl Pts',(-19.5721020466077,-13.0555568045526,
116.583136613397)) ;
#182968 = CARTESIAN_POINT('Ctrl Pts',(-19.5495669925005,-13.0788343995772,
116.514498473725)) ;
#182969 = CARTESIAN_POINT('Ctrl Pts',(-19.4996422792964,-12.8175211583994,
116.397794021949)) ;
#182970 = CARTESIAN_POINT('Ctrl Pts',(-19.4798288097377,-12.8590768776832,
116.337445389538)) ;
#182971 = CARTESIAN_POINT('Ctrl Pts',(-19.4060249573596,-12.8590768329722,
116.361676403939)) ;
#182972 = CARTESIAN_POINT('Ctrl Pts',(-19.3322211049816,-12.8590767882613,
116.38590741834)) ;
#182973 = CARTESIAN_POINT('Ctrl Pts',(-19.3520345745402,-12.8175210689774,
116.446256050751)) ;
#182974 = CARTESIAN_POINT('Ctrl Pts',(-19.3718480440989,-12.7759653496935,
116.506604683163)) ;
#182975 = CARTESIAN_POINT('Ctrl Pts',(-19.445651896477,-12.7759653944045,
116.482373668762)) ;
#182976 = CARTESIAN_POINT('Ctrl Pts',(-19.519455748855,-12.7759654391155,
116.458142654361)) ;
#182977 = CARTESIAN_POINT('Ctrl Pts',(-19.4996422792964,-12.8175211583994,
116.397794021949)) ;
#182978 = CARTESIAN_POINT('Ctrl Pts',(-19.4293404722098,-12.5984995679009,
116.219119607498)) ;
#182979 = CARTESIAN_POINT('Ctrl Pts',(-19.4136731235186,-12.6554070787726,
116.171399390111)) ;
#182980 = CARTESIAN_POINT('Ctrl Pts',(-19.3398692657786,-12.6554070377801,
116.195630388181)) ;
#182981 = CARTESIAN_POINT('Ctrl Pts',(-19.2660654080387,-12.6554069967877,
116.21986138625)) ;
#182982 = CARTESIAN_POINT('Ctrl Pts',(-19.2817327567299,-12.5984994859161,
116.267581603637)) ;
#182983 = CARTESIAN_POINT('Ctrl Pts',(-19.2974001054211,-12.5415919750444,
116.315301821023)) ;
#182984 = CARTESIAN_POINT('Ctrl Pts',(-19.3712039631611,-12.5415920160368,
116.291070822954)) ;
#182985 = CARTESIAN_POINT('Ctrl Pts',(-19.445007820901,-12.5415920570292,
116.266839824884)) ;
#182986 = CARTESIAN_POINT('Ctrl Pts',(-19.4293404722098,-12.5984995679009,
116.219119607498)) ;
#182987 = CARTESIAN_POINT('Ctrl Pts',(-19.3431976343271,-12.4381081950322,
115.992149215875)) ;
#182988 = CARTESIAN_POINT('Ctrl Pts',(-19.3327893138113,-12.5062960463662,
115.960447149621)) ;
#182989 = CARTESIAN_POINT('Ctrl Pts',(-19.2589854510198,-12.5062960154841,
115.984678132304)) ;
#182990 = CARTESIAN_POINT('Ctrl Pts',(-19.1851815882283,-12.506295984602,
116.008909114987)) ;
#182991 = CARTESIAN_POINT('Ctrl Pts',(-19.1955899087441,-12.4381081332681,
116.040611181242)) ;
#182992 = CARTESIAN_POINT('Ctrl Pts',(-19.2059982292598,-12.3699202819341,
116.072313247497)) ;
#182993 = CARTESIAN_POINT('Ctrl Pts',(-19.2798020920513,-12.3699203128162,
116.048082264814)) ;
#182994 = CARTESIAN_POINT('Ctrl Pts',(-19.3536059548428,-12.3699203436983,
116.02385128213)) ;
#182995 = CARTESIAN_POINT('Ctrl Pts',(-19.3431976343271,-12.4381081950322,
115.992149215875)) ;
#182996 = CARTESIAN_POINT('Ctrl Pts',(-19.2456411710222,-12.3474840033873,
115.730719198245)) ;
#182997 = CARTESIAN_POINT('Ctrl Pts',(-19.2412898424851,-12.4220984887537,
115.717465752075)) ;
#182998 = CARTESIAN_POINT('Ctrl Pts',(-19.1674859748129,-12.4220984739895,
115.741696719893)) ;
#182999 = CARTESIAN_POINT('Ctrl Pts',(-19.0936821071408,-12.4220984592253,
115.76592768771)) ;
#183000 = CARTESIAN_POINT('Ctrl Pts',(-19.0980334356779,-12.3474839738589,
115.779181133881)) ;
#183001 = CARTESIAN_POINT('Ctrl Pts',(-19.1023847642151,-12.2728694884925,
115.792434580051)) ;
#183002 = CARTESIAN_POINT('Ctrl Pts',(-19.1761886318872,-12.2728695032567,
115.768203612233)) ;
#183003 = CARTESIAN_POINT('Ctrl Pts',(-19.2499924995594,-12.2728695180209,
115.743972644416)) ;
#183004 = CARTESIAN_POINT('Ctrl Pts',(-19.2456411710222,-12.3474840033873,
115.730719198245)) ;
#183005 = CARTESIAN_POINT('Ctrl Pts',(-19.1449743145035,-12.3342746176406,
115.45936107608)) ;
#183006 = CARTESIAN_POINT('Ctrl Pts',(-19.1469154659611,-12.4099190416296,
115.465273508583)) ;
#183007 = CARTESIAN_POINT('Ctrl Pts',(-19.0731115962662,-12.4099190485564,
115.489504470239)) ;
#183008 = CARTESIAN_POINT('Ctrl Pts',(-18.9993077265714,-12.4099190554831,
115.513735431896)) ;
#183009 = CARTESIAN_POINT('Ctrl Pts',(-18.9973665751139,-12.3342746314941,
115.507822999394)) ;
#183010 = CARTESIAN_POINT('Ctrl Pts',(-18.9954254236563,-12.2586302075051,
115.501910566892)) ;
#183011 = CARTESIAN_POINT('Ctrl Pts',(-19.0692292933512,-12.2586302005783,
115.477679605235)) ;
#183012 = CARTESIAN_POINT('Ctrl Pts',(-19.143033163046,-12.2586301936515,
115.453448643578)) ;
#183013 = CARTESIAN_POINT('Ctrl Pts',(-19.1449743145035,-12.3342746176406,
115.45936107608)) ;
#183014 = CARTESIAN_POINT('Ctrl Pts',(-19.0456937210243,-12.3983523506611,
115.192496748361)) ;
#183015 = CARTESIAN_POINT('Ctrl Pts',(-19.0538339702952,-12.4696333213927,
115.21729063245)) ;
#183016 = CARTESIAN_POINT('Ctrl Pts',(-18.9800301001254,-12.4696333527669,
115.24152159266)) ;
#183017 = CARTESIAN_POINT('Ctrl Pts',(-18.9062262299556,-12.4696333841411,
115.26575255287)) ;
#183018 = CARTESIAN_POINT('Ctrl Pts',(-18.8980859806847,-12.3983524134095,
115.240958668781)) ;
#183019 = CARTESIAN_POINT('Ctrl Pts',(-18.8899457314137,-12.3270714426779,
115.216164784692)) ;
#183020 = CARTESIAN_POINT('Ctrl Pts',(-18.9637496015835,-12.3270714113037,
115.191933824481)) ;
#183021 = CARTESIAN_POINT('Ctrl Pts',(-19.0375534717533,-12.3270713799295,
115.167702864271)) ;
#183022 = CARTESIAN_POINT('Ctrl Pts',(-19.0456937210243,-12.3983523506611,
115.192496748361)) ;
#183023 = CARTESIAN_POINT('Ctrl Pts',(-18.9551049831602,-12.5353914606374,
114.952015661837)) ;
#183024 = CARTESIAN_POINT('Ctrl Pts',(-18.9688484070963,-12.5972087494759,
114.993875911784)) ;
#183025 = CARTESIAN_POINT('Ctrl Pts',(-18.8950445391368,-12.5972088056809,
115.018106878726)) ;
#183026 = CARTESIAN_POINT('Ctrl Pts',(-18.8212406711773,-12.5972088618859,
115.042337845668)) ;
#183027 = CARTESIAN_POINT('Ctrl Pts',(-18.8074972472412,-12.5353915730474,
115.000477595721)) ;
#183028 = CARTESIAN_POINT('Ctrl Pts',(-18.7937538233051,-12.4735742842089,
114.958617345773)) ;
#183029 = CARTESIAN_POINT('Ctrl Pts',(-18.8675576912646,-12.4735742280039,
114.934386378831)) ;
#183030 = CARTESIAN_POINT('Ctrl Pts',(-18.9413615592241,-12.4735741717989,
114.910155411889)) ;
#183031 = CARTESIAN_POINT('Ctrl Pts',(-18.9551049831602,-12.5353914606374,
114.952015661837)) ;
#183032 = CARTESIAN_POINT('Ctrl Pts',(-18.8783820413473,-12.7368848040207,
114.753966045534)) ;
#183033 = CARTESIAN_POINT('Ctrl Pts',(-18.8967647782412,-12.7847255574639,
114.8099568941)) ;
#183034 = CARTESIAN_POINT('Ctrl Pts',(-18.8229609148592,-12.7847256367286,
114.834187874984)) ;
#183035 = CARTESIAN_POINT('Ctrl Pts',(-18.7491570514771,-12.7847257159933,
114.858418855869)) ;
#183036 = CARTESIAN_POINT('Ctrl Pts',(-18.7307743145832,-12.7368849625501,
114.802428007303)) ;
#183037 = CARTESIAN_POINT('Ctrl Pts',(-18.7123915776892,-12.6890442091069,
114.746437158737)) ;
#183038 = CARTESIAN_POINT('Ctrl Pts',(-18.7861954410713,-12.6890441298422,
114.722206177853)) ;
#183039 = CARTESIAN_POINT('Ctrl Pts',(-18.8599993044534,-12.6890440505775,
114.697975196968)) ;
#183040 = CARTESIAN_POINT('Ctrl Pts',(-18.8783820413473,-12.7368848040207,
114.753966045534)) ;
#183041 = CARTESIAN_POINT('Ctrl Pts',(-18.8212505018881,-12.9849643669818,
114.615234103962)) ;
#183042 = CARTESIAN_POINT('Ctrl Pts',(-18.8429187755215,-13.0155548424745,
114.681232167266)) ;
#183043 = CARTESIAN_POINT('Ctrl Pts',(-18.7691149190821,-13.0155549383142,
114.705463169296)) ;
#183044 = CARTESIAN_POINT('Ctrl Pts',(-18.6953110626427,-13.0155550341539,
114.729694171327)) ;
#183045 = CARTESIAN_POINT('Ctrl Pts',(-18.6736427890092,-12.9849645586612,
114.663696108023)) ;
#183046 = CARTESIAN_POINT('Ctrl Pts',(-18.6519745153757,-12.9543740831685,
114.597698044719)) ;
#183047 = CARTESIAN_POINT('Ctrl Pts',(-18.7257783718151,-12.9543739873288,
114.573467042688)) ;
#183048 = CARTESIAN_POINT('Ctrl Pts',(-18.7995822282546,-12.9543738914891,
114.549236040658)) ;
#183049 = CARTESIAN_POINT('Ctrl Pts',(-18.8212505018881,-12.9849643669818,
114.615234103962)) ;
#183050 = CARTESIAN_POINT('Ctrl Pts',(-18.785989087223,-13.2657001242146,
114.543367393447)) ;
#183051 = CARTESIAN_POINT('Ctrl Pts',(-18.8094158544499,-13.2767359206685,
114.614721544454)) ;
#183052 = CARTESIAN_POINT('Ctrl Pts',(-18.7356120063235,-13.2767360267194,
114.638952571805)) ;
#183053 = CARTESIAN_POINT('Ctrl Pts',(-18.6618081581972,-13.2767361327703,
114.663183599156)) ;
#183054 = CARTESIAN_POINT('Ctrl Pts',(-18.6383813909702,-13.2657003363164,
114.591829448148)) ;
#183055 = CARTESIAN_POINT('Ctrl Pts',(-18.6149546237433,-13.2546645398624,
114.52047529714)) ;
#183056 = CARTESIAN_POINT('Ctrl Pts',(-18.6887584718697,-13.2546644338116,
114.496244269789)) ;
#183057 = CARTESIAN_POINT('Ctrl Pts',(-18.762562319996,-13.2546643277607,
114.472013242439)) ;
#183058 = CARTESIAN_POINT('Ctrl Pts',(-18.785989087223,-13.2657001242146,
114.543367393447)) ;
#183059 = CARTESIAN_POINT('Ctrl Pts',(-18.7749409518522,-13.5562446654925,
114.545103589634)) ;
#183060 = CARTESIAN_POINT('Ctrl Pts',(-18.7984413535009,-13.5470119024509,
114.616682019189)) ;
#183061 = CARTESIAN_POINT('Ctrl Pts',(-18.7246375143752,-13.5470120097675,
114.640913073955)) ;
#183062 = CARTESIAN_POINT('Ctrl Pts',(-18.6508336752495,-13.5470121170841,
114.66514412872)) ;
#183063 = CARTESIAN_POINT('Ctrl Pts',(-18.6273332736008,-13.5562448801257,
114.593565699165)) ;
#183064 = CARTESIAN_POINT('Ctrl Pts',(-18.6038328719521,-13.5654776431673,
114.52198726961)) ;
#183065 = CARTESIAN_POINT('Ctrl Pts',(-18.6776367110778,-13.5654775358507,
114.497756214844)) ;
#183066 = CARTESIAN_POINT('Ctrl Pts',(-18.7514405502036,-13.5654774285341,
114.473525160079)) ;
#183067 = CARTESIAN_POINT('Ctrl Pts',(-18.7749409518522,-13.5562446654925,
114.545103589634)) ;
#183068 = CARTESIAN_POINT('Ctrl Pts',(-18.7878772786409,-13.837740260252,
114.619989429758)) ;
#183069 = CARTESIAN_POINT('Ctrl Pts',(-18.8097751113286,-13.8088409661864,
114.686686692827)) ;
#183070 = CARTESIAN_POINT('Ctrl Pts',(-18.7359712810008,-13.8088410662031,
114.710917774389)) ;
#183071 = CARTESIAN_POINT('Ctrl Pts',(-18.6621674506729,-13.8088411662199,
114.735148855951)) ;
#183072 = CARTESIAN_POINT('Ctrl Pts',(-18.6402696179852,-13.8377404602855,
114.668451592882)) ;
#183073 = CARTESIAN_POINT('Ctrl Pts',(-18.6183717852975,-13.8666397543512,
114.601754329814)) ;
#183074 = CARTESIAN_POINT('Ctrl Pts',(-18.6921756156254,-13.8666396543344,
114.577523248252)) ;
#183075 = CARTESIAN_POINT('Ctrl Pts',(-18.7659794459532,-13.8666395543177,
114.553292166689)) ;
#183076 = CARTESIAN_POINT('Ctrl Pts',(-18.7878772786409,-13.837740260252,
114.619989429758)) ;
#183077 = CARTESIAN_POINT('Ctrl Pts',(-18.823586104698,-14.0900089023239,
114.76439949876)) ;
#183078 = CARTESIAN_POINT('Ctrl Pts',(-18.8422860154947,-14.0434540249531,
114.821356407761)) ;
#183079 = CARTESIAN_POINT('Ctrl Pts',(-18.7684821927334,-14.0434541089459,
114.845587512369)) ;
#183080 = CARTESIAN_POINT('Ctrl Pts',(-18.694678369972,-14.0434541929387,
114.869818616978)) ;
#183081 = CARTESIAN_POINT('Ctrl Pts',(-18.6759784591753,-14.0900090703095,
114.812861707977)) ;
#183082 = CARTESIAN_POINT('Ctrl Pts',(-18.6572785483786,-14.1365639476803,
114.755904798977)) ;
#183083 = CARTESIAN_POINT('Ctrl Pts',(-18.73108237114,-14.1365638636875,114.731673694368)) ;
#183084 = CARTESIAN_POINT('Ctrl Pts',(-18.8048861939013,-14.1365637796947,
114.70744258976)) ;
#183085 = CARTESIAN_POINT('Ctrl Pts',(-18.823586104698,-14.0900089023239,
114.76439949876)) ;
#183086 = CARTESIAN_POINT('Ctrl Pts',(-18.8778061466655,-14.2916996646196,
114.964766086765)) ;
#183087 = CARTESIAN_POINT('Ctrl Pts',(-18.8920194354158,-14.2309943169081,
115.008057468957)) ;
#183088 = CARTESIAN_POINT('Ctrl Pts',(-18.8182156184406,-14.230994379438,
115.03228859119)) ;
#183089 = CARTESIAN_POINT('Ctrl Pts',(-18.7444118014655,-14.2309944419679,
115.056519713422)) ;
#183090 = CARTESIAN_POINT('Ctrl Pts',(-18.7301985127151,-14.2916997896794,
115.01322833123)) ;
#183091 = CARTESIAN_POINT('Ctrl Pts',(-18.7159852239648,-14.3524051373909,
114.969936949037)) ;
#183092 = CARTESIAN_POINT('Ctrl Pts',(-18.7897890409399,-14.352405074861,
114.945705826805)) ;
#183093 = CARTESIAN_POINT('Ctrl Pts',(-18.8635928579151,-14.352405012331,
114.921474704573)) ;
#183094 = CARTESIAN_POINT('Ctrl Pts',(-18.8778061466655,-14.2916996646196,
114.964766086765)) ;
#183095 = CARTESIAN_POINT('Ctrl Pts',(-18.9472129540579,-14.4330905333239,
115.211832429368)) ;
#183096 = CARTESIAN_POINT('Ctrl Pts',(-18.9558639366158,-14.362422601594,
115.23818192445)) ;
#183097 = CARTESIAN_POINT('Ctrl Pts',(-18.8820601227543,-14.3624226376889,
115.262413056166)) ;
#183098 = CARTESIAN_POINT('Ctrl Pts',(-18.8082563088927,-14.3624226737838,
115.286644187882)) ;
#183099 = CARTESIAN_POINT('Ctrl Pts',(-18.7996053263348,-14.4330906055137,
115.2602946928)) ;
#183100 = CARTESIAN_POINT('Ctrl Pts',(-18.7909543437769,-14.5037585372437,
115.233945197718)) ;
#183101 = CARTESIAN_POINT('Ctrl Pts',(-18.8647581576385,-14.5037585011487,
115.209714066002)) ;
#183102 = CARTESIAN_POINT('Ctrl Pts',(-18.9385619715001,-14.5037584650538,
115.185482934287)) ;
#183103 = CARTESIAN_POINT('Ctrl Pts',(-18.9472129540579,-14.4330905333239,
115.211832429368)) ;
#183104 = CARTESIAN_POINT('Ctrl Pts',(-19.0250383188823,-14.5004556458798,
115.484322413278)) ;
#183105 = CARTESIAN_POINT('Ctrl Pts',(-19.0275352173107,-14.424978464963,
115.491927561146)) ;
#183106 = CARTESIAN_POINT('Ctrl Pts',(-18.9537314039739,-14.4249784742085,
115.51615869446)) ;
#183107 = CARTESIAN_POINT('Ctrl Pts',(-18.879927590637,-14.4249784834539,
115.540389827774)) ;
#183108 = CARTESIAN_POINT('Ctrl Pts',(-18.8774306922086,-14.5004556643706,
115.532784679906)) ;
#183109 = CARTESIAN_POINT('Ctrl Pts',(-18.8749337937802,-14.5759328452874,
115.525179532038)) ;
#183110 = CARTESIAN_POINT('Ctrl Pts',(-18.9487376071171,-14.5759328360419,
115.500948398724)) ;
#183111 = CARTESIAN_POINT('Ctrl Pts',(-19.0225414204539,-14.5759328267965,
115.47671726541)) ;
#183112 = CARTESIAN_POINT('Ctrl Pts',(-19.0250383188823,-14.5004556458798,
115.484322413278)) ;
#183113 = CARTESIAN_POINT('Ctrl Pts',(-19.1050415480743,-14.4906784452632,
115.763353035226)) ;
#183114 = CARTESIAN_POINT('Ctrl Pts',(-19.1012249635907,-14.4157707960699,
115.751728332911)) ;
#183115 = CARTESIAN_POINT('Ctrl Pts',(-19.0274211485121,-14.4157707802425,
115.77595946092)) ;
#183116 = CARTESIAN_POINT('Ctrl Pts',(-18.9536173334336,-14.4157707644151,
115.80019058893)) ;
#183117 = CARTESIAN_POINT('Ctrl Pts',(-18.9574339179171,-14.4906784136084,
115.811815291245)) ;
#183118 = CARTESIAN_POINT('Ctrl Pts',(-18.9612505024007,-14.5655860628017,
115.82343999356)) ;
#183119 = CARTESIAN_POINT('Ctrl Pts',(-19.0350543174793,-14.5655860786291,
115.79920886555)) ;
#183120 = CARTESIAN_POINT('Ctrl Pts',(-19.1088581325578,-14.5655860944565,
115.774977737541)) ;
#183121 = CARTESIAN_POINT('Ctrl Pts',(-19.1050415480743,-14.4906784452632,
115.763353035226)) ;
#183122 = CARTESIAN_POINT('Ctrl Pts',(-19.1811866606781,-14.4044504861589,
116.030699387926)) ;
#183123 = CARTESIAN_POINT('Ctrl Pts',(-19.171315094255,-14.3354504116019,
116.000632187703)) ;
#183124 = CARTESIAN_POINT('Ctrl Pts',(-19.0975112751908,-14.3354503745246,
116.024863303572)) ;
#183125 = CARTESIAN_POINT('Ctrl Pts',(-19.0237074561265,-14.3354503374474,
116.049094419442)) ;
#183126 = CARTESIAN_POINT('Ctrl Pts',(-19.0335790225497,-14.4044504120043,
116.079161619665)) ;
#183127 = CARTESIAN_POINT('Ctrl Pts',(-19.0434505889729,-14.4734504865613,
116.109228819889)) ;
#183128 = CARTESIAN_POINT('Ctrl Pts',(-19.1172544080371,-14.4734505236385,
116.084997704019)) ;
#183129 = CARTESIAN_POINT('Ctrl Pts',(-19.1910582271013,-14.4734505607158,
116.06076658815)) ;
#183130 = CARTESIAN_POINT('Ctrl Pts',(-19.1811866606781,-14.4044504861589,
116.030699387926)) ;
#183131 = CARTESIAN_POINT('Ctrl Pts',(-19.2474615033651,-14.2464177648016,
116.26820558113)) ;
#183132 = CARTESIAN_POINT('Ctrl Pts',(-19.2322101937286,-14.1883465874269,
116.22175255126)) ;
#183133 = CARTESIAN_POINT('Ctrl Pts',(-19.1584063686785,-14.1883465362759,
116.245983648898)) ;
#183134 = CARTESIAN_POINT('Ctrl Pts',(-19.0846025436284,-14.1883464851249,
116.270214746535)) ;
#183135 = CARTESIAN_POINT('Ctrl Pts',(-19.0998538532649,-14.2464176624996,
116.316667776405)) ;
#183136 = CARTESIAN_POINT('Ctrl Pts',(-19.1151051629013,-14.3044888398743,
116.363120806274)) ;
#183137 = CARTESIAN_POINT('Ctrl Pts',(-19.1889089879514,-14.3044888910253,
116.338889708637)) ;
#183138 = CARTESIAN_POINT('Ctrl Pts',(-19.2627128130015,-14.3044889421763,
116.314658611)) ;
#183139 = CARTESIAN_POINT('Ctrl Pts',(-19.2474615033651,-14.2464177648016,
116.26820558113)) ;
#183140 = CARTESIAN_POINT('Ctrl Pts',(-19.2975522404832,-14.0296079395376,
116.456228657709)) ;
#183141 = CARTESIAN_POINT('Ctrl Pts',(-19.2780468758366,-13.9865865421538,
116.396818462815)) ;
#183142 = CARTESIAN_POINT('Ctrl Pts',(-19.2042430445828,-13.9865864836806,
116.421049541558)) ;
#183143 = CARTESIAN_POINT('Ctrl Pts',(-19.1304392133291,-13.9865864252074,
116.4452806203)) ;
#183144 = CARTESIAN_POINT('Ctrl Pts',(-19.1499445779758,-14.0296078225912,
116.504690815193)) ;
#183145 = CARTESIAN_POINT('Ctrl Pts',(-19.1694499426224,-14.072629219975,
116.564101010086)) ;
#183146 = CARTESIAN_POINT('Ctrl Pts',(-19.2432537738762,-14.0726292784482,
116.539869931344)) ;
#183147 = CARTESIAN_POINT('Ctrl Pts',(-19.3170576051299,-14.0726293369214,
116.515638852602)) ;
#183148 = CARTESIAN_POINT('Ctrl Pts',(-19.2975522404832,-14.0296079395376,
116.456228657709)) ;
#183149 = CARTESIAN_POINT('Ctrl Pts',(-19.3275320163761,-13.7700542634679,
116.582883427607)) ;
#183150 = CARTESIAN_POINT('Ctrl Pts',(-19.3051727068637,-13.7450900092007,
116.514780577272)) ;
#183151 = CARTESIAN_POINT('Ctrl Pts',(-19.2313688696332,-13.7450899491233,
116.539011637809)) ;
#183152 = CARTESIAN_POINT('Ctrl Pts',(-19.1575650324027,-13.7450898890458,
116.563242698347)) ;
#183153 = CARTESIAN_POINT('Ctrl Pts',(-19.179924341915,-13.7700541433129,
116.631345548683)) ;
#183154 = CARTESIAN_POINT('Ctrl Pts',(-19.2022836514274,-13.79501839758,116.699448399019)) ;
#183155 = CARTESIAN_POINT('Ctrl Pts',(-19.2760874886579,-13.7950184576575,
116.675217338481)) ;
#183156 = CARTESIAN_POINT('Ctrl Pts',(-19.3498913258885,-13.795018517735,
116.650986277943)) ;
#183157 = CARTESIAN_POINT('Ctrl Pts',(-19.3275320163761,-13.7700542634679,
116.582883427607)) ;
#183158 = CARTESIAN_POINT('Ctrl Pts',(-19.3346750163065,-13.4844393542531,
116.640102123225)) ;
#183159 = CARTESIAN_POINT('Ctrl Pts',(-19.311049259971,-13.4793790766449,
116.56814188037)) ;
#183160 = CARTESIAN_POINT('Ctrl Pts',(-19.2372454173489,-13.4793790219259,
116.592372924486)) ;
#183161 = CARTESIAN_POINT('Ctrl Pts',(-19.1634415747268,-13.479378967207,
116.616603968602)) ;
#183162 = CARTESIAN_POINT('Ctrl Pts',(-19.1870673310623,-13.4844392448151,
116.688564211457)) ;
#183163 = CARTESIAN_POINT('Ctrl Pts',(-19.2106930873978,-13.4894995224233,
116.760524454312)) ;
#183164 = CARTESIAN_POINT('Ctrl Pts',(-19.2844969300199,-13.4894995771423,
116.736293410196)) ;
#183165 = CARTESIAN_POINT('Ctrl Pts',(-19.358300772642,-13.4894996318613,
116.71206236608)) ;
#183166 = CARTESIAN_POINT('Ctrl Pts',(-19.3346750163065,-13.4844393542531,
116.640102123225)) ;
#183167 = CARTESIAN_POINT('Ctrl Pts',(-19.3174944725961,-13.1938467066394,
116.623262581033)) ;
#183168 = CARTESIAN_POINT('Ctrl Pts',(-19.2942980324291,-13.2090684129076,
116.55260996613)) ;
#183169 = CARTESIAN_POINT('Ctrl Pts',(-19.2204941858365,-13.2090683682137,
116.576840998153)) ;
#183170 = CARTESIAN_POINT('Ctrl Pts',(-19.1466903392439,-13.2090683235198,
116.601072030175)) ;
#183171 = CARTESIAN_POINT('Ctrl Pts',(-19.1698867794109,-13.1938466172516,
116.671724645078)) ;
#183172 = CARTESIAN_POINT('Ctrl Pts',(-19.1930832195779,-13.1786249109835,
116.74237725998)) ;
#183173 = CARTESIAN_POINT('Ctrl Pts',(-19.2668870661705,-13.1786249556774,
116.718146227958)) ;
#183174 = CARTESIAN_POINT('Ctrl Pts',(-19.3406909127631,-13.1786250003713,
116.693915195935)) ;
#183175 = CARTESIAN_POINT('Ctrl Pts',(-19.3174944725961,-13.1938467066394,
116.623262581033)) ;
#183176 = CARTESIAN_POINT('Ctrl Pts',(-19.2765712704978,-12.9193998282655,
116.534084192877)) ;
#183177 = CARTESIAN_POINT('Ctrl Pts',(-19.2554630438177,-12.9538071121124,
116.469791939493)) ;
#183178 = CARTESIAN_POINT('Ctrl Pts',(-19.1816591948598,-12.9538070795867,
116.494022964311)) ;
#183179 = CARTESIAN_POINT('Ctrl Pts',(-19.107855345902,-12.9538070470611,
116.51825398913)) ;
#183180 = CARTESIAN_POINT('Ctrl Pts',(-19.1289635725821,-12.9193997632142,
116.582546242514)) ;
#183181 = CARTESIAN_POINT('Ctrl Pts',(-19.1500717992623,-12.8849924793673,
116.646838495899)) ;
#183182 = CARTESIAN_POINT('Ctrl Pts',(-19.2238756482201,-12.884992511893,
116.62260747108)) ;
#183183 = CARTESIAN_POINT('Ctrl Pts',(-19.297679497178,-12.8849925444186,
116.598376446262)) ;
#183184 = CARTESIAN_POINT('Ctrl Pts',(-19.2765712704978,-12.9193998282655,
116.534084192877)) ;
#183185 = CARTESIAN_POINT('Ctrl Pts',(-19.2136556163805,-12.679977460876,
116.378071311553)) ;
#183186 = CARTESIAN_POINT('Ctrl Pts',(-19.1961712122001,-12.7311545599109,
116.324816636992)) ;
#183187 = CARTESIAN_POINT('Ctrl Pts',(-19.1223673628755,-12.7311545403401,
116.349047660693)) ;
#183188 = CARTESIAN_POINT('Ctrl Pts',(-19.0485635135508,-12.7311545207693,
116.373278684394)) ;
#183189 = CARTESIAN_POINT('Ctrl Pts',(-19.0660479177312,-12.6799774217345,
116.426533358955)) ;
#183190 = CARTESIAN_POINT('Ctrl Pts',(-19.0835323219115,-12.6288003226997,
116.479788033517)) ;
#183191 = CARTESIAN_POINT('Ctrl Pts',(-19.1573361712362,-12.6288003422704,
116.455557009816)) ;
#183192 = CARTESIAN_POINT('Ctrl Pts',(-19.2311400205609,-12.6288003618412,
116.431325986115)) ;
#183193 = CARTESIAN_POINT('Ctrl Pts',(-19.2136556163805,-12.679977460876,
116.378071311553)) ;
#183194 = CARTESIAN_POINT('Ctrl Pts',(-19.1338523199838,-12.4956043021029,
116.170183536347)) ;
#183195 = CARTESIAN_POINT('Ctrl Pts',(-19.1211857358534,-12.5597317655866,
116.13160316441)) ;
#183196 = CARTESIAN_POINT('Ctrl Pts',(-19.0473818865867,-12.5597317545878,
116.155834188288)) ;
#183197 = CARTESIAN_POINT('Ctrl Pts',(-18.9735780373201,-12.5597317435889,
116.180065212166)) ;
#183198 = CARTESIAN_POINT('Ctrl Pts',(-18.9862446214504,-12.4956042801052,
116.218645584102)) ;
#183199 = CARTESIAN_POINT('Ctrl Pts',(-18.9989112055808,-12.4314768166214,
116.257225956039)) ;
#183200 = CARTESIAN_POINT('Ctrl Pts',(-19.0727150548475,-12.4314768276203,
116.232994932161)) ;
#183201 = CARTESIAN_POINT('Ctrl Pts',(-19.1465189041141,-12.4314768386191,
116.208763908283)) ;
#183202 = CARTESIAN_POINT('Ctrl Pts',(-19.1338523199838,-12.4956043021029,
116.170183536347)) ;
#183203 = CARTESIAN_POINT('Ctrl Pts',(-19.0401108727425,-12.3751190535725,
115.920306886088)) ;
#183204 = CARTESIAN_POINT('Ctrl Pts',(-19.0332329599517,-12.4477568900421,
115.899357873225)) ;
#183205 = CARTESIAN_POINT('Ctrl Pts',(-18.9594291126121,-12.4477568870231,
115.923588902972)) ;
#183206 = CARTESIAN_POINT('Ctrl Pts',(-18.8856252652726,-12.4477568840041,
115.94781993272)) ;
#183207 = CARTESIAN_POINT('Ctrl Pts',(-18.8925031780634,-12.3751190475345,
115.968768945583)) ;
#183208 = CARTESIAN_POINT('Ctrl Pts',(-18.8993810908542,-12.3024812110649,
115.989717958446)) ;
#183209 = CARTESIAN_POINT('Ctrl Pts',(-18.9731849381938,-12.3024812140839,
115.965486928699)) ;
#183210 = CARTESIAN_POINT('Ctrl Pts',(-19.0469887855334,-12.3024812171029,
115.941255898952)) ;
#183211 = CARTESIAN_POINT('Ctrl Pts',(-19.0401108727425,-12.3751190535725,
115.920306886088)) ;
#183212 = CARTESIAN_POINT('Ctrl Pts',(-18.9401330390511,-12.3303020351126,
115.651151126256)) ;
#183213 = CARTESIAN_POINT('Ctrl Pts',(-18.9394940201831,-12.4061784488461,
115.649204777747)) ;
#183214 = CARTESIAN_POINT('Ctrl Pts',(-18.8656901744884,-12.4061784491626,
115.673435812505)) ;
#183215 = CARTESIAN_POINT('Ctrl Pts',(-18.7918863287937,-12.4061784494791,
115.697666847262)) ;
#183216 = CARTESIAN_POINT('Ctrl Pts',(-18.7925253476617,-12.3303020357456,
115.699613195771)) ;
#183217 = CARTESIAN_POINT('Ctrl Pts',(-18.7931643665296,-12.2544256220122,
115.701559544279)) ;
#183218 = CARTESIAN_POINT('Ctrl Pts',(-18.8669682122243,-12.2544256216956,
115.677328509522)) ;
#183219 = CARTESIAN_POINT('Ctrl Pts',(-18.940772057919,-12.2544256213791,
115.653097474764)) ;
#183220 = CARTESIAN_POINT('Ctrl Pts',(-18.9401330390511,-12.3303020351126,
115.651151126256)) ;
#183221 = CARTESIAN_POINT('Ctrl Pts',(-18.839178326217,-12.3631774170788,
115.379196252521)) ;
#183222 = CARTESIAN_POINT('Ctrl Pts',(-18.8448523121877,-12.4368724586972,
115.396478298259)) ;
#183223 = CARTESIAN_POINT('Ctrl Pts',(-18.7710484682646,-12.4368724595397,
115.420709338412)) ;
#183224 = CARTESIAN_POINT('Ctrl Pts',(-18.6972446243415,-12.4368724603823,
115.444940378566)) ;
#183225 = CARTESIAN_POINT('Ctrl Pts',(-18.6915706383708,-12.363177418764,
115.427658332828)) ;
#183226 = CARTESIAN_POINT('Ctrl Pts',(-18.6858966524001,-12.2894823771457,
115.41037628709)) ;
#183227 = CARTESIAN_POINT('Ctrl Pts',(-18.7597004963232,-12.2894823763031,
115.386145246937)) ;
#183228 = CARTESIAN_POINT('Ctrl Pts',(-18.8335043402463,-12.2894823754605,
115.361914206783)) ;
#183229 = CARTESIAN_POINT('Ctrl Pts',(-18.839178326217,-12.3631774170788,
115.379196252521)) ;
#183230 = CARTESIAN_POINT('Ctrl Pts',(-18.7446035699514,-12.4713342743348,
115.126509818248)) ;
#183231 = CARTESIAN_POINT('Ctrl Pts',(-18.756157869452,-12.5375870378766,
115.161702350275)) ;
#183232 = CARTESIAN_POINT('Ctrl Pts',(-18.6823540264618,-12.5375870373685,
115.18593339327)) ;
#183233 = CARTESIAN_POINT('Ctrl Pts',(-18.6085501834715,-12.5375870368604,
115.210164436265)) ;
#183234 = CARTESIAN_POINT('Ctrl Pts',(-18.5969958839709,-12.4713342733185,
115.174971904238)) ;
#183235 = CARTESIAN_POINT('Ctrl Pts',(-18.5854415844703,-12.4050815097766,
115.139779372211)) ;
#183236 = CARTESIAN_POINT('Ctrl Pts',(-18.6592454274606,-12.4050815102848,
115.115548329217)) ;
#183237 = CARTESIAN_POINT('Ctrl Pts',(-18.7330492704508,-12.4050815107929,
115.091317286222)) ;
#183238 = CARTESIAN_POINT('Ctrl Pts',(-18.7446035699514,-12.4713342743348,
115.126509818248)) ;
#183239 = CARTESIAN_POINT('Ctrl Pts',(-18.6616637495359,-12.6476404276989,
114.909396069518)) ;
#183240 = CARTESIAN_POINT('Ctrl Pts',(-18.6782920578757,-12.7016806543081,
114.960043213818)) ;
#183241 = CARTESIAN_POINT('Ctrl Pts',(-18.6044882152249,-12.7016806520052,
114.984274257847)) ;
#183242 = CARTESIAN_POINT('Ctrl Pts',(-18.530684372574,-12.7016806497023,
115.008505301875)) ;
#183243 = CARTESIAN_POINT('Ctrl Pts',(-18.5140560642342,-12.6476404230932,
114.957858157575)) ;
#183244 = CARTESIAN_POINT('Ctrl Pts',(-18.4974277558943,-12.5936001964841,
114.907211013275)) ;
#183245 = CARTESIAN_POINT('Ctrl Pts',(-18.5712315985452,-12.5936001987869,
114.882979969247)) ;
#183246 = CARTESIAN_POINT('Ctrl Pts',(-18.6450354411961,-12.5936002010898,
114.858748925218)) ;
#183247 = CARTESIAN_POINT('Ctrl Pts',(-18.6616637495359,-12.6476404276989,
114.909396069518)) ;
#183248 = CARTESIAN_POINT('Ctrl Pts',(-18.5959843317389,-12.8790215196565,
114.744812606196)) ;
#183249 = CARTESIAN_POINT('Ctrl Pts',(-18.6164896477251,-12.9169844114343,
114.807268490226)) ;
#183250 = CARTESIAN_POINT('Ctrl Pts',(-18.542685804714,-12.916984408831,114.831499533157)) ;
#183251 = CARTESIAN_POINT('Ctrl Pts',(-18.468881961703,-12.9169844062277,
114.855730576088)) ;
#183252 = CARTESIAN_POINT('Ctrl Pts',(-18.4483766457167,-12.87902151445,114.793274692059)) ;
#183253 = CARTESIAN_POINT('Ctrl Pts',(-18.4278713297304,-12.8410586226723,
114.730818808029)) ;
#183254 = CARTESIAN_POINT('Ctrl Pts',(-18.5016751727415,-12.8410586252756,
114.706587765098)) ;
#183255 = CARTESIAN_POINT('Ctrl Pts',(-18.5754790157526,-12.8410586278788,
114.682356722167)) ;
#183256 = CARTESIAN_POINT('Ctrl Pts',(-18.5959843317389,-12.8790215196565,
114.744812606196)) ;
#183257 = CARTESIAN_POINT('Ctrl Pts',(-18.5513499003185,-13.1499133657009,
114.644442101082)) ;
#183258 = CARTESIAN_POINT('Ctrl Pts',(-18.574265896151,-13.1690162421117,
114.714240526902)) ;
#183259 = CARTESIAN_POINT('Ctrl Pts',(-18.5004620526313,-13.1690162422106,
114.738471568284)) ;
#183260 = CARTESIAN_POINT('Ctrl Pts',(-18.4266582091115,-13.1690162423095,
114.762702609666)) ;
#183261 = CARTESIAN_POINT('Ctrl Pts',(-18.403742213279,-13.1499133658987,
114.692904183846)) ;
#183262 = CARTESIAN_POINT('Ctrl Pts',(-18.3808262174465,-13.1308104894879,
114.623105758027)) ;
#183263 = CARTESIAN_POINT('Ctrl Pts',(-18.4546300609663,-13.130810489389,
114.598874716645)) ;
#183264 = CARTESIAN_POINT('Ctrl Pts',(-18.528433904486,-13.1308104892901,
114.574643675262)) ;
#183265 = CARTESIAN_POINT('Ctrl Pts',(-18.5513499003185,-13.1499133657009,
114.644442101082)) ;
#183266 = CARTESIAN_POINT('Ctrl Pts',(-18.5304611078023,-13.4386144880716,
114.616209853643)) ;
#183267 = CARTESIAN_POINT('Ctrl Pts',(-18.5541367214207,-13.437586579743,
114.688321952596)) ;
#183268 = CARTESIAN_POINT('Ctrl Pts',(-18.4803328778889,-13.4375865840391,
114.712552993941)) ;
#183269 = CARTESIAN_POINT('Ctrl Pts',(-18.406529034357,-13.4375865883353,
114.736784035286)) ;
#183270 = CARTESIAN_POINT('Ctrl Pts',(-18.3828534207386,-13.438614496664,
114.664671936333)) ;
#183271 = CARTESIAN_POINT('Ctrl Pts',(-18.3591778071202,-13.4396424049927,
114.59255983738)) ;
#183272 = CARTESIAN_POINT('Ctrl Pts',(-18.4329816506521,-13.4396424006965,
114.568328796035)) ;
#183273 = CARTESIAN_POINT('Ctrl Pts',(-18.5067854941839,-13.4396423964003,
114.54409775469)) ;
#183274 = CARTESIAN_POINT('Ctrl Pts',(-18.5304611078023,-13.4386144880716,
114.616209853643)) ;
#183275 = CARTESIAN_POINT('Ctrl Pts',(-18.5338401235194,-13.7268235527867,
114.662025079469)) ;
#183276 = CARTESIAN_POINT('Ctrl Pts',(-18.556579229651,-13.7056699529127,
114.731284727602)) ;
#183277 = CARTESIAN_POINT('Ctrl Pts',(-18.4827753870096,-13.7056699630902,
114.75551577166)) ;
#183278 = CARTESIAN_POINT('Ctrl Pts',(-18.4089715443681,-13.7056699732676,
114.779746815717)) ;
#183279 = CARTESIAN_POINT('Ctrl Pts',(-18.3862324382365,-13.7268235731417,
114.710487167584)) ;
#183280 = CARTESIAN_POINT('Ctrl Pts',(-18.3634933321048,-13.7479771730157,
114.64122751945)) ;
#183281 = CARTESIAN_POINT('Ctrl Pts',(-18.4372971747463,-13.7479771628382,
114.616996475393)) ;
#183282 = CARTESIAN_POINT('Ctrl Pts',(-18.5111010173877,-13.7479771526607,
114.592765431336)) ;
#183283 = CARTESIAN_POINT('Ctrl Pts',(-18.5338401235194,-13.7268235527867,
114.662025079469)) ;
#183284 = CARTESIAN_POINT('Ctrl Pts',(-18.5603928248668,-13.9914324144424,
114.778219545102)) ;
#183285 = CARTESIAN_POINT('Ctrl Pts',(-18.5805799757975,-13.9517725540924,
114.839706349339)) ;
#183286 = CARTESIAN_POINT('Ctrl Pts',(-18.5067761349001,-13.9517725681727,
114.863937398709)) ;
#183287 = CARTESIAN_POINT('Ctrl Pts',(-18.4329722940027,-13.9517725822531,
114.888168448078)) ;
#183288 = CARTESIAN_POINT('Ctrl Pts',(-18.4127851430721,-13.9914324426031,
114.826681643841)) ;
#183289 = CARTESIAN_POINT('Ctrl Pts',(-18.3925979921414,-14.0310923029532,
114.765194839604)) ;
#183290 = CARTESIAN_POINT('Ctrl Pts',(-18.4664018330387,-14.0310922888728,
114.740963790235)) ;
#183291 = CARTESIAN_POINT('Ctrl Pts',(-18.5402056739361,-14.0310922747924,
114.716732740866)) ;
#183292 = CARTESIAN_POINT('Ctrl Pts',(-18.5603928248668,-13.9914324144424,
114.778219545102)) ;
#183293 = CARTESIAN_POINT('Ctrl Pts',(-18.6076829202727,-14.2164140691066,
114.957760632545)) ;
#183294 = CARTESIAN_POINT('Ctrl Pts',(-18.6238627885757,-14.1609879110475,
115.007041900317)) ;
#183295 = CARTESIAN_POINT('Ctrl Pts',(-18.5500589505241,-14.1609879280051,
115.031272958354)) ;
#183296 = CARTESIAN_POINT('Ctrl Pts',(-18.4762551124724,-14.1609879449628,
115.055504016391)) ;
#183297 = CARTESIAN_POINT('Ctrl Pts',(-18.4600752441693,-14.2164141030218,
115.006222748618)) ;
#183298 = CARTESIAN_POINT('Ctrl Pts',(-18.4438953758662,-14.2718402610809,
114.956941480846)) ;
#183299 = CARTESIAN_POINT('Ctrl Pts',(-18.5176992139179,-14.2718402441232,
114.932710422809)) ;
#183300 = CARTESIAN_POINT('Ctrl Pts',(-18.5915030519696,-14.2718402271656,
114.908479364772)) ;
#183301 = CARTESIAN_POINT('Ctrl Pts',(-18.6076829202727,-14.2164140691066,
114.957760632545)) ;
#183302 = CARTESIAN_POINT('Ctrl Pts',(-18.6716131600408,-14.384032579335,
115.188003285153)) ;
#183303 = CARTESIAN_POINT('Ctrl Pts',(-18.6826177315112,-14.3168227397863,
115.221521433634)) ;
#183304 = CARTESIAN_POINT('Ctrl Pts',(-18.6088138971231,-14.3168227556033,
115.24575250283)) ;
#183305 = CARTESIAN_POINT('Ctrl Pts',(-18.5350100627351,-14.3168227714204,
115.269983572026)) ;
#183306 = CARTESIAN_POINT('Ctrl Pts',(-18.5240054912648,-14.3840326109691,
115.236465423545)) ;
#183307 = CARTESIAN_POINT('Ctrl Pts',(-18.5130009197944,-14.4512424505178,
115.202947275064)) ;
#183308 = CARTESIAN_POINT('Ctrl Pts',(-18.5868047541824,-14.4512424347008,
115.178716205868)) ;
#183309 = CARTESIAN_POINT('Ctrl Pts',(-18.6606085885704,-14.4512424188837,
115.154485136673)) ;
#183310 = CARTESIAN_POINT('Ctrl Pts',(-18.6716131600408,-14.384032579335,
115.188003285153)) ;
#183311 = CARTESIAN_POINT('Ctrl Pts',(-18.7465062676533,-14.4820529544929,
115.451530561366)) ;
#183312 = CARTESIAN_POINT('Ctrl Pts',(-18.751564849774,-14.40790231883,115.466938185513)) ;
#183313 = CARTESIAN_POINT('Ctrl Pts',(-18.6777610188436,-14.4079023280758,
115.49116926524)) ;
#183314 = CARTESIAN_POINT('Ctrl Pts',(-18.6039571879133,-14.4079023373216,
115.515400344967)) ;
#183315 = CARTESIAN_POINT('Ctrl Pts',(-18.5988986057926,-14.4820529729845,
115.499992720821)) ;
#183316 = CARTESIAN_POINT('Ctrl Pts',(-18.593840023672,-14.5562036086474,
115.484585096674)) ;
#183317 = CARTESIAN_POINT('Ctrl Pts',(-18.6676438546023,-14.5562035994016,
115.460354016947)) ;
#183318 = CARTESIAN_POINT('Ctrl Pts',(-18.7414476855327,-14.5562035901558,
115.43612293722)) ;
#183319 = CARTESIAN_POINT('Ctrl Pts',(-18.7465062676533,-14.4820529544929,
115.451530561366)) ;
#183320 = CARTESIAN_POINT('Ctrl Pts',(-18.8266090365466,-14.5042250600488,
115.730991693486)) ;
#183321 = CARTESIAN_POINT('Ctrl Pts',(-18.8253480296144,-14.4284191898376,
115.727150868868)) ;
#183322 = CARTESIAN_POINT('Ctrl Pts',(-18.7515442017851,-14.4284191877868,
115.751381958041)) ;
#183323 = CARTESIAN_POINT('Ctrl Pts',(-18.6777403739558,-14.428419185736,
115.775613047213)) ;
#183324 = CARTESIAN_POINT('Ctrl Pts',(-18.679001380888,-14.5042250559472,
115.779453871831)) ;
#183325 = CARTESIAN_POINT('Ctrl Pts',(-18.6802623878202,-14.5800309261584,
115.78329469645)) ;
#183326 = CARTESIAN_POINT('Ctrl Pts',(-18.7540662156495,-14.5800309282092,
115.759063607277)) ;
#183327 = CARTESIAN_POINT('Ctrl Pts',(-18.8278700434788,-14.58003093026,115.734832518105)) ;
#183328 = CARTESIAN_POINT('Ctrl Pts',(-18.8266090365466,-14.5042250600488,
115.730991693486)) ;
#183329 = CARTESIAN_POINT('Ctrl Pts',(-18.9055245763069,-14.4479097103847,
116.006958567327)) ;
#183330 = CARTESIAN_POINT('Ctrl Pts',(-18.8980152465996,-14.3759257111989,
115.984086359506)) ;
#183331 = CARTESIAN_POINT('Ctrl Pts',(-18.8242114209466,-14.3759256925376,
116.008317455307)) ;
#183332 = CARTESIAN_POINT('Ctrl Pts',(-18.7504075952935,-14.3759256738764,
116.032548551108)) ;
#183333 = CARTESIAN_POINT('Ctrl Pts',(-18.7579169250007,-14.4479096730622,
116.055420758929)) ;
#183334 = CARTESIAN_POINT('Ctrl Pts',(-18.7654262547079,-14.519893672248,
116.078292966749)) ;
#183335 = CARTESIAN_POINT('Ctrl Pts',(-18.839230080361,-14.5198936909092,
116.054061870948)) ;
#183336 = CARTESIAN_POINT('Ctrl Pts',(-18.9130339060141,-14.5198937095705,
116.029830775147)) ;
#183337 = CARTESIAN_POINT('Ctrl Pts',(-18.9055245763069,-14.4479097103847,
116.006958567327)) ;
#183338 = CARTESIAN_POINT('Ctrl Pts',(-18.9759850270256,-14.3189148106109,
116.25684843315)) ;
#183339 = CARTESIAN_POINT('Ctrl Pts',(-18.9628155048468,-14.2558334084202,
116.216736192202)) ;
#183340 = CARTESIAN_POINT('Ctrl Pts',(-18.889011678749,-14.2558333716659,
116.240967286648)) ;
#183341 = CARTESIAN_POINT('Ctrl Pts',(-18.8152078526511,-14.2558333349115,
116.265198381095)) ;
#183342 = CARTESIAN_POINT('Ctrl Pts',(-18.82837737483,-14.3189147371022,116.305310622043)) ;
#183343 = CARTESIAN_POINT('Ctrl Pts',(-18.8415468970088,-14.3819961392929,
116.345422862991)) ;
#183344 = CARTESIAN_POINT('Ctrl Pts',(-18.9153507231067,-14.3819961760472,
116.321191768545)) ;
#183345 = CARTESIAN_POINT('Ctrl Pts',(-18.9891545492045,-14.3819962128016,
116.296960674098)) ;
#183346 = CARTESIAN_POINT('Ctrl Pts',(-18.9759850270256,-14.3189148106109,
116.25684843315)) ;
#183347 = CARTESIAN_POINT('Ctrl Pts',(-19.0333811299086,-14.1239822238445,
116.467278862587)) ;
#183348 = CARTESIAN_POINT('Ctrl Pts',(-19.0154483528946,-14.0744187665949,
116.412658515781)) ;
#183349 = CARTESIAN_POINT('Ctrl Pts',(-18.9416445249628,-14.074418709394,
116.436889604641)) ;
#183350 = CARTESIAN_POINT('Ctrl Pts',(-18.8678406970309,-14.0744186521931,
116.461120693501)) ;
#183351 = CARTESIAN_POINT('Ctrl Pts',(-18.8857734740448,-14.1239821094427,
116.515741040307)) ;
#183352 = CARTESIAN_POINT('Ctrl Pts',(-18.9037062510588,-14.1735455666924,
116.570361387112)) ;
#183353 = CARTESIAN_POINT('Ctrl Pts',(-18.9775100789907,-14.1735456238933,
116.546130298252)) ;
#183354 = CARTESIAN_POINT('Ctrl Pts',(-19.0513139069226,-14.1735456810942,
116.521899209392)) ;
#183355 = CARTESIAN_POINT('Ctrl Pts',(-19.0333811299086,-14.1239822238445,
116.467278862587)) ;
#183356 = CARTESIAN_POINT('Ctrl Pts',(-19.0719097483262,-13.8804446676162,
116.619916310961)) ;
#183357 = CARTESIAN_POINT('Ctrl Pts',(-19.0505310135905,-13.8478127953866,
116.554800132824)) ;
#183358 = CARTESIAN_POINT('Ctrl Pts',(-18.9767271811777,-13.8478127217154,
116.579031208036)) ;
#183359 = CARTESIAN_POINT('Ctrl Pts',(-18.902923348765,-13.8478126480443,
116.603262283248)) ;
#183360 = CARTESIAN_POINT('Ctrl Pts',(-18.9243020835006,-13.8804445202739,
116.668378461384)) ;
#183361 = CARTESIAN_POINT('Ctrl Pts',(-18.9456808182363,-13.9130763925035,
116.733494639521)) ;
#183362 = CARTESIAN_POINT('Ctrl Pts',(-19.0194846506491,-13.9130764661746,
116.709263564309)) ;
#183363 = CARTESIAN_POINT('Ctrl Pts',(-19.0932884830618,-13.9130765398458,
116.685032489097)) ;
#183364 = CARTESIAN_POINT('Ctrl Pts',(-19.0719097483262,-13.8804446676162,
116.619916310961)) ;
#183365 = CARTESIAN_POINT('Ctrl Pts',(-19.088702598421,-13.6007259227713,
116.70677615132)) ;
#183366 = CARTESIAN_POINT('Ctrl Pts',(-19.0653812357714,-13.5875751539527,
116.635743041836)) ;
#183367 = CARTESIAN_POINT('Ctrl Pts',(-18.9915773972596,-13.5875750652436,
116.659974098472)) ;
#183368 = CARTESIAN_POINT('Ctrl Pts',(-18.9177735587479,-13.5875749765345,
116.684205155107)) ;
#183369 = CARTESIAN_POINT('Ctrl Pts',(-18.9410949213975,-13.6007257453531,
116.755238264591)) ;
#183370 = CARTESIAN_POINT('Ctrl Pts',(-18.9644162840471,-13.6138765141717,
116.826271374075)) ;
#183371 = CARTESIAN_POINT('Ctrl Pts',(-19.0382201225589,-13.6138766028808,
116.80204031744)) ;
#183372 = CARTESIAN_POINT('Ctrl Pts',(-19.1120239610706,-13.6138766915899,
116.777809260804)) ;
#183373 = CARTESIAN_POINT('Ctrl Pts',(-19.088702598421,-13.6007259227713,
116.70677615132)) ;
#183374 = CARTESIAN_POINT('Ctrl Pts',(-19.0813475062609,-13.310886389785,
116.719690814776)) ;
#183375 = CARTESIAN_POINT('Ctrl Pts',(-19.0577750307551,-13.3179522424612,
116.647892855958)) ;
#183376 = CARTESIAN_POINT('Ctrl Pts',(-18.9839711845376,-13.3179521481175,
116.672123889123)) ;
#183377 = CARTESIAN_POINT('Ctrl Pts',(-18.9101673383201,-13.3179520537738,
116.696354922288)) ;
#183378 = CARTESIAN_POINT('Ctrl Pts',(-18.933739813826,-13.3108862010977,
116.768152881106)) ;
#183379 = CARTESIAN_POINT('Ctrl Pts',(-18.9573122893318,-13.3038203484215,
116.839950839923)) ;
#183380 = CARTESIAN_POINT('Ctrl Pts',(-19.0311161355493,-13.3038204427652,
116.815719806758)) ;
#183381 = CARTESIAN_POINT('Ctrl Pts',(-19.1049199817667,-13.3038205371088,
116.791488773593)) ;
#183382 = CARTESIAN_POINT('Ctrl Pts',(-19.0813475062609,-13.310886389785,
116.719690814776)) ;
#183383 = CARTESIAN_POINT('Ctrl Pts',(-19.0499358228212,-13.0275729196668,
116.659478806876)) ;
#183384 = CARTESIAN_POINT('Ctrl Pts',(-19.0277881847409,-13.0544289037497,
116.592020672865)) ;
#183385 = CARTESIAN_POINT('Ctrl Pts',(-18.9539843302875,-13.0544288105617,
116.616251680945)) ;
#183386 = CARTESIAN_POINT('Ctrl Pts',(-18.8801804758341,-13.0544287173738,
116.640482689024)) ;
#183387 = CARTESIAN_POINT('Ctrl Pts',(-18.9023281139144,-13.0275727332909,
116.707940823035)) ;
#183388 = CARTESIAN_POINT('Ctrl Pts',(-18.9244757519947,-13.000716749208,
116.775398957047)) ;
#183389 = CARTESIAN_POINT('Ctrl Pts',(-18.9982796064481,-13.000716842396,
116.751167948967)) ;
#183390 = CARTESIAN_POINT('Ctrl Pts',(-19.0720834609015,-13.000716935584,
116.726936940887)) ;
#183391 = CARTESIAN_POINT('Ctrl Pts',(-19.0499358228212,-13.0275729196668,
116.659478806876)) ;
#183392 = CARTESIAN_POINT('Ctrl Pts',(-18.9956010454947,-12.7715214711428,
116.529545008738)) ;
#183393 = CARTESIAN_POINT('Ctrl Pts',(-18.9764784771327,-12.8162933310401,
116.471300748914)) ;
#183394 = CARTESIAN_POINT('Ctrl Pts',(-18.9026746145278,-12.8162932472945,
116.495531732165)) ;
#183395 = CARTESIAN_POINT('Ctrl Pts',(-18.8288707519228,-12.8162931635489,
116.519762715417)) ;
#183396 = CARTESIAN_POINT('Ctrl Pts',(-18.8479933202848,-12.7715213036516,
116.578006975241)) ;
#183397 = CARTESIAN_POINT('Ctrl Pts',(-18.8671158886468,-12.7267494437543,
116.636251235064)) ;
#183398 = CARTESIAN_POINT('Ctrl Pts',(-18.9409197512517,-12.7267495274999,
116.612020251813)) ;
#183399 = CARTESIAN_POINT('Ctrl Pts',(-19.0147236138567,-12.7267496112455,
116.587789268561)) ;
#183400 = CARTESIAN_POINT('Ctrl Pts',(-18.9956010454947,-12.7715214711428,
116.529545008738)) ;
#183401 = CARTESIAN_POINT('Ctrl Pts',(-18.9217241255641,-12.5625540682405,
116.340023816642)) ;
#183402 = CARTESIAN_POINT('Ctrl Pts',(-18.9069967558379,-12.6219811291845,
116.295166622649)) ;
#183403 = CARTESIAN_POINT('Ctrl Pts',(-18.8331928863221,-12.6219810632867,
116.319397584851)) ;
#183404 = CARTESIAN_POINT('Ctrl Pts',(-18.7593890168062,-12.6219809973889,
116.343628547053)) ;
#183405 = CARTESIAN_POINT('Ctrl Pts',(-18.7741163865324,-12.5625539364449,
116.388485741045)) ;
#183406 = CARTESIAN_POINT('Ctrl Pts',(-18.7888437562586,-12.5031268755009,
116.433342935038)) ;
#183407 = CARTESIAN_POINT('Ctrl Pts',(-18.8626476257744,-12.5031269413987,
116.409111972836)) ;
#183408 = CARTESIAN_POINT('Ctrl Pts',(-18.9364514952903,-12.5031270072965,
116.384881010634)) ;
#183409 = CARTESIAN_POINT('Ctrl Pts',(-18.9217241255641,-12.5625540682405,
116.340023816642)) ;
#183410 = CARTESIAN_POINT('Ctrl Pts',(-18.8334781141802,-12.4155360311479,
116.106499613622)) ;
#183411 = CARTESIAN_POINT('Ctrl Pts',(-18.824160647094,-12.4853145096468,
116.078120110162)) ;
#183412 = CARTESIAN_POINT('Ctrl Pts',(-18.7503567727018,-12.4853144677288,
116.102351057511)) ;
#183413 = CARTESIAN_POINT('Ctrl Pts',(-18.6765528983095,-12.4853144258108,
116.12658200486)) ;
#183414 = CARTESIAN_POINT('Ctrl Pts',(-18.6858703653957,-12.4155359473118,
116.154961508321)) ;
#183415 = CARTESIAN_POINT('Ctrl Pts',(-18.6951878324819,-12.3457574688128,
116.183341011781)) ;
#183416 = CARTESIAN_POINT('Ctrl Pts',(-18.7689917068741,-12.3457575107309,
116.159110064432)) ;
#183417 = CARTESIAN_POINT('Ctrl Pts',(-18.8427955812663,-12.3457575526489,
116.134879117083)) ;
#183418 = CARTESIAN_POINT('Ctrl Pts',(-18.8334781141802,-12.4155360311479,
116.106499613622)) ;
#183419 = CARTESIAN_POINT('Ctrl Pts',(-18.7350882955953,-12.339199302571,
115.842366036142)) ;
#183420 = CARTESIAN_POINT('Ctrl Pts',(-18.7318906960185,-12.4144106897109,
115.832626661666)) ;
#183421 = CARTESIAN_POINT('Ctrl Pts',(-18.6580868190615,-12.41441067568,115.856857601203)) ;
#183422 = CARTESIAN_POINT('Ctrl Pts',(-18.5842829421045,-12.4144106616491,
115.881088540741)) ;
#183423 = CARTESIAN_POINT('Ctrl Pts',(-18.5874805416813,-12.3391992745091,
115.890827915217)) ;
#183424 = CARTESIAN_POINT('Ctrl Pts',(-18.5906781412581,-12.2639878873692,
115.900567289693)) ;
#183425 = CARTESIAN_POINT('Ctrl Pts',(-18.6644820182151,-12.2639879014001,
115.876336350156)) ;
#183426 = CARTESIAN_POINT('Ctrl Pts',(-18.7382858951721,-12.2639879154311,
115.852105410619)) ;
#183427 = CARTESIAN_POINT('Ctrl Pts',(-18.7350882955953,-12.339199302571,
115.842366036142)) ;
#183428 = CARTESIAN_POINT('Ctrl Pts',(-18.6339421925997,-12.3403409953756,
115.569683136395)) ;
#183429 = CARTESIAN_POINT('Ctrl Pts',(-18.6370692220127,-12.4155840268561,
115.579207561357)) ;
#183430 = CARTESIAN_POINT('Ctrl Pts',(-18.5632653452636,-12.4155840418634,
115.603438501527)) ;
#183431 = CARTESIAN_POINT('Ctrl Pts',(-18.4894614685145,-12.4155840568707,
115.627669441698)) ;
#183432 = CARTESIAN_POINT('Ctrl Pts',(-18.4863344391015,-12.3403410253901,
115.618145016736)) ;
#183433 = CARTESIAN_POINT('Ctrl Pts',(-18.4832074096885,-12.2650979939095,
115.608620591774)) ;
#183434 = CARTESIAN_POINT('Ctrl Pts',(-18.5570112864376,-12.2650979789023,
115.584389651604)) ;
#183435 = CARTESIAN_POINT('Ctrl Pts',(-18.6308151631867,-12.265097963895,
115.560158711433)) ;
#183436 = CARTESIAN_POINT('Ctrl Pts',(-18.6339421925997,-12.3403409953756,
115.569683136395)) ;
#183437 = CARTESIAN_POINT('Ctrl Pts',(-18.5356154875398,-12.4190382667156,
115.305787998287)) ;
#183438 = CARTESIAN_POINT('Ctrl Pts',(-18.5448755304968,-12.488899337021,
115.333992592985)) ;
#183439 = CARTESIAN_POINT('Ctrl Pts',(-18.4710716567852,-12.488899379198,
115.358223542407)) ;
#183440 = CARTESIAN_POINT('Ctrl Pts',(-18.3972677830735,-12.488899421375,
115.382454491829)) ;
#183441 = CARTESIAN_POINT('Ctrl Pts',(-18.3880077401164,-12.4190383510696,
115.354249897131)) ;
#183442 = CARTESIAN_POINT('Ctrl Pts',(-18.3787476971593,-12.3491772807642,
115.326045302433)) ;
#183443 = CARTESIAN_POINT('Ctrl Pts',(-18.452551570871,-12.3491772385872,
115.301814353011)) ;
#183444 = CARTESIAN_POINT('Ctrl Pts',(-18.5263554445827,-12.3491771964102,
115.277583403589)) ;
#183445 = CARTESIAN_POINT('Ctrl Pts',(-18.5356154875398,-12.4190382667156,
115.305787998287)) ;
#183446 = CARTESIAN_POINT('Ctrl Pts',(-18.4475845571782,-12.5685297170459,
115.072992627023)) ;
#183447 = CARTESIAN_POINT('Ctrl Pts',(-18.4622733767878,-12.6280576016783,
115.117732399523)) ;
#183448 = CARTESIAN_POINT('Ctrl Pts',(-18.3884695082534,-12.6280576665216,
115.141963364715)) ;
#183449 = CARTESIAN_POINT('Ctrl Pts',(-18.314665639719,-12.6280577313649,
115.166194329906)) ;
#183450 = CARTESIAN_POINT('Ctrl Pts',(-18.2999768201094,-12.5685298467324,
115.121454557406)) ;
#183451 = CARTESIAN_POINT('Ctrl Pts',(-18.2852880004998,-12.5090019621,115.076714784906)) ;
#183452 = CARTESIAN_POINT('Ctrl Pts',(-18.3590918690342,-12.5090018972567,
115.052483819715)) ;
#183453 = CARTESIAN_POINT('Ctrl Pts',(-18.4328957375686,-12.5090018324134,
115.028252854523)) ;
#183454 = CARTESIAN_POINT('Ctrl Pts',(-18.4475845571782,-12.5685297170459,
115.072992627023)) ;
#183455 = CARTESIAN_POINT('Ctrl Pts',(-18.3743096061269,-12.7793086778933,
114.885300417553)) ;
#183456 = CARTESIAN_POINT('Ctrl Pts',(-18.3934018856474,-12.8242097756673,
114.943452418522)) ;
#183457 = CARTESIAN_POINT('Ctrl Pts',(-18.3195980241341,-12.8242098564781,
114.967683405098)) ;
#183458 = CARTESIAN_POINT('Ctrl Pts',(-18.2457941626207,-12.8242099372889,
114.991914391674)) ;
#183459 = CARTESIAN_POINT('Ctrl Pts',(-18.2267018831002,-12.7793088395149,
114.933762390705)) ;
#183460 = CARTESIAN_POINT('Ctrl Pts',(-18.2076096035796,-12.7344077417409,
114.875610389736)) ;
#183461 = CARTESIAN_POINT('Ctrl Pts',(-18.281413465093,-12.7344076609301,
114.85137940316)) ;
#183462 = CARTESIAN_POINT('Ctrl Pts',(-18.3552173266063,-12.7344075801193,
114.827148416584)) ;
#183463 = CARTESIAN_POINT('Ctrl Pts',(-18.3743096061269,-12.7793086778933,
114.885300417553)) ;
#183464 = CARTESIAN_POINT('Ctrl Pts',(-18.3207591758651,-13.0361487300971,
114.757699953502)) ;
#183465 = CARTESIAN_POINT('Ctrl Pts',(-18.3428842461716,-13.0631853690337,
114.825089345966)) ;
#183466 = CARTESIAN_POINT('Ctrl Pts',(-18.2690803925913,-13.0631854575266,
114.849320356705)) ;
#183467 = CARTESIAN_POINT('Ctrl Pts',(-18.195276539011,-13.0631855460195,
114.873551367444)) ;
#183468 = CARTESIAN_POINT('Ctrl Pts',(-18.1731514687044,-13.0361489070829,
114.80616197498)) ;
#183469 = CARTESIAN_POINT('Ctrl Pts',(-18.1510263983979,-13.0091122681464,
114.738772582515)) ;
#183470 = CARTESIAN_POINT('Ctrl Pts',(-18.2248302519782,-13.0091121796535,
114.714541571777)) ;
#183471 = CARTESIAN_POINT('Ctrl Pts',(-18.2986341055586,-13.0091120911606,
114.690310561038)) ;
#183472 = CARTESIAN_POINT('Ctrl Pts',(-18.3207591758651,-13.0361487300971,
114.757699953502)) ;
#183473 = CARTESIAN_POINT('Ctrl Pts',(-18.2900556295031,-13.3199156358865,
114.699632332883)) ;
#183474 = CARTESIAN_POINT('Ctrl Pts',(-18.3136241193877,-13.3271808481679,
114.771418148599)) ;
#183475 = CARTESIAN_POINT('Ctrl Pts',(-18.2398202736646,-13.3271809363831,
114.79564918327)) ;
#183476 = CARTESIAN_POINT('Ctrl Pts',(-18.1660164279415,-13.3271810245983,
114.819880217941)) ;
#183477 = CARTESIAN_POINT('Ctrl Pts',(-18.1424479380569,-13.3199158123169,
114.748094402225)) ;
#183478 = CARTESIAN_POINT('Ctrl Pts',(-18.1188794481722,-13.3126506000355,
114.676308586509)) ;
#183479 = CARTESIAN_POINT('Ctrl Pts',(-18.1926832938953,-13.3126505118203,
114.652077551838)) ;
#183480 = CARTESIAN_POINT('Ctrl Pts',(-18.2664871396184,-13.312650423605,
114.627846517168)) ;
#183481 = CARTESIAN_POINT('Ctrl Pts',(-18.2900556295031,-13.3199156358865,
114.699632332883)) ;
#183482 = CARTESIAN_POINT('Ctrl Pts',(-18.2835244771423,-13.61053350134,114.715169773089)) ;
#183483 = CARTESIAN_POINT('Ctrl Pts',(-18.3068513562178,-13.5975190949255,
114.786219681388)) ;
#183484 = CARTESIAN_POINT('Ctrl Pts',(-18.2330475175386,-13.5975191756466,
114.810450737514)) ;
#183485 = CARTESIAN_POINT('Ctrl Pts',(-18.1592436788595,-13.5975192563676,
114.834681793639)) ;
#183486 = CARTESIAN_POINT('Ctrl Pts',(-18.1359167997839,-13.6105336627821,
114.76363188534)) ;
#183487 = CARTESIAN_POINT('Ctrl Pts',(-18.1125899207084,-13.6235480691965,
114.692581977042)) ;
#183488 = CARTESIAN_POINT('Ctrl Pts',(-18.1863937593876,-13.6235479884755,
114.668350920916)) ;
#183489 = CARTESIAN_POINT('Ctrl Pts',(-18.2601975980667,-13.6235479077544,
114.644119864791)) ;
#183490 = CARTESIAN_POINT('Ctrl Pts',(-18.2835244771423,-13.61053350134,114.715169773089)) ;
#183491 = CARTESIAN_POINT('Ctrl Pts',(-18.300904682681,-13.8877845324202,
114.80358738621)) ;
#183492 = CARTESIAN_POINT('Ctrl Pts',(-18.3223191972819,-13.8553930149523,
114.868812541022)) ;
#183493 = CARTESIAN_POINT('Ctrl Pts',(-18.2485153641365,-13.8553930819553,
114.893043614003)) ;
#183494 = CARTESIAN_POINT('Ctrl Pts',(-18.1747115309911,-13.8553931489583,
114.917274686983)) ;
#183495 = CARTESIAN_POINT('Ctrl Pts',(-18.1532970163902,-13.8877846664262,
114.85204953217)) ;
#183496 = CARTESIAN_POINT('Ctrl Pts',(-18.1318825017893,-13.9201761838941,
114.786824377358)) ;
#183497 = CARTESIAN_POINT('Ctrl Pts',(-18.2056863349347,-13.9201761168911,
114.762593304377)) ;
#183498 = CARTESIAN_POINT('Ctrl Pts',(-18.2794901680801,-13.9201760498881,
114.738362231397)) ;
#183499 = CARTESIAN_POINT('Ctrl Pts',(-18.300904682681,-13.8877845324202,
114.80358738621)) ;
#183500 = CARTESIAN_POINT('Ctrl Pts',(-18.3402955625269,-14.1315208949384,
114.95907694666)) ;
#183501 = CARTESIAN_POINT('Ctrl Pts',(-18.3582574587125,-14.0820626171462,
115.01378598302)) ;
#183502 = CARTESIAN_POINT('Ctrl Pts',(-18.2844536290332,-14.0820626666498,
115.038017066558)) ;
#183503 = CARTESIAN_POINT('Ctrl Pts',(-18.210649799354,-14.0820627161535,
115.062248150096)) ;
#183504 = CARTESIAN_POINT('Ctrl Pts',(-18.1926879031684,-14.1315209939457,
115.007539113736)) ;
#183505 = CARTESIAN_POINT('Ctrl Pts',(-18.1747260069828,-14.1809792717379,
114.952830077376)) ;
#183506 = CARTESIAN_POINT('Ctrl Pts',(-18.2485298366621,-14.1809792222342,
114.928598993838)) ;
#183507 = CARTESIAN_POINT('Ctrl Pts',(-18.3223336663413,-14.1809791727306,
114.9043679103)) ;
#183508 = CARTESIAN_POINT('Ctrl Pts',(-18.3402955625269,-14.1315208949384,
114.95907694666)) ;
#183509 = CARTESIAN_POINT('Ctrl Pts',(-18.3979499293583,-14.3236676354294,
115.170121270634)) ;
#183510 = CARTESIAN_POINT('Ctrl Pts',(-18.4111802519547,-14.2607186290668,
115.210418697435)) ;
#183511 = CARTESIAN_POINT('Ctrl Pts',(-18.3373764237579,-14.260718660624,
115.234649785488)) ;
#183512 = CARTESIAN_POINT('Ctrl Pts',(-18.2635725955611,-14.2607186921811,
115.258880873542)) ;
#183513 = CARTESIAN_POINT('Ctrl Pts',(-18.2503422729647,-14.3236676985437,
115.21858344674)) ;
#183514 = CARTESIAN_POINT('Ctrl Pts',(-18.2371119503683,-14.3866167049062,
115.178286019939)) ;
#183515 = CARTESIAN_POINT('Ctrl Pts',(-18.3109157785651,-14.3866166733491,
115.154054931886)) ;
#183516 = CARTESIAN_POINT('Ctrl Pts',(-18.3847196067618,-14.3866166417919,
115.129823843832)) ;
#183517 = CARTESIAN_POINT('Ctrl Pts',(-18.3979499293583,-14.3236676354294,
115.170121270634)) ;
#183518 = CARTESIAN_POINT('Ctrl Pts',(-18.4691141873596,-14.451213086268,
115.422348614941)) ;
#183519 = CARTESIAN_POINT('Ctrl Pts',(-18.4766617833605,-14.3792631912131,
115.445337373605)) ;
#183520 = CARTESIAN_POINT('Ctrl Pts',(-18.402857954655,-14.3792632058746,
115.469568460109)) ;
#183521 = CARTESIAN_POINT('Ctrl Pts',(-18.3290541259495,-14.3792632205361,
115.493799546613)) ;
#183522 = CARTESIAN_POINT('Ctrl Pts',(-18.3215065299486,-14.451213115591,
115.470810787948)) ;
#183523 = CARTESIAN_POINT('Ctrl Pts',(-18.3139589339478,-14.5231630106458,
115.447822029284)) ;
#183524 = CARTESIAN_POINT('Ctrl Pts',(-18.3877627626533,-14.5231629959843,
115.42359094278)) ;
#183525 = CARTESIAN_POINT('Ctrl Pts',(-18.4615665913588,-14.5231629813228,
115.399359856276)) ;
#183526 = CARTESIAN_POINT('Ctrl Pts',(-18.4691141873596,-14.451213086268,
115.422348614941)) ;
#183527 = CARTESIAN_POINT('Ctrl Pts',(-18.5480547946809,-14.5046478984509,
115.698323016836)) ;
#183528 = CARTESIAN_POINT('Ctrl Pts',(-18.5493667384091,-14.4288576762163,
115.702318984979)) ;
#183529 = CARTESIAN_POINT('Ctrl Pts',(-18.4755629074551,-14.4288576774106,
115.726550064634)) ;
#183530 = CARTESIAN_POINT('Ctrl Pts',(-18.4017590765011,-14.4288576786049,
115.750781144289)) ;
#183531 = CARTESIAN_POINT('Ctrl Pts',(-18.4004471327729,-14.5046479008395,
115.746785176146)) ;
#183532 = CARTESIAN_POINT('Ctrl Pts',(-18.3991351890446,-14.5804381230741,
115.742789208003)) ;
#183533 = CARTESIAN_POINT('Ctrl Pts',(-18.4729390199986,-14.5804381218798,
115.718558128348)) ;
#183534 = CARTESIAN_POINT('Ctrl Pts',(-18.5467428509526,-14.5804381206855,
115.694327048693)) ;
#183535 = CARTESIAN_POINT('Ctrl Pts',(-18.5480547946809,-14.5046478984509,
115.698323016836)) ;
#183536 = CARTESIAN_POINT('Ctrl Pts',(-18.6278722273307,-14.4801334339684,
115.976822091214)) ;
#183537 = CARTESIAN_POINT('Ctrl Pts',(-18.6228807745293,-14.4059401882447,
115.961618930727)) ;
#183538 = CARTESIAN_POINT('Ctrl Pts',(-18.5490769408651,-14.405940180657,
115.985850002128)) ;
#183539 = CARTESIAN_POINT('Ctrl Pts',(-18.475273107201,-14.4059401730692,
116.010081073528)) ;
#183540 = CARTESIAN_POINT('Ctrl Pts',(-18.4802645600025,-14.4801334187929,
116.025284234015)) ;
#183541 = CARTESIAN_POINT('Ctrl Pts',(-18.4852560128039,-14.5543266645165,
116.040487394502)) ;
#183542 = CARTESIAN_POINT('Ctrl Pts',(-18.5590598464681,-14.5543266721042,
116.016256323101)) ;
#183543 = CARTESIAN_POINT('Ctrl Pts',(-18.6328636801322,-14.554326679692,
115.9920252517)) ;
#183544 = CARTESIAN_POINT('Ctrl Pts',(-18.6278722273307,-14.4801334339684,
115.976822091214)) ;
#183545 = CARTESIAN_POINT('Ctrl Pts',(-18.7025035045635,-14.3800974324411,
116.239533090197)) ;
#183546 = CARTESIAN_POINT('Ctrl Pts',(-18.6915610435405,-14.3127767665056,
116.206204119007)) ;
#183547 = CARTESIAN_POINT('Ctrl Pts',(-18.6177572067622,-14.3127767543614,
116.230435180923)) ;
#183548 = CARTESIAN_POINT('Ctrl Pts',(-18.5439533699839,-14.3127767422172,
116.254666242838)) ;
#183549 = CARTESIAN_POINT('Ctrl Pts',(-18.5548958310069,-14.3800974081526,
116.287995214028)) ;
#183550 = CARTESIAN_POINT('Ctrl Pts',(-18.56583829203,-14.4474180740881,116.321324185218)) ;
#183551 = CARTESIAN_POINT('Ctrl Pts',(-18.6396421288082,-14.4474180862324,
116.297093123302)) ;
#183552 = CARTESIAN_POINT('Ctrl Pts',(-18.7134459655865,-14.4474180983766,
116.272862061387)) ;
#183553 = CARTESIAN_POINT('Ctrl Pts',(-18.7025035045635,-14.3800974324411,
116.239533090197)) ;
#183554 = CARTESIAN_POINT('Ctrl Pts',(-18.7661852178501,-14.2097836883392,
116.469145099282)) ;
#183555 = CARTESIAN_POINT('Ctrl Pts',(-18.7500418045665,-14.1542529210645,
116.419974866854)) ;
#183556 = CARTESIAN_POINT('Ctrl Pts',(-18.6762379644893,-14.1542529100711,
116.444205918722)) ;
#183557 = CARTESIAN_POINT('Ctrl Pts',(-18.6024341244121,-14.1542528990776,
116.468436970589)) ;
#183558 = CARTESIAN_POINT('Ctrl Pts',(-18.6185775376956,-14.2097836663522,
116.517607203017)) ;
#183559 = CARTESIAN_POINT('Ctrl Pts',(-18.6347209509792,-14.2653144336269,
116.566777435444)) ;
#183560 = CARTESIAN_POINT('Ctrl Pts',(-18.7085247910564,-14.2653144446203,
116.542546383577)) ;
#183561 = CARTESIAN_POINT('Ctrl Pts',(-18.7823286311337,-14.2653144556138,
116.518315331709)) ;
#183562 = CARTESIAN_POINT('Ctrl Pts',(-18.7661852178501,-14.2097836883392,
116.469145099282)) ;
#183563 = CARTESIAN_POINT('Ctrl Pts',(-18.8126736298305,-13.9844447661634,
116.646062755378)) ;
#183564 = CARTESIAN_POINT('Ctrl Pts',(-18.7925289620469,-13.944564790948,
116.584705347452)) ;
#183565 = CARTESIAN_POINT('Ctrl Pts',(-18.7187251200822,-13.9445647824093,
116.60893639357)) ;
#183566 = CARTESIAN_POINT('Ctrl Pts',(-18.6449212781175,-13.9445647738706,
116.633167439689)) ;
#183567 = CARTESIAN_POINT('Ctrl Pts',(-18.6650659459011,-13.984444749086,
116.694524847615)) ;
#183568 = CARTESIAN_POINT('Ctrl Pts',(-18.6852106136848,-14.0243247243014,
116.755882255542)) ;
#183569 = CARTESIAN_POINT('Ctrl Pts',(-18.7590144556495,-14.0243247328401,
116.731651209424)) ;
#183570 = CARTESIAN_POINT('Ctrl Pts',(-18.8328182976142,-14.0243247413788,
116.707420163305)) ;
#183571 = CARTESIAN_POINT('Ctrl Pts',(-18.8126736298305,-13.9844447661634,
116.646062755378)) ;
#183572 = CARTESIAN_POINT('Ctrl Pts',(-18.8387106000838,-13.7175338810347,
116.760872830317)) ;
#183573 = CARTESIAN_POINT('Ctrl Pts',(-18.815982735405,-13.6962312533339,
116.691647421561)) ;
#183574 = CARTESIAN_POINT('Ctrl Pts',(-18.7421788921662,-13.6962312496336,
116.715878463799)) ;
#183575 = CARTESIAN_POINT('Ctrl Pts',(-18.6683750489273,-13.6962312459334,
116.740109506036)) ;
#183576 = CARTESIAN_POINT('Ctrl Pts',(-18.691102913606,-13.7175338736341,
116.809334914792)) ;
#183577 = CARTESIAN_POINT('Ctrl Pts',(-18.7138307782847,-13.7388365013348,
116.878560323548)) ;
#183578 = CARTESIAN_POINT('Ctrl Pts',(-18.7876346215236,-13.7388365050351,
116.85432928131)) ;
#183579 = CARTESIAN_POINT('Ctrl Pts',(-18.8614384647625,-13.7388365087354,
116.830098239072)) ;
#183580 = CARTESIAN_POINT('Ctrl Pts',(-18.8387106000838,-13.7175338810347,
116.760872830317)) ;
#183581 = CARTESIAN_POINT('Ctrl Pts',(-18.8412499966495,-13.4290941380284,
116.804105500737)) ;
#183582 = CARTESIAN_POINT('Ctrl Pts',(-18.8175760945561,-13.42790072271,116.731998614741)) ;
#183583 = CARTESIAN_POINT('Ctrl Pts',(-18.7437722510543,-13.4279007232461,
116.756229656177)) ;
#183584 = CARTESIAN_POINT('Ctrl Pts',(-18.6699684075526,-13.4279007237822,
116.780460697614)) ;
#183585 = CARTESIAN_POINT('Ctrl Pts',(-18.693642309646,-13.4290941391006,
116.852567583611)) ;
#183586 = CARTESIAN_POINT('Ctrl Pts',(-18.7173162117394,-13.430287554419,
116.924674469607)) ;
#183587 = CARTESIAN_POINT('Ctrl Pts',(-18.7911200552412,-13.4302875538829,
116.90044342817)) ;
#183588 = CARTESIAN_POINT('Ctrl Pts',(-18.864923898743,-13.4302875533468,
116.876212386733)) ;
#183589 = CARTESIAN_POINT('Ctrl Pts',(-18.8412499966495,-13.4290941380284,
116.804105500737)) ;
#183590 = CARTESIAN_POINT('Ctrl Pts',(-18.8195971871137,-13.1407025280343,
116.773545460015)) ;
#183591 = CARTESIAN_POINT('Ctrl Pts',(-18.7966675811409,-13.1596450179659,
116.703705579957)) ;
#183592 = CARTESIAN_POINT('Ctrl Pts',(-18.7228637379266,-13.1596450208018,
116.727936622269)) ;
#183593 = CARTESIAN_POINT('Ctrl Pts',(-18.6490598947122,-13.1596450236377,
116.752167664581)) ;
#183594 = CARTESIAN_POINT('Ctrl Pts',(-18.671989500685,-13.1407025337061,
116.82200754464)) ;
#183595 = CARTESIAN_POINT('Ctrl Pts',(-18.6949191066578,-13.1217600437745,
116.891847424699)) ;
#183596 = CARTESIAN_POINT('Ctrl Pts',(-18.7687229498721,-13.1217600409386,
116.867616382386)) ;
#183597 = CARTESIAN_POINT('Ctrl Pts',(-18.8425267930865,-13.1217600381026,
116.843385340074)) ;
#183598 = CARTESIAN_POINT('Ctrl Pts',(-18.8195971871137,-13.1407025280343,
116.773545460015)) ;
#183599 = CARTESIAN_POINT('Ctrl Pts',(-18.7741929648226,-12.8707969653127,
116.670833856634)) ;
#183600 = CARTESIAN_POINT('Ctrl Pts',(-18.7536634762867,-12.9086154474282,
116.608304347037)) ;
#183601 = CARTESIAN_POINT('Ctrl Pts',(-18.6798596333953,-12.9086154501767,
116.632535390332)) ;
#183602 = CARTESIAN_POINT('Ctrl Pts',(-18.6060557905039,-12.9086154529253,
116.656766433628)) ;
#183603 = CARTESIAN_POINT('Ctrl Pts',(-18.6265852790397,-12.8707969708098,
116.719295943226)) ;
#183604 = CARTESIAN_POINT('Ctrl Pts',(-18.6471147675756,-12.8329784886943,
116.781825452824)) ;
#183605 = CARTESIAN_POINT('Ctrl Pts',(-18.720918610467,-12.8329784859458,
116.757594409528)) ;
#183606 = CARTESIAN_POINT('Ctrl Pts',(-18.7947224533584,-12.8329784831972,
116.733363366232)) ;
#183607 = CARTESIAN_POINT('Ctrl Pts',(-18.7741929648226,-12.8707969653127,
116.670833856634)) ;
#183608 = CARTESIAN_POINT('Ctrl Pts',(-18.7081893525992,-12.6417711077458,
116.505122794438)) ;
#183609 = CARTESIAN_POINT('Ctrl Pts',(-18.6915075220937,-12.6956372286185,
116.454312630352)) ;
#183610 = CARTESIAN_POINT('Ctrl Pts',(-18.6177036790936,-12.6956372295276,
116.478543673317)) ;
#183611 = CARTESIAN_POINT('Ctrl Pts',(-18.5438998360935,-12.6956372304368,
116.502774716282)) ;
#183612 = CARTESIAN_POINT('Ctrl Pts',(-18.5605816665991,-12.6417711095641,
116.553584880368)) ;
#183613 = CARTESIAN_POINT('Ctrl Pts',(-18.5772634971046,-12.5879049886915,
116.604395044454)) ;
#183614 = CARTESIAN_POINT('Ctrl Pts',(-18.6510673401047,-12.5879049877823,
116.580164001489)) ;
#183615 = CARTESIAN_POINT('Ctrl Pts',(-18.7248711831048,-12.5879049868731,
116.555932958525)) ;
#183616 = CARTESIAN_POINT('Ctrl Pts',(-18.7081893525992,-12.6417711077458,
116.505122794438)) ;
#183617 = CARTESIAN_POINT('Ctrl Pts',(-18.624745958435,-12.4670674817275,
116.286513958254)) ;
#183618 = CARTESIAN_POINT('Ctrl Pts',(-18.6131306242191,-12.5332118470618,
116.251135524313)) ;
#183619 = CARTESIAN_POINT('Ctrl Pts',(-18.5393267802208,-12.5332118456008,
116.275366564238)) ;
#183620 = CARTESIAN_POINT('Ctrl Pts',(-18.4655229362226,-12.5332118441398,
116.299597604162)) ;
#183621 = CARTESIAN_POINT('Ctrl Pts',(-18.4771382704385,-12.4670674788054,
116.334976038103)) ;
#183622 = CARTESIAN_POINT('Ctrl Pts',(-18.4887536046544,-12.4009231134711,
116.370354472043)) ;
#183623 = CARTESIAN_POINT('Ctrl Pts',(-18.5625574486526,-12.4009231149321,
116.346123432119)) ;
#183624 = CARTESIAN_POINT('Ctrl Pts',(-18.6363612926509,-12.4009231163931,
116.321892392194)) ;
#183625 = CARTESIAN_POINT('Ctrl Pts',(-18.624745958435,-12.4670674817275,
116.286513958254)) ;
#183626 = CARTESIAN_POINT('Ctrl Pts',(-18.5299237726579,-12.3610581795072,
116.033065517688)) ;
#183627 = CARTESIAN_POINT('Ctrl Pts',(-18.5241806065629,-12.434700867629,
116.015572760285)) ;
#183628 = CARTESIAN_POINT('Ctrl Pts',(-18.4503767610872,-12.4347008654183,
116.039803795709)) ;
#183629 = CARTESIAN_POINT('Ctrl Pts',(-18.3765729156115,-12.4347008632077,
116.064034831134)) ;
#183630 = CARTESIAN_POINT('Ctrl Pts',(-18.3823160817065,-12.3610581750859,
116.081527588537)) ;
#183631 = CARTESIAN_POINT('Ctrl Pts',(-18.3880592478014,-12.2874154869641,
116.09902034594)) ;
#183632 = CARTESIAN_POINT('Ctrl Pts',(-18.4618630932771,-12.2874154891748,
116.074789310515)) ;
#183633 = CARTESIAN_POINT('Ctrl Pts',(-18.5356669387528,-12.2874154913854,
116.050558275091)) ;
#183634 = CARTESIAN_POINT('Ctrl Pts',(-18.5299237726579,-12.3610581795072,
116.033065517688)) ;
#183635 = CARTESIAN_POINT('Ctrl Pts',(-18.4285423943449,-12.3304705905987,
115.759931665259)) ;
#183636 = CARTESIAN_POINT('Ctrl Pts',(-18.4291318873858,-12.4063567534876,
115.761727165661)) ;
#183637 = CARTESIAN_POINT('Ctrl Pts',(-18.3553280393615,-12.4063567532817,
115.785958193323)) ;
#183638 = CARTESIAN_POINT('Ctrl Pts',(-18.2815241913372,-12.4063567530759,
115.810189220985)) ;
#183639 = CARTESIAN_POINT('Ctrl Pts',(-18.2809346982963,-12.330470590187,
115.808393720582)) ;
#183640 = CARTESIAN_POINT('Ctrl Pts',(-18.2803452052554,-12.2545844272981,
115.80659822018)) ;
#183641 = CARTESIAN_POINT('Ctrl Pts',(-18.3541490532797,-12.254584427504,
115.782367192518)) ;
#183642 = CARTESIAN_POINT('Ctrl Pts',(-18.427952901304,-12.2545844277098,
115.758136164857)) ;
#183643 = CARTESIAN_POINT('Ctrl Pts',(-18.4285423943449,-12.3304705905987,
115.759931665259)) ;
#183644 = CARTESIAN_POINT('Ctrl Pts',(-18.3286734717406,-12.3780041179342,
115.491117750201)) ;
#183645 = CARTESIAN_POINT('Ctrl Pts',(-18.3355049446952,-12.4506811357788,
115.511925314151)) ;
#183646 = CARTESIAN_POINT('Ctrl Pts',(-18.2617010948026,-12.4506811414498,
115.536156336123)) ;
#183647 = CARTESIAN_POINT('Ctrl Pts',(-18.1878972449099,-12.4506811471207,
115.560387358094)) ;
#183648 = CARTESIAN_POINT('Ctrl Pts',(-18.1810657719553,-12.3780041292761,
115.539579794144)) ;
#183649 = CARTESIAN_POINT('Ctrl Pts',(-18.1742342990006,-12.3053271114316,
115.518772230194)) ;
#183650 = CARTESIAN_POINT('Ctrl Pts',(-18.2480381488933,-12.3053271057606,
115.494541208223)) ;
#183651 = CARTESIAN_POINT('Ctrl Pts',(-18.321841998786,-12.3053271000897,
115.470310186251)) ;
#183652 = CARTESIAN_POINT('Ctrl Pts',(-18.3286734717406,-12.3780041179342,
115.491117750201)) ;
#183653 = CARTESIAN_POINT('Ctrl Pts',(-18.2355472337233,-12.5002675543906,
115.242998586149)) ;
#183654 = CARTESIAN_POINT('Ctrl Pts',(-18.2481556577856,-12.5645133223993,
115.281401810897)) ;
#183655 = CARTESIAN_POINT('Ctrl Pts',(-18.1743518063322,-12.5645133380227,
115.305632828115)) ;
#183656 = CARTESIAN_POINT('Ctrl Pts',(-18.1005479548788,-12.5645133536461,
115.329863845332)) ;
#183657 = CARTESIAN_POINT('Ctrl Pts',(-18.0879395308165,-12.5002675856374,
115.291460620583)) ;
#183658 = CARTESIAN_POINT('Ctrl Pts',(-18.0753311067543,-12.4360218176287,
115.253057395835)) ;
#183659 = CARTESIAN_POINT('Ctrl Pts',(-18.1491349582077,-12.4360218020053,
115.228826378617)) ;
#183660 = CARTESIAN_POINT('Ctrl Pts',(-18.2229388096611,-12.4360217863819,
115.2045953614)) ;
#183661 = CARTESIAN_POINT('Ctrl Pts',(-18.2355472337233,-12.5002675543906,
115.242998586149)) ;
#183662 = CARTESIAN_POINT('Ctrl Pts',(-18.1559065411703,-12.6872113223539,
115.03574587489)) ;
#183663 = CARTESIAN_POINT('Ctrl Pts',(-18.1733627764867,-12.7384971666027,
115.08891475039)) ;
#183664 = CARTESIAN_POINT('Ctrl Pts',(-18.099558925084,-12.7384971937162,
115.113145767762)) ;
#183665 = CARTESIAN_POINT('Ctrl Pts',(-18.0257550736814,-12.7384972208297,
115.137376785134)) ;
#183666 = CARTESIAN_POINT('Ctrl Pts',(-18.008298838365,-12.6872113765809,
115.084207909633)) ;
#183667 = CARTESIAN_POINT('Ctrl Pts',(-17.9908426030485,-12.635925532332,
115.031039034133)) ;
#183668 = CARTESIAN_POINT('Ctrl Pts',(-18.0646464544512,-12.6359255052185,
115.006808016761)) ;
#183669 = CARTESIAN_POINT('Ctrl Pts',(-18.1384503058539,-12.635925478105,
114.98257699939)) ;
#183670 = CARTESIAN_POINT('Ctrl Pts',(-18.1559065411703,-12.6872113223539,
115.03574587489)) ;
#183671 = CARTESIAN_POINT('Ctrl Pts',(-18.0936528156396,-12.928470822573,
114.881781285062)) ;
#183672 = CARTESIAN_POINT('Ctrl Pts',(-18.1147432667107,-12.9629864518457,
114.946019395169)) ;
#183673 = CARTESIAN_POINT('Ctrl Pts',(-18.0409394163538,-12.9629864941427,
114.970250415726)) ;
#183674 = CARTESIAN_POINT('Ctrl Pts',(-17.9671355659969,-12.9629865364398,
114.994481436283)) ;
#183675 = CARTESIAN_POINT('Ctrl Pts',(-17.9460451149259,-12.9284709071671,
114.930243326176)) ;
#183676 = CARTESIAN_POINT('Ctrl Pts',(-17.9249546638548,-12.8939552778944,
114.866005216069)) ;
#183677 = CARTESIAN_POINT('Ctrl Pts',(-17.9987585142116,-12.8939552355973,
114.841774195512)) ;
#183678 = CARTESIAN_POINT('Ctrl Pts',(-18.0725623645685,-12.8939551933003,
114.817543174955)) ;
#183679 = CARTESIAN_POINT('Ctrl Pts',(-18.0936528156396,-12.928470822573,
114.881781285062)) ;
#183680 = CARTESIAN_POINT('Ctrl Pts',(-18.053566961881,-13.2034657060163,
114.795110966265)) ;
#183681 = CARTESIAN_POINT('Ctrl Pts',(-18.0767535884705,-13.2188313176784,
114.865733688623)) ;
#183682 = CARTESIAN_POINT('Ctrl Pts',(-18.0029497413991,-13.2188313725587,
114.889964719188)) ;
#183683 = CARTESIAN_POINT('Ctrl Pts',(-17.9291458943278,-13.218831427439,
114.914195749752)) ;
#183684 = CARTESIAN_POINT('Ctrl Pts',(-17.9059592677383,-13.2034658157769,
114.843573027393)) ;
#183685 = CARTESIAN_POINT('Ctrl Pts',(-17.8827726411489,-13.1881002041148,
114.772950305034)) ;
#183686 = CARTESIAN_POINT('Ctrl Pts',(-17.9565764882202,-13.1881001492345,
114.74871927447)) ;
#183687 = CARTESIAN_POINT('Ctrl Pts',(-18.0303803352916,-13.1881000943542,
114.724488243906)) ;
#183688 = CARTESIAN_POINT('Ctrl Pts',(-18.053566961881,-13.2034657060163,
114.795110966265)) ;
#183689 = CARTESIAN_POINT('Ctrl Pts',(-18.0372153758526,-13.4939400108665,
114.780761585915)) ;
#183690 = CARTESIAN_POINT('Ctrl Pts',(-18.0608435214232,-13.4890474543543,
114.852729103689)) ;
#183691 = CARTESIAN_POINT('Ctrl Pts',(-17.9870396792037,-13.4890475187126,
114.876960149031)) ;
#183692 = CARTESIAN_POINT('Ctrl Pts',(-17.9132358369841,-13.4890475830709,
114.901191194373)) ;
#183693 = CARTESIAN_POINT('Ctrl Pts',(-17.8896076914135,-13.4939401395831,
114.829223676599)) ;
#183694 = CARTESIAN_POINT('Ctrl Pts',(-17.8659795458429,-13.4988326960953,
114.757256158824)) ;
#183695 = CARTESIAN_POINT('Ctrl Pts',(-17.9397833880625,-13.498832631737,
114.733025113482)) ;
#183696 = CARTESIAN_POINT('Ctrl Pts',(-18.0135872302821,-13.4988325673787,
114.70879406814)) ;
#183697 = CARTESIAN_POINT('Ctrl Pts',(-18.0372153758526,-13.4939400108665,
114.780761585915)) ;
#183698 = CARTESIAN_POINT('Ctrl Pts',(-18.045087176113,-13.7785749983251,
114.84013824791)) ;
#183699 = CARTESIAN_POINT('Ctrl Pts',(-18.0674673661548,-13.7538028114636,
114.908304694356)) ;
#183700 = CARTESIAN_POINT('Ctrl Pts',(-17.9936635300079,-13.7538028795782,
114.932535758194)) ;
#183701 = CARTESIAN_POINT('Ctrl Pts',(-17.9198596938609,-13.7538029476928,
114.956766822033)) ;
#183702 = CARTESIAN_POINT('Ctrl Pts',(-17.8974795038191,-13.7785751345543,
114.888600375587)) ;
#183703 = CARTESIAN_POINT('Ctrl Pts',(-17.8750993137773,-13.8033473214157,
114.820433929141)) ;
#183704 = CARTESIAN_POINT('Ctrl Pts',(-17.9489031499242,-13.8033472533012,
114.796202865303)) ;
#183705 = CARTESIAN_POINT('Ctrl Pts',(-18.0227069860712,-13.8033471851866,
114.771971801464)) ;
#183706 = CARTESIAN_POINT('Ctrl Pts',(-18.045087176113,-13.7785749983251,
114.84013824791)) ;
#183707 = CARTESIAN_POINT('Ctrl Pts',(-18.0758126785522,-14.0376123935157,
114.969142216543)) ;
#183708 = CARTESIAN_POINT('Ctrl Pts',(-18.0953472138535,-13.9947190826741,
115.028641257654)) ;
#183709 = CARTESIAN_POINT('Ctrl Pts',(-18.0215433843608,-13.9947191481114,
115.05287234176)) ;
#183710 = CARTESIAN_POINT('Ctrl Pts',(-17.947739554868,-13.9947192135486,
115.077103425866)) ;
#183711 = CARTESIAN_POINT('Ctrl Pts',(-17.9282050195667,-14.0376125243903,
115.017604384755)) ;
#183712 = CARTESIAN_POINT('Ctrl Pts',(-17.9086704842654,-14.0805058352319,
114.958105343643)) ;
#183713 = CARTESIAN_POINT('Ctrl Pts',(-17.9824743137582,-14.0805057697947,
114.933874259537)) ;
#183714 = CARTESIAN_POINT('Ctrl Pts',(-18.0562781432509,-14.0805057043574,
114.909643175431)) ;
#183715 = CARTESIAN_POINT('Ctrl Pts',(-18.0758126785522,-14.0376123935157,
114.969142216543)) ;
#183716 = CARTESIAN_POINT('Ctrl Pts',(-18.126546298458,-14.2526152270872,
115.159131089373)) ;
#183717 = CARTESIAN_POINT('Ctrl Pts',(-18.1418333641264,-14.1946488297789,
115.205693023175)) ;
#183718 = CARTESIAN_POINT('Ctrl Pts',(-18.0680295412189,-14.1946488854693,
115.229924127339)) ;
#183719 = CARTESIAN_POINT('Ctrl Pts',(-17.9942257183115,-14.1946489411597,
115.254155231503)) ;
#183720 = CARTESIAN_POINT('Ctrl Pts',(-17.9789386526431,-14.252615338468,
115.207593297701)) ;
#183721 = CARTESIAN_POINT('Ctrl Pts',(-17.9636515869747,-14.3105817357762,
115.161031363899)) ;
#183722 = CARTESIAN_POINT('Ctrl Pts',(-18.0374554098822,-14.3105816800858,
115.136800259735)) ;
#183723 = CARTESIAN_POINT('Ctrl Pts',(-18.1112592327896,-14.3105816243954,
115.112569155571)) ;
#183724 = CARTESIAN_POINT('Ctrl Pts',(-18.126546298458,-14.2526152270872,
115.159131089373)) ;
#183725 = CARTESIAN_POINT('Ctrl Pts',(-18.1929627182085,-14.4080507138092,
115.39693012817)) ;
#183726 = CARTESIAN_POINT('Ctrl Pts',(-18.202900452688,-14.3391479238767,
115.427198862157)) ;
#183727 = CARTESIAN_POINT('Ctrl Pts',(-18.1290966355056,-14.3391479627699,
115.451429983758)) ;
#183728 = CARTESIAN_POINT('Ctrl Pts',(-18.055292818323,-14.3391480016631,
115.475661105359)) ;
#183729 = CARTESIAN_POINT('Ctrl Pts',(-18.0453550838435,-14.4080507915956,
115.445392371372)) ;
#183730 = CARTESIAN_POINT('Ctrl Pts',(-18.0354173493639,-14.4769535815281,
115.415123637385)) ;
#183731 = CARTESIAN_POINT('Ctrl Pts',(-18.1092211665464,-14.4769535426349,
115.390892515784)) ;
#183732 = CARTESIAN_POINT('Ctrl Pts',(-18.1830249837289,-14.4769535037417,
115.366661394183)) ;
#183733 = CARTESIAN_POINT('Ctrl Pts',(-18.1929627182085,-14.4080507138092,
115.39693012817)) ;
#183734 = CARTESIAN_POINT('Ctrl Pts',(-18.2695829032393,-14.4922598223547,
115.665846830142)) ;
#183735 = CARTESIAN_POINT('Ctrl Pts',(-18.2734503895257,-14.4173770699575,
115.677626567456)) ;
#183736 = CARTESIAN_POINT('Ctrl Pts',(-18.1996465763506,-14.4173770858156,
115.701857701262)) ;
#183737 = CARTESIAN_POINT('Ctrl Pts',(-18.1258427631755,-14.4173771016737,
115.726088835069)) ;
#183738 = CARTESIAN_POINT('Ctrl Pts',(-18.1219752768891,-14.4922598540709,
115.714309097756)) ;
#183739 = CARTESIAN_POINT('Ctrl Pts',(-18.1181077906028,-14.5671426064681,
115.702529360442)) ;
#183740 = CARTESIAN_POINT('Ctrl Pts',(-18.1919116037779,-14.56714259061,115.678298226636)) ;
#183741 = CARTESIAN_POINT('Ctrl Pts',(-18.265715416953,-14.5671425747519,
115.654067092829)) ;
#183742 = CARTESIAN_POINT('Ctrl Pts',(-18.2695829032393,-14.4922598223547,
115.665846830142)) ;
#183743 = CARTESIAN_POINT('Ctrl Pts',(-18.3495327203372,-14.4995566650645,
115.94467290167)) ;
#183744 = CARTESIAN_POINT('Ctrl Pts',(-18.3470933653197,-14.4240553765711,
115.937243017908)) ;
#183745 = CARTESIAN_POINT('Ctrl Pts',(-18.2732895534782,-14.4240553658153,
115.961474155777)) ;
#183746 = CARTESIAN_POINT('Ctrl Pts',(-18.1994857416366,-14.4240553550595,
115.985705293645)) ;
#183747 = CARTESIAN_POINT('Ctrl Pts',(-18.2019250966542,-14.4995566435528,
115.993135177407)) ;
#183748 = CARTESIAN_POINT('Ctrl Pts',(-18.2043644516717,-14.5750579320462,
116.000565061168)) ;
#183749 = CARTESIAN_POINT('Ctrl Pts',(-18.2781682635132,-14.575057942802,
115.9763339233)) ;
#183750 = CARTESIAN_POINT('Ctrl Pts',(-18.3519720753547,-14.5750579535578,
115.952102785431)) ;
#183751 = CARTESIAN_POINT('Ctrl Pts',(-18.3495327203372,-14.4995566650645,
115.94467290167)) ;
#183752 = CARTESIAN_POINT('Ctrl Pts',(-18.4275077803074,-14.4291954268347,
116.217786788456)) ;
#183753 = CARTESIAN_POINT('Ctrl Pts',(-18.418884064598,-14.3584951723125,
116.191520339796)) ;
#183754 = CARTESIAN_POINT('Ctrl Pts',(-18.3450802518238,-14.3584951335383,
116.215751474823)) ;
#183755 = CARTESIAN_POINT('Ctrl Pts',(-18.2712764390496,-14.358495094764,
116.239982609851)) ;
#183756 = CARTESIAN_POINT('Ctrl Pts',(-18.279900154759,-14.4291953492863,
116.266249058511)) ;
#183757 = CARTESIAN_POINT('Ctrl Pts',(-18.2885238704684,-14.4998956038086,
116.292515507171)) ;
#183758 = CARTESIAN_POINT('Ctrl Pts',(-18.3623276832426,-14.4998956425828,
116.268284372143)) ;
#183759 = CARTESIAN_POINT('Ctrl Pts',(-18.4361314960168,-14.499895681357,
116.244053237115)) ;
#183760 = CARTESIAN_POINT('Ctrl Pts',(-18.4275077803074,-14.4291954268347,
116.217786788456)) ;
#183761 = CARTESIAN_POINT('Ctrl Pts',(-18.4961354751818,-14.2862746553945,
116.462278671806)) ;
#183762 = CARTESIAN_POINT('Ctrl Pts',(-18.4819739418317,-14.2254484542933,
116.4191449241)) ;
#183763 = CARTESIAN_POINT('Ctrl Pts',(-18.4081701251921,-14.2254483895805,
116.443376047354)) ;
#183764 = CARTESIAN_POINT('Ctrl Pts',(-18.3343663085526,-14.2254483248678,
116.467607170609)) ;
#183765 = CARTESIAN_POINT('Ctrl Pts',(-18.3485278419026,-14.286274525969,
116.510740918315)) ;
#183766 = CARTESIAN_POINT('Ctrl Pts',(-18.3626893752527,-14.3471007270702,
116.553874666022)) ;
#183767 = CARTESIAN_POINT('Ctrl Pts',(-18.4364931918923,-14.347100791783,
116.529643542767)) ;
#183768 = CARTESIAN_POINT('Ctrl Pts',(-18.5102970085318,-14.3471008564957,
116.505412419513)) ;
#183769 = CARTESIAN_POINT('Ctrl Pts',(-18.4961354751818,-14.2862746553945,
116.462278671806)) ;
#183770 = CARTESIAN_POINT('Ctrl Pts',(-18.5499768620455,-14.0821782924177,
116.661608442272)) ;
#183771 = CARTESIAN_POINT('Ctrl Pts',(-18.5313042749872,-14.0355118999346,
116.60473475281)) ;
#183772 = CARTESIAN_POINT('Ctrl Pts',(-18.4575004522042,-14.0355118141507,
116.628965857352)) ;
#183773 = CARTESIAN_POINT('Ctrl Pts',(-18.3836966294212,-14.0355117283667,
116.653196961895)) ;
#183774 = CARTESIAN_POINT('Ctrl Pts',(-18.4023692164795,-14.0821781208498,
116.710070651357)) ;
#183775 = CARTESIAN_POINT('Ctrl Pts',(-18.4210418035377,-14.1288445133328,
116.766944340819)) ;
#183776 = CARTESIAN_POINT('Ctrl Pts',(-18.4948456263207,-14.1288445991168,
116.742713236277)) ;
#183777 = CARTESIAN_POINT('Ctrl Pts',(-18.5686494491038,-14.1288446849008,
116.718482131734)) ;
#183778 = CARTESIAN_POINT('Ctrl Pts',(-18.5499768620455,-14.0821782924177,
116.661608442272)) ;
#183779 = CARTESIAN_POINT('Ctrl Pts',(-18.5848332719322,-13.8298750263426,
116.803243954575)) ;
#183780 = CARTESIAN_POINT('Ctrl Pts',(-18.5629655938444,-13.8007543288235,
116.736638533363)) ;
#183781 = CARTESIAN_POINT('Ctrl Pts',(-18.4891617631906,-13.8007542285384,
116.760869613933)) ;
#183782 = CARTESIAN_POINT('Ctrl Pts',(-18.4153579325368,-13.8007541282534,
116.785100694502)) ;
#183783 = CARTESIAN_POINT('Ctrl Pts',(-18.4372256106246,-13.8298748257726,
116.851706115714)) ;
#183784 = CARTESIAN_POINT('Ctrl Pts',(-18.4590932887124,-13.8589955232917,
116.918311536925)) ;
#183785 = CARTESIAN_POINT('Ctrl Pts',(-18.5328971193662,-13.8589956235767,
116.894080456356)) ;
#183786 = CARTESIAN_POINT('Ctrl Pts',(-18.6067009500199,-13.8589957238618,
116.869849375786)) ;
#183787 = CARTESIAN_POINT('Ctrl Pts',(-18.5848332719322,-13.8298750263426,
116.803243954575)) ;
#183788 = CARTESIAN_POINT('Ctrl Pts',(-18.597136541653,-13.5470860719876,
116.876296357144)) ;
#183789 = CARTESIAN_POINT('Ctrl Pts',(-18.5736411104493,-13.5376651784076,
116.804733062608)) ;
#183790 = CARTESIAN_POINT('Ctrl Pts',(-18.4998372709234,-13.5376650723535,
116.828964116154)) ;
#183791 = CARTESIAN_POINT('Ctrl Pts',(-18.4260334313975,-13.5376649662995,
116.8531951697)) ;
#183792 = CARTESIAN_POINT('Ctrl Pts',(-18.4495288626012,-13.5470858598794,
116.924758464237)) ;
#183793 = CARTESIAN_POINT('Ctrl Pts',(-18.4730242938049,-13.5565067534594,
116.996321758773)) ;
#183794 = CARTESIAN_POINT('Ctrl Pts',(-18.5468281333308,-13.5565068595135,
116.972090705226)) ;
#183795 = CARTESIAN_POINT('Ctrl Pts',(-18.6206319728567,-13.5565069655676,
116.94785965168)) ;
#183796 = CARTESIAN_POINT('Ctrl Pts',(-18.597136541653,-13.5470860719876,
116.876296357144)) ;
#183797 = CARTESIAN_POINT('Ctrl Pts',(-18.5852386802465,-13.2560613841224,
116.875504551637)) ;
#183798 = CARTESIAN_POINT('Ctrl Pts',(-18.561805431591,-13.2669448864172,
116.804130655157)) ;
#183799 = CARTESIAN_POINT('Ctrl Pts',(-18.4880015832393,-13.266944783336,
116.828361681822)) ;
#183800 = CARTESIAN_POINT('Ctrl Pts',(-18.4141977348876,-13.2669446802549,
116.852592708486)) ;
#183801 = CARTESIAN_POINT('Ctrl Pts',(-18.4376309835431,-13.2560611779601,
116.923966604966)) ;
#183802 = CARTESIAN_POINT('Ctrl Pts',(-18.4610642321986,-13.2451776756653,
116.995340501446)) ;
#183803 = CARTESIAN_POINT('Ctrl Pts',(-18.5348680805503,-13.2451777787465,
116.971109474781)) ;
#183804 = CARTESIAN_POINT('Ctrl Pts',(-18.6086719289019,-13.2451778818276,
116.946878448116)) ;
#183805 = CARTESIAN_POINT('Ctrl Pts',(-18.5852386802465,-13.2560613841224,
116.875504551637)) ;
#183806 = CARTESIAN_POINT('Ctrl Pts',(-18.549259012026,-12.9762949722028,
116.801413358043)) ;
#183807 = CARTESIAN_POINT('Ctrl Pts',(-18.5275681764739,-13.0067272528639,
116.735346570811)) ;
#183808 = CARTESIAN_POINT('Ctrl Pts',(-18.4537643202221,-13.0067271611354,
116.759577573413)) ;
#183809 = CARTESIAN_POINT('Ctrl Pts',(-18.3799604639702,-13.0067270694068,
116.783808576015)) ;
#183810 = CARTESIAN_POINT('Ctrl Pts',(-18.4016512995223,-12.9762947887458,
116.849875363246)) ;
#183811 = CARTESIAN_POINT('Ctrl Pts',(-18.4233421350744,-12.9458625080848,
116.915942150478)) ;
#183812 = CARTESIAN_POINT('Ctrl Pts',(-18.4971459913262,-12.9458625998133,
116.891711147876)) ;
#183813 = CARTESIAN_POINT('Ctrl Pts',(-18.570949847578,-12.9458626915418,
116.867480145274)) ;
#183814 = CARTESIAN_POINT('Ctrl Pts',(-18.549259012026,-12.9762949722028,
116.801413358043)) ;
#183815 = CARTESIAN_POINT('Ctrl Pts',(-18.4912772241492,-12.729021213087,
116.66017876415)) ;
#183816 = CARTESIAN_POINT('Ctrl Pts',(-18.4728702553292,-12.7767631435002,
116.604114105214)) ;
#183817 = CARTESIAN_POINT('Ctrl Pts',(-18.3990663927569,-12.7767630691524,
116.628345088564)) ;
#183818 = CARTESIAN_POINT('Ctrl Pts',(-18.3252625301846,-12.7767629948046,
116.652576071915)) ;
#183819 = CARTESIAN_POINT('Ctrl Pts',(-18.3436694990045,-12.7290210643915,
116.708640730851)) ;
#183820 = CARTESIAN_POINT('Ctrl Pts',(-18.3620764678245,-12.6812791339783,
116.764705389787)) ;
#183821 = CARTESIAN_POINT('Ctrl Pts',(-18.4358803303968,-12.6812792083261,
116.740474406437)) ;
#183822 = CARTESIAN_POINT('Ctrl Pts',(-18.5096841929691,-12.6812792826738,
116.716243423086)) ;
#183823 = CARTESIAN_POINT('Ctrl Pts',(-18.4912772241492,-12.729021213087,
116.66017876415)) ;
#183824 = CARTESIAN_POINT('Ctrl Pts',(-18.4142572250889,-12.5300504685621,
116.461103914665)) ;
#183825 = CARTESIAN_POINT('Ctrl Pts',(-18.4004650084343,-12.5917559666324,
116.419095046349)) ;
#183826 = CARTESIAN_POINT('Ctrl Pts',(-18.3266611418317,-12.5917559147477,
116.443326017425)) ;
#183827 = CARTESIAN_POINT('Ctrl Pts',(-18.2528572752292,-12.5917558628629,
116.4675569885)) ;
#183828 = CARTESIAN_POINT('Ctrl Pts',(-18.2666494918838,-12.5300503647925,
116.509565856816)) ;
#183829 = CARTESIAN_POINT('Ctrl Pts',(-18.2804417085384,-12.4683448667222,
116.551574725132)) ;
#183830 = CARTESIAN_POINT('Ctrl Pts',(-18.3542455751409,-12.468344918607,
116.527343754057)) ;
#183831 = CARTESIAN_POINT('Ctrl Pts',(-18.4280494417435,-12.4683449704918,
116.503112782981)) ;
#183832 = CARTESIAN_POINT('Ctrl Pts',(-18.4142572250889,-12.5300504685621,
116.461103914665)) ;
#183833 = CARTESIAN_POINT('Ctrl Pts',(-18.3230315098279,-12.3949013412461,
116.218789967548)) ;
#183834 = CARTESIAN_POINT('Ctrl Pts',(-18.3148521863386,-12.4661360013531,
116.193877066313)) ;
#183835 = CARTESIAN_POINT('Ctrl Pts',(-18.2410483183401,-12.4661359735393,
116.218108033137)) ;
#183836 = CARTESIAN_POINT('Ctrl Pts',(-18.1672444503415,-12.4661359457255,
116.24233899996)) ;
#183837 = CARTESIAN_POINT('Ctrl Pts',(-18.1754237738308,-12.3949012856185,
116.267251901195)) ;
#183838 = CARTESIAN_POINT('Ctrl Pts',(-18.18360309732,-12.3236666255115,116.29216480243)) ;
#183839 = CARTESIAN_POINT('Ctrl Pts',(-18.2574069653186,-12.3236666533253,
116.267933835606)) ;
#183840 = CARTESIAN_POINT('Ctrl Pts',(-18.3312108333171,-12.3236666811392,
116.243702868783)) ;
#183841 = CARTESIAN_POINT('Ctrl Pts',(-18.3230315098279,-12.3949013412461,
116.218789967548)) ;
#183842 = CARTESIAN_POINT('Ctrl Pts',(-18.223852812221,-12.3334783627152,
115.952132037095)) ;
#183843 = CARTESIAN_POINT('Ctrl Pts',(-18.2218527152486,-12.4091090544744,
115.946040062949)) ;
#183844 = CARTESIAN_POINT('Ctrl Pts',(-18.1480488479811,-12.4091090490569,
115.970271031999)) ;
#183845 = CARTESIAN_POINT('Ctrl Pts',(-18.0742449807137,-12.4091090436395,
115.99450200105)) ;
#183846 = CARTESIAN_POINT('Ctrl Pts',(-18.0762450776861,-12.3334783518803,
116.000593975195)) ;
#183847 = CARTESIAN_POINT('Ctrl Pts',(-18.0782451746585,-12.2578476601211,
116.006685949341)) ;
#183848 = CARTESIAN_POINT('Ctrl Pts',(-18.1520490419259,-12.2578476655386,
115.98245498029)) ;
#183849 = CARTESIAN_POINT('Ctrl Pts',(-18.2258529091934,-12.257847670956,
115.95822401124)) ;
#183850 = CARTESIAN_POINT('Ctrl Pts',(-18.223852812221,-12.3334783627152,
115.952132037095)) ;
#183851 = CARTESIAN_POINT('Ctrl Pts',(-18.1228645176016,-12.3494129205617,
115.679929191813)) ;
#183852 = CARTESIAN_POINT('Ctrl Pts',(-18.1271800410317,-12.4240452801496,
115.69307357853)) ;
#183853 = CARTESIAN_POINT('Ctrl Pts',(-18.0533761763498,-12.4240452938977,
115.717304555455)) ;
#183854 = CARTESIAN_POINT('Ctrl Pts',(-17.9795723116678,-12.4240453076458,
115.74153553238)) ;
#183855 = CARTESIAN_POINT('Ctrl Pts',(-17.9752567882376,-12.3494129480579,
115.728391145663)) ;
#183856 = CARTESIAN_POINT('Ctrl Pts',(-17.9709412648075,-12.27478058847,115.715246758947)) ;
#183857 = CARTESIAN_POINT('Ctrl Pts',(-18.0447451294895,-12.2747805747219,
115.691015782021)) ;
#183858 = CARTESIAN_POINT('Ctrl Pts',(-18.1185489941715,-12.2747805609737,
115.666784805096)) ;
#183859 = CARTESIAN_POINT('Ctrl Pts',(-18.1228645176016,-12.3494129205617,
115.679929191813)) ;
#183860 = CARTESIAN_POINT('Ctrl Pts',(-18.0261149973896,-12.4418688951199,
115.420743578469)) ;
#183861 = CARTESIAN_POINT('Ctrl Pts',(-18.036457582096,-12.5101591784945,
115.452245421536)) ;
#183862 = CARTESIAN_POINT('Ctrl Pts',(-17.9626537217423,-12.5101592062549,
115.476476411644)) ;
#183863 = CARTESIAN_POINT('Ctrl Pts',(-17.8888498613887,-12.5101592340153,
115.500707401753)) ;
#183864 = CARTESIAN_POINT('Ctrl Pts',(-17.8785072766823,-12.4418689506407,
115.469205558686)) ;
#183865 = CARTESIAN_POINT('Ctrl Pts',(-17.868164691976,-12.373578667266,115.43770371562)) ;
#183866 = CARTESIAN_POINT('Ctrl Pts',(-17.9419685523296,-12.3735786395056,
115.413472725511)) ;
#183867 = CARTESIAN_POINT('Ctrl Pts',(-18.0157724126832,-12.3735786117452,
115.389241735402)) ;
#183868 = CARTESIAN_POINT('Ctrl Pts',(-18.0261149973896,-12.4418688951199,
115.420743578469)) ;
#183869 = CARTESIAN_POINT('Ctrl Pts',(-17.9399661082425,-12.6051421932678,
115.193941498684)) ;
#183870 = CARTESIAN_POINT('Ctrl Pts',(-17.955602936904,-12.6621364558016,
115.241568754806)) ;
#183871 = CARTESIAN_POINT('Ctrl Pts',(-17.881799081728,-12.6621364903346,
115.265799760685)) ;
#183872 = CARTESIAN_POINT('Ctrl Pts',(-17.807995226552,-12.6621365248676,
115.290030766564)) ;
#183873 = CARTESIAN_POINT('Ctrl Pts',(-17.7923583978905,-12.6051422623338,
115.242403510442)) ;
#183874 = CARTESIAN_POINT('Ctrl Pts',(-17.776721569229,-12.5481479998,115.19477625432)) ;
#183875 = CARTESIAN_POINT('Ctrl Pts',(-17.850525424405,-12.548147965267,115.170545248441)) ;
#183876 = CARTESIAN_POINT('Ctrl Pts',(-17.9243292795811,-12.548147930734,
115.146314242563)) ;
#183877 = CARTESIAN_POINT('Ctrl Pts',(-17.9399661082425,-12.6051421932678,
115.193941498684)) ;
#183878 = CARTESIAN_POINT('Ctrl Pts',(-17.8706577437902,-12.824581983231,
115.018086912983)) ;
#183879 = CARTESIAN_POINT('Ctrl Pts',(-17.8904279981358,-12.866340572483,
115.078303916939)) ;
#183880 = CARTESIAN_POINT('Ctrl Pts',(-17.8166241473241,-12.8663406101773,
115.102534936111)) ;
#183881 = CARTESIAN_POINT('Ctrl Pts',(-17.7428202965123,-12.8663406478716,
115.126765955283)) ;
#183882 = CARTESIAN_POINT('Ctrl Pts',(-17.7230500421668,-12.8245820586196,
115.066548951326)) ;
#183883 = CARTESIAN_POINT('Ctrl Pts',(-17.7032797878212,-12.7828234693676,
115.00633194737)) ;
#183884 = CARTESIAN_POINT('Ctrl Pts',(-17.7770836386329,-12.7828234316733,
114.982100928198)) ;
#183885 = CARTESIAN_POINT('Ctrl Pts',(-17.8508874894446,-12.782823393979,
114.957869909026)) ;
#183886 = CARTESIAN_POINT('Ctrl Pts',(-17.8706577437902,-12.824581983231,
115.018086912983)) ;
#183887 = CARTESIAN_POINT('Ctrl Pts',(-17.8211647568461,-13.0878606072953,
114.902837359147)) ;
#183888 = CARTESIAN_POINT('Ctrl Pts',(-17.843686172388,-13.1112998695193,
114.971433956383)) ;
#183889 = CARTESIAN_POINT('Ctrl Pts',(-17.7698823258549,-13.1112999036755,
114.995664988587)) ;
#183890 = CARTESIAN_POINT('Ctrl Pts',(-17.6960784793217,-13.1112999378317,
115.019896020791)) ;
#183891 = CARTESIAN_POINT('Ctrl Pts',(-17.6735570637799,-13.0878606756077,
114.951299423555)) ;
#183892 = CARTESIAN_POINT('Ctrl Pts',(-17.651035648238,-13.0644214133836,
114.882702826318)) ;
#183893 = CARTESIAN_POINT('Ctrl Pts',(-17.7248394947711,-13.0644213792274,
114.858471794115)) ;
#183894 = CARTESIAN_POINT('Ctrl Pts',(-17.7986433413042,-13.0644213450712,
114.834240761911)) ;
#183895 = CARTESIAN_POINT('Ctrl Pts',(-17.8211647568461,-13.0878606072953,
114.902837359147)) ;
#183896 = CARTESIAN_POINT('Ctrl Pts',(-17.7949112979524,-13.3747557627756,
114.858346400162)) ;
#183897 = CARTESIAN_POINT('Ctrl Pts',(-17.818565917269,-13.378198596209,114.930394553419)) ;
#183898 = CARTESIAN_POINT('Ctrl Pts',(-17.7447620737718,-13.3781986232595,
114.954625594869)) ;
#183899 = CARTESIAN_POINT('Ctrl Pts',(-17.6709582302744,-13.37819865031,114.97885663632)) ;
#183900 = CARTESIAN_POINT('Ctrl Pts',(-17.6473036109578,-13.3747558168767,
114.906808483063)) ;
#183901 = CARTESIAN_POINT('Ctrl Pts',(-17.6236489916412,-13.3713129834433,
114.834760329806)) ;
#183902 = CARTESIAN_POINT('Ctrl Pts',(-17.6974528351385,-13.3713129563928,
114.810529288356)) ;
#183903 = CARTESIAN_POINT('Ctrl Pts',(-17.7712566786358,-13.3713129293423,
114.786298246905)) ;
#183904 = CARTESIAN_POINT('Ctrl Pts',(-17.7949112979524,-13.3747557627756,
114.858346400162)) ;
#183905 = CARTESIAN_POINT('Ctrl Pts',(-17.7930142307547,-13.6654070056361,
114.888132109586)) ;
#183906 = CARTESIAN_POINT('Ctrl Pts',(-17.8161012539618,-13.648560400251,
114.958451456842)) ;
#183907 = CARTESIAN_POINT('Ctrl Pts',(-17.7422974120605,-13.6485604179734,
114.982682503154)) ;
#183908 = CARTESIAN_POINT('Ctrl Pts',(-17.6684935701592,-13.6485604356957,
115.006913549465)) ;
#183909 = CARTESIAN_POINT('Ctrl Pts',(-17.6454065469521,-13.6654070410809,
114.936594202209)) ;
#183910 = CARTESIAN_POINT('Ctrl Pts',(-17.6223195237451,-13.682253646466,
114.866274854952)) ;
#183911 = CARTESIAN_POINT('Ctrl Pts',(-17.6961233656464,-13.6822536287436,
114.84204380864)) ;
#183912 = CARTESIAN_POINT('Ctrl Pts',(-17.7699272075477,-13.6822536110213,
114.817812762329)) ;
#183913 = CARTESIAN_POINT('Ctrl Pts',(-17.7930142307547,-13.6654070056361,
114.888132109586)) ;
#183914 = CARTESIAN_POINT('Ctrl Pts',(-17.8147252087611,-13.9370542943595,
114.989647338605)) ;
#183915 = CARTESIAN_POINT('Ctrl Pts',(-17.835598783078,-13.901214603103,115.053224877806)) ;
#183916 = CARTESIAN_POINT('Ctrl Pts',(-17.7617949415956,-13.9012146131836,
115.077455925394)) ;
#183917 = CARTESIAN_POINT('Ctrl Pts',(-17.6879911001133,-13.9012146232642,
115.101686972982)) ;
#183918 = CARTESIAN_POINT('Ctrl Pts',(-17.6671175257964,-13.9370543145207,
115.03810943378)) ;
#183919 = CARTESIAN_POINT('Ctrl Pts',(-17.6462439514795,-13.9728940057772,
114.974531894578)) ;
#183920 = CARTESIAN_POINT('Ctrl Pts',(-17.7200477929618,-13.9728939956966,
114.95030084699)) ;
#183921 = CARTESIAN_POINT('Ctrl Pts',(-17.7938516344442,-13.972893985616,
114.926069799403)) ;
#183922 = CARTESIAN_POINT('Ctrl Pts',(-17.8147252087611,-13.9370542943595,
114.989647338605)) ;
#183923 = CARTESIAN_POINT('Ctrl Pts',(-17.8580728556449,-14.1729033532404,
115.157292589129)) ;
#183924 = CARTESIAN_POINT('Ctrl Pts',(-17.8752140934939,-14.1205407691761,
115.209502033795)) ;
#183925 = CARTESIAN_POINT('Ctrl Pts',(-17.8014102512489,-14.1205407723559,
115.233733079059)) ;
#183926 = CARTESIAN_POINT('Ctrl Pts',(-17.7276064090039,-14.1205407755357,
115.257964124324)) ;
#183927 = CARTESIAN_POINT('Ctrl Pts',(-17.7104651711549,-14.1729033596,115.205754679658)) ;
#183928 = CARTESIAN_POINT('Ctrl Pts',(-17.6933239333059,-14.2252659436643,
115.153545234993)) ;
#183929 = CARTESIAN_POINT('Ctrl Pts',(-17.7671277755509,-14.2252659404845,
115.129314189728)) ;
#183930 = CARTESIAN_POINT('Ctrl Pts',(-17.8409316177959,-14.2252659373047,
115.105083144464)) ;
#183931 = CARTESIAN_POINT('Ctrl Pts',(-17.8580728556449,-14.1729033532404,
115.157292589129)) ;
#183932 = CARTESIAN_POINT('Ctrl Pts',(-17.9184133421674,-14.3528610645483,
115.376351104933)) ;
#183933 = CARTESIAN_POINT('Ctrl Pts',(-17.9306369507618,-14.2878546501218,
115.413582244416)) ;
#183934 = CARTESIAN_POINT('Ctrl Pts',(-17.8568331077171,-14.2878546504462,
115.437813287245)) ;
#183935 = CARTESIAN_POINT('Ctrl Pts',(-17.7830292646724,-14.2878546507707,
115.462044330074)) ;
#183936 = CARTESIAN_POINT('Ctrl Pts',(-17.7708056560779,-14.3528610651972,
115.42481319059)) ;
#183937 = CARTESIAN_POINT('Ctrl Pts',(-17.7585820474835,-14.4178674796237,
115.387582051107)) ;
#183938 = CARTESIAN_POINT('Ctrl Pts',(-17.8323858905282,-14.4178674792993,
115.363351008278)) ;
#183939 = CARTESIAN_POINT('Ctrl Pts',(-17.906189733573,-14.4178674789748,
115.339119965449)) ;
#183940 = CARTESIAN_POINT('Ctrl Pts',(-17.9184133421674,-14.3528610645483,
115.376351104933)) ;
#183941 = CARTESIAN_POINT('Ctrl Pts',(-17.991766676009,-14.4673900074207,
115.635384696762)) ;
#183942 = CARTESIAN_POINT('Ctrl Pts',(-17.9981494388776,-14.3942885636895,
115.654825562653)) ;
#183943 = CARTESIAN_POINT('Ctrl Pts',(-17.9243455947338,-14.39428856281,115.679056602134)) ;
#183944 = CARTESIAN_POINT('Ctrl Pts',(-17.8505417505901,-14.3942885619306,
115.703287641616)) ;
#183945 = CARTESIAN_POINT('Ctrl Pts',(-17.8441589877216,-14.4673900056618,
115.683846775725)) ;
#183946 = CARTESIAN_POINT('Ctrl Pts',(-17.837776224853,-14.5404914493931,
115.664405909834)) ;
#183947 = CARTESIAN_POINT('Ctrl Pts',(-17.9115800689967,-14.5404914502725,
115.640174870352)) ;
#183948 = CARTESIAN_POINT('Ctrl Pts',(-17.9853839131405,-14.540491451152,
115.615943830871)) ;
#183949 = CARTESIAN_POINT('Ctrl Pts',(-17.991766676009,-14.4673900074207,
115.635384696762)) ;
#183950 = CARTESIAN_POINT('Ctrl Pts',(-18.0711284340199,-14.5059091307987,
115.912498667304)) ;
#183951 = CARTESIAN_POINT('Ctrl Pts',(-18.0712464888033,-14.4300095722764,
115.91285824319)) ;
#183952 = CARTESIAN_POINT('Ctrl Pts',(-17.9974426443487,-14.4300095722936,
115.937089281725)) ;
#183953 = CARTESIAN_POINT('Ctrl Pts',(-17.9236387998941,-14.4300095723109,
115.96132032026)) ;
#183954 = CARTESIAN_POINT('Ctrl Pts',(-17.9235207451107,-14.5059091308332,
115.960960744373)) ;
#183955 = CARTESIAN_POINT('Ctrl Pts',(-17.9234026903274,-14.5818086893555,
115.960601168487)) ;
#183956 = CARTESIAN_POINT('Ctrl Pts',(-17.997206534782,-14.5818086893382,
115.936370129952)) ;
#183957 = CARTESIAN_POINT('Ctrl Pts',(-18.0710103792366,-14.581808689321,
115.912139091418)) ;
#183958 = CARTESIAN_POINT('Ctrl Pts',(-18.0711284340199,-14.5059091307987,
115.912498667304)) ;
#183959 = CARTESIAN_POINT('Ctrl Pts',(-18.1505342643703,-14.467003448986,
116.1897784186)) ;
#183960 = CARTESIAN_POINT('Ctrl Pts',(-18.1443746311779,-14.3937086480908,
116.171017169796)) ;
#183961 = CARTESIAN_POINT('Ctrl Pts',(-18.0705707870571,-14.3937086489183,
116.195248209347)) ;
#183962 = CARTESIAN_POINT('Ctrl Pts',(-17.9967669429363,-14.3937086497458,
116.219479248898)) ;
#183963 = CARTESIAN_POINT('Ctrl Pts',(-18.0029265761288,-14.4670034506409,
116.238240497703)) ;
#183964 = CARTESIAN_POINT('Ctrl Pts',(-18.0090862093212,-14.5402982515361,
116.257001746507)) ;
#183965 = CARTESIAN_POINT('Ctrl Pts',(-18.082890053442,-14.5402982507086,
116.232770706956)) ;
#183966 = CARTESIAN_POINT('Ctrl Pts',(-18.1566938975628,-14.5402982498811,
116.208539667404)) ;
#183967 = CARTESIAN_POINT('Ctrl Pts',(-18.1505342643703,-14.467003448986,
116.1897784186)) ;
#183968 = CARTESIAN_POINT('Ctrl Pts',(-18.2236575677772,-14.3526296857438,
116.448006484568)) ;
#183969 = CARTESIAN_POINT('Ctrl Pts',(-18.2116480597675,-14.2872135873285,
116.411427460882)) ;
#183970 = CARTESIAN_POINT('Ctrl Pts',(-18.1378442166257,-14.2872135872054,
116.435658503415)) ;
#183971 = CARTESIAN_POINT('Ctrl Pts',(-18.0640403734839,-14.2872135870823,
116.459889545948)) ;
#183972 = CARTESIAN_POINT('Ctrl Pts',(-18.0760498814937,-14.3526296854977,
116.496468569635)) ;
#183973 = CARTESIAN_POINT('Ctrl Pts',(-18.0880593895034,-14.418045783913,
116.533047593321)) ;
#183974 = CARTESIAN_POINT('Ctrl Pts',(-18.1618632326452,-14.4180457840361,
116.508816550788)) ;
#183975 = CARTESIAN_POINT('Ctrl Pts',(-18.2356670757869,-14.4180457841592,
116.484585508255)) ;
#183976 = CARTESIAN_POINT('Ctrl Pts',(-18.2236575677772,-14.3526296857438,
116.448006484568)) ;
#183977 = CARTESIAN_POINT('Ctrl Pts',(-18.2841253649015,-14.1719531187117,
116.667560097024)) ;
#183978 = CARTESIAN_POINT('Ctrl Pts',(-18.2671440519089,-14.1190573784708,
116.615837757477)) ;
#183979 = CARTESIAN_POINT('Ctrl Pts',(-18.1933402096846,-14.1190573751839,
116.640068802804)) ;
#183980 = CARTESIAN_POINT('Ctrl Pts',(-18.1195363674603,-14.119057371897,
116.664299848132)) ;
#183981 = CARTESIAN_POINT('Ctrl Pts',(-18.1365176804528,-14.1719531121379,
116.716022187679)) ;
#183982 = CARTESIAN_POINT('Ctrl Pts',(-18.1534989934453,-14.2248488523788,
116.767744527226)) ;
#183983 = CARTESIAN_POINT('Ctrl Pts',(-18.2273028356696,-14.2248488556657,
116.743513481899)) ;
#183984 = CARTESIAN_POINT('Ctrl Pts',(-18.301106677894,-14.2248488589527,
116.719282436571)) ;
#183985 = CARTESIAN_POINT('Ctrl Pts',(-18.2841253649015,-14.1719531187117,
116.667560097024)) ;
#183986 = CARTESIAN_POINT('Ctrl Pts',(-18.3272925522858,-13.936583984801,
116.834555335885)) ;
#183987 = CARTESIAN_POINT('Ctrl Pts',(-18.3065373884678,-13.9000456634002,
116.771338455511)) ;
#183988 = CARTESIAN_POINT('Ctrl Pts',(-18.2327335469008,-13.9000456537943,
116.79556950284)) ;
#183989 = CARTESIAN_POINT('Ctrl Pts',(-18.1589297053339,-13.9000456441885,
116.81980055017)) ;
#183990 = CARTESIAN_POINT('Ctrl Pts',(-18.1796848691519,-13.9365839655893,
116.883017430544)) ;
#183991 = CARTESIAN_POINT('Ctrl Pts',(-18.2004400329699,-13.9731222869902,
116.946234310919)) ;
#183992 = CARTESIAN_POINT('Ctrl Pts',(-18.2742438745369,-13.973122296596,
116.922003263589)) ;
#183993 = CARTESIAN_POINT('Ctrl Pts',(-18.3480477161039,-13.9731223062019,
116.897772216259)) ;
#183994 = CARTESIAN_POINT('Ctrl Pts',(-18.3272925522858,-13.936583984801,
116.834555335885)) ;
#183995 = CARTESIAN_POINT('Ctrl Pts',(-18.3489789369998,-13.6642946874373,
116.936073490923)) ;
#183996 = CARTESIAN_POINT('Ctrl Pts',(-18.3259455354646,-13.6467154172206,
116.865917465918)) ;
#183997 = CARTESIAN_POINT('Ctrl Pts',(-18.2521416935426,-13.646715399489,
116.890148512166)) ;
#183998 = CARTESIAN_POINT('Ctrl Pts',(-18.1783378516205,-13.6467153817574,
116.914379558414)) ;
#183999 = CARTESIAN_POINT('Ctrl Pts',(-18.2013712531556,-13.664294651974,
116.984535583419)) ;
#184000 = CARTESIAN_POINT('Ctrl Pts',(-18.2244046546907,-13.6818739221906,
117.054691608424)) ;
#184001 = CARTESIAN_POINT('Ctrl Pts',(-18.2982084966128,-13.6818739399222,
117.030460562176)) ;
#184002 = CARTESIAN_POINT('Ctrl Pts',(-18.3720123385349,-13.6818739576539,
117.006229515928)) ;
#184003 = CARTESIAN_POINT('Ctrl Pts',(-18.3489789369998,-13.6642946874373,
116.936073490923)) ;
#184004 = CARTESIAN_POINT('Ctrl Pts',(-18.3470303613831,-13.3747428455626,
116.965562261399)) ;
#184005 = CARTESIAN_POINT('Ctrl Pts',(-18.3233666532677,-13.377355159395,
116.893486424106)) ;
#184006 = CARTESIAN_POINT('Ctrl Pts',(-18.2495628097586,-13.3773551335995,
116.91771746552)) ;
#184007 = CARTESIAN_POINT('Ctrl Pts',(-18.1757589662495,-13.3773551078041,
116.941948506935)) ;
#184008 = CARTESIAN_POINT('Ctrl Pts',(-18.199422674365,-13.3747427939718,
117.014024344228)) ;
#184009 = CARTESIAN_POINT('Ctrl Pts',(-18.2230863824804,-13.3721304801394,
117.086100181521)) ;
#184010 = CARTESIAN_POINT('Ctrl Pts',(-18.2968902259895,-13.3721305059348,
117.061869140106)) ;
#184011 = CARTESIAN_POINT('Ctrl Pts',(-18.3706940694986,-13.3721305317302,
117.037638098692)) ;
#184012 = CARTESIAN_POINT('Ctrl Pts',(-18.3470303613831,-13.3747428455626,
116.965562261399)) ;
#184013 = CARTESIAN_POINT('Ctrl Pts',(-18.3207665837922,-13.0876482903165,
116.921069134503)) ;
#184014 = CARTESIAN_POINT('Ctrl Pts',(-18.2981677310769,-13.1103096275797,
116.852236674777)) ;
#184015 = CARTESIAN_POINT('Ctrl Pts',(-18.2243638846365,-13.1103095944857,
116.876467707263)) ;
#184016 = CARTESIAN_POINT('Ctrl Pts',(-18.1505600381961,-13.1103095613917,
116.900698739749)) ;
#184017 = CARTESIAN_POINT('Ctrl Pts',(-18.1731588909114,-13.0876482241285,
116.969531199475)) ;
#184018 = CARTESIAN_POINT('Ctrl Pts',(-18.1957577436267,-13.0649868868653,
117.038363659201)) ;
#184019 = CARTESIAN_POINT('Ctrl Pts',(-18.2695615900671,-13.0649869199593,
117.014132626715)) ;
#184020 = CARTESIAN_POINT('Ctrl Pts',(-18.3433654365075,-13.0649869530533,
116.989901594229)) ;
#184021 = CARTESIAN_POINT('Ctrl Pts',(-18.3207665837922,-13.0876482903165,
116.921069134503)) ;
#184022 = CARTESIAN_POINT('Ctrl Pts',(-18.2712815660308,-12.8243385253649,
116.805840132971)) ;
#184023 = CARTESIAN_POINT('Ctrl Pts',(-18.2513706019285,-12.8654169528501,
116.745194548098)) ;
#184024 = CARTESIAN_POINT('Ctrl Pts',(-18.1775667513243,-12.8654169160371,
116.769425567902)) ;
#184025 = CARTESIAN_POINT('Ctrl Pts',(-18.1037629007201,-12.8654168792241,
116.793656587706)) ;
#184026 = CARTESIAN_POINT('Ctrl Pts',(-18.1236738648224,-12.824338451739,
116.854302172579)) ;
#184027 = CARTESIAN_POINT('Ctrl Pts',(-18.1435848289247,-12.7832600242539,
116.914947757451)) ;
#184028 = CARTESIAN_POINT('Ctrl Pts',(-18.2173886795289,-12.7832600610668,
116.890716737647)) ;
#184029 = CARTESIAN_POINT('Ctrl Pts',(-18.2911925301331,-12.7832600978798,
116.866485717843)) ;
#184030 = CARTESIAN_POINT('Ctrl Pts',(-18.2712815660308,-12.8243385253649,
116.805840132971)) ;
#184031 = CARTESIAN_POINT('Ctrl Pts',(-18.2015034322164,-12.6038922563675,
116.628754857575)) ;
#184032 = CARTESIAN_POINT('Ctrl Pts',(-18.1857020695232,-12.6604213844926,
116.580626455347)) ;
#184033 = CARTESIAN_POINT('Ctrl Pts',(-18.1118982141328,-12.6604213494665,
116.604857460573)) ;
#184034 = CARTESIAN_POINT('Ctrl Pts',(-18.0380943587424,-12.6604213144404,
116.629088465799)) ;
#184035 = CARTESIAN_POINT('Ctrl Pts',(-18.0538957214356,-12.6038921863153,
116.677216868027)) ;
#184036 = CARTESIAN_POINT('Ctrl Pts',(-18.0696970841289,-12.5473630581902,
116.725345270255)) ;
#184037 = CARTESIAN_POINT('Ctrl Pts',(-18.1435009395192,-12.5473630932163,
116.701114265029)) ;
#184038 = CARTESIAN_POINT('Ctrl Pts',(-18.2173047949096,-12.5473631282424,
116.676883259803)) ;
#184039 = CARTESIAN_POINT('Ctrl Pts',(-18.2015034322164,-12.6038922563675,
116.628754857575)) ;
#184040 = CARTESIAN_POINT('Ctrl Pts',(-18.1155659825145,-12.4415502102937,
116.402472433253)) ;
#184041 = CARTESIAN_POINT('Ctrl Pts',(-18.1050078606537,-12.5094955214015,
116.370314096439)) ;
#184042 = CARTESIAN_POINT('Ctrl Pts',(-18.0312040003716,-12.5094954939584,
116.394545086766)) ;
#184043 = CARTESIAN_POINT('Ctrl Pts',(-17.9574001400895,-12.5094954665153,
116.418776077093)) ;
#184044 = CARTESIAN_POINT('Ctrl Pts',(-17.9679582619504,-12.4415501554076,
116.450934413906)) ;
#184045 = CARTESIAN_POINT('Ctrl Pts',(-17.9785163838113,-12.3736048442999,
116.483092750719)) ;
#184046 = CARTESIAN_POINT('Ctrl Pts',(-18.0523202440933,-12.3736048717429,
116.458861760393)) ;
#184047 = CARTESIAN_POINT('Ctrl Pts',(-18.1261241043754,-12.373604899186,
116.434630770066)) ;
#184048 = CARTESIAN_POINT('Ctrl Pts',(-18.1155659825145,-12.4415502102937,
116.402472433253)) ;
#184049 = CARTESIAN_POINT('Ctrl Pts',(-18.0188186140626,-12.3493107874977,
116.143292052209)) ;
#184050 = CARTESIAN_POINT('Ctrl Pts',(-18.0142654159233,-12.4237944597024,
116.129423743995)) ;
#184051 = CARTESIAN_POINT('Ctrl Pts',(-17.9404615513583,-12.4237944461757,
116.153654721277)) ;
#184052 = CARTESIAN_POINT('Ctrl Pts',(-17.8666576867933,-12.4237944326489,
116.177885698558)) ;
#184053 = CARTESIAN_POINT('Ctrl Pts',(-17.8712108849327,-12.3493107604442,
116.191754006772)) ;
#184054 = CARTESIAN_POINT('Ctrl Pts',(-17.8757640830721,-12.2748270882395,
116.205622314986)) ;
#184055 = CARTESIAN_POINT('Ctrl Pts',(-17.949567947637,-12.2748271017662,
116.181391337704)) ;
#184056 = CARTESIAN_POINT('Ctrl Pts',(-18.023371812202,-12.274827115293,116.157160360422)) ;
#184057 = CARTESIAN_POINT('Ctrl Pts',(-18.0188186140626,-12.3493107874977,
116.143292052209)) ;
#184058 = CARTESIAN_POINT('Ctrl Pts',(-17.917965944462,-12.3333698024851,
115.871447888668)) ;
#184059 = CARTESIAN_POINT('Ctrl Pts',(-17.9197162551571,-12.409073916813,
115.876779051166)) ;
#184060 = CARTESIAN_POINT('Ctrl Pts',(-17.8459123881107,-12.409073922124,
115.901010020889)) ;
#184061 = CARTESIAN_POINT('Ctrl Pts',(-17.7721085210643,-12.4090739274351,
115.925240990613)) ;
#184062 = CARTESIAN_POINT('Ctrl Pts',(-17.7703582103692,-12.3333698131071,
115.919909828115)) ;
#184063 = CARTESIAN_POINT('Ctrl Pts',(-17.7686078996741,-12.2576656987791,
115.914578665616)) ;
#184064 = CARTESIAN_POINT('Ctrl Pts',(-17.8424117667205,-12.2576656934681,
115.890347695893)) ;
#184065 = CARTESIAN_POINT('Ctrl Pts',(-17.9162156337669,-12.2576656881571,
115.86611672617)) ;
#184066 = CARTESIAN_POINT('Ctrl Pts',(-17.917965944462,-12.3333698024851,
115.871447888668)) ;
#184067 = CARTESIAN_POINT('Ctrl Pts',(-17.8179951285442,-12.3958418590805,
115.602676622725)) ;
#184068 = CARTESIAN_POINT('Ctrl Pts',(-17.825988435529,-12.4672950791635,
115.627022944439)) ;
#184069 = CARTESIAN_POINT('Ctrl Pts',(-17.7521845670926,-12.467295107772,
115.651253909928)) ;
#184070 = CARTESIAN_POINT('Ctrl Pts',(-17.6783806986561,-12.4672951363806,
115.675484875418)) ;
#184071 = CARTESIAN_POINT('Ctrl Pts',(-17.6703873916712,-12.3958419162977,
115.651138553704)) ;
#184072 = CARTESIAN_POINT('Ctrl Pts',(-17.6623940846864,-12.3243886962147,
115.62679223199)) ;
#184073 = CARTESIAN_POINT('Ctrl Pts',(-17.7361979531229,-12.3243886676062,
115.6025612665)) ;
#184074 = CARTESIAN_POINT('Ctrl Pts',(-17.8100018215593,-12.3243886389976,
115.578330301011)) ;
#184075 = CARTESIAN_POINT('Ctrl Pts',(-17.8179951285442,-12.3958418590805,
115.602676622725)) ;
#184076 = CARTESIAN_POINT('Ctrl Pts',(-17.7275667072708,-12.5305465195612,
115.362515531508)) ;
#184077 = CARTESIAN_POINT('Ctrl Pts',(-17.7411552505888,-12.5926984144573,
115.40390404021)) ;
#184078 = CARTESIAN_POINT('Ctrl Pts',(-17.6673513841811,-12.592698466259,
115.428135011879)) ;
#184079 = CARTESIAN_POINT('Ctrl Pts',(-17.5935475177734,-12.5926985180608,
115.452365983547)) ;
#184080 = CARTESIAN_POINT('Ctrl Pts',(-17.5799589744555,-12.5305466231647,
115.410977474846)) ;
#184081 = CARTESIAN_POINT('Ctrl Pts',(-17.5663704311375,-12.4683947282686,
115.369588966144)) ;
#184082 = CARTESIAN_POINT('Ctrl Pts',(-17.6401742975452,-12.4683946764668,
115.345357994475)) ;
#184083 = CARTESIAN_POINT('Ctrl Pts',(-17.7139781639529,-12.4683946246651,
115.321127022806)) ;
#184084 = CARTESIAN_POINT('Ctrl Pts',(-17.7275667072708,-12.5305465195612,
115.362515531508)) ;
#184085 = CARTESIAN_POINT('Ctrl Pts',(-17.6506148333136,-12.7291635452138,
115.163608506426)) ;
#184086 = CARTESIAN_POINT('Ctrl Pts',(-17.6688616218621,-12.7775393659294,
115.219185278384)) ;
#184087 = CARTESIAN_POINT('Ctrl Pts',(-17.5950577594212,-12.7775394398199,
115.243416262135)) ;
#184088 = CARTESIAN_POINT('Ctrl Pts',(-17.5212538969802,-12.7775395137104,
115.267647245886)) ;
#184089 = CARTESIAN_POINT('Ctrl Pts',(-17.5030071084317,-12.7291636929948,
115.212070473928)) ;
#184090 = CARTESIAN_POINT('Ctrl Pts',(-17.4847603198832,-12.6807878722793,
115.15649370197)) ;
#184091 = CARTESIAN_POINT('Ctrl Pts',(-17.5585641823242,-12.6807877983888,
115.132262718219)) ;
#184092 = CARTESIAN_POINT('Ctrl Pts',(-17.6323680447651,-12.6807877244983,
115.108031734468)) ;
#184093 = CARTESIAN_POINT('Ctrl Pts',(-17.6506148333136,-12.7291635452138,
115.163608506426)) ;
#184094 = CARTESIAN_POINT('Ctrl Pts',(-17.5925315518145,-12.9771312925897,
115.022149073148)) ;
#184095 = CARTESIAN_POINT('Ctrl Pts',(-17.6141265834111,-13.0082656414961,
115.087924053104)) ;
#184096 = CARTESIAN_POINT('Ctrl Pts',(-17.5403227272072,-13.0082657332076,
115.112155055852)) ;
#184097 = CARTESIAN_POINT('Ctrl Pts',(-17.4665188710033,-13.008265824919,
115.1363860586)) ;
#184098 = CARTESIAN_POINT('Ctrl Pts',(-17.4449238394067,-12.9771314760126,
115.070611078644)) ;
#184099 = CARTESIAN_POINT('Ctrl Pts',(-17.4233288078101,-12.9459971271062,
115.004836098687)) ;
#184100 = CARTESIAN_POINT('Ctrl Pts',(-17.497132664014,-12.9459970353947,
114.980605095939)) ;
#184101 = CARTESIAN_POINT('Ctrl Pts',(-17.5709365202179,-12.9459969436833,
114.956374093191)) ;
#184102 = CARTESIAN_POINT('Ctrl Pts',(-17.5925315518145,-12.9771312925897,
115.022149073148)) ;
#184103 = CARTESIAN_POINT('Ctrl Pts',(-17.5565878319294,-13.2574946761857,
114.948229481288)) ;
#184104 = CARTESIAN_POINT('Ctrl Pts',(-17.5799882779951,-13.269101018714,
115.019503462338)) ;
#184105 = CARTESIAN_POINT('Ctrl Pts',(-17.5061844297033,-13.2691011219862,
115.043734489184)) ;
#184106 = CARTESIAN_POINT('Ctrl Pts',(-17.4323805814114,-13.2691012252584,
115.067965516031)) ;
#184107 = CARTESIAN_POINT('Ctrl Pts',(-17.4089801353457,-13.2574948827302,
114.996691534982)) ;
#184108 = CARTESIAN_POINT('Ctrl Pts',(-17.38557968928,-13.2458885402019,114.925417553932)) ;
#184109 = CARTESIAN_POINT('Ctrl Pts',(-17.4593835375718,-13.2458884369297,
114.901186527085)) ;
#184110 = CARTESIAN_POINT('Ctrl Pts',(-17.5331873858637,-13.2458883336575,
114.876955500239)) ;
#184111 = CARTESIAN_POINT('Ctrl Pts',(-17.5565878319294,-13.2574946761857,
114.948229481288)) ;
#184112 = CARTESIAN_POINT('Ctrl Pts',(-17.5448475110634,-13.5486172877669,
114.947929919244)) ;
#184113 = CARTESIAN_POINT('Ctrl Pts',(-17.5683683296816,-13.5399156323179,
115.01957053562)) ;
#184114 = CARTESIAN_POINT('Ctrl Pts',(-17.4945644902396,-13.5399157383977,
115.043801589422)) ;
#184115 = CARTESIAN_POINT('Ctrl Pts',(-17.4207606507977,-13.5399158444775,
115.068032643224)) ;
#184116 = CARTESIAN_POINT('Ctrl Pts',(-17.3972398321794,-13.5486174999264,
114.996392026848)) ;
#184117 = CARTESIAN_POINT('Ctrl Pts',(-17.3737190135613,-13.5573191553753,
114.924751410472)) ;
#184118 = CARTESIAN_POINT('Ctrl Pts',(-17.4475228530032,-13.5573190492956,
114.90052035667)) ;
#184119 = CARTESIAN_POINT('Ctrl Pts',(-17.5213266924452,-13.5573189432158,
114.876289302868)) ;
#184120 = CARTESIAN_POINT('Ctrl Pts',(-17.5448475110634,-13.5486172877669,
114.947929919244)) ;
#184121 = CARTESIAN_POINT('Ctrl Pts',(-17.5571682124288,-13.8299622964239,
115.020863384168)) ;
#184122 = CARTESIAN_POINT('Ctrl Pts',(-17.5791308719583,-13.8016053515907,
115.087758099343)) ;
#184123 = CARTESIAN_POINT('Ctrl Pts',(-17.5053270413127,-13.8016054516698,
115.111989179937)) ;
#184124 = CARTESIAN_POINT('Ctrl Pts',(-17.4315232106671,-13.8016055517489,
115.136220260531)) ;
#184125 = CARTESIAN_POINT('Ctrl Pts',(-17.4095605511376,-13.8299624965821,
115.069325545356)) ;
#184126 = CARTESIAN_POINT('Ctrl Pts',(-17.3875978916081,-13.8583194414153,
115.002430830181)) ;
#184127 = CARTESIAN_POINT('Ctrl Pts',(-17.4614017222537,-13.8583193413362,
114.978199749587)) ;
#184128 = CARTESIAN_POINT('Ctrl Pts',(-17.5352055528993,-13.8583192412571,
114.953968668993)) ;
#184129 = CARTESIAN_POINT('Ctrl Pts',(-17.5571682124288,-13.8299622964239,
115.020863384168)) ;
#184130 = CARTESIAN_POINT('Ctrl Pts',(-17.5919536420937,-14.082140489746,
115.162256577588)) ;
#184131 = CARTESIAN_POINT('Ctrl Pts',(-17.6107868349062,-14.0361354675862,
115.219619442075)) ;
#184132 = CARTESIAN_POINT('Ctrl Pts',(-17.5369830121559,-14.0361355534221,
115.243850546717)) ;
#184133 = CARTESIAN_POINT('Ctrl Pts',(-17.4631791894057,-14.0361356392581,
115.268081651359)) ;
#184134 = CARTESIAN_POINT('Ctrl Pts',(-17.4443459965932,-14.0821406614179,
115.210718786872)) ;
#184135 = CARTESIAN_POINT('Ctrl Pts',(-17.4255128037808,-14.1281456835778,
115.153355922385)) ;
#184136 = CARTESIAN_POINT('Ctrl Pts',(-17.499316626531,-14.1281455977418,
115.129124817743)) ;
#184137 = CARTESIAN_POINT('Ctrl Pts',(-17.5731204492813,-14.1281455119059,
115.104893713101)) ;
#184138 = CARTESIAN_POINT('Ctrl Pts',(-17.5919536420937,-14.082140489746,
115.162256577588)) ;
#184139 = CARTESIAN_POINT('Ctrl Pts',(-17.6460547424978,-14.2871395255682,
115.362533542529)) ;
#184140 = CARTESIAN_POINT('Ctrl Pts',(-17.6604043679569,-14.2267539066878,
115.406240184295)) ;
#184141 = CARTESIAN_POINT('Ctrl Pts',(-17.5866005513895,-14.2267539712464,
115.430471307769)) ;
#184142 = CARTESIAN_POINT('Ctrl Pts',(-17.5127967348221,-14.2267540358049,
115.454702431244)) ;
#184143 = CARTESIAN_POINT('Ctrl Pts',(-17.498447109363,-14.2871396546853,
115.410995789478)) ;
#184144 = CARTESIAN_POINT('Ctrl Pts',(-17.4840974839038,-14.3475252735657,
115.367289147712)) ;
#184145 = CARTESIAN_POINT('Ctrl Pts',(-17.5579013004713,-14.3475252090071,
115.343058024237)) ;
#184146 = CARTESIAN_POINT('Ctrl Pts',(-17.6317051170386,-14.3475251444486,
115.318826900763)) ;
#184147 = CARTESIAN_POINT('Ctrl Pts',(-17.6460547424978,-14.2871395255682,
115.362533542529)) ;
#184148 = CARTESIAN_POINT('Ctrl Pts',(-17.7149985645736,-14.4298488440199,
115.608097682744)) ;
#184149 = CARTESIAN_POINT('Ctrl Pts',(-17.7238201732498,-14.3594095209829,
115.634966877378)) ;
#184150 = CARTESIAN_POINT('Ctrl Pts',(-17.6500163603788,-14.3594095593736,
115.659198012111)) ;
#184151 = CARTESIAN_POINT('Ctrl Pts',(-17.5762125475078,-14.3594095977643,
115.683429146844)) ;
#184152 = CARTESIAN_POINT('Ctrl Pts',(-17.5673909388317,-14.4298489208013,
115.65655995221)) ;
#184153 = CARTESIAN_POINT('Ctrl Pts',(-17.5585693301555,-14.5002882438384,
115.629690757576)) ;
#184154 = CARTESIAN_POINT('Ctrl Pts',(-17.6323731430264,-14.5002882054477,
115.605459622843)) ;
#184155 = CARTESIAN_POINT('Ctrl Pts',(-17.7061769558974,-14.500288167057,
115.58122848811)) ;
#184156 = CARTESIAN_POINT('Ctrl Pts',(-17.7149985645736,-14.4298488440199,
115.608097682744)) ;
#184157 = CARTESIAN_POINT('Ctrl Pts',(-17.7923224785126,-14.4994383097765,
115.878923588417)) ;
#184158 = CARTESIAN_POINT('Ctrl Pts',(-17.7950280138778,-14.4240356160354,
115.887164210622)) ;
#184159 = CARTESIAN_POINT('Ctrl Pts',(-17.7212242022659,-14.4240356268717,
115.91139534919)) ;
#184160 = CARTESIAN_POINT('Ctrl Pts',(-17.6474203906539,-14.424035637708,
115.935626487757)) ;
#184161 = CARTESIAN_POINT('Ctrl Pts',(-17.6447148552887,-14.4994383314491,
115.927385865553)) ;
#184162 = CARTESIAN_POINT('Ctrl Pts',(-17.6420093199235,-14.5748410251902,
115.919145243348)) ;
#184163 = CARTESIAN_POINT('Ctrl Pts',(-17.7158131315355,-14.5748410143539,
115.89491410478)) ;
#184164 = CARTESIAN_POINT('Ctrl Pts',(-17.7896169431474,-14.5748410035177,
115.870682966212)) ;
#184165 = CARTESIAN_POINT('Ctrl Pts',(-17.7923224785126,-14.4994383097765,
115.878923588417)) ;
#184166 = CARTESIAN_POINT('Ctrl Pts',(-17.8726588843966,-14.4922423916848,
116.159099968041)) ;
#184167 = CARTESIAN_POINT('Ctrl Pts',(-17.8690253884429,-14.4172290917828,
116.148032923727)) ;
#184168 = CARTESIAN_POINT('Ctrl Pts',(-17.7952215753068,-14.4172290756449,
116.172264057653)) ;
#184169 = CARTESIAN_POINT('Ctrl Pts',(-17.7214177621707,-14.417229059507,
116.196495191578)) ;
#184170 = CARTESIAN_POINT('Ctrl Pts',(-17.7250512581244,-14.492242359409,
116.207562235892)) ;
#184171 = CARTESIAN_POINT('Ctrl Pts',(-17.7286847540781,-14.567255659311,
116.218629280206)) ;
#184172 = CARTESIAN_POINT('Ctrl Pts',(-17.8024885672142,-14.5672556754489,
116.194398146281)) ;
#184173 = CARTESIAN_POINT('Ctrl Pts',(-17.8762923803503,-14.5672556915868,
116.170167012355)) ;
#184174 = CARTESIAN_POINT('Ctrl Pts',(-17.8726588843966,-14.4922423916848,
116.159099968041)) ;
#184175 = CARTESIAN_POINT('Ctrl Pts',(-17.9492605892441,-14.4074859363464,
116.427972082509)) ;
#184176 = CARTESIAN_POINT('Ctrl Pts',(-17.9395377455059,-14.3382771247353,
116.398357867468)) ;
#184177 = CARTESIAN_POINT('Ctrl Pts',(-17.8657339283016,-14.3382770857767,
116.422588989002)) ;
#184178 = CARTESIAN_POINT('Ctrl Pts',(-17.7919301110973,-14.3382770468181,
116.446820110537)) ;
#184179 = CARTESIAN_POINT('Ctrl Pts',(-17.8016529548354,-14.4074858584293,
116.476434325578)) ;
#184180 = CARTESIAN_POINT('Ctrl Pts',(-17.8113757985735,-14.4766946700404,
116.506048540618)) ;
#184181 = CARTESIAN_POINT('Ctrl Pts',(-17.8851796157779,-14.476694708999,
116.481817419084)) ;
#184182 = CARTESIAN_POINT('Ctrl Pts',(-17.9589834329822,-14.4766947479576,
116.45758629755)) ;
#184183 = CARTESIAN_POINT('Ctrl Pts',(-17.9492605892441,-14.4074859363464,
116.427972082509)) ;
#184184 = CARTESIAN_POINT('Ctrl Pts',(-18.0153695983152,-14.2527213410347,
116.664674816876)) ;
#184185 = CARTESIAN_POINT('Ctrl Pts',(-18.00028515088,-14.1942140636659,116.618730022167)) ;
#184186 = CARTESIAN_POINT('Ctrl Pts',(-17.9264813282525,-14.1942140071928,
116.642961127183)) ;
#184187 = CARTESIAN_POINT('Ctrl Pts',(-17.8526775056251,-14.1942139507198,
116.6671922322)) ;
#184188 = CARTESIAN_POINT('Ctrl Pts',(-17.8677619530604,-14.2527212280886,
116.713137026909)) ;
#184189 = CARTESIAN_POINT('Ctrl Pts',(-17.8828464004957,-14.3112285054574,
116.759081821618)) ;
#184190 = CARTESIAN_POINT('Ctrl Pts',(-17.9566502231231,-14.3112285619304,
116.734850716602)) ;
#184191 = CARTESIAN_POINT('Ctrl Pts',(-18.0304540457505,-14.3112286184035,
116.710619611585)) ;
#184192 = CARTESIAN_POINT('Ctrl Pts',(-18.0153695983152,-14.2527213410347,
116.664674816876)) ;
#184193 = CARTESIAN_POINT('Ctrl Pts',(-18.0662184898938,-14.0372448891262,
116.855097648155)) ;
#184194 = CARTESIAN_POINT('Ctrl Pts',(-18.0468255144096,-13.9936933807782,
116.796029772331)) ;
#184195 = CARTESIAN_POINT('Ctrl Pts',(-17.9730216850138,-13.993693314701,
116.820260856732)) ;
#184196 = CARTESIAN_POINT('Ctrl Pts',(-17.8992178556179,-13.9936932486239,
116.844491941133)) ;
#184197 = CARTESIAN_POINT('Ctrl Pts',(-17.9186108311021,-14.0372447569719,
116.903559816957)) ;
#184198 = CARTESIAN_POINT('Ctrl Pts',(-17.9380038065863,-14.08079626532,116.96262769278)) ;
#184199 = CARTESIAN_POINT('Ctrl Pts',(-18.0118076359821,-14.0807963313971,
116.938396608379)) ;
#184200 = CARTESIAN_POINT('Ctrl Pts',(-18.085611465378,-14.0807963974743,
116.914165523978)) ;
#184201 = CARTESIAN_POINT('Ctrl Pts',(-18.0662184898938,-14.0372448891262,
116.855097648155)) ;
#184202 = CARTESIAN_POINT('Ctrl Pts',(-18.0969238178348,-13.7782273369584,
116.984027397216)) ;
#184203 = CARTESIAN_POINT('Ctrl Pts',(-18.0746250853086,-13.7526945200312,
116.91610905442)) ;
#184204 = CARTESIAN_POINT('Ctrl Pts',(-18.0008212491944,-13.75269445107,116.940340118358)) ;
#184205 = CARTESIAN_POINT('Ctrl Pts',(-17.9270174130802,-13.7526943821088,
116.964571182296)) ;
#184206 = CARTESIAN_POINT('Ctrl Pts',(-17.9493161456064,-13.778227199036,
117.032489525092)) ;
#184207 = CARTESIAN_POINT('Ctrl Pts',(-17.9716148781326,-13.8037600159632,
117.100407867887)) ;
#184208 = CARTESIAN_POINT('Ctrl Pts',(-18.0454187142468,-13.8037600849244,
117.076176803949)) ;
#184209 = CARTESIAN_POINT('Ctrl Pts',(-18.119222550361,-13.8037601538856,
117.051945740011)) ;
#184210 = CARTESIAN_POINT('Ctrl Pts',(-18.0969238178348,-13.7782273369584,
116.984027397216)) ;
#184211 = CARTESIAN_POINT('Ctrl Pts',(-18.1047200617367,-13.4921296981973,
117.043351119596)) ;
#184212 = CARTESIAN_POINT('Ctrl Pts',(-18.0811069226382,-13.4865334475081,
116.971429306637)) ;
#184213 = CARTESIAN_POINT('Ctrl Pts',(-18.0073030803503,-13.4865333838988,
116.995660351771)) ;
#184214 = CARTESIAN_POINT('Ctrl Pts',(-17.9334992380623,-13.4865333202894,
117.019891396905)) ;
#184215 = CARTESIAN_POINT('Ctrl Pts',(-17.9571123771608,-13.4921295709785,
117.091813209864)) ;
#184216 = CARTESIAN_POINT('Ctrl Pts',(-17.9807255162593,-13.4977258216677,
117.163735022823)) ;
#184217 = CARTESIAN_POINT('Ctrl Pts',(-18.0545293585472,-13.497725885277,
117.139503977689)) ;
#184218 = CARTESIAN_POINT('Ctrl Pts',(-18.1283332008352,-13.4977259488864,
117.115272932555)) ;
#184219 = CARTESIAN_POINT('Ctrl Pts',(-18.1047200617367,-13.4921296981973,
117.043351119596)) ;
#184220 = CARTESIAN_POINT('Ctrl Pts',(-18.0883120122329,-13.2025980491625,
117.028710821866)) ;
#184221 = CARTESIAN_POINT('Ctrl Pts',(-18.0650776141143,-13.2172086619386,
116.957942592962)) ;
#184222 = CARTESIAN_POINT('Ctrl Pts',(-17.9912737669891,-13.2172086067816,
116.982173623362)) ;
#184223 = CARTESIAN_POINT('Ctrl Pts',(-17.9174699198639,-13.2172085516246,
117.006404653763)) ;
#184224 = CARTESIAN_POINT('Ctrl Pts',(-17.9407043179825,-13.2025979388484,
117.077172882667)) ;
#184225 = CARTESIAN_POINT('Ctrl Pts',(-17.9639387161011,-13.1879873260723,
117.14794111157)) ;
#184226 = CARTESIAN_POINT('Ctrl Pts',(-18.0377425632263,-13.1879873812294,
117.12371008117)) ;
#184227 = CARTESIAN_POINT('Ctrl Pts',(-18.1115464103515,-13.1879874363864,
117.09947905077)) ;
#184228 = CARTESIAN_POINT('Ctrl Pts',(-18.0883120122329,-13.2025980491625,
117.028710821866)) ;
#184229 = CARTESIAN_POINT('Ctrl Pts',(-18.0479516493469,-12.9267373644591,
116.941340583606)) ;
#184230 = CARTESIAN_POINT('Ctrl Pts',(-18.0267640646557,-12.960631185249,
116.876806618336)) ;
#184231 = CARTESIAN_POINT('Ctrl Pts',(-17.9529602144129,-12.9606311438607,
116.901037639241)) ;
#184232 = CARTESIAN_POINT('Ctrl Pts',(-17.8791563641702,-12.9606311024724,
116.925268660146)) ;
#184233 = CARTESIAN_POINT('Ctrl Pts',(-17.9003439488613,-12.9267372816824,
116.989802625416)) ;
#184234 = CARTESIAN_POINT('Ctrl Pts',(-17.9215315335525,-12.8928434608925,
117.054336590686)) ;
#184235 = CARTESIAN_POINT('Ctrl Pts',(-17.9953353837953,-12.8928435022808,
117.030105569781)) ;
#184236 = CARTESIAN_POINT('Ctrl Pts',(-18.0691392340381,-12.8928435436691,
117.005874548876)) ;
#184237 = CARTESIAN_POINT('Ctrl Pts',(-18.0479516493469,-12.9267373644591,
116.941340583606)) ;
#184238 = CARTESIAN_POINT('Ctrl Pts',(-17.9859929653459,-12.6871394629104,
116.788053385825)) ;
#184239 = CARTESIAN_POINT('Ctrl Pts',(-17.9683662277458,-12.7378139602179,
116.734365186415)) ;
#184240 = CARTESIAN_POINT('Ctrl Pts',(-17.894562376113,-12.7378139322017,
116.758596203086)) ;
#184241 = CARTESIAN_POINT('Ctrl Pts',(-17.8207585244803,-12.7378139041855,
116.782827219757)) ;
#184242 = CARTESIAN_POINT('Ctrl Pts',(-17.8383852620805,-12.687139406878,
116.836515419167)) ;
#184243 = CARTESIAN_POINT('Ctrl Pts',(-17.8560119996807,-12.6364649095704,
116.890203618577)) ;
#184244 = CARTESIAN_POINT('Ctrl Pts',(-17.9298158513134,-12.6364649375867,
116.865972601906)) ;
#184245 = CARTESIAN_POINT('Ctrl Pts',(-18.0036197029461,-12.6364649656029,
116.841741585235)) ;
#184246 = CARTESIAN_POINT('Ctrl Pts',(-17.9859929653459,-12.6871394629104,
116.788053385825)) ;
#184247 = CARTESIAN_POINT('Ctrl Pts',(-17.906099050151,-12.4995507390681,
116.580148460195)) ;
#184248 = CARTESIAN_POINT('Ctrl Pts',(-17.8932906510401,-12.5633999915825,
116.541136142548)) ;
#184249 = CARTESIAN_POINT('Ctrl Pts',(-17.8194867995482,-12.5633999761432,
116.565367159648)) ;
#184250 = CARTESIAN_POINT('Ctrl Pts',(-17.7456829480562,-12.5633999607039,
116.589598176748)) ;
#184251 = CARTESIAN_POINT('Ctrl Pts',(-17.7584913471671,-12.4995507081895,
116.628610494395)) ;
#184252 = CARTESIAN_POINT('Ctrl Pts',(-17.7712997462779,-12.4357014556752,
116.667622812042)) ;
#184253 = CARTESIAN_POINT('Ctrl Pts',(-17.8451035977699,-12.4357014711144,
116.643391794942)) ;
#184254 = CARTESIAN_POINT('Ctrl Pts',(-17.9189074492618,-12.4357014865537,
116.619160777842)) ;
#184255 = CARTESIAN_POINT('Ctrl Pts',(-17.906099050151,-12.4995507390681,
116.580148460195)) ;
#184256 = CARTESIAN_POINT('Ctrl Pts',(-17.8126198276704,-12.3773999719713,
116.331056854077)) ;
#184257 = CARTESIAN_POINT('Ctrl Pts',(-17.8055817580206,-12.4498755259628,
116.309620029115)) ;
#184258 = CARTESIAN_POINT('Ctrl Pts',(-17.7317779084013,-12.4498755206207,
116.333851051918)) ;
#184259 = CARTESIAN_POINT('Ctrl Pts',(-17.657974058782,-12.4498755152786,
116.358082074722)) ;
#184260 = CARTESIAN_POINT('Ctrl Pts',(-17.6650121284318,-12.377399961287,
116.379518899685)) ;
#184261 = CARTESIAN_POINT('Ctrl Pts',(-17.6720501980816,-12.3049244072955,
116.400955724648)) ;
#184262 = CARTESIAN_POINT('Ctrl Pts',(-17.7458540477008,-12.3049244126376,
116.376724701844)) ;
#184263 = CARTESIAN_POINT('Ctrl Pts',(-17.8196578973201,-12.3049244179797,
116.35249367904)) ;
#184264 = CARTESIAN_POINT('Ctrl Pts',(-17.8126198276704,-12.3773999719713,
116.331056854077)) ;
#184265 = CARTESIAN_POINT('Ctrl Pts',(-17.7129634648674,-12.3305982965088,
116.062809081793)) ;
#184266 = CARTESIAN_POINT('Ctrl Pts',(-17.7121429577396,-12.4064507655152,
116.060309949185)) ;
#184267 = CARTESIAN_POINT('Ctrl Pts',(-17.6383391097371,-12.4064507656023,
116.084540976913)) ;
#184268 = CARTESIAN_POINT('Ctrl Pts',(-17.5645352617346,-12.4064507656893,
116.108772004641)) ;
#184269 = CARTESIAN_POINT('Ctrl Pts',(-17.5653557688624,-12.3305982966829,
116.111271137249)) ;
#184270 = CARTESIAN_POINT('Ctrl Pts',(-17.5661762759903,-12.2547458276765,
116.113770269857)) ;
#184271 = CARTESIAN_POINT('Ctrl Pts',(-17.6399801239928,-12.2547458275895,
116.089539242129)) ;
#184272 = CARTESIAN_POINT('Ctrl Pts',(-17.7137839719953,-12.2547458275024,
116.0653082144)) ;
#184273 = CARTESIAN_POINT('Ctrl Pts',(-17.7129634648674,-12.3305982965088,
116.062809081793)) ;
#184274 = CARTESIAN_POINT('Ctrl Pts',(-17.6121496035904,-12.3609522062499,
115.791201386233)) ;
#184275 = CARTESIAN_POINT('Ctrl Pts',(-17.617633502554,-12.4347996190351,
115.807904457495)) ;
#184276 = CARTESIAN_POINT('Ctrl Pts',(-17.5438296567185,-12.4347996215548,
115.832135491824)) ;
#184277 = CARTESIAN_POINT('Ctrl Pts',(-17.4700258108831,-12.4347996240744,
115.856366526153)) ;
#184278 = CARTESIAN_POINT('Ctrl Pts',(-17.4645419119195,-12.3609522112891,
115.839663454891)) ;
#184279 = CARTESIAN_POINT('Ctrl Pts',(-17.4590580129559,-12.2871047985038,
115.822960383629)) ;
#184280 = CARTESIAN_POINT('Ctrl Pts',(-17.5328618587913,-12.2871047959842,
115.7987293493)) ;
#184281 = CARTESIAN_POINT('Ctrl Pts',(-17.6066657046268,-12.2871047934646,
115.774498314971)) ;
#184282 = CARTESIAN_POINT('Ctrl Pts',(-17.6121496035904,-12.3609522062499,
115.791201386233)) ;
#184283 = CARTESIAN_POINT('Ctrl Pts',(-17.5168160586638,-12.4676416333475,
115.536394386331)) ;
#184284 = CARTESIAN_POINT('Ctrl Pts',(-17.5282291491706,-12.5341505224267,
115.571156818475)) ;
#184285 = CARTESIAN_POINT('Ctrl Pts',(-17.4544253052102,-12.5341505238971,
115.595387858515)) ;
#184286 = CARTESIAN_POINT('Ctrl Pts',(-17.3806214612499,-12.5341505253675,
115.619618898555)) ;
#184287 = CARTESIAN_POINT('Ctrl Pts',(-17.3692083707431,-12.4676416362883,
115.584856466411)) ;
#184288 = CARTESIAN_POINT('Ctrl Pts',(-17.3577952802364,-12.4011327472091,
115.550094034267)) ;
#184289 = CARTESIAN_POINT('Ctrl Pts',(-17.4315991241967,-12.4011327457387,
115.525862994227)) ;
#184290 = CARTESIAN_POINT('Ctrl Pts',(-17.5054029681571,-12.4011327442682,
115.501631954187)) ;
#184291 = CARTESIAN_POINT('Ctrl Pts',(-17.5168160586638,-12.4676416333475,
115.536394386331)) ;
#184292 = CARTESIAN_POINT('Ctrl Pts',(-17.4336916866709,-12.6420295507419,
115.31863885574)) ;
#184293 = CARTESIAN_POINT('Ctrl Pts',(-17.450193039918,-12.6964607838734,
115.368899315271)) ;
#184294 = CARTESIAN_POINT('Ctrl Pts',(-17.3763891968336,-12.6964607831673,
115.393130357979)) ;
#184295 = CARTESIAN_POINT('Ctrl Pts',(-17.3025853537493,-12.6964607824612,
115.417361400687)) ;
#184296 = CARTESIAN_POINT('Ctrl Pts',(-17.2860840005021,-12.6420295493297,
115.367100941156)) ;
#184297 = CARTESIAN_POINT('Ctrl Pts',(-17.269582647255,-12.5875983161982,
115.316840481625)) ;
#184298 = CARTESIAN_POINT('Ctrl Pts',(-17.3433864903394,-12.5875983169043,
115.292609438917)) ;
#184299 = CARTESIAN_POINT('Ctrl Pts',(-17.4171903334238,-12.5875983176104,
115.268378396209)) ;
#184300 = CARTESIAN_POINT('Ctrl Pts',(-17.4336916866709,-12.6420295507419,
115.31863885574)) ;
#184301 = CARTESIAN_POINT('Ctrl Pts',(-17.3676172772984,-12.8715204701867,
115.152776949811)) ;
#184302 = CARTESIAN_POINT('Ctrl Pts',(-17.3880246049082,-12.9100077875802,
115.21493437706)) ;
#184303 = CARTESIAN_POINT('Ctrl Pts',(-17.3142207620158,-12.9100077849432,
115.239165420353)) ;
#184304 = CARTESIAN_POINT('Ctrl Pts',(-17.2404169191235,-12.9100077823063,
115.263396463646)) ;
#184305 = CARTESIAN_POINT('Ctrl Pts',(-17.2200095915137,-12.8715204649127,
115.201239036397)) ;
#184306 = CARTESIAN_POINT('Ctrl Pts',(-17.1996022639038,-12.8330331475192,
115.139081609148)) ;
#184307 = CARTESIAN_POINT('Ctrl Pts',(-17.2734061067962,-12.8330331501562,
115.114850565855)) ;
#184308 = CARTESIAN_POINT('Ctrl Pts',(-17.3472099496886,-12.8330331527932,
115.090619522562)) ;
#184309 = CARTESIAN_POINT('Ctrl Pts',(-17.3676172772984,-12.8715204701867,
115.152776949811)) ;
#184310 = CARTESIAN_POINT('Ctrl Pts',(-17.3223473460117,-13.1406452081899,
115.050364660564)) ;
#184311 = CARTESIAN_POINT('Ctrl Pts',(-17.3452119870668,-13.1603966221908,
115.120006668083)) ;
#184312 = CARTESIAN_POINT('Ctrl Pts',(-17.2714081438692,-13.1603966190533,
115.144237710446)) ;
#184313 = CARTESIAN_POINT('Ctrl Pts',(-17.1976043006715,-13.1603966159158,
115.168468752809)) ;
#184314 = CARTESIAN_POINT('Ctrl Pts',(-17.1747396596163,-13.1406452019148,
115.09882674529)) ;
#184315 = CARTESIAN_POINT('Ctrl Pts',(-17.1518750185612,-13.1208937879139,
115.02918473777)) ;
#184316 = CARTESIAN_POINT('Ctrl Pts',(-17.2256788617588,-13.1208937910514,
115.004953695407)) ;
#184317 = CARTESIAN_POINT('Ctrl Pts',(-17.2994827049565,-13.1208937941889,
114.980722653044)) ;
#184318 = CARTESIAN_POINT('Ctrl Pts',(-17.3223473460117,-13.1406452081899,
115.050364660564)) ;
#184319 = CARTESIAN_POINT('Ctrl Pts',(-17.3006206315397,-13.4310927688211,
115.019830516096)) ;
#184320 = CARTESIAN_POINT('Ctrl Pts',(-17.3242986066671,-13.4305915609801,
115.091949807911)) ;
#184321 = CARTESIAN_POINT('Ctrl Pts',(-17.2504947631562,-13.4305915607747,
115.11618084932)) ;
#184322 = CARTESIAN_POINT('Ctrl Pts',(-17.1766909196454,-13.4305915605693,
115.140411890729)) ;
#184323 = CARTESIAN_POINT('Ctrl Pts',(-17.153012944518,-13.4310927684104,
115.068292598915)) ;
#184324 = CARTESIAN_POINT('Ctrl Pts',(-17.1293349693906,-13.4315939762514,
114.9961733071)) ;
#184325 = CARTESIAN_POINT('Ctrl Pts',(-17.2031388129014,-13.4315939764568,
114.971942265691)) ;
#184326 = CARTESIAN_POINT('Ctrl Pts',(-17.2769426564123,-13.4315939766622,
114.947711224282)) ;
#184327 = CARTESIAN_POINT('Ctrl Pts',(-17.3006206315397,-13.4310927688211,
115.019830516096)) ;
#184328 = CARTESIAN_POINT('Ctrl Pts',(-17.3033372707699,-13.7181744540682,
115.063445924555)) ;
#184329 = CARTESIAN_POINT('Ctrl Pts',(-17.3261287288481,-13.6976269857138,
115.132865028405)) ;
#184330 = CARTESIAN_POINT('Ctrl Pts',(-17.2523248856312,-13.6976269892172,
115.157096070709)) ;
#184331 = CARTESIAN_POINT('Ctrl Pts',(-17.1785210424142,-13.6976269927207,
115.181327113013)) ;
#184332 = CARTESIAN_POINT('Ctrl Pts',(-17.155729584336,-13.718174461075,115.111908009164)) ;
#184333 = CARTESIAN_POINT('Ctrl Pts',(-17.1329381262578,-13.7387219294293,
115.042488905314)) ;
#184334 = CARTESIAN_POINT('Ctrl Pts',(-17.2067419694747,-13.7387219259259,
115.01825786301)) ;
#184335 = CARTESIAN_POINT('Ctrl Pts',(-17.2805458126917,-13.7387219224225,
114.994026820705)) ;
#184336 = CARTESIAN_POINT('Ctrl Pts',(-17.3033372707699,-13.7181744540682,
115.063445924555)) ;
#184337 = CARTESIAN_POINT('Ctrl Pts',(-17.3292593238166,-13.9844854804917,
115.177817625919)) ;
#184338 = CARTESIAN_POINT('Ctrl Pts',(-17.349541065467,-13.9453130684822,
115.239592538371)) ;
#184339 = CARTESIAN_POINT('Ctrl Pts',(-17.2757372233181,-13.9453130761656,
115.263823583929)) ;
#184340 = CARTESIAN_POINT('Ctrl Pts',(-17.2019333811692,-13.945313083849,
115.288054629486)) ;
#184341 = CARTESIAN_POINT('Ctrl Pts',(-17.1816516395188,-13.9844854958585,
115.226279717033)) ;
#184342 = CARTESIAN_POINT('Ctrl Pts',(-17.1613698978684,-14.023657907868,
115.164504804581)) ;
#184343 = CARTESIAN_POINT('Ctrl Pts',(-17.2351737400173,-14.0236579001846,
115.140273759023)) ;
#184344 = CARTESIAN_POINT('Ctrl Pts',(-17.3089775821662,-14.0236578925012,
115.116042713466)) ;
#184345 = CARTESIAN_POINT('Ctrl Pts',(-17.3292593238166,-13.9844854804917,
115.177817625919)) ;
#184346 = CARTESIAN_POINT('Ctrl Pts',(-17.3760632823759,-14.2108138750807,
115.35588254334)) ;
#184347 = CARTESIAN_POINT('Ctrl Pts',(-17.3923717224603,-14.1557813405772,
115.405555420177)) ;
#184348 = CARTESIAN_POINT('Ctrl Pts',(-17.3185678824734,-14.1557813517834,
115.42978647232)) ;
#184349 = CARTESIAN_POINT('Ctrl Pts',(-17.2447640424865,-14.1557813629896,
115.454017524462)) ;
#184350 = CARTESIAN_POINT('Ctrl Pts',(-17.2284556024021,-14.2108138974931,
115.404344647625)) ;
#184351 = CARTESIAN_POINT('Ctrl Pts',(-17.2121471623177,-14.2658464319965,
115.354671770788)) ;
#184352 = CARTESIAN_POINT('Ctrl Pts',(-17.2859510023046,-14.2658464207903,
115.330440718646)) ;
#184353 = CARTESIAN_POINT('Ctrl Pts',(-17.3597548422915,-14.2658464095841,
115.306209666503)) ;
#184354 = CARTESIAN_POINT('Ctrl Pts',(-17.3760632823759,-14.2108138750807,
115.35588254334)) ;
#184355 = CARTESIAN_POINT('Ctrl Pts',(-17.4394638024811,-14.3800184665147,
115.584449969473)) ;
#184356 = CARTESIAN_POINT('Ctrl Pts',(-17.4506353318876,-14.313091902712,
115.618476645077)) ;
#184357 = CARTESIAN_POINT('Ctrl Pts',(-17.37683149478,-14.3130919141767,115.64270770599)) ;
#184358 = CARTESIAN_POINT('Ctrl Pts',(-17.3030276576725,-14.3130919256413,
115.666938766902)) ;
#184359 = CARTESIAN_POINT('Ctrl Pts',(-17.291856128266,-14.3800184894439,
115.632912091298)) ;
#184360 = CARTESIAN_POINT('Ctrl Pts',(-17.2806845988595,-14.4469450532465,
115.598885415694)) ;
#184361 = CARTESIAN_POINT('Ctrl Pts',(-17.3544884359671,-14.4469450417819,
115.574654354782)) ;
#184362 = CARTESIAN_POINT('Ctrl Pts',(-17.4282922730746,-14.4469450303173,
115.55042329387)) ;
#184363 = CARTESIAN_POINT('Ctrl Pts',(-17.4394638024811,-14.3800184665147,
115.584449969473)) ;
#184364 = CARTESIAN_POINT('Ctrl Pts',(-17.5142370059596,-14.4803359496639,
115.847668381267)) ;
#184365 = CARTESIAN_POINT('Ctrl Pts',(-17.5194699341939,-14.4063082157353,
115.863607035731)) ;
#184366 = CARTESIAN_POINT('Ctrl Pts',(-17.4456661003206,-14.4063082232175,
115.887838106494)) ;
#184367 = CARTESIAN_POINT('Ctrl Pts',(-17.3718622664474,-14.4063082306997,
115.912069177258)) ;
#184368 = CARTESIAN_POINT('Ctrl Pts',(-17.3666293382131,-14.4803359646283,
115.896130522795)) ;
#184369 = CARTESIAN_POINT('Ctrl Pts',(-17.3613964099789,-14.554363698557,
115.880191868331)) ;
#184370 = CARTESIAN_POINT('Ctrl Pts',(-17.4352002438521,-14.5543636910748,
115.855960797567)) ;
#184371 = CARTESIAN_POINT('Ctrl Pts',(-17.5090040777254,-14.5543636835926,
115.831729726804)) ;
#184372 = CARTESIAN_POINT('Ctrl Pts',(-17.5142370059596,-14.4803359496639,
115.847668381267)) ;
#184373 = CARTESIAN_POINT('Ctrl Pts',(-17.5941239798052,-14.5045829128103,
116.126404146317)) ;
#184374 = CARTESIAN_POINT('Ctrl Pts',(-17.5930539491612,-14.4287553960091,
116.123145004861)) ;
#184375 = CARTESIAN_POINT('Ctrl Pts',(-17.5192501180761,-14.4287553947463,
116.147376084117)) ;
#184376 = CARTESIAN_POINT('Ctrl Pts',(-17.4454462869911,-14.4287553934836,
116.171607163373)) ;
#184377 = CARTESIAN_POINT('Ctrl Pts',(-17.446516317635,-14.5045829102848,
116.174866304829)) ;
#184378 = CARTESIAN_POINT('Ctrl Pts',(-17.447586348279,-14.580410427086,116.178125446286)) ;
#184379 = CARTESIAN_POINT('Ctrl Pts',(-17.5213901793641,-14.5804104283487,
116.15389436703)) ;
#184380 = CARTESIAN_POINT('Ctrl Pts',(-17.5951940104491,-14.5804104296115,
116.129663287774)) ;
#184381 = CARTESIAN_POINT('Ctrl Pts',(-17.5941239798052,-14.5045829128103,
116.126404146317)) ;
#184382 = CARTESIAN_POINT('Ctrl Pts',(-17.6729871089332,-14.4510580252238,
116.402111327135)) ;
#184383 = CARTESIAN_POINT('Ctrl Pts',(-17.665674706909,-14.3788579006376,
116.379838929482)) ;
#184384 = CARTESIAN_POINT('Ctrl Pts',(-17.5918708779827,-14.3788578861591,
116.404070015313)) ;
#184385 = CARTESIAN_POINT('Ctrl Pts',(-17.5180670490564,-14.3788578716805,
116.428301101144)) ;
#184386 = CARTESIAN_POINT('Ctrl Pts',(-17.5253794510806,-14.4510579962666,
116.450573498798)) ;
#184387 = CARTESIAN_POINT('Ctrl Pts',(-17.5326918531049,-14.5232581208527,
116.472845896452)) ;
#184388 = CARTESIAN_POINT('Ctrl Pts',(-17.6064956820311,-14.5232581353313,
116.448614810621)) ;
#184389 = CARTESIAN_POINT('Ctrl Pts',(-17.6802995109574,-14.5232581498099,
116.424383724789)) ;
#184390 = CARTESIAN_POINT('Ctrl Pts',(-17.6729871089332,-14.4510580252238,
116.402111327135)) ;
#184391 = CARTESIAN_POINT('Ctrl Pts',(-17.7442108074172,-14.3231627979094,
116.654564949859)) ;
#184392 = CARTESIAN_POINT('Ctrl Pts',(-17.7311801239932,-14.2597876685306,
116.614875589526)) ;
#184393 = CARTESIAN_POINT('Ctrl Pts',(-17.6573762957046,-14.2597876370506,
116.639106677299)) ;
#184394 = CARTESIAN_POINT('Ctrl Pts',(-17.583572467416,-14.2597876055706,
116.663337765073)) ;
#184395 = CARTESIAN_POINT('Ctrl Pts',(-17.59660315084,-14.3231627349493,116.703027125406)) ;
#184396 = CARTESIAN_POINT('Ctrl Pts',(-17.6096338342639,-14.386537864328,
116.74271648574)) ;
#184397 = CARTESIAN_POINT('Ctrl Pts',(-17.6834376625525,-14.3865378958081,
116.718485397966)) ;
#184398 = CARTESIAN_POINT('Ctrl Pts',(-17.7572414908411,-14.3865379272881,
116.694254310193)) ;
#184399 = CARTESIAN_POINT('Ctrl Pts',(-17.7442108074172,-14.3231627979094,
116.654564949859)) ;
#184400 = CARTESIAN_POINT('Ctrl Pts',(-17.8017294897933,-14.1311846385056,
116.865136329538)) ;
#184401 = CARTESIAN_POINT('Ctrl Pts',(-17.7839321083557,-14.0811216324566,
116.810928376012)) ;
#184402 = CARTESIAN_POINT('Ctrl Pts',(-17.7101282784815,-14.0811215835067,
116.835159458956)) ;
#184403 = CARTESIAN_POINT('Ctrl Pts',(-17.6363244486073,-14.0811215345568,
116.8593905419)) ;
#184404 = CARTESIAN_POINT('Ctrl Pts',(-17.6541218300448,-14.1311845406059,
116.913598495426)) ;
#184405 = CARTESIAN_POINT('Ctrl Pts',(-17.6719192114823,-14.181247546655,
116.967806448952)) ;
#184406 = CARTESIAN_POINT('Ctrl Pts',(-17.7457230413565,-14.1812475956048,
116.943575366008)) ;
#184407 = CARTESIAN_POINT('Ctrl Pts',(-17.8195268712308,-14.1812476445547,
116.919344283064)) ;
#184408 = CARTESIAN_POINT('Ctrl Pts',(-17.8017294897933,-14.1311846385056,
116.865136329538)) ;
#184409 = CARTESIAN_POINT('Ctrl Pts',(-17.841097170979,-13.8873682377616,
117.020560844287)) ;
#184410 = CARTESIAN_POINT('Ctrl Pts',(-17.8197905237819,-13.8542552865156,
116.955664233311)) ;
#184411 = CARTESIAN_POINT('Ctrl Pts',(-17.7459866905101,-13.8542552201397,
116.979895305907)) ;
#184412 = CARTESIAN_POINT('Ctrl Pts',(-17.6721828572383,-13.8542551537638,
117.004126378502)) ;
#184413 = CARTESIAN_POINT('Ctrl Pts',(-17.6934895044355,-13.8873681050098,
117.069022989479)) ;
#184414 = CARTESIAN_POINT('Ctrl Pts',(-17.7147961516327,-13.9204810562558,
117.133919600455)) ;
#184415 = CARTESIAN_POINT('Ctrl Pts',(-17.7885999849044,-13.9204811226317,
117.109688527859)) ;
#184416 = CARTESIAN_POINT('Ctrl Pts',(-17.8624038181762,-13.9204811890076,
117.085457455263)) ;
#184417 = CARTESIAN_POINT('Ctrl Pts',(-17.841097170979,-13.8873682377616,
117.020560844287)) ;
#184418 = CARTESIAN_POINT('Ctrl Pts',(-17.858439925497,-13.6103444957185,
117.108831164747)) ;
#184419 = CARTESIAN_POINT('Ctrl Pts',(-17.8351581118065,-13.5965245493847,
117.037918515183)) ;
#184420 = CARTESIAN_POINT('Ctrl Pts',(-17.7613542730539,-13.5965244695658,
117.062149571085)) ;
#184421 = CARTESIAN_POINT('Ctrl Pts',(-17.6875504343013,-13.5965243897469,
117.086380626987)) ;
#184422 = CARTESIAN_POINT('Ctrl Pts',(-17.7108322479918,-13.6103443360808,
117.157293276551)) ;
#184423 = CARTESIAN_POINT('Ctrl Pts',(-17.7341140616824,-13.6241642824146,
117.228205926115)) ;
#184424 = CARTESIAN_POINT('Ctrl Pts',(-17.807917900435,-13.6241643622335,
117.203974870213)) ;
#184425 = CARTESIAN_POINT('Ctrl Pts',(-17.8817217391876,-13.6241644420523,
117.179743814311)) ;
#184426 = CARTESIAN_POINT('Ctrl Pts',(-17.858439925497,-13.6103444957185,
117.108831164747)) ;
#184427 = CARTESIAN_POINT('Ctrl Pts',(-17.8518767191496,-13.3193309051749,
117.12431916614)) ;
#184428 = CARTESIAN_POINT('Ctrl Pts',(-17.8282851787465,-13.3258084661624,
117.052463138851)) ;
#184429 = CARTESIAN_POINT('Ctrl Pts',(-17.7544813330107,-13.3258083784264,
117.076694173483)) ;
#184430 = CARTESIAN_POINT('Ctrl Pts',(-17.680677487275,-13.3258082906904,
117.100925208115)) ;
#184431 = CARTESIAN_POINT('Ctrl Pts',(-17.7042690276781,-13.3193307297029,
117.172781235404)) ;
#184432 = CARTESIAN_POINT('Ctrl Pts',(-17.7278605680812,-13.3128531687154,
117.244637262693)) ;
#184433 = CARTESIAN_POINT('Ctrl Pts',(-17.801664413817,-13.3128532564514,
117.22040622806)) ;
#184434 = CARTESIAN_POINT('Ctrl Pts',(-17.8754682595527,-13.3128533441874,
117.196175193428)) ;
#184435 = CARTESIAN_POINT('Ctrl Pts',(-17.8518767191496,-13.3193309051749,
117.12431916614)) ;
#184436 = CARTESIAN_POINT('Ctrl Pts',(-17.8211064298511,-13.0356124679736,
117.066047429482)) ;
#184437 = CARTESIAN_POINT('Ctrl Pts',(-17.7988953105037,-13.0619076839879,
116.998395941887)) ;
#184438 = CARTESIAN_POINT('Ctrl Pts',(-17.7250914569277,-13.061907595961,
117.022626952639)) ;
#184439 = CARTESIAN_POINT('Ctrl Pts',(-17.6512876033518,-13.061907507934,
117.046857963391)) ;
#184440 = CARTESIAN_POINT('Ctrl Pts',(-17.6734987226992,-13.0356122919197,
117.114509450987)) ;
#184441 = CARTESIAN_POINT('Ctrl Pts',(-17.6957098420467,-13.0093170759053,
117.182160938582)) ;
#184442 = CARTESIAN_POINT('Ctrl Pts',(-17.7695136956227,-13.0093171639322,
117.15792992783)) ;
#184443 = CARTESIAN_POINT('Ctrl Pts',(-17.8433175491986,-13.0093172519592,
117.133698917078)) ;
#184444 = CARTESIAN_POINT('Ctrl Pts',(-17.8211064298511,-13.0356124679736,
117.066047429482)) ;
#184445 = CARTESIAN_POINT('Ctrl Pts',(-17.7676238677098,-12.7792808148317,
116.938592617512)) ;
#184446 = CARTESIAN_POINT('Ctrl Pts',(-17.7483808915062,-12.8235105133311,
116.87998161493)) ;
#184447 = CARTESIAN_POINT('Ctrl Pts',(-17.6745770300968,-12.8235104331366,
116.904212601823)) ;
#184448 = CARTESIAN_POINT('Ctrl Pts',(-17.6007731686875,-12.8235103529421,
116.928443588715)) ;
#184449 = CARTESIAN_POINT('Ctrl Pts',(-17.6200161448911,-12.7792806544427,
116.987054591298)) ;
#184450 = CARTESIAN_POINT('Ctrl Pts',(-17.6392591210947,-12.7350509559433,
117.045665593881)) ;
#184451 = CARTESIAN_POINT('Ctrl Pts',(-17.7130629825041,-12.7350510361378,
117.021434606988)) ;
#184452 = CARTESIAN_POINT('Ctrl Pts',(-17.7868668439134,-12.7350511163323,
116.997203620095)) ;
#184453 = CARTESIAN_POINT('Ctrl Pts',(-17.7676238677098,-12.7792808148317,
116.938592617512)) ;
#184454 = CARTESIAN_POINT('Ctrl Pts',(-17.6943411970397,-12.568318140118,
116.750890389629)) ;
#184455 = CARTESIAN_POINT('Ctrl Pts',(-17.6794516619109,-12.6273412297626,
116.705539266054)) ;
#184456 = CARTESIAN_POINT('Ctrl Pts',(-17.6056477934581,-12.6273411651946,
116.729770231493)) ;
#184457 = CARTESIAN_POINT('Ctrl Pts',(-17.5318439250053,-12.6273411006266,
116.754001196933)) ;
#184458 = CARTESIAN_POINT('Ctrl Pts',(-17.5467334601341,-12.568318010982,
116.799352320509)) ;
#184459 = CARTESIAN_POINT('Ctrl Pts',(-17.5616229952629,-12.5092949213373,
116.844703444085)) ;
#184460 = CARTESIAN_POINT('Ctrl Pts',(-17.6354268637157,-12.5092949859053,
116.820472478645)) ;
#184461 = CARTESIAN_POINT('Ctrl Pts',(-17.7092307321685,-12.5092950504733,
116.796241513205)) ;
#184462 = CARTESIAN_POINT('Ctrl Pts',(-17.6943411970397,-12.568318140118,
116.750890389629)) ;
#184463 = CARTESIAN_POINT('Ctrl Pts',(-17.6058868196778,-12.4185302079718,
116.516953818039)) ;
#184464 = CARTESIAN_POINT('Ctrl Pts',(-17.5964167836325,-12.4880976547663,
116.488109614182)) ;
#184465 = CARTESIAN_POINT('Ctrl Pts',(-17.5226129098786,-12.4880976127796,
116.512340563475)) ;
#184466 = CARTESIAN_POINT('Ctrl Pts',(-17.4488090361247,-12.4880975707929,
116.536571512769)) ;
#184467 = CARTESIAN_POINT('Ctrl Pts',(-17.45827907217,-12.4185301239984,116.565415716626)) ;
#184468 = CARTESIAN_POINT('Ctrl Pts',(-17.4677491082153,-12.3489626772039,
116.594259920483)) ;
#184469 = CARTESIAN_POINT('Ctrl Pts',(-17.5415529819692,-12.3489627191906,
116.57002897119)) ;
#184470 = CARTESIAN_POINT('Ctrl Pts',(-17.6153568557232,-12.3489627611773,
116.545798021896)) ;
#184471 = CARTESIAN_POINT('Ctrl Pts',(-17.6058868196778,-12.4185302079718,
116.516953818039)) ;
#184472 = CARTESIAN_POINT('Ctrl Pts',(-17.5081423472344,-12.3404555156159,
116.254614223986)) ;
#184473 = CARTESIAN_POINT('Ctrl Pts',(-17.5047506152582,-12.415576081878,
116.24428355356)) ;
#184474 = CARTESIAN_POINT('Ctrl Pts',(-17.4309467386001,-12.415576066971,
116.268514494008)) ;
#184475 = CARTESIAN_POINT('Ctrl Pts',(-17.3571428619421,-12.415576052064,
116.292745434456)) ;
#184476 = CARTESIAN_POINT('Ctrl Pts',(-17.3605345939183,-12.3404554858018,
116.303076104882)) ;
#184477 = CARTESIAN_POINT('Ctrl Pts',(-17.3639263258945,-12.2653349195397,
116.313406775308)) ;
#184478 = CARTESIAN_POINT('Ctrl Pts',(-17.4377302025526,-12.2653349344467,
116.28917583486)) ;
#184479 = CARTESIAN_POINT('Ctrl Pts',(-17.5115340792106,-12.2653349493537,
116.264944894412)) ;
#184480 = CARTESIAN_POINT('Ctrl Pts',(-17.5081423472344,-12.3404555156159,
116.254614223986)) ;
#184481 = CARTESIAN_POINT('Ctrl Pts',(-17.4066726357581,-12.3391866191646,
115.981062491338)) ;
#184482 = CARTESIAN_POINT('Ctrl Pts',(-17.4096253543423,-12.414506911119,
115.990055993629)) ;
#184483 = CARTESIAN_POINT('Ctrl Pts',(-17.3358214773743,-12.4145069252737,
116.014286933133)) ;
#184484 = CARTESIAN_POINT('Ctrl Pts',(-17.2620176004063,-12.4145069394284,
116.038517872637)) ;
#184485 = CARTESIAN_POINT('Ctrl Pts',(-17.2590648818221,-12.339186647474,
116.029524370346)) ;
#184486 = CARTESIAN_POINT('Ctrl Pts',(-17.2561121632379,-12.2638663555197,
116.020530868055)) ;
#184487 = CARTESIAN_POINT('Ctrl Pts',(-17.3299160402059,-12.263866341365,
115.996299928551)) ;
#184488 = CARTESIAN_POINT('Ctrl Pts',(-17.4037199171738,-12.2638663272102,
115.972068989047)) ;
#184489 = CARTESIAN_POINT('Ctrl Pts',(-17.4066726357581,-12.3391866191646,
115.981062491338)) ;
#184490 = CARTESIAN_POINT('Ctrl Pts',(-17.3082335377069,-12.4158174303531,
115.716800039723)) ;
#184491 = CARTESIAN_POINT('Ctrl Pts',(-17.3173273514836,-12.4858997019266,
115.74449832712)) ;
#184492 = CARTESIAN_POINT('Ctrl Pts',(-17.2435234770911,-12.4858997440293,
115.768729274469)) ;
#184493 = CARTESIAN_POINT('Ctrl Pts',(-17.1697196026986,-12.4858997861321,
115.792960221817)) ;
#184494 = CARTESIAN_POINT('Ctrl Pts',(-17.160625788922,-12.4158175145586,
115.76526193442)) ;
#184495 = CARTESIAN_POINT('Ctrl Pts',(-17.1515319751453,-12.3457352429851,
115.737563647023)) ;
#184496 = CARTESIAN_POINT('Ctrl Pts',(-17.2253358495378,-12.3457352008824,
115.713332699674)) ;
#184497 = CARTESIAN_POINT('Ctrl Pts',(-17.2991397239303,-12.3457351587796,
115.689101752326)) ;
#184498 = CARTESIAN_POINT('Ctrl Pts',(-17.3082335377069,-12.4158174303531,
115.716800039723)) ;
#184499 = CARTESIAN_POINT('Ctrl Pts',(-17.219815391379,-12.5633739390689,
115.482834834317)) ;
#184500 = CARTESIAN_POINT('Ctrl Pts',(-17.2343644873207,-12.6232581610032,
115.527149031009)) ;
#184501 = CARTESIAN_POINT('Ctrl Pts',(-17.1605606178606,-12.623258227084,
115.551379993381)) ;
#184502 = CARTESIAN_POINT('Ctrl Pts',(-17.0867567484005,-12.6232582931649,
115.575610955753)) ;
#184503 = CARTESIAN_POINT('Ctrl Pts',(-17.0722076524589,-12.5633740712307,
115.53129675906)) ;
#184504 = CARTESIAN_POINT('Ctrl Pts',(-17.0576585565172,-12.5034898492964,
115.486982562368)) ;
#184505 = CARTESIAN_POINT('Ctrl Pts',(-17.1314624259772,-12.5034897832155,
115.462751599996)) ;
#184506 = CARTESIAN_POINT('Ctrl Pts',(-17.2052662954373,-12.5034897171346,
115.438520637625)) ;
#184507 = CARTESIAN_POINT('Ctrl Pts',(-17.219815391379,-12.5633739390689,
115.482834834317)) ;
#184508 = CARTESIAN_POINT('Ctrl Pts',(-17.1458699167164,-12.7732714821549,
115.293194413268)) ;
#184509 = CARTESIAN_POINT('Ctrl Pts',(-17.1648670745331,-12.8185910964645,
115.351056688798)) ;
#184510 = CARTESIAN_POINT('Ctrl Pts',(-17.0910632120963,-12.8185911800319,
115.375287672561)) ;
#184511 = CARTESIAN_POINT('Ctrl Pts',(-17.0172593496596,-12.8185912635994,
115.399518656325)) ;
#184512 = CARTESIAN_POINT('Ctrl Pts',(-16.9982621918429,-12.7732716492898,
115.341656380795)) ;
#184513 = CARTESIAN_POINT('Ctrl Pts',(-16.9792650340262,-12.7279520349803,
115.283794105265)) ;
#184514 = CARTESIAN_POINT('Ctrl Pts',(-17.053068896463,-12.7279519514128,
115.259563121501)) ;
#184515 = CARTESIAN_POINT('Ctrl Pts',(-17.1268727588998,-12.7279518678453,
115.235332137738)) ;
#184516 = CARTESIAN_POINT('Ctrl Pts',(-17.1458699167164,-12.7732714821549,
115.293194413268)) ;
#184517 = CARTESIAN_POINT('Ctrl Pts',(-17.0918463264668,-13.0290278048664,
115.164127748858)) ;
#184518 = CARTESIAN_POINT('Ctrl Pts',(-17.1139095830556,-13.0565590545988,
115.231328866614)) ;
#184519 = CARTESIAN_POINT('Ctrl Pts',(-17.0401057286706,-13.0565591475459,
115.255559874902)) ;
#184520 = CARTESIAN_POINT('Ctrl Pts',(-16.9663018742856,-13.056559240493,
115.27979088319)) ;
#184521 = CARTESIAN_POINT('Ctrl Pts',(-16.9442386176968,-13.0290279907607,
115.212589765435)) ;
#184522 = CARTESIAN_POINT('Ctrl Pts',(-16.922175361108,-13.0014967410283,
115.145388647679)) ;
#184523 = CARTESIAN_POINT('Ctrl Pts',(-16.995979215493,-13.0014966480811,
115.121157639391)) ;
#184524 = CARTESIAN_POINT('Ctrl Pts',(-17.0697830698779,-13.001496555134,
115.096926631103)) ;
#184525 = CARTESIAN_POINT('Ctrl Pts',(-17.0918463264668,-13.0290278048664,
115.164127748858)) ;
#184526 = CARTESIAN_POINT('Ctrl Pts',(-17.0605849362923,-13.311039520292,
115.10420715475)) ;
#184527 = CARTESIAN_POINT('Ctrl Pts',(-17.0841334043175,-13.3189223773524,
115.175931986978)) ;
#184528 = CARTESIAN_POINT('Ctrl Pts',(-17.0103295581193,-13.3189224724508,
115.200163020201)) ;
#184529 = CARTESIAN_POINT('Ctrl Pts',(-16.936525711921,-13.3189225675491,
115.224394053425)) ;
#184530 = CARTESIAN_POINT('Ctrl Pts',(-16.9129772438958,-13.3110397104886,
115.152669221197)) ;
#184531 = CARTESIAN_POINT('Ctrl Pts',(-16.8894287758706,-13.3031568534281,
115.08094438897)) ;
#184532 = CARTESIAN_POINT('Ctrl Pts',(-16.9632326220688,-13.3031567583298,
115.056713355746)) ;
#184533 = CARTESIAN_POINT('Ctrl Pts',(-17.0370364682671,-13.3031566632315,
115.032482322523)) ;
#184534 = CARTESIAN_POINT('Ctrl Pts',(-17.0605849362923,-13.311039520292,
115.10420715475)) ;
#184535 = CARTESIAN_POINT('Ctrl Pts',(-17.0532782891826,-13.6025944687999,
115.117484856744)) ;
#184536 = CARTESIAN_POINT('Ctrl Pts',(-17.0766371468441,-13.5901335291486,
115.188632166515)) ;
#184537 = CARTESIAN_POINT('Ctrl Pts',(-17.0028333083748,-13.5901336172138,
115.212863223279)) ;
#184538 = CARTESIAN_POINT('Ctrl Pts',(-16.9290294699055,-13.5901337052789,
115.237094280044)) ;
#184539 = CARTESIAN_POINT('Ctrl Pts',(-16.905670612244,-13.6025946449302,
115.165946970274)) ;
#184540 = CARTESIAN_POINT('Ctrl Pts',(-16.8823117545824,-13.6150555845815,
115.094799660503)) ;
#184541 = CARTESIAN_POINT('Ctrl Pts',(-16.9561155930517,-13.6150554965163,
115.070568603739)) ;
#184542 = CARTESIAN_POINT('Ctrl Pts',(-17.029919431521,-13.6150554084512,
115.046337546974)) ;
#184543 = CARTESIAN_POINT('Ctrl Pts',(-17.0532782891826,-13.6025944687999,
115.117484856744)) ;
#184544 = CARTESIAN_POINT('Ctrl Pts',(-17.070132390923,-13.8812809383862,
115.204405035369)) ;
#184545 = CARTESIAN_POINT('Ctrl Pts',(-17.0916135474401,-13.8493436684039,
115.269833170565)) ;
#184546 = CARTESIAN_POINT('Ctrl Pts',(-17.0178097151085,-13.8493437421996,
115.294064246025)) ;
#184547 = CARTESIAN_POINT('Ctrl Pts',(-16.9440058827769,-13.8493438159953,
115.318295321484)) ;
#184548 = CARTESIAN_POINT('Ctrl Pts',(-16.9225247262599,-13.8812810859776,
115.252867186287)) ;
#184549 = CARTESIAN_POINT('Ctrl Pts',(-16.9010435697428,-13.91321835596,115.187439051091)) ;
#184550 = CARTESIAN_POINT('Ctrl Pts',(-16.9748474020744,-13.9132182821642,
115.163207975632)) ;
#184551 = CARTESIAN_POINT('Ctrl Pts',(-17.048651234406,-13.9132182083685,
115.138976900173)) ;
#184552 = CARTESIAN_POINT('Ctrl Pts',(-17.070132390923,-13.8812809383862,
115.204405035369)) ;
#184553 = CARTESIAN_POINT('Ctrl Pts',(-17.1089513768232,-14.1255805603194,
115.358085859789)) ;
#184554 = CARTESIAN_POINT('Ctrl Pts',(-17.1270212361338,-14.0765381533461,
115.413123734245)) ;
#184555 = CARTESIAN_POINT('Ctrl Pts',(-17.0532174080133,-14.0765382096367,
115.437354822531)) ;
#184556 = CARTESIAN_POINT('Ctrl Pts',(-16.9794135798929,-14.0765382659272,
115.461585910816)) ;
#184557 = CARTESIAN_POINT('Ctrl Pts',(-16.9613437205823,-14.1255806729005,
115.40654803636)) ;
#184558 = CARTESIAN_POINT('Ctrl Pts',(-16.9432738612718,-14.1746230798738,
115.351510161904)) ;
#184559 = CARTESIAN_POINT('Ctrl Pts',(-17.0170776893922,-14.1746230235832,
115.327279073618)) ;
#184560 = CARTESIAN_POINT('Ctrl Pts',(-17.0908815175127,-14.1746229672927,
115.303047985333)) ;
#184561 = CARTESIAN_POINT('Ctrl Pts',(-17.1089513768232,-14.1255805603194,
115.358085859789)) ;
#184562 = CARTESIAN_POINT('Ctrl Pts',(-17.1659520639075,-14.3187775567506,
115.567024046266)) ;
#184563 = CARTESIAN_POINT('Ctrl Pts',(-17.1793384581924,-14.2561721996919,
115.607796842057)) ;
#184564 = CARTESIAN_POINT('Ctrl Pts',(-17.1055346324634,-14.2561722372695,
115.632027937627)) ;
#184565 = CARTESIAN_POINT('Ctrl Pts',(-17.0317308067344,-14.256172274847,
115.656259033196)) ;
#184566 = CARTESIAN_POINT('Ctrl Pts',(-17.0183444124495,-14.3187776319056,
115.615486237406)) ;
#184567 = CARTESIAN_POINT('Ctrl Pts',(-17.0049580181646,-14.3813829889642,
115.574713441615)) ;
#184568 = CARTESIAN_POINT('Ctrl Pts',(-17.0787618438936,-14.3813829513867,
115.550482346045)) ;
#184569 = CARTESIAN_POINT('Ctrl Pts',(-17.1525656696226,-14.3813829138092,
115.526251250476)) ;
#184570 = CARTESIAN_POINT('Ctrl Pts',(-17.1659520639075,-14.3187775567506,
115.567024046266)) ;
#184571 = CARTESIAN_POINT('Ctrl Pts',(-17.2367614107398,-14.4483980300764,
115.818159542775)) ;
#184572 = CARTESIAN_POINT('Ctrl Pts',(-17.2444903655536,-14.3766476693991,
115.841700690922)) ;
#184573 = CARTESIAN_POINT('Ctrl Pts',(-17.1706865398769,-14.3766476878194,
115.865931786651)) ;
#184574 = CARTESIAN_POINT('Ctrl Pts',(-17.0968827142002,-14.3766477062396,
115.89016288238)) ;
#184575 = CARTESIAN_POINT('Ctrl Pts',(-17.0891537593863,-14.4483980669169,
115.866621734233)) ;
#184576 = CARTESIAN_POINT('Ctrl Pts',(-17.0814248045724,-14.5201484275943,
115.843080586087)) ;
#184577 = CARTESIAN_POINT('Ctrl Pts',(-17.1552286302491,-14.520148409174,
115.818849490358)) ;
#184578 = CARTESIAN_POINT('Ctrl Pts',(-17.2290324559259,-14.5201483907537,
115.794618394629)) ;
#184579 = CARTESIAN_POINT('Ctrl Pts',(-17.2367614107398,-14.4483980300764,
115.818159542775)) ;
#184580 = CARTESIAN_POINT('Ctrl Pts',(-17.3155873842172,-14.5042941688686,
116.093793589286)) ;
#184581 = CARTESIAN_POINT('Ctrl Pts',(-17.3170888936789,-14.4285319857966,
116.098366943866)) ;
#184582 = CARTESIAN_POINT('Ctrl Pts',(-17.2432850659568,-14.4285319877587,
116.122598033365)) ;
#184583 = CARTESIAN_POINT('Ctrl Pts',(-17.1694812382346,-14.4285319897207,
116.146829122864)) ;
#184584 = CARTESIAN_POINT('Ctrl Pts',(-17.1679797287729,-14.5042941727927,
116.142255768284)) ;
#184585 = CARTESIAN_POINT('Ctrl Pts',(-17.1664782193112,-14.5800563558646,
116.137682413704)) ;
#184586 = CARTESIAN_POINT('Ctrl Pts',(-17.2402820470333,-14.5800563539026,
116.113451324205)) ;
#184587 = CARTESIAN_POINT('Ctrl Pts',(-17.3140858747555,-14.5800563519406,
116.089220234706)) ;
#184588 = CARTESIAN_POINT('Ctrl Pts',(-17.3155873842172,-14.5042941688686,
116.093793589286)) ;
#184589 = CARTESIAN_POINT('Ctrl Pts',(-17.3959128562578,-14.4816544194473,
116.374043524353)) ;
#184590 = CARTESIAN_POINT('Ctrl Pts',(-17.3910716132192,-14.4073576522614,
116.359297878409)) ;
#184591 = CARTESIAN_POINT('Ctrl Pts',(-17.3172677820769,-14.4073576431116,
116.383528957491)) ;
#184592 = CARTESIAN_POINT('Ctrl Pts',(-17.2434639509345,-14.4073576339619,
116.407760036573)) ;
#184593 = CARTESIAN_POINT('Ctrl Pts',(-17.2483051939732,-14.4816544011478,
116.422505682517)) ;
#184594 = CARTESIAN_POINT('Ctrl Pts',(-17.2531464370118,-14.5559511683337,
116.437251328461)) ;
#184595 = CARTESIAN_POINT('Ctrl Pts',(-17.3269502681541,-14.5559511774834,
116.413020249379)) ;
#184596 = CARTESIAN_POINT('Ctrl Pts',(-17.4007540992964,-14.5559511866331,
116.388789170297)) ;
#184597 = CARTESIAN_POINT('Ctrl Pts',(-17.3959128562578,-14.4816544194473,
116.374043524353)) ;
#184598 = CARTESIAN_POINT('Ctrl Pts',(-17.470339914178,-14.3839486349316,
116.635941043976)) ;
#184599 = CARTESIAN_POINT('Ctrl Pts',(-17.4595662274915,-14.3163620052717,
116.603126131994)) ;
#184600 = CARTESIAN_POINT('Ctrl Pts',(-17.3857623934809,-14.3163619889056,
116.627357202339)) ;
#184601 = CARTESIAN_POINT('Ctrl Pts',(-17.3119585594702,-14.3163619725394,
116.651588272685)) ;
#184602 = CARTESIAN_POINT('Ctrl Pts',(-17.3227322461567,-14.3839486021993,
116.684403184667)) ;
#184603 = CARTESIAN_POINT('Ctrl Pts',(-17.3335059328432,-14.4515352318592,
116.717218096649)) ;
#184604 = CARTESIAN_POINT('Ctrl Pts',(-17.4073097668538,-14.4515352482253,
116.692987026303)) ;
#184605 = CARTESIAN_POINT('Ctrl Pts',(-17.4811136008645,-14.4515352645915,
116.668755955958)) ;
#184606 = CARTESIAN_POINT('Ctrl Pts',(-17.470339914178,-14.3839486349316,
116.635941043976)) ;
#184607 = CARTESIAN_POINT('Ctrl Pts',(-17.5344056730198,-14.2160711628555,
116.866668150428)) ;
#184608 = CARTESIAN_POINT('Ctrl Pts',(-17.5184057446407,-14.1601035188724,
116.817934949686)) ;
#184609 = CARTESIAN_POINT('Ctrl Pts',(-17.4446019067002,-14.1601035014112,
116.842166008062)) ;
#184610 = CARTESIAN_POINT('Ctrl Pts',(-17.3707980687597,-14.1601034839499,
116.866397066437)) ;
#184611 = CARTESIAN_POINT('Ctrl Pts',(-17.3867979971388,-14.216071127933,
116.915130267179)) ;
#184612 = CARTESIAN_POINT('Ctrl Pts',(-17.4027979255179,-14.272038771916,
116.96386346792)) ;
#184613 = CARTESIAN_POINT('Ctrl Pts',(-17.4766017634584,-14.2720387893772,
116.939632409545)) ;
#184614 = CARTESIAN_POINT('Ctrl Pts',(-17.5504056013989,-14.2720388068385,
116.915401351169)) ;
#184615 = CARTESIAN_POINT('Ctrl Pts',(-17.5344056730198,-14.2160711628555,
116.866668150428)) ;
#184616 = CARTESIAN_POINT('Ctrl Pts',(-17.5816569877728,-13.9907700541576,
117.046110214416)) ;
#184617 = CARTESIAN_POINT('Ctrl Pts',(-17.5615983820216,-13.9504492968838,
116.985014937421)) ;
#184618 = CARTESIAN_POINT('Ctrl Pts',(-17.4877945411903,-13.950449282471,
117.009245986992)) ;
#184619 = CARTESIAN_POINT('Ctrl Pts',(-17.4139907003589,-13.9504492680581,
117.033477036562)) ;
#184620 = CARTESIAN_POINT('Ctrl Pts',(-17.4340493061101,-13.9907700253318,
117.094572313557)) ;
#184621 = CARTESIAN_POINT('Ctrl Pts',(-17.4541079118614,-14.0310907826056,
117.155667590553)) ;
#184622 = CARTESIAN_POINT('Ctrl Pts',(-17.5279117526927,-14.0310907970185,
117.131436540982)) ;
#184623 = CARTESIAN_POINT('Ctrl Pts',(-17.601715593524,-14.0310908114314,
117.107205491412)) ;
#184624 = CARTESIAN_POINT('Ctrl Pts',(-17.5816569877728,-13.9907700541576,
117.046110214416)) ;
#184625 = CARTESIAN_POINT('Ctrl Pts',(-17.6081495369059,-13.7263636069236,
117.162089654627)) ;
#184626 = CARTESIAN_POINT('Ctrl Pts',(-17.5854807397544,-13.7044442251976,
117.093044155887)) ;
#184627 = CARTESIAN_POINT('Ctrl Pts',(-17.5116768971497,-13.7044442144499,
117.117275200056)) ;
#184628 = CARTESIAN_POINT('Ctrl Pts',(-17.437873054545,-13.7044442037021,
117.141506244225)) ;
#184629 = CARTESIAN_POINT('Ctrl Pts',(-17.4605418516965,-13.7263635854281,
117.210551742966)) ;
#184630 = CARTESIAN_POINT('Ctrl Pts',(-17.4832106488481,-13.7482829671541,
117.279597241706)) ;
#184631 = CARTESIAN_POINT('Ctrl Pts',(-17.5570144914527,-13.7482829779018,
117.255366197537)) ;
#184632 = CARTESIAN_POINT('Ctrl Pts',(-17.6308183340574,-13.7482829886496,
117.231135153367)) ;
#184633 = CARTESIAN_POINT('Ctrl Pts',(-17.6081495369059,-13.7263636069236,
117.162089654627)) ;
#184634 = CARTESIAN_POINT('Ctrl Pts',(-17.6114977252136,-13.4372481920934,
117.207915677809)) ;
#184635 = CARTESIAN_POINT('Ctrl Pts',(-17.5878235258813,-13.4354837655308,
117.135807886383)) ;
#184636 = CARTESIAN_POINT('Ctrl Pts',(-17.5140196823244,-13.4354837614887,
117.160038927651)) ;
#184637 = CARTESIAN_POINT('Ctrl Pts',(-17.4402158387675,-13.4354837574465,
117.18426996892)) ;
#184638 = CARTESIAN_POINT('Ctrl Pts',(-17.4638900380998,-13.4372481840091,
117.256377760346)) ;
#184639 = CARTESIAN_POINT('Ctrl Pts',(-17.4875642374321,-13.4390126105717,
117.328485551772)) ;
#184640 = CARTESIAN_POINT('Ctrl Pts',(-17.561368080989,-13.4390126146139,
117.304254510503)) ;
#184641 = CARTESIAN_POINT('Ctrl Pts',(-17.6351719245459,-13.4390126186561,
117.280023469235)) ;
#184642 = CARTESIAN_POINT('Ctrl Pts',(-17.6114977252136,-13.4372481920934,
117.207915677809)) ;
#184643 = CARTESIAN_POINT('Ctrl Pts',(-17.5903413936119,-13.1479585724495,
117.178954366257)) ;
#184644 = CARTESIAN_POINT('Ctrl Pts',(-17.5673748053404,-13.1663919966203,
117.10900184403)) ;
#184645 = CARTESIAN_POINT('Ctrl Pts',(-17.4935709618626,-13.1663919968395,
117.13323288554)) ;
#184646 = CARTESIAN_POINT('Ctrl Pts',(-17.4197671183847,-13.1663919970587,
117.157463927049)) ;
#184647 = CARTESIAN_POINT('Ctrl Pts',(-17.4427337066562,-13.1479585728878,
117.227416449276)) ;
#184648 = CARTESIAN_POINT('Ctrl Pts',(-17.4657002949275,-13.1295251487169,
117.297368971502)) ;
#184649 = CARTESIAN_POINT('Ctrl Pts',(-17.5395041384054,-13.1295251484978,
117.273137929993)) ;
#184650 = CARTESIAN_POINT('Ctrl Pts',(-17.6133079818833,-13.1295251482786,
117.248906888483)) ;
#184651 = CARTESIAN_POINT('Ctrl Pts',(-17.5903413936119,-13.1479585724495,
117.178954366257)) ;
#184652 = CARTESIAN_POINT('Ctrl Pts',(-17.5459869448181,-12.8791408632362,
117.079169963688)) ;
#184653 = CARTESIAN_POINT('Ctrl Pts',(-17.52535255275,-12.9163723052174,117.016320934844)) ;
#184654 = CARTESIAN_POINT('Ctrl Pts',(-17.4515487096923,-12.9163723075118,
117.040551977634)) ;
#184655 = CARTESIAN_POINT('Ctrl Pts',(-17.3777448666347,-12.9163723098062,
117.064783020423)) ;
#184656 = CARTESIAN_POINT('Ctrl Pts',(-17.3983792587028,-12.8791408678251,
117.127632049267)) ;
#184657 = CARTESIAN_POINT('Ctrl Pts',(-17.419013650771,-12.8419094258439,
117.19048107811)) ;
#184658 = CARTESIAN_POINT('Ctrl Pts',(-17.4928174938286,-12.8419094235494,
117.166250035321)) ;
#184659 = CARTESIAN_POINT('Ctrl Pts',(-17.5666213368863,-12.841909421255,
117.142018992531)) ;
#184660 = CARTESIAN_POINT('Ctrl Pts',(-17.5459869448181,-12.8791408632362,
117.079169963688)) ;
#184661 = CARTESIAN_POINT('Ctrl Pts',(-17.480026568366,-12.6468837882592,
116.913878073808)) ;
#184662 = CARTESIAN_POINT('Ctrl Pts',(-17.4632304799261,-12.7003895422397,
116.862719898524)) ;
#184663 = CARTESIAN_POINT('Ctrl Pts',(-17.389426637272,-12.7003895445952,
116.886950942542)) ;
#184664 = CARTESIAN_POINT('Ctrl Pts',(-17.3156227946178,-12.7003895469507,
116.911181986561)) ;
#184665 = CARTESIAN_POINT('Ctrl Pts',(-17.3324188830577,-12.6468837929702,
116.962340161844)) ;
#184666 = CARTESIAN_POINT('Ctrl Pts',(-17.3492149714976,-12.5933780389898,
117.013498337128)) ;
#184667 = CARTESIAN_POINT('Ctrl Pts',(-17.4230188141518,-12.5933780366342,
116.98926729311)) ;
#184668 = CARTESIAN_POINT('Ctrl Pts',(-17.4968226568059,-12.5933780342787,
116.965036249091)) ;
#184669 = CARTESIAN_POINT('Ctrl Pts',(-17.480026568366,-12.6468837882592,
116.913878073808)) ;
#184670 = CARTESIAN_POINT('Ctrl Pts',(-17.3974510186948,-12.471578495706,
116.697698668639)) ;
#184671 = CARTESIAN_POINT('Ctrl Pts',(-17.3856651005318,-12.5374039130151,
116.661800663601)) ;
#184672 = CARTESIAN_POINT('Ctrl Pts',(-17.3118612576612,-12.5374039137778,
116.68603170696)) ;
#184673 = CARTESIAN_POINT('Ctrl Pts',(-17.2380574147905,-12.5374039145406,
116.710262750319)) ;
#184674 = CARTESIAN_POINT('Ctrl Pts',(-17.2498433329535,-12.4715784972316,
116.746160755357)) ;
#184675 = CARTESIAN_POINT('Ctrl Pts',(-17.2616292511165,-12.4057530799226,
116.782058760395)) ;
#184676 = CARTESIAN_POINT('Ctrl Pts',(-17.3354330939871,-12.4057530791598,
116.757827717036)) ;
#184677 = CARTESIAN_POINT('Ctrl Pts',(-17.4092369368578,-12.405753078397,
116.733596673676)) ;
#184678 = CARTESIAN_POINT('Ctrl Pts',(-17.3974510186948,-12.471578495706,
116.697698668639)) ;
#184679 = CARTESIAN_POINT('Ctrl Pts',(-17.3026957115669,-12.3629963199509,
116.444542308675)) ;
#184680 = CARTESIAN_POINT('Ctrl Pts',(-17.2967752602771,-12.4365002767228,
116.426509569284)) ;
#184681 = CARTESIAN_POINT('Ctrl Pts',(-17.2229714165425,-12.4365002760064,
116.450740610012)) ;
#184682 = CARTESIAN_POINT('Ctrl Pts',(-17.1491675728079,-12.4365002752899,
116.47497165074)) ;
#184683 = CARTESIAN_POINT('Ctrl Pts',(-17.1550880240977,-12.362996318518,
116.49300439013)) ;
#184684 = CARTESIAN_POINT('Ctrl Pts',(-17.1610084753875,-12.289492361746,
116.51103712952)) ;
#184685 = CARTESIAN_POINT('Ctrl Pts',(-17.2348123191221,-12.2894923624625,
116.486806088793)) ;
#184686 = CARTESIAN_POINT('Ctrl Pts',(-17.3086161628567,-12.289492363179,
116.462575048065)) ;
#184687 = CARTESIAN_POINT('Ctrl Pts',(-17.3026957115669,-12.3629963199509,
116.444542308675)) ;
#184688 = CARTESIAN_POINT('Ctrl Pts',(-17.2013092259047,-12.3302292617424,
116.171414664088)) ;
#184689 = CARTESIAN_POINT('Ctrl Pts',(-17.2017212267144,-12.4061292172083,
116.172669551933)) ;
#184690 = CARTESIAN_POINT('Ctrl Pts',(-17.1279173809519,-12.4061292167983,
116.196900586484)) ;
#184691 = CARTESIAN_POINT('Ctrl Pts',(-17.0541135351894,-12.4061292163883,
116.221131621035)) ;
#184692 = CARTESIAN_POINT('Ctrl Pts',(-17.0537015343797,-12.3302292609224,
116.21987673319)) ;
#184693 = CARTESIAN_POINT('Ctrl Pts',(-17.05328953357,-12.2543293054565,116.218621845346)) ;
#184694 = CARTESIAN_POINT('Ctrl Pts',(-17.1270933793325,-12.2543293058665,
116.194390810795)) ;
#184695 = CARTESIAN_POINT('Ctrl Pts',(-17.200897225095,-12.2543293062765,
116.170159776244)) ;
#184696 = CARTESIAN_POINT('Ctrl Pts',(-17.2013092259047,-12.3302292617424,
116.171414664088)) ;
#184697 = CARTESIAN_POINT('Ctrl Pts',(-17.1012548069171,-12.3757631813199,
115.902068780532)) ;
#184698 = CARTESIAN_POINT('Ctrl Pts',(-17.1079209304104,-12.4485939704729,
115.922372716854)) ;
#184699 = CARTESIAN_POINT('Ctrl Pts',(-17.03411708288,-12.448593973849,115.946603746021)) ;
#184700 = CARTESIAN_POINT('Ctrl Pts',(-16.9603132353497,-12.448593977225,
115.970834775187)) ;
#184701 = CARTESIAN_POINT('Ctrl Pts',(-16.9536471118565,-12.3757631880721,
115.950530838865)) ;
#184702 = CARTESIAN_POINT('Ctrl Pts',(-16.9469809883632,-12.3029323989191,
115.930226902543)) ;
#184703 = CARTESIAN_POINT('Ctrl Pts',(-17.0207848358935,-12.302932395543,
115.905995873376)) ;
#184704 = CARTESIAN_POINT('Ctrl Pts',(-17.0945886834239,-12.302932392167,
115.88176484421)) ;
#184705 = CARTESIAN_POINT('Ctrl Pts',(-17.1012548069171,-12.3757631813199,
115.902068780532)) ;
#184706 = CARTESIAN_POINT('Ctrl Pts',(-17.0081478668239,-12.4955339259777,
115.653885289273)) ;
#184707 = CARTESIAN_POINT('Ctrl Pts',(-17.0205919444078,-12.560107521336,
115.691787941355)) ;
#184708 = CARTESIAN_POINT('Ctrl Pts',(-16.946788095502,-12.5601075316302,
115.716018966332)) ;
#184709 = CARTESIAN_POINT('Ctrl Pts',(-16.8729842465962,-12.5601075419243,
115.740249991309)) ;
#184710 = CARTESIAN_POINT('Ctrl Pts',(-16.8605401690123,-12.495533946566,
115.702347339227)) ;
#184711 = CARTESIAN_POINT('Ctrl Pts',(-16.8480960914284,-12.4309603512076,
115.664444687145)) ;
#184712 = CARTESIAN_POINT('Ctrl Pts',(-16.9218999403342,-12.4309603409135,
115.640213662168)) ;
#184713 = CARTESIAN_POINT('Ctrl Pts',(-16.99570378924,-12.4309603306194,115.615982637191)) ;
#184714 = CARTESIAN_POINT('Ctrl Pts',(-17.0081478668239,-12.4955339259777,
115.653885289273)) ;
#184715 = CARTESIAN_POINT('Ctrl Pts',(-16.927880930918,-12.6811191445398,
115.444803605489)) ;
#184716 = CARTESIAN_POINT('Ctrl Pts',(-16.9452148438001,-12.7328282545194,
115.497599906775)) ;
#184717 = CARTESIAN_POINT('Ctrl Pts',(-16.8714109943575,-12.7328282744618,
115.521830930117)) ;
#184718 = CARTESIAN_POINT('Ctrl Pts',(-16.7976071449149,-12.7328282944042,
115.546061953459)) ;
#184719 = CARTESIAN_POINT('Ctrl Pts',(-16.7802732320328,-12.6811191844247,
115.493265652173)) ;
#184720 = CARTESIAN_POINT('Ctrl Pts',(-16.7629393191507,-12.6294100744451,
115.440469350888)) ;
#184721 = CARTESIAN_POINT('Ctrl Pts',(-16.8367431685933,-12.6294100545027,
115.416238327546)) ;
#184722 = CARTESIAN_POINT('Ctrl Pts',(-16.9105470180359,-12.6294100345603,
115.392007304204)) ;
#184723 = CARTESIAN_POINT('Ctrl Pts',(-16.927880930918,-12.6811191445398,
115.444803605489)) ;
#184724 = CARTESIAN_POINT('Ctrl Pts',(-16.8652589405334,-12.9201897809832,
115.289585909363)) ;
#184725 = CARTESIAN_POINT('Ctrl Pts',(-16.8862552957216,-12.9552816729516,
115.353537418807)) ;
#184726 = CARTESIAN_POINT('Ctrl Pts',(-16.8124514468531,-12.9552817052441,
115.377768443898)) ;
#184727 = CARTESIAN_POINT('Ctrl Pts',(-16.7386475979846,-12.9552817375366,
115.401999468988)) ;
#184728 = CARTESIAN_POINT('Ctrl Pts',(-16.7176512427965,-12.9201898455682,
115.338047959545)) ;
#184729 = CARTESIAN_POINT('Ctrl Pts',(-16.6966548876083,-12.8850979535998,
115.274096450101)) ;
#184730 = CARTESIAN_POINT('Ctrl Pts',(-16.7704587364768,-12.8850979213072,
115.24986542501)) ;
#184731 = CARTESIAN_POINT('Ctrl Pts',(-16.8442625853453,-12.8850978890147,
115.225634399919)) ;
#184732 = CARTESIAN_POINT('Ctrl Pts',(-16.8652589405334,-12.9201897809832,
115.289585909363)) ;
#184733 = CARTESIAN_POINT('Ctrl Pts',(-16.8243940341797,-13.1945616988577,
115.200574037482)) ;
#184734 = CARTESIAN_POINT('Ctrl Pts',(-16.8475402280435,-13.2105476900329,
115.271073608491)) ;
#184735 = CARTESIAN_POINT('Ctrl Pts',(-16.7737363815082,-13.2105477342474,
115.295304640688)) ;
#184736 = CARTESIAN_POINT('Ctrl Pts',(-16.699932534973,-13.2105477784618,
115.319535672885)) ;
#184737 = CARTESIAN_POINT('Ctrl Pts',(-16.6767863411092,-13.1945617872866,
115.249036101877)) ;
#184738 = CARTESIAN_POINT('Ctrl Pts',(-16.6536401472453,-13.1785757961114,
115.178536530868)) ;
#184739 = CARTESIAN_POINT('Ctrl Pts',(-16.7274439937806,-13.178575751897,
115.154305498671)) ;
#184740 = CARTESIAN_POINT('Ctrl Pts',(-16.8012478403159,-13.1785757076825,
115.130074466474)) ;
#184741 = CARTESIAN_POINT('Ctrl Pts',(-16.8243940341797,-13.1945616988577,
115.200574037482)) ;
#184742 = CARTESIAN_POINT('Ctrl Pts',(-16.8072714937354,-13.4849425718836,
115.183882623779)) ;
#184743 = CARTESIAN_POINT('Ctrl Pts',(-16.8309128359796,-13.4806775745737,
115.255890336694)) ;
#184744 = CARTESIAN_POINT('Ctrl Pts',(-16.7571089933573,-13.4806776285265,
115.28012138081)) ;
#184745 = CARTESIAN_POINT('Ctrl Pts',(-16.683305150735,-13.4806776824793,
115.304352424926)) ;
#184746 = CARTESIAN_POINT('Ctrl Pts',(-16.6596638084908,-13.4849426797892,
115.23234471201)) ;
#184747 = CARTESIAN_POINT('Ctrl Pts',(-16.6360224662466,-13.4892076770991,
115.160336999094)) ;
#184748 = CARTESIAN_POINT('Ctrl Pts',(-16.7098263088689,-13.4892076231463,
115.136105954979)) ;
#184749 = CARTESIAN_POINT('Ctrl Pts',(-16.7836301514911,-13.4892075691935,
115.111874910863)) ;
#184750 = CARTESIAN_POINT('Ctrl Pts',(-16.8072714937354,-13.4849425718836,
115.183882623779)) ;
#184751 = CARTESIAN_POINT('Ctrl Pts',(-16.8144795961222,-13.7714537290315,
115.241411416659)) ;
#184752 = CARTESIAN_POINT('Ctrl Pts',(-16.8369158670254,-13.7471788354609,
115.309748676522)) ;
#184753 = CARTESIAN_POINT('Ctrl Pts',(-16.7631120298244,-13.7471788958938,
115.33397973715)) ;
#184754 = CARTESIAN_POINT('Ctrl Pts',(-16.6893081926234,-13.7471789563267,
115.358210797778)) ;
#184755 = CARTESIAN_POINT('Ctrl Pts',(-16.6668719217202,-13.7714538498972,
115.289873537915)) ;
#184756 = CARTESIAN_POINT('Ctrl Pts',(-16.6444356508169,-13.7957287434678,
115.221536278052)) ;
#184757 = CARTESIAN_POINT('Ctrl Pts',(-16.718239488018,-13.7957286830349,
115.197305217424)) ;
#184758 = CARTESIAN_POINT('Ctrl Pts',(-16.792043325219,-13.7957286226021,
115.173074156796)) ;
#184759 = CARTESIAN_POINT('Ctrl Pts',(-16.8144795961222,-13.7714537290315,
115.241411416659)) ;
#184760 = CARTESIAN_POINT('Ctrl Pts',(-16.8447740676149,-14.0317199143361,
115.369164792903)) ;
#184761 = CARTESIAN_POINT('Ctrl Pts',(-16.8643935570099,-13.9892386384962,
115.428922590618)) ;
#184762 = CARTESIAN_POINT('Ctrl Pts',(-16.7905897260983,-13.9892386981122,
115.453153670403)) ;
#184763 = CARTESIAN_POINT('Ctrl Pts',(-16.7167858951867,-13.9892387577282,
115.477384750187)) ;
#184764 = CARTESIAN_POINT('Ctrl Pts',(-16.6971664057917,-14.0317200335681,
115.417626952471)) ;
#184765 = CARTESIAN_POINT('Ctrl Pts',(-16.6775469163966,-14.074201309408,
115.357869154755)) ;
#184766 = CARTESIAN_POINT('Ctrl Pts',(-16.7513507473083,-14.074201249792,
115.333638074971)) ;
#184767 = CARTESIAN_POINT('Ctrl Pts',(-16.8251545782199,-14.074201190176,
115.309406995187)) ;
#184768 = CARTESIAN_POINT('Ctrl Pts',(-16.8447740676149,-14.0317199143361,
115.369164792903)) ;
#184769 = CARTESIAN_POINT('Ctrl Pts',(-16.8947662272287,-14.2471737495219,
115.556725502171)) ;
#184770 = CARTESIAN_POINT('Ctrl Pts',(-16.9101934226221,-14.1895888186294,
115.603714248662)) ;
#184771 = CARTESIAN_POINT('Ctrl Pts',(-16.836389597641,-14.1895888696549,
115.627945346509)) ;
#184772 = CARTESIAN_POINT('Ctrl Pts',(-16.7625857726599,-14.1895889206804,
115.652176444357)) ;
#184773 = CARTESIAN_POINT('Ctrl Pts',(-16.7471585772665,-14.2471738515729,
115.605187697866)) ;
#184774 = CARTESIAN_POINT('Ctrl Pts',(-16.7317313818732,-14.3047587824654,
115.558198951375)) ;
#184775 = CARTESIAN_POINT('Ctrl Pts',(-16.8055352068543,-14.3047587314399,
115.533967853527)) ;
#184776 = CARTESIAN_POINT('Ctrl Pts',(-16.8793390318354,-14.3047586804144,
115.50973675568)) ;
#184777 = CARTESIAN_POINT('Ctrl Pts',(-16.8947662272287,-14.2471737495219,
115.556725502171)) ;
#184778 = CARTESIAN_POINT('Ctrl Pts',(-16.961109045615,-14.4050269028801,
115.794454092593)) ;
#184779 = CARTESIAN_POINT('Ctrl Pts',(-16.9711891073453,-14.3363371537911,
115.825156332537)) ;
#184780 = CARTESIAN_POINT('Ctrl Pts',(-16.8973852883592,-14.3363371907916,
115.849387448645)) ;
#184781 = CARTESIAN_POINT('Ctrl Pts',(-16.8235814693732,-14.3363372277921,
115.873618564752)) ;
#184782 = CARTESIAN_POINT('Ctrl Pts',(-16.813501407643,-14.4050269768811,
115.842916324808)) ;
#184783 = CARTESIAN_POINT('Ctrl Pts',(-16.8034213459128,-14.47371672597,115.812214084863)) ;
#184784 = CARTESIAN_POINT('Ctrl Pts',(-16.8772251648988,-14.4737166889695,
115.787982968756)) ;
#184785 = CARTESIAN_POINT('Ctrl Pts',(-16.9510289838848,-14.473716651969,
115.763751852648)) ;
#184786 = CARTESIAN_POINT('Ctrl Pts',(-16.961109045615,-14.4050269028801,
115.794454092593)) ;
#184787 = CARTESIAN_POINT('Ctrl Pts',(-17.0371572122292,-14.4907853879862,
116.061445277914)) ;
#184788 = CARTESIAN_POINT('Ctrl Pts',(-17.0412107801516,-14.4160085433366,
116.073791789988)) ;
#184789 = CARTESIAN_POINT('Ctrl Pts',(-16.9674069650101,-14.4160085589544,
116.098022917805)) ;
#184790 = CARTESIAN_POINT('Ctrl Pts',(-16.8936031498686,-14.4160085745722,
116.122254045622)) ;
#184791 = CARTESIAN_POINT('Ctrl Pts',(-16.8895495819462,-14.4907854192218,
116.109907533549)) ;
#184792 = CARTESIAN_POINT('Ctrl Pts',(-16.8854960140238,-14.5655622638714,
116.097561021475)) ;
#184793 = CARTESIAN_POINT('Ctrl Pts',(-16.9592998291653,-14.5655622482536,
116.073329893658)) ;
#184794 = CARTESIAN_POINT('Ctrl Pts',(-17.0331036443068,-14.5655622326357,
116.04909876584)) ;
#184795 = CARTESIAN_POINT('Ctrl Pts',(-17.0371572122292,-14.4907853879862,
116.061445277914)) ;
#184796 = CARTESIAN_POINT('Ctrl Pts',(-17.1172490342387,-14.5004458117326,
116.340780850017)) ;
#184797 = CARTESIAN_POINT('Ctrl Pts',(-17.1149845378817,-14.4248856962509,
116.333883557615)) ;
#184798 = CARTESIAN_POINT('Ctrl Pts',(-17.0411807245678,-14.4248856868723,
116.358114690999)) ;
#184799 = CARTESIAN_POINT('Ctrl Pts',(-16.9673769112539,-14.4248856774938,
116.382345824383)) ;
#184800 = CARTESIAN_POINT('Ctrl Pts',(-16.9696414076109,-14.5004457929755,
116.389243116785)) ;
#184801 = CARTESIAN_POINT('Ctrl Pts',(-16.9719059039679,-14.5760059084573,
116.396140409187)) ;
#184802 = CARTESIAN_POINT('Ctrl Pts',(-17.0457097172818,-14.5760059178358,
116.371909275803)) ;
#184803 = CARTESIAN_POINT('Ctrl Pts',(-17.1195135305957,-14.5760059272144,
116.347678142419)) ;
#184804 = CARTESIAN_POINT('Ctrl Pts',(-17.1172490342387,-14.5004458117326,
116.340780850017)) ;
#184805 = CARTESIAN_POINT('Ctrl Pts',(-17.195241265685,-14.4322721687238,
116.613881501569)) ;
#184806 = CARTESIAN_POINT('Ctrl Pts',(-17.1867927976471,-14.3613608624439,
116.588148829115)) ;
#184807 = CARTESIAN_POINT('Ctrl Pts',(-17.1129889838628,-14.3613608259143,
116.612379961066)) ;
#184808 = CARTESIAN_POINT('Ctrl Pts',(-17.0391851700784,-14.3613607893847,
116.636611093017)) ;
#184809 = CARTESIAN_POINT('Ctrl Pts',(-17.0476336381162,-14.4322720956646,
116.662343765471)) ;
#184810 = CARTESIAN_POINT('Ctrl Pts',(-17.056082106154,-14.5031834019444,
116.688076437926)) ;
#184811 = CARTESIAN_POINT('Ctrl Pts',(-17.1298859199384,-14.5031834384741,
116.663845305975)) ;
#184812 = CARTESIAN_POINT('Ctrl Pts',(-17.2036897337228,-14.5031834750037,
116.639614174024)) ;
#184813 = CARTESIAN_POINT('Ctrl Pts',(-17.195241265685,-14.4322721687238,
116.613881501569)) ;
#184814 = CARTESIAN_POINT('Ctrl Pts',(-17.2641686388444,-14.2916898608516,
116.859246556023)) ;
#184815 = CARTESIAN_POINT('Ctrl Pts',(-17.2501625770948,-14.2304895577996,
116.816586349776)) ;
#184816 = CARTESIAN_POINT('Ctrl Pts',(-17.1763587600007,-14.2304894954371,
116.840817471646)) ;
#184817 = CARTESIAN_POINT('Ctrl Pts',(-17.1025549429065,-14.2304894330745,
116.865048593516)) ;
#184818 = CARTESIAN_POINT('Ctrl Pts',(-17.1165610046561,-14.2916897361264,
116.907708799763)) ;
#184819 = CARTESIAN_POINT('Ctrl Pts',(-17.1305670664057,-14.3528900391783,
116.95036900601)) ;
#184820 = CARTESIAN_POINT('Ctrl Pts',(-17.2043708834998,-14.3528901015409,
116.92613788414)) ;
#184821 = CARTESIAN_POINT('Ctrl Pts',(-17.278174700594,-14.3528901639035,
116.90190676227)) ;
#184822 = CARTESIAN_POINT('Ctrl Pts',(-17.2641686388444,-14.2916898608516,
116.859246556023)) ;
#184823 = CARTESIAN_POINT('Ctrl Pts',(-17.3187345972075,-14.0883182665925,
117.060933073971)) ;
#184824 = CARTESIAN_POINT('Ctrl Pts',(-17.3001640538882,-14.0412264219864,
117.004370193295)) ;
#184825 = CARTESIAN_POINT('Ctrl Pts',(-17.226360231113,-14.0412263375894,
117.028601297861)) ;
#184826 = CARTESIAN_POINT('Ctrl Pts',(-17.1525564083378,-14.0412262531924,
117.052832402427)) ;
#184827 = CARTESIAN_POINT('Ctrl Pts',(-17.171126951657,-14.0883180977985,
117.109395283104)) ;
#184828 = CARTESIAN_POINT('Ctrl Pts',(-17.1896974949763,-14.1354099424045,
117.165958163781)) ;
#184829 = CARTESIAN_POINT('Ctrl Pts',(-17.2635013177515,-14.1354100268015,
117.141727059215)) ;
#184830 = CARTESIAN_POINT('Ctrl Pts',(-17.3373051405268,-14.1354101111986,
117.117495954648)) ;
#184831 = CARTESIAN_POINT('Ctrl Pts',(-17.3187345972075,-14.0883182665925,
117.060933073971)) ;
#184832 = CARTESIAN_POINT('Ctrl Pts',(-17.3540623162582,-13.837248063462,
117.203966576996)) ;
#184833 = CARTESIAN_POINT('Ctrl Pts',(-17.3322648072597,-13.8076155637165,
117.137574879509)) ;
#184834 = CARTESIAN_POINT('Ctrl Pts',(-17.2584609768669,-13.8076154638135,
117.161805960873)) ;
#184835 = CARTESIAN_POINT('Ctrl Pts',(-17.184657146474,-13.8076153639105,
117.186037042237)) ;
#184836 = CARTESIAN_POINT('Ctrl Pts',(-17.2064546554726,-13.837247863656,
117.252428739724)) ;
#184837 = CARTESIAN_POINT('Ctrl Pts',(-17.2282521644711,-13.8668803634015,
117.318820437211)) ;
#184838 = CARTESIAN_POINT('Ctrl Pts',(-17.3020559948639,-13.8668804633045,
117.294589355847)) ;
#184839 = CARTESIAN_POINT('Ctrl Pts',(-17.3758598252568,-13.8668805632075,
117.270358274483)) ;
#184840 = CARTESIAN_POINT('Ctrl Pts',(-17.3540623162582,-13.837248063462,
117.203966576996)) ;
#184841 = CARTESIAN_POINT('Ctrl Pts',(-17.3670526898512,-13.5564419727403,
117.278940688503)) ;
#184842 = CARTESIAN_POINT('Ctrl Pts',(-17.3435833841598,-13.5463705176912,
117.20745696803)) ;
#184843 = CARTESIAN_POINT('Ctrl Pts',(-17.2697795450213,-13.5463704101859,
117.231688022757)) ;
#184844 = CARTESIAN_POINT('Ctrl Pts',(-17.1959757058828,-13.5463703026806,
117.255919077483)) ;
#184845 = CARTESIAN_POINT('Ctrl Pts',(-17.2194450115743,-13.5564417577297,
117.327402797955)) ;
#184846 = CARTESIAN_POINT('Ctrl Pts',(-17.2429143172658,-13.5665132127787,
117.398886518428)) ;
#184847 = CARTESIAN_POINT('Ctrl Pts',(-17.3167181564042,-13.5665133202841,
117.374655463701)) ;
#184848 = CARTESIAN_POINT('Ctrl Pts',(-17.3905219955427,-13.5665134277894,
117.350424408975)) ;
#184849 = CARTESIAN_POINT('Ctrl Pts',(-17.3670526898512,-13.5564419727403,
117.278940688503)) ;
#184850 = CARTESIAN_POINT('Ctrl Pts',(-17.355858225208,-13.2643191465395,
117.280425433147)) ;
#184851 = CARTESIAN_POINT('Ctrl Pts',(-17.3323992611542,-13.2746275458087,
117.20897321166)) ;
#184852 = CARTESIAN_POINT('Ctrl Pts',(-17.2585954129658,-13.2746274398407,
117.233204238822)) ;
#184853 = CARTESIAN_POINT('Ctrl Pts',(-17.1847915647773,-13.2746273338727,
117.257435265983)) ;
#184854 = CARTESIAN_POINT('Ctrl Pts',(-17.2082505288311,-13.2643189346036,
117.328887487471)) ;
#184855 = CARTESIAN_POINT('Ctrl Pts',(-17.2317094928849,-13.2540105353345,
117.400339708958)) ;
#184856 = CARTESIAN_POINT('Ctrl Pts',(-17.3055133410734,-13.2540106413025,
117.376108681796)) ;
#184857 = CARTESIAN_POINT('Ctrl Pts',(-17.3793171892618,-13.2540107472704,
117.351877654634)) ;
#184858 = CARTESIAN_POINT('Ctrl Pts',(-17.355858225208,-13.2643191465395,
117.280425433147)) ;
#184859 = CARTESIAN_POINT('Ctrl Pts',(-17.3206670190795,-12.984649033957,
117.208638071495)) ;
#184860 = CARTESIAN_POINT('Ctrl Pts',(-17.2988976194389,-13.0144985177463,
117.142331990642)) ;
#184861 = CARTESIAN_POINT('Ctrl Pts',(-17.2250937629149,-13.0144984216522,
117.166562992415)) ;
#184862 = CARTESIAN_POINT('Ctrl Pts',(-17.1512899063909,-13.0144983255582,
117.190793994188)) ;
#184863 = CARTESIAN_POINT('Ctrl Pts',(-17.1730593060315,-12.9846488417689,
117.257100075041)) ;
#184864 = CARTESIAN_POINT('Ctrl Pts',(-17.1948287056722,-12.9547993579796,
117.323406155894)) ;
#184865 = CARTESIAN_POINT('Ctrl Pts',(-17.2686325621962,-12.9547994540736,
117.299175154121)) ;
#184866 = CARTESIAN_POINT('Ctrl Pts',(-17.3424364187202,-12.9547995501676,
117.274944152348)) ;
#184867 = CARTESIAN_POINT('Ctrl Pts',(-17.3206670190795,-12.984649033957,
117.208638071495)) ;
#184868 = CARTESIAN_POINT('Ctrl Pts',(-17.2631129943276,-12.7352694992048,
117.068833096118)) ;
#184869 = CARTESIAN_POINT('Ctrl Pts',(-17.2445948108717,-12.782574545107,
117.012429695249)) ;
#184870 = CARTESIAN_POINT('Ctrl Pts',(-17.1707909475106,-12.7825744663775,
117.036660676197)) ;
#184871 = CARTESIAN_POINT('Ctrl Pts',(-17.0969870841495,-12.782574387648,
117.060891657145)) ;
#184872 = CARTESIAN_POINT('Ctrl Pts',(-17.1155052676054,-12.7352693417458,
117.117295058015)) ;
#184873 = CARTESIAN_POINT('Ctrl Pts',(-17.1340234510614,-12.6879642958436,
117.173698458884)) ;
#184874 = CARTESIAN_POINT('Ctrl Pts',(-17.2078273144225,-12.6879643745731,
117.149467477936)) ;
#184875 = CARTESIAN_POINT('Ctrl Pts',(-17.2816311777836,-12.6879644533026,
117.125236496987)) ;
#184876 = CARTESIAN_POINT('Ctrl Pts',(-17.2631129943276,-12.7352694992048,
117.068833096118)) ;
#184877 = CARTESIAN_POINT('Ctrl Pts',(-17.1866392534368,-12.5350620992742,
116.87137248245)) ;
#184878 = CARTESIAN_POINT('Ctrl Pts',(-17.1726986483145,-12.5964160722861,
116.828911646682)) ;
#184879 = CARTESIAN_POINT('Ctrl Pts',(-17.0988947802738,-12.5964160160119,
116.853142613377)) ;
#184880 = CARTESIAN_POINT('Ctrl Pts',(-17.0250909122331,-12.5964159597377,
116.877373580072)) ;
#184881 = CARTESIAN_POINT('Ctrl Pts',(-17.0390315173554,-12.5350619867258,
116.91983441584)) ;
#184882 = CARTESIAN_POINT('Ctrl Pts',(-17.0529721224778,-12.4737080137138,
116.962295251609)) ;
#184883 = CARTESIAN_POINT('Ctrl Pts',(-17.1267759905185,-12.4737080699881,
116.938064284914)) ;
#184884 = CARTESIAN_POINT('Ctrl Pts',(-17.2005798585592,-12.4737081262623,
116.913833318219)) ;
#184885 = CARTESIAN_POINT('Ctrl Pts',(-17.1866392534368,-12.5350620992742,
116.87137248245)) ;
#184886 = CARTESIAN_POINT('Ctrl Pts',(-17.0960336520393,-12.3981381252086,
116.630846912972)) ;
#184887 = CARTESIAN_POINT('Ctrl Pts',(-17.0876645823112,-12.4691440372206,
116.605356075152)) ;
#184888 = CARTESIAN_POINT('Ctrl Pts',(-17.0138607120287,-12.4691440057978,
116.629587035019)) ;
#184889 = CARTESIAN_POINT('Ctrl Pts',(-16.9400568417462,-12.4691439743751,
116.653817994886)) ;
#184890 = CARTESIAN_POINT('Ctrl Pts',(-16.9484259114743,-12.3981380623631,
116.679308832706)) ;
#184891 = CARTESIAN_POINT('Ctrl Pts',(-16.9567949812024,-12.3271321503511,
116.704799670525)) ;
#184892 = CARTESIAN_POINT('Ctrl Pts',(-17.0305988514848,-12.3271321817739,
116.680568710658)) ;
#184893 = CARTESIAN_POINT('Ctrl Pts',(-17.1044027217673,-12.3271322131966,
116.656337750791)) ;
#184894 = CARTESIAN_POINT('Ctrl Pts',(-17.0960336520393,-12.3981381252086,
116.630846912972)) ;
#184895 = CARTESIAN_POINT('Ctrl Pts',(-16.9968920488552,-12.3341497286325,
116.364349421587)) ;
#184896 = CARTESIAN_POINT('Ctrl Pts',(-16.9946982815475,-12.4097302348877,
116.35766755868)) ;
#184897 = CARTESIAN_POINT('Ctrl Pts',(-16.9208944115846,-12.4097302280834,
116.381898519521)) ;
#184898 = CARTESIAN_POINT('Ctrl Pts',(-16.8470905416218,-12.409730221279,
116.406129480361)) ;
#184899 = CARTESIAN_POINT('Ctrl Pts',(-16.8492843089295,-12.3341497150238,
116.412811343268)) ;
#184900 = CARTESIAN_POINT('Ctrl Pts',(-16.8514780762372,-12.2585692087685,
116.419493206174)) ;
#184901 = CARTESIAN_POINT('Ctrl Pts',(-16.9252819462,-12.2585692155729,116.395262245333)) ;
#184902 = CARTESIAN_POINT('Ctrl Pts',(-16.9990858161628,-12.2585692223772,
116.371031284493)) ;
#184903 = CARTESIAN_POINT('Ctrl Pts',(-16.9968920488552,-12.3341497286325,
116.364349421587)) ;
#184904 = CARTESIAN_POINT('Ctrl Pts',(-16.8955934699839,-12.3478638226298,
116.091294655271)) ;
#184905 = CARTESIAN_POINT('Ctrl Pts',(-16.89973469377,-12.4226010423524,116.103908153229)) ;
#184906 = CARTESIAN_POINT('Ctrl Pts',(-16.8259308264129,-12.4226010571477,
116.128139122006)) ;
#184907 = CARTESIAN_POINT('Ctrl Pts',(-16.7521269590558,-12.422601071943,
116.152370090783)) ;
#184908 = CARTESIAN_POINT('Ctrl Pts',(-16.7479857352698,-12.3478638522204,
116.139756592826)) ;
#184909 = CARTESIAN_POINT('Ctrl Pts',(-16.7438445114837,-12.2731266324978,
116.127143094869)) ;
#184910 = CARTESIAN_POINT('Ctrl Pts',(-16.8176483788408,-12.2731266177025,
116.102912126092)) ;
#184911 = CARTESIAN_POINT('Ctrl Pts',(-16.8914522461979,-12.2731266029072,
116.078681157314)) ;
#184912 = CARTESIAN_POINT('Ctrl Pts',(-16.8955934699839,-12.3478638226298,
116.091294655271)) ;
#184913 = CARTESIAN_POINT('Ctrl Pts',(-16.7987277286322,-12.4382992209291,
115.831728050634)) ;
#184914 = CARTESIAN_POINT('Ctrl Pts',(-16.8089043705112,-12.5068353759983,
115.862724458441)) ;
#184915 = CARTESIAN_POINT('Ctrl Pts',(-16.7351005074183,-12.5068354072617,
115.886955440206)) ;
#184916 = CARTESIAN_POINT('Ctrl Pts',(-16.6612966443254,-12.5068354385251,
115.911186421972)) ;
#184917 = CARTESIAN_POINT('Ctrl Pts',(-16.6511200024464,-12.4382992834559,
115.880190014164)) ;
#184918 = CARTESIAN_POINT('Ctrl Pts',(-16.6409433605675,-12.3697631283867,
115.849193606357)) ;
#184919 = CARTESIAN_POINT('Ctrl Pts',(-16.7147472236604,-12.3697630971233,
115.824962624592)) ;
#184920 = CARTESIAN_POINT('Ctrl Pts',(-16.7885510867532,-12.3697630658599,
115.800731642826)) ;
#184921 = CARTESIAN_POINT('Ctrl Pts',(-16.7987277286322,-12.4382992209291,
115.831728050634)) ;
#184922 = CARTESIAN_POINT('Ctrl Pts',(-16.7125017303928,-12.5986984925073,
115.604533974206)) ;
#184923 = CARTESIAN_POINT('Ctrl Pts',(-16.7279808214323,-12.6561393028317,
115.651680786763)) ;
#184924 = CARTESIAN_POINT('Ctrl Pts',(-16.654176963508,-12.65613934453,115.675911784271)) ;
#184925 = CARTESIAN_POINT('Ctrl Pts',(-16.5803731055837,-12.6561393862282,
115.700142781779)) ;
#184926 = CARTESIAN_POINT('Ctrl Pts',(-16.5648940145443,-12.5986985759038,
115.652995969222)) ;
#184927 = CARTESIAN_POINT('Ctrl Pts',(-16.5494149235048,-12.5412577655794,
115.605849156666)) ;
#184928 = CARTESIAN_POINT('Ctrl Pts',(-16.6232187814291,-12.5412577238812,
115.581618159158)) ;
#184929 = CARTESIAN_POINT('Ctrl Pts',(-16.6970226393534,-12.541257682183,
115.557387161649)) ;
#184930 = CARTESIAN_POINT('Ctrl Pts',(-16.7125017303928,-12.5986984925073,
115.604533974206)) ;
#184931 = CARTESIAN_POINT('Ctrl Pts',(-16.6421521442805,-12.8181589219149,
115.425759855238)) ;
#184932 = CARTESIAN_POINT('Ctrl Pts',(-16.6618320255675,-12.8603639864266,
115.485701597265)) ;
#184933 = CARTESIAN_POINT('Ctrl Pts',(-16.5880281731401,-12.8603640315663,
115.509932611516)) ;
#184934 = CARTESIAN_POINT('Ctrl Pts',(-16.5142243207128,-12.8603640767059,
115.534163625767)) ;
#184935 = CARTESIAN_POINT('Ctrl Pts',(-16.4945444394258,-12.8181590121942,
115.47422188374)) ;
#184936 = CARTESIAN_POINT('Ctrl Pts',(-16.4748645581388,-12.7759539476825,
115.414280141713)) ;
#184937 = CARTESIAN_POINT('Ctrl Pts',(-16.5486684105661,-12.7759539025429,
115.390049127462)) ;
#184938 = CARTESIAN_POINT('Ctrl Pts',(-16.6224722629935,-12.7759538574032,
115.365818113211)) ;
#184939 = CARTESIAN_POINT('Ctrl Pts',(-16.6421521442805,-12.8181589219149,
115.425759855238)) ;
#184940 = CARTESIAN_POINT('Ctrl Pts',(-16.5922545474962,-13.0797516616193,
115.309162122654)) ;
#184941 = CARTESIAN_POINT('Ctrl Pts',(-16.6147159819925,-13.1037557901174,
115.377576027107)) ;
#184942 = CARTESIAN_POINT('Ctrl Pts',(-16.5409121343667,-13.1037558337794,
115.401807055983)) ;
#184943 = CARTESIAN_POINT('Ctrl Pts',(-16.4671082867409,-13.1037558774415,
115.426038084858)) ;
#184944 = CARTESIAN_POINT('Ctrl Pts',(-16.4446468522446,-13.0797517489434,
115.357624180405)) ;
#184945 = CARTESIAN_POINT('Ctrl Pts',(-16.4221854177483,-13.0557476204452,
115.289210275952)) ;
#184946 = CARTESIAN_POINT('Ctrl Pts',(-16.4959892653741,-13.0557475767832,
115.264979247076)) ;
#184947 = CARTESIAN_POINT('Ctrl Pts',(-16.5697931129999,-13.0557475331212,
115.2407482182)) ;
#184948 = CARTESIAN_POINT('Ctrl Pts',(-16.5922545474962,-13.0797516616193,
115.309162122654)) ;
#184949 = CARTESIAN_POINT('Ctrl Pts',(-16.5652750102249,-13.3661182947965,
115.262452316505)) ;
#184950 = CARTESIAN_POINT('Ctrl Pts',(-16.5889203991877,-13.3701640997913,
115.334472355401)) ;
#184951 = CARTESIAN_POINT('Ctrl Pts',(-16.5151165554926,-13.3701641367874,
115.358703396249)) ;
#184952 = CARTESIAN_POINT('Ctrl Pts',(-16.4413127117975,-13.3701641737835,
115.382934437097)) ;
#184953 = CARTESIAN_POINT('Ctrl Pts',(-16.4176673228348,-13.3661183687887,
115.310914398201)) ;
#184954 = CARTESIAN_POINT('Ctrl Pts',(-16.394021933872,-13.3620725637939,
115.238894359305)) ;
#184955 = CARTESIAN_POINT('Ctrl Pts',(-16.4678257775671,-13.3620725267978,
115.214663318457)) ;
#184956 = CARTESIAN_POINT('Ctrl Pts',(-16.5416296212622,-13.3620724898017,
115.190432277609)) ;
#184957 = CARTESIAN_POINT('Ctrl Pts',(-16.5652750102249,-13.3661182947965,
115.262452316505)) ;
#184958 = CARTESIAN_POINT('Ctrl Pts',(-16.5626467913676,-13.656951267572,
115.290002450311)) ;
#184959 = CARTESIAN_POINT('Ctrl Pts',(-16.5857758666926,-13.6406962235438,
115.360449881353)) ;
#184960 = CARTESIAN_POINT('Ctrl Pts',(-16.5119720254153,-13.6406962503813,
115.384680929566)) ;
#184961 = CARTESIAN_POINT('Ctrl Pts',(-16.438168184138,-13.6406962772189,
115.408911977778)) ;
#184962 = CARTESIAN_POINT('Ctrl Pts',(-16.4150391088129,-13.6569513212471,
115.338464546735)) ;
#184963 = CARTESIAN_POINT('Ctrl Pts',(-16.3919100334878,-13.6732063652754,
115.268017115692)) ;
#184964 = CARTESIAN_POINT('Ctrl Pts',(-16.4657138747652,-13.6732063384378,
115.24378606748)) ;
#184965 = CARTESIAN_POINT('Ctrl Pts',(-16.5395177160425,-13.6732063116003,
115.219555019268)) ;
#184966 = CARTESIAN_POINT('Ctrl Pts',(-16.5626467913676,-13.656951267572,
115.290002450311)) ;
#184967 = CARTESIAN_POINT('Ctrl Pts',(-16.5837488475447,-13.9296721739865,
115.389708810494)) ;
#184968 = CARTESIAN_POINT('Ctrl Pts',(-16.6047062406092,-13.8943500486195,
115.453541647919)) ;
#184969 = CARTESIAN_POINT('Ctrl Pts',(-16.5309024003191,-13.8943500659771,
115.477772699138)) ;
#184970 = CARTESIAN_POINT('Ctrl Pts',(-16.457098560029,-13.8943500833347,
115.502003750357)) ;
#184971 = CARTESIAN_POINT('Ctrl Pts',(-16.4361411669645,-13.9296722087017,
115.438170912932)) ;
#184972 = CARTESIAN_POINT('Ctrl Pts',(-16.4151837738999,-13.9649943340687,
115.374338075508)) ;
#184973 = CARTESIAN_POINT('Ctrl Pts',(-16.48898761419,-13.9649943167111,115.350107024289)) ;
#184974 = CARTESIAN_POINT('Ctrl Pts',(-16.5627914544801,-13.9649942993535,
115.32587597307)) ;
#184975 = CARTESIAN_POINT('Ctrl Pts',(-16.5837488475447,-13.9296721739865,
115.389708810494)) ;
#184976 = CARTESIAN_POINT('Ctrl Pts',(-16.6262908326384,-14.1660389555352,
115.554751277984)) ;
#184977 = CARTESIAN_POINT('Ctrl Pts',(-16.6435754639849,-14.1141591424512,
115.607397475954)) ;
#184978 = CARTESIAN_POINT('Ctrl Pts',(-16.569771623452,-14.114159151286,115.631628526433)) ;
#184979 = CARTESIAN_POINT('Ctrl Pts',(-16.495967782919,-14.1141591601208,
115.655859576913)) ;
#184980 = CARTESIAN_POINT('Ctrl Pts',(-16.4786831515725,-14.1660389732048,
115.603213378943)) ;
#184981 = CARTESIAN_POINT('Ctrl Pts',(-16.461398520226,-14.2179187862889,
115.550567180973)) ;
#184982 = CARTESIAN_POINT('Ctrl Pts',(-16.535202360759,-14.2179187774541,
115.526336130494)) ;
#184983 = CARTESIAN_POINT('Ctrl Pts',(-16.609006201292,-14.2179187686193,
115.502105080014)) ;
#184984 = CARTESIAN_POINT('Ctrl Pts',(-16.6262908326384,-14.1660389555352,
115.554751277984)) ;
#184985 = CARTESIAN_POINT('Ctrl Pts',(-16.6865043266641,-14.3487828478669,
115.773619369682)) ;
#184986 = CARTESIAN_POINT('Ctrl Pts',(-16.6988765648799,-14.2840645582721,
115.811303210909)) ;
#184987 = CARTESIAN_POINT('Ctrl Pts',(-16.625072723286,-14.2840645612063,
115.835534258157)) ;
#184988 = CARTESIAN_POINT('Ctrl Pts',(-16.5512688816921,-14.2840645641405,
115.859765305405)) ;
#184989 = CARTESIAN_POINT('Ctrl Pts',(-16.5388966434763,-14.3487828537354,
115.822081464178)) ;
#184990 = CARTESIAN_POINT('Ctrl Pts',(-16.5265244052603,-14.4135011433302,
115.784397622951)) ;
#184991 = CARTESIAN_POINT('Ctrl Pts',(-16.6003282468543,-14.413501140396,
115.760166575704)) ;
#184992 = CARTESIAN_POINT('Ctrl Pts',(-16.6741320884482,-14.4135011374618,
115.735935528456)) ;
#184993 = CARTESIAN_POINT('Ctrl Pts',(-16.6865043266641,-14.3487828478669,
115.773619369682)) ;
#184994 = CARTESIAN_POINT('Ctrl Pts',(-16.7592456254264,-14.4648357931477,
116.030618712201)) ;
#184995 = CARTESIAN_POINT('Ctrl Pts',(-16.7658237132317,-14.391916747365,
116.050654506254)) ;
#184996 = CARTESIAN_POINT('Ctrl Pts',(-16.6920198703368,-14.3919167474485,
116.074885549539)) ;
#184997 = CARTESIAN_POINT('Ctrl Pts',(-16.6182160274419,-14.391916747532,
116.099116592824)) ;
#184998 = CARTESIAN_POINT('Ctrl Pts',(-16.6116379396366,-14.4648357933146,
116.079080798771)) ;
#184999 = CARTESIAN_POINT('Ctrl Pts',(-16.6050598518314,-14.5377548390973,
116.059045004718)) ;
#185000 = CARTESIAN_POINT('Ctrl Pts',(-16.6788636947263,-14.5377548390138,
116.034813961433)) ;
#185001 = CARTESIAN_POINT('Ctrl Pts',(-16.7526675376212,-14.5377548389303,
116.010582918148)) ;
#185002 = CARTESIAN_POINT('Ctrl Pts',(-16.7592456254264,-14.4648357931477,
116.030618712201)) ;
#185003 = CARTESIAN_POINT('Ctrl Pts',(-16.8386665689219,-14.5058959818021,
116.307994675603)) ;
#185004 = CARTESIAN_POINT('Ctrl Pts',(-16.8389745832277,-14.4300007264442,
116.308932837514)) ;
#185005 = CARTESIAN_POINT('Ctrl Pts',(-16.7651707392682,-14.4300007261889,
116.333163877557)) ;
#185006 = CARTESIAN_POINT('Ctrl Pts',(-16.6913668953086,-14.4300007259336,
116.357394917599)) ;
#185007 = CARTESIAN_POINT('Ctrl Pts',(-16.6910588810028,-14.5058959812914,
116.356456755687)) ;
#185008 = CARTESIAN_POINT('Ctrl Pts',(-16.690750866697,-14.5817912366492,
116.355518593776)) ;
#185009 = CARTESIAN_POINT('Ctrl Pts',(-16.7645547106565,-14.5817912369046,
116.331287553734)) ;
#185010 = CARTESIAN_POINT('Ctrl Pts',(-16.8383585546161,-14.5817912371599,
116.307056513691)) ;
#185011 = CARTESIAN_POINT('Ctrl Pts',(-16.8386665689219,-14.5058959818021,
116.307994675603)) ;
#185012 = CARTESIAN_POINT('Ctrl Pts',(-16.9180971410873,-14.4694242942484,
116.585309225375)) ;
#185013 = CARTESIAN_POINT('Ctrl Pts',(-16.9121269062051,-14.3959630196689,
116.567124853285)) ;
#185014 = CARTESIAN_POINT('Ctrl Pts',(-16.8383230617492,-14.3959630205436,
116.591355891816)) ;
#185015 = CARTESIAN_POINT('Ctrl Pts',(-16.7645192172934,-14.3959630214183,
116.615586930346)) ;
#185016 = CARTESIAN_POINT('Ctrl Pts',(-16.7704894521756,-14.4694242959978,
116.633771302437)) ;
#185017 = CARTESIAN_POINT('Ctrl Pts',(-16.7764596870578,-14.5428855705773,
116.651955674527)) ;
#185018 = CARTESIAN_POINT('Ctrl Pts',(-16.8502635315136,-14.5428855697026,
116.627724635996)) ;
#185019 = CARTESIAN_POINT('Ctrl Pts',(-16.9240673759695,-14.542885568828,
116.603493597466)) ;
#185020 = CARTESIAN_POINT('Ctrl Pts',(-16.9180971410873,-14.4694242942484,
116.585309225375)) ;
#185021 = CARTESIAN_POINT('Ctrl Pts',(-16.9919081234988,-14.356381751671,
116.845841056527)) ;
#185022 = CARTESIAN_POINT('Ctrl Pts',(-16.980035442802,-14.2907051755566,
116.809678786819)) ;
#185023 = CARTESIAN_POINT('Ctrl Pts',(-16.9062315987896,-14.2907051768879,
116.833909826701)) ;
#185024 = CARTESIAN_POINT('Ctrl Pts',(-16.8324277547772,-14.2907051782191,
116.858140866582)) ;
#185025 = CARTESIAN_POINT('Ctrl Pts',(-16.8443004354741,-14.3563817543336,
116.89430313629)) ;
#185026 = CARTESIAN_POINT('Ctrl Pts',(-16.8561731161709,-14.422058330448,
116.930465405997)) ;
#185027 = CARTESIAN_POINT('Ctrl Pts',(-16.9299769601833,-14.4220583291168,
116.906234366116)) ;
#185028 = CARTESIAN_POINT('Ctrl Pts',(-17.0037808041957,-14.4220583277855,
116.882003326234)) ;
#185029 = CARTESIAN_POINT('Ctrl Pts',(-16.9919081234988,-14.356381751671,
116.845841056527)) ;
#185030 = CARTESIAN_POINT('Ctrl Pts',(-17.0525352838852,-14.1778422798436,
117.06575399033)) ;
#185031 = CARTESIAN_POINT('Ctrl Pts',(-17.0356824497799,-14.1245364286659,
117.014422976839)) ;
#185032 = CARTESIAN_POINT('Ctrl Pts',(-16.9618786064408,-14.1245364288381,
117.038654018772)) ;
#185033 = CARTESIAN_POINT('Ctrl Pts',(-16.8880747631017,-14.1245364290103,
117.062885060704)) ;
#185034 = CARTESIAN_POINT('Ctrl Pts',(-16.904927597207,-14.177842280188,117.114216074195)) ;
#185035 = CARTESIAN_POINT('Ctrl Pts',(-16.9217804313123,-14.2311481313656,
117.165547087685)) ;
#185036 = CARTESIAN_POINT('Ctrl Pts',(-16.9955842746514,-14.2311481311934,
117.141316045753)) ;
#185037 = CARTESIAN_POINT('Ctrl Pts',(-17.0693881179905,-14.2311481310212,
117.117085003821)) ;
#185038 = CARTESIAN_POINT('Ctrl Pts',(-17.0525352838852,-14.1778422798436,
117.06575399033)) ;
#185039 = CARTESIAN_POINT('Ctrl Pts',(-17.0962610112578,-13.9441247450056,
117.234417675053)) ;
#185040 = CARTESIAN_POINT('Ctrl Pts',(-17.0755960229063,-13.9070603957443,
117.171475454734)) ;
#185041 = CARTESIAN_POINT('Ctrl Pts',(-17.0017921802879,-13.9070603921811,
117.195706498861)) ;
#185042 = CARTESIAN_POINT('Ctrl Pts',(-16.9279883376695,-13.9070603886178,
117.219937542989)) ;
#185043 = CARTESIAN_POINT('Ctrl Pts',(-16.948653326021,-13.9441247378791,
117.282879763307)) ;
#185044 = CARTESIAN_POINT('Ctrl Pts',(-16.9693183143724,-13.9811890871404,
117.345821983626)) ;
#185045 = CARTESIAN_POINT('Ctrl Pts',(-17.0431221569908,-13.9811890907036,
117.321590939499)) ;
#185046 = CARTESIAN_POINT('Ctrl Pts',(-17.1169259996092,-13.9811890942669,
117.297359895372)) ;
#185047 = CARTESIAN_POINT('Ctrl Pts',(-17.0962610112578,-13.9441247450056,
117.234417675053)) ;
#185048 = CARTESIAN_POINT('Ctrl Pts',(-17.1185983352745,-13.6724643503177,
117.337941114439)) ;
#185049 = CARTESIAN_POINT('Ctrl Pts',(-17.0956091461605,-13.6543146170461,
117.267919753489)) ;
#185050 = CARTESIAN_POINT('Ctrl Pts',(-17.021805303656,-13.6543146070783,
117.292150797963)) ;
#185051 = CARTESIAN_POINT('Ctrl Pts',(-16.9480014611515,-13.6543145971105,
117.316381842438)) ;
#185052 = CARTESIAN_POINT('Ctrl Pts',(-16.9709906502654,-13.6724643303821,
117.386403203388)) ;
#185053 = CARTESIAN_POINT('Ctrl Pts',(-16.9939798393793,-13.6906140636538,
117.456424564338)) ;
#185054 = CARTESIAN_POINT('Ctrl Pts',(-17.0677836818839,-13.6906140736215,
117.432193519863)) ;
#185055 = CARTESIAN_POINT('Ctrl Pts',(-17.1415875243884,-13.6906140835893,
117.407962475389)) ;
#185056 = CARTESIAN_POINT('Ctrl Pts',(-17.1185983352745,-13.6724643503177,
117.337941114439)) ;
#185057 = CARTESIAN_POINT('Ctrl Pts',(-17.117418789511,-13.3835337156027,
117.369720038339)) ;
#185058 = CARTESIAN_POINT('Ctrl Pts',(-17.0937466861375,-13.3855315872837,
117.297618630625)) ;
#185059 = CARTESIAN_POINT('Ctrl Pts',(-17.019942842807,-13.3855315707962,
117.321849672584)) ;
#185060 = CARTESIAN_POINT('Ctrl Pts',(-16.9461389994764,-13.3855315543086,
117.346080714542)) ;
#185061 = CARTESIAN_POINT('Ctrl Pts',(-16.96981110285,-13.3835336826277,117.418182122256)) ;
#185062 = CARTESIAN_POINT('Ctrl Pts',(-16.9934832062235,-13.3815358109467,
117.49028352997)) ;
#185063 = CARTESIAN_POINT('Ctrl Pts',(-17.067287049554,-13.3815358274342,
117.466052488011)) ;
#185064 = CARTESIAN_POINT('Ctrl Pts',(-17.1410908928846,-13.3815358439218,
117.441821446053)) ;
#185065 = CARTESIAN_POINT('Ctrl Pts',(-17.117418789511,-13.3835337156027,
117.369720038339)) ;
#185066 = CARTESIAN_POINT('Ctrl Pts',(-17.0915909181535,-13.0942320536069,
117.326791158127)) ;
#185067 = CARTESIAN_POINT('Ctrl Pts',(-17.0689480758727,-13.1164328568091,
117.257824713433)) ;
#185068 = CARTESIAN_POINT('Ctrl Pts',(-16.9951442302083,-13.1164328311838,
117.282055748283)) ;
#185069 = CARTESIAN_POINT('Ctrl Pts',(-16.9213403845439,-13.1164328055585,
117.306286783133)) ;
#185070 = CARTESIAN_POINT('Ctrl Pts',(-16.9439832268247,-13.0942320023563,
117.375253227826)) ;
#185071 = CARTESIAN_POINT('Ctrl Pts',(-16.9666260691055,-13.0720311991542,
117.444219672519)) ;
#185072 = CARTESIAN_POINT('Ctrl Pts',(-17.0404299147699,-13.0720312247795,
117.419988637669)) ;
#185073 = CARTESIAN_POINT('Ctrl Pts',(-17.1142337604343,-13.0720312504048,
117.39575760282)) ;
#185074 = CARTESIAN_POINT('Ctrl Pts',(-17.0915909181535,-13.0942320536069,
117.326791158127)) ;
#185075 = CARTESIAN_POINT('Ctrl Pts',(-17.0430263168028,-12.8318300831267,
117.214118671673)) ;
#185076 = CARTESIAN_POINT('Ctrl Pts',(-17.0230123581187,-12.8723837829672,
117.153159382125)) ;
#185077 = CARTESIAN_POINT('Ctrl Pts',(-16.9492085093455,-12.8723837548031,
117.177390407506)) ;
#185078 = CARTESIAN_POINT('Ctrl Pts',(-16.8754046605723,-12.872383726639,
117.201621432886)) ;
#185079 = CARTESIAN_POINT('Ctrl Pts',(-16.8954186192564,-12.8318300267985,
117.262580722435)) ;
#185080 = CARTESIAN_POINT('Ctrl Pts',(-16.9154325779404,-12.791276326958,
117.323540011983)) ;
#185081 = CARTESIAN_POINT('Ctrl Pts',(-16.9892364267137,-12.7912763551221,
117.299308986602)) ;
#185082 = CARTESIAN_POINT('Ctrl Pts',(-17.0630402754869,-12.7912763832862,
117.275077961222)) ;
#185083 = CARTESIAN_POINT('Ctrl Pts',(-17.0430263168028,-12.8318300831267,
117.214118671673)) ;
#185084 = CARTESIAN_POINT('Ctrl Pts',(-16.9734981845306,-12.608937228869,
117.037951919378)) ;
#185085 = CARTESIAN_POINT('Ctrl Pts',(-16.957572902719,-12.6651122393528,
116.989446079685)) ;
#185086 = CARTESIAN_POINT('Ctrl Pts',(-16.8837690495209,-12.6651122100812,
117.013677091588)) ;
#185087 = CARTESIAN_POINT('Ctrl Pts',(-16.8099651963227,-12.6651121808096,
117.037908103491)) ;
#185088 = CARTESIAN_POINT('Ctrl Pts',(-16.8258904781343,-12.6089371703258,
117.086413943185)) ;
#185089 = CARTESIAN_POINT('Ctrl Pts',(-16.8418157599459,-12.5527621598419,
117.134919782878)) ;
#185090 = CARTESIAN_POINT('Ctrl Pts',(-16.9156196131441,-12.5527621891136,
117.110688770975)) ;
#185091 = CARTESIAN_POINT('Ctrl Pts',(-16.9894234663423,-12.5527622183852,
117.086457759072)) ;
#185092 = CARTESIAN_POINT('Ctrl Pts',(-16.9734981845306,-12.608937228869,
117.037951919378)) ;
#185093 = CARTESIAN_POINT('Ctrl Pts',(-16.8882820075866,-12.4456165862493,
116.813713510996)) ;
#185094 = CARTESIAN_POINT('Ctrl Pts',(-16.8775527597793,-12.5132753292444,
116.781033952363)) ;
#185095 = CARTESIAN_POINT('Ctrl Pts',(-16.8037489024639,-12.5132753061601,
116.805264951725)) ;
#185096 = CARTESIAN_POINT('Ctrl Pts',(-16.7299450451485,-12.5132752830759,
116.829495951088)) ;
#185097 = CARTESIAN_POINT('Ctrl Pts',(-16.7406742929557,-12.4456165400809,
116.862175509721)) ;
#185098 = CARTESIAN_POINT('Ctrl Pts',(-16.751403540763,-12.3779577970859,
116.894855068354)) ;
#185099 = CARTESIAN_POINT('Ctrl Pts',(-16.8252073980784,-12.3779578201701,
116.870624068992)) ;
#185100 = CARTESIAN_POINT('Ctrl Pts',(-16.8990112553938,-12.3779578432543,
116.846393069629)) ;
#185101 = CARTESIAN_POINT('Ctrl Pts',(-16.8882820075866,-12.4456165862493,
116.813713510996)) ;
#185102 = CARTESIAN_POINT('Ctrl Pts',(-16.7917570614056,-12.3507741827119,
116.555224982685)) ;
#185103 = CARTESIAN_POINT('Ctrl Pts',(-16.7870167098958,-12.4251525805178,
116.540786635693)) ;
#185104 = CARTESIAN_POINT('Ctrl Pts',(-16.713212848396,-12.425152568096,116.565017622311)) ;
#185105 = CARTESIAN_POINT('Ctrl Pts',(-16.6394089868962,-12.4251525556743,
116.589248608929)) ;
#185106 = CARTESIAN_POINT('Ctrl Pts',(-16.644149338406,-12.3507741578684,
116.603686955921)) ;
#185107 = CARTESIAN_POINT('Ctrl Pts',(-16.6488896899159,-12.2763957600624,
116.618125302913)) ;
#185108 = CARTESIAN_POINT('Ctrl Pts',(-16.7226935514157,-12.2763957724842,
116.593894316295)) ;
#185109 = CARTESIAN_POINT('Ctrl Pts',(-16.7964974129154,-12.276395784906,
116.569663329677)) ;
#185110 = CARTESIAN_POINT('Ctrl Pts',(-16.7917570614056,-12.3507741827119,
116.555224982685)) ;
#185111 = CARTESIAN_POINT('Ctrl Pts',(-16.6902172566931,-12.3329811601702,
116.281543753901)) ;
#185112 = CARTESIAN_POINT('Ctrl Pts',(-16.6918228500276,-12.4087098331506,
116.286434130807)) ;
#185113 = CARTESIAN_POINT('Ctrl Pts',(-16.6180189852007,-12.4087098375423,
116.310665107291)) ;
#185114 = CARTESIAN_POINT('Ctrl Pts',(-16.5442151203738,-12.408709841934,
116.334896083775)) ;
#185115 = CARTESIAN_POINT('Ctrl Pts',(-16.5426095270393,-12.3329811689535,
116.330005706869)) ;
#185116 = CARTESIAN_POINT('Ctrl Pts',(-16.5410039337048,-12.2572524959731,
116.325115329963)) ;
#185117 = CARTESIAN_POINT('Ctrl Pts',(-16.6148077985317,-12.2572524915815,
116.30088435348)) ;
#185118 = CARTESIAN_POINT('Ctrl Pts',(-16.6886116633586,-12.2572524871898,
116.276653376996)) ;
#185119 = CARTESIAN_POINT('Ctrl Pts',(-16.6902172566931,-12.3329811601702,
116.281543753901)) ;
#185120 = CARTESIAN_POINT('Ctrl Pts',(-16.5913515055266,-12.3924859215409,
116.015688386954)) ;
#185121 = CARTESIAN_POINT('Ctrl Pts',(-16.5991321052098,-12.4641691937461,
116.039386836745)) ;
#185122 = CARTESIAN_POINT('Ctrl Pts',(-16.5253282397077,-12.4641692182498,
116.063617811173)) ;
#185123 = CARTESIAN_POINT('Ctrl Pts',(-16.4515243742057,-12.4641692427536,
116.0878487856)) ;
#185124 = CARTESIAN_POINT('Ctrl Pts',(-16.4437437745226,-12.3924859705485,
116.064150335809)) ;
#185125 = CARTESIAN_POINT('Ctrl Pts',(-16.4359631748395,-12.3208026983433,
116.040451886018)) ;
#185126 = CARTESIAN_POINT('Ctrl Pts',(-16.5097670403415,-12.3208026738395,
116.01622091159)) ;
#185127 = CARTESIAN_POINT('Ctrl Pts',(-16.5835709058435,-12.3208026493358,
115.991989937163)) ;
#185128 = CARTESIAN_POINT('Ctrl Pts',(-16.5913515055266,-12.3924859215409,
116.015688386954)) ;
#185129 = CARTESIAN_POINT('Ctrl Pts',(-16.4999410090283,-12.5254680767671,
115.772761598066)) ;
#185130 = CARTESIAN_POINT('Ctrl Pts',(-16.513380438689,-12.5879710242858,
115.813695930772)) ;
#185131 = CARTESIAN_POINT('Ctrl Pts',(-16.4395765740198,-12.587971070974,
115.837926907736)) ;
#185132 = CARTESIAN_POINT('Ctrl Pts',(-16.3657727093505,-12.5879711176621,
115.8621578847)) ;
#185133 = CARTESIAN_POINT('Ctrl Pts',(-16.3523332796897,-12.5254681701434,
115.821223551993)) ;
#185134 = CARTESIAN_POINT('Ctrl Pts',(-16.338893850029,-12.4629652226247,
115.780289219287)) ;
#185135 = CARTESIAN_POINT('Ctrl Pts',(-16.4126977146982,-12.4629651759366,
115.756058242323)) ;
#185136 = CARTESIAN_POINT('Ctrl Pts',(-16.4865015793675,-12.4629651292484,
115.731827265359)) ;
#185137 = CARTESIAN_POINT('Ctrl Pts',(-16.4999410090283,-12.5254680767671,
115.772761598066)) ;
#185138 = CARTESIAN_POINT('Ctrl Pts',(-16.4223757171239,-12.7232333026618,
115.572077481631)) ;
#185139 = CARTESIAN_POINT('Ctrl Pts',(-16.4405141467196,-12.7720201100749,
115.627324209818)) ;
#185140 = CARTESIAN_POINT('Ctrl Pts',(-16.3667102852944,-12.7720201789256,
115.651555196663)) ;
#185141 = CARTESIAN_POINT('Ctrl Pts',(-16.2929064238692,-12.7720202477763,
115.675786183508)) ;
#185142 = CARTESIAN_POINT('Ctrl Pts',(-16.2747679942734,-12.7232334403633,
115.620539455321)) ;
#185143 = CARTESIAN_POINT('Ctrl Pts',(-16.2566295646777,-12.6744466329502,
115.565292727134)) ;
#185144 = CARTESIAN_POINT('Ctrl Pts',(-16.3304334261029,-12.6744465640995,
115.541061740289)) ;
#185145 = CARTESIAN_POINT('Ctrl Pts',(-16.4042372875281,-12.6744464952487,
115.516830753444)) ;
#185146 = CARTESIAN_POINT('Ctrl Pts',(-16.4223757171239,-12.7232333026618,
115.572077481631)) ;
#185147 = CARTESIAN_POINT('Ctrl Pts',(-16.3639160111054,-12.9691613747719,
115.429347837265)) ;
#185148 = CARTESIAN_POINT('Ctrl Pts',(-16.3854312159419,-13.0008491150667,
115.494879677901)) ;
#185149 = CARTESIAN_POINT('Ctrl Pts',(-16.3116273602281,-13.0008492011903,
115.519110682142)) ;
#185150 = CARTESIAN_POINT('Ctrl Pts',(-16.2378235045142,-13.0008492873139,
115.543341686382)) ;
#185151 = CARTESIAN_POINT('Ctrl Pts',(-16.2163082996777,-12.9691615470191,
115.477809845746)) ;
#185152 = CARTESIAN_POINT('Ctrl Pts',(-16.1947930948412,-12.9374738067243,
115.41227800511)) ;
#185153 = CARTESIAN_POINT('Ctrl Pts',(-16.268596950555,-12.9374737206007,
115.38804700087)) ;
#185154 = CARTESIAN_POINT('Ctrl Pts',(-16.3424008062689,-12.937473634477,
115.363815996629)) ;
#185155 = CARTESIAN_POINT('Ctrl Pts',(-16.3639160111054,-12.9691613747719,
115.429347837265)) ;
#185156 = CARTESIAN_POINT('Ctrl Pts',(-16.3272518685413,-13.2488218748192,
115.353233566025)) ;
#185157 = CARTESIAN_POINT('Ctrl Pts',(-16.3506225649115,-13.2610313034061,
115.424416934386)) ;
#185158 = CARTESIAN_POINT('Ctrl Pts',(-16.2768187165298,-13.2610314022195,
115.448647960959)) ;
#185159 = CARTESIAN_POINT('Ctrl Pts',(-16.203014868148,-13.2610315010329,
115.472878987532)) ;
#185160 = CARTESIAN_POINT('Ctrl Pts',(-16.1796441717778,-13.248822072446,
115.401695619171)) ;
#185161 = CARTESIAN_POINT('Ctrl Pts',(-16.1562734754075,-13.2366126438591,
115.330512250809)) ;
#185162 = CARTESIAN_POINT('Ctrl Pts',(-16.2300773237893,-13.2366125450457,
115.306281224236)) ;
#185163 = CARTESIAN_POINT('Ctrl Pts',(-16.303881172171,-13.2366124462323,
115.282050197664)) ;
#185164 = CARTESIAN_POINT('Ctrl Pts',(-16.3272518685413,-13.2488218748192,
115.353233566025)) ;
#185165 = CARTESIAN_POINT('Ctrl Pts',(-16.3147673231041,-13.5399745855604,
115.350672599282)) ;
#185166 = CARTESIAN_POINT('Ctrl Pts',(-16.3383100754923,-13.5318747593251,
115.422380022441)) ;
#185167 = CARTESIAN_POINT('Ctrl Pts',(-16.2645062356431,-13.5318748625201,
115.446611075003)) ;
#185168 = CARTESIAN_POINT('Ctrl Pts',(-16.1907023957939,-13.5318749657152,
115.470842127564)) ;
#185169 = CARTESIAN_POINT('Ctrl Pts',(-16.1671596434057,-13.5399747919505,
115.399134704405)) ;
#185170 = CARTESIAN_POINT('Ctrl Pts',(-16.1436168910174,-13.5480746181859,
115.327427281246)) ;
#185171 = CARTESIAN_POINT('Ctrl Pts',(-16.2174207308666,-13.5480745149908,
115.303196228684)) ;
#185172 = CARTESIAN_POINT('Ctrl Pts',(-16.2912245707158,-13.5480744117958,
115.278965176123)) ;
#185173 = CARTESIAN_POINT('Ctrl Pts',(-16.3147673231041,-13.5399745855604,
115.350672599282)) ;
#185174 = CARTESIAN_POINT('Ctrl Pts',(-16.3264516296071,-13.8224630035439,
115.42174671114)) ;
#185175 = CARTESIAN_POINT('Ctrl Pts',(-16.3484790098761,-13.7946290334854,
115.488838555276)) ;
#185176 = CARTESIAN_POINT('Ctrl Pts',(-16.2746751787747,-13.7946291324029,
115.513069634482)) ;
#185177 = CARTESIAN_POINT('Ctrl Pts',(-16.2008713476733,-13.7946292313203,
115.537300713688)) ;
#185178 = CARTESIAN_POINT('Ctrl Pts',(-16.1788439674043,-13.8224632013788,
115.470208869552)) ;
#185179 = CARTESIAN_POINT('Ctrl Pts',(-16.1568165871353,-13.8502971714373,
115.403117025416)) ;
#185180 = CARTESIAN_POINT('Ctrl Pts',(-16.2306204182367,-13.8502970725198,
115.378885946209)) ;
#185181 = CARTESIAN_POINT('Ctrl Pts',(-16.3044242493381,-13.8502969736024,
115.354654867003)) ;
#185182 = CARTESIAN_POINT('Ctrl Pts',(-16.3264516296071,-13.8224630035439,
115.42174671114)) ;
#185183 = CARTESIAN_POINT('Ctrl Pts',(-16.3605782808278,-14.0755037719121,
115.561087662163)) ;
#185184 = CARTESIAN_POINT('Ctrl Pts',(-16.3795230750246,-14.0299625115252,
115.618790446467)) ;
#185185 = CARTESIAN_POINT('Ctrl Pts',(-16.3057192519711,-14.0299625976229,
115.643021550186)) ;
#185186 = CARTESIAN_POINT('Ctrl Pts',(-16.2319154289175,-14.0299626837205,
115.667252653904)) ;
#185187 = CARTESIAN_POINT('Ctrl Pts',(-16.2129706347207,-14.0755039441074,
115.6095498696)) ;
#185188 = CARTESIAN_POINT('Ctrl Pts',(-16.1940258405239,-14.1210452044942,
115.551847085295)) ;
#185189 = CARTESIAN_POINT('Ctrl Pts',(-16.2678296635774,-14.1210451183966,
115.527615981577)) ;
#185190 = CARTESIAN_POINT('Ctrl Pts',(-16.3416334866309,-14.121045032299,
115.503384877858)) ;
#185191 = CARTESIAN_POINT('Ctrl Pts',(-16.3605782808278,-14.0755037719121,
115.561087662163)) ;
#185192 = CARTESIAN_POINT('Ctrl Pts',(-16.4144569396317,-14.2826234653696,
115.760827462951)) ;
#185193 = CARTESIAN_POINT('Ctrl Pts',(-16.4289310027573,-14.2225542775354,
115.804913121755)) ;
#185194 = CARTESIAN_POINT('Ctrl Pts',(-16.3551271862276,-14.2225543432862,
115.829144245344)) ;
#185195 = CARTESIAN_POINT('Ctrl Pts',(-16.2813233696978,-14.222554409037,
115.853375368933)) ;
#185196 = CARTESIAN_POINT('Ctrl Pts',(-16.2668493065721,-14.2826235968712,
115.809289710129)) ;
#185197 = CARTESIAN_POINT('Ctrl Pts',(-16.2523752434465,-14.3426927847054,
115.765204051324)) ;
#185198 = CARTESIAN_POINT('Ctrl Pts',(-16.3261790599763,-14.3426927189546,
115.740972927735)) ;
#185199 = CARTESIAN_POINT('Ctrl Pts',(-16.399982876506,-14.3426926532038,
115.716741804146)) ;
#185200 = CARTESIAN_POINT('Ctrl Pts',(-16.4144569396317,-14.2826234653696,
115.760827462951)) ;
#185201 = CARTESIAN_POINT('Ctrl Pts',(-16.4823985818851,-14.4260980932151,
116.003005069228)) ;
#185202 = CARTESIAN_POINT('Ctrl Pts',(-16.4914213499877,-14.3559233104312,
116.030486962966)) ;
#185203 = CARTESIAN_POINT('Ctrl Pts',(-16.4176175377613,-14.3559233508218,
116.054718099662)) ;
#185204 = CARTESIAN_POINT('Ctrl Pts',(-16.3438137255349,-14.3559233912124,
116.078949236359)) ;
#185205 = CARTESIAN_POINT('Ctrl Pts',(-16.3347909574323,-14.4260981739963,
116.05146734262)) ;
#185206 = CARTESIAN_POINT('Ctrl Pts',(-16.3257681893297,-14.4962729567803,
116.023985448882)) ;
#185207 = CARTESIAN_POINT('Ctrl Pts',(-16.3995720015561,-14.4962729163896,
115.999754312186)) ;
#185208 = CARTESIAN_POINT('Ctrl Pts',(-16.4733758137825,-14.496272875999,
115.975523175489)) ;
#185209 = CARTESIAN_POINT('Ctrl Pts',(-16.4823985818851,-14.4260980932151,
116.003005069228)) ;
#185210 = CARTESIAN_POINT('Ctrl Pts',(-16.5601782984998,-14.4987580687002,
116.275521075133)) ;
#185211 = CARTESIAN_POINT('Ctrl Pts',(-16.5630474354816,-14.4234055963817,
116.284260001402)) ;
#185212 = CARTESIAN_POINT('Ctrl Pts',(-16.4892436248514,-14.423405608344,
116.308491142959)) ;
#185213 = CARTESIAN_POINT('Ctrl Pts',(-16.4154398142211,-14.4234056203062,
116.332722284517)) ;
#185214 = CARTESIAN_POINT('Ctrl Pts',(-16.4125706772393,-14.4987580926247,
116.323983358248)) ;
#185215 = CARTESIAN_POINT('Ctrl Pts',(-16.4097015402575,-14.5741105649432,
116.315244431979)) ;
#185216 = CARTESIAN_POINT('Ctrl Pts',(-16.4835053508878,-14.5741105529809,
116.291013290421)) ;
#185217 = CARTESIAN_POINT('Ctrl Pts',(-16.557309161518,-14.5741105410186,
116.266782148863)) ;
#185218 = CARTESIAN_POINT('Ctrl Pts',(-16.5601782984998,-14.4987580687002,
116.275521075133)) ;
#185219 = CARTESIAN_POINT('Ctrl Pts',(-16.6403598990909,-14.4933400096758,
116.55514982289)) ;
#185220 = CARTESIAN_POINT('Ctrl Pts',(-16.636902579237,-14.4182534186233,
116.544619382463)) ;
#185221 = CARTESIAN_POINT('Ctrl Pts',(-16.5630987675235,-14.4182534027344,
116.568850520722)) ;
#185222 = CARTESIAN_POINT('Ctrl Pts',(-16.48929495581,-14.4182533868454,116.59308165898)) ;
#185223 = CARTESIAN_POINT('Ctrl Pts',(-16.4927522756639,-14.493339977898,
116.603612099407)) ;
#185224 = CARTESIAN_POINT('Ctrl Pts',(-16.4962095955177,-14.5684265689505,
116.614142539833)) ;
#185225 = CARTESIAN_POINT('Ctrl Pts',(-16.5700134072313,-14.5684265848394,
116.589911401574)) ;
#185226 = CARTESIAN_POINT('Ctrl Pts',(-16.6438172189447,-14.5684266007284,
116.565680263316)) ;
#185227 = CARTESIAN_POINT('Ctrl Pts',(-16.6403598990909,-14.4933400096758,
116.55514982289)) ;
#185228 = CARTESIAN_POINT('Ctrl Pts',(-16.716958755928,-14.4113489345642,
116.823901650034)) ;
#185229 = CARTESIAN_POINT('Ctrl Pts',(-16.7074149546365,-14.3418743538158,
116.794832769273)) ;
#185230 = CARTESIAN_POINT('Ctrl Pts',(-16.6336111393608,-14.3418743129385,
116.819063896682)) ;
#185231 = CARTESIAN_POINT('Ctrl Pts',(-16.559807324085,-14.3418742720612,
116.84329502409)) ;
#185232 = CARTESIAN_POINT('Ctrl Pts',(-16.5693511253766,-14.4113488528096,
116.872363904851)) ;
#185233 = CARTESIAN_POINT('Ctrl Pts',(-16.5788949266681,-14.4808234335579,
116.901432785613)) ;
#185234 = CARTESIAN_POINT('Ctrl Pts',(-16.6526987419438,-14.4808234744352,
116.877201658204)) ;
#185235 = CARTESIAN_POINT('Ctrl Pts',(-16.7265025572196,-14.4808235153125,
116.852970530796)) ;
#185236 = CARTESIAN_POINT('Ctrl Pts',(-16.716958755928,-14.4113489345642,
116.823901650034)) ;
#185237 = CARTESIAN_POINT('Ctrl Pts',(-16.7838983833734,-14.2570982982162,
117.06340817062)) ;
#185238 = CARTESIAN_POINT('Ctrl Pts',(-16.768929594028,-14.1982882942638,
117.017815651682)) ;
#185239 = CARTESIAN_POINT('Ctrl Pts',(-16.6951257728925,-14.1982882346942,
117.042046761243)) ;
#185240 = CARTESIAN_POINT('Ctrl Pts',(-16.6213219517571,-14.1982881751247,
117.066277870804)) ;
#185241 = CARTESIAN_POINT('Ctrl Pts',(-16.6362907411025,-14.2570981790771,
117.111870389742)) ;
#185242 = CARTESIAN_POINT('Ctrl Pts',(-16.651259530448,-14.3159081830295,
117.15746290868)) ;
#185243 = CARTESIAN_POINT('Ctrl Pts',(-16.7250633515835,-14.3159082425991,
117.133231799119)) ;
#185244 = CARTESIAN_POINT('Ctrl Pts',(-16.7988671727189,-14.3159083021687,
117.109000689558)) ;
#185245 = CARTESIAN_POINT('Ctrl Pts',(-16.7838983833734,-14.2570982982162,
117.06340817062)) ;
#185246 = CARTESIAN_POINT('Ctrl Pts',(-16.834856327063,-14.044633200838,117.25389164477)) ;
#185247 = CARTESIAN_POINT('Ctrl Pts',(-16.8155774044462,-14.000569128791,
117.195171155415)) ;
#185248 = CARTESIAN_POINT('Ctrl Pts',(-16.7417735767459,-14.0005690563028,
117.219402244981)) ;
#185249 = CARTESIAN_POINT('Ctrl Pts',(-16.6679697490455,-14.0005689838146,
117.243633334546)) ;
#185250 = CARTESIAN_POINT('Ctrl Pts',(-16.6872486716623,-14.0446330558616,
117.3023538239)) ;
#185251 = CARTESIAN_POINT('Ctrl Pts',(-16.7065275942791,-14.0886971279086,
117.361074313255)) ;
#185252 = CARTESIAN_POINT('Ctrl Pts',(-16.7803314219795,-14.0886972003968,
117.336843223689)) ;
#185253 = CARTESIAN_POINT('Ctrl Pts',(-16.8541352496798,-14.088697272885,
117.312612134124)) ;
#185254 = CARTESIAN_POINT('Ctrl Pts',(-16.834856327063,-14.044633200838,117.25389164477)) ;
#185255 = CARTESIAN_POINT('Ctrl Pts',(-16.8663296783061,-13.785410087343,
117.385342864865)) ;
#185256 = CARTESIAN_POINT('Ctrl Pts',(-16.8440877467271,-13.7593778661625,
117.31759752844)) ;
#185257 = CARTESIAN_POINT('Ctrl Pts',(-16.7702839116196,-13.7593777900464,
117.341828595444)) ;
#185258 = CARTESIAN_POINT('Ctrl Pts',(-16.6964800765121,-13.7593777139303,
117.366059662449)) ;
#185259 = CARTESIAN_POINT('Ctrl Pts',(-16.718722008091,-13.7854099351107,
117.433804998873)) ;
#185260 = CARTESIAN_POINT('Ctrl Pts',(-16.74096393967,-13.8114421562912,117.501550335298)) ;
#185261 = CARTESIAN_POINT('Ctrl Pts',(-16.8147677747775,-13.8114422324073,
117.477319268294)) ;
#185262 = CARTESIAN_POINT('Ctrl Pts',(-16.888571609885,-13.8114423085234,
117.45308820129)) ;
#185263 = CARTESIAN_POINT('Ctrl Pts',(-16.8663296783061,-13.785410087343,
117.385342864865)) ;
#185264 = CARTESIAN_POINT('Ctrl Pts',(-16.8748051062788,-13.5013707464361,
117.446525551891)) ;
#185265 = CARTESIAN_POINT('Ctrl Pts',(-16.8512060293604,-13.4951307017579,
117.374646569865)) ;
#185266 = CARTESIAN_POINT('Ctrl Pts',(-16.7774021874673,-13.4951306279953,
117.398877616201)) ;
#185267 = CARTESIAN_POINT('Ctrl Pts',(-16.7035983455741,-13.4951305542326,
117.423108662538)) ;
#185268 = CARTESIAN_POINT('Ctrl Pts',(-16.7271974224926,-13.5013705989108,
117.494987644563)) ;
#185269 = CARTESIAN_POINT('Ctrl Pts',(-16.7507964994111,-13.507610643589,
117.566866626589)) ;
#185270 = CARTESIAN_POINT('Ctrl Pts',(-16.8246003413042,-13.5076107173517,
117.542635580253)) ;
#185271 = CARTESIAN_POINT('Ctrl Pts',(-16.8984041831973,-13.5076107911143,
117.518404533917)) ;
#185272 = CARTESIAN_POINT('Ctrl Pts',(-16.8748051062788,-13.5013707464361,
117.446525551891)) ;
#185273 = CARTESIAN_POINT('Ctrl Pts',(-16.8588838729658,-13.209135818783,
117.433694846988)) ;
#185274 = CARTESIAN_POINT('Ctrl Pts',(-16.8356225305324,-13.2232901390273,
117.362844549901)) ;
#185275 = CARTESIAN_POINT('Ctrl Pts',(-16.7618186830723,-13.2232900762476,
117.387075579282)) ;
#185276 = CARTESIAN_POINT('Ctrl Pts',(-16.6880148356122,-13.2232900134679,
117.411306608662)) ;
#185277 = CARTESIAN_POINT('Ctrl Pts',(-16.7112761780455,-13.2091356932237,
117.482156905748)) ;
#185278 = CARTESIAN_POINT('Ctrl Pts',(-16.7345375204789,-13.1949813729794,
117.553007202835)) ;
#185279 = CARTESIAN_POINT('Ctrl Pts',(-16.8083413679391,-13.1949814357591,
117.528776173455)) ;
#185280 = CARTESIAN_POINT('Ctrl Pts',(-16.8821452153992,-13.1949814985388,
117.504545144075)) ;
#185281 = CARTESIAN_POINT('Ctrl Pts',(-16.8588838729658,-13.209135818783,
117.433694846988)) ;
#185282 = CARTESIAN_POINT('Ctrl Pts',(-16.8195694538494,-12.935507537228,
117.349125089638)) ;
#185283 = CARTESIAN_POINT('Ctrl Pts',(-16.7982901950563,-12.9687880563088,
117.284311899622)) ;
#185284 = CARTESIAN_POINT('Ctrl Pts',(-16.7244863433739,-12.9687880043352,
117.308542916142)) ;
#185285 = CARTESIAN_POINT('Ctrl Pts',(-16.6506824916915,-12.9687879523617,
117.332773932661)) ;
#185286 = CARTESIAN_POINT('Ctrl Pts',(-16.6719617504845,-12.9355074332809,
117.397587122678)) ;
#185287 = CARTESIAN_POINT('Ctrl Pts',(-16.6932410092776,-12.9022269142001,
117.462400312694)) ;
#185288 = CARTESIAN_POINT('Ctrl Pts',(-16.76704486096,-12.9022269661736,117.438169296175)) ;
#185289 = CARTESIAN_POINT('Ctrl Pts',(-16.8408487126425,-12.9022270181472,
117.413938279655)) ;
#185290 = CARTESIAN_POINT('Ctrl Pts',(-16.8195694538494,-12.935507537228,
117.349125089638)) ;
#185291 = CARTESIAN_POINT('Ctrl Pts',(-16.7579313251563,-12.6930981261278,
117.197023501417)) ;
#185292 = CARTESIAN_POINT('Ctrl Pts',(-16.7401858356171,-12.7433547054021,
117.142973602577)) ;
#185293 = CARTESIAN_POINT('Ctrl Pts',(-16.6663819820211,-12.7433546700873,
117.167204613268)) ;
#185294 = CARTESIAN_POINT('Ctrl Pts',(-16.5925781284251,-12.7433546347726,
117.191435623959)) ;
#185295 = CARTESIAN_POINT('Ctrl Pts',(-16.6103236179643,-12.6930980554983,
117.2454855228)) ;
#185296 = CARTESIAN_POINT('Ctrl Pts',(-16.6280691075034,-12.642841476224,
117.299535421641)) ;
#185297 = CARTESIAN_POINT('Ctrl Pts',(-16.7018729610994,-12.6428415115388,
117.27530441095)) ;
#185298 = CARTESIAN_POINT('Ctrl Pts',(-16.7756768146954,-12.6428415468535,
117.251073400258)) ;
#185299 = CARTESIAN_POINT('Ctrl Pts',(-16.7579313251563,-12.6930981261278,
117.197023501417)) ;
#185300 = CARTESIAN_POINT('Ctrl Pts',(-16.6787204475409,-12.5044954568888,
116.991078724866)) ;
#185301 = CARTESIAN_POINT('Ctrl Pts',(-16.6657479281678,-12.5679966014652,
116.951566523176)) ;
#185302 = CARTESIAN_POINT('Ctrl Pts',(-16.5919440739595,-12.5679965800268,
116.975797532002)) ;
#185303 = CARTESIAN_POINT('Ctrl Pts',(-16.5181402197511,-12.5679965585884,
117.000028540829)) ;
#185304 = CARTESIAN_POINT('Ctrl Pts',(-16.5311127391241,-12.504495414012,
117.039540742518)) ;
#185305 = CARTESIAN_POINT('Ctrl Pts',(-16.5440852584971,-12.4409942694355,
117.079052944207)) ;
#185306 = CARTESIAN_POINT('Ctrl Pts',(-16.6178891127055,-12.440994290874,
117.054821935381)) ;
#185307 = CARTESIAN_POINT('Ctrl Pts',(-16.6916929669139,-12.4409943123124,
117.030590926555)) ;
#185308 = CARTESIAN_POINT('Ctrl Pts',(-16.6787204475409,-12.5044954568888,
116.991078724866)) ;
#185309 = CARTESIAN_POINT('Ctrl Pts',(-16.5854915695396,-12.3799491141259,
116.742785488435)) ;
#185310 = CARTESIAN_POINT('Ctrl Pts',(-16.5782707497597,-12.4522433406483,
116.720792035876)) ;
#185311 = CARTESIAN_POINT('Ctrl Pts',(-16.5044668972683,-12.4522433323691,
116.745023049931)) ;
#185312 = CARTESIAN_POINT('Ctrl Pts',(-16.4306630447769,-12.4522433240898,
116.769254063987)) ;
#185313 = CARTESIAN_POINT('Ctrl Pts',(-16.4378838645568,-12.3799490975675,
116.791247516546)) ;
#185314 = CARTESIAN_POINT('Ctrl Pts',(-16.4451046843367,-12.3076548710451,
116.813240969105)) ;
#185315 = CARTESIAN_POINT('Ctrl Pts',(-16.5189085368281,-12.3076548793244,
116.789009955049)) ;
#185316 = CARTESIAN_POINT('Ctrl Pts',(-16.5927123893195,-12.3076548876036,
116.764778940994)) ;
#185317 = CARTESIAN_POINT('Ctrl Pts',(-16.5854915695396,-12.3799491141259,
116.742785488435)) ;
#185318 = CARTESIAN_POINT('Ctrl Pts',(-16.4858486944927,-12.3308555788642,
116.474611823742)) ;
#185319 = CARTESIAN_POINT('Ctrl Pts',(-16.4848434460203,-12.4066867963508,
116.471549998639)) ;
#185320 = CARTESIAN_POINT('Ctrl Pts',(-16.4110395953124,-12.4066867960904,
116.495781018126)) ;
#185321 = CARTESIAN_POINT('Ctrl Pts',(-16.3372357446044,-12.4066867958299,
116.520012037614)) ;
#185322 = CARTESIAN_POINT('Ctrl Pts',(-16.3382409930768,-12.3308555783432,
116.523073862718)) ;
#185323 = CARTESIAN_POINT('Ctrl Pts',(-16.3392462415492,-12.2550243608565,
116.526135687821)) ;
#185324 = CARTESIAN_POINT('Ctrl Pts',(-16.4130500922572,-12.255024361117,
116.501904668333)) ;
#185325 = CARTESIAN_POINT('Ctrl Pts',(-16.4868539429651,-12.2550243613775,
116.477673648845)) ;
#185326 = CARTESIAN_POINT('Ctrl Pts',(-16.4858486944927,-12.3308555788642,
116.474611823742)) ;
#185327 = CARTESIAN_POINT('Ctrl Pts',(-16.3849423803949,-12.3590358220882,
116.202733804349)) ;
#185328 = CARTESIAN_POINT('Ctrl Pts',(-16.3902473975342,-12.4330140750954,
116.218892030289)) ;
#185329 = CARTESIAN_POINT('Ctrl Pts',(-16.3164435493756,-12.4330140793916,
116.243123057542)) ;
#185330 = CARTESIAN_POINT('Ctrl Pts',(-16.242639701217,-12.4330140836878,
116.267354084794)) ;
#185331 = CARTESIAN_POINT('Ctrl Pts',(-16.2373346840777,-12.3590358306806,
116.251195858855)) ;
#185332 = CARTESIAN_POINT('Ctrl Pts',(-16.2320296669384,-12.2850575776733,
116.235037632915)) ;
#185333 = CARTESIAN_POINT('Ctrl Pts',(-16.305833515097,-12.2850575733772,
116.210806605662)) ;
#185334 = CARTESIAN_POINT('Ctrl Pts',(-16.3796373632556,-12.285057569081,
116.186575578409)) ;
#185335 = CARTESIAN_POINT('Ctrl Pts',(-16.3849423803949,-12.3590358220882,
116.202733804349)) ;
#185336 = CARTESIAN_POINT('Ctrl Pts',(-16.2895213068132,-12.4632787296656,
115.947588740383)) ;
#185337 = CARTESIAN_POINT('Ctrl Pts',(-16.3007626967771,-12.5300899100408,
115.981828200251)) ;
#185338 = CARTESIAN_POINT('Ctrl Pts',(-16.2269588510408,-12.5300899147854,
116.006059234882)) ;
#185339 = CARTESIAN_POINT('Ctrl Pts',(-16.1531550053045,-12.5300899195299,
116.030290269513)) ;
#185340 = CARTESIAN_POINT('Ctrl Pts',(-16.1419136153406,-12.4632787391547,
115.996050809645)) ;
#185341 = CARTESIAN_POINT('Ctrl Pts',(-16.1306722253766,-12.3964675587795,
115.961811349777)) ;
#185342 = CARTESIAN_POINT('Ctrl Pts',(-16.2044760711129,-12.396467554035,
115.937580315146)) ;
#185343 = CARTESIAN_POINT('Ctrl Pts',(-16.2782799168492,-12.3964675492904,
115.913349280515)) ;
#185344 = CARTESIAN_POINT('Ctrl Pts',(-16.2895213068132,-12.4632787296656,
115.947588740383)) ;
#185345 = CARTESIAN_POINT('Ctrl Pts',(-16.205735751125,-12.6363587431469,
115.727927057703)) ;
#185346 = CARTESIAN_POINT('Ctrl Pts',(-16.2221091925139,-12.6911848598895,
115.77779791827)) ;
#185347 = CARTESIAN_POINT('Ctrl Pts',(-16.1483053485157,-12.6911848623011,
115.802028958194)) ;
#185348 = CARTESIAN_POINT('Ctrl Pts',(-16.0745015045173,-12.6911848647128,
115.826259998119)) ;
#185349 = CARTESIAN_POINT('Ctrl Pts',(-16.0581280631284,-12.6363587479702,
115.776389137552)) ;
#185350 = CARTESIAN_POINT('Ctrl Pts',(-16.0417546217395,-12.5815326312277,
115.726518276985)) ;
#185351 = CARTESIAN_POINT('Ctrl Pts',(-16.1155584657378,-12.5815326288161,
115.70228723706)) ;
#185352 = CARTESIAN_POINT('Ctrl Pts',(-16.1893623097361,-12.5815326264044,
115.678056197136)) ;
#185353 = CARTESIAN_POINT('Ctrl Pts',(-16.205735751125,-12.6363587431469,
115.727927057703)) ;
#185354 = CARTESIAN_POINT('Ctrl Pts',(-16.139154962057,-12.864158222785,115.560475584254)) ;
#185355 = CARTESIAN_POINT('Ctrl Pts',(-16.1594705534534,-12.9031598637825,
115.622353597751)) ;
#185356 = CARTESIAN_POINT('Ctrl Pts',(-16.0856667102229,-12.9031598633717,
115.646584640014)) ;
#185357 = CARTESIAN_POINT('Ctrl Pts',(-16.0118628669925,-12.9031598629608,
115.670815682277)) ;
#185358 = CARTESIAN_POINT('Ctrl Pts',(-15.9915472755961,-12.8641582219634,
115.60893766878)) ;
#185359 = CARTESIAN_POINT('Ctrl Pts',(-15.9712316841997,-12.8251565809659,
115.547059655283)) ;
#185360 = CARTESIAN_POINT('Ctrl Pts',(-16.0450355274302,-12.8251565813767,
115.52282861302)) ;
#185361 = CARTESIAN_POINT('Ctrl Pts',(-16.1188393706606,-12.8251565817875,
115.498597570757)) ;
#185362 = CARTESIAN_POINT('Ctrl Pts',(-16.139154962057,-12.864158222785,115.560475584254)) ;
#185363 = CARTESIAN_POINT('Ctrl Pts',(-16.0930899176048,-13.1343225359667,
115.455877741141)) ;
#185364 = CARTESIAN_POINT('Ctrl Pts',(-16.1159137349886,-13.1545167875365,
115.525395406345)) ;
#185365 = CARTESIAN_POINT('Ctrl Pts',(-16.0421098918826,-13.1545167844315,
115.549626448987)) ;
#185366 = CARTESIAN_POINT('Ctrl Pts',(-15.9683060487766,-13.1545167813264,
115.57385749163)) ;
#185367 = CARTESIAN_POINT('Ctrl Pts',(-15.9454822313929,-13.1343225297566,
115.504339826425)) ;
#185368 = CARTESIAN_POINT('Ctrl Pts',(-15.9226584140091,-13.1141282781868,
115.434822161221)) ;
#185369 = CARTESIAN_POINT('Ctrl Pts',(-15.9964622571151,-13.1141282812919,
115.410591118579)) ;
#185370 = CARTESIAN_POINT('Ctrl Pts',(-16.0702661002211,-13.114128284397,
115.386360075936)) ;
#185371 = CARTESIAN_POINT('Ctrl Pts',(-16.0930899176048,-13.1343225359667,
115.455877741141)) ;
#185372 = CARTESIAN_POINT('Ctrl Pts',(-16.0709494733631,-13.4205967944479,
115.423599773257)) ;
#185373 = CARTESIAN_POINT('Ctrl Pts',(-16.094625220264,-13.4208311388444,
115.495712278311)) ;
#185374 = CARTESIAN_POINT('Ctrl Pts',(-16.0208213768168,-13.4208311356135,
115.519943319914)) ;
#185375 = CARTESIAN_POINT('Ctrl Pts',(-15.9470175333695,-13.4208311323827,
115.544174361517)) ;
#185376 = CARTESIAN_POINT('Ctrl Pts',(-15.9233417864687,-13.4205967879863,
115.472061856462)) ;
#185377 = CARTESIAN_POINT('Ctrl Pts',(-15.8996660395678,-13.4203624435898,
115.399949351408)) ;
#185378 = CARTESIAN_POINT('Ctrl Pts',(-15.9734698830151,-13.4203624468207,
115.375718309805)) ;
#185379 = CARTESIAN_POINT('Ctrl Pts',(-16.0472737264623,-13.4203624500515,
115.351487268202)) ;
#185380 = CARTESIAN_POINT('Ctrl Pts',(-16.0709494733631,-13.4205967944479,
115.423599773257)) ;
#185381 = CARTESIAN_POINT('Ctrl Pts',(-16.0728139419201,-13.7102521447362,
115.464896490808)) ;
#185382 = CARTESIAN_POINT('Ctrl Pts',(-16.0956574052163,-13.6902603542672,
115.534473994251)) ;
#185383 = CARTESIAN_POINT('Ctrl Pts',(-16.021853561637,-13.6902603532413,
115.558705035452)) ;
#185384 = CARTESIAN_POINT('Ctrl Pts',(-15.9480497180577,-13.6902603522153,
115.582936076653)) ;
#185385 = CARTESIAN_POINT('Ctrl Pts',(-15.9252062547615,-13.7102521426842,
115.51335857321)) ;
#185386 = CARTESIAN_POINT('Ctrl Pts',(-15.9023627914653,-13.7302439331532,
115.443781069767)) ;
#185387 = CARTESIAN_POINT('Ctrl Pts',(-15.9761666350445,-13.7302439341791,
115.419550028566)) ;
#185388 = CARTESIAN_POINT('Ctrl Pts',(-16.0499704786238,-13.7302439352051,
115.395318987366)) ;
#185389 = CARTESIAN_POINT('Ctrl Pts',(-16.0728139419201,-13.7102521447362,
115.464896490808)) ;
#185390 = CARTESIAN_POINT('Ctrl Pts',(-16.0981489870159,-13.9772668612757,
115.577456504473)) ;
#185391 = CARTESIAN_POINT('Ctrl Pts',(-16.1185243546186,-13.9386012749513,
115.639516586589)) ;
#185392 = CARTESIAN_POINT('Ctrl Pts',(-16.0447205114953,-13.9386012773307,
115.663747629179)) ;
#185393 = CARTESIAN_POINT('Ctrl Pts',(-15.970916668372,-13.9386012797101,
115.687978671768)) ;
#185394 = CARTESIAN_POINT('Ctrl Pts',(-15.9505413007694,-13.9772668660344,
115.625918589653)) ;
#185395 = CARTESIAN_POINT('Ctrl Pts',(-15.9301659331668,-14.0159324523587,
115.563858507537)) ;
#185396 = CARTESIAN_POINT('Ctrl Pts',(-16.0039697762901,-14.0159324499793,
115.539627464947)) ;
#185397 = CARTESIAN_POINT('Ctrl Pts',(-16.0777736194133,-14.0159324476,115.515396422358)) ;
#185398 = CARTESIAN_POINT('Ctrl Pts',(-16.0981489870159,-13.9772668612757,
115.577456504473)) ;
#185399 = CARTESIAN_POINT('Ctrl Pts',(-16.1444518589437,-14.2052355202481,
115.754036564004)) ;
#185400 = CARTESIAN_POINT('Ctrl Pts',(-16.1608882398116,-14.1505953290783,
115.804099127967)) ;
#185401 = CARTESIAN_POINT('Ctrl Pts',(-16.0870843981636,-14.1505953352011,
115.82833017505)) ;
#185402 = CARTESIAN_POINT('Ctrl Pts',(-16.0132805565157,-14.150595341324,
115.852561222133)) ;
#185403 = CARTESIAN_POINT('Ctrl Pts',(-15.9968441756478,-14.2052355324938,
115.802498658171)) ;
#185404 = CARTESIAN_POINT('Ctrl Pts',(-15.9804077947799,-14.2598757236637,
115.752436094208)) ;
#185405 = CARTESIAN_POINT('Ctrl Pts',(-16.0542116364279,-14.2598757175408,
115.728205047125)) ;
#185406 = CARTESIAN_POINT('Ctrl Pts',(-16.1280154780758,-14.259875711418,
115.703974000042)) ;
#185407 = CARTESIAN_POINT('Ctrl Pts',(-16.1444518589437,-14.2052355202481,
115.754036564004)) ;
#185408 = CARTESIAN_POINT('Ctrl Pts',(-16.2073387806654,-14.3759216033723,
115.980973148425)) ;
#185409 = CARTESIAN_POINT('Ctrl Pts',(-16.2186756236728,-14.3092842663228,
116.015503342754)) ;
#185410 = CARTESIAN_POINT('Ctrl Pts',(-16.1448717841291,-14.309284273676,
116.039734396247)) ;
#185411 = CARTESIAN_POINT('Ctrl Pts',(-16.0710679445855,-14.3092842810292,
116.06396544974)) ;
#185412 = CARTESIAN_POINT('Ctrl Pts',(-16.0597311015782,-14.3759216180787,
116.02943525541)) ;
#185413 = CARTESIAN_POINT('Ctrl Pts',(-16.0483942585708,-14.4425589551282,
115.994905061081)) ;
#185414 = CARTESIAN_POINT('Ctrl Pts',(-16.1221980981144,-14.442558947775,
115.970674007588)) ;
#185415 = CARTESIAN_POINT('Ctrl Pts',(-16.196001937658,-14.4425589404218,
115.946442954095)) ;
#185416 = CARTESIAN_POINT('Ctrl Pts',(-16.2073387806654,-14.3759216033723,
115.980973148425)) ;
#185417 = CARTESIAN_POINT('Ctrl Pts',(-16.2818319731242,-14.478404639523,
116.243331183075)) ;
#185418 = CARTESIAN_POINT('Ctrl Pts',(-16.2872500889696,-14.404515033937,
116.259833889309)) ;
#185419 = CARTESIAN_POINT('Ctrl Pts',(-16.2134462521354,-14.4045150394246,
116.284064951054)) ;
#185420 = CARTESIAN_POINT('Ctrl Pts',(-16.1396424153012,-14.4045150449122,
116.308296012799)) ;
#185421 = CARTESIAN_POINT('Ctrl Pts',(-16.1342242994558,-14.4784046504982,
116.291793306565)) ;
#185422 = CARTESIAN_POINT('Ctrl Pts',(-16.1288061836104,-14.5522942560841,
116.275290600331)) ;
#185423 = CARTESIAN_POINT('Ctrl Pts',(-16.2026100204446,-14.5522942505966,
116.251059538586)) ;
#185424 = CARTESIAN_POINT('Ctrl Pts',(-16.2764138572788,-14.552294245109,
116.226828476841)) ;
#185425 = CARTESIAN_POINT('Ctrl Pts',(-16.2818319731242,-14.478404639523,
116.243331183075)) ;
#185426 = CARTESIAN_POINT('Ctrl Pts',(-16.3616827803532,-14.505089399069,
116.521964167678)) ;
#185427 = CARTESIAN_POINT('Ctrl Pts',(-16.3608004973226,-14.4292297938268,
116.519276875353)) ;
#185428 = CARTESIAN_POINT('Ctrl Pts',(-16.2869966631093,-14.4292297934085,
116.543507945081)) ;
#185429 = CARTESIAN_POINT('Ctrl Pts',(-16.2131928288959,-14.4292297929902,
116.567739014809)) ;
#185430 = CARTESIAN_POINT('Ctrl Pts',(-16.2140751119266,-14.5050893982325,
116.570426307133)) ;
#185431 = CARTESIAN_POINT('Ctrl Pts',(-16.2149573949572,-14.5809490034747,
116.573113599458)) ;
#185432 = CARTESIAN_POINT('Ctrl Pts',(-16.2887612291705,-14.580949003893,
116.54888252973)) ;
#185433 = CARTESIAN_POINT('Ctrl Pts',(-16.3625650633839,-14.5809490043113,
116.524651460002)) ;
#185434 = CARTESIAN_POINT('Ctrl Pts',(-16.3616827803532,-14.505089399069,
116.521964167678)) ;
#185435 = CARTESIAN_POINT('Ctrl Pts',(-16.4409954196579,-14.4533114988155,
116.799196663572)) ;
#185436 = CARTESIAN_POINT('Ctrl Pts',(-16.4338362755014,-14.3809567964235,
116.777391064824)) ;
#185437 = CARTESIAN_POINT('Ctrl Pts',(-16.3600324439956,-14.3809567849074,
116.801622142798)) ;
#185438 = CARTESIAN_POINT('Ctrl Pts',(-16.2862286124899,-14.3809567733913,
116.825853220773)) ;
#185439 = CARTESIAN_POINT('Ctrl Pts',(-16.2933877566465,-14.4533114757834,
116.847658819521)) ;
#185440 = CARTESIAN_POINT('Ctrl Pts',(-16.300546900803,-14.5256661781754,
116.869464418269)) ;
#185441 = CARTESIAN_POINT('Ctrl Pts',(-16.3743507323088,-14.5256661896915,
116.845233340294)) ;
#185442 = CARTESIAN_POINT('Ctrl Pts',(-16.4481545638145,-14.5256662012075,
116.821002262319)) ;
#185443 = CARTESIAN_POINT('Ctrl Pts',(-16.4409954196579,-14.4533114988155,
116.799196663572)) ;
#185444 = CARTESIAN_POINT('Ctrl Pts',(-16.5121187619909,-14.3281114059052,
117.051140482076)) ;
#185445 = CARTESIAN_POINT('Ctrl Pts',(-16.4992528101108,-14.2643939997168,
117.011952867652)) ;
#185446 = CARTESIAN_POINT('Ctrl Pts',(-16.4254489791142,-14.26439397447,117.036183947178)) ;
#185447 = CARTESIAN_POINT('Ctrl Pts',(-16.3516451481177,-14.2643939492231,
117.060415026704)) ;
#185448 = CARTESIAN_POINT('Ctrl Pts',(-16.3645110999979,-14.3281113554114,
117.099602641127)) ;
#185449 = CARTESIAN_POINT('Ctrl Pts',(-16.377377051878,-14.3918287615997,
117.138790255551)) ;
#185450 = CARTESIAN_POINT('Ctrl Pts',(-16.4511808828745,-14.3918287868466,
117.114559176025)) ;
#185451 = CARTESIAN_POINT('Ctrl Pts',(-16.524984713871,-14.3918288120935,
117.090328096499)) ;
#185452 = CARTESIAN_POINT('Ctrl Pts',(-16.5121187619909,-14.3281114059052,
117.051140482076)) ;
#185453 = CARTESIAN_POINT('Ctrl Pts',(-16.5703367983849,-14.1371521548342,
117.263984046408)) ;
#185454 = CARTESIAN_POINT('Ctrl Pts',(-16.5526525054601,-14.0866750756418,
117.210120542421)) ;
#185455 = CARTESIAN_POINT('Ctrl Pts',(-16.4788486738412,-14.0866750338847,
117.234351620051)) ;
#185456 = CARTESIAN_POINT('Ctrl Pts',(-16.4050448422222,-14.0866749921275,
117.258582697681)) ;
#185457 = CARTESIAN_POINT('Ctrl Pts',(-16.4227291351469,-14.1371520713199,
117.312446201668)) ;
#185458 = CARTESIAN_POINT('Ctrl Pts',(-16.4404134280717,-14.1876291505123,
117.366309705655)) ;
#185459 = CARTESIAN_POINT('Ctrl Pts',(-16.5142172596906,-14.1876291922694,
117.342078628026)) ;
#185460 = CARTESIAN_POINT('Ctrl Pts',(-16.5880210913096,-14.1876292340265,
117.317847550396)) ;
#185461 = CARTESIAN_POINT('Ctrl Pts',(-16.5703367983849,-14.1371521548342,
117.263984046408)) ;
#185462 = CARTESIAN_POINT('Ctrl Pts',(-16.6101467780063,-13.8952369066383,
117.420645973384)) ;
#185463 = CARTESIAN_POINT('Ctrl Pts',(-16.588924848466,-13.8615770485299,
117.356007398908)) ;
#185464 = CARTESIAN_POINT('Ctrl Pts',(-16.5151210140409,-13.861576991076,
117.380238467991)) ;
#185465 = CARTESIAN_POINT('Ctrl Pts',(-16.4413171796157,-13.8615769336222,
117.404469537073)) ;
#185466 = CARTESIAN_POINT('Ctrl Pts',(-16.4625391091561,-13.8952367917306,
117.469108111549)) ;
#185467 = CARTESIAN_POINT('Ctrl Pts',(-16.4837610386964,-13.928896649839,
117.533746686025)) ;
#185468 = CARTESIAN_POINT('Ctrl Pts',(-16.5575648731215,-13.9288967072929,
117.509515616943)) ;
#185469 = CARTESIAN_POINT('Ctrl Pts',(-16.6313687075466,-13.9288967647467,
117.48528454786)) ;
#185470 = CARTESIAN_POINT('Ctrl Pts',(-16.6101467780063,-13.8952369066383,
117.420645973384)) ;
#185471 = CARTESIAN_POINT('Ctrl Pts',(-16.6282135641197,-13.6186018565224,
117.511169862453)) ;
#185472 = CARTESIAN_POINT('Ctrl Pts',(-16.6049650461497,-13.6042072181223,
117.440358626447)) ;
#185473 = CARTESIAN_POINT('Ctrl Pts',(-16.5311612071269,-13.6042071468649,
117.464589681526)) ;
#185474 = CARTESIAN_POINT('Ctrl Pts',(-16.4573573681042,-13.6042070756075,
117.488820736605)) ;
#185475 = CARTESIAN_POINT('Ctrl Pts',(-16.4806058860742,-13.6186017140076,
117.559631972611)) ;
#185476 = CARTESIAN_POINT('Ctrl Pts',(-16.5038544040443,-13.6329963524077,
117.630443208617)) ;
#185477 = CARTESIAN_POINT('Ctrl Pts',(-16.577658243067,-13.6329964236651,
117.606212153538)) ;
#185478 = CARTESIAN_POINT('Ctrl Pts',(-16.6514620820897,-13.6329964949225,
117.581981098459)) ;
#185479 = CARTESIAN_POINT('Ctrl Pts',(-16.6282135641197,-13.6186018565224,
117.511169862453)) ;
#185480 = CARTESIAN_POINT('Ctrl Pts',(-16.6223501381899,-13.3278430882069,
117.528769090005)) ;
#185481 = CARTESIAN_POINT('Ctrl Pts',(-16.5987435957387,-13.3337275360589,
117.456867369051)) ;
#185482 = CARTESIAN_POINT('Ctrl Pts',(-16.524939750447,-13.3337274561623,
117.481098405036)) ;
#185483 = CARTESIAN_POINT('Ctrl Pts',(-16.4511359051553,-13.3337273762658,
117.505329441021)) ;
#185484 = CARTESIAN_POINT('Ctrl Pts',(-16.4747424476065,-13.3278429284139,
117.577231161974)) ;
#185485 = CARTESIAN_POINT('Ctrl Pts',(-16.4983489900577,-13.3219584805619,
117.649132882927)) ;
#185486 = CARTESIAN_POINT('Ctrl Pts',(-16.5721528353494,-13.3219585604584,
117.624901846943)) ;
#185487 = CARTESIAN_POINT('Ctrl Pts',(-16.645956680641,-13.3219586403549,
117.600670810958)) ;
#185488 = CARTESIAN_POINT('Ctrl Pts',(-16.6223501381899,-13.3278430882069,
117.528769090005)) ;
#185489 = CARTESIAN_POINT('Ctrl Pts',(-16.5922344703617,-13.0431633993278,
117.472546786263)) ;
#185490 = CARTESIAN_POINT('Ctrl Pts',(-16.5699615140208,-13.0689317715885,
117.404706953289)) ;
#185491 = CARTESIAN_POINT('Ctrl Pts',(-16.4961576613975,-13.0689316894194,
117.428937966943)) ;
#185492 = CARTESIAN_POINT('Ctrl Pts',(-16.4223538087744,-13.0689316072503,
117.453168980598)) ;
#185493 = CARTESIAN_POINT('Ctrl Pts',(-16.4446267651153,-13.0431632349896,
117.521008813571)) ;
#185494 = CARTESIAN_POINT('Ctrl Pts',(-16.4668997214564,-13.0173948627289,
117.588848646545)) ;
#185495 = CARTESIAN_POINT('Ctrl Pts',(-16.5407035740795,-13.017394944898,
117.564617632891)) ;
#185496 = CARTESIAN_POINT('Ctrl Pts',(-16.6145074267027,-13.0173950270671,
117.540386619237)) ;
#185497 = CARTESIAN_POINT('Ctrl Pts',(-16.5922344703617,-13.0431633993278,
117.472546786263)) ;
#185498 = CARTESIAN_POINT('Ctrl Pts',(-16.5392017956511,-12.7854826732307,
117.346522184248)) ;
#185499 = CARTESIAN_POINT('Ctrl Pts',(-16.5198642813153,-12.8292789756885,
117.28762323387)) ;
#185500 = CARTESIAN_POINT('Ctrl Pts',(-16.4460604210477,-12.8292788993553,
117.311854224241)) ;
#185501 = CARTESIAN_POINT('Ctrl Pts',(-16.3722565607802,-12.8292788230221,
117.336085214612)) ;
#185502 = CARTESIAN_POINT('Ctrl Pts',(-16.3915940751159,-12.7854825205643,
117.39498416499)) ;
#185503 = CARTESIAN_POINT('Ctrl Pts',(-16.4109315894516,-12.7416862181065,
117.453883115367)) ;
#185504 = CARTESIAN_POINT('Ctrl Pts',(-16.4847354497192,-12.7416862944397,
117.429652124997)) ;
#185505 = CARTESIAN_POINT('Ctrl Pts',(-16.5585393099868,-12.7416863707729,
117.405421134626)) ;
#185506 = CARTESIAN_POINT('Ctrl Pts',(-16.5392017956511,-12.7854826732307,
117.346522184248)) ;
#185507 = CARTESIAN_POINT('Ctrl Pts',(-16.4667915995857,-12.5740916835464,
117.161296219297)) ;
#185508 = CARTESIAN_POINT('Ctrl Pts',(-16.451750503951,-12.6327102616695,
117.115483466974)) ;
#185509 = CARTESIAN_POINT('Ctrl Pts',(-16.3779466369284,-12.6327101996491,
117.13971443677)) ;
#185510 = CARTESIAN_POINT('Ctrl Pts',(-16.3041427699058,-12.6327101376288,
117.163945406566)) ;
#185511 = CARTESIAN_POINT('Ctrl Pts',(-16.3191838655404,-12.5740915595058,
117.209758158888)) ;
#185512 = CARTESIAN_POINT('Ctrl Pts',(-16.3342249611751,-12.5154729813828,
117.255570911211)) ;
#185513 = CARTESIAN_POINT('Ctrl Pts',(-16.4080288281977,-12.5154730434031,
117.231339941415)) ;
#185514 = CARTESIAN_POINT('Ctrl Pts',(-16.4818326952203,-12.5154731054234,
117.207108971619)) ;
#185515 = CARTESIAN_POINT('Ctrl Pts',(-16.4667915995857,-12.5740916835464,
117.161296219297)) ;
#185516 = CARTESIAN_POINT('Ctrl Pts',(-16.3787109405611,-12.4220262848849,
116.928516659474)) ;
#185517 = CARTESIAN_POINT('Ctrl Pts',(-16.3690627026773,-12.4913473054171,
116.89912968164)) ;
#185518 = CARTESIAN_POINT('Ctrl Pts',(-16.2952588300958,-12.49134726396,116.923360634505)) ;
#185519 = CARTESIAN_POINT('Ctrl Pts',(-16.2214549575144,-12.491347222503,
116.947591587369)) ;
#185520 = CARTESIAN_POINT('Ctrl Pts',(-16.2311031953983,-12.4220262019709,
116.976978565203)) ;
#185521 = CARTESIAN_POINT('Ctrl Pts',(-16.2407514332821,-12.3527051814387,
117.006365543037)) ;
#185522 = CARTESIAN_POINT('Ctrl Pts',(-16.3145553058636,-12.3527052228958,
116.982134590172)) ;
#185523 = CARTESIAN_POINT('Ctrl Pts',(-16.388359178445,-12.3527052643528,
116.957903637308)) ;
#185524 = CARTESIAN_POINT('Ctrl Pts',(-16.3787109405611,-12.4220262848849,
116.928516659474)) ;
#185525 = CARTESIAN_POINT('Ctrl Pts',(-16.2808900951267,-12.3415697140928,
116.666038345692)) ;
#185526 = CARTESIAN_POINT('Ctrl Pts',(-16.277323271128,-12.4166096733525,
116.655174373259)) ;
#185527 = CARTESIAN_POINT('Ctrl Pts',(-16.2035193951826,-12.4166096578571,
116.679405315878)) ;
#185528 = CARTESIAN_POINT('Ctrl Pts',(-16.1297155192372,-12.4166096423617,
116.703636258496)) ;
#185529 = CARTESIAN_POINT('Ctrl Pts',(-16.1332823432358,-12.341569683102,
116.714500230929)) ;
#185530 = CARTESIAN_POINT('Ctrl Pts',(-16.1368491672345,-12.2665297238424,
116.725364203362)) ;
#185531 = CARTESIAN_POINT('Ctrl Pts',(-16.2106530431799,-12.2665297393378,
116.701133260744)) ;
#185532 = CARTESIAN_POINT('Ctrl Pts',(-16.2844569191253,-12.2665297548332,
116.676902318125)) ;
#185533 = CARTESIAN_POINT('Ctrl Pts',(-16.2808900951267,-12.3415697140928,
116.666038345692)) ;
#185534 = CARTESIAN_POINT('Ctrl Pts',(-16.1795322882749,-12.3382226972324,
116.392792739754)) ;
#185535 = CARTESIAN_POINT('Ctrl Pts',(-16.1823026066868,-12.4136068588393,
116.40123068057)) ;
#185536 = CARTESIAN_POINT('Ctrl Pts',(-16.1084987299936,-12.413606871913,
116.425461620911)) ;
#185537 = CARTESIAN_POINT('Ctrl Pts',(-16.0346948533003,-12.4136068849868,
116.449692561251)) ;
#185538 = CARTESIAN_POINT('Ctrl Pts',(-16.0319245348884,-12.3382227233798,
116.441254620435)) ;
#185539 = CARTESIAN_POINT('Ctrl Pts',(-16.0291542164764,-12.2628385617728,
116.432816679619)) ;
#185540 = CARTESIAN_POINT('Ctrl Pts',(-16.1029580931697,-12.2628385486991,
116.408585739279)) ;
#185541 = CARTESIAN_POINT('Ctrl Pts',(-16.1767619698629,-12.2628385356254,
116.384354798938)) ;
#185542 = CARTESIAN_POINT('Ctrl Pts',(-16.1795322882749,-12.3382226972324,
116.392792739754)) ;
#185543 = CARTESIAN_POINT('Ctrl Pts',(-16.081237325198,-12.4121411260321,
116.128842285068)) ;
#185544 = CARTESIAN_POINT('Ctrl Pts',(-16.0901410081958,-12.4824758625955,
116.155961464781)) ;
#185545 = CARTESIAN_POINT('Ctrl Pts',(-16.0163371335278,-12.4824759039206,
116.18019241129)) ;
#185546 = CARTESIAN_POINT('Ctrl Pts',(-15.9425332588598,-12.4824759452457,
116.204423357799)) ;
#185547 = CARTESIAN_POINT('Ctrl Pts',(-15.933629575862,-12.4121412086823,
116.177304178087)) ;
#185548 = CARTESIAN_POINT('Ctrl Pts',(-15.9247258928641,-12.3418064721188,
116.150184998374)) ;
#185549 = CARTESIAN_POINT('Ctrl Pts',(-15.9985297675321,-12.3418064307938,
116.125954051865)) ;
#185550 = CARTESIAN_POINT('Ctrl Pts',(-16.0723336422001,-12.3418063894687,
116.101723105356)) ;
#185551 = CARTESIAN_POINT('Ctrl Pts',(-16.081237325198,-12.4121411260321,
116.128842285068)) ;
#185552 = CARTESIAN_POINT('Ctrl Pts',(-15.9921008262012,-12.5582147089023,
115.892828190481)) ;
#185553 = CARTESIAN_POINT('Ctrl Pts',(-16.0065067244686,-12.6184554167387,
115.93670623013)) ;
#185554 = CARTESIAN_POINT('Ctrl Pts',(-15.9327028544161,-12.6184554831094,
115.960937190697)) ;
#185555 = CARTESIAN_POINT('Ctrl Pts',(-15.8588989843637,-12.61845554948,115.985168151265)) ;
#185556 = CARTESIAN_POINT('Ctrl Pts',(-15.8444930860963,-12.5582148416436,
115.941290111616)) ;
#185557 = CARTESIAN_POINT('Ctrl Pts',(-15.8300871878288,-12.4979741338071,
115.897412071967)) ;
#185558 = CARTESIAN_POINT('Ctrl Pts',(-15.9038910578813,-12.4979740674365,
115.873181111399)) ;
#185559 = CARTESIAN_POINT('Ctrl Pts',(-15.9776949279337,-12.4979740010659,
115.848950150832)) ;
#185560 = CARTESIAN_POINT('Ctrl Pts',(-15.9921008262012,-12.5582147089023,
115.892828190481)) ;
#185561 = CARTESIAN_POINT('Ctrl Pts',(-15.917928987099,-12.7657436426172,
115.702363572167)) ;
#185562 = CARTESIAN_POINT('Ctrl Pts',(-15.936801184951,-12.8115849189124,
115.759845239742)) ;
#185563 = CARTESIAN_POINT('Ctrl Pts',(-15.8629973216198,-12.8115850045316,
115.784076220781)) ;
#185564 = CARTESIAN_POINT('Ctrl Pts',(-15.7891934582887,-12.8115850901508,
115.808307201821)) ;
#185565 = CARTESIAN_POINT('Ctrl Pts',(-15.7703212604367,-12.7657438138556,
115.750825534246)) ;
#185566 = CARTESIAN_POINT('Ctrl Pts',(-15.7514490625847,-12.7199025375603,
115.693343866671)) ;
#185567 = CARTESIAN_POINT('Ctrl Pts',(-15.8252529259159,-12.7199024519411,
115.669112885632)) ;
#185568 = CARTESIAN_POINT('Ctrl Pts',(-15.8990567892471,-12.7199023663219,
115.644881904592)) ;
#185569 = CARTESIAN_POINT('Ctrl Pts',(-15.917928987099,-12.7657436426172,
115.702363572167)) ;
#185570 = CARTESIAN_POINT('Ctrl Pts',(-15.8631509693549,-13.0202106019441,
115.571004295202)) ;
#185571 = CARTESIAN_POINT('Ctrl Pts',(-15.8851414927432,-13.0483542398271,
115.637983879269)) ;
#185572 = CARTESIAN_POINT('Ctrl Pts',(-15.8113376375345,-13.0483543369911,
115.662214885049)) ;
#185573 = CARTESIAN_POINT('Ctrl Pts',(-15.7375337823258,-13.0483544341551,
115.686445890828)) ;
#185574 = CARTESIAN_POINT('Ctrl Pts',(-15.7155432589375,-13.0202107962721,
115.61946630676)) ;
#185575 = CARTESIAN_POINT('Ctrl Pts',(-15.6935527355492,-12.992067158389,
115.552486722692)) ;
#185576 = CARTESIAN_POINT('Ctrl Pts',(-15.7673565907579,-12.9920670612251,
115.528255716913)) ;
#185577 = CARTESIAN_POINT('Ctrl Pts',(-15.8411604459666,-12.9920669640611,
115.504024711134)) ;
#185578 = CARTESIAN_POINT('Ctrl Pts',(-15.8631509693549,-13.0202106019441,
115.571004295202)) ;
#185579 = CARTESIAN_POINT('Ctrl Pts',(-15.8310465221303,-13.3031020545658,
115.508689927351)) ;
#185580 = CARTESIAN_POINT('Ctrl Pts',(-15.8545774432419,-13.3115371239571,
115.580361314412)) ;
#185581 = CARTESIAN_POINT('Ctrl Pts',(-15.7807735966424,-13.3115372240585,
115.604592346413)) ;
#185582 = CARTESIAN_POINT('Ctrl Pts',(-15.7069697500429,-13.3115373241599,
115.628823378414)) ;
#185583 = CARTESIAN_POINT('Ctrl Pts',(-15.6834388289312,-13.3031022547687,
115.557151991353)) ;
#185584 = CARTESIAN_POINT('Ctrl Pts',(-15.6599079078196,-13.2946671853774,
115.485480604292)) ;
#185585 = CARTESIAN_POINT('Ctrl Pts',(-15.7337117544191,-13.2946670852759,
115.461249572291)) ;
#185586 = CARTESIAN_POINT('Ctrl Pts',(-15.8075156010186,-13.2946669851745,
115.437018540289)) ;
#185587 = CARTESIAN_POINT('Ctrl Pts',(-15.8310465221303,-13.3031020545658,
115.508689927351)) ;
#185588 = CARTESIAN_POINT('Ctrl Pts',(-15.8231198539142,-13.593918747588,
115.519982474148)) ;
#185589 = CARTESIAN_POINT('Ctrl Pts',(-15.8465062326338,-13.5820623140505,
115.591213608491)) ;
#185590 = CARTESIAN_POINT('Ctrl Pts',(-15.7727023942151,-13.5820624088636,
115.61544466541)) ;
#185591 = CARTESIAN_POINT('Ctrl Pts',(-15.6988985557964,-13.5820625036768,
115.639675722329)) ;
#185592 = CARTESIAN_POINT('Ctrl Pts',(-15.6755121770768,-13.5939189372143,
115.568444587986)) ;
#185593 = CARTESIAN_POINT('Ctrl Pts',(-15.6521257983572,-13.6057753707518,
115.497213453642)) ;
#185594 = CARTESIAN_POINT('Ctrl Pts',(-15.7259296367759,-13.6057752759387,
115.472982396723)) ;
#185595 = CARTESIAN_POINT('Ctrl Pts',(-15.7997334751946,-13.6057751811255,
115.448751339805)) ;
#185596 = CARTESIAN_POINT('Ctrl Pts',(-15.8231198539142,-13.593918747588,
115.519982474148)) ;
#185597 = CARTESIAN_POINT('Ctrl Pts',(-15.8391226607634,-13.8723058564386,
115.604173660196)) ;
#185598 = CARTESIAN_POINT('Ctrl Pts',(-15.8606934004284,-13.8409951979867,
115.669874651036)) ;
#185599 = CARTESIAN_POINT('Ctrl Pts',(-15.7868895690113,-13.8409952801853,
115.694105729281)) ;
#185600 = CARTESIAN_POINT('Ctrl Pts',(-15.7130857375942,-13.8409953623839,
115.718336807525)) ;
#185601 = CARTESIAN_POINT('Ctrl Pts',(-15.6915149979293,-13.8723060208357,
115.652635816686)) ;
#185602 = CARTESIAN_POINT('Ctrl Pts',(-15.6699442582643,-13.9036166792876,
115.586934825846)) ;
#185603 = CARTESIAN_POINT('Ctrl Pts',(-15.7437480896814,-13.903616597089,
115.562703747601)) ;
#185604 = CARTESIAN_POINT('Ctrl Pts',(-15.8175519210985,-13.9036165148904,
115.538472669357)) ;
#185605 = CARTESIAN_POINT('Ctrl Pts',(-15.8391226607634,-13.8723058564386,
115.604173660196)) ;
#185606 = CARTESIAN_POINT('Ctrl Pts',(-15.8773871785258,-14.118869151071,
115.756288039499)) ;
#185607 = CARTESIAN_POINT('Ctrl Pts',(-15.8955830177552,-14.070296502829,
115.81170962829)) ;
#185608 = CARTESIAN_POINT('Ctrl Pts',(-15.8217791912897,-14.0702965663063,
115.835940721616)) ;
#185609 = CARTESIAN_POINT('Ctrl Pts',(-15.7479753648241,-14.0702966297837,
115.860171814942)) ;
#185610 = CARTESIAN_POINT('Ctrl Pts',(-15.7297795255947,-14.1188692780257,
115.804750226151)) ;
#185611 = CARTESIAN_POINT('Ctrl Pts',(-15.7115836863652,-14.1674419262677,
115.749328637361)) ;
#185612 = CARTESIAN_POINT('Ctrl Pts',(-15.7853875128308,-14.1674418627903,
115.725097544035)) ;
#185613 = CARTESIAN_POINT('Ctrl Pts',(-15.8591913392963,-14.167441799313,
115.700866450708)) ;
#185614 = CARTESIAN_POINT('Ctrl Pts',(-15.8773871785258,-14.118869151071,
115.756288039499)) ;
#185615 = CARTESIAN_POINT('Ctrl Pts',(-15.9340609590514,-14.3141618691383,
115.964310153546)) ;
#185616 = CARTESIAN_POINT('Ctrl Pts',(-15.9475947541449,-14.2518807456653,
116.005531908246)) ;
#185617 = CARTESIAN_POINT('Ctrl Pts',(-15.8737909305843,-14.2518807886643,
116.029763010421)) ;
#185618 = CARTESIAN_POINT('Ctrl Pts',(-15.7999871070237,-14.2518808316633,
116.053994112595)) ;
#185619 = CARTESIAN_POINT('Ctrl Pts',(-15.7864533119302,-14.3141619551363,
116.012772357894)) ;
#185620 = CARTESIAN_POINT('Ctrl Pts',(-15.7729195168366,-14.3764430786093,
115.971550603193)) ;
#185621 = CARTESIAN_POINT('Ctrl Pts',(-15.8467233403972,-14.3764430356103,
115.947319501019)) ;
#185622 = CARTESIAN_POINT('Ctrl Pts',(-15.9205271639579,-14.3764429926113,
115.923088398845)) ;
#185623 = CARTESIAN_POINT('Ctrl Pts',(-15.9340609590514,-14.3141618691383,
115.964310153546)) ;
#185624 = CARTESIAN_POINT('Ctrl Pts',(-16.0045560916089,-14.4456574881185,
116.214482017729)) ;
#185625 = CARTESIAN_POINT('Ctrl Pts',(-16.0124547601936,-14.3741011608773,
116.238540086457)) ;
#185626 = CARTESIAN_POINT('Ctrl Pts',(-15.9386509372217,-14.3741011828996,
116.262771190424)) ;
#185627 = CARTESIAN_POINT('Ctrl Pts',(-15.8648471142499,-14.3741012049218,
116.287002294392)) ;
#185628 = CARTESIAN_POINT('Ctrl Pts',(-15.8569484456653,-14.4456575321631,
116.262944225664)) ;
#185629 = CARTESIAN_POINT('Ctrl Pts',(-15.8490497770806,-14.5172138594043,
116.238886156936)) ;
#185630 = CARTESIAN_POINT('Ctrl Pts',(-15.9228536000524,-14.5172138373821,
116.214655052969)) ;
#185631 = CARTESIAN_POINT('Ctrl Pts',(-15.9966574230242,-14.5172138153598,
116.190423949001)) ;
#185632 = CARTESIAN_POINT('Ctrl Pts',(-16.0045560916089,-14.4456574881185,
116.214482017729)) ;
#185633 = CARTESIAN_POINT('Ctrl Pts',(-16.0830095747665,-14.5036635199146,
116.488878900793)) ;
#185634 = CARTESIAN_POINT('Ctrl Pts',(-16.0847092169098,-14.4279488253923,
116.494055735345)) ;
#185635 = CARTESIAN_POINT('Ctrl Pts',(-16.0109053925219,-14.4279488285843,
116.518286835)) ;
#185636 = CARTESIAN_POINT('Ctrl Pts',(-15.9371015681339,-14.4279488317762,
116.542517934654)) ;
#185637 = CARTESIAN_POINT('Ctrl Pts',(-15.9354019259906,-14.5036635262985,
116.537341100102)) ;
#185638 = CARTESIAN_POINT('Ctrl Pts',(-15.9337022838474,-14.5793782208208,
116.53216426555)) ;
#185639 = CARTESIAN_POINT('Ctrl Pts',(-16.0075061082353,-14.5793782176288,
116.507933165896)) ;
#185640 = CARTESIAN_POINT('Ctrl Pts',(-16.0813099326232,-14.5793782144369,
116.483702066242)) ;
#185641 = CARTESIAN_POINT('Ctrl Pts',(-16.0830095747665,-14.5036635199146,
116.488878900793)) ;
#185642 = CARTESIAN_POINT('Ctrl Pts',(-16.1633742770454,-14.4836080857303,
116.76924043046)) ;
#185643 = CARTESIAN_POINT('Ctrl Pts',(-16.1587290093675,-14.409178476904,
116.755091693632)) ;
#185644 = CARTESIAN_POINT('Ctrl Pts',(-16.0849251815922,-14.4091784657996,
116.779322782969)) ;
#185645 = CARTESIAN_POINT('Ctrl Pts',(-16.011121353817,-14.4091784546952,
116.803553872307)) ;
#185646 = CARTESIAN_POINT('Ctrl Pts',(-16.0157666214949,-14.4836080635215,
116.817702609134)) ;
#185647 = CARTESIAN_POINT('Ctrl Pts',(-16.0204118891728,-14.5580376723478,
116.831851345961)) ;
#185648 = CARTESIAN_POINT('Ctrl Pts',(-16.094215716948,-14.5580376834522,
116.807620256624)) ;
#185649 = CARTESIAN_POINT('Ctrl Pts',(-16.1680195447233,-14.5580376945566,
116.783389167287)) ;
#185650 = CARTESIAN_POINT('Ctrl Pts',(-16.1633742770454,-14.4836080857303,
116.76924043046)) ;
#185651 = CARTESIAN_POINT('Ctrl Pts',(-16.2383518880624,-14.3877127605132,
117.03295492109)) ;
#185652 = CARTESIAN_POINT('Ctrl Pts',(-16.2277331466029,-14.319866136678,
117.000611947086)) ;
#185653 = CARTESIAN_POINT('Ctrl Pts',(-16.1539293152376,-14.3198661161146,
117.024843025489)) ;
#185654 = CARTESIAN_POINT('Ctrl Pts',(-16.0801254838723,-14.3198660955512,
117.049074103891)) ;
#185655 = CARTESIAN_POINT('Ctrl Pts',(-16.0907442253319,-14.3877127193864,
117.081417077895)) ;
#185656 = CARTESIAN_POINT('Ctrl Pts',(-16.1013629667914,-14.4555593432216,
117.113760051899)) ;
#185657 = CARTESIAN_POINT('Ctrl Pts',(-16.1751667981567,-14.455559363785,
117.089528973497)) ;
#185658 = CARTESIAN_POINT('Ctrl Pts',(-16.2489706295219,-14.4555593843484,
117.065297895094)) ;
#185659 = CARTESIAN_POINT('Ctrl Pts',(-16.2383518880624,-14.3877127605132,
117.03295492109)) ;
#185660 = CARTESIAN_POINT('Ctrl Pts',(-16.3028078351628,-14.2212524561287,
117.264903394669)) ;
#185661 = CARTESIAN_POINT('Ctrl Pts',(-16.2869351807354,-14.1649252203371,
117.216557849678)) ;
#185662 = CARTESIAN_POINT('Ctrl Pts',(-16.2131313448875,-14.1649251971047,
117.240788914427)) ;
#185663 = CARTESIAN_POINT('Ctrl Pts',(-16.1393275090396,-14.1649251738723,
117.265019979176)) ;
#185664 = CARTESIAN_POINT('Ctrl Pts',(-16.155200163467,-14.2212524096639,
117.313365524167)) ;
#185665 = CARTESIAN_POINT('Ctrl Pts',(-16.1710728178944,-14.2775796454555,
117.361711069158)) ;
#185666 = CARTESIAN_POINT('Ctrl Pts',(-16.2448766537423,-14.2775796686879,
117.337480004409)) ;
#185667 = CARTESIAN_POINT('Ctrl Pts',(-16.3186804895902,-14.2775796919203,
117.31324893966)) ;
#185668 = CARTESIAN_POINT('Ctrl Pts',(-16.3028078351628,-14.2212524561287,
117.264903394669)) ;
#185669 = CARTESIAN_POINT('Ctrl Pts',(-16.3503835879466,-13.9987538981264,
117.445133843183)) ;
#185670 = CARTESIAN_POINT('Ctrl Pts',(-16.3304341319157,-13.9578771653023,
117.384371018433)) ;
#185671 = CARTESIAN_POINT('Ctrl Pts',(-16.2566302927543,-13.9578771425154,
117.408602073089)) ;
#185672 = CARTESIAN_POINT('Ctrl Pts',(-16.1828264535928,-13.9578771197285,
117.432833127746)) ;
#185673 = CARTESIAN_POINT('Ctrl Pts',(-16.2027759096237,-13.9987538525526,
117.493595952497)) ;
#185674 = CARTESIAN_POINT('Ctrl Pts',(-16.2227253656546,-14.0396305853768,
117.554358777247)) ;
#185675 = CARTESIAN_POINT('Ctrl Pts',(-16.296529204816,-14.0396306081637,
117.530127722591)) ;
#185676 = CARTESIAN_POINT('Ctrl Pts',(-16.3703330439775,-14.0396306309506,
117.505896667934)) ;
#185677 = CARTESIAN_POINT('Ctrl Pts',(-16.3503835879466,-13.9987538981264,
117.445133843183)) ;
#185678 = CARTESIAN_POINT('Ctrl Pts',(-16.3776742277473,-13.7338214529053,
117.563745231452)) ;
#185679 = CARTESIAN_POINT('Ctrl Pts',(-16.3550546145414,-13.7113815142411,
117.494849538931)) ;
#185680 = CARTESIAN_POINT('Ctrl Pts',(-16.2812507726019,-13.7113814963311,
117.519080585126)) ;
#185681 = CARTESIAN_POINT('Ctrl Pts',(-16.2074469306623,-13.7113814784212,
117.543311631321)) ;
#185682 = CARTESIAN_POINT('Ctrl Pts',(-16.2300665438682,-13.7338214170854,
117.612207323843)) ;
#185683 = CARTESIAN_POINT('Ctrl Pts',(-16.2526861570741,-13.7562613557496,
117.681103016364)) ;
#185684 = CARTESIAN_POINT('Ctrl Pts',(-16.3264899990136,-13.7562613736596,
117.656871970169)) ;
#185685 = CARTESIAN_POINT('Ctrl Pts',(-16.4002938409532,-13.7562613915695,
117.632640923974)) ;
#185686 = CARTESIAN_POINT('Ctrl Pts',(-16.3776742277473,-13.7338214529053,
117.563745231452)) ;
#185687 = CARTESIAN_POINT('Ctrl Pts',(-16.3816715029604,-13.4466916236415,
117.611342756202)) ;
#185688 = CARTESIAN_POINT('Ctrl Pts',(-16.3580056108764,-13.4442666484752,
117.539260267165)) ;
#185689 = CARTESIAN_POINT('Ctrl Pts',(-16.2842017673765,-13.4442666367421,
117.563491308608)) ;
#185690 = CARTESIAN_POINT('Ctrl Pts',(-16.2103979238767,-13.4442666250089,
117.58772235005)) ;
#185691 = CARTESIAN_POINT('Ctrl Pts',(-16.2340638159607,-13.4466916001752,
117.659804839087)) ;
#185692 = CARTESIAN_POINT('Ctrl Pts',(-16.2577297080446,-13.4491165753415,
117.731887328124)) ;
#185693 = CARTESIAN_POINT('Ctrl Pts',(-16.3315335515445,-13.4491165870746,
117.707656286682)) ;
#185694 = CARTESIAN_POINT('Ctrl Pts',(-16.4053373950444,-13.4491165988078,
117.683425245239)) ;
#185695 = CARTESIAN_POINT('Ctrl Pts',(-16.3816715029604,-13.4466916236415,
117.611342756202)) ;
#185696 = CARTESIAN_POINT('Ctrl Pts',(-16.3613250579378,-13.1565169960044,
117.584919941758)) ;
#185697 = CARTESIAN_POINT('Ctrl Pts',(-16.3383084793065,-13.1743502694123,
117.51481515686)) ;
#185698 = CARTESIAN_POINT('Ctrl Pts',(-16.2645046353523,-13.1743502645941,
117.539046196918)) ;
#185699 = CARTESIAN_POINT('Ctrl Pts',(-16.1907007913981,-13.174350259776,
117.563277236977)) ;
#185700 = CARTESIAN_POINT('Ctrl Pts',(-16.2137173700294,-13.156516986368,
117.633382021875)) ;
#185701 = CARTESIAN_POINT('Ctrl Pts',(-16.2367339486607,-13.1386837129601,
117.703486806774)) ;
#185702 = CARTESIAN_POINT('Ctrl Pts',(-16.3105377926149,-13.1386837177783,
117.679255766715)) ;
#185703 = CARTESIAN_POINT('Ctrl Pts',(-16.3843416365691,-13.1386837225965,
117.655024726656)) ;
#185704 = CARTESIAN_POINT('Ctrl Pts',(-16.3613250579378,-13.1565169960044,
117.584919941758)) ;
#185705 = CARTESIAN_POINT('Ctrl Pts',(-16.3173032833634,-12.8855146893556,
117.486337024747)) ;
#185706 = CARTESIAN_POINT('Ctrl Pts',(-16.2965914011344,-12.9222982070888,
117.423251973321)) ;
#185707 = CARTESIAN_POINT('Ctrl Pts',(-16.2227875575851,-12.9222982069282,
117.447483014612)) ;
#185708 = CARTESIAN_POINT('Ctrl Pts',(-16.1489837140357,-12.9222982067677,
117.471714055904)) ;
#185709 = CARTESIAN_POINT('Ctrl Pts',(-16.1696955962647,-12.8855146890345,
117.534799107331)) ;
#185710 = CARTESIAN_POINT('Ctrl Pts',(-16.1904074784936,-12.8487311713013,
117.597884158757)) ;
#185711 = CARTESIAN_POINT('Ctrl Pts',(-16.2642113220429,-12.8487311714619,
117.573653117466)) ;
#185712 = CARTESIAN_POINT('Ctrl Pts',(-16.3380151655923,-12.8487311716225,
117.549422076174)) ;
#185713 = CARTESIAN_POINT('Ctrl Pts',(-16.3173032833634,-12.8855146893556,
117.486337024747)) ;
#185714 = CARTESIAN_POINT('Ctrl Pts',(-16.2522540404142,-12.6534167842388,
117.323607876768)) ;
#185715 = CARTESIAN_POINT('Ctrl Pts',(-16.2353209157865,-12.7064619703102,
117.272032311344)) ;
#185716 = CARTESIAN_POINT('Ctrl Pts',(-16.1615170728299,-12.706461972049,
117.296263354442)) ;
#185717 = CARTESIAN_POINT('Ctrl Pts',(-16.0877132298733,-12.7064619737879,
117.320494397539)) ;
#185718 = CARTESIAN_POINT('Ctrl Pts',(-16.104646354501,-12.6534167877166,
117.372069962962)) ;
#185719 = CARTESIAN_POINT('Ctrl Pts',(-16.1215794791288,-12.6003716016452,
117.423645528385)) ;
#185720 = CARTESIAN_POINT('Ctrl Pts',(-16.1953833220854,-12.6003715999064,
117.399414485288)) ;
#185721 = CARTESIAN_POINT('Ctrl Pts',(-16.269187165042,-12.6003715981675,
117.375183442191)) ;
#185722 = CARTESIAN_POINT('Ctrl Pts',(-16.2522540404142,-12.6534167842388,
117.323607876768)) ;
#185723 = CARTESIAN_POINT('Ctrl Pts',(-16.1701161398685,-12.475742126735,
117.108794315217)) ;
#185724 = CARTESIAN_POINT('Ctrl Pts',(-16.158161556272,-12.5412726842435,
117.072382582516)) ;
#185725 = CARTESIAN_POINT('Ctrl Pts',(-16.0843577138288,-12.5412726859999,
117.096613627177)) ;
#185726 = CARTESIAN_POINT('Ctrl Pts',(-16.0105538713855,-12.5412726877563,
117.120844671838)) ;
#185727 = CARTESIAN_POINT('Ctrl Pts',(-16.0225084549819,-12.4757421302478,
117.157256404539)) ;
#185728 = CARTESIAN_POINT('Ctrl Pts',(-16.0344630385783,-12.4102115727394,
117.19366813724)) ;
#185729 = CARTESIAN_POINT('Ctrl Pts',(-16.1082668810216,-12.410211570983,
117.169437092579)) ;
#185730 = CARTESIAN_POINT('Ctrl Pts',(-16.1820707234649,-12.4102115692266,
117.145206047918)) ;
#185731 = CARTESIAN_POINT('Ctrl Pts',(-16.1701161398685,-12.475742126735,
117.108794315217)) ;
#185732 = CARTESIAN_POINT('Ctrl Pts',(-16.0748178977869,-12.3646792210001,
116.854266992389)) ;
#185733 = CARTESIAN_POINT('Ctrl Pts',(-16.0687608064458,-12.438062944576,
116.835818069506)) ;
#185734 = CARTESIAN_POINT('Ctrl Pts',(-15.994956963594,-12.4380629448186,
116.860049112923)) ;
#185735 = CARTESIAN_POINT('Ctrl Pts',(-15.9211531207422,-12.4380629450611,
116.884280156339)) ;
#185736 = CARTESIAN_POINT('Ctrl Pts',(-15.9272102120833,-12.3646792214852,
116.902729079222)) ;
#185737 = CARTESIAN_POINT('Ctrl Pts',(-15.9332673034244,-12.2912954979092,
116.921178002105)) ;
#185738 = CARTESIAN_POINT('Ctrl Pts',(-16.0070711462762,-12.2912954976667,
116.896946958688)) ;
#185739 = CARTESIAN_POINT('Ctrl Pts',(-16.080874989128,-12.2912954974242,
116.872715915272)) ;
#185740 = CARTESIAN_POINT('Ctrl Pts',(-16.0748178977869,-12.3646792210001,
116.854266992389)) ;
#185741 = CARTESIAN_POINT('Ctrl Pts',(-15.974621026397,-12.33019827638,116.584367210853)) ;
#185742 = CARTESIAN_POINT('Ctrl Pts',(-15.9748212050105,-12.4060967099992,
116.584976922591)) ;
#185743 = CARTESIAN_POINT('Ctrl Pts',(-15.9010173612801,-12.4060967096592,
116.609207963332)) ;
#185744 = CARTESIAN_POINT('Ctrl Pts',(-15.8272135175496,-12.4060967093193,
116.633439004072)) ;
#185745 = CARTESIAN_POINT('Ctrl Pts',(-15.8270133389361,-12.3301982757,116.632829292334)) ;
#185746 = CARTESIAN_POINT('Ctrl Pts',(-15.8268131603226,-12.2542998420808,
116.632219580595)) ;
#185747 = CARTESIAN_POINT('Ctrl Pts',(-15.900617004053,-12.2542998424208,
116.607988539855)) ;
#185748 = CARTESIAN_POINT('Ctrl Pts',(-15.9744208477835,-12.2542998427607,
116.583757499115)) ;
#185749 = CARTESIAN_POINT('Ctrl Pts',(-15.974621026397,-12.33019827638,116.584367210853)) ;
#185750 = CARTESIAN_POINT('Ctrl Pts',(-15.8740611512203,-12.3732244526573,
116.313621656584)) ;
#185751 = CARTESIAN_POINT('Ctrl Pts',(-15.8805477737599,-12.4462297114867,
116.333378862108)) ;
#185752 = CARTESIAN_POINT('Ctrl Pts',(-15.8067439284556,-12.4462297127272,
116.357609898054)) ;
#185753 = CARTESIAN_POINT('Ctrl Pts',(-15.7329400831513,-12.4462297139677,
116.381840934001)) ;
#185754 = CARTESIAN_POINT('Ctrl Pts',(-15.7264534606117,-12.3732244551383,
116.362083728477)) ;
#185755 = CARTESIAN_POINT('Ctrl Pts',(-15.7199668380721,-12.300219196309,
116.342326522954)) ;
#185756 = CARTESIAN_POINT('Ctrl Pts',(-15.7937706833764,-12.3002191950685,
116.318095487007)) ;
#185757 = CARTESIAN_POINT('Ctrl Pts',(-15.8675745286806,-12.300219193828,
116.293864451061)) ;
#185758 = CARTESIAN_POINT('Ctrl Pts',(-15.8740611512203,-12.3732244526573,
116.313621656584)) ;
#185759 = CARTESIAN_POINT('Ctrl Pts',(-15.7806896879086,-12.4909980427198,
116.064622149398)) ;
#185760 = CARTESIAN_POINT('Ctrl Pts',(-15.7929728305085,-12.5558859351168,
116.102034619648)) ;
#185761 = CARTESIAN_POINT('Ctrl Pts',(-15.7191689838426,-12.555885940904,
116.126265651448)) ;
#185762 = CARTESIAN_POINT('Ctrl Pts',(-15.6453651371768,-12.5558859466913,
116.150496683248)) ;
#185763 = CARTESIAN_POINT('Ctrl Pts',(-15.6330819945769,-12.4909980542943,
116.113084212997)) ;
#185764 = CARTESIAN_POINT('Ctrl Pts',(-15.6207988519771,-12.4261101618973,
116.075671742746)) ;
#185765 = CARTESIAN_POINT('Ctrl Pts',(-15.6946026986429,-12.4261101561101,
116.051440710946)) ;
#185766 = CARTESIAN_POINT('Ctrl Pts',(-15.7684065453087,-12.4261101503228,
116.027209679147)) ;
#185767 = CARTESIAN_POINT('Ctrl Pts',(-15.7806896879086,-12.4909980427198,
116.064622149398)) ;
#185768 = CARTESIAN_POINT('Ctrl Pts',(-15.6998735281005,-12.67497986033,115.853907441211)) ;
#185769 = CARTESIAN_POINT('Ctrl Pts',(-15.7170839596561,-12.7271157689749,
115.906327638474)) ;
#185770 = CARTESIAN_POINT('Ctrl Pts',(-15.6432801120866,-12.727115782205,
115.930558667521)) ;
#185771 = CARTESIAN_POINT('Ctrl Pts',(-15.569476264517,-12.7271157954351,
115.954789696568)) ;
#185772 = CARTESIAN_POINT('Ctrl Pts',(-15.5522658329614,-12.6749798867901,
115.902369499305)) ;
#185773 = CARTESIAN_POINT('Ctrl Pts',(-15.5350554014057,-12.6228439781452,
115.849949302042)) ;
#185774 = CARTESIAN_POINT('Ctrl Pts',(-15.6088592489752,-12.6228439649152,
115.825718272995)) ;
#185775 = CARTESIAN_POINT('Ctrl Pts',(-15.6826630965448,-12.6228439516851,
115.801487243948)) ;
#185776 = CARTESIAN_POINT('Ctrl Pts',(-15.6998735281005,-12.67497986033,115.853907441211)) ;
#185777 = CARTESIAN_POINT('Ctrl Pts',(-15.6366680399121,-12.9129719673497,
115.696933930181)) ;
#185778 = CARTESIAN_POINT('Ctrl Pts',(-15.6575811570006,-12.9485664184321,
115.760631909985)) ;
#185779 = CARTESIAN_POINT('Ctrl Pts',(-15.5837773094315,-12.9485664423294,
115.784862939033)) ;
#185780 = CARTESIAN_POINT('Ctrl Pts',(-15.5099734618623,-12.9485664662267,
115.809093968081)) ;
#185781 = CARTESIAN_POINT('Ctrl Pts',(-15.4890603447738,-12.9129720151443,
115.745395988277)) ;
#185782 = CARTESIAN_POINT('Ctrl Pts',(-15.4681472276853,-12.8773775640619,
115.681698008474)) ;
#185783 = CARTESIAN_POINT('Ctrl Pts',(-15.5419510752545,-12.8773775401646,
115.657466979426)) ;
#185784 = CARTESIAN_POINT('Ctrl Pts',(-15.6157549228236,-12.8773775162673,
115.633235950377)) ;
#185785 = CARTESIAN_POINT('Ctrl Pts',(-15.6366680399121,-12.9129719673497,
115.696933930181)) ;
#185786 = CARTESIAN_POINT('Ctrl Pts',(-15.5952249708799,-13.1860117694584,
115.606088574179)) ;
#185787 = CARTESIAN_POINT('Ctrl Pts',(-15.6183296594594,-13.2025937727261,
115.676461726988)) ;
#185788 = CARTESIAN_POINT('Ctrl Pts',(-15.5445258135152,-13.2025938067603,
115.700692760986)) ;
#185789 = CARTESIAN_POINT('Ctrl Pts',(-15.4707219675711,-13.2025938407946,
115.724923794983)) ;
#185790 = CARTESIAN_POINT('Ctrl Pts',(-15.4476172789917,-13.1860118375269,
115.654550642175)) ;
#185791 = CARTESIAN_POINT('Ctrl Pts',(-15.4245125904123,-13.1694298342593,
115.584177489366)) ;
#185792 = CARTESIAN_POINT('Ctrl Pts',(-15.4983164363564,-13.169429800225,
115.559946455368)) ;
#185793 = CARTESIAN_POINT('Ctrl Pts',(-15.5721202823005,-13.1694297661908,
115.53571542137)) ;
#185794 = CARTESIAN_POINT('Ctrl Pts',(-15.5952249708799,-13.1860117694584,
115.606088574179)) ;
#185795 = CARTESIAN_POINT('Ctrl Pts',(-15.5773486535781,-13.4763914936473,
115.587122093888)) ;
#185796 = CARTESIAN_POINT('Ctrl Pts',(-15.6010006622766,-13.4727232020181,
115.659162295299)) ;
#185797 = CARTESIAN_POINT('Ctrl Pts',(-15.5271968193326,-13.4727232458184,
115.683393338435)) ;
#185798 = CARTESIAN_POINT('Ctrl Pts',(-15.4533929763885,-13.4727232896187,
115.70762438157)) ;
#185799 = CARTESIAN_POINT('Ctrl Pts',(-15.42974096769,-13.4763915812479,115.635584180159)) ;
#185800 = CARTESIAN_POINT('Ctrl Pts',(-15.4060889589915,-13.4800598728771,
115.563543978747)) ;
#185801 = CARTESIAN_POINT('Ctrl Pts',(-15.4798928019355,-13.4800598290768,
115.539312935612)) ;
#185802 = CARTESIAN_POINT('Ctrl Pts',(-15.5536966448795,-13.4800597852765,
115.515081892476)) ;
#185803 = CARTESIAN_POINT('Ctrl Pts',(-15.5773486535781,-13.4763914936473,
115.587122093888)) ;
#185804 = CARTESIAN_POINT('Ctrl Pts',(-15.5838924485424,-13.7633156829476,
115.642631367891)) ;
#185805 = CARTESIAN_POINT('Ctrl Pts',(-15.6063856690625,-13.7396092222064,
115.711142087291)) ;
#185806 = CARTESIAN_POINT('Ctrl Pts',(-15.5325818307443,-13.7396092733025,
115.735373144516)) ;
#185807 = CARTESIAN_POINT('Ctrl Pts',(-15.4587779924262,-13.7396093243987,
115.759604201741)) ;
#185808 = CARTESIAN_POINT('Ctrl Pts',(-15.4362847719061,-13.7633157851398,
115.691093482342)) ;
#185809 = CARTESIAN_POINT('Ctrl Pts',(-15.4137915513859,-13.787022245881,
115.622582762942)) ;
#185810 = CARTESIAN_POINT('Ctrl Pts',(-15.4875953897041,-13.7870221947849,
115.598351705717)) ;
#185811 = CARTESIAN_POINT('Ctrl Pts',(-15.5613992280222,-13.7870221436888,
115.574120648491)) ;
#185812 = CARTESIAN_POINT('Ctrl Pts',(-15.5838924485424,-13.7633156829476,
115.642631367891)) ;
#185813 = CARTESIAN_POINT('Ctrl Pts',(-15.6133732890566,-14.0239605605361,
115.767794362967)) ;
#185814 = CARTESIAN_POINT('Ctrl Pts',(-15.6331087715713,-13.9820221332016,
115.827905457214)) ;
#185815 = CARTESIAN_POINT('Ctrl Pts',(-15.5593049386299,-13.9820221845115,
115.852136530816)) ;
#185816 = CARTESIAN_POINT('Ctrl Pts',(-15.4855011056886,-13.9820222358214,
115.876367604418)) ;
#185817 = CARTESIAN_POINT('Ctrl Pts',(-15.4657656231739,-14.023960663156,
115.816256510171)) ;
#185818 = CARTESIAN_POINT('Ctrl Pts',(-15.4460301406592,-14.0658990904905,
115.756145415925)) ;
#185819 = CARTESIAN_POINT('Ctrl Pts',(-15.5198339736006,-14.0658990391806,
115.731914342323)) ;
#185820 = CARTESIAN_POINT('Ctrl Pts',(-15.5936378065419,-14.0658989878706,
115.707683268721)) ;
#185821 = CARTESIAN_POINT('Ctrl Pts',(-15.6133732890566,-14.0239605605361,
115.767794362967)) ;
#185822 = CARTESIAN_POINT('Ctrl Pts',(-15.6631890060082,-14.2421936446632,
115.955049772158)) ;
#185823 = CARTESIAN_POINT('Ctrl Pts',(-15.678739990713,-14.1849578741807,
116.002415561072)) ;
#185824 = CARTESIAN_POINT('Ctrl Pts',(-15.604936163726,-14.1849579203882,
116.026646652811)) ;
#185825 = CARTESIAN_POINT('Ctrl Pts',(-15.5311323367391,-14.1849579665956,
116.050877744549)) ;
#185826 = CARTESIAN_POINT('Ctrl Pts',(-15.5155813520343,-14.2421937370781,
116.003511955634)) ;
#185827 = CARTESIAN_POINT('Ctrl Pts',(-15.5000303673295,-14.2994295075606,
115.95614616672)) ;
#185828 = CARTESIAN_POINT('Ctrl Pts',(-15.5738341943165,-14.2994294613532,
115.931915074982)) ;
#185829 = CARTESIAN_POINT('Ctrl Pts',(-15.6476380213034,-14.2994294151457,
115.907683983244)) ;
#185830 = CARTESIAN_POINT('Ctrl Pts',(-15.6631890060082,-14.2421936446632,
115.955049772158)) ;
#185831 = CARTESIAN_POINT('Ctrl Pts',(-15.728520728614,-14.4005934040497,
116.189363403692)) ;
#185832 = CARTESIAN_POINT('Ctrl Pts',(-15.7388019491786,-14.3322159891563,
116.220678341182)) ;
#185833 = CARTESIAN_POINT('Ctrl Pts',(-15.664998127278,-14.3322160226317,
116.244909448412)) ;
#185834 = CARTESIAN_POINT('Ctrl Pts',(-15.5911943053774,-14.332216056107,
116.269140555643)) ;
#185835 = CARTESIAN_POINT('Ctrl Pts',(-15.5809130848128,-14.4005934710005,
116.237825618152)) ;
#185836 = CARTESIAN_POINT('Ctrl Pts',(-15.5706318642482,-14.4689708858939,
116.206510680662)) ;
#185837 = CARTESIAN_POINT('Ctrl Pts',(-15.6444356861487,-14.4689708524185,
116.182279573432)) ;
#185838 = CARTESIAN_POINT('Ctrl Pts',(-15.7182395080493,-14.4689708189432,
116.158048466201)) ;
#185839 = CARTESIAN_POINT('Ctrl Pts',(-15.728520728614,-14.4005934040497,
116.189363403692)) ;
#185840 = CARTESIAN_POINT('Ctrl Pts',(-15.80481754392,-14.4895021228897,116.457354192915)) ;
#185841 = CARTESIAN_POINT('Ctrl Pts',(-15.8090502714838,-14.4148177682025,
116.470246396486)) ;
#185842 = CARTESIAN_POINT('Ctrl Pts',(-15.7352464541145,-14.4148177835068,
116.494477517518)) ;
#185843 = CARTESIAN_POINT('Ctrl Pts',(-15.6614426367453,-14.4148177988111,
116.51870863855)) ;
#185844 = CARTESIAN_POINT('Ctrl Pts',(-15.6572099091815,-14.4895021534983,
116.505816434979)) ;
#185845 = CARTESIAN_POINT('Ctrl Pts',(-15.6529771816177,-14.5641865081855,
116.492924231409)) ;
#185846 = CARTESIAN_POINT('Ctrl Pts',(-15.7267809989869,-14.5641864928812,
116.468693110377)) ;
#185847 = CARTESIAN_POINT('Ctrl Pts',(-15.8005848163562,-14.5641864775769,
116.444461989345)) ;
#185848 = CARTESIAN_POINT('Ctrl Pts',(-15.80481754392,-14.4895021228897,116.457354192915)) ;
#185849 = CARTESIAN_POINT('Ctrl Pts',(-15.8848712831143,-14.5012817728617,
116.736556722847)) ;
#185850 = CARTESIAN_POINT('Ctrl Pts',(-15.8827891653978,-14.425666653241,
116.73021492648)) ;
#185851 = CARTESIAN_POINT('Ctrl Pts',(-15.8089853501543,-14.4256666452889,
116.754446053986)) ;
#185852 = CARTESIAN_POINT('Ctrl Pts',(-15.7351815349108,-14.4256666373369,
116.778677181493)) ;
#185853 = CARTESIAN_POINT('Ctrl Pts',(-15.7372636526273,-14.5012817569575,
116.78501897786)) ;
#185854 = CARTESIAN_POINT('Ctrl Pts',(-15.7393457703438,-14.5768968765781,
116.791360774228)) ;
#185855 = CARTESIAN_POINT('Ctrl Pts',(-15.8131495855873,-14.5768968845302,
116.767129646721)) ;
#185856 = CARTESIAN_POINT('Ctrl Pts',(-15.8869534008308,-14.5768968924823,
116.742898519214)) ;
#185857 = CARTESIAN_POINT('Ctrl Pts',(-15.8848712831143,-14.5012817728617,
116.736556722847)) ;
#185858 = CARTESIAN_POINT('Ctrl Pts',(-15.9632161467547,-14.43501211062,117.010828764806)) ;
#185859 = CARTESIAN_POINT('Ctrl Pts',(-15.9549236920078,-14.363912820796,
116.985571283752)) ;
#185860 = CARTESIAN_POINT('Ctrl Pts',(-15.8811198769776,-14.3639127866614,
117.009802411908)) ;
#185861 = CARTESIAN_POINT('Ctrl Pts',(-15.8073160619473,-14.3639127525269,
117.034033540064)) ;
#185862 = CARTESIAN_POINT('Ctrl Pts',(-15.8156085166942,-14.4350120423509,
117.059291021119)) ;
#185863 = CARTESIAN_POINT('Ctrl Pts',(-15.823900971441,-14.506111332175,117.084548502173)) ;
#185864 = CARTESIAN_POINT('Ctrl Pts',(-15.8977047864712,-14.5061113663095,
117.060317374017)) ;
#185865 = CARTESIAN_POINT('Ctrl Pts',(-15.9715086015015,-14.5061114004441,
117.036086245861)) ;
#185866 = CARTESIAN_POINT('Ctrl Pts',(-15.9632161467547,-14.43501211062,117.010828764806)) ;
#185867 = CARTESIAN_POINT('Ctrl Pts',(-16.0321824010801,-14.2968843843662,
117.256163976492)) ;
#185868 = CARTESIAN_POINT('Ctrl Pts',(-16.0183329772586,-14.2353253070851,
117.213980864183)) ;
#185869 = CARTESIAN_POINT('Ctrl Pts',(-15.9445291592642,-14.2353252479564,
117.238211983311)) ;
#185870 = CARTESIAN_POINT('Ctrl Pts',(-15.8707253412697,-14.2353251888277,
117.262443102438)) ;
#185871 = CARTESIAN_POINT('Ctrl Pts',(-15.8845747650913,-14.2968842661087,
117.304626214748)) ;
#185872 = CARTESIAN_POINT('Ctrl Pts',(-15.8984241889128,-14.3584433433898,
117.346809327058)) ;
#185873 = CARTESIAN_POINT('Ctrl Pts',(-15.9722280069073,-14.3584434025185,
117.32257820793)) ;
#185874 = CARTESIAN_POINT('Ctrl Pts',(-16.0460318249017,-14.3584434616473,
117.298347088802)) ;
#185875 = CARTESIAN_POINT('Ctrl Pts',(-16.0321824010801,-14.2968843843662,
117.256163976492)) ;
#185876 = CARTESIAN_POINT('Ctrl Pts',(-16.0872824733374,-14.0952651274861,
117.459484020203)) ;
#185877 = CARTESIAN_POINT('Ctrl Pts',(-16.0688314524017,-14.0476919571474,
117.403285185476)) ;
#185878 = CARTESIAN_POINT('Ctrl Pts',(-15.9950276293236,-14.0476918755957,
117.42751628912)) ;
#185879 = CARTESIAN_POINT('Ctrl Pts',(-15.9212238062455,-14.047691794044,
117.451747392764)) ;
#185880 = CARTESIAN_POINT('Ctrl Pts',(-15.9396748271812,-14.0952649643827,
117.507946227491)) ;
#185881 = CARTESIAN_POINT('Ctrl Pts',(-15.9581258481169,-14.1428381347214,
117.564145062217)) ;
#185882 = CARTESIAN_POINT('Ctrl Pts',(-16.031929671195,-14.1428382162731,
117.539913958574)) ;
#185883 = CARTESIAN_POINT('Ctrl Pts',(-16.1057334942731,-14.1428382978248,
117.51568285493)) ;
#185884 = CARTESIAN_POINT('Ctrl Pts',(-16.0872824733374,-14.0952651274861,
117.459484020203)) ;
#185885 = CARTESIAN_POINT('Ctrl Pts',(-16.1232711688005,-13.8453444760412,
117.604537921654)) ;
#185886 = CARTESIAN_POINT('Ctrl Pts',(-16.101547172297,-13.8151498849244,
117.538370131394)) ;
#185887 = CARTESIAN_POINT('Ctrl Pts',(-16.0277433420106,-13.8151497867456,
117.562601213082)) ;
#185888 = CARTESIAN_POINT('Ctrl Pts',(-15.9539395117242,-13.8151496885667,
117.586832294771)) ;
#185889 = CARTESIAN_POINT('Ctrl Pts',(-15.9756635082278,-13.8453442796835,
117.653000085031)) ;
#185890 = CARTESIAN_POINT('Ctrl Pts',(-15.9973875047314,-13.8755388708002,
117.719167875291)) ;
#185891 = CARTESIAN_POINT('Ctrl Pts',(-16.0711913350178,-13.8755389689791,
117.694936793603)) ;
#185892 = CARTESIAN_POINT('Ctrl Pts',(-16.1449951653041,-13.8755390671579,
117.670705711914)) ;
#185893 = CARTESIAN_POINT('Ctrl Pts',(-16.1232711688005,-13.8453444760412,
117.604537921654)) ;
#185894 = CARTESIAN_POINT('Ctrl Pts',(-16.1369703680654,-13.5639203016943,
117.681820810949)) ;
#185895 = CARTESIAN_POINT('Ctrl Pts',(-16.1135220904896,-13.5533288537195,
117.610401138726)) ;
#185896 = CARTESIAN_POINT('Ctrl Pts',(-16.0397182516176,-13.5533287463832,
117.634632194264)) ;
#185897 = CARTESIAN_POINT('Ctrl Pts',(-15.9659144127456,-13.5533286390469,
117.658863249802)) ;
#185898 = CARTESIAN_POINT('Ctrl Pts',(-15.9893626903214,-13.5639200870216,
117.730282922026)) ;
#185899 = CARTESIAN_POINT('Ctrl Pts',(-16.0128109678972,-13.5745115349964,
117.801702594249)) ;
#185900 = CARTESIAN_POINT('Ctrl Pts',(-16.0866148067692,-13.5745116423327,
117.777471538711)) ;
#185901 = CARTESIAN_POINT('Ctrl Pts',(-16.1604186456412,-13.574511749669,
117.753240483173)) ;
#185902 = CARTESIAN_POINT('Ctrl Pts',(-16.1369703680654,-13.5639203016943,
117.681820810949)) ;
#185903 = CARTESIAN_POINT('Ctrl Pts',(-16.1263949656492,-13.2722319962961,
117.685137077864)) ;
#185904 = CARTESIAN_POINT('Ctrl Pts',(-16.102915121327,-13.2819894198182,
117.613621258424)) ;
#185905 = CARTESIAN_POINT('Ctrl Pts',(-16.0291112733662,-13.2819893125246,
117.637852286279)) ;
#185906 = CARTESIAN_POINT('Ctrl Pts',(-15.9553074254054,-13.281989205231,
117.662083314134)) ;
#185907 = CARTESIAN_POINT('Ctrl Pts',(-15.9787872697277,-13.2722317817088,
117.733599133574)) ;
#185908 = CARTESIAN_POINT('Ctrl Pts',(-16.0022671140499,-13.2624743581867,
117.805114953013)) ;
#185909 = CARTESIAN_POINT('Ctrl Pts',(-16.0760709620107,-13.2624744654803,
117.780883925158)) ;
#185910 = CARTESIAN_POINT('Ctrl Pts',(-16.1498748099715,-13.262474572774,
117.756652897303)) ;
#185911 = CARTESIAN_POINT('Ctrl Pts',(-16.1263949656492,-13.2722319962961,
117.685137077864)) ;
#185912 = CARTESIAN_POINT('Ctrl Pts',(-16.0919950705927,-12.9927108288244,
117.6156635482)) ;
#185913 = CARTESIAN_POINT('Ctrl Pts',(-16.070151731594,-13.0219980101555,
117.549132259942)) ;
#185914 = CARTESIAN_POINT('Ctrl Pts',(-15.9963478750301,-13.0219979113137,
117.573363261593)) ;
#185915 = CARTESIAN_POINT('Ctrl Pts',(-15.9225440184661,-13.0219978124719,
117.597594263245)) ;
#185916 = CARTESIAN_POINT('Ctrl Pts',(-15.9443873574648,-12.9927106311408,
117.664125551502)) ;
#185917 = CARTESIAN_POINT('Ctrl Pts',(-15.9662306964635,-12.9634234498097,
117.730656839759)) ;
#185918 = CARTESIAN_POINT('Ctrl Pts',(-16.0400345530275,-12.9634235486515,
117.706425838108)) ;
#185919 = CARTESIAN_POINT('Ctrl Pts',(-16.1138384095914,-12.9634236474933,
117.682194836457)) ;
#185920 = CARTESIAN_POINT('Ctrl Pts',(-16.0919950705927,-12.9927108288244,
117.6156635482)) ;
#185921 = CARTESIAN_POINT('Ctrl Pts',(-16.0350077383484,-12.7419081122581,
117.477619455827)) ;
#185922 = CARTESIAN_POINT('Ctrl Pts',(-16.016375282967,-12.7887491311702,
117.420868001036)) ;
#185923 = CARTESIAN_POINT('Ctrl Pts',(-15.942571419085,-12.78874904886,117.445098980398)) ;
#185924 = CARTESIAN_POINT('Ctrl Pts',(-15.8687675552031,-12.7887489665498,
117.46932995976)) ;
#185925 = CARTESIAN_POINT('Ctrl Pts',(-15.8874000105845,-12.7419079476376,
117.52608141455)) ;
#185926 = CARTESIAN_POINT('Ctrl Pts',(-15.9060324659659,-12.6950669287254,
117.582832869341)) ;
#185927 = CARTESIAN_POINT('Ctrl Pts',(-15.9798363298478,-12.6950670110357,
117.558601889979)) ;
#185928 = CARTESIAN_POINT('Ctrl Pts',(-16.0536401937297,-12.6950670933459,
117.534370910617)) ;
#185929 = CARTESIAN_POINT('Ctrl Pts',(-16.0350077383484,-12.7419081122581,
117.477619455827)) ;
#185930 = CARTESIAN_POINT('Ctrl Pts',(-15.9591220993108,-12.5402274188012,
117.281908126571)) ;
#185931 = CARTESIAN_POINT('Ctrl Pts',(-15.9450269627281,-12.6012191381552,
117.238976612807)) ;
#185932 = CARTESIAN_POINT('Ctrl Pts',(-15.8712230935302,-12.6012190780927,
117.263207575978)) ;
#185933 = CARTESIAN_POINT('Ctrl Pts',(-15.7974192243324,-12.6012190180302,
117.287438539148)) ;
#185934 = CARTESIAN_POINT('Ctrl Pts',(-15.8115143609151,-12.5402272986761,
117.330370052912)) ;
#185935 = CARTESIAN_POINT('Ctrl Pts',(-15.8256094974978,-12.479235579322,
117.373301566676)) ;
#185936 = CARTESIAN_POINT('Ctrl Pts',(-15.8994133666956,-12.4792356393845,
117.349070603506)) ;
#185937 = CARTESIAN_POINT('Ctrl Pts',(-15.9732172358935,-12.4792356994471,
117.324839640335)) ;
#185938 = CARTESIAN_POINT('Ctrl Pts',(-15.9591220993108,-12.5402274188012,
117.281908126571)) ;
#185939 = CARTESIAN_POINT('Ctrl Pts',(-15.8687073550715,-12.4011175779625,
117.042022844154)) ;
#185940 = CARTESIAN_POINT('Ctrl Pts',(-15.8601689623456,-12.4719130809355,
117.016016275687)) ;
#185941 = CARTESIAN_POINT('Ctrl Pts',(-15.7863650903915,-12.4719130465785,
117.040247230462)) ;
#185942 = CARTESIAN_POINT('Ctrl Pts',(-15.7125612184373,-12.4719130122216,
117.064478185237)) ;
#185943 = CARTESIAN_POINT('Ctrl Pts',(-15.7210996111632,-12.4011175092485,
117.090484753705)) ;
#185944 = CARTESIAN_POINT('Ctrl Pts',(-15.729638003889,-12.3303220062755,
117.116491322172)) ;
#185945 = CARTESIAN_POINT('Ctrl Pts',(-15.8034418758432,-12.3303220406325,
117.092260367396)) ;
#185946 = CARTESIAN_POINT('Ctrl Pts',(-15.8772457477973,-12.3303220749894,
117.068029412621)) ;
#185947 = CARTESIAN_POINT('Ctrl Pts',(-15.8687073550715,-12.4011175779625,
117.042022844154)) ;
#185948 = CARTESIAN_POINT('Ctrl Pts',(-15.7700176989328,-12.3349520470046,
116.776796250554)) ;
#185949 = CARTESIAN_POINT('Ctrl Pts',(-15.767625022208,-12.4104731774987,
116.769508541507)) ;
#185950 = CARTESIAN_POINT('Ctrl Pts',(-15.6938211498566,-12.4104731691892,
116.793739495072)) ;
#185951 = CARTESIAN_POINT('Ctrl Pts',(-15.6200172775051,-12.4104731608796,
116.817970448637)) ;
#185952 = CARTESIAN_POINT('Ctrl Pts',(-15.6224099542299,-12.3349520303855,
116.825258157684)) ;
#185953 = CARTESIAN_POINT('Ctrl Pts',(-15.6248026309546,-12.2594308998913,
116.832545866731)) ;
#185954 = CARTESIAN_POINT('Ctrl Pts',(-15.6986065033061,-12.2594309082008,
116.808314913166)) ;
#185955 = CARTESIAN_POINT('Ctrl Pts',(-15.7724103756575,-12.2594309165104,
116.784083959601)) ;
#185956 = CARTESIAN_POINT('Ctrl Pts',(-15.7700176989328,-12.3349520470046,
116.776796250554)) ;
#185957 = CARTESIAN_POINT('Ctrl Pts',(-15.6682261809247,-12.346456548631,
116.502406394127)) ;
#185958 = CARTESIAN_POINT('Ctrl Pts',(-15.6721990720837,-12.4212888141347,
116.514507177916)) ;
#185959 = CARTESIAN_POINT('Ctrl Pts',(-15.5983952023686,-12.4212888296186,
116.538738139512)) ;
#185960 = CARTESIAN_POINT('Ctrl Pts',(-15.5245913326536,-12.4212888451025,
116.562969101107)) ;
#185961 = CARTESIAN_POINT('Ctrl Pts',(-15.5206184414946,-12.3464565795988,
116.550868317317)) ;
#185962 = CARTESIAN_POINT('Ctrl Pts',(-15.5166455503357,-12.2716243140951,
116.538767533527)) ;
#185963 = CARTESIAN_POINT('Ctrl Pts',(-15.5904494200508,-12.2716242986112,
116.514536571932)) ;
#185964 = CARTESIAN_POINT('Ctrl Pts',(-15.6642532897658,-12.2716242831273,
116.490305610337)) ;
#185965 = CARTESIAN_POINT('Ctrl Pts',(-15.6682261809247,-12.346456548631,
116.502406394127)) ;
#185966 = CARTESIAN_POINT('Ctrl Pts',(-15.5714939849773,-12.4344867986536,
116.243115588663)) ;
#185967 = CARTESIAN_POINT('Ctrl Pts',(-15.5814953588048,-12.5032854856229,
116.273578158085)) ;
#185968 = CARTESIAN_POINT('Ctrl Pts',(-15.5076914930099,-12.5032855202655,
116.297809131621)) ;
#185969 = CARTESIAN_POINT('Ctrl Pts',(-15.4338876272149,-12.503285554908,
116.322040105156)) ;
#185970 = CARTESIAN_POINT('Ctrl Pts',(-15.4238862533874,-12.4344868679388,
116.291577535733)) ;
#185971 = CARTESIAN_POINT('Ctrl Pts',(-15.4138848795598,-12.3656881809695,
116.261114966311)) ;
#185972 = CARTESIAN_POINT('Ctrl Pts',(-15.4876887453548,-12.365688146327,
116.236883992776)) ;
#185973 = CARTESIAN_POINT('Ctrl Pts',(-15.5614926111498,-12.3656881116844,
116.21265301924)) ;
#185974 = CARTESIAN_POINT('Ctrl Pts',(-15.5714939849773,-12.4344867986536,
116.243115588663)) ;
#185975 = CARTESIAN_POINT('Ctrl Pts',(-15.4847018094329,-12.5932721982848,
116.014273618595)) ;
#185976 = CARTESIAN_POINT('Ctrl Pts',(-15.5000432541393,-12.6510887725529,
116.061001182452)) ;
#185977 = CARTESIAN_POINT('Ctrl Pts',(-15.4262393939096,-12.6510888198682,
116.085232172938)) ;
#185978 = CARTESIAN_POINT('Ctrl Pts',(-15.3524355336799,-12.6510888671835,
116.109463163424)) ;
#185979 = CARTESIAN_POINT('Ctrl Pts',(-15.3370940889735,-12.5932722929155,
116.062735599568)) ;
#185980 = CARTESIAN_POINT('Ctrl Pts',(-15.3217526442671,-12.5354557186474,
116.016008035711)) ;
#185981 = CARTESIAN_POINT('Ctrl Pts',(-15.3955565044968,-12.5354556713321,
115.991777045225)) ;
#185982 = CARTESIAN_POINT('Ctrl Pts',(-15.4693603647265,-12.5354556240167,
115.967546054739)) ;
#185983 = CARTESIAN_POINT('Ctrl Pts',(-15.4847018094329,-12.5932721982848,
116.014273618595)) ;
#185984 = CARTESIAN_POINT('Ctrl Pts',(-15.4140311873583,-12.8103924299054,
115.834395867115)) ;
#185985 = CARTESIAN_POINT('Ctrl Pts',(-15.4335980718028,-12.8531370145114,
115.893993438782)) ;
#185986 = CARTESIAN_POINT('Ctrl Pts',(-15.3597942173693,-12.8531370683972,
115.918224446923)) ;
#185987 = CARTESIAN_POINT('Ctrl Pts',(-15.2859903629358,-12.8531371222829,
115.942455455063)) ;
#185988 = CARTESIAN_POINT('Ctrl Pts',(-15.2664234784913,-12.810392537677,
115.882857883396)) ;
#185989 = CARTESIAN_POINT('Ctrl Pts',(-15.2468565940469,-12.767647953071,
115.823260311728)) ;
#185990 = CARTESIAN_POINT('Ctrl Pts',(-15.3206604484804,-12.7676478991852,
115.799029303588)) ;
#185991 = CARTESIAN_POINT('Ctrl Pts',(-15.3944643029138,-12.7676478452995,
115.774798295448)) ;
#185992 = CARTESIAN_POINT('Ctrl Pts',(-15.4140311873583,-12.8103924299054,
115.834395867115)) ;
#185993 = CARTESIAN_POINT('Ctrl Pts',(-15.3631390797612,-13.0726323412443,
115.714998308832)) ;
#185994 = CARTESIAN_POINT('Ctrl Pts',(-15.3855521726195,-13.0971322435792,
115.783264972285)) ;
#185995 = CARTESIAN_POINT('Ctrl Pts',(-15.3117483240823,-13.0971322955942,
115.807495998385)) ;
#185996 = CARTESIAN_POINT('Ctrl Pts',(-15.2379444755452,-13.0971323476091,
115.831727024485)) ;
#185997 = CARTESIAN_POINT('Ctrl Pts',(-15.2155313826869,-13.0726324452743,
115.763460361032)) ;
#185998 = CARTESIAN_POINT('Ctrl Pts',(-15.1931182898287,-13.0481325429394,
115.695193697579)) ;
#185999 = CARTESIAN_POINT('Ctrl Pts',(-15.2669221383658,-13.0481324909245,
115.670962671479)) ;
#186000 = CARTESIAN_POINT('Ctrl Pts',(-15.3407259869029,-13.0481324389095,
115.646731645379)) ;
#186001 = CARTESIAN_POINT('Ctrl Pts',(-15.3631390797612,-13.0726323412443,
115.714998308832)) ;
#186002 = CARTESIAN_POINT('Ctrl Pts',(-15.335631959363,-13.3588849654739,
115.66670490255)) ;
#186003 = CARTESIAN_POINT('Ctrl Pts',(-15.359265307546,-13.3634353466295,
115.738688267008)) ;
#186004 = CARTESIAN_POINT('Ctrl Pts',(-15.2854614635794,-13.3634353921752,
115.762919307028)) ;
#186005 = CARTESIAN_POINT('Ctrl Pts',(-15.2116576196127,-13.3634354377208,
115.787150347049)) ;
#186006 = CARTESIAN_POINT('Ctrl Pts',(-15.1880242714297,-13.3588850565651,
115.715166982591)) ;
#186007 = CARTESIAN_POINT('Ctrl Pts',(-15.1643909232466,-13.3543346754094,
115.643183618133)) ;
#186008 = CARTESIAN_POINT('Ctrl Pts',(-15.2381947672133,-13.3543346298638,
115.618952578112)) ;
#186009 = CARTESIAN_POINT('Ctrl Pts',(-15.3119986111799,-13.3543345843182,
115.594721538092)) ;
#186010 = CARTESIAN_POINT('Ctrl Pts',(-15.335631959363,-13.3588849654739,
115.66670490255)) ;
#186011 = CARTESIAN_POINT('Ctrl Pts',(-15.3323120932461,-13.6479812710763,
115.691913999484)) ;
#186012 = CARTESIAN_POINT('Ctrl Pts',(-15.3554820543391,-13.6323532637261,
115.762485961773)) ;
#186013 = CARTESIAN_POINT('Ctrl Pts',(-15.2816782136833,-13.6323533009956,
115.786717011878)) ;
#186014 = CARTESIAN_POINT('Ctrl Pts',(-15.2078743730274,-13.632353338265,
115.810948061983)) ;
#186015 = CARTESIAN_POINT('Ctrl Pts',(-15.1847044119345,-13.6479813456151,
115.740376099694)) ;
#186016 = CARTESIAN_POINT('Ctrl Pts',(-15.1615344508415,-13.6636093529653,
115.669804137404)) ;
#186017 = CARTESIAN_POINT('Ctrl Pts',(-15.2353382914973,-13.6636093156958,
115.645573087299)) ;
#186018 = CARTESIAN_POINT('Ctrl Pts',(-15.3091421321531,-13.6636092784264,
115.621342037194)) ;
#186019 = CARTESIAN_POINT('Ctrl Pts',(-15.3323120932461,-13.6479812710763,
115.691913999484)) ;
#186020 = CARTESIAN_POINT('Ctrl Pts',(-15.3527558752554,-13.9223253071587,
115.789719726039)) ;
#186021 = CARTESIAN_POINT('Ctrl Pts',(-15.3737981985428,-13.8875179705717,
115.853811247044)) ;
#186022 = CARTESIAN_POINT('Ctrl Pts',(-15.2999943595609,-13.8875179960034,
115.878042302247)) ;
#186023 = CARTESIAN_POINT('Ctrl Pts',(-15.2261905205791,-13.8875180214352,
115.902273357451)) ;
#186024 = CARTESIAN_POINT('Ctrl Pts',(-15.2051481972916,-13.9223253580222,
115.838181836446)) ;
#186025 = CARTESIAN_POINT('Ctrl Pts',(-15.1841058740042,-13.9571326946092,
115.774090315441)) ;
#186026 = CARTESIAN_POINT('Ctrl Pts',(-15.2579097129861,-13.9571326691774,
115.749859260238)) ;
#186027 = CARTESIAN_POINT('Ctrl Pts',(-15.3317135519679,-13.9571326437457,
115.725628205034)) ;
#186028 = CARTESIAN_POINT('Ctrl Pts',(-15.3527558752554,-13.9223253071587,
115.789719726039)) ;
#186029 = CARTESIAN_POINT('Ctrl Pts',(-15.3947103578552,-14.1598247969233,
115.952946574138)) ;
#186030 = CARTESIAN_POINT('Ctrl Pts',(-15.4121217162786,-14.1083816279705,
116.005978762172)) ;
#186031 = CARTESIAN_POINT('Ctrl Pts',(-15.3383178775536,-14.1083816430256,
116.030209818158)) ;
#186032 = CARTESIAN_POINT('Ctrl Pts',(-15.2645140388287,-14.1083816580807,
116.054440874144)) ;
#186033 = CARTESIAN_POINT('Ctrl Pts',(-15.2471026804054,-14.1598248270335,
116.00140868611)) ;
#186034 = CARTESIAN_POINT('Ctrl Pts',(-15.229691321982,-14.2112679959863,
115.948376498076)) ;
#186035 = CARTESIAN_POINT('Ctrl Pts',(-15.303495160707,-14.2112679809312,
115.92414544209)) ;
#186036 = CARTESIAN_POINT('Ctrl Pts',(-15.3772989994319,-14.2112679658761,
115.899914386104)) ;
#186037 = CARTESIAN_POINT('Ctrl Pts',(-15.3947103578552,-14.1598247969233,
115.952946574138)) ;
#186038 = CARTESIAN_POINT('Ctrl Pts',(-15.4546404114478,-14.3448019435796,
116.171044680752)) ;
#186039 = CARTESIAN_POINT('Ctrl Pts',(-15.4671576233587,-14.2803646984367,
116.209170088335)) ;
#186040 = CARTESIAN_POINT('Ctrl Pts',(-15.3933537835408,-14.2803647047343,
116.233401140992)) ;
#186041 = CARTESIAN_POINT('Ctrl Pts',(-15.3195499437229,-14.2803647110319,
116.257632193649)) ;
#186042 = CARTESIAN_POINT('Ctrl Pts',(-15.307032731812,-14.3448019561748,
116.219506786067)) ;
#186043 = CARTESIAN_POINT('Ctrl Pts',(-15.2945155199011,-14.4092392013176,
116.181381378484)) ;
#186044 = CARTESIAN_POINT('Ctrl Pts',(-15.368319359719,-14.40923919502,116.157150325827)) ;
#186045 = CARTESIAN_POINT('Ctrl Pts',(-15.4421231995369,-14.4092391887224,
116.13291927317)) ;
#186046 = CARTESIAN_POINT('Ctrl Pts',(-15.4546404114478,-14.3448019435796,
116.171044680752)) ;
#186047 = CARTESIAN_POINT('Ctrl Pts',(-15.527126191388,-14.4625579261475,
116.427260546478)) ;
#186048 = CARTESIAN_POINT('Ctrl Pts',(-15.5338675385338,-14.3898012184393,
116.447793602035)) ;
#186049 = CARTESIAN_POINT('Ctrl Pts',(-15.4600636972832,-14.3898012199962,
116.472024650328)) ;
#186050 = CARTESIAN_POINT('Ctrl Pts',(-15.3862598560326,-14.3898012215531,
116.496255698622)) ;
#186051 = CARTESIAN_POINT('Ctrl Pts',(-15.3795185088869,-14.4625579292612,
116.475722643065)) ;
#186052 = CARTESIAN_POINT('Ctrl Pts',(-15.3727771617411,-14.5353146369693,
116.455189587508)) ;
#186053 = CARTESIAN_POINT('Ctrl Pts',(-15.4465810029917,-14.5353146354125,
116.430958539215)) ;
#186054 = CARTESIAN_POINT('Ctrl Pts',(-15.5203848442423,-14.5353146338556,
116.406727490921)) ;
#186055 = CARTESIAN_POINT('Ctrl Pts',(-15.527126191388,-14.4625579261475,
116.427260546478)) ;
#186056 = CARTESIAN_POINT('Ctrl Pts',(-15.6061068479536,-14.5058691718866,
116.703142474044)) ;
#186057 = CARTESIAN_POINT('Ctrl Pts',(-15.6066125191928,-14.4299792998369,
116.704682666998)) ;
#186058 = CARTESIAN_POINT('Ctrl Pts',(-15.5328086766044,-14.429979299475,
116.728913711217)) ;
#186059 = CARTESIAN_POINT('Ctrl Pts',(-15.4590048340161,-14.4299792991131,
116.753144755436)) ;
#186060 = CARTESIAN_POINT('Ctrl Pts',(-15.4584991627769,-14.5058691711628,
116.751604562482)) ;
#186061 = CARTESIAN_POINT('Ctrl Pts',(-15.4579934915378,-14.5817590432124,
116.750064369528)) ;
#186062 = CARTESIAN_POINT('Ctrl Pts',(-15.5317973341261,-14.5817590435743,
116.725833325309)) ;
#186063 = CARTESIAN_POINT('Ctrl Pts',(-15.6056011767145,-14.5817590439362,
116.70160228109)) ;
#186064 = CARTESIAN_POINT('Ctrl Pts',(-15.6061068479536,-14.5058691718866,
116.703142474044)) ;
#186065 = CARTESIAN_POINT('Ctrl Pts',(-15.6860762715054,-14.471221053196,
116.98231319858)) ;
#186066 = CARTESIAN_POINT('Ctrl Pts',(-15.6802618468492,-14.3976366078093,
116.964603399263)) ;
#186067 = CARTESIAN_POINT('Ctrl Pts',(-15.6064580029253,-14.397636607939,
116.988834439414)) ;
#186068 = CARTESIAN_POINT('Ctrl Pts',(-15.5326541590014,-14.3976366080687,
117.013065479565)) ;
#186069 = CARTESIAN_POINT('Ctrl Pts',(-15.5384685836576,-14.4712210534553,
117.030775278883)) ;
#186070 = CARTESIAN_POINT('Ctrl Pts',(-15.5442830083138,-14.5448054988419,
117.0484850782)) ;
#186071 = CARTESIAN_POINT('Ctrl Pts',(-15.6180868522377,-14.5448054987123,
117.024254038049)) ;
#186072 = CARTESIAN_POINT('Ctrl Pts',(-15.6918906961616,-14.5448054985826,
117.000022997898)) ;
#186073 = CARTESIAN_POINT('Ctrl Pts',(-15.6860762715054,-14.471221053196,
116.98231319858)) ;
#186074 = CARTESIAN_POINT('Ctrl Pts',(-15.7595355968029,-14.3613267795073,
117.241458486077)) ;
#186075 = CARTESIAN_POINT('Ctrl Pts',(-15.7478503794398,-14.2953066789367,
117.205867199456)) ;
#186076 = CARTESIAN_POINT('Ctrl Pts',(-15.6740465351294,-14.2953066805575,
117.23009823843)) ;
#186077 = CARTESIAN_POINT('Ctrl Pts',(-15.6002426908189,-14.2953066821784,
117.254329277403)) ;
#186078 = CARTESIAN_POINT('Ctrl Pts',(-15.611927908182,-14.361326782749,117.289920564025)) ;
#186079 = CARTESIAN_POINT('Ctrl Pts',(-15.6236131255451,-14.4273468833197,
117.325511850646)) ;
#186080 = CARTESIAN_POINT('Ctrl Pts',(-15.6974169698556,-14.4273468816988,
117.301280811672)) ;
#186081 = CARTESIAN_POINT('Ctrl Pts',(-15.771220814166,-14.4273468800779,
117.277049772699)) ;
#186082 = CARTESIAN_POINT('Ctrl Pts',(-15.7595355968029,-14.3613267795073,
117.241458486077)) ;
#186083 = CARTESIAN_POINT('Ctrl Pts',(-15.8211678092068,-14.1831445066676,
117.464752006046)) ;
#186084 = CARTESIAN_POINT('Ctrl Pts',(-15.8044252431337,-14.1294690686809,
117.413756851243)) ;
#186085 = CARTESIAN_POINT('Ctrl Pts',(-15.7306213991478,-14.1294690707301,
117.437987891205)) ;
#186086 = CARTESIAN_POINT('Ctrl Pts',(-15.6568175551618,-14.1294690727794,
117.462218931167)) ;
#186087 = CARTESIAN_POINT('Ctrl Pts',(-15.6735601212348,-14.1831445107661,
117.513214085969)) ;
#186088 = CARTESIAN_POINT('Ctrl Pts',(-15.6903026873078,-14.2368199487529,
117.564209240772)) ;
#186089 = CARTESIAN_POINT('Ctrl Pts',(-15.7641065312938,-14.2368199467036,
117.53997820081)) ;
#186090 = CARTESIAN_POINT('Ctrl Pts',(-15.8379103752798,-14.2368199446543,
117.515747160848)) ;
#186091 = CARTESIAN_POINT('Ctrl Pts',(-15.8211678092068,-14.1831445066676,
117.464752006046)) ;
#186092 = CARTESIAN_POINT('Ctrl Pts',(-15.8652118608313,-13.9512771233317,
117.634264239109)) ;
#186093 = CARTESIAN_POINT('Ctrl Pts',(-15.8446375283888,-13.9137135164908,
117.571598142153)) ;
#186094 = CARTESIAN_POINT('Ctrl Pts',(-15.7708336850023,-13.9137135169973,
117.59582918394)) ;
#186095 = CARTESIAN_POINT('Ctrl Pts',(-15.6970298416157,-13.9137135175038,
117.620060225728)) ;
#186096 = CARTESIAN_POINT('Ctrl Pts',(-15.7176041740582,-13.9512771243447,
117.682726322684)) ;
#186097 = CARTESIAN_POINT('Ctrl Pts',(-15.7381785065007,-13.9888407311855,
117.74539241964)) ;
#186098 = CARTESIAN_POINT('Ctrl Pts',(-15.8119823498873,-13.988840730679,
117.721161377852)) ;
#186099 = CARTESIAN_POINT('Ctrl Pts',(-15.8857861932738,-13.9888407301726,
117.696930336064)) ;
#186100 = CARTESIAN_POINT('Ctrl Pts',(-15.8652118608313,-13.9512771233317,
117.634264239109)) ;
#186101 = CARTESIAN_POINT('Ctrl Pts',(-15.8882370524503,-13.6804917592119,
117.739885224289)) ;
#186102 = CARTESIAN_POINT('Ctrl Pts',(-15.8652903721225,-13.6617810820817,
117.669993338368)) ;
#186103 = CARTESIAN_POINT('Ctrl Pts',(-15.7914865291288,-13.6617810784038,
117.694224381352)) ;
#186104 = CARTESIAN_POINT('Ctrl Pts',(-15.717682686135,-13.6617810747259,
117.718455424336)) ;
#186105 = CARTESIAN_POINT('Ctrl Pts',(-15.7406293664628,-13.6804917518562,
117.788347310257)) ;
#186106 = CARTESIAN_POINT('Ctrl Pts',(-15.7635760467906,-13.6992024289864,
117.858239196178)) ;
#186107 = CARTESIAN_POINT('Ctrl Pts',(-15.8373798897843,-13.6992024326643,
117.834008153193)) ;
#186108 = CARTESIAN_POINT('Ctrl Pts',(-15.9111837327781,-13.6992024363421,
117.809777110209)) ;
#186109 = CARTESIAN_POINT('Ctrl Pts',(-15.8882370524503,-13.6804917592119,
117.739885224289)) ;
#186110 = CARTESIAN_POINT('Ctrl Pts',(-15.8876883146916,-13.3916820675785,
117.773598447878)) ;
#186111 = CARTESIAN_POINT('Ctrl Pts',(-15.8640143289905,-13.3931100750182,
117.701491307042)) ;
#186112 = CARTESIAN_POINT('Ctrl Pts',(-15.7902104856931,-13.3931100660094,
117.725722349101)) ;
#186113 = CARTESIAN_POINT('Ctrl Pts',(-15.7164066423956,-13.3931100570005,
117.74995339116)) ;
#186114 = CARTESIAN_POINT('Ctrl Pts',(-15.7400806280968,-13.3916820495608,
117.822060531996)) ;
#186115 = CARTESIAN_POINT('Ctrl Pts',(-15.7637546137979,-13.390254042121,
117.894167672832)) ;
#186116 = CARTESIAN_POINT('Ctrl Pts',(-15.8375584570953,-13.3902540511299,
117.869936630773)) ;
#186117 = CARTESIAN_POINT('Ctrl Pts',(-15.9113623003928,-13.3902540601387,
117.845705588714)) ;
#186118 = CARTESIAN_POINT('Ctrl Pts',(-15.8876883146916,-13.3916820675785,
117.773598447878)) ;
#186119 = CARTESIAN_POINT('Ctrl Pts',(-15.8627383173475,-13.10326146677,117.733182994211)) ;
#186120 = CARTESIAN_POINT('Ctrl Pts',(-15.8400356809096,-13.1248302660667,
117.664034426357)) ;
#186121 = CARTESIAN_POINT('Ctrl Pts',(-15.7662318362027,-13.12483024999,117.688265464123)) ;
#186122 = CARTESIAN_POINT('Ctrl Pts',(-15.6924279914958,-13.1248302339134,
117.712496501889)) ;
#186123 = CARTESIAN_POINT('Ctrl Pts',(-15.7151306279336,-13.1032614346168,
117.781645069743)) ;
#186124 = CARTESIAN_POINT('Ctrl Pts',(-15.7378332643715,-13.0816926353201,
117.850793637597)) ;
#186125 = CARTESIAN_POINT('Ctrl Pts',(-15.8116371090784,-13.0816926513967,
117.82656259983)) ;
#186126 = CARTESIAN_POINT('Ctrl Pts',(-15.8854409537853,-13.0816926674734,
117.802331562064)) ;
#186127 = CARTESIAN_POINT('Ctrl Pts',(-15.8627383173475,-13.10326146677,117.733182994211)) ;
#186128 = CARTESIAN_POINT('Ctrl Pts',(-15.8145961245661,-12.8385043736975,
117.621981799066)) ;
#186129 = CARTESIAN_POINT('Ctrl Pts',(-15.794488798957,-12.8785902983801,
117.560738129102)) ;
#186130 = CARTESIAN_POINT('Ctrl Pts',(-15.7206849517495,-12.8785902776547,
117.584969159251)) ;
#186131 = CARTESIAN_POINT('Ctrl Pts',(-15.6468811045419,-12.8785902569293,
117.609200189401)) ;
#186132 = CARTESIAN_POINT('Ctrl Pts',(-15.6669884301511,-12.8385043322466,
117.670443859365)) ;
#186133 = CARTESIAN_POINT('Ctrl Pts',(-15.6870957557602,-12.7984184075639,
117.73168752933)) ;
#186134 = CARTESIAN_POINT('Ctrl Pts',(-15.7608996029678,-12.7984184282893,
117.70745649918)) ;
#186135 = CARTESIAN_POINT('Ctrl Pts',(-15.8347034501753,-12.7984184490148,
117.683225469031)) ;
#186136 = CARTESIAN_POINT('Ctrl Pts',(-15.8145961245661,-12.8385043736975,
117.621981799066)) ;
#186137 = CARTESIAN_POINT('Ctrl Pts',(-15.7456754097843,-12.6146172171064,
117.447606611484)) ;
#186138 = CARTESIAN_POINT('Ctrl Pts',(-15.7296155103452,-12.6703934014124,
117.398690748409)) ;
#186139 = CARTESIAN_POINT('Ctrl Pts',(-15.655811659486,-12.6703933786195,
117.422921767436)) ;
#186140 = CARTESIAN_POINT('Ctrl Pts',(-15.5820078086268,-12.6703933558266,
117.447152786463)) ;
#186141 = CARTESIAN_POINT('Ctrl Pts',(-15.598067708066,-12.6146171715207,
117.496068649538)) ;
#186142 = CARTESIAN_POINT('Ctrl Pts',(-15.6141276075051,-12.5588409872148,
117.544984512613)) ;
#186143 = CARTESIAN_POINT('Ctrl Pts',(-15.6879314583643,-12.5588410100077,
117.520753493586)) ;
#186144 = CARTESIAN_POINT('Ctrl Pts',(-15.7617353092235,-12.5588410328005,
117.496522474558)) ;
#186145 = CARTESIAN_POINT('Ctrl Pts',(-15.7456754097843,-12.6146172171064,
117.447606611484)) ;
#186146 = CARTESIAN_POINT('Ctrl Pts',(-15.6606952599714,-12.4490452703409,
117.224157743888)) ;
#186147 = CARTESIAN_POINT('Ctrl Pts',(-15.6498132626341,-12.5164621248353,
117.191012935012)) ;
#186148 = CARTESIAN_POINT('Ctrl Pts',(-15.5760094079726,-12.5164621055273,
117.215243942458)) ;
#186149 = CARTESIAN_POINT('Ctrl Pts',(-15.5022055533111,-12.5164620862193,
117.239474949904)) ;
#186150 = CARTESIAN_POINT('Ctrl Pts',(-15.5130875506483,-12.449045231725,
117.27261975878)) ;
#186151 = CARTESIAN_POINT('Ctrl Pts',(-15.5239695479856,-12.3816283772306,
117.305764567655)) ;
#186152 = CARTESIAN_POINT('Ctrl Pts',(-15.5977734026471,-12.3816283965386,
117.28153356021)) ;
#186153 = CARTESIAN_POINT('Ctrl Pts',(-15.6715772573086,-12.3816284158465,
117.257302552764)) ;
#186154 = CARTESIAN_POINT('Ctrl Pts',(-15.6606952599714,-12.4490452703409,
117.224157743888)) ;
#186155 = CARTESIAN_POINT('Ctrl Pts',(-15.5642062371029,-12.3524023594542,
116.965836028037)) ;
#186156 = CARTESIAN_POINT('Ctrl Pts',(-15.5593092972053,-12.4266644816829,
116.950920738249)) ;
#186157 = CARTESIAN_POINT('Ctrl Pts',(-15.4855054383831,-12.4266644707959,
116.975151733023)) ;
#186158 = CARTESIAN_POINT('Ctrl Pts',(-15.4117015795609,-12.4266644599088,
116.999382727796)) ;
#186159 = CARTESIAN_POINT('Ctrl Pts',(-15.4165985194586,-12.3524023376801,
117.014298017584)) ;
#186160 = CARTESIAN_POINT('Ctrl Pts',(-15.4214954593561,-12.2781402154514,
117.029213307372)) ;
#186161 = CARTESIAN_POINT('Ctrl Pts',(-15.4952993181783,-12.2781402263384,
117.004982312599)) ;
#186162 = CARTESIAN_POINT('Ctrl Pts',(-15.5691031770005,-12.2781402372254,
116.980751317825)) ;
#186163 = CARTESIAN_POINT('Ctrl Pts',(-15.5642062371029,-12.3524023594542,
116.965836028037)) ;
#186164 = CARTESIAN_POINT('Ctrl Pts',(-15.4635911617765,-12.3322917866331,
116.694660585488)) ;
#186165 = CARTESIAN_POINT('Ctrl Pts',(-15.4649819187286,-12.4080647606153,
116.698896605655)) ;
#186166 = CARTESIAN_POINT('Ctrl Pts',(-15.3911780574036,-12.4080647636104,
116.723127592805)) ;
#186167 = CARTESIAN_POINT('Ctrl Pts',(-15.3173741960785,-12.4080647666054,
116.747358579955)) ;
#186168 = CARTESIAN_POINT('Ctrl Pts',(-15.3159834391265,-12.3322917926232,
116.743122559788)) ;
#186169 = CARTESIAN_POINT('Ctrl Pts',(-15.3145926821743,-12.256518818641,
116.73888653962)) ;
#186170 = CARTESIAN_POINT('Ctrl Pts',(-15.3883965434994,-12.256518815646,
116.71465555247)) ;
#186171 = CARTESIAN_POINT('Ctrl Pts',(-15.4622004048243,-12.2565188126509,
116.69042456532)) ;
#186172 = CARTESIAN_POINT('Ctrl Pts',(-15.4635911617765,-12.3322917866331,
116.694660585488)) ;
#186173 = CARTESIAN_POINT('Ctrl Pts',(-15.363777095621,-12.3899082998251,
116.426207229955)) ;
#186174 = CARTESIAN_POINT('Ctrl Pts',(-15.3714027978846,-12.4617684939858,
116.449433887356)) ;
#186175 = CARTESIAN_POINT('Ctrl Pts',(-15.2975989347207,-12.4617685151837,
116.473664868905)) ;
#186176 = CARTESIAN_POINT('Ctrl Pts',(-15.2237950715568,-12.4617685363815,
116.497895850454)) ;
#186177 = CARTESIAN_POINT('Ctrl Pts',(-15.2161693692933,-12.3899083422208,
116.474669193054)) ;
#186178 = CARTESIAN_POINT('Ctrl Pts',(-15.2085436670297,-12.3180481480601,
116.451442535653)) ;
#186179 = CARTESIAN_POINT('Ctrl Pts',(-15.2823475301936,-12.3180481268623,
116.427211554104)) ;
#186180 = CARTESIAN_POINT('Ctrl Pts',(-15.3561513933575,-12.3180481056645,
116.402980572555)) ;
#186181 = CARTESIAN_POINT('Ctrl Pts',(-15.363777095621,-12.3899082998251,
116.426207229955)) ;
#186182 = CARTESIAN_POINT('Ctrl Pts',(-15.2724808702363,-12.5204817202917,
116.18346404372)) ;
#186183 = CARTESIAN_POINT('Ctrl Pts',(-15.2857605963654,-12.5833292491025,
116.223911945411)) ;
#186184 = CARTESIAN_POINT('Ctrl Pts',(-15.211956733883,-12.5833292901703,
116.248142929035)) ;
#186185 = CARTESIAN_POINT('Ctrl Pts',(-15.1381528714006,-12.5833293312382,
116.27237391266)) ;
#186186 = CARTESIAN_POINT('Ctrl Pts',(-15.1248731452714,-12.5204818024274,
116.231926010969)) ;
#186187 = CARTESIAN_POINT('Ctrl Pts',(-15.1115934191423,-12.4576342736166,
116.191478109279)) ;
#186188 = CARTESIAN_POINT('Ctrl Pts',(-15.1853972816247,-12.4576342325488,
116.167247125654)) ;
#186189 = CARTESIAN_POINT('Ctrl Pts',(-15.2592011441071,-12.457634191481,
116.143016142029)) ;
#186190 = CARTESIAN_POINT('Ctrl Pts',(-15.2724808702363,-12.5204817202917,
116.18346404372)) ;
#186191 = CARTESIAN_POINT('Ctrl Pts',(-15.1942105603966,-12.7170079033734,
115.980733336847)) ;
#186192 = CARTESIAN_POINT('Ctrl Pts',(-15.2122362128416,-12.7662262828423,
116.035636564168)) ;
#186193 = CARTESIAN_POINT('Ctrl Pts',(-15.1384323526754,-12.7662263456653,
116.059867554848)) ;
#186194 = CARTESIAN_POINT('Ctrl Pts',(-15.0646284925093,-12.7662264084883,
116.084098545527)) ;
#186195 = CARTESIAN_POINT('Ctrl Pts',(-15.0466028400643,-12.7170080290195,
116.029195318206)) ;
#186196 = CARTESIAN_POINT('Ctrl Pts',(-15.0285771876193,-12.6677896495507,
115.974292090885)) ;
#186197 = CARTESIAN_POINT('Ctrl Pts',(-15.1023810477854,-12.6677895867277,
115.950061100206)) ;
#186198 = CARTESIAN_POINT('Ctrl Pts',(-15.1761849079516,-12.6677895239046,
115.925830109526)) ;
#186199 = CARTESIAN_POINT('Ctrl Pts',(-15.1942105603966,-12.7170079033734,
115.980733336847)) ;
#186200 = CARTESIAN_POINT('Ctrl Pts',(-15.1352265619382,-12.9615280720901,
115.836366093429)) ;
#186201 = CARTESIAN_POINT('Ctrl Pts',(-15.1566661866156,-12.9937459693296,
115.901667729225)) ;
#186202 = CARTESIAN_POINT('Ctrl Pts',(-15.0828623315335,-12.9937460490588,
115.92589873539)) ;
#186203 = CARTESIAN_POINT('Ctrl Pts',(-15.0090584764514,-12.9937461287879,
115.950129741554)) ;
#186204 = CARTESIAN_POINT('Ctrl Pts',(-14.987618851774,-12.9615282315483,
115.884828105759)) ;
#186205 = CARTESIAN_POINT('Ctrl Pts',(-14.9661792270966,-12.9293103343088,
115.819526469964)) ;
#186206 = CARTESIAN_POINT('Ctrl Pts',(-15.0399830821787,-12.9293102545796,
115.795295463799)) ;
#186207 = CARTESIAN_POINT('Ctrl Pts',(-15.1137869372607,-12.9293101748505,
115.771064457634)) ;
#186208 = CARTESIAN_POINT('Ctrl Pts',(-15.1352265619382,-12.9615280720901,
115.836366093429)) ;
#186209 = CARTESIAN_POINT('Ctrl Pts',(-15.0978086326599,-13.241668548695,
115.758096626062)) ;
#186210 = CARTESIAN_POINT('Ctrl Pts',(-15.1211533914122,-13.2543754677215,
115.829200992715)) ;
#186211 = CARTESIAN_POINT('Ctrl Pts',(-15.0473495430318,-13.2543755617733,
115.853432019292)) ;
#186212 = CARTESIAN_POINT('Ctrl Pts',(-14.9735456946513,-13.2543756558251,
115.877663045869)) ;
#186213 = CARTESIAN_POINT('Ctrl Pts',(-14.9502009358991,-13.2416687367986,
115.806558679216)) ;
#186214 = CARTESIAN_POINT('Ctrl Pts',(-14.9268561771469,-13.228961817772,
115.735454312564)) ;
#186215 = CARTESIAN_POINT('Ctrl Pts',(-15.0006600255273,-13.2289617237202,
115.711223285987)) ;
#186216 = CARTESIAN_POINT('Ctrl Pts',(-15.0744638739077,-13.2289616296684,
115.68699225941)) ;
#186217 = CARTESIAN_POINT('Ctrl Pts',(-15.0978086326599,-13.241668548695,
115.758096626062)) ;
#186218 = CARTESIAN_POINT('Ctrl Pts',(-15.084760361114,-13.5312927388049,
115.753637119194)) ;
#186219 = CARTESIAN_POINT('Ctrl Pts',(-15.1083199747751,-13.5237974675911,
115.825395899159)) ;
#186220 = CARTESIAN_POINT('Ctrl Pts',(-15.0345161345071,-13.5237975662632,
115.849626950445)) ;
#186221 = CARTESIAN_POINT('Ctrl Pts',(-14.9607122942391,-13.5237976649353,
115.873858001731)) ;
#186222 = CARTESIAN_POINT('Ctrl Pts',(-14.9371526805781,-13.5312929361492,
115.802099221766)) ;
#186223 = CARTESIAN_POINT('Ctrl Pts',(-14.913593066917,-13.538788207363,115.730340441801)) ;
#186224 = CARTESIAN_POINT('Ctrl Pts',(-14.987396907185,-13.5387881086909,
115.706109390515)) ;
#186225 = CARTESIAN_POINT('Ctrl Pts',(-15.061200747453,-13.5387880100187,
115.681878339228)) ;
#186226 = CARTESIAN_POINT('Ctrl Pts',(-15.084760361114,-13.5312927388049,
115.753637119194)) ;
#186227 = CARTESIAN_POINT('Ctrl Pts',(-15.0956720661844,-13.8141856043051,
115.822335205277)) ;
#186228 = CARTESIAN_POINT('Ctrl Pts',(-15.1177705883915,-13.7869289146623,
115.889643736342)) ;
#186229 = CARTESIAN_POINT('Ctrl Pts',(-15.0439667566183,-13.7869290108332,
115.913874813502)) ;
#186230 = CARTESIAN_POINT('Ctrl Pts',(-14.9701629248451,-13.7869291070041,
115.938105890662)) ;
#186231 = CARTESIAN_POINT('Ctrl Pts',(-14.9480644026381,-13.8141857966469,
115.870797359597)) ;
#186232 = CARTESIAN_POINT('Ctrl Pts',(-14.925965880431,-13.8414424862897,
115.803488828531)) ;
#186233 = CARTESIAN_POINT('Ctrl Pts',(-14.9997697122042,-13.8414423901188,
115.779257751371)) ;
#186234 = CARTESIAN_POINT('Ctrl Pts',(-15.0735735439773,-13.8414422939479,
115.755026674211)) ;
#186235 = CARTESIAN_POINT('Ctrl Pts',(-15.0956720661844,-13.8141856043051,
115.822335205277)) ;
#186236 = CARTESIAN_POINT('Ctrl Pts',(-15.1292184993136,-14.0686273114668,
115.959949911345)) ;
#186237 = CARTESIAN_POINT('Ctrl Pts',(-15.1482741234775,-14.0235664995227,
116.017990265886)) ;
#186238 = CARTESIAN_POINT('Ctrl Pts',(-15.0744702998026,-14.0235665846011,
116.042221367712)) ;
#186239 = CARTESIAN_POINT('Ctrl Pts',(-15.0006664761278,-14.0235666696795,
116.066452469538)) ;
#186240 = CARTESIAN_POINT('Ctrl Pts',(-14.9816108519638,-14.0686274816236,
116.008412114997)) ;
#186241 = CARTESIAN_POINT('Ctrl Pts',(-14.9625552277998,-14.1136882935678,
115.950371760456)) ;
#186242 = CARTESIAN_POINT('Ctrl Pts',(-15.0363590514747,-14.1136882084894,
115.92614065863)) ;
#186243 = CARTESIAN_POINT('Ctrl Pts',(-15.1101628751496,-14.113688123411,
115.901909556804)) ;
#186244 = CARTESIAN_POINT('Ctrl Pts',(-15.1292184993136,-14.0686273114668,
115.959949911345)) ;
#186245 = CARTESIAN_POINT('Ctrl Pts',(-15.1825001129318,-14.2772225776637,
116.157827602682)) ;
#186246 = CARTESIAN_POINT('Ctrl Pts',(-15.1971276181691,-14.2175318931739,
116.202380621409)) ;
#186247 = CARTESIAN_POINT('Ctrl Pts',(-15.1233238013441,-14.2175319594466,
116.226611744099)) ;
#186248 = CARTESIAN_POINT('Ctrl Pts',(-15.0495199845191,-14.2175320257193,
116.250842866789)) ;
#186249 = CARTESIAN_POINT('Ctrl Pts',(-15.0348924792818,-14.2772227102091,
116.206289848062)) ;
#186250 = CARTESIAN_POINT('Ctrl Pts',(-15.0202649740445,-14.3369133946989,
116.161736829335)) ;
#186251 = CARTESIAN_POINT('Ctrl Pts',(-15.0940687908695,-14.3369133284262,
116.137505706645)) ;
#186252 = CARTESIAN_POINT('Ctrl Pts',(-15.1678726076945,-14.3369132621536,
116.113274583955)) ;
#186253 = CARTESIAN_POINT('Ctrl Pts',(-15.1825001129318,-14.2772225776637,
116.157827602682)) ;
#186254 = CARTESIAN_POINT('Ctrl Pts',(-15.2502956526181,-14.4229662306659,
116.399664973007)) ;
#186255 = CARTESIAN_POINT('Ctrl Pts',(-15.2594801383945,-14.3530122150386,
116.427639432676)) ;
#186256 = CARTESIAN_POINT('Ctrl Pts',(-15.1856763262186,-14.3530122565041,
116.451870569526)) ;
#186257 = CARTESIAN_POINT('Ctrl Pts',(-15.1118725140427,-14.3530122979697,
116.476101706376)) ;
#186258 = CARTESIAN_POINT('Ctrl Pts',(-15.1026880282663,-14.4229663135971,
116.448127246707)) ;
#186259 = CARTESIAN_POINT('Ctrl Pts',(-15.0935035424898,-14.4929203292244,
116.420152787038)) ;
#186260 = CARTESIAN_POINT('Ctrl Pts',(-15.1673073546657,-14.4929202877588,
116.395921650188)) ;
#186261 = CARTESIAN_POINT('Ctrl Pts',(-15.2411111668416,-14.4929202462933,
116.371690513338)) ;
#186262 = CARTESIAN_POINT('Ctrl Pts',(-15.2502956526181,-14.4229662306659,
116.399664973007)) ;
#186263 = CARTESIAN_POINT('Ctrl Pts',(-15.3275171004924,-14.4976749709137,
116.670306720102)) ;
#186264 = CARTESIAN_POINT('Ctrl Pts',(-15.3305906375755,-14.4224014624097,
116.679668216054)) ;
#186265 = CARTESIAN_POINT('Ctrl Pts',(-15.2567868276272,-14.4224014756821,
116.70389935969)) ;
#186266 = CARTESIAN_POINT('Ctrl Pts',(-15.182983017679,-14.4224014889544,
116.728130503325)) ;
#186267 = CARTESIAN_POINT('Ctrl Pts',(-15.179909480596,-14.4976749974584,
116.718769007372)) ;
#186268 = CARTESIAN_POINT('Ctrl Pts',(-15.176835943513,-14.5729485059623,
116.70940751142)) ;
#186269 = CARTESIAN_POINT('Ctrl Pts',(-15.2506397534612,-14.57294849269,116.685176367784)) ;
#186270 = CARTESIAN_POINT('Ctrl Pts',(-15.3244435634094,-14.5729484794176,
116.660945224149)) ;
#186271 = CARTESIAN_POINT('Ctrl Pts',(-15.3275171004924,-14.4976749709137,
116.670306720102)) ;
#186272 = CARTESIAN_POINT('Ctrl Pts',(-15.4083349615168,-14.4944851703305,
116.952154625279)) ;
#186273 = CARTESIAN_POINT('Ctrl Pts',(-15.4050322512228,-14.4193216059584,
116.942095100569)) ;
#186274 = CARTESIAN_POINT('Ctrl Pts',(-15.3312284404642,-14.4193215903829,
116.966326241736)) ;
#186275 = CARTESIAN_POINT('Ctrl Pts',(-15.2574246297056,-14.4193215748074,
116.990557382903)) ;
#186276 = CARTESIAN_POINT('Ctrl Pts',(-15.2607273399995,-14.4944851391795,
117.000616907613)) ;
#186277 = CARTESIAN_POINT('Ctrl Pts',(-15.2640300502934,-14.5696487035515,
117.010676432323)) ;
#186278 = CARTESIAN_POINT('Ctrl Pts',(-15.3378338610521,-14.5696487191271,
116.986445291156)) ;
#186279 = CARTESIAN_POINT('Ctrl Pts',(-15.4116376718107,-14.5696487347026,
116.962214149989)) ;
#186280 = CARTESIAN_POINT('Ctrl Pts',(-15.4083349615168,-14.4944851703305,
116.952154625279)) ;
#186281 = CARTESIAN_POINT('Ctrl Pts',(-15.4846889044359,-14.4147277655596,
117.219968470872)) ;
#186282 = CARTESIAN_POINT('Ctrl Pts',(-15.4753209992311,-14.3450211180556,
117.191435341122)) ;
#186283 = CARTESIAN_POINT('Ctrl Pts',(-15.4015171853854,-14.3450210762549,
117.215666472886)) ;
#186284 = CARTESIAN_POINT('Ctrl Pts',(-15.3277133715397,-14.3450210344541,
117.23989760465)) ;
#186285 = CARTESIAN_POINT('Ctrl Pts',(-15.3370812767445,-14.4147276819581,
117.2684307344)) ;
#186286 = CARTESIAN_POINT('Ctrl Pts',(-15.3464491819492,-14.4844343294621,
117.29696386415)) ;
#186287 = CARTESIAN_POINT('Ctrl Pts',(-15.4202529957949,-14.4844343712628,
117.272732732386)) ;
#186288 = CARTESIAN_POINT('Ctrl Pts',(-15.4940568096406,-14.4844344130636,
117.248501600622)) ;
#186289 = CARTESIAN_POINT('Ctrl Pts',(-15.4846889044359,-14.4147277655596,
117.219968470872)) ;
#186290 = CARTESIAN_POINT('Ctrl Pts',(-15.5519059399888,-14.2631098096402,
117.460240523406)) ;
#186291 = CARTESIAN_POINT('Ctrl Pts',(-15.5370957241803,-14.2038841179929,
117.41513099375)) ;
#186292 = CARTESIAN_POINT('Ctrl Pts',(-15.4632919047968,-14.2038840550099,
117.439362108647)) ;
#186293 = CARTESIAN_POINT('Ctrl Pts',(-15.3894880854134,-14.203883992027,
117.463593223544)) ;
#186294 = CARTESIAN_POINT('Ctrl Pts',(-15.4042983012219,-14.2631096836743,
117.5087027532)) ;
#186295 = CARTESIAN_POINT('Ctrl Pts',(-15.4191085170304,-14.3223353753216,
117.553812282856)) ;
#186296 = CARTESIAN_POINT('Ctrl Pts',(-15.4929123364138,-14.3223354383045,
117.529581167959)) ;
#186297 = CARTESIAN_POINT('Ctrl Pts',(-15.5667161557973,-14.3223355012875,
117.505350053062)) ;
#186298 = CARTESIAN_POINT('Ctrl Pts',(-15.5519059399888,-14.2631098096402,
117.460240523406)) ;
#186299 = CARTESIAN_POINT('Ctrl Pts',(-15.6035818704614,-14.0515534840703,
117.653029803228)) ;
#186300 = CARTESIAN_POINT('Ctrl Pts',(-15.5844092168002,-14.0070094522688,
117.594632991836)) ;
#186301 = CARTESIAN_POINT('Ctrl Pts',(-15.5106053905118,-14.0070093747174,
117.618864085702)) ;
#186302 = CARTESIAN_POINT('Ctrl Pts',(-15.4368015642234,-14.007009297166,
117.643095179568)) ;
#186303 = CARTESIAN_POINT('Ctrl Pts',(-15.4559742178847,-14.0515533289676,
117.70149199096)) ;
#186304 = CARTESIAN_POINT('Ctrl Pts',(-15.4751468715459,-14.0960973607691,
117.759888802352)) ;
#186305 = CARTESIAN_POINT('Ctrl Pts',(-15.5489506978343,-14.0960974383204,
117.735657708486)) ;
#186306 = CARTESIAN_POINT('Ctrl Pts',(-15.6227545241227,-14.0960975158718,
117.711426614621)) ;
#186307 = CARTESIAN_POINT('Ctrl Pts',(-15.6035818704614,-14.0515534840703,
117.653029803228)) ;
#186308 = CARTESIAN_POINT('Ctrl Pts',(-15.6356848695643,-13.793288943793,
117.786406026282)) ;
#186309 = CARTESIAN_POINT('Ctrl Pts',(-15.6135053515169,-13.7667090894671,
117.718850791254)) ;
#186310 = CARTESIAN_POINT('Ctrl Pts',(-15.539701517435,-13.7667090063188,
117.743081861382)) ;
#186311 = CARTESIAN_POINT('Ctrl Pts',(-15.465897683353,-13.7667089231704,
117.76731293151)) ;
#186312 = CARTESIAN_POINT('Ctrl Pts',(-15.4880772014003,-13.7932887774963,
117.834868166537)) ;
#186313 = CARTESIAN_POINT('Ctrl Pts',(-15.5102567194477,-13.8198686318222,
117.902423401565)) ;
#186314 = CARTESIAN_POINT('Ctrl Pts',(-15.5840605535297,-13.8198687149705,
117.878192331437)) ;
#186315 = CARTESIAN_POINT('Ctrl Pts',(-15.6578643876116,-13.8198687981189,
117.853961261309)) ;
#186316 = CARTESIAN_POINT('Ctrl Pts',(-15.6356848695643,-13.793288943793,
117.786406026282)) ;
#186317 = CARTESIAN_POINT('Ctrl Pts',(-15.6447985101952,-13.5095097704303,
117.849560702245)) ;
#186318 = CARTESIAN_POINT('Ctrl Pts',(-15.6212168570663,-13.5027030390007,
117.777734790113)) ;
#186319 = CARTESIAN_POINT('Ctrl Pts',(-15.5474130156155,-13.5027029571053,
117.801965837796)) ;
#186320 = CARTESIAN_POINT('Ctrl Pts',(-15.4736091741646,-13.50270287521,117.826196885479)) ;
#186321 = CARTESIAN_POINT('Ctrl Pts',(-15.4971908272935,-13.5095096066396,
117.898022797612)) ;
#186322 = CARTESIAN_POINT('Ctrl Pts',(-15.5207724804223,-13.5163163380692,
117.969848709744)) ;
#186323 = CARTESIAN_POINT('Ctrl Pts',(-15.5945763218732,-13.5163164199646,
117.945617662061)) ;
#186324 = CARTESIAN_POINT('Ctrl Pts',(-15.668380163324,-13.5163165018599,
117.921386614378)) ;
#186325 = CARTESIAN_POINT('Ctrl Pts',(-15.6447985101952,-13.5095097704303,
117.849560702245)) ;
#186326 = CARTESIAN_POINT('Ctrl Pts',(-15.6297417008337,-13.218674427129,
117.839172279436)) ;
#186327 = CARTESIAN_POINT('Ctrl Pts',(-15.6064416512002,-13.2321633115492,
117.768204086257)) ;
#186328 = CARTESIAN_POINT('Ctrl Pts',(-15.5326378033173,-13.2321632381837,
117.79243511435)) ;
#186329 = CARTESIAN_POINT('Ctrl Pts',(-15.4588339554343,-13.2321631648182,
117.816666142442)) ;
#186330 = CARTESIAN_POINT('Ctrl Pts',(-15.4821340050678,-13.2186742803981,
117.887634335621)) ;
#186331 = CARTESIAN_POINT('Ctrl Pts',(-15.5054340547013,-13.2051853959779,
117.9586025288)) ;
#186332 = CARTESIAN_POINT('Ctrl Pts',(-15.5792379025843,-13.2051854693434,
117.934371500708)) ;
#186333 = CARTESIAN_POINT('Ctrl Pts',(-15.6530417504672,-13.2051855427089,
117.910140472615)) ;
#186334 = CARTESIAN_POINT('Ctrl Pts',(-15.6297417008337,-13.218674427129,
117.839172279436)) ;
#186335 = CARTESIAN_POINT('Ctrl Pts',(-15.5909058637976,-12.9425272619773,
117.756286254308)) ;
#186336 = CARTESIAN_POINT('Ctrl Pts',(-15.5695495533161,-12.9753170489684,
117.691238377106)) ;
#186337 = CARTESIAN_POINT('Ctrl Pts',(-15.4957457004882,-12.9753169887403,
117.715469390137)) ;
#186338 = CARTESIAN_POINT('Ctrl Pts',(-15.4219418476603,-12.9753169285121,
117.739700403168)) ;
#186339 = CARTESIAN_POINT('Ctrl Pts',(-15.4432981581418,-12.942527141521,
117.804748280369)) ;
#186340 = CARTESIAN_POINT('Ctrl Pts',(-15.4646544686234,-12.9097373545299,
117.86979615757)) ;
#186341 = CARTESIAN_POINT('Ctrl Pts',(-15.5384583214513,-12.9097374147581,
117.84556514454)) ;
#186342 = CARTESIAN_POINT('Ctrl Pts',(-15.6122621742792,-12.9097374749862,
117.821334131509)) ;
#186343 = CARTESIAN_POINT('Ctrl Pts',(-15.5909058637976,-12.9425272619773,
117.756286254308)) ;
#186344 = CARTESIAN_POINT('Ctrl Pts',(-15.5297839260892,-12.6990701230285,
117.605746240807)) ;
#186345 = CARTESIAN_POINT('Ctrl Pts',(-15.511925441269,-12.7489081846955,
117.55135217639)) ;
#186346 = CARTESIAN_POINT('Ctrl Pts',(-15.438121585841,-12.748908142065,117.575583181502)) ;
#186347 = CARTESIAN_POINT('Ctrl Pts',(-15.364317730413,-12.7489080994345,
117.599814186613)) ;
#186348 = CARTESIAN_POINT('Ctrl Pts',(-15.3821762152333,-12.6990700377675,
117.65420825103)) ;
#186349 = CARTESIAN_POINT('Ctrl Pts',(-15.4000347000535,-12.6492319761005,
117.708602315447)) ;
#186350 = CARTESIAN_POINT('Ctrl Pts',(-15.4738385554815,-12.649232018731,
117.684371310335)) ;
#186351 = CARTESIAN_POINT('Ctrl Pts',(-15.5476424109095,-12.6492320613615,
117.660140305224)) ;
#186352 = CARTESIAN_POINT('Ctrl Pts',(-15.5297839260892,-12.6990701230285,
117.605746240807)) ;
#186353 = CARTESIAN_POINT('Ctrl Pts',(-15.4511561549076,-12.5091750901202,
117.40151828196)) ;
#186354 = CARTESIAN_POINT('Ctrl Pts',(-15.438030988428,-12.5723470280859,
117.361541141619)) ;
#186355 = CARTESIAN_POINT('Ctrl Pts',(-15.3642271316641,-12.5723470007831,
117.385772142662)) ;
#186356 = CARTESIAN_POINT('Ctrl Pts',(-15.2904232749002,-12.5723469734802,
117.410003143704)) ;
#186357 = CARTESIAN_POINT('Ctrl Pts',(-15.3035484413797,-12.5091750355146,
117.449980284045)) ;
#186358 = CARTESIAN_POINT('Ctrl Pts',(-15.3166736078593,-12.4460030975489,
117.489957424385)) ;
#186359 = CARTESIAN_POINT('Ctrl Pts',(-15.3904774646233,-12.4460031248517,
117.465726423343)) ;
#186360 = CARTESIAN_POINT('Ctrl Pts',(-15.4642813213872,-12.4460031521546,
117.441495422301)) ;
#186361 = CARTESIAN_POINT('Ctrl Pts',(-15.4511561549076,-12.5091750901202,
117.40151828196)) ;
#186362 = CARTESIAN_POINT('Ctrl Pts',(-15.3584459875218,-12.3826566850404,
117.154731104865)) ;
#186363 = CARTESIAN_POINT('Ctrl Pts',(-15.3510375064598,-12.4547585599534,
117.132166066116)) ;
#186364 = CARTESIAN_POINT('Ctrl Pts',(-15.2772336508438,-12.4547585482587,
117.156397070654)) ;
#186365 = CARTESIAN_POINT('Ctrl Pts',(-15.2034297952278,-12.4547585365639,
117.180628075193)) ;
#186366 = CARTESIAN_POINT('Ctrl Pts',(-15.2108382762898,-12.3826566616509,
117.203193113943)) ;
#186367 = CARTESIAN_POINT('Ctrl Pts',(-15.2182467573518,-12.3105547867379,
117.225758152692)) ;
#186368 = CARTESIAN_POINT('Ctrl Pts',(-15.2920506129678,-12.3105547984326,
117.201527148153)) ;
#186369 = CARTESIAN_POINT('Ctrl Pts',(-15.3658544685838,-12.3105548101274,
117.177296143615)) ;
#186370 = CARTESIAN_POINT('Ctrl Pts',(-15.3584459875218,-12.3826566850404,
117.154731104865)) ;
#186371 = CARTESIAN_POINT('Ctrl Pts',(-15.2584754294207,-12.3310754563828,
116.885718823753)) ;
#186372 = CARTESIAN_POINT('Ctrl Pts',(-15.2573017097217,-12.4068883304643,
116.882143862309)) ;
#186373 = CARTESIAN_POINT('Ctrl Pts',(-15.1834978563234,-12.406888329813,
116.906374873603)) ;
#186374 = CARTESIAN_POINT('Ctrl Pts',(-15.1096940029252,-12.4068883291616,
116.930605884896)) ;
#186375 = CARTESIAN_POINT('Ctrl Pts',(-15.1108677226242,-12.3310754550801,
116.93418084634)) ;
#186376 = CARTESIAN_POINT('Ctrl Pts',(-15.1120414423232,-12.2552625809986,
116.937755807783)) ;
#186377 = CARTESIAN_POINT('Ctrl Pts',(-15.1858452957214,-12.25526258165,116.91352479649)) ;
#186378 = CARTESIAN_POINT('Ctrl Pts',(-15.2596491491197,-12.2552625823013,
116.889293785196)) ;
#186379 = CARTESIAN_POINT('Ctrl Pts',(-15.2584754294207,-12.3310754563828,
116.885718823753)) ;
#186380 = CARTESIAN_POINT('Ctrl Pts',(-15.1575649005721,-12.357364074466,
116.613810250569)) ;
#186381 = CARTESIAN_POINT('Ctrl Pts',(-15.1627017931781,-12.4314561765023,
116.629456396148)) ;
#186382 = CARTESIAN_POINT('Ctrl Pts',(-15.0888979425083,-12.4314561824614,
116.653687415753)) ;
#186383 = CARTESIAN_POINT('Ctrl Pts',(-15.0150940918386,-12.4314561884204,
116.677918435357)) ;
#186384 = CARTESIAN_POINT('Ctrl Pts',(-15.0099571992326,-12.3573640863842,
116.662272289777)) ;
#186385 = CARTESIAN_POINT('Ctrl Pts',(-15.0048203066266,-12.2832719843479,
116.646626144198)) ;
#186386 = CARTESIAN_POINT('Ctrl Pts',(-15.0786241572964,-12.2832719783889,
116.622395124594)) ;
#186387 = CARTESIAN_POINT('Ctrl Pts',(-15.1524280079661,-12.2832719724298,
116.59816410499)) ;
#186388 = CARTESIAN_POINT('Ctrl Pts',(-15.1575649005721,-12.357364074466,
116.613810250569)) ;
#186389 = CARTESIAN_POINT('Ctrl Pts',(-15.0622843285041,-12.4589530543375,
116.358945148846)) ;
#186390 = CARTESIAN_POINT('Ctrl Pts',(-15.0733504108087,-12.5260636075349,
116.392650649706)) ;
#186391 = CARTESIAN_POINT('Ctrl Pts',(-14.9995465627523,-12.5260636163209,
116.41688167727)) ;
#186392 = CARTESIAN_POINT('Ctrl Pts',(-14.9257427146959,-12.5260636251069,
116.441112704835)) ;
#186393 = CARTESIAN_POINT('Ctrl Pts',(-14.9146766323914,-12.4589530719095,
116.407407203975)) ;
#186394 = CARTESIAN_POINT('Ctrl Pts',(-14.9036105500868,-12.3918425187121,
116.373701703115)) ;
#186395 = CARTESIAN_POINT('Ctrl Pts',(-14.9774143981431,-12.3918425099261,
116.349470675551)) ;
#186396 = CARTESIAN_POINT('Ctrl Pts',(-15.0512182461995,-12.3918425011401,
116.325239647987)) ;
#186397 = CARTESIAN_POINT('Ctrl Pts',(-15.0622843285041,-12.4589530543375,
116.358945148846)) ;
#186398 = CARTESIAN_POINT('Ctrl Pts',(-14.9777630331864,-12.6306888766498,
116.137164147509)) ;
#186399 = CARTESIAN_POINT('Ctrl Pts',(-14.9940098346291,-12.6859095379068,
116.186649283117)) ;
#186400 = CARTESIAN_POINT('Ctrl Pts',(-14.9202059893101,-12.6859095445597,
116.210880319019)) ;
#186401 = CARTESIAN_POINT('Ctrl Pts',(-14.8464021439911,-12.6859095512127,
116.235111354921)) ;
#186402 = CARTESIAN_POINT('Ctrl Pts',(-14.8301553425484,-12.6306888899557,
116.185626219312)) ;
#186403 = CARTESIAN_POINT('Ctrl Pts',(-14.8139085411057,-12.5754682286988,
116.136141083704)) ;
#186404 = CARTESIAN_POINT('Ctrl Pts',(-14.8877123864247,-12.5754682220458,
116.111910047802)) ;
#186405 = CARTESIAN_POINT('Ctrl Pts',(-14.9615162317436,-12.5754682153929,
116.0876790119)) ;
#186406 = CARTESIAN_POINT('Ctrl Pts',(-14.9777630331864,-12.6306888766498,
116.137164147509)) ;
#186407 = CARTESIAN_POINT('Ctrl Pts',(-14.9108196105475,-12.8569331102211,
115.968557829525)) ;
#186408 = CARTESIAN_POINT('Ctrl Pts',(-14.9310347417438,-12.8964388496988,
116.030129857362)) ;
#186409 = CARTESIAN_POINT('Ctrl Pts',(-14.8572308977073,-12.8964388537721,
116.05436089717)) ;
#186410 = CARTESIAN_POINT('Ctrl Pts',(-14.7834270536708,-12.8964388578454,
116.078591936978)) ;
#186411 = CARTESIAN_POINT('Ctrl Pts',(-14.7632119224746,-12.8569331183677,
116.017019909141)) ;
#186412 = CARTESIAN_POINT('Ctrl Pts',(-14.7429967912783,-12.81742737889,115.955447881304)) ;
#186413 = CARTESIAN_POINT('Ctrl Pts',(-14.8168006353148,-12.8174273748167,
115.931216841496)) ;
#186414 = CARTESIAN_POINT('Ctrl Pts',(-14.8906044793512,-12.8174273707434,
115.906985801688)) ;
#186415 = CARTESIAN_POINT('Ctrl Pts',(-14.9108196105475,-12.8569331102211,
115.968557829525)) ;
#186416 = CARTESIAN_POINT('Ctrl Pts',(-14.8642028462685,-13.124308622433,
115.862054279518)) ;
#186417 = CARTESIAN_POINT('Ctrl Pts',(-14.8869691156441,-13.1452036324507,
115.931396662715)) ;
#186418 = CARTESIAN_POINT('Ctrl Pts',(-14.8131652723611,-13.1452036323883,
115.955627704818)) ;
#186419 = CARTESIAN_POINT('Ctrl Pts',(-14.739361429078,-13.1452036323259,
115.979858746921)) ;
#186420 = CARTESIAN_POINT('Ctrl Pts',(-14.7165951597023,-13.1243086223082,
115.910516363724)) ;
#186421 = CARTESIAN_POINT('Ctrl Pts',(-14.6938288903267,-13.1034136122904,
115.841173980526)) ;
#186422 = CARTESIAN_POINT('Ctrl Pts',(-14.7676327336098,-13.1034136123528,
115.816942938423)) ;
#186423 = CARTESIAN_POINT('Ctrl Pts',(-14.8414365768928,-13.1034136124152,
115.79271189632)) ;
#186424 = CARTESIAN_POINT('Ctrl Pts',(-14.8642028462685,-13.124308622433,
115.862054279518)) ;
#186425 = CARTESIAN_POINT('Ctrl Pts',(-14.8411123635601,-13.4140118065031,
115.82734739657)) ;
#186426 = CARTESIAN_POINT('Ctrl Pts',(-14.8647879122609,-13.4147080729357,
115.899459297934)) ;
#186427 = CARTESIAN_POINT('Ctrl Pts',(-14.7909840688978,-13.414708069978,
115.923690339793)) ;
#186428 = CARTESIAN_POINT('Ctrl Pts',(-14.7171802255347,-13.4147080670203,
115.947921381652)) ;
#186429 = CARTESIAN_POINT('Ctrl Pts',(-14.693504676834,-13.4140118005876,
115.875809480288)) ;
#186430 = CARTESIAN_POINT('Ctrl Pts',(-14.6698291281333,-13.413315534155,
115.803697578925)) ;
#186431 = CARTESIAN_POINT('Ctrl Pts',(-14.7436329714963,-13.4133155371127,
115.779466537066)) ;
#186432 = CARTESIAN_POINT('Ctrl Pts',(-14.8174368148594,-13.4133155400704,
115.755235495206)) ;
#186433 = CARTESIAN_POINT('Ctrl Pts',(-14.8411123635601,-13.4140118065031,
115.82734739657)) ;
#186434 = CARTESIAN_POINT('Ctrl Pts',(-14.8423364229059,-13.700942777731,
115.866314358884)) ;
#186435 = CARTESIAN_POINT('Ctrl Pts',(-14.8652321436292,-13.6816044417709,
115.936051030061)) ;
#186436 = CARTESIAN_POINT('Ctrl Pts',(-14.791428299926,-13.6816044385339,
115.960282070884)) ;
#186437 = CARTESIAN_POINT('Ctrl Pts',(-14.7176244562229,-13.6816044352969,
115.984513111707)) ;
#186438 = CARTESIAN_POINT('Ctrl Pts',(-14.6947287354995,-13.700942771257,
115.91477644053)) ;
#186439 = CARTESIAN_POINT('Ctrl Pts',(-14.6718330147762,-13.7202811072171,
115.845039769353)) ;
#186440 = CARTESIAN_POINT('Ctrl Pts',(-14.7456368584794,-13.7202811104541,
115.82080872853)) ;
#186441 = CARTESIAN_POINT('Ctrl Pts',(-14.8194407021826,-13.7202811136911,
115.796577687706)) ;
#186442 = CARTESIAN_POINT('Ctrl Pts',(-14.8423364229059,-13.700942777731,
115.866314358884)) ;
#186443 = CARTESIAN_POINT('Ctrl Pts',(-14.8671060908768,-13.9707477592159,
115.9774009813)) ;
#186444 = CARTESIAN_POINT('Ctrl Pts',(-14.8875684376904,-13.9325402407103,
116.039725988136)) ;
#186445 = CARTESIAN_POINT('Ctrl Pts',(-14.81376459397,-13.9325402395383,116.063957028906)) ;
#186446 = CARTESIAN_POINT('Ctrl Pts',(-14.7399607502495,-13.9325402383663,
116.088188069677)) ;
#186447 = CARTESIAN_POINT('Ctrl Pts',(-14.7194984034359,-13.9707477568719,
116.025863062841)) ;
#186448 = CARTESIAN_POINT('Ctrl Pts',(-14.6990360566222,-14.0089552753775,
115.963538056005)) ;
#186449 = CARTESIAN_POINT('Ctrl Pts',(-14.7728399003427,-14.0089552765495,
115.939307015234)) ;
#186450 = CARTESIAN_POINT('Ctrl Pts',(-14.8466437440631,-14.0089552777215,
115.915075974463)) ;
#186451 = CARTESIAN_POINT('Ctrl Pts',(-14.8671060908768,-13.9707477592159,
115.9774009813)) ;
#186452 = CARTESIAN_POINT('Ctrl Pts',(-14.9128113608891,-14.199353333197,
116.152059746698)) ;
#186453 = CARTESIAN_POINT('Ctrl Pts',(-14.9293786536738,-14.1451271098491,
116.202521047353)) ;
#186454 = CARTESIAN_POINT('Ctrl Pts',(-14.8555748106877,-14.1451271117169,
116.226752090361)) ;
#186455 = CARTESIAN_POINT('Ctrl Pts',(-14.7817709677015,-14.1451271135848,
116.250983133368)) ;
#186456 = CARTESIAN_POINT('Ctrl Pts',(-14.7652036749168,-14.1993533369326,
116.200521832713)) ;
#186457 = CARTESIAN_POINT('Ctrl Pts',(-14.7486363821321,-14.2535795602805,
116.150060532057)) ;
#186458 = CARTESIAN_POINT('Ctrl Pts',(-14.8224402251183,-14.2535795584127,
116.12582948905)) ;
#186459 = CARTESIAN_POINT('Ctrl Pts',(-14.8962440681044,-14.2535795565448,
116.101598446043)) ;
#186460 = CARTESIAN_POINT('Ctrl Pts',(-14.9128113608891,-14.199353333197,
116.152059746698)) ;
#186461 = CARTESIAN_POINT('Ctrl Pts',(-14.9753472996786,-14.3720888987135,
116.377975410379)) ;
#186462 = CARTESIAN_POINT('Ctrl Pts',(-14.986838764229,-14.3057223139106,
116.412976557117)) ;
#186463 = CARTESIAN_POINT('Ctrl Pts',(-14.9130349227356,-14.3057223178457,
116.437207604671)) ;
#186464 = CARTESIAN_POINT('Ctrl Pts',(-14.8392310812422,-14.3057223217808,
116.461438652225)) ;
#186465 = CARTESIAN_POINT('Ctrl Pts',(-14.8277396166918,-14.3720889065837,
116.426437505486)) ;
#186466 = CARTESIAN_POINT('Ctrl Pts',(-14.8162481521414,-14.4384554913866,
116.391436358748)) ;
#186467 = CARTESIAN_POINT('Ctrl Pts',(-14.8900519936348,-14.4384554874515,
116.367205311194)) ;
#186468 = CARTESIAN_POINT('Ctrl Pts',(-14.9638558351282,-14.4384554835164,
116.34297426364)) ;
#186469 = CARTESIAN_POINT('Ctrl Pts',(-14.9753472996786,-14.3720888987135,
116.377975410379)) ;
#186470 = CARTESIAN_POINT('Ctrl Pts',(-15.0495832763769,-14.4765884160959,
116.639535491124)) ;
#186471 = CARTESIAN_POINT('Ctrl Pts',(-15.0551744341217,-14.4028287794428,
116.656565255222)) ;
#186472 = CARTESIAN_POINT('Ctrl Pts',(-14.9813705947848,-14.4028287831727,
116.680796309345)) ;
#186473 = CARTESIAN_POINT('Ctrl Pts',(-14.907566755448,-14.4028287869026,
116.705027363467)) ;
#186474 = CARTESIAN_POINT('Ctrl Pts',(-14.9019755977032,-14.4765884235558,
116.687997599369)) ;
#186475 = CARTESIAN_POINT('Ctrl Pts',(-14.8963844399584,-14.5503480602089,
116.67096783527)) ;
#186476 = CARTESIAN_POINT('Ctrl Pts',(-14.9701882792953,-14.550348056479,
116.646736781148)) ;
#186477 = CARTESIAN_POINT('Ctrl Pts',(-15.0439921186321,-14.550348052749,
116.622505727025)) ;
#186478 = CARTESIAN_POINT('Ctrl Pts',(-15.0495832763769,-14.4765884160959,
116.639535491124)) ;
#186479 = CARTESIAN_POINT('Ctrl Pts',(-15.1294503292581,-14.5052820126098,
116.918258658341)) ;
#186480 = CARTESIAN_POINT('Ctrl Pts',(-15.1287392558924,-14.4294119228674,
116.916092843196)) ;
#186481 = CARTESIAN_POINT('Ctrl Pts',(-15.054935418997,-14.4294119227756,
116.940323904755)) ;
#186482 = CARTESIAN_POINT('Ctrl Pts',(-14.9811315821015,-14.4294119226838,
116.964554966313)) ;
#186483 = CARTESIAN_POINT('Ctrl Pts',(-14.9818426554672,-14.5052820124263,
116.966720781458)) ;
#186484 = CARTESIAN_POINT('Ctrl Pts',(-14.9825537288328,-14.5811521021687,
116.968886596602)) ;
#186485 = CARTESIAN_POINT('Ctrl Pts',(-15.0563575657283,-14.5811521022605,
116.944655535043)) ;
#186486 = CARTESIAN_POINT('Ctrl Pts',(-15.1301614026238,-14.5811521023523,
116.920424473485)) ;
#186487 = CARTESIAN_POINT('Ctrl Pts',(-15.1294503292581,-14.5052820126098,
116.918258658341)) ;
#186488 = CARTESIAN_POINT('Ctrl Pts',(-15.2083554184061,-14.4562719682351,
117.194003127052)) ;
#186489 = CARTESIAN_POINT('Ctrl Pts',(-15.2014012663886,-14.3837141408082,
117.172821901506)) ;
#186490 = CARTESIAN_POINT('Ctrl Pts',(-15.1275974315029,-14.383714132999,
117.197052969186)) ;
#186491 = CARTESIAN_POINT('Ctrl Pts',(-15.0537935966172,-14.3837141251898,
117.221284036866)) ;
#186492 = CARTESIAN_POINT('Ctrl Pts',(-15.0607477486347,-14.4562719526167,
117.242465262412)) ;
#186493 = CARTESIAN_POINT('Ctrl Pts',(-15.0677019006523,-14.5288297800436,
117.263646487958)) ;
#186494 = CARTESIAN_POINT('Ctrl Pts',(-15.141505735538,-14.5288297878528,
117.239415420278)) ;
#186495 = CARTESIAN_POINT('Ctrl Pts',(-15.2153095704236,-14.528829795662,
117.215184352598)) ;
#186496 = CARTESIAN_POINT('Ctrl Pts',(-15.2083554184061,-14.4562719682351,
117.194003127052)) ;
#186497 = CARTESIAN_POINT('Ctrl Pts',(-15.2801775082366,-14.3327513043896,
117.448257959663)) ;
#186498 = CARTESIAN_POINT('Ctrl Pts',(-15.2674641035531,-14.2687127593662,
117.409534979579)) ;
#186499 = CARTESIAN_POINT('Ctrl Pts',(-15.1936602700235,-14.2687127399002,
117.433766051389)) ;
#186500 = CARTESIAN_POINT('Ctrl Pts',(-15.1198564364938,-14.2687127204341,
117.4579971232)) ;
#186501 = CARTESIAN_POINT('Ctrl Pts',(-15.1325698411772,-14.3327512654575,
117.496720103284)) ;
#186502 = CARTESIAN_POINT('Ctrl Pts',(-15.1452832458607,-14.3967898104809,
117.535443083367)) ;
#186503 = CARTESIAN_POINT('Ctrl Pts',(-15.2190870793904,-14.3967898299469,
117.511212011557)) ;
#186504 = CARTESIAN_POINT('Ctrl Pts',(-15.29289091292,-14.396789849413,117.486980939747)) ;
#186505 = CARTESIAN_POINT('Ctrl Pts',(-15.2801775082366,-14.3327513043896,
117.448257959663)) ;
#186506 = CARTESIAN_POINT('Ctrl Pts',(-15.3387805415736,-14.1436492001557,
117.662231074929)) ;
#186507 = CARTESIAN_POINT('Ctrl Pts',(-15.321222983922,-14.0927211498799,
117.608753586334)) ;
#186508 = CARTESIAN_POINT('Ctrl Pts',(-15.2474191502595,-14.0927211161122,
117.63298465774)) ;
#186509 = CARTESIAN_POINT('Ctrl Pts',(-15.173615316597,-14.0927210823444,
117.657215729146)) ;
#186510 = CARTESIAN_POINT('Ctrl Pts',(-15.1911728742487,-14.1436491326202,
117.71069321774)) ;
#186511 = CARTESIAN_POINT('Ctrl Pts',(-15.2087304319003,-14.194577182896,
117.764170706335)) ;
#186512 = CARTESIAN_POINT('Ctrl Pts',(-15.2825342655628,-14.1945772166637,
117.739939634929)) ;
#186513 = CARTESIAN_POINT('Ctrl Pts',(-15.3563380992252,-14.1945772504315,
117.715708563523)) ;
#186514 = CARTESIAN_POINT('Ctrl Pts',(-15.3387805415736,-14.1436492001557,
117.662231074929)) ;
#186515 = CARTESIAN_POINT('Ctrl Pts',(-15.3792583067542,-13.9025966993027,
117.820992658252)) ;
#186516 = CARTESIAN_POINT('Ctrl Pts',(-15.3581152443244,-13.8684250728151,
117.756594300452)) ;
#186517 = CARTESIAN_POINT('Ctrl Pts',(-15.2843114087381,-13.8684250241037,
117.780825365998)) ;
#186518 = CARTESIAN_POINT('Ctrl Pts',(-15.2105075731519,-13.8684249753923,
117.805056431544)) ;
#186519 = CARTESIAN_POINT('Ctrl Pts',(-15.2316506355817,-13.9025966018799,
117.869454789344)) ;
#186520 = CARTESIAN_POINT('Ctrl Pts',(-15.2527936980115,-13.9367682283676,
117.933853147143)) ;
#186521 = CARTESIAN_POINT('Ctrl Pts',(-15.3265975335978,-13.936768277079,
117.909622081597)) ;
#186522 = CARTESIAN_POINT('Ctrl Pts',(-15.400401369184,-13.9367683257904,
117.885391016051)) ;
#186523 = CARTESIAN_POINT('Ctrl Pts',(-15.3792583067542,-13.9025966993027,
117.820992658252)) ;
#186524 = CARTESIAN_POINT('Ctrl Pts',(-15.3979595900405,-13.6267191611602,
117.91343726374)) ;
#186525 = CARTESIAN_POINT('Ctrl Pts',(-15.3747460243894,-13.6117593942212,
117.842732487035)) ;
#186526 = CARTESIAN_POINT('Ctrl Pts',(-15.3009421849996,-13.6117593320571,
117.866963540996)) ;
#186527 = CARTESIAN_POINT('Ctrl Pts',(-15.2271383456097,-13.6117592698929,
117.891194594957)) ;
#186528 = CARTESIAN_POINT('Ctrl Pts',(-15.2503519112607,-13.6267190368318,
117.961899371662)) ;
#186529 = CARTESIAN_POINT('Ctrl Pts',(-15.2735654769117,-13.6416788037708,
118.032604148367)) ;
#186530 = CARTESIAN_POINT('Ctrl Pts',(-15.3473693163016,-13.641678865935,
118.008373094406)) ;
#186531 = CARTESIAN_POINT('Ctrl Pts',(-15.4211731556915,-13.6416789280991,
117.984142040445)) ;
#186532 = CARTESIAN_POINT('Ctrl Pts',(-15.3979595900405,-13.6267191611602,
117.91343726374)) ;
#186533 = CARTESIAN_POINT('Ctrl Pts',(-15.3927825723995,-13.3360804435672,
117.933129443873)) ;
#186534 = CARTESIAN_POINT('Ctrl Pts',(-15.3691631161479,-13.3413907563864,
117.861188389733)) ;
#186535 = CARTESIAN_POINT('Ctrl Pts',(-15.2953592712623,-13.3413906849688,
117.885419426954)) ;
#186536 = CARTESIAN_POINT('Ctrl Pts',(-15.2215554263766,-13.3413906135511,
117.909650464176)) ;
#186537 = CARTESIAN_POINT('Ctrl Pts',(-15.2451748826282,-13.3360803007319,
117.981591518316)) ;
#186538 = CARTESIAN_POINT('Ctrl Pts',(-15.2687943388797,-13.3307699879127,
118.053532572457)) ;
#186539 = CARTESIAN_POINT('Ctrl Pts',(-15.3425981837654,-13.3307700593304,
118.029301535235)) ;
#186540 = CARTESIAN_POINT('Ctrl Pts',(-15.416402028651,-13.330770130748,118.005070498014)) ;
#186541 = CARTESIAN_POINT('Ctrl Pts',(-15.3927825723995,-13.3360804435672,
117.933129443873)) ;
#186542 = CARTESIAN_POINT('Ctrl Pts',(-15.3633873922544,-13.0512189530207,
117.879062741303)) ;
#186543 = CARTESIAN_POINT('Ctrl Pts',(-15.3410521280606,-13.076425168365,
117.811033128819)) ;
#186544 = CARTESIAN_POINT('Ctrl Pts',(-15.2672482765079,-13.0764250935319,
117.835264145734)) ;
#186545 = CARTESIAN_POINT('Ctrl Pts',(-15.1934444249552,-13.0764250186989,
117.859495162648)) ;
#186546 = CARTESIAN_POINT('Ctrl Pts',(-15.215779689149,-13.0512188033546,
117.927524775132)) ;
#186547 = CARTESIAN_POINT('Ctrl Pts',(-15.2381149533427,-13.0260125880103,
117.995554387616)) ;
#186548 = CARTESIAN_POINT('Ctrl Pts',(-15.3119188048954,-13.0260126628434,
117.971323370702)) ;
#186549 = CARTESIAN_POINT('Ctrl Pts',(-15.3857226564481,-13.0260127376764,
117.947092353787)) ;
#186550 = CARTESIAN_POINT('Ctrl Pts',(-15.3633873922544,-13.0512189530207,
117.879062741303)) ;
#186551 = CARTESIAN_POINT('Ctrl Pts',(-15.3109908652404,-12.7925464774136,
117.754972225267)) ;
#186552 = CARTESIAN_POINT('Ctrl Pts',(-15.291546720893,-12.835849054134,117.695748497217)) ;
#186553 = CARTESIAN_POINT('Ctrl Pts',(-15.2177428621128,-12.8358489831972,
117.719979492118)) ;
#186554 = CARTESIAN_POINT('Ctrl Pts',(-15.1439390033326,-12.8358489122603,
117.744210487019)) ;
#186555 = CARTESIAN_POINT('Ctrl Pts',(-15.16338314768,-12.7925463355399,117.803434215069)) ;
#186556 = CARTESIAN_POINT('Ctrl Pts',(-15.1828272920273,-12.7492437588195,
117.86265794312)) ;
#186557 = CARTESIAN_POINT('Ctrl Pts',(-15.2566311508075,-12.7492438297564,
117.838426948219)) ;
#186558 = CARTESIAN_POINT('Ctrl Pts',(-15.3304350095877,-12.7492439006932,
117.814195953318)) ;
#186559 = CARTESIAN_POINT('Ctrl Pts',(-15.3109908652404,-12.7925464774136,
117.754972225267)) ;
#186560 = CARTESIAN_POINT('Ctrl Pts',(-15.2391823230942,-12.5795095572681,
117.571559510383)) ;
#186561 = CARTESIAN_POINT('Ctrl Pts',(-15.2239929392201,-12.6377483614764,
117.525295096131)) ;
#186562 = CARTESIAN_POINT('Ctrl Pts',(-15.1501890738939,-12.6377483026741,
117.549526071094)) ;
#186563 = CARTESIAN_POINT('Ctrl Pts',(-15.0763852085677,-12.6377482438719,
117.573757046056)) ;
#186564 = CARTESIAN_POINT('Ctrl Pts',(-15.0915745924417,-12.5795094396635,
117.620021460309)) ;
#186565 = CARTESIAN_POINT('Ctrl Pts',(-15.1067639763158,-12.5212706354552,
117.666285874561)) ;
#186566 = CARTESIAN_POINT('Ctrl Pts',(-15.180567841642,-12.5212706942575,
117.642054899598)) ;
#186567 = CARTESIAN_POINT('Ctrl Pts',(-15.2543717069682,-12.5212707530598,
117.617823924636)) ;
#186568 = CARTESIAN_POINT('Ctrl Pts',(-15.2391823230942,-12.5795095572681,
117.571559510383)) ;
#186569 = CARTESIAN_POINT('Ctrl Pts',(-15.1507434986883,-12.4247175389401,
117.337961032472)) ;
#186570 = CARTESIAN_POINT('Ctrl Pts',(-15.140965995546,-12.4938489762306,
117.308180333589)) ;
#186571 = CARTESIAN_POINT('Ctrl Pts',(-15.067162124109,-12.4938489356481,
117.332411289939)) ;
#186572 = CARTESIAN_POINT('Ctrl Pts',(-14.993358252672,-12.4938488950656,
117.356642246289)) ;
#186573 = CARTESIAN_POINT('Ctrl Pts',(-15.0031357558144,-12.4247174577751,
117.386422945172)) ;
#186574 = CARTESIAN_POINT('Ctrl Pts',(-15.0129132589567,-12.3555860204846,
117.416203644056)) ;
#186575 = CARTESIAN_POINT('Ctrl Pts',(-15.0867171303937,-12.3555860610671,
117.391972687705)) ;
#186576 = CARTESIAN_POINT('Ctrl Pts',(-15.1605210018307,-12.3555861016496,
117.367741731355)) ;
#186577 = CARTESIAN_POINT('Ctrl Pts',(-15.1507434986883,-12.4247175389401,
117.337961032472)) ;
#186578 = CARTESIAN_POINT('Ctrl Pts',(-15.0539963052002,-12.3430591277612,
117.078422578942)) ;
#186579 = CARTESIAN_POINT('Ctrl Pts',(-15.050232182881,-12.417991968948,117.06695766774)) ;
#186580 = CARTESIAN_POINT('Ctrl Pts',(-14.976428308272,-12.4179919531806,
117.091188614429)) ;
#186581 = CARTESIAN_POINT('Ctrl Pts',(-14.902624433663,-12.4179919374132,
117.115419561118)) ;
#186582 = CARTESIAN_POINT('Ctrl Pts',(-14.9063885559822,-12.3430590962263,
117.12688447232)) ;
#186583 = CARTESIAN_POINT('Ctrl Pts',(-14.9101526783013,-12.2681262550395,
117.138349383522)) ;
#186584 = CARTESIAN_POINT('Ctrl Pts',(-14.9839565529103,-12.2681262708069,
117.114118436833)) ;
#186585 = CARTESIAN_POINT('Ctrl Pts',(-15.0577604275193,-12.2681262865743,
117.089887490144)) ;
#186586 = CARTESIAN_POINT('Ctrl Pts',(-15.0539963052002,-12.3430591277612,
117.078422578942)) ;
#186587 = CARTESIAN_POINT('Ctrl Pts',(-14.9522545120357,-12.3371678726539,
116.804152632931)) ;
#186588 = CARTESIAN_POINT('Ctrl Pts',(-14.9548509777493,-12.4126223874774,
116.812061046522)) ;
#186589 = CARTESIAN_POINT('Ctrl Pts',(-14.8810471017157,-12.4126223993309,
116.836291988872)) ;
#186590 = CARTESIAN_POINT('Ctrl Pts',(-14.8072432256821,-12.4126224111843,
116.860522931222)) ;
#186591 = CARTESIAN_POINT('Ctrl Pts',(-14.8046467599684,-12.3371678963608,
116.852614517631)) ;
#186592 = CARTESIAN_POINT('Ctrl Pts',(-14.8020502942548,-12.2617133815373,
116.84470610404)) ;
#186593 = CARTESIAN_POINT('Ctrl Pts',(-14.8758541702884,-12.2617133696838,
116.82047516169)) ;
#186594 = CARTESIAN_POINT('Ctrl Pts',(-14.949658046322,-12.2617133578303,
116.79624421934)) ;
#186595 = CARTESIAN_POINT('Ctrl Pts',(-14.9522545120357,-12.3371678726539,
116.804152632931)) ;
#186596 = CARTESIAN_POINT('Ctrl Pts',(-14.8538527368102,-12.4090465693171,
116.539851551766)) ;
#186597 = CARTESIAN_POINT('Ctrl Pts',(-14.8625902865125,-12.4795937186109,
116.566464716288)) ;
#186598 = CARTESIAN_POINT('Ctrl Pts',(-14.7887864120648,-12.4795937586664,
116.590695663468)) ;
#186599 = CARTESIAN_POINT('Ctrl Pts',(-14.7149825376171,-12.4795937987218,
116.614926610649)) ;
#186600 = CARTESIAN_POINT('Ctrl Pts',(-14.7062449879148,-12.409046649428,
116.588313446127)) ;
#186601 = CARTESIAN_POINT('Ctrl Pts',(-14.6975074382125,-12.3384995001342,
116.561700281605)) ;
#186602 = CARTESIAN_POINT('Ctrl Pts',(-14.7713113126602,-12.3384994600787,
116.537469334425)) ;
#186603 = CARTESIAN_POINT('Ctrl Pts',(-14.8451151871079,-12.3384994200233,
116.513238387244)) ;
#186604 = CARTESIAN_POINT('Ctrl Pts',(-14.8538527368102,-12.4090465693171,
116.539851551766)) ;
#186605 = CARTESIAN_POINT('Ctrl Pts',(-14.7642677691781,-12.5533759332391,
116.302515678383)) ;
#186606 = CARTESIAN_POINT('Ctrl Pts',(-14.778537622709,-12.6139509456652,
116.345979347711)) ;
#186607 = CARTESIAN_POINT('Ctrl Pts',(-14.7047337524295,-12.6139510114575,
116.370210307587)) ;
#186608 = CARTESIAN_POINT('Ctrl Pts',(-14.63092988215,-12.6139510772497,116.394441267463)) ;
#186609 = CARTESIAN_POINT('Ctrl Pts',(-14.616660028619,-12.5533760648236,
116.350977598135)) ;
#186610 = CARTESIAN_POINT('Ctrl Pts',(-14.6023901750881,-12.4928010523974,
116.307513928807)) ;
#186611 = CARTESIAN_POINT('Ctrl Pts',(-14.6761940453676,-12.4928009866052,
116.283282968931)) ;
#186612 = CARTESIAN_POINT('Ctrl Pts',(-14.7499979156471,-12.4928009208129,
116.259052009055)) ;
#186613 = CARTESIAN_POINT('Ctrl Pts',(-14.7642677691781,-12.5533759332391,
116.302515678383)) ;
#186614 = CARTESIAN_POINT('Ctrl Pts',(-14.6896786909459,-12.75934674632,116.110760879403)) ;
#186615 = CARTESIAN_POINT('Ctrl Pts',(-14.7084440858535,-12.8056312692346,
116.167917242415)) ;
#186616 = CARTESIAN_POINT('Ctrl Pts',(-14.6346402220319,-12.8056313554312,
116.19214822196)) ;
#186617 = CARTESIAN_POINT('Ctrl Pts',(-14.5608363582103,-12.8056314416279,
116.216379201506)) ;
#186618 = CARTESIAN_POINT('Ctrl Pts',(-14.5420709633026,-12.7593469187134,
116.159222838494)) ;
#186619 = CARTESIAN_POINT('Ctrl Pts',(-14.523305568395,-12.7130623957988,
116.102066475482)) ;
#186620 = CARTESIAN_POINT('Ctrl Pts',(-14.5971094322166,-12.7130623096021,
116.077835495937)) ;
#186621 = CARTESIAN_POINT('Ctrl Pts',(-14.6709132960383,-12.7130622234055,
116.053604516391)) ;
#186622 = CARTESIAN_POINT('Ctrl Pts',(-14.6896786909459,-12.75934674632,116.110760879403)) ;
#186623 = CARTESIAN_POINT('Ctrl Pts',(-14.6343789414248,-13.0122957598429,
115.977755201021)) ;
#186624 = CARTESIAN_POINT('Ctrl Pts',(-14.6562999607946,-13.0409889610471,
116.044523087009)) ;
#186625 = CARTESIAN_POINT('Ctrl Pts',(-14.5824961049884,-13.0409890604734,
116.068754090968)) ;
#186626 = CARTESIAN_POINT('Ctrl Pts',(-14.5086922491823,-13.0409891598997,
116.092985094927)) ;
#186627 = CARTESIAN_POINT('Ctrl Pts',(-14.4867712298125,-13.0122959586955,
116.02621720894)) ;
#186628 = CARTESIAN_POINT('Ctrl Pts',(-14.4648502104427,-12.9836027574913,
115.959449322952)) ;
#186629 = CARTESIAN_POINT('Ctrl Pts',(-14.5386540662488,-12.983602658065,
115.935218318993)) ;
#186630 = CARTESIAN_POINT('Ctrl Pts',(-14.612457922055,-12.9836025586387,
115.910987315034)) ;
#186631 = CARTESIAN_POINT('Ctrl Pts',(-14.6343789414248,-13.0122957598429,
115.977755201021)) ;
#186632 = CARTESIAN_POINT('Ctrl Pts',(-14.6015670654935,-13.2947806869138,
115.913305234625)) ;
#186633 = CARTESIAN_POINT('Ctrl Pts',(-14.6250772645124,-13.3037945330256,
115.984913505458)) ;
#186634 = CARTESIAN_POINT('Ctrl Pts',(-14.5512734174972,-13.303794637043,
116.009144536193)) ;
#186635 = CARTESIAN_POINT('Ctrl Pts',(-14.4774695704819,-13.3037947410603,
116.033375566928)) ;
#186636 = CARTESIAN_POINT('Ctrl Pts',(-14.4539593714631,-13.2947808949484,
115.961767296095)) ;
#186637 = CARTESIAN_POINT('Ctrl Pts',(-14.4304491724442,-13.2857670488366,
115.890159025263)) ;
#186638 = CARTESIAN_POINT('Ctrl Pts',(-14.5042530194594,-13.2857669448193,
115.865927994528)) ;
#186639 = CARTESIAN_POINT('Ctrl Pts',(-14.5780568664746,-13.2857668408019,
115.841696963793)) ;
#186640 = CARTESIAN_POINT('Ctrl Pts',(-14.6015670654935,-13.2947806869138,
115.913305234625)) ;
#186641 = CARTESIAN_POINT('Ctrl Pts',(-14.5929308331265,-13.5857642149866,
115.922448315919)) ;
#186642 = CARTESIAN_POINT('Ctrl Pts',(-14.6163456531128,-13.5744758994453,
115.993766077673)) ;
#186643 = CARTESIAN_POINT('Ctrl Pts',(-14.542541814698,-13.574475999467,116.017997134604)) ;
#186644 = CARTESIAN_POINT('Ctrl Pts',(-14.4687379762832,-13.5744760994887,
116.042228191534)) ;
#186645 = CARTESIAN_POINT('Ctrl Pts',(-14.4453231562969,-13.58576441503,115.970910429781)) ;
#186646 = CARTESIAN_POINT('Ctrl Pts',(-14.4219083363105,-13.5970527305713,
115.899592668027)) ;
#186647 = CARTESIAN_POINT('Ctrl Pts',(-14.4957121747253,-13.5970526305496,
115.875361611096)) ;
#186648 = CARTESIAN_POINT('Ctrl Pts',(-14.5695160131401,-13.5970525305279,
115.851130554166)) ;
#186649 = CARTESIAN_POINT('Ctrl Pts',(-14.5929308331265,-13.5857642149866,
115.922448315919)) ;
#186650 = CARTESIAN_POINT('Ctrl Pts',(-14.6083539544559,-13.8655802602202,
116.00497775363)) ;
#186651 = CARTESIAN_POINT('Ctrl Pts',(-14.6299915248511,-13.8347390280632,
116.070882299983)) ;
#186652 = CARTESIAN_POINT('Ctrl Pts',(-14.5561876939648,-13.8347391156571,
116.095113379844)) ;
#186653 = CARTESIAN_POINT('Ctrl Pts',(-14.4823838630785,-13.834739203251,
116.119344459705)) ;
#186654 = CARTESIAN_POINT('Ctrl Pts',(-14.4607462926832,-13.865580435408,
116.053439913352)) ;
#186655 = CARTESIAN_POINT('Ctrl Pts',(-14.439108722288,-13.8964216675651,
115.987535367)) ;
#186656 = CARTESIAN_POINT('Ctrl Pts',(-14.5129125531743,-13.8964215799712,
115.963304287139)) ;
#186657 = CARTESIAN_POINT('Ctrl Pts',(-14.5867163840606,-13.8964214923772,
115.939073207277)) ;
#186658 = CARTESIAN_POINT('Ctrl Pts',(-14.6083539544559,-13.8655802602202,
116.00497775363)) ;
#186659 = CARTESIAN_POINT('Ctrl Pts',(-14.6460817889764,-14.1129045177148,
116.155423205873)) ;
#186660 = CARTESIAN_POINT('Ctrl Pts',(-14.6643826463311,-14.0647490921529,
116.211164662798)) ;
#186661 = CARTESIAN_POINT('Ctrl Pts',(-14.5905788210321,-14.0647491613001,
116.235395759677)) ;
#186662 = CARTESIAN_POINT('Ctrl Pts',(-14.516774995733,-14.0647492304473,
116.259626856556)) ;
#186663 = CARTESIAN_POINT('Ctrl Pts',(-14.4984741383783,-14.1129046560093,
116.203885399631)) ;
#186664 = CARTESIAN_POINT('Ctrl Pts',(-14.4801732810236,-14.1610600815713,
116.148143942706)) ;
#186665 = CARTESIAN_POINT('Ctrl Pts',(-14.5539771063227,-14.161060012424,
116.123912845827)) ;
#186666 = CARTESIAN_POINT('Ctrl Pts',(-14.6277809316217,-14.1610599432768,
116.099681748948)) ;
#186667 = CARTESIAN_POINT('Ctrl Pts',(-14.6460817889764,-14.1129045177148,
116.155423205873)) ;
#186668 = CARTESIAN_POINT('Ctrl Pts',(-14.7021022989247,-14.3092608415155,
116.361345320201)) ;
#186669 = CARTESIAN_POINT('Ctrl Pts',(-14.7157890443858,-14.2473238052157,
116.403032936882)) ;
#186670 = CARTESIAN_POINT('Ctrl Pts',(-14.6419852228446,-14.2473238535572,
116.427264045207)) ;
#186671 = CARTESIAN_POINT('Ctrl Pts',(-14.5681814013034,-14.2473239018987,
116.451495153532)) ;
#186672 = CARTESIAN_POINT('Ctrl Pts',(-14.5544946558422,-14.3092609381985,
116.409807536851)) ;
#186673 = CARTESIAN_POINT('Ctrl Pts',(-14.5408079103811,-14.3711979744983,
116.368119920171)) ;
#186674 = CARTESIAN_POINT('Ctrl Pts',(-14.6146117319223,-14.3711979261568,
116.343888811846)) ;
#186675 = CARTESIAN_POINT('Ctrl Pts',(-14.6884155534635,-14.3711978778153,
116.319657703521)) ;
#186676 = CARTESIAN_POINT('Ctrl Pts',(-14.7021022989247,-14.3092608415155,
116.361345320201)) ;
#186677 = CARTESIAN_POINT('Ctrl Pts',(-14.7724489534844,-14.4430503329775,
116.611150402582)) ;
#186678 = CARTESIAN_POINT('Ctrl Pts',(-14.7805094778502,-14.3716785302195,
116.635701457742)) ;
#186679 = CARTESIAN_POINT('Ctrl Pts',(-14.7067056572874,-14.371678555561,
116.659932569047)) ;
#186680 = CARTESIAN_POINT('Ctrl Pts',(-14.6329018367247,-14.3716785809024,
116.684163680352)) ;
#186681 = CARTESIAN_POINT('Ctrl Pts',(-14.6248413123589,-14.4430503836605,
116.659612625192)) ;
#186682 = CARTESIAN_POINT('Ctrl Pts',(-14.6167807879931,-14.5144221864185,
116.635061570032)) ;
#186683 = CARTESIAN_POINT('Ctrl Pts',(-14.6905846085559,-14.5144221610771,
116.610830458727)) ;
#186684 = CARTESIAN_POINT('Ctrl Pts',(-14.7643884291186,-14.5144221357356,
116.586599347422)) ;
#186685 = CARTESIAN_POINT('Ctrl Pts',(-14.7724489534844,-14.4430503329775,
116.611150402582)) ;
#186686 = CARTESIAN_POINT('Ctrl Pts',(-14.8505663309753,-14.5029681127336,
116.88443223403)) ;
#186687 = CARTESIAN_POINT('Ctrl Pts',(-14.852453421253,-14.4273052047568,
116.890180005168)) ;
#186688 = CARTESIAN_POINT('Ctrl Pts',(-14.778649599869,-14.427305209291,116.914411113971)) ;
#186689 = CARTESIAN_POINT('Ctrl Pts',(-14.704845778485,-14.4273052138253,
116.938642222775)) ;
#186690 = CARTESIAN_POINT('Ctrl Pts',(-14.7029586882074,-14.5029681218021,
116.932894451638)) ;
#186691 = CARTESIAN_POINT('Ctrl Pts',(-14.7010715979297,-14.5786310297789,
116.927146680501)) ;
#186692 = CARTESIAN_POINT('Ctrl Pts',(-14.7748754193137,-14.5786310252447,
116.902915571697)) ;
#186693 = CARTESIAN_POINT('Ctrl Pts',(-14.8486792406976,-14.5786310207104,
116.878684462893)) ;
#186694 = CARTESIAN_POINT('Ctrl Pts',(-14.8505663309753,-14.5029681127336,
116.88443223403)) ;
#186695 = CARTESIAN_POINT('Ctrl Pts',(-14.9309079279403,-14.4854361051768,
117.164690654725)) ;
#186696 = CARTESIAN_POINT('Ctrl Pts',(-14.9264527867039,-14.4108823854582,
117.151121012159)) ;
#186697 = CARTESIAN_POINT('Ctrl Pts',(-14.8526489621555,-14.4108823726848,
117.175352111325)) ;
#186698 = CARTESIAN_POINT('Ctrl Pts',(-14.7788451376072,-14.4108823599115,
117.199583210491)) ;
#186699 = CARTESIAN_POINT('Ctrl Pts',(-14.7833002788435,-14.4854360796301,
117.213152853056)) ;
#186700 = CARTESIAN_POINT('Ctrl Pts',(-14.7877554200799,-14.5599897993486,
117.226722495622)) ;
#186701 = CARTESIAN_POINT('Ctrl Pts',(-14.8615592446283,-14.559989812122,
117.202491396456)) ;
#186702 = CARTESIAN_POINT('Ctrl Pts',(-14.9353630691767,-14.5599898248954,
117.17826029729)) ;
#186703 = CARTESIAN_POINT('Ctrl Pts',(-14.9309079279403,-14.4854361051768,
117.164690654725)) ;
#186704 = CARTESIAN_POINT('Ctrl Pts',(-15.0063578899015,-14.3912934817558,
117.429961830675)) ;
#186705 = CARTESIAN_POINT('Ctrl Pts',(-14.9958941718393,-14.3231998086573,
117.398091032744)) ;
#186706 = CARTESIAN_POINT('Ctrl Pts',(-14.9220903431598,-14.323199784148,
117.422322119327)) ;
#186707 = CARTESIAN_POINT('Ctrl Pts',(-14.8482865144804,-14.3231997596387,
117.44655320591)) ;
#186708 = CARTESIAN_POINT('Ctrl Pts',(-14.8587502325426,-14.3912934327372,
117.478424003842)) ;
#186709 = CARTESIAN_POINT('Ctrl Pts',(-14.8692139506049,-14.4593871058357,
117.510294801773)) ;
#186710 = CARTESIAN_POINT('Ctrl Pts',(-14.9430177792843,-14.459387130345,
117.48606371519)) ;
#186711 = CARTESIAN_POINT('Ctrl Pts',(-15.0168216079637,-14.4593871548543,
117.461832628607)) ;
#186712 = CARTESIAN_POINT('Ctrl Pts',(-15.0063578899015,-14.3912934817558,
117.429961830675)) ;
#186713 = CARTESIAN_POINT('Ctrl Pts',(-15.0709894180942,-14.2271892392871,
117.662327292392)) ;
#186714 = CARTESIAN_POINT('Ctrl Pts',(-15.0552623334199,-14.1704502048887,
117.614425129178)) ;
#186715 = CARTESIAN_POINT('Ctrl Pts',(-14.9814585000848,-14.1704501748707,
117.638656201581)) ;
#186716 = CARTESIAN_POINT('Ctrl Pts',(-14.9076546667496,-14.1704501448526,
117.662887273983)) ;
#186717 = CARTESIAN_POINT('Ctrl Pts',(-14.923381751424,-14.227189179251,117.710789437197)) ;
#186718 = CARTESIAN_POINT('Ctrl Pts',(-14.9391088360983,-14.2839282136493,
117.758691600411)) ;
#186719 = CARTESIAN_POINT('Ctrl Pts',(-15.0129126694335,-14.2839282436673,
117.734460528009)) ;
#186720 = CARTESIAN_POINT('Ctrl Pts',(-15.0867165027686,-14.2839282736854,
117.710229455606)) ;
#186721 = CARTESIAN_POINT('Ctrl Pts',(-15.0709894180942,-14.2271892392871,
117.662327292392)) ;
#186722 = CARTESIAN_POINT('Ctrl Pts',(-15.1191773884386,-14.0061849375035,
117.844439920784)) ;
#186723 = CARTESIAN_POINT('Ctrl Pts',(-15.0993306388851,-13.9647911087946,
117.783989923197)) ;
#186724 = CARTESIAN_POINT('Ctrl Pts',(-15.0255268014512,-13.9647910776001,
117.808220983116)) ;
#186725 = CARTESIAN_POINT('Ctrl Pts',(-14.9517229640173,-13.9647910464057,
117.832452043034)) ;
#186726 = CARTESIAN_POINT('Ctrl Pts',(-14.9715697135709,-14.0061848751146,
117.892902040621)) ;
#186727 = CARTESIAN_POINT('Ctrl Pts',(-14.9914164631244,-14.0475787038235,
117.953352038208)) ;
#186728 = CARTESIAN_POINT('Ctrl Pts',(-15.0652203005583,-14.047578735018,
117.929120978289)) ;
#186729 = CARTESIAN_POINT('Ctrl Pts',(-15.1390241379922,-14.0475787662124,
117.904889918371)) ;
#186730 = CARTESIAN_POINT('Ctrl Pts',(-15.1191773884386,-14.0061849375035,
117.844439920784)) ;
#186731 = CARTESIAN_POINT('Ctrl Pts',(-15.147137619444,-13.7418695803109,
117.965135185314)) ;
#186732 = CARTESIAN_POINT('Ctrl Pts',(-15.1245731450587,-13.7188682914606,
117.896407436568)) ;
#186733 = CARTESIAN_POINT('Ctrl Pts',(-15.0507693039846,-13.7188682649132,
117.920638485399)) ;
#186734 = CARTESIAN_POINT('Ctrl Pts',(-14.9769654629104,-13.7188682383657,
117.94486953423)) ;
#186735 = CARTESIAN_POINT('Ctrl Pts',(-14.9995299372958,-13.741869527216,
118.013597282976)) ;
#186736 = CARTESIAN_POINT('Ctrl Pts',(-15.022094411681,-13.7648708160662,
118.082325031721)) ;
#186737 = CARTESIAN_POINT('Ctrl Pts',(-15.0958982527552,-13.7648708426137,
118.05809398289)) ;
#186738 = CARTESIAN_POINT('Ctrl Pts',(-15.1697020938293,-13.7648708691611,
118.033862934059)) ;
#186739 = CARTESIAN_POINT('Ctrl Pts',(-15.147137619444,-13.7418695803109,
117.965135185314)) ;
#186740 = CARTESIAN_POINT('Ctrl Pts',(-15.1518624783003,-13.4550293844737,
118.014955235042)) ;
#186741 = CARTESIAN_POINT('Ctrl Pts',(-15.1282007920477,-13.4520215652615,
117.942885556132)) ;
#186742 = CARTESIAN_POINT('Ctrl Pts',(-15.0543969486045,-13.4520215454244,
117.967116597747)) ;
#186743 = CARTESIAN_POINT('Ctrl Pts',(-14.9805931051612,-13.4520215255873,
117.991347639362)) ;
#186744 = CARTESIAN_POINT('Ctrl Pts',(-15.0042547914137,-13.4550293447994,
118.063417318272)) ;
#186745 = CARTESIAN_POINT('Ctrl Pts',(-15.0279164776663,-13.4580371640116,
118.135486997181)) ;
#186746 = CARTESIAN_POINT('Ctrl Pts',(-15.1017203211096,-13.4580371838487,
118.111255955567)) ;
#186747 = CARTESIAN_POINT('Ctrl Pts',(-15.1755241645529,-13.4580372036859,
118.087024913952)) ;
#186748 = CARTESIAN_POINT('Ctrl Pts',(-15.1518624783003,-13.4550293844737,
118.014955235042)) ;
#186749 = CARTESIAN_POINT('Ctrl Pts',(-15.1320243079306,-13.1635845721582,
117.990218757168)) ;
#186750 = CARTESIAN_POINT('Ctrl Pts',(-15.1089733666003,-13.180922781359,
117.920009308918)) ;
#186751 = CARTESIAN_POINT('Ctrl Pts',(-15.0351695222069,-13.1809227707576,
117.944240347639)) ;
#186752 = CARTESIAN_POINT('Ctrl Pts',(-14.9613656778135,-13.1809227601562,
117.96847138636)) ;
#186753 = CARTESIAN_POINT('Ctrl Pts',(-14.9844166191439,-13.1635845509553,
118.03868083461)) ;
#186754 = CARTESIAN_POINT('Ctrl Pts',(-15.0074675604742,-13.1462463417545,
118.10889028286)) ;
#186755 = CARTESIAN_POINT('Ctrl Pts',(-15.0812714048676,-13.1462463523559,
118.084659244139)) ;
#186756 = CARTESIAN_POINT('Ctrl Pts',(-15.155075249261,-13.1462463629573,
118.060428205418)) ;
#186757 = CARTESIAN_POINT('Ctrl Pts',(-15.1320243079306,-13.1635845721582,
117.990218757168)) ;
#186758 = CARTESIAN_POINT('Ctrl Pts',(-15.0890308858548,-12.8938493439813,
117.894483238794)) ;
#186759 = CARTESIAN_POINT('Ctrl Pts',(-15.0682186826188,-12.9300476003649,
117.831092625647)) ;
#186760 = CARTESIAN_POINT('Ctrl Pts',(-14.9944148381014,-12.9300475948517,
117.85532366399)) ;
#186761 = CARTESIAN_POINT('Ctrl Pts',(-14.9206109935841,-12.9300475893384,
117.879554702334)) ;
#186762 = CARTESIAN_POINT('Ctrl Pts',(-14.9414231968201,-12.8938493329547,
117.942945315481)) ;
#186763 = CARTESIAN_POINT('Ctrl Pts',(-14.962235400056,-12.857651076571,118.006335928628)) ;
#186764 = CARTESIAN_POINT('Ctrl Pts',(-15.0360392445734,-12.8576510820843,
117.982104890284)) ;
#186765 = CARTESIAN_POINT('Ctrl Pts',(-15.1098430890907,-12.8576510875976,
117.957873851941)) ;
#186766 = CARTESIAN_POINT('Ctrl Pts',(-15.0890308858548,-12.8938493439813,
117.894483238794)) ;
#186767 = CARTESIAN_POINT('Ctrl Pts',(-15.0240348200628,-12.658475902558,
117.732210088055)) ;
#186768 = CARTESIAN_POINT('Ctrl Pts',(-15.006991084424,-12.7111646806542,
117.680297619284)) ;
#186769 = CARTESIAN_POINT('Ctrl Pts',(-14.9331872407942,-12.7111646805121,
117.704528660331)) ;
#186770 = CARTESIAN_POINT('Ctrl Pts',(-14.8593833971644,-12.7111646803699,
117.728759701378)) ;
#186771 = CARTESIAN_POINT('Ctrl Pts',(-14.8764271328032,-12.6584759022737,
117.780672170148)) ;
#186772 = CARTESIAN_POINT('Ctrl Pts',(-14.8934708684419,-12.6057871241775,
117.832584638919)) ;
#186773 = CARTESIAN_POINT('Ctrl Pts',(-14.9672747120717,-12.6057871243196,
117.808353597872)) ;
#186774 = CARTESIAN_POINT('Ctrl Pts',(-15.0410785557015,-12.6057871244618,
117.784122556825)) ;
#186775 = CARTESIAN_POINT('Ctrl Pts',(-15.0240348200628,-12.658475902558,
117.732210088055)) ;
#186776 = CARTESIAN_POINT('Ctrl Pts',(-14.9426437722386,-12.480124052921,
117.519499741541)) ;
#186777 = CARTESIAN_POINT('Ctrl Pts',(-14.930529597909,-12.545344547809,117.482601921182)) ;
#186778 = CARTESIAN_POINT('Ctrl Pts',(-14.8567257549558,-12.5453445488469,
117.506832964289)) ;
#186779 = CARTESIAN_POINT('Ctrl Pts',(-14.7829219120025,-12.5453445498848,
117.531064007397)) ;
#186780 = CARTESIAN_POINT('Ctrl Pts',(-14.7950360863321,-12.4801240549968,
117.567961827756)) ;
#186781 = CARTESIAN_POINT('Ctrl Pts',(-14.8071502606617,-12.4149035601088,
117.604859648115)) ;
#186782 = CARTESIAN_POINT('Ctrl Pts',(-14.8809541036149,-12.414903559071,
117.580628605007)) ;
#186783 = CARTESIAN_POINT('Ctrl Pts',(-14.9547579465681,-12.4149035580331,
117.556397561899)) ;
#186784 = CARTESIAN_POINT('Ctrl Pts',(-14.9426437722386,-12.480124052921,
117.519499741541)) ;
#186785 = CARTESIAN_POINT('Ctrl Pts',(-14.8475793344936,-12.366810202119,
117.265710821588)) ;
#186786 = CARTESIAN_POINT('Ctrl Pts',(-14.8413454317599,-12.4400414291151,
117.246723359765)) ;
#186787 = CARTESIAN_POINT('Ctrl Pts',(-14.7675415893947,-12.4400414300861,
117.270954404664)) ;
#186788 = CARTESIAN_POINT('Ctrl Pts',(-14.6937377470295,-12.4400414310572,
117.295185449562)) ;
#186789 = CARTESIAN_POINT('Ctrl Pts',(-14.6999716497632,-12.3668102040611,
117.314172911385)) ;
#186790 = CARTESIAN_POINT('Ctrl Pts',(-14.7062055524968,-12.2935789770651,
117.333160373209)) ;
#186791 = CARTESIAN_POINT('Ctrl Pts',(-14.780009394862,-12.293578976094,117.30892932831)) ;
#186792 = CARTESIAN_POINT('Ctrl Pts',(-14.8538132372272,-12.293578975123,
117.284698283411)) ;
#186793 = CARTESIAN_POINT('Ctrl Pts',(-14.8475793344936,-12.366810202119,
117.265710821588)) ;
#186794 = CARTESIAN_POINT('Ctrl Pts',(-14.7476028807063,-12.3300613553443,
116.996429637178)) ;
#186795 = CARTESIAN_POINT('Ctrl Pts',(-14.7476117897904,-12.4059660659724,
116.99645677286)) ;
#186796 = CARTESIAN_POINT('Ctrl Pts',(-14.6738079471839,-12.4059660657075,
117.020687817024)) ;
#186797 = CARTESIAN_POINT('Ctrl Pts',(-14.6000041045774,-12.4059660654426,
117.044918861187)) ;
#186798 = CARTESIAN_POINT('Ctrl Pts',(-14.5999951954933,-12.3300613548144,
117.044891725505)) ;
#186799 = CARTESIAN_POINT('Ctrl Pts',(-14.5999862864092,-12.2541566441862,
117.044864589822)) ;
#186800 = CARTESIAN_POINT('Ctrl Pts',(-14.6737901290157,-12.2541566444512,
117.020633545659)) ;
#186801 = CARTESIAN_POINT('Ctrl Pts',(-14.7475939716222,-12.2541566447161,
116.996402501495)) ;
#186802 = CARTESIAN_POINT('Ctrl Pts',(-14.7476028807063,-12.3300613553443,
116.996429637178)) ;
#186803 = CARTESIAN_POINT('Ctrl Pts',(-14.6466367120282,-12.3711193571588,
116.724562625234)) ;
#186804 = CARTESIAN_POINT('Ctrl Pts',(-14.6529580061683,-12.4442691147832,
116.743816267228)) ;
#186805 = CARTESIAN_POINT('Ctrl Pts',(-14.5791541624313,-12.4442691147866,
116.768047307948)) ;
#186806 = CARTESIAN_POINT('Ctrl Pts',(-14.5053503186943,-12.44426911479,116.792278348668)) ;
#186807 = CARTESIAN_POINT('Ctrl Pts',(-14.4990290245542,-12.3711193571657,
116.773024706675)) ;
#186808 = CARTESIAN_POINT('Ctrl Pts',(-14.4927077304141,-12.2979695995413,
116.753771064681)) ;
#186809 = CARTESIAN_POINT('Ctrl Pts',(-14.5665115741511,-12.2979695995379,
116.72954002396)) ;
#186810 = CARTESIAN_POINT('Ctrl Pts',(-14.6403154178881,-12.2979695995345,
116.70530898324)) ;
#186811 = CARTESIAN_POINT('Ctrl Pts',(-14.6466367120282,-12.3711193571588,
116.724562625234)) ;
#186812 = CARTESIAN_POINT('Ctrl Pts',(-14.5534726344851,-12.4860834955726,
116.475997560767)) ;
#186813 = CARTESIAN_POINT('Ctrl Pts',(-14.5655797908285,-12.5513121633835,
116.512874005424)) ;
#186814 = CARTESIAN_POINT('Ctrl Pts',(-14.4917759461966,-12.5513121652031,
116.537105043419)) ;
#186815 = CARTESIAN_POINT('Ctrl Pts',(-14.4179721015648,-12.5513121670227,
116.561336081413)) ;
#186816 = CARTESIAN_POINT('Ctrl Pts',(-14.4058649452214,-12.4860834992117,
116.524459636757)) ;
#186817 = CARTESIAN_POINT('Ctrl Pts',(-14.393757788878,-12.4208548314008,
116.4875831921)) ;
#186818 = CARTESIAN_POINT('Ctrl Pts',(-14.4675616335099,-12.4208548295812,
116.463352154105)) ;
#186819 = CARTESIAN_POINT('Ctrl Pts',(-14.5413654781417,-12.4208548277616,
116.439121116111)) ;
#186820 = CARTESIAN_POINT('Ctrl Pts',(-14.5534726344851,-12.4860834955726,
116.475997560767)) ;
#186821 = CARTESIAN_POINT('Ctrl Pts',(-14.4716712825806,-12.6694591781323,
116.26251906764)) ;
#186822 = CARTESIAN_POINT('Ctrl Pts',(-14.488769754576,-12.7219791159764,
116.314598254288)) ;
#186823 = CARTESIAN_POINT('Ctrl Pts',(-14.4149659085601,-12.7219791238396,
116.338829288067)) ;
#186824 = CARTESIAN_POINT('Ctrl Pts',(-14.3411620625442,-12.7219791317028,
116.363060321847)) ;
#186825 = CARTESIAN_POINT('Ctrl Pts',(-14.3240635905488,-12.6694591938587,
116.310981135199)) ;
#186826 = CARTESIAN_POINT('Ctrl Pts',(-14.3069651185534,-12.6169392560146,
116.258901948551)) ;
#186827 = CARTESIAN_POINT('Ctrl Pts',(-14.3807689645693,-12.6169392481514,
116.234670914771)) ;
#186828 = CARTESIAN_POINT('Ctrl Pts',(-14.4545728105852,-12.6169392402883,
116.210439880992)) ;
#186829 = CARTESIAN_POINT('Ctrl Pts',(-14.4716712825806,-12.6694591781323,
116.26251906764)) ;
#186830 = CARTESIAN_POINT('Ctrl Pts',(-14.4081656716587,-12.9054683696908,
116.104505284909)) ;
#186831 = CARTESIAN_POINT('Ctrl Pts',(-14.4289902353886,-12.9415855764778,
116.167933545647)) ;
#186832 = CARTESIAN_POINT('Ctrl Pts',(-14.3551863891245,-12.9415855922766,
116.19216457867)) ;
#186833 = CARTESIAN_POINT('Ctrl Pts',(-14.2813825428604,-12.9415856080754,
116.216395611693)) ;
#186834 = CARTESIAN_POINT('Ctrl Pts',(-14.2605579791305,-12.9054684012884,
116.152967350955)) ;
#186835 = CARTESIAN_POINT('Ctrl Pts',(-14.2397334154006,-12.8693511945013,
116.089539090218)) ;
#186836 = CARTESIAN_POINT('Ctrl Pts',(-14.3135372616647,-12.8693511787026,
116.065308057194)) ;
#186837 = CARTESIAN_POINT('Ctrl Pts',(-14.3873411079288,-12.8693511629038,
116.041077024171)) ;
#186838 = CARTESIAN_POINT('Ctrl Pts',(-14.4081656716587,-12.9054683696908,
116.104505284909)) ;
#186839 = CARTESIAN_POINT('Ctrl Pts',(-14.3659620806529,-13.1783417993353,
116.011426957597)) ;
#186840 = CARTESIAN_POINT('Ctrl Pts',(-14.389029628698,-13.1954587831432,
116.081686986504)) ;
#186841 = CARTESIAN_POINT('Ctrl Pts',(-14.3152257832912,-13.1954588083928,
116.105918022139)) ;
#186842 = CARTESIAN_POINT('Ctrl Pts',(-14.2414219378845,-13.1954588336424,
116.130149057773)) ;
#186843 = CARTESIAN_POINT('Ctrl Pts',(-14.2183543898394,-13.1783418498345,
116.059889028866)) ;
#186844 = CARTESIAN_POINT('Ctrl Pts',(-14.1952868417943,-13.1612248660266,
115.98962899996)) ;
#186845 = CARTESIAN_POINT('Ctrl Pts',(-14.269090687201,-13.161224840777,115.965397964325)) ;
#186846 = CARTESIAN_POINT('Ctrl Pts',(-14.3428945326078,-13.1612248155274,
115.941166928691)) ;
#186847 = CARTESIAN_POINT('Ctrl Pts',(-14.3659620806529,-13.1783417993353,
116.011426957597)) ;
#186848 = CARTESIAN_POINT('Ctrl Pts',(-14.3475114543578,-13.4677014527882,
115.990609557701)) ;
#186849 = CARTESIAN_POINT('Ctrl Pts',(-14.3711684091168,-13.4646398279822,
116.062664824212)) ;
#186850 = CARTESIAN_POINT('Ctrl Pts',(-14.2973645659806,-13.4646398615466,
116.086895866763)) ;
#186851 = CARTESIAN_POINT('Ctrl Pts',(-14.2235607228445,-13.464639895111,
116.111126909313)) ;
#186852 = CARTESIAN_POINT('Ctrl Pts',(-14.1999037680856,-13.4677015199171,
116.039071642802)) ;
#186853 = CARTESIAN_POINT('Ctrl Pts',(-14.1762468133266,-13.4707631447231,
115.967016376291)) ;
#186854 = CARTESIAN_POINT('Ctrl Pts',(-14.2500506564628,-13.4707631111587,
115.94278533374)) ;
#186855 = CARTESIAN_POINT('Ctrl Pts',(-14.3238544995989,-13.4707630775943,
115.91855429119)) ;
#186856 = CARTESIAN_POINT('Ctrl Pts',(-14.3475114543578,-13.4677014527882,
115.990609557701)) ;
#186857 = CARTESIAN_POINT('Ctrl Pts',(-14.3531957687261,-13.7542094632266,
116.043383175808)) ;
#186858 = CARTESIAN_POINT('Ctrl Pts',(-14.3757562745192,-13.7311394476093,
116.112098835515)) ;
#186859 = CARTESIAN_POINT('Ctrl Pts',(-14.3019524349061,-13.7311394879972,
116.136329888796)) ;
#186860 = CARTESIAN_POINT('Ctrl Pts',(-14.2281485952931,-13.7311395283851,
116.160560942077)) ;
#186861 = CARTESIAN_POINT('Ctrl Pts',(-14.2055880895,-13.7542095440024,116.09184528237)) ;
#186862 = CARTESIAN_POINT('Ctrl Pts',(-14.1830275837069,-13.7772795596197,
116.023129622664)) ;
#186863 = CARTESIAN_POINT('Ctrl Pts',(-14.25683142332,-13.7772795192318,115.998898569382)) ;
#186864 = CARTESIAN_POINT('Ctrl Pts',(-14.330635262933,-13.7772794788439,
115.974667516101)) ;
#186865 = CARTESIAN_POINT('Ctrl Pts',(-14.3531957687261,-13.7542094632266,
116.043383175808)) ;
#186866 = CARTESIAN_POINT('Ctrl Pts',(-14.3823024085504,-14.0177953901298,
116.167684414506)) ;
#186867 = CARTESIAN_POINT('Ctrl Pts',(-14.4021258436985,-13.976288401055,
116.228063398449)) ;
#186868 = CARTESIAN_POINT('Ctrl Pts',(-14.32832200916,-13.9762884453848,116.252294467187)) ;
#186869 = CARTESIAN_POINT('Ctrl Pts',(-14.2545181746215,-13.9762884897146,
116.276525535924)) ;
#186870 = CARTESIAN_POINT('Ctrl Pts',(-14.2346947394735,-14.0177954787893,
116.216146551981)) ;
#186871 = CARTESIAN_POINT('Ctrl Pts',(-14.2148713043254,-14.0593024678641,
116.155767568038)) ;
#186872 = CARTESIAN_POINT('Ctrl Pts',(-14.2886751388639,-14.0593024235343,
116.1315364993)) ;
#186873 = CARTESIAN_POINT('Ctrl Pts',(-14.3624789734024,-14.0593023792045,
116.107305430563)) ;
#186874 = CARTESIAN_POINT('Ctrl Pts',(-14.3823024085504,-14.0177953901298,
116.167684414506)) ;
#186875 = CARTESIAN_POINT('Ctrl Pts',(-14.4312100219503,-14.2358411050757,
116.351892811391)) ;
#186876 = CARTESIAN_POINT('Ctrl Pts',(-14.4469180075591,-14.1790508956255,
116.399736799939)) ;
#186877 = CARTESIAN_POINT('Ctrl Pts',(-14.3731141778863,-14.1790509350975,
116.423967883496)) ;
#186878 = CARTESIAN_POINT('Ctrl Pts',(-14.2993103482134,-14.1790509745695,
116.448198967053)) ;
#186879 = CARTESIAN_POINT('Ctrl Pts',(-14.2836023626046,-14.2358411840197,
116.400354978505)) ;
#186880 = CARTESIAN_POINT('Ctrl Pts',(-14.2678943769957,-14.2926313934699,
116.352510989957)) ;
#186881 = CARTESIAN_POINT('Ctrl Pts',(-14.3416982066686,-14.2926313539979,
116.3282799064)) ;
#186882 = CARTESIAN_POINT('Ctrl Pts',(-14.4155020363414,-14.2926313145259,
116.304048822843)) ;
#186883 = CARTESIAN_POINT('Ctrl Pts',(-14.4312100219503,-14.2358411050757,
116.351892811391)) ;
#186884 = CARTESIAN_POINT('Ctrl Pts',(-14.496559976539,-14.3973545116793,
116.586508356455)) ;
#186885 = CARTESIAN_POINT('Ctrl Pts',(-14.5069921514621,-14.3292054144305,
116.618283076722)) ;
#186886 = CARTESIAN_POINT('Ctrl Pts',(-14.4331883271676,-14.3292054449857,
116.642514176661)) ;
#186887 = CARTESIAN_POINT('Ctrl Pts',(-14.3593845028732,-14.3292054755409,
116.6667452766)) ;
#186888 = CARTESIAN_POINT('Ctrl Pts',(-14.3489523279501,-14.3973545727897,
116.634970556333)) ;
#186889 = CARTESIAN_POINT('Ctrl Pts',(-14.3385201530271,-14.4655036700385,
116.603195836066)) ;
#186890 = CARTESIAN_POINT('Ctrl Pts',(-14.4123239773215,-14.4655036394833,
116.578964736127)) ;
#186891 = CARTESIAN_POINT('Ctrl Pts',(-14.4861278016159,-14.4655036089281,
116.554733636188)) ;
#186892 = CARTESIAN_POINT('Ctrl Pts',(-14.496559976539,-14.3973545116793,
116.586508356455)) ;
#186893 = CARTESIAN_POINT('Ctrl Pts',(-14.5724186742539,-14.487909543941,
116.85304175223)) ;
#186894 = CARTESIAN_POINT('Ctrl Pts',(-14.5768355566869,-14.4133393487521,
116.866494861983)) ;
#186895 = CARTESIAN_POINT('Ctrl Pts',(-14.5030317366878,-14.4133393631785,
116.890725975005)) ;
#186896 = CARTESIAN_POINT('Ctrl Pts',(-14.4292279166886,-14.413339377605,
116.914957088027)) ;
#186897 = CARTESIAN_POINT('Ctrl Pts',(-14.4248110342556,-14.4879095727939,
116.901503978274)) ;
#186898 = CARTESIAN_POINT('Ctrl Pts',(-14.4203941518226,-14.5624797679828,
116.888050868521)) ;
#186899 = CARTESIAN_POINT('Ctrl Pts',(-14.4941979718218,-14.5624797535563,
116.863819755499)) ;
#186900 = CARTESIAN_POINT('Ctrl Pts',(-14.5680017918209,-14.5624797391299,
116.839588642478)) ;
#186901 = CARTESIAN_POINT('Ctrl Pts',(-14.5724186742539,-14.487909543941,
116.85304175223)) ;
#186902 = CARTESIAN_POINT('Ctrl Pts',(-14.6524842329724,-14.501998059837,
117.132307744548)) ;
#186903 = CARTESIAN_POINT('Ctrl Pts',(-14.6505851061445,-14.4263362561648,
117.126523309047)) ;
#186904 = CARTESIAN_POINT('Ctrl Pts',(-14.576781288592,-14.4263362496198,
117.15075442952)) ;
#186905 = CARTESIAN_POINT('Ctrl Pts',(-14.5029774710394,-14.4263362430748,
117.174985549994)) ;
#186906 = CARTESIAN_POINT('Ctrl Pts',(-14.5048765978673,-14.501998046747,
117.180769985496)) ;
#186907 = CARTESIAN_POINT('Ctrl Pts',(-14.5067757246951,-14.5776598504192,
117.186554420997)) ;
#186908 = CARTESIAN_POINT('Ctrl Pts',(-14.5805795422476,-14.5776598569642,
117.162323300523)) ;
#186909 = CARTESIAN_POINT('Ctrl Pts',(-14.6543833598002,-14.5776598635092,
117.13809218005)) ;
#186910 = CARTESIAN_POINT('Ctrl Pts',(-14.6524842329724,-14.501998059837,
117.132307744548)) ;
#186911 = CARTESIAN_POINT('Ctrl Pts',(-14.7306703976459,-14.4383564825309,
117.405946024149)) ;
#186912 = CARTESIAN_POINT('Ctrl Pts',(-14.7225753482943,-14.3670278101873,
117.381289808219)) ;
#186913 = CARTESIAN_POINT('Ctrl Pts',(-14.6487715312239,-14.3670277794582,
117.405520930161)) ;
#186914 = CARTESIAN_POINT('Ctrl Pts',(-14.5749677141534,-14.3670277487292,
117.429752052103)) ;
#186915 = CARTESIAN_POINT('Ctrl Pts',(-14.583062763505,-14.4383564210728,
117.454408268033)) ;
#186916 = CARTESIAN_POINT('Ctrl Pts',(-14.5911578128565,-14.5096850934165,
117.479064483963)) ;
#186917 = CARTESIAN_POINT('Ctrl Pts',(-14.6649616299269,-14.5096851241455,
117.454833362021)) ;
#186918 = CARTESIAN_POINT('Ctrl Pts',(-14.7387654469974,-14.5096851548746,
117.430602240079)) ;
#186919 = CARTESIAN_POINT('Ctrl Pts',(-14.7306703976459,-14.4383564825309,
117.405946024149)) ;
#186920 = CARTESIAN_POINT('Ctrl Pts',(-14.8002394306533,-14.3021834028963,
117.653221965588)) ;
#186921 = CARTESIAN_POINT('Ctrl Pts',(-14.7865434900334,-14.2402581580985,
117.611506338454)) ;
#186922 = CARTESIAN_POINT('Ctrl Pts',(-14.7127396708168,-14.2402581030473,
117.635737453859)) ;
#186923 = CARTESIAN_POINT('Ctrl Pts',(-14.6389358516002,-14.2402580479961,
117.659968569264)) ;
#186924 = CARTESIAN_POINT('Ctrl Pts',(-14.6526317922202,-14.3021832927938,
117.701684196398)) ;
#186925 = CARTESIAN_POINT('Ctrl Pts',(-14.6663277328401,-14.3641085375916,
117.743399823533)) ;
#186926 = CARTESIAN_POINT('Ctrl Pts',(-14.7401315520567,-14.3641085926428,
117.719168708127)) ;
#186927 = CARTESIAN_POINT('Ctrl Pts',(-14.8139353712733,-14.364108647694,
117.694937592722)) ;
#186928 = CARTESIAN_POINT('Ctrl Pts',(-14.8002394306533,-14.3021834028963,
117.653221965588)) ;
#186929 = CARTESIAN_POINT('Ctrl Pts',(-14.8560459100839,-14.1010124276425,
117.858868514753)) ;
#186930 = CARTESIAN_POINT('Ctrl Pts',(-14.8376956312076,-14.0530410261757,
117.802976524153)) ;
#186931 = CARTESIAN_POINT('Ctrl Pts',(-14.7638918076274,-14.0530409478965,
117.827207626268)) ;
#186932 = CARTESIAN_POINT('Ctrl Pts',(-14.6900879840472,-14.0530408696173,
117.851438728382)) ;
#186933 = CARTESIAN_POINT('Ctrl Pts',(-14.7084382629236,-14.101012271084,
117.907330718982)) ;
#186934 = CARTESIAN_POINT('Ctrl Pts',(-14.7267885417999,-14.1489836725507,
117.963222709582)) ;
#186935 = CARTESIAN_POINT('Ctrl Pts',(-14.8005923653801,-14.14898375083,117.938991607467)) ;
#186936 = CARTESIAN_POINT('Ctrl Pts',(-14.8743961889603,-14.1489838291092,
117.914760505353)) ;
#186937 = CARTESIAN_POINT('Ctrl Pts',(-14.8560459100839,-14.1010124276425,
117.858868514753)) ;
#186938 = CARTESIAN_POINT('Ctrl Pts',(-14.8924029143783,-13.8533300885713,
118.004875316646)) ;
#186939 = CARTESIAN_POINT('Ctrl Pts',(-14.8707577701644,-13.822581157602,
117.938947697799)) ;
#186940 = CARTESIAN_POINT('Ctrl Pts',(-14.7969539397415,-13.8225810627118,
117.963178779072)) ;
#186941 = CARTESIAN_POINT('Ctrl Pts',(-14.7231501093185,-13.8225809678216,
117.987409860344)) ;
#186942 = CARTESIAN_POINT('Ctrl Pts',(-14.7447952535323,-13.8533298987908,
118.053337479191)) ;
#186943 = CARTESIAN_POINT('Ctrl Pts',(-14.7664403977462,-13.8840788297601,
118.119265098038)) ;
#186944 = CARTESIAN_POINT('Ctrl Pts',(-14.8402442281691,-13.8840789246503,
118.095034016765)) ;
#186945 = CARTESIAN_POINT('Ctrl Pts',(-14.9140480585921,-13.8840790195405,
118.070802935493)) ;
#186946 = CARTESIAN_POINT('Ctrl Pts',(-14.8924029143783,-13.8533300885713,
118.004875316646)) ;
#186947 = CARTESIAN_POINT('Ctrl Pts',(-14.9068420422244,-13.5731370136184,
118.084346390465)) ;
#186948 = CARTESIAN_POINT('Ctrl Pts',(-14.8834226218003,-13.5619047330003,
118.013014612504)) ;
#186949 = CARTESIAN_POINT('Ctrl Pts',(-14.8096187831826,-13.5619046275825,
118.037245668817)) ;
#186950 = CARTESIAN_POINT('Ctrl Pts',(-14.735814944565,-13.5619045221647,
118.061476725129)) ;
#186951 = CARTESIAN_POINT('Ctrl Pts',(-14.7592343649891,-13.5731368027828,
118.132808503091)) ;
#186952 = CARTESIAN_POINT('Ctrl Pts',(-14.7826537854132,-13.5843690834008,
118.204140281052)) ;
#186953 = CARTESIAN_POINT('Ctrl Pts',(-14.8564576240309,-13.5843691888186,
118.179909224739)) ;
#186954 = CARTESIAN_POINT('Ctrl Pts',(-14.9302614626486,-13.5843692942365,
118.155678168426)) ;
#186955 = CARTESIAN_POINT('Ctrl Pts',(-14.9068420422244,-13.5731370136184,
118.084346390465)) ;
#186956 = CARTESIAN_POINT('Ctrl Pts',(-14.8970281712621,-13.2811248351023,
118.09002242941)) ;
#186957 = CARTESIAN_POINT('Ctrl Pts',(-14.873523327877,-13.2902630338005,
118.018430466862)) ;
#186958 = CARTESIAN_POINT('Ctrl Pts',(-14.7997194802372,-13.2902629265376,
118.042661495695)) ;
#186959 = CARTESIAN_POINT('Ctrl Pts',(-14.7259156325975,-13.2902628192747,
118.066892524528)) ;
#186960 = CARTESIAN_POINT('Ctrl Pts',(-14.7494204759826,-13.2811246205765,
118.138484487076)) ;
#186961 = CARTESIAN_POINT('Ctrl Pts',(-14.7729253193677,-13.2719864218783,
118.210076449624)) ;
#186962 = CARTESIAN_POINT('Ctrl Pts',(-14.8467291670075,-13.2719865291412,
118.185845420791)) ;
#186963 = CARTESIAN_POINT('Ctrl Pts',(-14.9205330146472,-13.2719866364041,
118.161614391958)) ;
#186964 = CARTESIAN_POINT('Ctrl Pts',(-14.8970281712621,-13.2811248351023,
118.09002242941)) ;
#186965 = CARTESIAN_POINT('Ctrl Pts',(-14.8632710167406,-13.0003515927813,
118.022582055255)) ;
#186966 = CARTESIAN_POINT('Ctrl Pts',(-14.8413562508323,-13.0291058472193,
117.955833212136)) ;
#186967 = CARTESIAN_POINT('Ctrl Pts',(-14.7675523944075,-13.029105747077,
117.980064214212)) ;
#186968 = CARTESIAN_POINT('Ctrl Pts',(-14.6937485379827,-13.0291056469348,
118.004295216287)) ;
#186969 = CARTESIAN_POINT('Ctrl Pts',(-14.715663303891,-13.0003513924967,
118.071044059405)) ;
#186970 = CARTESIAN_POINT('Ctrl Pts',(-14.7375780697992,-12.9715971380587,
118.137792902524)) ;
#186971 = CARTESIAN_POINT('Ctrl Pts',(-14.811381926224,-12.971597238201,118.113561900449)) ;
#186972 = CARTESIAN_POINT('Ctrl Pts',(-14.8851857826488,-12.9715973383433,
118.089330898374)) ;
#186973 = CARTESIAN_POINT('Ctrl Pts',(-14.8632710167406,-13.0003515927813,
118.022582055255)) ;
#186974 = CARTESIAN_POINT('Ctrl Pts',(-14.8066072910896,-12.7476820967297,
117.885649589391)) ;
#186975 = CARTESIAN_POINT('Ctrl Pts',(-14.7878780661755,-12.7941196142379,
117.828603390177)) ;
#186976 = CARTESIAN_POINT('Ctrl Pts',(-14.7140742020926,-12.794119529764,
117.852834368926)) ;
#186977 = CARTESIAN_POINT('Ctrl Pts',(-14.6402703380096,-12.7941194452901,
117.877065347676)) ;
#186978 = CARTESIAN_POINT('Ctrl Pts',(-14.6589995629237,-12.7476819277819,
117.93411154689)) ;
#186979 = CARTESIAN_POINT('Ctrl Pts',(-14.6777287878378,-12.7012444102737,
117.991157746104)) ;
#186980 = CARTESIAN_POINT('Ctrl Pts',(-14.7515326519207,-12.7012444947476,
117.966926767354)) ;
#186981 = CARTESIAN_POINT('Ctrl Pts',(-14.8253365160036,-12.7012445792215,
117.942695788605)) ;
#186982 = CARTESIAN_POINT('Ctrl Pts',(-14.8066072910896,-12.7476820967297,
117.885649589391)) ;
#186983 = CARTESIAN_POINT('Ctrl Pts',(-14.731619858714,-12.5456564605608,
117.692468627956)) ;
#186984 = CARTESIAN_POINT('Ctrl Pts',(-14.7173696349214,-12.6062676271749,
117.649064743502)) ;
#186985 = CARTESIAN_POINT('Ctrl Pts',(-14.6435657649829,-12.6062675641062,
117.673295704416)) ;
#186986 = CARTESIAN_POINT('Ctrl Pts',(-14.5697618950443,-12.6062675010375,
117.697526665331)) ;
#186987 = CARTESIAN_POINT('Ctrl Pts',(-14.584012118837,-12.5456563344234,
117.740930549785)) ;
#186988 = CARTESIAN_POINT('Ctrl Pts',(-14.5982623426296,-12.4850451678094,
117.784334434238)) ;
#186989 = CARTESIAN_POINT('Ctrl Pts',(-14.6720662125682,-12.4850452308781,
117.760103473324)) ;
#186990 = CARTESIAN_POINT('Ctrl Pts',(-14.7458700825067,-12.4850452939468,
117.735872512409)) ;
#186991 = CARTESIAN_POINT('Ctrl Pts',(-14.731619858714,-12.5456564605608,
117.692468627956)) ;
#186992 = CARTESIAN_POINT('Ctrl Pts',(-14.6415003508754,-12.4041536111177,
117.453518839536)) ;
#186993 = CARTESIAN_POINT('Ctrl Pts',(-14.6327852655242,-12.4747346832578,
117.426974093744)) ;
#186994 = CARTESIAN_POINT('Ctrl Pts',(-14.5589813922061,-12.474734646304,
117.451205044365)) ;
#186995 = CARTESIAN_POINT('Ctrl Pts',(-14.485177518888,-12.4747346093502,
117.475435994985)) ;
#186996 = CARTESIAN_POINT('Ctrl Pts',(-14.4938926042392,-12.4041535372102,
117.501980740777)) ;
#186997 = CARTESIAN_POINT('Ctrl Pts',(-14.5026076895904,-12.3335724650701,
117.528525486569)) ;
#186998 = CARTESIAN_POINT('Ctrl Pts',(-14.5764115629085,-12.3335725020239,
117.504294535948)) ;
#186999 = CARTESIAN_POINT('Ctrl Pts',(-14.6502154362266,-12.3335725389777,
117.480063585327)) ;
#187000 = CARTESIAN_POINT('Ctrl Pts',(-14.6415003508754,-12.4041536111177,
117.453518839536)) ;
#187001 = CARTESIAN_POINT('Ctrl Pts',(-14.5427756645505,-12.3358248594298,
117.188253387746)) ;
#187002 = CARTESIAN_POINT('Ctrl Pts',(-14.540207049171,-12.4112821257934,
117.180429797836)) ;
#187003 = CARTESIAN_POINT('Ctrl Pts',(-14.4664031750961,-12.4112821160611,
117.204660746152)) ;
#187004 = CARTESIAN_POINT('Ctrl Pts',(-14.3925993010213,-12.4112821063287,
117.228891694468)) ;
#187005 = CARTESIAN_POINT('Ctrl Pts',(-14.3951679164008,-12.3358248399652,
117.236715284378)) ;
#187006 = CARTESIAN_POINT('Ctrl Pts',(-14.3977365317803,-12.2603675736016,
117.244538874289)) ;
#187007 = CARTESIAN_POINT('Ctrl Pts',(-14.4715404058551,-12.2603675833339,
117.220307925973)) ;
#187008 = CARTESIAN_POINT('Ctrl Pts',(-14.54534427993,-12.2603675930662,117.196076977657)) ;
#187009 = CARTESIAN_POINT('Ctrl Pts',(-14.5427756645505,-12.3358248594298,
117.188253387746)) ;
#187010 = CARTESIAN_POINT('Ctrl Pts',(-14.4412974521352,-12.3448661715,116.914695399422)) ;
#187011 = CARTESIAN_POINT('Ctrl Pts',(-14.445074775662,-12.4198057290159,
116.926200515611)) ;
#187012 = CARTESIAN_POINT('Ctrl Pts',(-14.3712709035495,-12.41980574501,116.950431469904)) ;
#187013 = CARTESIAN_POINT('Ctrl Pts',(-14.2974670314371,-12.4198057610042,
116.974662424197)) ;
#187014 = CARTESIAN_POINT('Ctrl Pts',(-14.2936897079104,-12.3448662034884,
116.963157308008)) ;
#187015 = CARTESIAN_POINT('Ctrl Pts',(-14.2899123843836,-12.2699266459725,
116.95165219182)) ;
#187016 = CARTESIAN_POINT('Ctrl Pts',(-14.363716256496,-12.2699266299783,
116.927421237527)) ;
#187017 = CARTESIAN_POINT('Ctrl Pts',(-14.4375201286084,-12.2699266139842,
116.903190283233)) ;
#187018 = CARTESIAN_POINT('Ctrl Pts',(-14.4412974521352,-12.3448661715,116.914695399422)) ;
#187019 = CARTESIAN_POINT('Ctrl Pts',(-14.343860133739,-12.4312374679016,
116.653442961443)) ;
#187020 = CARTESIAN_POINT('Ctrl Pts',(-14.3537109607349,-12.5002598101882,
116.683446989369)) ;
#187021 = CARTESIAN_POINT('Ctrl Pts',(-14.2799070928255,-12.5002598472916,
116.707677956464)) ;
#187022 = CARTESIAN_POINT('Ctrl Pts',(-14.206103224916,-12.5002598843951,
116.731908923559)) ;
#187023 = CARTESIAN_POINT('Ctrl Pts',(-14.1962523979201,-12.4312375421085,
116.701904895633)) ;
#187024 = CARTESIAN_POINT('Ctrl Pts',(-14.1864015709241,-12.3622151998219,
116.671900867707)) ;
#187025 = CARTESIAN_POINT('Ctrl Pts',(-14.2602054388336,-12.3622151627184,
116.647669900612)) ;
#187026 = CARTESIAN_POINT('Ctrl Pts',(-14.334009306743,-12.362215125615,116.623438933518)) ;
#187027 = CARTESIAN_POINT('Ctrl Pts',(-14.343860133739,-12.4312374679016,
116.653442961443)) ;
#187028 = CARTESIAN_POINT('Ctrl Pts',(-14.2571254625577,-12.5874506151636,
116.424600508651)) ;
#187029 = CARTESIAN_POINT('Ctrl Pts',(-14.2723156315512,-12.6456701044934,
116.470867310915)) ;
#187030 = CARTESIAN_POINT('Ctrl Pts',(-14.1985117689653,-12.6456701572597,
116.495098294225)) ;
#187031 = CARTESIAN_POINT('Ctrl Pts',(-14.1247079063794,-12.6456702100259,
116.519329277534)) ;
#187032 = CARTESIAN_POINT('Ctrl Pts',(-14.1095177373858,-12.5874507206961,
116.47306247527)) ;
#187033 = CARTESIAN_POINT('Ctrl Pts',(-14.0943275683923,-12.5292312313663,
116.426795673006)) ;
#187034 = CARTESIAN_POINT('Ctrl Pts',(-14.1681314309782,-12.5292311786001,
116.402564689697)) ;
#187035 = CARTESIAN_POINT('Ctrl Pts',(-14.2419352935641,-12.5292311258338,
116.378333706388)) ;
#187036 = CARTESIAN_POINT('Ctrl Pts',(-14.2571254625577,-12.5874506151636,
116.424600508651)) ;
#187037 = CARTESIAN_POINT('Ctrl Pts',(-14.1857294690377,-12.8034012905554,
116.242593659253)) ;
#187038 = CARTESIAN_POINT('Ctrl Pts',(-14.2051937787915,-12.8466312900345,
116.301878804784)) ;
#187039 = CARTESIAN_POINT('Ctrl Pts',(-14.1313899225984,-12.8466313512928,
116.326109807565)) ;
#187040 = CARTESIAN_POINT('Ctrl Pts',(-14.0575860664052,-12.8466314125512,
116.350340810346)) ;
#187041 = CARTESIAN_POINT('Ctrl Pts',(-14.0381217566514,-12.8034014130721,
116.291055664815)) ;
#187042 = CARTESIAN_POINT('Ctrl Pts',(-14.0186574468976,-12.760171413593,
116.231770519284)) ;
#187043 = CARTESIAN_POINT('Ctrl Pts',(-14.0924613030908,-12.7601713523347,
116.207539516503)) ;
#187044 = CARTESIAN_POINT('Ctrl Pts',(-14.1662651592839,-12.7601712910763,
116.183308513722)) ;
#187045 = CARTESIAN_POINT('Ctrl Pts',(-14.1857294690377,-12.8034012905554,
116.242593659253)) ;
#187046 = CARTESIAN_POINT('Ctrl Pts',(-14.1342915112544,-13.0643708673509,
116.121492146728)) ;
#187047 = CARTESIAN_POINT('Ctrl Pts',(-14.1566407442375,-13.0894456413712,
116.18956430311)) ;
#187048 = CARTESIAN_POINT('Ctrl Pts',(-14.0828368945042,-13.0894457028003,
116.213795325566)) ;
#187049 = CARTESIAN_POINT('Ctrl Pts',(-14.009033044771,-13.0894457642295,
116.238026348023)) ;
#187050 = CARTESIAN_POINT('Ctrl Pts',(-13.9866838117879,-13.0643709902092,
116.169954191642)) ;
#187051 = CARTESIAN_POINT('Ctrl Pts',(-13.9643345788048,-13.0392962161889,
116.10188203526)) ;
#187052 = CARTESIAN_POINT('Ctrl Pts',(-14.0381384285381,-13.0392961547597,
116.077651012804)) ;
#187053 = CARTESIAN_POINT('Ctrl Pts',(-14.1119422782713,-13.0392960933306,
116.053419990347)) ;
#187054 = CARTESIAN_POINT('Ctrl Pts',(-14.1342915112544,-13.0643708673509,
116.121492146728)) ;
#187055 = CARTESIAN_POINT('Ctrl Pts',(-14.1060138274789,-13.3499213722247,
116.070822960069)) ;
#187056 = CARTESIAN_POINT('Ctrl Pts',(-14.1296375462713,-13.355096833582,
116.142776994751)) ;
#187057 = CARTESIAN_POINT('Ctrl Pts',(-14.0558337020276,-13.3550968897529,
116.167008033928)) ;
#187058 = CARTESIAN_POINT('Ctrl Pts',(-13.982029857784,-13.3550969459238,
116.191239073105)) ;
#187059 = CARTESIAN_POINT('Ctrl Pts',(-13.9584061389915,-13.3499214845666,
116.119285038423)) ;
#187060 = CARTESIAN_POINT('Ctrl Pts',(-13.9347824201991,-13.3447460232093,
116.047331003741)) ;
#187061 = CARTESIAN_POINT('Ctrl Pts',(-14.0085862644428,-13.3447459670383,
116.023099964565)) ;
#187062 = CARTESIAN_POINT('Ctrl Pts',(-14.0823901086865,-13.3447459108674,
115.998868925388)) ;
#187063 = CARTESIAN_POINT('Ctrl Pts',(-14.1060138274789,-13.3499213722247,
116.070822960069)) ;
#187064 = CARTESIAN_POINT('Ctrl Pts',(-14.1020431169035,-13.6410985525755,
116.094287590877)) ;
#187065 = CARTESIAN_POINT('Ctrl Pts',(-14.1252441893859,-13.6259514029626,
116.164954313278)) ;
#187066 = CARTESIAN_POINT('Ctrl Pts',(-14.0514403491928,-13.625951448446,
116.189185364793)) ;
#187067 = CARTESIAN_POINT('Ctrl Pts',(-13.9776365089998,-13.6259514939294,
116.213416416307)) ;
#187068 = CARTESIAN_POINT('Ctrl Pts',(-13.9544354365173,-13.6410986435423,
116.142749693906)) ;
#187069 = CARTESIAN_POINT('Ctrl Pts',(-13.9312343640349,-13.6562457931553,
116.072082971505)) ;
#187070 = CARTESIAN_POINT('Ctrl Pts',(-14.0050382042279,-13.6562457476719,
116.04785191999)) ;
#187071 = CARTESIAN_POINT('Ctrl Pts',(-14.078842044421,-13.6562457021885,
116.023620868476)) ;
#187072 = CARTESIAN_POINT('Ctrl Pts',(-14.1020431169035,-13.6410985525755,
116.094287590877)) ;
#187073 = CARTESIAN_POINT('Ctrl Pts',(-14.1217724434522,-13.9144130152127,
116.189693352615)) ;
#187074 = CARTESIAN_POINT('Ctrl Pts',(-14.142900281541,-13.8801596021724,
116.254045337708)) ;
#187075 = CARTESIAN_POINT('Ctrl Pts',(-14.06909644393,-13.8801596369213,116.278276397087)) ;
#187076 = CARTESIAN_POINT('Ctrl Pts',(-13.995292606319,-13.8801596716703,
116.302507456466)) ;
#187077 = CARTESIAN_POINT('Ctrl Pts',(-13.9741647682302,-13.9144130847105,
116.238155471373)) ;
#187078 = CARTESIAN_POINT('Ctrl Pts',(-13.9530369301413,-13.9486664977508,
116.173803486281)) ;
#187079 = CARTESIAN_POINT('Ctrl Pts',(-14.0268407677523,-13.9486664630018,
116.149572426902)) ;
#187080 = CARTESIAN_POINT('Ctrl Pts',(-14.1006446053633,-13.9486664282529,
116.125341367522)) ;
#187081 = CARTESIAN_POINT('Ctrl Pts',(-14.1217724434522,-13.9144130152127,
116.189693352615)) ;
#187082 = CARTESIAN_POINT('Ctrl Pts',(-14.1631227784727,-14.1534993419982,
116.351109244316)) ;
#187083 = CARTESIAN_POINT('Ctrl Pts',(-14.1806614860516,-14.1025003039047,
116.404529317146)) ;
#187084 = CARTESIAN_POINT('Ctrl Pts',(-14.1068576493241,-14.1025003260636,
116.428760379216)) ;
#187085 = CARTESIAN_POINT('Ctrl Pts',(-14.0330538125967,-14.1025003482225,
116.452991441286)) ;
#187086 = CARTESIAN_POINT('Ctrl Pts',(-14.0155151050178,-14.153499386316,
116.399571368456)) ;
#187087 = CARTESIAN_POINT('Ctrl Pts',(-13.9979763974389,-14.2044984244094,
116.346151295626)) ;
#187088 = CARTESIAN_POINT('Ctrl Pts',(-14.0717802341664,-14.2044984022505,
116.321920233556)) ;
#187089 = CARTESIAN_POINT('Ctrl Pts',(-14.1455840708938,-14.2044983800916,
116.297689171486)) ;
#187090 = CARTESIAN_POINT('Ctrl Pts',(-14.1631227784727,-14.1534993419982,
116.351109244316)) ;
#187091 = CARTESIAN_POINT('Ctrl Pts',(-14.2224761505657,-14.3398532357648,
116.567378763877)) ;
#187092 = CARTESIAN_POINT('Ctrl Pts',(-14.2351627561795,-14.2757649069183,
116.606020117166)) ;
#187093 = CARTESIAN_POINT('Ctrl Pts',(-14.1613589188212,-14.275764918267,
116.630251177315)) ;
#187094 = CARTESIAN_POINT('Ctrl Pts',(-14.0875550814629,-14.2757649296157,
116.654482237464)) ;
#187095 = CARTESIAN_POINT('Ctrl Pts',(-14.074868475849,-14.3398532584622,
116.615840884175)) ;
#187096 = CARTESIAN_POINT('Ctrl Pts',(-14.0621818702352,-14.4039415873087,
116.577199530885)) ;
#187097 = CARTESIAN_POINT('Ctrl Pts',(-14.1359857075935,-14.4039415759601,
116.552968470736)) ;
#187098 = CARTESIAN_POINT('Ctrl Pts',(-14.2097895449518,-14.4039415646114,
116.528737410587)) ;
#187099 = CARTESIAN_POINT('Ctrl Pts',(-14.2224761505657,-14.3398532357648,
116.567378763877)) ;
#187100 = CARTESIAN_POINT('Ctrl Pts',(-14.2946184727388,-14.4601239905911,
116.822545240019)) ;
#187101 = CARTESIAN_POINT('Ctrl Pts',(-14.3015537228685,-14.3875409587586,
116.843668892623)) ;
#187102 = CARTESIAN_POINT('Ctrl Pts',(-14.2277498840453,-14.3875409624437,
116.86789994831)) ;
#187103 = CARTESIAN_POINT('Ctrl Pts',(-14.153946045222,-14.3875409661288,
116.892131003996)) ;
#187104 = CARTESIAN_POINT('Ctrl Pts',(-14.1470107950923,-14.4601239979614,
116.871007351393)) ;
#187105 = CARTESIAN_POINT('Ctrl Pts',(-14.1400755449626,-14.532707029794,
116.849883698789)) ;
#187106 = CARTESIAN_POINT('Ctrl Pts',(-14.2138793837858,-14.5327070261088,
116.825652643102)) ;
#187107 = CARTESIAN_POINT('Ctrl Pts',(-14.2876832226091,-14.5327070224237,
116.801421587416)) ;
#187108 = CARTESIAN_POINT('Ctrl Pts',(-14.2946184727388,-14.4601239905911,
116.822545240019)) ;
#187109 = CARTESIAN_POINT('Ctrl Pts',(-14.3741114267092,-14.5056532387337,
117.100264991934)) ;
#187110 = CARTESIAN_POINT('Ctrl Pts',(-14.3747697725925,-14.4297812015044,
117.102270207122)) ;
#187111 = CARTESIAN_POINT('Ctrl Pts',(-14.3009659315983,-14.4297812011716,
117.126501256196)) ;
#187112 = CARTESIAN_POINT('Ctrl Pts',(-14.227162090604,-14.4297812008388,
117.150732305271)) ;
#187113 = CARTESIAN_POINT('Ctrl Pts',(-14.2265037447207,-14.5056532380682,
117.148727090083)) ;
#187114 = CARTESIAN_POINT('Ctrl Pts',(-14.2258453988374,-14.5815252752975,
117.146721874895)) ;
#187115 = CARTESIAN_POINT('Ctrl Pts',(-14.2996492398317,-14.5815252756303,
117.122490825821)) ;
#187116 = CARTESIAN_POINT('Ctrl Pts',(-14.3734530808259,-14.5815252759631,
117.098259776747)) ;
#187117 = CARTESIAN_POINT('Ctrl Pts',(-14.3741114267092,-14.5056532387337,
117.100264991934)) ;
#187118 = CARTESIAN_POINT('Ctrl Pts',(-14.4533987795497,-14.4736304498916,
117.377007393314)) ;
#187119 = CARTESIAN_POINT('Ctrl Pts',(-14.4477925032055,-14.3998809483868,
117.35993158007)) ;
#187120 = CARTESIAN_POINT('Ctrl Pts',(-14.3739886608311,-14.3998809471274,
117.384162624941)) ;
#187121 = CARTESIAN_POINT('Ctrl Pts',(-14.3001848184568,-14.399880945868,
117.408393669812)) ;
#187122 = CARTESIAN_POINT('Ctrl Pts',(-14.305791094801,-14.4736304473727,
117.425469483055)) ;
#187123 = CARTESIAN_POINT('Ctrl Pts',(-14.3113973711451,-14.5473799488775,
117.442545296299)) ;
#187124 = CARTESIAN_POINT('Ctrl Pts',(-14.3852012135195,-14.5473799501369,
117.418314251428)) ;
#187125 = CARTESIAN_POINT('Ctrl Pts',(-14.4590050558939,-14.5473799513963,
117.394083206557)) ;
#187126 = CARTESIAN_POINT('Ctrl Pts',(-14.4533987795497,-14.4736304498916,
117.377007393314)) ;
#187127 = CARTESIAN_POINT('Ctrl Pts',(-14.5277960537178,-14.3649486844788,
117.639339779354)) ;
#187128 = CARTESIAN_POINT('Ctrl Pts',(-14.5162467148877,-14.2986771390851,
117.604162356787)) ;
#187129 = CARTESIAN_POINT('Ctrl Pts',(-14.4424428710041,-14.2986771395707,
117.628393397061)) ;
#187130 = CARTESIAN_POINT('Ctrl Pts',(-14.3686390271205,-14.2986771400562,
117.652624437334)) ;
#187131 = CARTESIAN_POINT('Ctrl Pts',(-14.3801883659506,-14.36494868545,117.687801859902)) ;
#187132 = CARTESIAN_POINT('Ctrl Pts',(-14.3917377047807,-14.4312202308437,
117.722979282469)) ;
#187133 = CARTESIAN_POINT('Ctrl Pts',(-14.4655415486643,-14.4312202303581,
117.698748242195)) ;
#187134 = CARTESIAN_POINT('Ctrl Pts',(-14.5393453925479,-14.4312202298725,
117.674517201921)) ;
#187135 = CARTESIAN_POINT('Ctrl Pts',(-14.5277960537178,-14.3649486844788,
117.639339779354)) ;
#187136 = CARTESIAN_POINT('Ctrl Pts',(-14.5893935819376,-14.1895250687342,
117.862280414285)) ;
#187137 = CARTESIAN_POINT('Ctrl Pts',(-14.5727948609667,-14.1354046364552,
117.81172338846)) ;
#187138 = CARTESIAN_POINT('Ctrl Pts',(-14.4989910168738,-14.1354046385753,
117.835954428096)) ;
#187139 = CARTESIAN_POINT('Ctrl Pts',(-14.4251871727808,-14.1354046406955,
117.860185467732)) ;
#187140 = CARTESIAN_POINT('Ctrl Pts',(-14.4417858937517,-14.1895250729745,
117.910742493557)) ;
#187141 = CARTESIAN_POINT('Ctrl Pts',(-14.4583846147226,-14.2436455052536,
117.961299519382)) ;
#187142 = CARTESIAN_POINT('Ctrl Pts',(-14.5321884588155,-14.2436455031334,
117.937068479746)) ;
#187143 = CARTESIAN_POINT('Ctrl Pts',(-14.6059923029085,-14.2436455010133,
117.91283744011)) ;
#187144 = CARTESIAN_POINT('Ctrl Pts',(-14.5893935819376,-14.1895250687342,
117.862280414285)) ;
#187145 = CARTESIAN_POINT('Ctrl Pts',(-14.6341408629526,-13.9587919846541,
118.03400595603)) ;
#187146 = CARTESIAN_POINT('Ctrl Pts',(-14.6136596183547,-13.9207033555361,
117.971623389682)) ;
#187147 = CARTESIAN_POINT('Ctrl Pts',(-14.5398557744747,-13.9207033583064,
117.995854429967)) ;
#187148 = CARTESIAN_POINT('Ctrl Pts',(-14.4660519305947,-13.9207033610767,
118.020085470252)) ;
#187149 = CARTESIAN_POINT('Ctrl Pts',(-14.4865331751926,-13.9587919901947,
118.0824680366)) ;
#187150 = CARTESIAN_POINT('Ctrl Pts',(-14.5070144197905,-13.9968806193127,
118.144850602948)) ;
#187151 = CARTESIAN_POINT('Ctrl Pts',(-14.5808182636705,-13.9968806165424,
118.120619562663)) ;
#187152 = CARTESIAN_POINT('Ctrl Pts',(-14.6546221075505,-13.9968806137721,
118.096388522378)) ;
#187153 = CARTESIAN_POINT('Ctrl Pts',(-14.6341408629526,-13.9587919846541,
118.03400595603)) ;
#187154 = CARTESIAN_POINT('Ctrl Pts',(-14.6578474674141,-13.6889251841896,
118.141687163371)) ;
#187155 = CARTESIAN_POINT('Ctrl Pts',(-14.6349465238755,-13.6696247434328,
118.071934584426)) ;
#187156 = CARTESIAN_POINT('Ctrl Pts',(-14.5611426804866,-13.6696247444935,
118.096165626206)) ;
#187157 = CARTESIAN_POINT('Ctrl Pts',(-14.4873388370977,-13.6696247455542,
118.120396667987)) ;
#187158 = CARTESIAN_POINT('Ctrl Pts',(-14.5102397806364,-13.688925186311,
118.190149246933)) ;
#187159 = CARTESIAN_POINT('Ctrl Pts',(-14.533140724175,-13.7082256270677,
118.259901825878)) ;
#187160 = CARTESIAN_POINT('Ctrl Pts',(-14.6069445675639,-13.708225626007,
118.235670784098)) ;
#187161 = CARTESIAN_POINT('Ctrl Pts',(-14.6807484109528,-13.7082256249463,
118.211439742317)) ;
#187162 = CARTESIAN_POINT('Ctrl Pts',(-14.6578474674141,-13.6889251841896,
118.141687163371)) ;
#187163 = CARTESIAN_POINT('Ctrl Pts',(-14.6579187734562,-13.3992086458092,
118.177435917564)) ;
#187164 = CARTESIAN_POINT('Ctrl Pts',(-14.6342439439393,-13.4001099249718,
118.10532620671)) ;
#187165 = CARTESIAN_POINT('Ctrl Pts',(-14.5604401006268,-13.4001099216027,
118.129557248723)) ;
#187166 = CARTESIAN_POINT('Ctrl Pts',(-14.4866362573143,-13.4001099182335,
118.153788290736)) ;
#187167 = CARTESIAN_POINT('Ctrl Pts',(-14.5103110868312,-13.3992086390708,
118.225898001591)) ;
#187168 = CARTESIAN_POINT('Ctrl Pts',(-14.5339859163481,-13.3983073599082,
118.298007712445)) ;
#187169 = CARTESIAN_POINT('Ctrl Pts',(-14.6077897596606,-13.3983073632774,
118.273776670431)) ;
#187170 = CARTESIAN_POINT('Ctrl Pts',(-14.6815936029731,-13.3983073666465,
118.249545628418)) ;
#187171 = CARTESIAN_POINT('Ctrl Pts',(-14.6579187734562,-13.3992086458092,
118.177435917564)) ;
#187172 = CARTESIAN_POINT('Ctrl Pts',(-14.6338690635927,-13.1124266878776,
118.139508403159)) ;
#187173 = CARTESIAN_POINT('Ctrl Pts',(-14.6111080927267,-13.13335350732,118.070182158217)) ;
#187174 = CARTESIAN_POINT('Ctrl Pts',(-14.5373042487991,-13.1333534995856,
118.094413198357)) ;
#187175 = CARTESIAN_POINT('Ctrl Pts',(-14.4635004048714,-13.1333534918511,
118.118644238497)) ;
#187176 = CARTESIAN_POINT('Ctrl Pts',(-14.4862613757375,-13.1124266724087,
118.187970483438)) ;
#187177 = CARTESIAN_POINT('Ctrl Pts',(-14.5090223466035,-13.0914998529662,
118.257296728379)) ;
#187178 = CARTESIAN_POINT('Ctrl Pts',(-14.5828261905311,-13.0914998607007,
118.233065688239)) ;
#187179 = CARTESIAN_POINT('Ctrl Pts',(-14.6566300344588,-13.0914998684351,
118.2088346481)) ;
#187180 = CARTESIAN_POINT('Ctrl Pts',(-14.6338690635927,-13.1124266878776,
118.139508403159)) ;
#187181 = CARTESIAN_POINT('Ctrl Pts',(-14.5860912781424,-12.8450096600115,
118.029650693302)) ;
#187182 = CARTESIAN_POINT('Ctrl Pts',(-14.5658950360717,-12.8846394195873,
117.968136198297)) ;
#187183 = CARTESIAN_POINT('Ctrl Pts',(-14.492091190218,-12.8846394056337,
117.99236723257)) ;
#187184 = CARTESIAN_POINT('Ctrl Pts',(-14.4182873443643,-12.8846393916802,
118.016598266843)) ;
#187185 = CARTESIAN_POINT('Ctrl Pts',(-14.4384835864349,-12.8450096321044,
118.078112761848)) ;
#187186 = CARTESIAN_POINT('Ctrl Pts',(-14.4586798285056,-12.8053798725287,
118.139627256853)) ;
#187187 = CARTESIAN_POINT('Ctrl Pts',(-14.5324836743593,-12.8053798864822,
118.11539622258)) ;
#187188 = CARTESIAN_POINT('Ctrl Pts',(-14.606287520213,-12.8053799004358,
118.091165188307)) ;
#187189 = CARTESIAN_POINT('Ctrl Pts',(-14.5860912781424,-12.8450096600115,
118.029650693302)) ;
#187190 = CARTESIAN_POINT('Ctrl Pts',(-14.5180421746605,-12.6209217910559,
117.857738555032)) ;
#187191 = CARTESIAN_POINT('Ctrl Pts',(-14.5018364773262,-12.6762550632743,
117.808378615293)) ;
#187192 = CARTESIAN_POINT('Ctrl Pts',(-14.4280326288564,-12.6762550473825,
117.832609641598)) ;
#187193 = CARTESIAN_POINT('Ctrl Pts',(-14.3542287803866,-12.6762550314906,
117.856840667903)) ;
#187194 = CARTESIAN_POINT('Ctrl Pts',(-14.370434477721,-12.6209217592723,
117.906200607642)) ;
#187195 = CARTESIAN_POINT('Ctrl Pts',(-14.3866401750554,-12.5655884870539,
117.955560547382)) ;
#187196 = CARTESIAN_POINT('Ctrl Pts',(-14.4604440235251,-12.5655885029457,
117.931329521077)) ;
#187197 = CARTESIAN_POINT('Ctrl Pts',(-14.5342478719949,-12.5655885188375,
117.907098494772)) ;
#187198 = CARTESIAN_POINT('Ctrl Pts',(-14.5180421746605,-12.6209217910559,
117.857738555032)) ;
#187199 = CARTESIAN_POINT('Ctrl Pts',(-14.4333682313744,-12.453038777336,
117.635286933608)) ;
#187200 = CARTESIAN_POINT('Ctrl Pts',(-14.4223175253448,-12.520173907181,
117.601628265473)) ;
#187201 = CARTESIAN_POINT('Ctrl Pts',(-14.3485136735579,-12.5201738923226,
117.625859281675)) ;
#187202 = CARTESIAN_POINT('Ctrl Pts',(-14.2747098217711,-12.5201738774643,
117.650090297877)) ;
#187203 = CARTESIAN_POINT('Ctrl Pts',(-14.2857605278008,-12.4530387476193,
117.683748966012)) ;
#187204 = CARTESIAN_POINT('Ctrl Pts',(-14.2968112338305,-12.3859036177743,
117.717407634146)) ;
#187205 = CARTESIAN_POINT('Ctrl Pts',(-14.3706150856173,-12.3859036326327,
117.693176617944)) ;
#187206 = CARTESIAN_POINT('Ctrl Pts',(-14.4444189374041,-12.385903647491,
117.668945601743)) ;
#187207 = CARTESIAN_POINT('Ctrl Pts',(-14.4333682313744,-12.453038777336,
117.635286933608)) ;
#187208 = CARTESIAN_POINT('Ctrl Pts',(-14.337341154014,-12.3543368017594,
117.378290551669)) ;
#187209 = CARTESIAN_POINT('Ctrl Pts',(-14.3322448096572,-12.4284604690025,
117.362767908288)) ;
#187210 = CARTESIAN_POINT('Ctrl Pts',(-14.2584409542665,-12.4284604600379,
117.386998913513)) ;
#187211 = CARTESIAN_POINT('Ctrl Pts',(-14.1846370988758,-12.4284604510733,
117.411229918738)) ;
#187212 = CARTESIAN_POINT('Ctrl Pts',(-14.1897334432325,-12.3543367838302,
117.426752562119)) ;
#187213 = CARTESIAN_POINT('Ctrl Pts',(-14.1948297875893,-12.2802131165871,
117.4422752055)) ;
#187214 = CARTESIAN_POINT('Ctrl Pts',(-14.26863364298,-12.2802131255517,117.418044200275)) ;
#187215 = CARTESIAN_POINT('Ctrl Pts',(-14.3424374983707,-12.2802131345163,
117.39381319505)) ;
#187216 = CARTESIAN_POINT('Ctrl Pts',(-14.337341154014,-12.3543368017594,
117.378290551669)) ;
#187217 = CARTESIAN_POINT('Ctrl Pts',(-14.2364443666952,-12.3316786589988,
117.10637745565)) ;
#187218 = CARTESIAN_POINT('Ctrl Pts',(-14.2376526605417,-12.4074912166658,
117.11005772283)) ;
#187219 = CARTESIAN_POINT('Ctrl Pts',(-14.1638488023011,-12.4074912185027,
117.134288719375)) ;
#187220 = CARTESIAN_POINT('Ctrl Pts',(-14.0900449440605,-12.4074912203397,
117.15851971592)) ;
#187221 = CARTESIAN_POINT('Ctrl Pts',(-14.0888366502139,-12.3316786626727,
117.15483944874)) ;
#187222 = CARTESIAN_POINT('Ctrl Pts',(-14.0876283563674,-12.2558661050058,
117.15115918156)) ;
#187223 = CARTESIAN_POINT('Ctrl Pts',(-14.161432214608,-12.2558661031688,
117.126928185015)) ;
#187224 = CARTESIAN_POINT('Ctrl Pts',(-14.2352360728486,-12.2558661013318,
117.10269718847)) ;
#187225 = CARTESIAN_POINT('Ctrl Pts',(-14.2364443666952,-12.3316786589988,
117.10637745565)) ;
#187226 = CARTESIAN_POINT('Ctrl Pts',(-14.1362341376129,-12.3873927929882,
116.836808898935)) ;
#187227 = CARTESIAN_POINT('Ctrl Pts',(-14.1437029646929,-12.4594256106333,
116.859557740007)) ;
#187228 = CARTESIAN_POINT('Ctrl Pts',(-14.0698991040459,-12.4594256285176,
116.883788729222)) ;
#187229 = CARTESIAN_POINT('Ctrl Pts',(-13.9960952433988,-12.4594256464019,
116.908019718436)) ;
#187230 = CARTESIAN_POINT('Ctrl Pts',(-13.9886264163189,-12.3873928287568,
116.885270877365)) ;
#187231 = CARTESIAN_POINT('Ctrl Pts',(-13.9811575892389,-12.3153600111117,
116.862522036293)) ;
#187232 = CARTESIAN_POINT('Ctrl Pts',(-14.0549614498859,-12.3153599932274,
116.838291047078)) ;
#187233 = CARTESIAN_POINT('Ctrl Pts',(-14.128765310533,-12.3153599753431,
116.814060057863)) ;
#187234 = CARTESIAN_POINT('Ctrl Pts',(-14.1362341376129,-12.3873927929882,
116.836808898935)) ;
#187235 = CARTESIAN_POINT('Ctrl Pts',(-14.0446632556128,-12.5162741275779,
116.593235944571)) ;
#187236 = CARTESIAN_POINT('Ctrl Pts',(-14.0578049538713,-12.5794124829248,
116.633263435799)) ;
#187237 = CARTESIAN_POINT('Ctrl Pts',(-13.9840010934612,-12.5794125189228,
116.657494425736)) ;
#187238 = CARTESIAN_POINT('Ctrl Pts',(-13.9101972330512,-12.5794125549208,
116.681725415673)) ;
#187239 = CARTESIAN_POINT('Ctrl Pts',(-13.8970555347928,-12.5162741995739,
116.641697924445)) ;
#187240 = CARTESIAN_POINT('Ctrl Pts',(-13.8839138365343,-12.453135844227,
116.601670433216)) ;
#187241 = CARTESIAN_POINT('Ctrl Pts',(-13.9577176969443,-12.453135808229,
116.57743944328)) ;
#187242 = CARTESIAN_POINT('Ctrl Pts',(-14.0315215573543,-12.453135772231,
116.553208453343)) ;
#187243 = CARTESIAN_POINT('Ctrl Pts',(-14.0446632556128,-12.5162741275779,
116.593235944571)) ;
#187244 = CARTESIAN_POINT('Ctrl Pts',(-13.9661822867413,-12.7104566542012,
116.389740888653)) ;
#187245 = CARTESIAN_POINT('Ctrl Pts',(-13.9840868963541,-12.7601293026598,
116.444275439204)) ;
#187246 = CARTESIAN_POINT('Ctrl Pts',(-13.9102830377639,-12.7601293584612,
116.468506434684)) ;
#187247 = CARTESIAN_POINT('Ctrl Pts',(-13.8364791791737,-12.7601294142626,
116.492737430164)) ;
#187248 = CARTESIAN_POINT('Ctrl Pts',(-13.8185745695609,-12.7104567658041,
116.438202879613)) ;
#187249 = CARTESIAN_POINT('Ctrl Pts',(-13.8006699599481,-12.6607841173455,
116.383668329061)) ;
#187250 = CARTESIAN_POINT('Ctrl Pts',(-13.8744738185383,-12.6607840615441,
116.359437333582)) ;
#187251 = CARTESIAN_POINT('Ctrl Pts',(-13.9482776771285,-12.6607840057427,
116.335206338102)) ;
#187252 = CARTESIAN_POINT('Ctrl Pts',(-13.9661822867413,-12.7104566542012,
116.389740888653)) ;
#187253 = CARTESIAN_POINT('Ctrl Pts',(-13.9065147105429,-12.9544063196606,
116.243378133493)) ;
#187254 = CARTESIAN_POINT('Ctrl Pts',(-13.9278790755324,-12.9871189134417,
116.308450540564)) ;
#187255 = CARTESIAN_POINT('Ctrl Pts',(-13.8540752212451,-12.9871189862544,
116.332681549149)) ;
#187256 = CARTESIAN_POINT('Ctrl Pts',(-13.7802713669579,-12.987119059067,
116.356912557735)) ;
#187257 = CARTESIAN_POINT('Ctrl Pts',(-13.7589070019684,-12.9544064652859,
116.291840150665)) ;
#187258 = CARTESIAN_POINT('Ctrl Pts',(-13.737542636979,-12.9216938715048,
116.226767743595)) ;
#187259 = CARTESIAN_POINT('Ctrl Pts',(-13.8113464912662,-12.9216937986921,
116.202536735009)) ;
#187260 = CARTESIAN_POINT('Ctrl Pts',(-13.8851503455534,-12.9216937258795,
116.178305726423)) ;
#187261 = CARTESIAN_POINT('Ctrl Pts',(-13.9065147105429,-12.9544063196606,
116.243378133493)) ;
#187262 = CARTESIAN_POINT('Ctrl Pts',(-13.8686602732645,-13.2316631461472,
116.163500825195)) ;
#187263 = CARTESIAN_POINT('Ctrl Pts',(-13.8919655852634,-13.2450660236381,
116.23448504356)) ;
#187264 = CARTESIAN_POINT('Ctrl Pts',(-13.8181617370342,-13.2450661094682,
116.258716070597)) ;
#187265 = CARTESIAN_POINT('Ctrl Pts',(-13.744357888805,-13.2450661952983,
116.282947097635)) ;
#187266 = CARTESIAN_POINT('Ctrl Pts',(-13.7210525768062,-13.2316633178074,
116.21196287927)) ;
#187267 = CARTESIAN_POINT('Ctrl Pts',(-13.6977472648073,-13.2182604403165,
116.140978660905)) ;
#187268 = CARTESIAN_POINT('Ctrl Pts',(-13.7715511130365,-13.2182603544864,
116.116747633868)) ;
#187269 = CARTESIAN_POINT('Ctrl Pts',(-13.8453549612656,-13.2182602686563,
116.09251660683)) ;
#187270 = CARTESIAN_POINT('Ctrl Pts',(-13.8686602732645,-13.2316631461472,
116.163500825195)) ;
#187271 = CARTESIAN_POINT('Ctrl Pts',(-13.854686359136,-13.5226486146427,
116.156402551173)) ;
#187272 = CARTESIAN_POINT('Ctrl Pts',(-13.8782674046233,-13.5157554602217,
116.228226609137)) ;
#187273 = CARTESIAN_POINT('Ctrl Pts',(-13.8044635638606,-13.5157555531286,
116.252457658916)) ;
#187274 = CARTESIAN_POINT('Ctrl Pts',(-13.7306597230979,-13.5157556460354,
116.276688708695)) ;
#187275 = CARTESIAN_POINT('Ctrl Pts',(-13.7070786776106,-13.5226488004565,
116.204864650732)) ;
#187276 = CARTESIAN_POINT('Ctrl Pts',(-13.6834976321233,-13.5295419548775,
116.133040592768)) ;
#187277 = CARTESIAN_POINT('Ctrl Pts',(-13.757301472886,-13.5295418619706,
116.108809542988)) ;
#187278 = CARTESIAN_POINT('Ctrl Pts',(-13.8311053136488,-13.5295417690637,
116.084578493209)) ;
#187279 = CARTESIAN_POINT('Ctrl Pts',(-13.854686359136,-13.5226486146427,
116.156402551173)) ;
#187280 = CARTESIAN_POINT('Ctrl Pts',(-13.8649983319088,-13.8069296281822,
116.223380345266)) ;
#187281 = CARTESIAN_POINT('Ctrl Pts',(-13.887157991961,-13.7801790343967,
116.290875092425)) ;
#187282 = CARTESIAN_POINT('Ctrl Pts',(-13.8133541594712,-13.7801791269532,
116.315106167402)) ;
#187283 = CARTESIAN_POINT('Ctrl Pts',(-13.7395503269813,-13.7801792195097,
116.339337242379)) ;
#187284 = CARTESIAN_POINT('Ctrl Pts',(-13.717390666929,-13.8069298132952,
116.27184249522)) ;
#187285 = CARTESIAN_POINT('Ctrl Pts',(-13.6952310068767,-13.8336804070807,
116.204347748061)) ;
#187286 = CARTESIAN_POINT('Ctrl Pts',(-13.7690348393666,-13.8336803145242,
116.180116673084)) ;
#187287 = CARTESIAN_POINT('Ctrl Pts',(-13.8428386718565,-13.8336802219677,
116.155885598107)) ;
#187288 = CARTESIAN_POINT('Ctrl Pts',(-13.8649983319088,-13.8069296281822,
116.223380345266)) ;
#187289 = CARTESIAN_POINT('Ctrl Pts',(-13.8980327908744,-14.0625497260425,
116.35946810785)) ;
#187290 = CARTESIAN_POINT('Ctrl Pts',(-13.917184644522,-14.0179135569207,
116.41780156193)) ;
#187291 = CARTESIAN_POINT('Ctrl Pts',(-13.8433808200787,-14.017913640046,
116.442032661416)) ;
#187292 = CARTESIAN_POINT('Ctrl Pts',(-13.7695769956354,-14.0179137231712,
116.466263760901)) ;
#187293 = CARTESIAN_POINT('Ctrl Pts',(-13.7504251419878,-14.062549892293,
116.407930306821)) ;
#187294 = CARTESIAN_POINT('Ctrl Pts',(-13.7312732883402,-14.1071860614148,
116.349596852741)) ;
#187295 = CARTESIAN_POINT('Ctrl Pts',(-13.8050771127835,-14.1071859782896,
116.325365753256)) ;
#187296 = CARTESIAN_POINT('Ctrl Pts',(-13.8788809372268,-14.1071858951643,
116.30113465377)) ;
#187297 = CARTESIAN_POINT('Ctrl Pts',(-13.8980327908744,-14.0625497260425,
116.35946810785)) ;
#187298 = CARTESIAN_POINT('Ctrl Pts',(-13.9507026046682,-14.2720262448878,
116.555387635034)) ;
#187299 = CARTESIAN_POINT('Ctrl Pts',(-13.9654709590495,-14.2126996245835,
116.600369657567)) ;
#187300 = CARTESIAN_POINT('Ctrl Pts',(-13.8916671415546,-14.2126996903488,
116.624600778216)) ;
#187301 = CARTESIAN_POINT('Ctrl Pts',(-13.8178633240598,-14.2126997561141,
116.648831898866)) ;
#187302 = CARTESIAN_POINT('Ctrl Pts',(-13.8030949696785,-14.2720263764183,
116.603849876333)) ;
#187303 = CARTESIAN_POINT('Ctrl Pts',(-13.7883266152972,-14.3313529967226,
116.558867853801)) ;
#187304 = CARTESIAN_POINT('Ctrl Pts',(-13.8621304327921,-14.3313529309573,
116.534636733152)) ;
#187305 = CARTESIAN_POINT('Ctrl Pts',(-13.9359342502869,-14.331352865192,
116.510405612502)) ;
#187306 = CARTESIAN_POINT('Ctrl Pts',(-13.9507026046682,-14.2720262448878,
116.555387635034)) ;
#187307 = CARTESIAN_POINT('Ctrl Pts',(-14.0181419135474,-14.4199161330371,
116.796147687548)) ;
#187308 = CARTESIAN_POINT('Ctrl Pts',(-14.027492125809,-14.3501772641186,
116.824626923365)) ;
#187309 = CARTESIAN_POINT('Ctrl Pts',(-13.9536883133137,-14.3501773061419,
116.848858059242)) ;
#187310 = CARTESIAN_POINT('Ctrl Pts',(-13.8798845008185,-14.3501773481651,
116.87308919512)) ;
#187311 = CARTESIAN_POINT('Ctrl Pts',(-13.8705342885569,-14.4199162170836,
116.844609959303)) ;
#187312 = CARTESIAN_POINT('Ctrl Pts',(-13.8611840762953,-14.489655086002,
116.816130723485)) ;
#187313 = CARTESIAN_POINT('Ctrl Pts',(-13.9349878887906,-14.4896550439788,
116.791899587608)) ;
#187314 = CARTESIAN_POINT('Ctrl Pts',(-14.0087917012858,-14.4896550019555,
116.767668451731)) ;
#187315 = CARTESIAN_POINT('Ctrl Pts',(-14.0181419135474,-14.4199161330371,
116.796147687548)) ;
#187316 = CARTESIAN_POINT('Ctrl Pts',(-14.0955313329315,-14.496610258064,
117.067451422001)) ;
#187317 = CARTESIAN_POINT('Ctrl Pts',(-14.098756043099,-14.4214134928077,
117.077273366771)) ;
#187318 = CARTESIAN_POINT('Ctrl Pts',(-14.0249522332246,-14.4214135069691,
117.101504510631)) ;
#187319 = CARTESIAN_POINT('Ctrl Pts',(-13.9511484233502,-14.4214135211306,
117.125735654491)) ;
#187320 = CARTESIAN_POINT('Ctrl Pts',(-13.9479237131826,-14.496610286387,
117.115913709721)) ;
#187321 = CARTESIAN_POINT('Ctrl Pts',(-13.9446990030151,-14.5718070516433,
117.106091764952)) ;
#187322 = CARTESIAN_POINT('Ctrl Pts',(-14.0185028128895,-14.5718070374819,
117.081860621092)) ;
#187323 = CARTESIAN_POINT('Ctrl Pts',(-14.0923066227639,-14.5718070233204,
117.057629477232)) ;
#187324 = CARTESIAN_POINT('Ctrl Pts',(-14.0955313329315,-14.496610258064,
117.067451422001)) ;
#187325 = CARTESIAN_POINT('Ctrl Pts',(-14.1754259823427,-14.4958941579837,
117.3460706369)) ;
#187326 = CARTESIAN_POINT('Ctrl Pts',(-14.1723475785296,-14.4206364931476,
117.336694313495)) ;
#187327 = CARTESIAN_POINT('Ctrl Pts',(-14.0985437685299,-14.4206364783751,
117.360925456973)) ;
#187328 = CARTESIAN_POINT('Ctrl Pts',(-14.0247399585301,-14.4206364636026,
117.385156600451)) ;
#187329 = CARTESIAN_POINT('Ctrl Pts',(-14.0278183623432,-14.4958941284387,
117.394532923857)) ;
#187330 = CARTESIAN_POINT('Ctrl Pts',(-14.0308967661563,-14.5711517932748,
117.403909247263)) ;
#187331 = CARTESIAN_POINT('Ctrl Pts',(-14.104700576156,-14.5711518080473,
117.379678103784)) ;
#187332 = CARTESIAN_POINT('Ctrl Pts',(-14.1785043861558,-14.5711518228198,
117.355446960306)) ;
#187333 = CARTESIAN_POINT('Ctrl Pts',(-14.1754259823427,-14.4958941579837,
117.3460706369)) ;
#187334 = CARTESIAN_POINT('Ctrl Pts',(-14.2526586700799,-14.4180076226564,
117.616872676187)) ;
#187335 = CARTESIAN_POINT('Ctrl Pts',(-14.2434477347778,-14.3480754910907,
117.588817651376)) ;
#187336 = CARTESIAN_POINT('Ctrl Pts',(-14.1696439218951,-14.3480754488814,
117.613048786073)) ;
#187337 = CARTESIAN_POINT('Ctrl Pts',(-14.0958401090124,-14.3480754066721,
117.63727992077)) ;
#187338 = CARTESIAN_POINT('Ctrl Pts',(-14.1050510443145,-14.4180075382377,
117.665334945581)) ;
#187339 = CARTESIAN_POINT('Ctrl Pts',(-14.1142619796166,-14.4879396698034,
117.693389970392)) ;
#187340 = CARTESIAN_POINT('Ctrl Pts',(-14.1880657924993,-14.4879397120127,
117.669158835695)) ;
#187341 = CARTESIAN_POINT('Ctrl Pts',(-14.261869605382,-14.4879397542221,
117.644927700998)) ;
#187342 = CARTESIAN_POINT('Ctrl Pts',(-14.2526586700799,-14.4180076226564,
117.616872676187)) ;
#187343 = CARTESIAN_POINT('Ctrl Pts',(-14.3200614063859,-14.2684543242656,
117.857623246459)) ;
#187344 = CARTESIAN_POINT('Ctrl Pts',(-14.3053972971681,-14.2088592298977,
117.812958733819)) ;
#187345 = CARTESIAN_POINT('Ctrl Pts',(-14.2315934790337,-14.2088591648377,
117.83718985252)) ;
#187346 = CARTESIAN_POINT('Ctrl Pts',(-14.1577896608992,-14.2088590997777,
117.861420971222)) ;
#187347 = CARTESIAN_POINT('Ctrl Pts',(-14.172453770117,-14.2684541941456,
117.906085483862)) ;
#187348 = CARTESIAN_POINT('Ctrl Pts',(-14.1871178793347,-14.3280492885136,
117.950749996502)) ;
#187349 = CARTESIAN_POINT('Ctrl Pts',(-14.2609216974692,-14.3280493535736,
117.926518877801)) ;
#187350 = CARTESIAN_POINT('Ctrl Pts',(-14.3347255156036,-14.3280494186336,
117.902287759099)) ;
#187351 = CARTESIAN_POINT('Ctrl Pts',(-14.3200614063859,-14.2684543242656,
117.857623246459)) ;
#187352 = CARTESIAN_POINT('Ctrl Pts',(-14.3723441508749,-14.0580103363769,
118.052339972716)) ;
#187353 = CARTESIAN_POINT('Ctrl Pts',(-14.3532738878019,-14.0130186488343,
117.994255026436)) ;
#187354 = CARTESIAN_POINT('Ctrl Pts',(-14.2794700626734,-14.0130185675702,
118.018486123834)) ;
#187355 = CARTESIAN_POINT('Ctrl Pts',(-14.2056662375449,-14.013018486306,
118.042717221233)) ;
#187356 = CARTESIAN_POINT('Ctrl Pts',(-14.2247365006178,-14.0580101738486,
118.100802167514)) ;
#187357 = CARTESIAN_POINT('Ctrl Pts',(-14.2438067636907,-14.1030018613912,
118.158887113794)) ;
#187358 = CARTESIAN_POINT('Ctrl Pts',(-14.3176105888193,-14.1030019426553,
118.134656016396)) ;
#187359 = CARTESIAN_POINT('Ctrl Pts',(-14.3914144139478,-14.1030020239195,
118.110424918997)) ;
#187360 = CARTESIAN_POINT('Ctrl Pts',(-14.3723441508749,-14.0580103363769,
118.052339972716)) ;
#187361 = CARTESIAN_POINT('Ctrl Pts',(-14.4049559952129,-13.8017355758307,
118.187134007754)) ;
#187362 = CARTESIAN_POINT('Ctrl Pts',(-14.3828464247468,-13.7745688567898,
118.119791821635)) ;
#187363 = CARTESIAN_POINT('Ctrl Pts',(-14.3090425916919,-13.7745687672832,
118.144022894892)) ;
#187364 = CARTESIAN_POINT('Ctrl Pts',(-14.2352387586371,-13.7745686777767,
118.168253968148)) ;
#187365 = CARTESIAN_POINT('Ctrl Pts',(-14.2573483291032,-13.8017353968177,
118.235596154267)) ;
#187366 = CARTESIAN_POINT('Ctrl Pts',(-14.2794578995694,-13.8289021158586,
118.302938340385)) ;
#187367 = CARTESIAN_POINT('Ctrl Pts',(-14.3532617326242,-13.8289022053652,
118.278707267129)) ;
#187368 = CARTESIAN_POINT('Ctrl Pts',(-14.4270655656791,-13.8289022948717,
118.254476193873)) ;
#187369 = CARTESIAN_POINT('Ctrl Pts',(-14.4049559952129,-13.8017355758307,
118.187134007754)) ;
#187370 = CARTESIAN_POINT('Ctrl Pts',(-14.4148166276004,-13.5177911289146,
118.252654045157)) ;
#187371 = CARTESIAN_POINT('Ctrl Pts',(-14.3912510399415,-13.5104079472705,
118.180877065709)) ;
#187372 = CARTESIAN_POINT('Ctrl Pts',(-14.3174471989152,-13.5104078579673,
118.205108114686)) ;
#187373 = CARTESIAN_POINT('Ctrl Pts',(-14.2436433578889,-13.5104077686641,
118.229339163662)) ;
#187374 = CARTESIAN_POINT('Ctrl Pts',(-14.2672089455478,-13.5177909503083,
118.30111614311)) ;
#187375 = CARTESIAN_POINT('Ctrl Pts',(-14.2907745332067,-13.5251741319524,
118.372893122558)) ;
#187376 = CARTESIAN_POINT('Ctrl Pts',(-14.364578374233,-13.5251742212556,
118.348662073581)) ;
#187377 = CARTESIAN_POINT('Ctrl Pts',(-14.4383822152593,-13.5251743105588,
118.324431024605)) ;
#187378 = CARTESIAN_POINT('Ctrl Pts',(-14.4148166276004,-13.5177911289146,
118.252654045157)) ;
#187379 = CARTESIAN_POINT('Ctrl Pts',(-14.4004650952962,-13.2272027816916,
118.244367863608)) ;
#187380 = CARTESIAN_POINT('Ctrl Pts',(-14.3771329630221,-13.2400970018567,
118.173301951716)) ;
#187381 = CARTESIAN_POINT('Ctrl Pts',(-14.3033291148763,-13.2400969198801,
118.197532979008)) ;
#187382 = CARTESIAN_POINT('Ctrl Pts',(-14.2295252667306,-13.2400968379035,
118.2217640063)) ;
#187383 = CARTESIAN_POINT('Ctrl Pts',(-14.2528573990047,-13.2272026177384,
118.292829918192)) ;
#187384 = CARTESIAN_POINT('Ctrl Pts',(-14.2761895312788,-13.2143083975732,
118.363895830085)) ;
#187385 = CARTESIAN_POINT('Ctrl Pts',(-14.3499933794246,-13.2143084795498,
118.339664802793)) ;
#187386 = CARTESIAN_POINT('Ctrl Pts',(-14.4237972275703,-13.2143085615265,
118.315433775501)) ;
#187387 = CARTESIAN_POINT('Ctrl Pts',(-14.4004650952962,-13.2272027816916,
118.244367863608)) ;
#187388 = CARTESIAN_POINT('Ctrl Pts',(-14.3623212862769,-12.9503466746931,
118.163591806745)) ;
#187389 = CARTESIAN_POINT('Ctrl Pts',(-14.3408845358734,-12.9825901613467,
118.098298922341)) ;
#187390 = CARTESIAN_POINT('Ctrl Pts',(-14.267080681969,-12.9825900924411,
118.122529932092)) ;
#187391 = CARTESIAN_POINT('Ctrl Pts',(-14.1932768280645,-12.9825900235354,
118.146760941844)) ;
#187392 = CARTESIAN_POINT('Ctrl Pts',(-14.214713578468,-12.9503465368818,
118.212053826248)) ;
#187393 = CARTESIAN_POINT('Ctrl Pts',(-14.2361503288715,-12.9181030502282,
118.277346710652)) ;
#187394 = CARTESIAN_POINT('Ctrl Pts',(-14.3099541827759,-12.9181031191338,
118.253115700901)) ;
#187395 = CARTESIAN_POINT('Ctrl Pts',(-14.3837580366804,-12.9181031880395,
118.228884691149)) ;
#187396 = CARTESIAN_POINT('Ctrl Pts',(-14.3623212862769,-12.9503466746931,
118.163591806745)) ;
#187397 = CARTESIAN_POINT('Ctrl Pts',(-14.3018636593907,-12.7057179827167,
118.015049850158)) ;
#187398 = CARTESIAN_POINT('Ctrl Pts',(-14.283878771003,-12.7550903667589,
117.960270780674)) ;
#187399 = CARTESIAN_POINT('Ctrl Pts',(-14.2100749136123,-12.7550903161595,
117.984501779807)) ;
#187400 = CARTESIAN_POINT('Ctrl Pts',(-14.1362710562215,-12.7550902655601,
118.00873277894)) ;
#187401 = CARTESIAN_POINT('Ctrl Pts',(-14.1542559446093,-12.7057178815179,
118.063511848424)) ;
#187402 = CARTESIAN_POINT('Ctrl Pts',(-14.172240832997,-12.6563454974757,
118.118290917909)) ;
#187403 = CARTESIAN_POINT('Ctrl Pts',(-14.2460446903878,-12.6563455480751,
118.094059918775)) ;
#187404 = CARTESIAN_POINT('Ctrl Pts',(-14.3198485477785,-12.6563455986745,
118.069828919642)) ;
#187405 = CARTESIAN_POINT('Ctrl Pts',(-14.3018636593907,-12.7057179827167,
118.015049850158)) ;
#187406 = CARTESIAN_POINT('Ctrl Pts',(-14.223542409614,-12.5137879422887,
117.811825999988)) ;
#187407 = CARTESIAN_POINT('Ctrl Pts',(-14.2102677240736,-12.5766355535095,
117.771393448525)) ;
#187408 = CARTESIAN_POINT('Ctrl Pts',(-14.1364638648589,-12.5766355204259,
117.795624442103)) ;
#187409 = CARTESIAN_POINT('Ctrl Pts',(-14.0626600056441,-12.5766354873422,
117.81985543568)) ;
#187410 = CARTESIAN_POINT('Ctrl Pts',(-14.0759346911844,-12.5137878761215,
117.860287987143)) ;
#187411 = CARTESIAN_POINT('Ctrl Pts',(-14.0892093767248,-12.4509402649008,
117.900720538606)) ;
#187412 = CARTESIAN_POINT('Ctrl Pts',(-14.1630132359396,-12.4509402979844,
117.876489545029)) ;
#187413 = CARTESIAN_POINT('Ctrl Pts',(-14.2368170951544,-12.450940331068,
117.852258551451)) ;
#187414 = CARTESIAN_POINT('Ctrl Pts',(-14.223542409614,-12.5137879422887,
117.811825999988)) ;
#187415 = CARTESIAN_POINT('Ctrl Pts',(-14.1314433751478,-12.3855428728414,
117.56678537301)) ;
#187416 = CARTESIAN_POINT('Ctrl Pts',(-14.1238448332789,-12.4574400165938,
117.543641439496)) ;
#187417 = CARTESIAN_POINT('Ctrl Pts',(-14.0500409744482,-12.4574400010847,
117.567872434243)) ;
#187418 = CARTESIAN_POINT('Ctrl Pts',(-13.9762371156176,-12.4574399855756,
117.592103428991)) ;
#187419 = CARTESIAN_POINT('Ctrl Pts',(-13.9838356574865,-12.3855428418231,
117.615247362505)) ;
#187420 = CARTESIAN_POINT('Ctrl Pts',(-13.9914341993555,-12.3136456980707,
117.638391296019)) ;
#187421 = CARTESIAN_POINT('Ctrl Pts',(-14.0652380581861,-12.3136457135799,
117.614160301271)) ;
#187422 = CARTESIAN_POINT('Ctrl Pts',(-14.1390419170168,-12.313645729089,
117.589929306524)) ;
#187423 = CARTESIAN_POINT('Ctrl Pts',(-14.1314433751478,-12.3855428728414,
117.56678537301)) ;
#187424 = CARTESIAN_POINT('Ctrl Pts',(-14.031461000016,-12.3315373856839,
117.297796004923)) ;
#187425 = CARTESIAN_POINT('Ctrl Pts',(-14.0300964367554,-12.4073146251765,
117.293639764585)) ;
#187426 = CARTESIAN_POINT('Ctrl Pts',(-13.9562925801431,-12.4073146237206,
117.317870766089)) ;
#187427 = CARTESIAN_POINT('Ctrl Pts',(-13.8824887235308,-12.4073146222647,
117.342101767593)) ;
#187428 = CARTESIAN_POINT('Ctrl Pts',(-13.8838532867914,-12.331537382772,
117.346258007932)) ;
#187429 = CARTESIAN_POINT('Ctrl Pts',(-13.885217850052,-12.2557601432794,
117.35041424827)) ;
#187430 = CARTESIAN_POINT('Ctrl Pts',(-13.9590217066643,-12.2557601447353,
117.326183246766)) ;
#187431 = CARTESIAN_POINT('Ctrl Pts',(-14.0328255632766,-12.2557601461912,
117.301952245262)) ;
#187432 = CARTESIAN_POINT('Ctrl Pts',(-14.031461000016,-12.3315373856839,
117.297796004923)) ;
#187433 = CARTESIAN_POINT('Ctrl Pts',(-13.930645096914,-12.3551820249381,
117.026108320911)) ;
#187434 = CARTESIAN_POINT('Ctrl Pts',(-13.9355855082574,-12.4294230563163,
117.041156016064)) ;
#187435 = CARTESIAN_POINT('Ctrl Pts',(-13.8617816544059,-12.4294230645316,
117.065387025977)) ;
#187436 = CARTESIAN_POINT('Ctrl Pts',(-13.7879778005545,-12.4294230727469,
117.08961803589)) ;
#187437 = CARTESIAN_POINT('Ctrl Pts',(-13.7830373892111,-12.3551820413687,
117.074570340737)) ;
#187438 = CARTESIAN_POINT('Ctrl Pts',(-13.7780969778677,-12.2809410099905,
117.059522645584)) ;
#187439 = CARTESIAN_POINT('Ctrl Pts',(-13.8519008317191,-12.2809410017752,
117.035291635671)) ;
#187440 = CARTESIAN_POINT('Ctrl Pts',(-13.9257046855706,-12.2809409935599,
117.011060625758)) ;
#187441 = CARTESIAN_POINT('Ctrl Pts',(-13.930645096914,-12.3551820249381,
117.026108320911)) ;
#187442 = CARTESIAN_POINT('Ctrl Pts',(-13.8342954331795,-12.4558831035982,
116.768314309388)) ;
#187443 = CARTESIAN_POINT('Ctrl Pts',(-13.8452327466786,-12.5232058909048,
116.801627601108)) ;
#187444 = CARTESIAN_POINT('Ctrl Pts',(-13.7714288966798,-12.52320590289,116.825858622756)) ;
#187445 = CARTESIAN_POINT('Ctrl Pts',(-13.6976250466809,-12.5232059148753,
116.850089644404)) ;
#187446 = CARTESIAN_POINT('Ctrl Pts',(-13.6866877331818,-12.4558831275687,
116.816776352684)) ;
#187447 = CARTESIAN_POINT('Ctrl Pts',(-13.6757504196827,-12.3885603402622,
116.783463060963)) ;
#187448 = CARTESIAN_POINT('Ctrl Pts',(-13.7495542696815,-12.3885603282769,
116.759232039315)) ;
#187449 = CARTESIAN_POINT('Ctrl Pts',(-13.8233581196804,-12.3885603162917,
116.735001017668)) ;
#187450 = CARTESIAN_POINT('Ctrl Pts',(-13.8342954331795,-12.4558831035982,
116.768314309388)) ;
#187451 = CARTESIAN_POINT('Ctrl Pts',(-13.7502969996175,-12.6240117159259,
116.547732522456)) ;
#187452 = CARTESIAN_POINT('Ctrl Pts',(-13.7663861121361,-12.6796964809936,
116.596737362866)) ;
#187453 = CARTESIAN_POINT('Ctrl Pts',(-13.6925822646977,-12.6796964939069,
116.620968392312)) ;
#187454 = CARTESIAN_POINT('Ctrl Pts',(-13.6187784172594,-12.6796965068202,
116.645199421759)) ;
#187455 = CARTESIAN_POINT('Ctrl Pts',(-13.6026893047407,-12.6240117417526,
116.596194581349)) ;
#187456 = CARTESIAN_POINT('Ctrl Pts',(-13.5866001922221,-12.568326976685,
116.547189740939)) ;
#187457 = CARTESIAN_POINT('Ctrl Pts',(-13.6604040396604,-12.5683269637716,
116.522958711493)) ;
#187458 = CARTESIAN_POINT('Ctrl Pts',(-13.7342078870988,-12.5683269508583,
116.498727682046)) ;
#187459 = CARTESIAN_POINT('Ctrl Pts',(-13.7502969996175,-12.6240117159259,
116.547732522456)) ;
#187460 = CARTESIAN_POINT('Ctrl Pts',(-13.6822000856196,-12.8504012275685,
116.375896123701)) ;
#187461 = CARTESIAN_POINT('Ctrl Pts',(-13.7023322685498,-12.8903625364955,
116.43721550439)) ;
#187462 = CARTESIAN_POINT('Ctrl Pts',(-13.6285284236176,-12.8903625457094,
116.46144654147)) ;
#187463 = CARTESIAN_POINT('Ctrl Pts',(-13.5547245786854,-12.8903625549234,
116.48567757855)) ;
#187464 = CARTESIAN_POINT('Ctrl Pts',(-13.5345923957552,-12.8504012459964,
116.424358197861)) ;
#187465 = CARTESIAN_POINT('Ctrl Pts',(-13.5144602128251,-12.8104399370694,
116.363038817172)) ;
#187466 = CARTESIAN_POINT('Ctrl Pts',(-13.5882640577573,-12.8104399278554,
116.338807780093)) ;
#187467 = CARTESIAN_POINT('Ctrl Pts',(-13.6620679026895,-12.8104399186415,
116.314576743013)) ;
#187468 = CARTESIAN_POINT('Ctrl Pts',(-13.6822000856196,-12.8504012275685,
116.375896123701)) ;
#187469 = CARTESIAN_POINT('Ctrl Pts',(-13.6351866805831,-13.116472804272,
116.268099937279)) ;
#187470 = CARTESIAN_POINT('Ctrl Pts',(-13.6578993214573,-13.1379154690077,
116.337278976615)) ;
#187471 = CARTESIAN_POINT('Ctrl Pts',(-13.5840954777456,-13.1379154738939,
116.361510017412)) ;
#187472 = CARTESIAN_POINT('Ctrl Pts',(-13.5102916340338,-13.13791547878,116.385741058209)) ;
#187473 = CARTESIAN_POINT('Ctrl Pts',(-13.4875789931596,-13.1164728140443,
116.316562018874)) ;
#187474 = CARTESIAN_POINT('Ctrl Pts',(-13.4648663522853,-13.0950301493086,
116.247382979538)) ;
#187475 = CARTESIAN_POINT('Ctrl Pts',(-13.5386701959971,-13.0950301444224,
116.223151938741)) ;
#187476 = CARTESIAN_POINT('Ctrl Pts',(-13.6124740397088,-13.0950301395363,
116.198920897944)) ;
#187477 = CARTESIAN_POINT('Ctrl Pts',(-13.6351866805831,-13.116472804272,
116.268099937279)) ;
#187478 = CARTESIAN_POINT('Ctrl Pts',(-13.6114099106661,-13.4044926459014,
116.231144735483)) ;
#187479 = CARTESIAN_POINT('Ctrl Pts',(-13.635082944032,-13.4058558527326,
116.303248975477)) ;
#187480 = CARTESIAN_POINT('Ctrl Pts',(-13.5612791007297,-13.4058558531923,
116.327480017521)) ;
#187481 = CARTESIAN_POINT('Ctrl Pts',(-13.4874752574274,-13.405855853652,
116.351711059566)) ;
#187482 = CARTESIAN_POINT('Ctrl Pts',(-13.4638022240615,-13.4044926468209,
116.279606819572)) ;
#187483 = CARTESIAN_POINT('Ctrl Pts',(-13.4401291906957,-13.4031294399897,
116.207502579578)) ;
#187484 = CARTESIAN_POINT('Ctrl Pts',(-13.513933033998,-13.40312943953,116.183271537533)) ;
#187485 = CARTESIAN_POINT('Ctrl Pts',(-13.5877368773003,-13.4031294390702,
116.159040495489)) ;
#187486 = CARTESIAN_POINT('Ctrl Pts',(-13.6114099106661,-13.4044926459014,
116.231144735483)) ;
#187487 = CARTESIAN_POINT('Ctrl Pts',(-13.6118756694188,-13.6930971947521,
116.26796761554)) ;
#187488 = CARTESIAN_POINT('Ctrl Pts',(-13.6348188255478,-13.6743099521877,
116.337848767292)) ;
#187489 = CARTESIAN_POINT('Ctrl Pts',(-13.5610149819962,-13.6743099497306,
116.362079808577)) ;
#187490 = CARTESIAN_POINT('Ctrl Pts',(-13.4872111384447,-13.6743099472734,
116.386310849862)) ;
#187491 = CARTESIAN_POINT('Ctrl Pts',(-13.4642679823157,-13.6930971898379,
116.31642969811)) ;
#187492 = CARTESIAN_POINT('Ctrl Pts',(-13.4413248261868,-13.7118844324023,
116.246548546358)) ;
#187493 = CARTESIAN_POINT('Ctrl Pts',(-13.5151286697383,-13.7118844348594,
116.222317505073)) ;
#187494 = CARTESIAN_POINT('Ctrl Pts',(-13.5889325132899,-13.7118844373166,
116.198086463788)) ;
#187495 = CARTESIAN_POINT('Ctrl Pts',(-13.6118756694188,-13.6930971947521,
116.26796761554)) ;
#187496 = CARTESIAN_POINT('Ctrl Pts',(-13.63611364525,-13.9640294815732,116.37748207908)) ;
#187497 = CARTESIAN_POINT('Ctrl Pts',(-13.6566598449573,-13.9262943650166,
116.440062488337)) ;
#187498 = CARTESIAN_POINT('Ctrl Pts',(-13.5828560010043,-13.9262943620916,
116.464293528399)) ;
#187499 = CARTESIAN_POINT('Ctrl Pts',(-13.5090521570513,-13.9262943591665,
116.488524568462)) ;
#187500 = CARTESIAN_POINT('Ctrl Pts',(-13.4885059573441,-13.9640294757231,
116.425944159205)) ;
#187501 = CARTESIAN_POINT('Ctrl Pts',(-13.4679597576368,-14.0017645922797,
116.363363749948)) ;
#187502 = CARTESIAN_POINT('Ctrl Pts',(-13.5417636015898,-14.0017645952047,
116.339132709885)) ;
#187503 = CARTESIAN_POINT('Ctrl Pts',(-13.6155674455427,-14.0017645981297,
116.314901669823)) ;
#187504 = CARTESIAN_POINT('Ctrl Pts',(-13.63611364525,-13.9640294815732,116.37748207908)) ;
#187505 = CARTESIAN_POINT('Ctrl Pts',(-13.6811255061301,-14.1931760928296,
116.549907692602)) ;
#187506 = CARTESIAN_POINT('Ctrl Pts',(-13.6978277312129,-14.1393849019779,
116.600779975346)) ;
#187507 = CARTESIAN_POINT('Ctrl Pts',(-13.6240238873508,-14.1393849008332,
116.625011015685)) ;
#187508 = CARTESIAN_POINT('Ctrl Pts',(-13.5502200434887,-14.1393848996885,
116.649242056024)) ;
#187509 = CARTESIAN_POINT('Ctrl Pts',(-13.533517818406,-14.1931760905402,
116.598369773281)) ;
#187510 = CARTESIAN_POINT('Ctrl Pts',(-13.5168155933232,-14.2469672813919,
116.547497490537)) ;
#187511 = CARTESIAN_POINT('Ctrl Pts',(-13.5906194371853,-14.2469672825366,
116.523266450198)) ;
#187512 = CARTESIAN_POINT('Ctrl Pts',(-13.6644232810473,-14.2469672836813,
116.499035409859)) ;
#187513 = CARTESIAN_POINT('Ctrl Pts',(-13.6811255061301,-14.1931760928296,
116.549907692602)) ;
#187514 = CARTESIAN_POINT('Ctrl Pts',(-13.7431234444794,-14.3676938142289,
116.774142291284)) ;
#187515 = CARTESIAN_POINT('Ctrl Pts',(-13.7547884992663,-14.3016378950291,
116.809672165995)) ;
#187516 = CARTESIAN_POINT('Ctrl Pts',(-13.6809846560937,-14.3016378958559,
116.833903208434)) ;
#187517 = CARTESIAN_POINT('Ctrl Pts',(-13.6071808129211,-14.3016378966827,
116.858134250874)) ;
#187518 = CARTESIAN_POINT('Ctrl Pts',(-13.5955157581342,-14.3676938158825,
116.822604376163)) ;
#187519 = CARTESIAN_POINT('Ctrl Pts',(-13.5838507033473,-14.4337497350823,
116.787074501452)) ;
#187520 = CARTESIAN_POINT('Ctrl Pts',(-13.6576545465199,-14.4337497342555,
116.762843459013)) ;
#187521 = CARTESIAN_POINT('Ctrl Pts',(-13.7314583896924,-14.4337497334287,
116.738612416573)) ;
#187522 = CARTESIAN_POINT('Ctrl Pts',(-13.7431234444794,-14.3676938142289,
116.774142291284)) ;
#187523 = CARTESIAN_POINT('Ctrl Pts',(-13.8171763031359,-14.4745465378171,
117.0351873098)) ;
#187524 = CARTESIAN_POINT('Ctrl Pts',(-13.8229531340849,-14.4009329542059,
117.052782604666)) ;
#187525 = CARTESIAN_POINT('Ctrl Pts',(-13.7491492924703,-14.4009329561401,
117.077013651851)) ;
#187526 = CARTESIAN_POINT('Ctrl Pts',(-13.6753454508558,-14.4009329580743,
117.101244699035)) ;
#187527 = CARTESIAN_POINT('Ctrl Pts',(-13.6695686199067,-14.4745465416855,
117.08364940417)) ;
#187528 = CARTESIAN_POINT('Ctrl Pts',(-13.6637917889576,-14.5481601252968,
117.066054109305)) ;
#187529 = CARTESIAN_POINT('Ctrl Pts',(-13.7375956305722,-14.5481601233625,
117.04182306212)) ;
#187530 = CARTESIAN_POINT('Ctrl Pts',(-13.8113994721868,-14.5481601214283,
117.017592014935)) ;
#187531 = CARTESIAN_POINT('Ctrl Pts',(-13.8171763031359,-14.4745465378171,
117.0351873098)) ;
#187532 = CARTESIAN_POINT('Ctrl Pts',(-13.8970345888385,-14.5056303399819,
117.313909070973)) ;
#187533 = CARTESIAN_POINT('Ctrl Pts',(-13.8965094386652,-14.4297391365026,
117.312309548038)) ;
#187534 = CARTESIAN_POINT('Ctrl Pts',(-13.8227055991251,-14.4297391368143,
117.336540601542)) ;
#187535 = CARTESIAN_POINT('Ctrl Pts',(-13.748901759585,-14.429739137126,117.360771655045)) ;
#187536 = CARTESIAN_POINT('Ctrl Pts',(-13.7494269097583,-14.5056303406052,
117.36237117798)) ;
#187537 = CARTESIAN_POINT('Ctrl Pts',(-13.7499520599316,-14.5815215440845,
117.363970700914)) ;
#187538 = CARTESIAN_POINT('Ctrl Pts',(-13.8237558994717,-14.5815215437728,
117.339739647411)) ;
#187539 = CARTESIAN_POINT('Ctrl Pts',(-13.8975597390118,-14.5815215434611,
117.315508593907)) ;
#187540 = CARTESIAN_POINT('Ctrl Pts',(-13.8970345888385,-14.5056303399819,
117.313909070973)) ;
#187541 = CARTESIAN_POINT('Ctrl Pts',(-13.9762710886277,-14.4584990503317,
117.590768049018)) ;
#187542 = CARTESIAN_POINT('Ctrl Pts',(-13.9694776476947,-14.3857884203973,
117.570076323666)) ;
#187543 = CARTESIAN_POINT('Ctrl Pts',(-13.8956738103242,-14.3857884151158,
117.594307383777)) ;
#187544 = CARTESIAN_POINT('Ctrl Pts',(-13.8218699729536,-14.3857884098344,
117.618538443888)) ;
#187545 = CARTESIAN_POINT('Ctrl Pts',(-13.8286634138866,-14.4584990397688,
117.639230169241)) ;
#187546 = CARTESIAN_POINT('Ctrl Pts',(-13.8354568548196,-14.5312096697032,
117.659921894593)) ;
#187547 = CARTESIAN_POINT('Ctrl Pts',(-13.9092606921902,-14.5312096749846,
117.635690834482)) ;
#187548 = CARTESIAN_POINT('Ctrl Pts',(-13.9830645295607,-14.5312096802661,
117.61145977437)) ;
#187549 = CARTESIAN_POINT('Ctrl Pts',(-13.9762710886277,-14.4584990503317,
117.590768049018)) ;
#187550 = CARTESIAN_POINT('Ctrl Pts',(-14.0480660570399,-14.3375927241235,
117.844776644025)) ;
#187551 = CARTESIAN_POINT('Ctrl Pts',(-14.0355188680038,-14.2732190066455,
117.806559930184)) ;
#187552 = CARTESIAN_POINT('Ctrl Pts',(-13.961715031784,-14.2732189929484,
117.830790993801)) ;
#187553 = CARTESIAN_POINT('Ctrl Pts',(-13.8879111955643,-14.2732189792513,
117.855022057418)) ;
#187554 = CARTESIAN_POINT('Ctrl Pts',(-13.9004583846004,-14.3375926967294,
117.893238771258)) ;
#187555 = CARTESIAN_POINT('Ctrl Pts',(-13.9130055736365,-14.4019664142074,
117.931455485098)) ;
#187556 = CARTESIAN_POINT('Ctrl Pts',(-13.9868094098562,-14.4019664279045,
117.907224421482)) ;
#187557 = CARTESIAN_POINT('Ctrl Pts',(-14.060613246076,-14.4019664416016,
117.882993357865)) ;
#187558 = CARTESIAN_POINT('Ctrl Pts',(-14.0480660570399,-14.3375927241235,
117.844776644025)) ;
#187559 = CARTESIAN_POINT('Ctrl Pts',(-14.1074172507216,-14.1494056626898,
118.061195966656)) ;
#187560 = CARTESIAN_POINT('Ctrl Pts',(-14.0899702434343,-14.0980778114582,
118.008055196809)) ;
#187561 = CARTESIAN_POINT('Ctrl Pts',(-14.0161664079691,-14.0980777847103,
118.032286262724)) ;
#187562 = CARTESIAN_POINT('Ctrl Pts',(-13.942362572504,-14.0980777579623,
118.056517328639)) ;
#187563 = CARTESIAN_POINT('Ctrl Pts',(-13.9598095797914,-14.1494056091939,
118.109658098486)) ;
#187564 = CARTESIAN_POINT('Ctrl Pts',(-13.9772565870787,-14.2007334604254,
118.162798868333)) ;
#187565 = CARTESIAN_POINT('Ctrl Pts',(-14.0510604225438,-14.2007334871734,
118.138567802417)) ;
#187566 = CARTESIAN_POINT('Ctrl Pts',(-14.1248642580089,-14.2007335139213,
118.114336736502)) ;
#187567 = CARTESIAN_POINT('Ctrl Pts',(-14.1074172507216,-14.1494056626898,
118.061195966656)) ;
#187568 = CARTESIAN_POINT('Ctrl Pts',(-14.1483544481985,-13.9095500364901,
118.221334237361)) ;
#187569 = CARTESIAN_POINT('Ctrl Pts',(-14.1272904544691,-13.8748947454948,
118.157176710245)) ;
#187570 = CARTESIAN_POINT('Ctrl Pts',(-14.0534866176551,-13.874894705204,
118.181407772051)) ;
#187571 = CARTESIAN_POINT('Ctrl Pts',(-13.9796827808411,-13.8748946649131,
118.205638833858)) ;
#187572 = CARTESIAN_POINT('Ctrl Pts',(-14.0007467745705,-13.9095499559084,
118.269796360974)) ;
#187573 = CARTESIAN_POINT('Ctrl Pts',(-14.0218107682998,-13.9442052469036,
118.33395388809)) ;
#187574 = CARTESIAN_POINT('Ctrl Pts',(-14.0956146051138,-13.9442052871945,
118.309722826283)) ;
#187575 = CARTESIAN_POINT('Ctrl Pts',(-14.1694184419278,-13.9442053274854,
118.285491764477)) ;
#187576 = CARTESIAN_POINT('Ctrl Pts',(-14.1483544481985,-13.9095500364901,
118.221334237361)) ;
#187577 = CARTESIAN_POINT('Ctrl Pts',(-14.1676613767387,-13.6354015229083,
118.315498195854)) ;
#187578 = CARTESIAN_POINT('Ctrl Pts',(-14.1444874123487,-13.6198370471349,
118.2449140384)) ;
#187579 = CARTESIAN_POINT('Ctrl Pts',(-14.0706835724671,-13.6198369951942,
118.269145090864)) ;
#187580 = CARTESIAN_POINT('Ctrl Pts',(-13.9968797325854,-13.6198369432535,
118.293376143327)) ;
#187581 = CARTESIAN_POINT('Ctrl Pts',(-14.0200536969754,-13.6354014190268,
118.36396030078)) ;
#187582 = CARTESIAN_POINT('Ctrl Pts',(-14.0432276613653,-13.6509658948002,
118.434544458234)) ;
#187583 = CARTESIAN_POINT('Ctrl Pts',(-14.117031501247,-13.6509659467409,
118.410313405771)) ;
#187584 = CARTESIAN_POINT('Ctrl Pts',(-14.1908353411286,-13.6509659986816,
118.386082353308)) ;
#187585 = CARTESIAN_POINT('Ctrl Pts',(-14.1676613767387,-13.6354015229083,
118.315498195854)) ;
#187586 = CARTESIAN_POINT('Ctrl Pts',(-14.1632252950628,-13.3449945339553,
118.337440153608)) ;
#187587 = CARTESIAN_POINT('Ctrl Pts',(-14.1395939545181,-13.3496833242157,
118.265462902021)) ;
#187588 = CARTESIAN_POINT('Ctrl Pts',(-14.0657901100262,-13.3496832627429,
118.289693940442)) ;
#187589 = CARTESIAN_POINT('Ctrl Pts',(-13.9919862655343,-13.3496832012701,
118.313924978863)) ;
#187590 = CARTESIAN_POINT('Ctrl Pts',(-14.015617606079,-13.3449944110097,
118.38590223045)) ;
#187591 = CARTESIAN_POINT('Ctrl Pts',(-14.0392489466237,-13.3403056207493,
118.457879482037)) ;
#187592 = CARTESIAN_POINT('Ctrl Pts',(-14.1130527911156,-13.3403056822221,
118.433648443616)) ;
#187593 = CARTESIAN_POINT('Ctrl Pts',(-14.1868566356075,-13.3403057436949,
118.409417405195)) ;
#187594 = CARTESIAN_POINT('Ctrl Pts',(-14.1632252950628,-13.3449945339553,
118.337440153608)) ;
#187595 = CARTESIAN_POINT('Ctrl Pts',(-14.1346590237781,-13.0600685836045,
118.285838693899)) ;
#187596 = CARTESIAN_POINT('Ctrl Pts',(-14.1122553485649,-13.0846570049903,
118.217600712678)) ;
#187597 = CARTESIAN_POINT('Ctrl Pts',(-14.0384514982716,-13.0846569392068,
118.241831733429)) ;
#187598 = CARTESIAN_POINT('Ctrl Pts',(-13.9646476479783,-13.0846568734233,
118.26606275418)) ;
#187599 = CARTESIAN_POINT('Ctrl Pts',(-13.9870513231916,-13.0600684520375,
118.3343007354)) ;
#187600 = CARTESIAN_POINT('Ctrl Pts',(-14.0094549984048,-13.0354800306517,
118.402538716621)) ;
#187601 = CARTESIAN_POINT('Ctrl Pts',(-14.0832588486981,-13.0354800964351,
118.37830769587)) ;
#187602 = CARTESIAN_POINT('Ctrl Pts',(-14.1570626989914,-13.0354801622186,
118.354076675119)) ;
#187603 = CARTESIAN_POINT('Ctrl Pts',(-14.1346590237781,-13.0600685836045,
118.285838693899)) ;
#187604 = CARTESIAN_POINT('Ctrl Pts',(-14.0826035780406,-12.7987719757991,
118.162997434216)) ;
#187605 = CARTESIAN_POINT('Ctrl Pts',(-14.0630626393208,-12.8416392533606,
118.103478886264)) ;
#187606 = CARTESIAN_POINT('Ctrl Pts',(-13.9892587820211,-12.8416391878999,
118.127709885675)) ;
#187607 = CARTESIAN_POINT('Ctrl Pts',(-13.9154549247215,-12.8416391224392,
118.151940885086)) ;
#187608 = CARTESIAN_POINT('Ctrl Pts',(-13.9349958634413,-12.7987718448777,
118.211459433038)) ;
#187609 = CARTESIAN_POINT('Ctrl Pts',(-13.9545368021612,-12.7559045673161,
118.27097798099)) ;
#187610 = CARTESIAN_POINT('Ctrl Pts',(-14.0283406594608,-12.7559046327768,
118.246746981579)) ;
#187611 = CARTESIAN_POINT('Ctrl Pts',(-14.1021445167604,-12.7559046982375,
118.222515982169)) ;
#187612 = CARTESIAN_POINT('Ctrl Pts',(-14.0826035780406,-12.7987719757991,
118.162997434216)) ;
#187613 = CARTESIAN_POINT('Ctrl Pts',(-14.0113057802947,-12.5848307790968,
117.981092726393)) ;
#187614 = CARTESIAN_POINT('Ctrl Pts',(-13.9959849291863,-12.6426967262578,
117.934427884294)) ;
#187615 = CARTESIAN_POINT('Ctrl Pts',(-13.9221810656705,-12.6426966715405,
117.958658864771)) ;
#187616 = CARTESIAN_POINT('Ctrl Pts',(-13.8483772021547,-12.6426966168232,
117.982889845248)) ;
#187617 = CARTESIAN_POINT('Ctrl Pts',(-13.863698053263,-12.5848306696622,
118.029554687347)) ;
#187618 = CARTESIAN_POINT('Ctrl Pts',(-13.8790189043714,-12.5269647225012,
118.076219529447)) ;
#187619 = CARTESIAN_POINT('Ctrl Pts',(-13.9528227678873,-12.5269647772185,
118.05198854897)) ;
#187620 = CARTESIAN_POINT('Ctrl Pts',(-14.0266266314031,-12.5269648319358,
118.027757568493)) ;
#187621 = CARTESIAN_POINT('Ctrl Pts',(-14.0113057802947,-12.5848307790968,
117.981092726393)) ;
#187622 = CARTESIAN_POINT('Ctrl Pts',(-13.923908857957,-12.428840573078,117.750424143547)) ;
#187623 = CARTESIAN_POINT('Ctrl Pts',(-13.9139322792742,-12.4976814923142,
117.720037092829)) ;
#187624 = CARTESIAN_POINT('Ctrl Pts',(-13.8401284100277,-12.4976814537986,
117.744268055851)) ;
#187625 = CARTESIAN_POINT('Ctrl Pts',(-13.7663245407813,-12.497681415283,
117.768499018874)) ;
#187626 = CARTESIAN_POINT('Ctrl Pts',(-13.776301119464,-12.4288404960468,
117.798886069592)) ;
#187627 = CARTESIAN_POINT('Ctrl Pts',(-13.7862776981468,-12.3599995768106,
117.829273120311)) ;
#187628 = CARTESIAN_POINT('Ctrl Pts',(-13.8600815673933,-12.3599996153262,
117.805042157288)) ;
#187629 = CARTESIAN_POINT('Ctrl Pts',(-13.9338854366397,-12.3599996538418,
117.780811194266)) ;
#187630 = CARTESIAN_POINT('Ctrl Pts',(-13.923908857957,-12.428840573078,117.750424143547)) ;
#187631 = CARTESIAN_POINT('Ctrl Pts',(-13.8265622817162,-12.3440689509793,
117.489359771701)) ;
#187632 = CARTESIAN_POINT('Ctrl Pts',(-13.822634283057,-12.4189286311326,
117.477395719697)) ;
#187633 = CARTESIAN_POINT('Ctrl Pts',(-13.7488304098932,-12.4189286151795,
117.501626670787)) ;
#187634 = CARTESIAN_POINT('Ctrl Pts',(-13.6750265367294,-12.4189285992263,
117.525857621878)) ;
#187635 = CARTESIAN_POINT('Ctrl Pts',(-13.6789545353885,-12.3440689190729,
117.537821673882)) ;
#187636 = CARTESIAN_POINT('Ctrl Pts',(-13.6828825340477,-12.2692092389195,
117.549785725887)) ;
#187637 = CARTESIAN_POINT('Ctrl Pts',(-13.7566864072115,-12.2692092548727,
117.525554774796)) ;
#187638 = CARTESIAN_POINT('Ctrl Pts',(-13.8304902803753,-12.2692092708259,
117.501323823705)) ;
#187639 = CARTESIAN_POINT('Ctrl Pts',(-13.8265622817162,-12.3440689509793,
117.489359771701)) ;
#187640 = CARTESIAN_POINT('Ctrl Pts',(-13.724775039694,-12.3364316802486,
117.214968341071)) ;
#187641 = CARTESIAN_POINT('Ctrl Pts',(-13.727210259981,-12.4119346033566,
117.222385627174)) ;
#187642 = CARTESIAN_POINT('Ctrl Pts',(-13.6534063849637,-12.4119346140826,
117.24661657262)) ;
#187643 = CARTESIAN_POINT('Ctrl Pts',(-13.5796025099464,-12.4119346248087,
117.270847518065)) ;
#187644 = CARTESIAN_POINT('Ctrl Pts',(-13.5771672896594,-12.3364317017007,
117.263430231962)) ;
#187645 = CARTESIAN_POINT('Ctrl Pts',(-13.5747320693725,-12.2609287785927,
117.256012945858)) ;
#187646 = CARTESIAN_POINT('Ctrl Pts',(-13.6485359443898,-12.2609287678666,
117.231782000413)) ;
#187647 = CARTESIAN_POINT('Ctrl Pts',(-13.722339819407,-12.2609287571406,
117.207551054968)) ;
#187648 = CARTESIAN_POINT('Ctrl Pts',(-13.724775039694,-12.3364316802486,
117.214968341071)) ;
#187649 = CARTESIAN_POINT('Ctrl Pts',(-13.6265849302069,-12.4059134721985,
116.95117861997)) ;
#187650 = CARTESIAN_POINT('Ctrl Pts',(-13.6351489860303,-12.4766756049436,
116.977263350182)) ;
#187651 = CARTESIAN_POINT('Ctrl Pts',(-13.5613451122622,-12.4766756431297,
117.001494299432)) ;
#187652 = CARTESIAN_POINT('Ctrl Pts',(-13.4875412384941,-12.4766756813157,
117.025725248682)) ;
#187653 = CARTESIAN_POINT('Ctrl Pts',(-13.4789771826708,-12.4059135485707,
116.99964051847)) ;
#187654 = CARTESIAN_POINT('Ctrl Pts',(-13.4704131268474,-12.3351514158256,
116.973555788258)) ;
#187655 = CARTESIAN_POINT('Ctrl Pts',(-13.5442170006155,-12.3351513776395,
116.949324839008)) ;
#187656 = CARTESIAN_POINT('Ctrl Pts',(-13.6180208743836,-12.3351513394535,
116.925093889758)) ;
#187657 = CARTESIAN_POINT('Ctrl Pts',(-13.6265849302069,-12.4059134721985,
116.95117861997)) ;
#187658 = CARTESIAN_POINT('Ctrl Pts',(-13.5366237570857,-12.5482447968648,
116.712705270971)) ;
#187659 = CARTESIAN_POINT('Ctrl Pts',(-13.5507458951502,-12.609174259838,
116.755719022846)) ;
#187660 = CARTESIAN_POINT('Ctrl Pts',(-13.4769420250043,-12.6091743240943,
116.779949983129)) ;
#187661 = CARTESIAN_POINT('Ctrl Pts',(-13.4031381548583,-12.6091743883507,
116.804180943411)) ;
#187662 = CARTESIAN_POINT('Ctrl Pts',(-13.3890160167938,-12.5482449253774,
116.761167191536)) ;
#187663 = CARTESIAN_POINT('Ctrl Pts',(-13.3748938787293,-12.4873154624041,
116.71815343966)) ;
#187664 = CARTESIAN_POINT('Ctrl Pts',(-13.4486977488753,-12.4873153981478,
116.693922479378)) ;
#187665 = CARTESIAN_POINT('Ctrl Pts',(-13.5225016190212,-12.4873153338915,
116.669691519095)) ;
#187666 = CARTESIAN_POINT('Ctrl Pts',(-13.5366237570857,-12.5482447968648,
116.712705270971)) ;
#187667 = CARTESIAN_POINT('Ctrl Pts',(-13.4616241401097,-12.7523234032848,
116.519655572722)) ;
#187668 = CARTESIAN_POINT('Ctrl Pts',(-13.4802710790298,-12.7990945462317,
116.576451137909)) ;
#187669 = CARTESIAN_POINT('Ctrl Pts',(-13.406467214966,-12.7990946317952,
116.600682116717)) ;
#187670 = CARTESIAN_POINT('Ctrl Pts',(-13.3326633509022,-12.7990947173587,
116.624913095525)) ;
#187671 = CARTESIAN_POINT('Ctrl Pts',(-13.314016411982,-12.7523235744117,
116.568117530338)) ;
#187672 = CARTESIAN_POINT('Ctrl Pts',(-13.2953694730618,-12.7055524314648,
116.51132196515)) ;
#187673 = CARTESIAN_POINT('Ctrl Pts',(-13.3691733371256,-12.7055523459013,
116.487090986342)) ;
#187674 = CARTESIAN_POINT('Ctrl Pts',(-13.4429772011895,-12.7055522603379,
116.462860007534)) ;
#187675 = CARTESIAN_POINT('Ctrl Pts',(-13.4616241401097,-12.7523234032848,
116.519655572722)) ;
#187676 = CARTESIAN_POINT('Ctrl Pts',(-13.4055646043146,-13.0044659647124,
116.384391147857)) ;
#187677 = CARTESIAN_POINT('Ctrl Pts',(-13.4274187926225,-13.0337028196908,
116.450955477187)) ;
#187678 = CARTESIAN_POINT('Ctrl Pts',(-13.3536149363877,-13.0337029200477,
116.47518647984)) ;
#187679 = CARTESIAN_POINT('Ctrl Pts',(-13.2798110801529,-13.0337030204046,
116.499417482494)) ;
#187680 = CARTESIAN_POINT('Ctrl Pts',(-13.2579568918449,-13.0044661654261,
116.432853153164)) ;
#187681 = CARTESIAN_POINT('Ctrl Pts',(-13.236102703537,-12.9752293104477,
116.366288823835)) ;
#187682 = CARTESIAN_POINT('Ctrl Pts',(-13.3099065597718,-12.9752292100908,
116.342057821181)) ;
#187683 = CARTESIAN_POINT('Ctrl Pts',(-13.3837104160066,-12.9752291097339,
116.317826818527)) ;
#187684 = CARTESIAN_POINT('Ctrl Pts',(-13.4055646043146,-13.0044659647124,
116.384391147857)) ;
#187685 = CARTESIAN_POINT('Ctrl Pts',(-13.3720356013224,-13.2877069321833,
116.317913961057)) ;
#187686 = CARTESIAN_POINT('Ctrl Pts',(-13.3955257178423,-13.2972126814731,
116.389461063794)) ;
#187687 = CARTESIAN_POINT('Ctrl Pts',(-13.3217218704914,-13.2972127876648,
116.413692093507)) ;
#187688 = CARTESIAN_POINT('Ctrl Pts',(-13.2479180231405,-13.2972128938564,
116.437923123219)) ;
#187689 = CARTESIAN_POINT('Ctrl Pts',(-13.2244279066205,-13.2877071445666,
116.366376020483)) ;
#187690 = CARTESIAN_POINT('Ctrl Pts',(-13.2009377901005,-13.2782013952768,
116.294828917746)) ;
#187691 = CARTESIAN_POINT('Ctrl Pts',(-13.2747416374515,-13.2782012890852,
116.270597888033)) ;
#187692 = CARTESIAN_POINT('Ctrl Pts',(-13.3485454848024,-13.2782011828935,
116.24636685832)) ;
#187693 = CARTESIAN_POINT('Ctrl Pts',(-13.3720356013224,-13.2877069321833,
116.317913961057)) ;
#187694 = CARTESIAN_POINT('Ctrl Pts',(-13.362788115581,-13.5768962487208,
116.324968700109)) ;
#187695 = CARTESIAN_POINT('Ctrl Pts',(-13.3862298492881,-13.5662255723237,
116.396368436635)) ;
#187696 = CARTESIAN_POINT('Ctrl Pts',(-13.312426010763,-13.5662256764684,
116.42059949323)) ;
#187697 = CARTESIAN_POINT('Ctrl Pts',(-13.2386221722379,-13.5662257806131,
116.444830549825)) ;
#187698 = CARTESIAN_POINT('Ctrl Pts',(-13.2151804385309,-13.5768964570101,
116.373430813298)) ;
#187699 = CARTESIAN_POINT('Ctrl Pts',(-13.1917387048238,-13.5875671334072,
116.302031076772)) ;
#187700 = CARTESIAN_POINT('Ctrl Pts',(-13.2655425433489,-13.5875670292625,
116.277800020177)) ;
#187701 = CARTESIAN_POINT('Ctrl Pts',(-13.339346381874,-13.5875669251178,
116.253568963582)) ;
#187702 = CARTESIAN_POINT('Ctrl Pts',(-13.362788115581,-13.5768962487208,
116.324968700109)) ;
#187703 = CARTESIAN_POINT('Ctrl Pts',(-13.3775423934189,-13.8582071770573,
116.405572255842)) ;
#187704 = CARTESIAN_POINT('Ctrl Pts',(-13.3992513169307,-13.8278804219563,
116.471694132178)) ;
#187705 = CARTESIAN_POINT('Ctrl Pts',(-13.3254474864398,-13.8278805144787,
116.495925213244)) ;
#187706 = CARTESIAN_POINT('Ctrl Pts',(-13.2516436559489,-13.8278806070012,
116.520156294309)) ;
#187707 = CARTESIAN_POINT('Ctrl Pts',(-13.229934732437,-13.8582073621022,
116.454034417973)) ;
#187708 = CARTESIAN_POINT('Ctrl Pts',(-13.2082258089251,-13.8885341172032,
116.387912541636)) ;
#187709 = CARTESIAN_POINT('Ctrl Pts',(-13.2820296394161,-13.8885340246808,
116.363681460571)) ;
#187710 = CARTESIAN_POINT('Ctrl Pts',(-13.355833469907,-13.8885339321583,
116.339450379505)) ;
#187711 = CARTESIAN_POINT('Ctrl Pts',(-13.3775423934189,-13.8582071770573,
116.405572255842)) ;
#187712 = CARTESIAN_POINT('Ctrl Pts',(-13.4146012475886,-14.1061445299723,
116.553894025949)) ;
#187713 = CARTESIAN_POINT('Ctrl Pts',(-13.4330218964066,-14.0584618505827,
116.610000348217)) ;
#187714 = CARTESIAN_POINT('Ctrl Pts',(-13.3592180722115,-14.0584619253186,
116.634231448458)) ;
#187715 = CARTESIAN_POINT('Ctrl Pts',(-13.2854142480164,-14.0584620000544,
116.6584625487)) ;
#187716 = CARTESIAN_POINT('Ctrl Pts',(-13.2669935991984,-14.106144679444,
116.602356226433)) ;
#187717 = CARTESIAN_POINT('Ctrl Pts',(-13.2485729503803,-14.1538273588336,
116.546249904166)) ;
#187718 = CARTESIAN_POINT('Ctrl Pts',(-13.3223767745754,-14.1538272840978,
116.522018803924)) ;
#187719 = CARTESIAN_POINT('Ctrl Pts',(-13.3961805987705,-14.1538272093619,
116.497787703682)) ;
#187720 = CARTESIAN_POINT('Ctrl Pts',(-13.4146012475886,-14.1061445299723,
116.553894025949)) ;
#187721 = CARTESIAN_POINT('Ctrl Pts',(-13.4702307809164,-14.3044364274605,
116.758686302977)) ;
#187722 = CARTESIAN_POINT('Ctrl Pts',(-13.4840635351767,-14.2428379118998,
116.800818638766)) ;
#187723 = CARTESIAN_POINT('Ctrl Pts',(-13.4102597152836,-14.2428379649648,
116.82504975211)) ;
#187724 = CARTESIAN_POINT('Ctrl Pts',(-13.3364558953904,-14.2428380180299,
116.849280865455)) ;
#187725 = CARTESIAN_POINT('Ctrl Pts',(-13.3226231411301,-14.3044365335905,
116.807148529667)) ;
#187726 = CARTESIAN_POINT('Ctrl Pts',(-13.3087903868698,-14.3660350491512,
116.765016193878)) ;
#187727 = CARTESIAN_POINT('Ctrl Pts',(-13.382594206763,-14.3660349960862,
116.740785080533)) ;
#187728 = CARTESIAN_POINT('Ctrl Pts',(-13.4563980266561,-14.3660349430211,
116.716553967189)) ;
#187729 = CARTESIAN_POINT('Ctrl Pts',(-13.4702307809164,-14.3044364274605,
116.758686302977)) ;
#187730 = CARTESIAN_POINT('Ctrl Pts',(-13.5399984230881,-14.4399899755949,
117.006607909742)) ;
#187731 = CARTESIAN_POINT('Ctrl Pts',(-13.5482480139637,-14.3688346755136,
117.031734830812)) ;
#187732 = CARTESIAN_POINT('Ctrl Pts',(-13.474444195943,-14.3688347045207,
117.05596594986)) ;
#187733 = CARTESIAN_POINT('Ctrl Pts',(-13.4006403779222,-14.3688347335278,
117.080197068908)) ;
#187734 = CARTESIAN_POINT('Ctrl Pts',(-13.3923907870465,-14.4399900336091,
117.055070147837)) ;
#187735 = CARTESIAN_POINT('Ctrl Pts',(-13.3841411961708,-14.5111453336905,
117.029943226766)) ;
#187736 = CARTESIAN_POINT('Ctrl Pts',(-13.4579450141916,-14.5111453046834,
117.005712107718)) ;
#187737 = CARTESIAN_POINT('Ctrl Pts',(-13.5317488322124,-14.5111452756763,
116.981480988671)) ;
#187738 = CARTESIAN_POINT('Ctrl Pts',(-13.5399984230881,-14.4399899755949,
117.006607909742)) ;
#187739 = CARTESIAN_POINT('Ctrl Pts',(-13.6186161086514,-14.5025588290042,
117.281708410836)) ;
#187740 = CARTESIAN_POINT('Ctrl Pts',(-13.6206516993991,-14.4269270667857,
117.287908490306)) ;
#187741 = CARTESIAN_POINT('Ctrl Pts',(-13.5468478802534,-14.4269270722705,
117.312139605927)) ;
#187742 = CARTESIAN_POINT('Ctrl Pts',(-13.4730440611076,-14.4269270777552,
117.336370721548)) ;
#187743 = CARTESIAN_POINT('Ctrl Pts',(-13.4710084703599,-14.5025588399736,
117.330170642078)) ;
#187744 = CARTESIAN_POINT('Ctrl Pts',(-13.4689728796121,-14.5781906021921,
117.323970562609)) ;
#187745 = CARTESIAN_POINT('Ctrl Pts',(-13.5427766987579,-14.5781905967074,
117.299739446988)) ;
#187746 = CARTESIAN_POINT('Ctrl Pts',(-13.6165805179036,-14.5781905912227,
117.275508331367)) ;
#187747 = CARTESIAN_POINT('Ctrl Pts',(-13.6186161086514,-14.5025588290042,
117.281708410836)) ;
#187748 = CARTESIAN_POINT('Ctrl Pts',(-13.6987823075738,-14.4867545034676,
117.561336491413)) ;
#187749 = CARTESIAN_POINT('Ctrl Pts',(-13.6944901322377,-14.4121117686934,
117.548263216521)) ;
#187750 = CARTESIAN_POINT('Ctrl Pts',(-13.6206863103232,-14.4121117549338,
117.572494323709)) ;
#187751 = CARTESIAN_POINT('Ctrl Pts',(-13.5468824884086,-14.4121117411741,
117.596725430897)) ;
#187752 = CARTESIAN_POINT('Ctrl Pts',(-13.5511746637448,-14.4867544759483,
117.609798705789)) ;
#187753 = CARTESIAN_POINT('Ctrl Pts',(-13.5554668390809,-14.5613972107224,
117.622871980681)) ;
#187754 = CARTESIAN_POINT('Ctrl Pts',(-13.6292706609955,-14.5613972244821,
117.598640873493)) ;
#187755 = CARTESIAN_POINT('Ctrl Pts',(-13.70307448291,-14.5613972382417,117.574409766305)) ;
#187756 = CARTESIAN_POINT('Ctrl Pts',(-13.6987823075738,-14.4867545034676,
117.561336491413)) ;
#187757 = CARTESIAN_POINT('Ctrl Pts',(-13.7741769319229,-14.395053842158,
117.826317562051)) ;
#187758 = CARTESIAN_POINT('Ctrl Pts',(-13.7638829047759,-14.3267009786415,
117.794963615073)) ;
#187759 = CARTESIAN_POINT('Ctrl Pts',(-13.6900790789911,-14.3267009501932,
117.819194710473)) ;
#187760 = CARTESIAN_POINT('Ctrl Pts',(-13.6162752532064,-14.3267009217449,
117.843425805873)) ;
#187761 = CARTESIAN_POINT('Ctrl Pts',(-13.6265692803534,-14.3950537852614,
117.874779752851)) ;
#187762 = CARTESIAN_POINT('Ctrl Pts',(-13.6368633075005,-14.463406648778,
117.906133699828)) ;
#187763 = CARTESIAN_POINT('Ctrl Pts',(-13.7106671332852,-14.4634066772262,
117.881902604428)) ;
#187764 = CARTESIAN_POINT('Ctrl Pts',(-13.78447095907,-14.4634067056745,117.857671509028)) ;
#187765 = CARTESIAN_POINT('Ctrl Pts',(-13.7741769319229,-14.395053842158,
117.826317562051)) ;
#187766 = CARTESIAN_POINT('Ctrl Pts',(-13.8391716224737,-14.2332235226471,
118.059743172962)) ;
#187767 = CARTESIAN_POINT('Ctrl Pts',(-13.8235901984031,-14.1760661182545,
118.012284668238)) ;
#187768 = CARTESIAN_POINT('Ctrl Pts',(-13.7497863676252,-14.1760660813659,
118.03651574843)) ;
#187769 = CARTESIAN_POINT('Ctrl Pts',(-13.6759825368474,-14.1760660444773,
118.060746828621)) ;
#187770 = CARTESIAN_POINT('Ctrl Pts',(-13.691563960918,-14.2332234488699,
118.108205333346)) ;
#187771 = CARTESIAN_POINT('Ctrl Pts',(-13.7071453849885,-14.2903808532625,
118.15566383807)) ;
#187772 = CARTESIAN_POINT('Ctrl Pts',(-13.7809492157664,-14.2903808901511,
118.131432757878)) ;
#187773 = CARTESIAN_POINT('Ctrl Pts',(-13.8547530465442,-14.2903809270397,
118.107201677686)) ;
#187774 = CARTESIAN_POINT('Ctrl Pts',(-13.8391716224737,-14.2332235226471,
118.059743172962)) ;
#187775 = CARTESIAN_POINT('Ctrl Pts',(-13.8880711188325,-14.0127300062097,
118.244172770846)) ;
#187776 = CARTESIAN_POINT('Ctrl Pts',(-13.8683174044897,-13.9708810531426,
118.184006143322)) ;
#187777 = CARTESIAN_POINT('Ctrl Pts',(-13.7945135686933,-13.9708810143348,
118.208237208228)) ;
#187778 = CARTESIAN_POINT('Ctrl Pts',(-13.7207097328969,-13.9708809755269,
118.232468273134)) ;
#187779 = CARTESIAN_POINT('Ctrl Pts',(-13.7404634472397,-14.0127299285939,
118.292634900658)) ;
#187780 = CARTESIAN_POINT('Ctrl Pts',(-13.7602171615824,-14.054578881661,
118.352801528181)) ;
#187781 = CARTESIAN_POINT('Ctrl Pts',(-13.8340209973788,-14.0545789204688,
118.328570463275)) ;
#187782 = CARTESIAN_POINT('Ctrl Pts',(-13.9078248331752,-14.0545789592767,
118.304339398369)) ;
#187783 = CARTESIAN_POINT('Ctrl Pts',(-13.8880711188325,-14.0127300062097,
118.244172770846)) ;
#187784 = CARTESIAN_POINT('Ctrl Pts',(-13.9166288887075,-13.7497867225439,
118.366622212608)) ;
#187785 = CARTESIAN_POINT('Ctrl Pts',(-13.8941173007303,-13.7262335262759,
118.298055547143)) ;
#187786 = CARTESIAN_POINT('Ctrl Pts',(-13.8203134605769,-13.7262334907042,
118.322286598779)) ;
#187787 = CARTESIAN_POINT('Ctrl Pts',(-13.7465096204236,-13.7262334551324,
118.346517650415)) ;
#187788 = CARTESIAN_POINT('Ctrl Pts',(-13.7690212084009,-13.7497866514004,
118.415084315879)) ;
#187789 = CARTESIAN_POINT('Ctrl Pts',(-13.7915327963782,-13.7733398476684,
118.483650981343)) ;
#187790 = CARTESIAN_POINT('Ctrl Pts',(-13.8653366365315,-13.7733398832402,
118.459419929707)) ;
#187791 = CARTESIAN_POINT('Ctrl Pts',(-13.9391404766848,-13.7733399188119,
118.435188878072)) ;
#187792 = CARTESIAN_POINT('Ctrl Pts',(-13.9166288887075,-13.7497867225439,
118.366622212608)) ;
#187793 = CARTESIAN_POINT('Ctrl Pts',(-13.9219007960497,-13.4618226176213,
118.418297641467)) ;
#187794 = CARTESIAN_POINT('Ctrl Pts',(-13.8982497624361,-13.4583403895165,
118.346260408634)) ;
#187795 = CARTESIAN_POINT('Ctrl Pts',(-13.8244459191647,-13.458340362269,
118.370491450772)) ;
#187796 = CARTESIAN_POINT('Ctrl Pts',(-13.7506420758933,-13.4583403350215,
118.394722492911)) ;
#187797 = CARTESIAN_POINT('Ctrl Pts',(-13.7742931095069,-13.4618225631264,
118.466759725744)) ;
#187798 = CARTESIAN_POINT('Ctrl Pts',(-13.7979441431205,-13.4653047912312,
118.538796958577)) ;
#187799 = CARTESIAN_POINT('Ctrl Pts',(-13.8717479863919,-13.4653048184787,
118.514565916438)) ;
#187800 = CARTESIAN_POINT('Ctrl Pts',(-13.9455518296633,-13.4653048457262,
118.4903348743)) ;
#187801 = CARTESIAN_POINT('Ctrl Pts',(-13.9219007960497,-13.4618226176213,
118.418297641467)) ;
#187802 = CARTESIAN_POINT('Ctrl Pts',(-13.903127021165,-13.1741720910159,
118.396295941709)) ;
#187803 = CARTESIAN_POINT('Ctrl Pts',(-13.8800232858796,-13.1907692085376,
118.325925691383)) ;
#187804 = CARTESIAN_POINT('Ctrl Pts',(-13.8062194407577,-13.1907691874801,
118.350156727884)) ;
#187805 = CARTESIAN_POINT('Ctrl Pts',(-13.7324155956357,-13.1907691664227,
118.374387764386)) ;
#187806 = CARTESIAN_POINT('Ctrl Pts',(-13.755519330921,-13.1741720489011,
118.444758014713)) ;
#187807 = CARTESIAN_POINT('Ctrl Pts',(-13.7786230662063,-13.1575749313794,
118.515128265039)) ;
#187808 = CARTESIAN_POINT('Ctrl Pts',(-13.8524269113283,-13.1575749524368,
118.490897228537)) ;
#187809 = CARTESIAN_POINT('Ctrl Pts',(-13.9262307564503,-13.1575749734943,
118.466666192035)) ;
#187810 = CARTESIAN_POINT('Ctrl Pts',(-13.903127021165,-13.1741720910159,
118.396295941709)) ;
#187811 = CARTESIAN_POINT('Ctrl Pts',(-13.8603632973549,-12.9003777795887,
118.301689211796)) ;
#187812 = CARTESIAN_POINT('Ctrl Pts',(-13.8394728277255,-12.9361179634059,
118.23806021172)) ;
#187813 = CARTESIAN_POINT('Ctrl Pts',(-13.7656689822045,-12.9361179523589,
118.262291247007)) ;
#187814 = CARTESIAN_POINT('Ctrl Pts',(-13.6918651366836,-12.9361179413118,
118.286522282294)) ;
#187815 = CARTESIAN_POINT('Ctrl Pts',(-13.712755606313,-12.9003777574947,
118.35015128237)) ;
#187816 = CARTESIAN_POINT('Ctrl Pts',(-13.7336460759424,-12.8646375736775,
118.413780282446)) ;
#187817 = CARTESIAN_POINT('Ctrl Pts',(-13.8074499214633,-12.8646375847245,
118.389549247159)) ;
#187818 = CARTESIAN_POINT('Ctrl Pts',(-13.8812537669843,-12.8646375957715,
118.365318211872)) ;
#187819 = CARTESIAN_POINT('Ctrl Pts',(-13.8603632973549,-12.9003777795887,
118.301689211796)) ;
#187820 = CARTESIAN_POINT('Ctrl Pts',(-13.7965184753655,-12.6657294356323,
118.142588775569)) ;
#187821 = CARTESIAN_POINT('Ctrl Pts',(-13.7793228293971,-12.7179077722526,
118.090213612314)) ;
#187822 = CARTESIAN_POINT('Ctrl Pts',(-13.7055189843026,-12.7179077672934,
118.1144446489)) ;
#187823 = CARTESIAN_POINT('Ctrl Pts',(-13.6317151392082,-12.7179077623343,
118.138675685485)) ;
#187824 = CARTESIAN_POINT('Ctrl Pts',(-13.6489107851767,-12.665729425714,
118.19105084874)) ;
#187825 = CARTESIAN_POINT('Ctrl Pts',(-13.6661064311451,-12.6135510890938,
118.243426011995)) ;
#187826 = CARTESIAN_POINT('Ctrl Pts',(-13.7399102762396,-12.6135510940529,
118.219194975409)) ;
#187827 = CARTESIAN_POINT('Ctrl Pts',(-13.813714121334,-12.6135510990121,
118.194963938823)) ;
#187828 = CARTESIAN_POINT('Ctrl Pts',(-13.7965184753655,-12.6657294356323,
118.142588775569)) ;
#187829 = CARTESIAN_POINT('Ctrl Pts',(-13.7148231526105,-12.4838951882172,
117.929294896523)) ;
#187830 = CARTESIAN_POINT('Ctrl Pts',(-13.7025707556539,-12.5488490680583,
117.891976072276)) ;
#187831 = CARTESIAN_POINT('Ctrl Pts',(-13.6287669116955,-12.5488490674887,
117.916207112322)) ;
#187832 = CARTESIAN_POINT('Ctrl Pts',(-13.5549630677371,-12.5488490669192,
117.940438152368)) ;
#187833 = CARTESIAN_POINT('Ctrl Pts',(-13.5672154646937,-12.4838951870781,
117.977756976615)) ;
#187834 = CARTESIAN_POINT('Ctrl Pts',(-13.5794678616503,-12.418941307237,
118.015075800863)) ;
#187835 = CARTESIAN_POINT('Ctrl Pts',(-13.6532717056087,-12.4189413078066,
117.990844760817)) ;
#187836 = CARTESIAN_POINT('Ctrl Pts',(-13.727075549567,-12.4189413083761,
117.966613720771)) ;
#187837 = CARTESIAN_POINT('Ctrl Pts',(-13.7148231526105,-12.4838951882172,
117.929294896523)) ;
#187838 = CARTESIAN_POINT('Ctrl Pts',(-13.6210385512733,-12.3696269961183,
117.679015146672)) ;
#187839 = CARTESIAN_POINT('Ctrl Pts',(-13.614584536571,-12.4426568392055,
117.659357259267)) ;
#187840 = CARTESIAN_POINT('Ctrl Pts',(-13.54078069357,-12.4426568397969,117.683588302229)) ;
#187841 = CARTESIAN_POINT('Ctrl Pts',(-13.466976850569,-12.4426568403884,
117.707819345191)) ;
#187842 = CARTESIAN_POINT('Ctrl Pts',(-13.4734308652713,-12.3696269973012,
117.727477232596)) ;
#187843 = CARTESIAN_POINT('Ctrl Pts',(-13.4798848799736,-12.2965971542141,
117.74713512)) ;
#187844 = CARTESIAN_POINT('Ctrl Pts',(-13.5536887229746,-12.2965971536226,
117.722904077038)) ;
#187845 = CARTESIAN_POINT('Ctrl Pts',(-13.6274925659757,-12.2965971530311,
117.698673034076)) ;
#187846 = CARTESIAN_POINT('Ctrl Pts',(-13.6210385512733,-12.3696269961183,
117.679015146672)) ;
#187847 = CARTESIAN_POINT('Ctrl Pts',(-13.5204267176276,-12.3300023799241,
117.408075297011)) ;
#187848 = CARTESIAN_POINT('Ctrl Pts',(-13.5202538843444,-12.4059080645877,
117.407548874782)) ;
#187849 = CARTESIAN_POINT('Ctrl Pts',(-13.4464500419793,-12.4059080646803,
117.431779919681)) ;
#187850 = CARTESIAN_POINT('Ctrl Pts',(-13.3726461996142,-12.4059080647729,
117.456010964579)) ;
#187851 = CARTESIAN_POINT('Ctrl Pts',(-13.3728190328973,-12.3300023801093,
117.456537386809)) ;
#187852 = CARTESIAN_POINT('Ctrl Pts',(-13.3729918661804,-12.2540966954457,
117.457063809038)) ;
#187853 = CARTESIAN_POINT('Ctrl Pts',(-13.4467957085455,-12.2540966953531,
117.432832764139)) ;
#187854 = CARTESIAN_POINT('Ctrl Pts',(-13.5205995509106,-12.2540966952605,
117.40860171924)) ;
#187855 = CARTESIAN_POINT('Ctrl Pts',(-13.5204267176276,-12.3300023799241,
117.408075297011)) ;
#187856 = CARTESIAN_POINT('Ctrl Pts',(-13.4198641245608,-12.3684199778557,
117.137243310197)) ;
#187857 = CARTESIAN_POINT('Ctrl Pts',(-13.4259793249483,-12.4417552779972,
117.155869223949)) ;
#187858 = CARTESIAN_POINT('Ctrl Pts',(-13.3521754823948,-12.4417552770606,
117.180100268274)) ;
#187859 = CARTESIAN_POINT('Ctrl Pts',(-13.2783716398414,-12.441755276124,
117.2043313126)) ;
#187860 = CARTESIAN_POINT('Ctrl Pts',(-13.272256439454,-12.3684199759825,
117.185705398848)) ;
#187861 = CARTESIAN_POINT('Ctrl Pts',(-13.2661412390666,-12.2950846758409,
117.167079485096)) ;
#187862 = CARTESIAN_POINT('Ctrl Pts',(-13.33994508162,-12.2950846767775,117.14284844077)) ;
#187863 = CARTESIAN_POINT('Ctrl Pts',(-13.4137489241733,-12.2950846777141,
117.118617396445)) ;
#187864 = CARTESIAN_POINT('Ctrl Pts',(-13.4198641245608,-12.3684199778557,
117.137243310197)) ;
#187865 = CARTESIAN_POINT('Ctrl Pts',(-13.3254467352035,-12.4825669571575,
116.885241947658)) ;
#187866 = CARTESIAN_POINT('Ctrl Pts',(-13.3374276722368,-12.5480396537864,
116.92173394874)) ;
#187867 = CARTESIAN_POINT('Ctrl Pts',(-13.2636238287276,-12.5480396536061,
116.945964990155)) ;
#187868 = CARTESIAN_POINT('Ctrl Pts',(-13.1898199852184,-12.5480396534258,
116.970196031569)) ;
#187869 = CARTESIAN_POINT('Ctrl Pts',(-13.1778390481851,-12.4825669567968,
116.933704030486)) ;
#187870 = CARTESIAN_POINT('Ctrl Pts',(-13.1658581111518,-12.4170942601679,
116.897212029403)) ;
#187871 = CARTESIAN_POINT('Ctrl Pts',(-13.239661954661,-12.4170942603482,
116.872980987989)) ;
#187872 = CARTESIAN_POINT('Ctrl Pts',(-13.3134657981702,-12.4170942605285,
116.848749946575)) ;
#187873 = CARTESIAN_POINT('Ctrl Pts',(-13.3254467352035,-12.4825669571575,
116.885241947658)) ;
#187874 = CARTESIAN_POINT('Ctrl Pts',(-13.2438983807686,-12.6630281231511,
116.672250461998)) ;
#187875 = CARTESIAN_POINT('Ctrl Pts',(-13.2608585513106,-12.7159956192618,
116.723908404873)) ;
#187876 = CARTESIAN_POINT('Ctrl Pts',(-13.1870547068666,-12.7159956220205,
116.74813944344)) ;
#187877 = CARTESIAN_POINT('Ctrl Pts',(-13.1132508624226,-12.7159956247792,
116.772370482007)) ;
#187878 = CARTESIAN_POINT('Ctrl Pts',(-13.0962906918806,-12.6630281286685,
116.720712539132)) ;
#187879 = CARTESIAN_POINT('Ctrl Pts',(-13.0793305213386,-12.6100606325577,
116.669054596257)) ;
#187880 = CARTESIAN_POINT('Ctrl Pts',(-13.1531343657826,-12.610060629799,
116.64482355769)) ;
#187881 = CARTESIAN_POINT('Ctrl Pts',(-13.2269382102266,-12.6100606270403,
116.620592519123)) ;
#187882 = CARTESIAN_POINT('Ctrl Pts',(-13.2438983807686,-12.6630281231511,
116.672250461998)) ;
#187883 = CARTESIAN_POINT('Ctrl Pts',(-13.1795990563112,-12.898267035054,
116.511928383513)) ;
#187884 = CARTESIAN_POINT('Ctrl Pts',(-13.2003385571015,-12.9348862826856,
116.575097556412)) ;
#187885 = CARTESIAN_POINT('Ctrl Pts',(-13.126534711989,-12.9348862916205,
116.599328592942)) ;
#187886 = CARTESIAN_POINT('Ctrl Pts',(-13.0527308668765,-12.9348863005553,
116.623559629473)) ;
#187887 = CARTESIAN_POINT('Ctrl Pts',(-13.0319913660862,-12.8982670529237,
116.560390456574)) ;
#187888 = CARTESIAN_POINT('Ctrl Pts',(-13.0112518652958,-12.8616478052921,
116.497221283675)) ;
#187889 = CARTESIAN_POINT('Ctrl Pts',(-13.0850557104084,-12.8616477963572,
116.472990247145)) ;
#187890 = CARTESIAN_POINT('Ctrl Pts',(-13.1588595555209,-12.8616477874224,
116.448759210614)) ;
#187891 = CARTESIAN_POINT('Ctrl Pts',(-13.1795990563112,-12.898267035054,
116.511928383513)) ;
#187892 = CARTESIAN_POINT('Ctrl Pts',(-13.1369040201403,-13.1692444185093,
116.417205413747)) ;
#187893 = CARTESIAN_POINT('Ctrl Pts',(-13.1599237253209,-13.1869963126333,
116.487319721198)) ;
#187894 = CARTESIAN_POINT('Ctrl Pts',(-13.0861198805798,-13.186996328282,
116.511550758859)) ;
#187895 = CARTESIAN_POINT('Ctrl Pts',(-13.0123160358387,-13.1869963439306,
116.535781796521)) ;
#187896 = CARTESIAN_POINT('Ctrl Pts',(-12.9892963306581,-13.1692444498067,
116.46566748907)) ;
#187897 = CARTESIAN_POINT('Ctrl Pts',(-12.9662766254774,-13.1514925556827,
116.395553181619)) ;
#187898 = CARTESIAN_POINT('Ctrl Pts',(-13.0400804702186,-13.1514925400341,
116.371322143957)) ;
#187899 = CARTESIAN_POINT('Ctrl Pts',(-13.1138843149597,-13.1514925243854,
116.347091106295)) ;
#187900 = CARTESIAN_POINT('Ctrl Pts',(-13.1369040201403,-13.1692444185093,
116.417205413747)) ;
#187901 = CARTESIAN_POINT('Ctrl Pts',(-13.1175944030743,-13.4593682561925,
116.393894522823)) ;
#187902 = CARTESIAN_POINT('Ctrl Pts',(-13.141261082871,-13.4568887930797,
116.465979410413)) ;
#187903 = CARTESIAN_POINT('Ctrl Pts',(-13.0674572395062,-13.4568888172156,
116.490210452267)) ;
#187904 = CARTESIAN_POINT('Ctrl Pts',(-12.9936533961414,-13.4568888413516,
116.514441494121)) ;
#187905 = CARTESIAN_POINT('Ctrl Pts',(-12.9699867163446,-13.4593683044645,
116.442356606531)) ;
#187906 = CARTESIAN_POINT('Ctrl Pts',(-12.9463200365478,-13.4618477675773,
116.370271718941)) ;
#187907 = CARTESIAN_POINT('Ctrl Pts',(-13.0201238799127,-13.4618477434414,
116.346040677087)) ;
#187908 = CARTESIAN_POINT('Ctrl Pts',(-13.0939277232775,-13.4618477193054,
116.321809635233)) ;
#187909 = CARTESIAN_POINT('Ctrl Pts',(-13.1175944030743,-13.4593682561925,
116.393894522823)) ;
#187910 = CARTESIAN_POINT('Ctrl Pts',(-13.1227026248899,-13.7466998259824,
116.444974799646)) ;
#187911 = CARTESIAN_POINT('Ctrl Pts',(-13.1453118932417,-13.7241548771273,
116.513838982417)) ;
#187912 = CARTESIAN_POINT('Ctrl Pts',(-13.071508052718,-13.7241549087659,
116.538070032924)) ;
#187913 = CARTESIAN_POINT('Ctrl Pts',(-12.9977042121942,-13.7241549404046,
116.562301083432)) ;
#187914 = CARTESIAN_POINT('Ctrl Pts',(-12.9750949438424,-13.7466998892598,
116.493436900661)) ;
#187915 = CARTESIAN_POINT('Ctrl Pts',(-12.9524856754905,-13.7692448381149,
116.42457271789)) ;
#187916 = CARTESIAN_POINT('Ctrl Pts',(-13.0262895160143,-13.7692448064763,
116.400341667382)) ;
#187917 = CARTESIAN_POINT('Ctrl Pts',(-13.100093356538,-13.7692447748376,
116.376110616875)) ;
#187918 = CARTESIAN_POINT('Ctrl Pts',(-13.1227026248899,-13.7466998259824,
116.444974799646)) ;
#187919 = CARTESIAN_POINT('Ctrl Pts',(-13.150926931708,-14.0096322945866,
116.566356438622)) ;
#187920 = CARTESIAN_POINT('Ctrl Pts',(-13.1708653800573,-13.9686968355008,
116.627085734444)) ;
#187921 = CARTESIAN_POINT('Ctrl Pts',(-13.0970615434274,-13.9686968703367,
116.651316796811)) ;
#187922 = CARTESIAN_POINT('Ctrl Pts',(-13.0232577067976,-13.9686969051726,
116.675547859179)) ;
#187923 = CARTESIAN_POINT('Ctrl Pts',(-13.0033192584483,-14.0096323642584,
116.614818563357)) ;
#187924 = CARTESIAN_POINT('Ctrl Pts',(-12.983380810099,-14.0505678233442,
116.554089267536)) ;
#187925 = CARTESIAN_POINT('Ctrl Pts',(-13.0571846467288,-14.0505677885083,
116.529858205168)) ;
#187926 = CARTESIAN_POINT('Ctrl Pts',(-13.1309884833587,-14.0505677536723,
116.505627142801)) ;
#187927 = CARTESIAN_POINT('Ctrl Pts',(-13.150926931708,-14.0096322945866,
116.566356438622)) ;
#187928 = CARTESIAN_POINT('Ctrl Pts',(-13.1995653491021,-14.2308164989726,
116.74998223283)) ;
#187929 = CARTESIAN_POINT('Ctrl Pts',(-13.2154025368311,-14.1743789457168,
116.798219750367)) ;
#187930 = CARTESIAN_POINT('Ctrl Pts',(-13.1415987048859,-14.1743789796015,
116.822450827003)) ;
#187931 = CARTESIAN_POINT('Ctrl Pts',(-13.0677948729407,-14.1743790134861,
116.846681903639)) ;
#187932 = CARTESIAN_POINT('Ctrl Pts',(-13.0519576852117,-14.2308165667419,
116.798444386103)) ;
#187933 = CARTESIAN_POINT('Ctrl Pts',(-13.0361204974827,-14.2872541199976,
116.750206868567)) ;
#187934 = CARTESIAN_POINT('Ctrl Pts',(-13.1099243294279,-14.287254086113,
116.72597579193)) ;
#187935 = CARTESIAN_POINT('Ctrl Pts',(-13.1837281613731,-14.2872540522283,
116.701744715294)) ;
#187936 = CARTESIAN_POINT('Ctrl Pts',(-13.1995653491021,-14.2308164989726,
116.74998223283)) ;
#187937 = CARTESIAN_POINT('Ctrl Pts',(-13.2646742672153,-14.3939170940553,
116.983896364824)) ;
#187938 = CARTESIAN_POINT('Ctrl Pts',(-13.2752519050489,-14.3260101541607,
117.016114141811)) ;
#187939 = CARTESIAN_POINT('Ctrl Pts',(-13.2014480783073,-14.3260101812409,
117.040345234297)) ;
#187940 = CARTESIAN_POINT('Ctrl Pts',(-13.1276442515657,-14.3260102083211,
117.064576326782)) ;
#187941 = CARTESIAN_POINT('Ctrl Pts',(-13.1170666137321,-14.3939171482158,
117.032358549795)) ;
#187942 = CARTESIAN_POINT('Ctrl Pts',(-13.1064889758985,-14.4618240881105,
117.000140772807)) ;
#187943 = CARTESIAN_POINT('Ctrl Pts',(-13.1802928026401,-14.4618240610302,
116.975909680322)) ;
#187944 = CARTESIAN_POINT('Ctrl Pts',(-13.2540966293817,-14.46182403395,116.951678587836)) ;
#187945 = CARTESIAN_POINT('Ctrl Pts',(-13.2646742672153,-14.3939170940553,
116.983896364824)) ;
#187946 = CARTESIAN_POINT('Ctrl Pts',(-13.3398740457565,-14.4862563732453,
117.248221458507)) ;
#187947 = CARTESIAN_POINT('Ctrl Pts',(-13.3444866220433,-14.411804800515,
117.262270620354)) ;
#187948 = CARTESIAN_POINT('Ctrl Pts',(-13.2706827989801,-14.4118048137988,
117.286501724043)) ;
#187949 = CARTESIAN_POINT('Ctrl Pts',(-13.1968789759169,-14.4118048270827,
117.310732827733)) ;
#187950 = CARTESIAN_POINT('Ctrl Pts',(-13.19226639963,-14.486256399813,117.296683665885)) ;
#187951 = CARTESIAN_POINT('Ctrl Pts',(-13.1876538233431,-14.5607079725433,
117.282634504038)) ;
#187952 = CARTESIAN_POINT('Ctrl Pts',(-13.2614576464064,-14.5607079592595,
117.258403400348)) ;
#187953 = CARTESIAN_POINT('Ctrl Pts',(-13.3352614694696,-14.5607079459756,
117.234172296659)) ;
#187954 = CARTESIAN_POINT('Ctrl Pts',(-13.3398740457565,-14.4862563732453,
117.248221458507)) ;
#187955 = CARTESIAN_POINT('Ctrl Pts',(-13.4203621530711,-14.5025873133897,
117.528986407561)) ;
#187956 = CARTESIAN_POINT('Ctrl Pts',(-13.4186251106891,-14.4268872889833,
117.523695655272)) ;
#187957 = CARTESIAN_POINT('Ctrl Pts',(-13.3448212908417,-14.4268872836565,
117.547926768756)) ;
#187958 = CARTESIAN_POINT('Ctrl Pts',(-13.2710174709942,-14.4268872783298,
117.57215788224)) ;
#187959 = CARTESIAN_POINT('Ctrl Pts',(-13.2727545133762,-14.5025873027362,
117.577448634529)) ;
#187960 = CARTESIAN_POINT('Ctrl Pts',(-13.2744915557582,-14.5782873271426,
117.582739386817)) ;
#187961 = CARTESIAN_POINT('Ctrl Pts',(-13.3482953756057,-14.5782873324694,
117.558508273334)) ;
#187962 = CARTESIAN_POINT('Ctrl Pts',(-13.4220991954531,-14.5782873377961,
117.53427715985)) ;
#187963 = CARTESIAN_POINT('Ctrl Pts',(-13.4203621530711,-14.5025873133897,
117.528986407561)) ;
#187964 = CARTESIAN_POINT('Ctrl Pts',(-13.4982693773669,-14.4415569455837,
117.801564735725)) ;
#187965 = CARTESIAN_POINT('Ctrl Pts',(-13.490360445347,-14.3700086479268,
117.777475403316)) ;
#187966 = CARTESIAN_POINT('Ctrl Pts',(-13.4165566259671,-14.370008620797,
117.801706518224)) ;
#187967 = CARTESIAN_POINT('Ctrl Pts',(-13.3427528065872,-14.3700085936673,
117.825937633132)) ;
#187968 = CARTESIAN_POINT('Ctrl Pts',(-13.3506617386071,-14.4415568913242,
117.850026965541)) ;
#187969 = CARTESIAN_POINT('Ctrl Pts',(-13.358570670627,-14.5131051889812,
117.87411629795)) ;
#187970 = CARTESIAN_POINT('Ctrl Pts',(-13.4323744900069,-14.5131052161109,
117.849885183042)) ;
#187971 = CARTESIAN_POINT('Ctrl Pts',(-13.5061783093868,-14.5131052432407,
117.825654068134)) ;
#187972 = CARTESIAN_POINT('Ctrl Pts',(-13.4982693773669,-14.4415569455837,
117.801564735725)) ;
#187973 = CARTESIAN_POINT('Ctrl Pts',(-13.5687615474577,-14.3059463498269,
118.051984040439)) ;
#187974 = CARTESIAN_POINT('Ctrl Pts',(-13.555180627917,-14.2437611215803,
118.01061874905)) ;
#187975 = CARTESIAN_POINT('Ctrl Pts',(-13.481376807545,-14.2437610699902,
118.034849860937)) ;
#187976 = CARTESIAN_POINT('Ctrl Pts',(-13.4075729871731,-14.2437610184,118.059080972823)) ;
#187977 = CARTESIAN_POINT('Ctrl Pts',(-13.4211539067137,-14.3059462466466,
118.100446264212)) ;
#187978 = CARTESIAN_POINT('Ctrl Pts',(-13.4347348262544,-14.3681314748932,
118.141811555601)) ;
#187979 = CARTESIAN_POINT('Ctrl Pts',(-13.5085386466263,-14.3681315264833,
118.117580443714)) ;
#187980 = CARTESIAN_POINT('Ctrl Pts',(-13.5823424669983,-14.3681315780735,
118.093349331828)) ;
#187981 = CARTESIAN_POINT('Ctrl Pts',(-13.5687615474577,-14.3059463498269,
118.051984040439)) ;
#187982 = CARTESIAN_POINT('Ctrl Pts',(-13.6244542300278,-14.1081523204692,
118.256932053002)) ;
#187983 = CARTESIAN_POINT('Ctrl Pts',(-13.6062345336819,-14.0596861997997,
118.201437795838)) ;
#187984 = CARTESIAN_POINT('Ctrl Pts',(-13.5324307091071,-14.0596861267513,
118.225668894923)) ;
#187985 = CARTESIAN_POINT('Ctrl Pts',(-13.4586268845323,-14.059686053703,
118.249899994008)) ;
#187986 = CARTESIAN_POINT('Ctrl Pts',(-13.4768465808782,-14.1081521743725,
118.305394251172)) ;
#187987 = CARTESIAN_POINT('Ctrl Pts',(-13.495066277224,-14.1566182950421,
118.360888508336)) ;
#187988 = CARTESIAN_POINT('Ctrl Pts',(-13.5688701017988,-14.1566183680904,
118.336657409251)) ;
#187989 = CARTESIAN_POINT('Ctrl Pts',(-13.6426739263736,-14.1566184411388,
118.312426310166)) ;
#187990 = CARTESIAN_POINT('Ctrl Pts',(-13.6244542300278,-14.1081523204692,
118.256932053002)) ;
#187991 = CARTESIAN_POINT('Ctrl Pts',(-13.6616915004186,-13.8605107481474,
118.405813682003)) ;
#187992 = CARTESIAN_POINT('Ctrl Pts',(-13.6401116629726,-13.8292631951763,
118.340084977109)) ;
#187993 = CARTESIAN_POINT('Ctrl Pts',(-13.5663078323218,-13.8292631042665,
118.364316057688)) ;
#187994 = CARTESIAN_POINT('Ctrl Pts',(-13.492504001671,-13.8292630133566,
118.388547138266)) ;
#187995 = CARTESIAN_POINT('Ctrl Pts',(-13.5140838391171,-13.8605105663277,
118.45427584316)) ;
#187996 = CARTESIAN_POINT('Ctrl Pts',(-13.5356636765632,-13.8917581192987,
118.520004548053)) ;
#187997 = CARTESIAN_POINT('Ctrl Pts',(-13.6094675072139,-13.8917582102086,
118.495773467475)) ;
#187998 = CARTESIAN_POINT('Ctrl Pts',(-13.6832713378647,-13.8917583011184,
118.471542386896)) ;
#187999 = CARTESIAN_POINT('Ctrl Pts',(-13.6616915004186,-13.8605107481474,
118.405813682003)) ;
#188000 = CARTESIAN_POINT('Ctrl Pts',(-13.6767027193647,-13.5802159839548,
118.487096599575)) ;
#188001 = CARTESIAN_POINT('Ctrl Pts',(-13.6533073461115,-13.5684914929652,
118.415838065467)) ;
#188002 = CARTESIAN_POINT('Ctrl Pts',(-13.5795035076158,-13.5684913902422,
118.440069122151)) ;
#188003 = CARTESIAN_POINT('Ctrl Pts',(-13.50569966912,-13.5684912875191,118.464300178835)) ;
#188004 = CARTESIAN_POINT('Ctrl Pts',(-13.5290950423732,-13.5802157785087,
118.535558712943)) ;
#188005 = CARTESIAN_POINT('Ctrl Pts',(-13.5524904156264,-13.5919402694983,
118.606817247052)) ;
#188006 = CARTESIAN_POINT('Ctrl Pts',(-13.6262942541222,-13.5919403722214,
118.582586190367)) ;
#188007 = CARTESIAN_POINT('Ctrl Pts',(-13.700098092618,-13.5919404749444,
118.558355133683)) ;
#188008 = CARTESIAN_POINT('Ctrl Pts',(-13.6767027193647,-13.5802159839548,
118.487096599575)) ;
#188009 = CARTESIAN_POINT('Ctrl Pts',(-13.6675174437681,-13.2888355614903,
118.494615718162)) ;
#188010 = CARTESIAN_POINT('Ctrl Pts',(-13.643994456241,-13.2974368879024,
118.422968491516)) ;
#188011 = CARTESIAN_POINT('Ctrl Pts',(-13.5701906089222,-13.2974367821204,
118.447199521326)) ;
#188012 = CARTESIAN_POINT('Ctrl Pts',(-13.4963867616034,-13.2974366763383,
118.471430551137)) ;
#188013 = CARTESIAN_POINT('Ctrl Pts',(-13.5199097491305,-13.2888353499262,
118.543077777783)) ;
#188014 = CARTESIAN_POINT('Ctrl Pts',(-13.5434327366576,-13.2802340235141,
118.61472500443)) ;
#188015 = CARTESIAN_POINT('Ctrl Pts',(-13.6172365839764,-13.2802341292962,
118.590493974619)) ;
#188016 = CARTESIAN_POINT('Ctrl Pts',(-13.6910404312952,-13.2802342350782,
118.566262944809)) ;
#188017 = CARTESIAN_POINT('Ctrl Pts',(-13.6675174437681,-13.2888355614903,
118.494615718162)) ;
#188018 = CARTESIAN_POINT('Ctrl Pts',(-13.6345263965788,-13.0084923611293,
118.429389220724)) ;
#188019 = CARTESIAN_POINT('Ctrl Pts',(-13.6125426984709,-13.0366789477102,
118.362430421261)) ;
#188020 = CARTESIAN_POINT('Ctrl Pts',(-13.5387388424139,-13.0366788478173,
118.386661424456)) ;
#188021 = CARTESIAN_POINT('Ctrl Pts',(-13.4649349863569,-13.0366787479245,
118.410892427651)) ;
#188022 = CARTESIAN_POINT('Ctrl Pts',(-13.4869186844647,-13.0084921613435,
118.477851227115)) ;
#188023 = CARTESIAN_POINT('Ctrl Pts',(-13.5089023825726,-12.9803055747626,
118.544810026578)) ;
#188024 = CARTESIAN_POINT('Ctrl Pts',(-13.5827062386296,-12.9803056746555,
118.520579023383)) ;
#188025 = CARTESIAN_POINT('Ctrl Pts',(-13.6565100946866,-12.9803057745484,
118.496348020188)) ;
#188026 = CARTESIAN_POINT('Ctrl Pts',(-13.6345263965788,-13.0084923611293,
118.429389220724)) ;
#188027 = CARTESIAN_POINT('Ctrl Pts',(-13.578743439224,-12.7552927085919,
118.295029267959)) ;
#188028 = CARTESIAN_POINT('Ctrl Pts',(-13.5598862064938,-12.8011984065865,
118.237593177571)) ;
#188029 = CARTESIAN_POINT('Ctrl Pts',(-13.4860823424701,-12.8011983205869,
118.261824156501)) ;
#188030 = CARTESIAN_POINT('Ctrl Pts',(-13.4122784784464,-12.8011982345872,
118.286055135431)) ;
#188031 = CARTESIAN_POINT('Ctrl Pts',(-13.4311357111765,-12.7552925365926,
118.343491225819)) ;
#188032 = CARTESIAN_POINT('Ctrl Pts',(-13.4499929439066,-12.709386838598,
118.400927316208)) ;
#188033 = CARTESIAN_POINT('Ctrl Pts',(-13.5237968079303,-12.7093869245976,
118.376696337278)) ;
#188034 = CARTESIAN_POINT('Ctrl Pts',(-13.5976006719541,-12.7093870105973,
118.352465358348)) ;
#188035 = CARTESIAN_POINT('Ctrl Pts',(-13.578743439224,-12.7552927085919,
118.295029267959)) ;
#188036 = CARTESIAN_POINT('Ctrl Pts',(-13.5039282764506,-12.5504983058309,
118.102546163647)) ;
#188037 = CARTESIAN_POINT('Ctrl Pts',(-13.489534151706,-12.6107700146374,
118.058703980073)) ;
#188038 = CARTESIAN_POINT('Ctrl Pts',(-13.4157302814213,-12.6107699496328,
118.082934939933)) ;
#188039 = CARTESIAN_POINT('Ctrl Pts',(-13.3419264111365,-12.6107698846282,
118.107165899793)) ;
#188040 = CARTESIAN_POINT('Ctrl Pts',(-13.3563205358811,-12.5504981758217,
118.151008083367)) ;
#188041 = CARTESIAN_POINT('Ctrl Pts',(-13.3707146606257,-12.4902264670152,
118.194850266941)) ;
#188042 = CARTESIAN_POINT('Ctrl Pts',(-13.4445185309104,-12.4902265320198,
118.170619307082)) ;
#188043 = CARTESIAN_POINT('Ctrl Pts',(-13.5183224011952,-12.4902265970244,
118.146388347222)) ;
#188044 = CARTESIAN_POINT('Ctrl Pts',(-13.5039282764506,-12.5504983058309,
118.102546163647)) ;
#188045 = CARTESIAN_POINT('Ctrl Pts',(-13.4139738325163,-12.4070470358761,
117.864151582069)) ;
#188046 = CARTESIAN_POINT('Ctrl Pts',(-13.4051020323662,-12.477423987992,
117.837129508225)) ;
#188047 = CARTESIAN_POINT('Ctrl Pts',(-13.3312981582326,-12.4774239490789,
117.861360456362)) ;
#188048 = CARTESIAN_POINT('Ctrl Pts',(-13.2574942840989,-12.4774239101657,
117.885591404498)) ;
#188049 = CARTESIAN_POINT('Ctrl Pts',(-13.266366084249,-12.4070469580498,
117.912613478343)) ;
#188050 = CARTESIAN_POINT('Ctrl Pts',(-13.2752378843991,-12.336670005934,
117.939635552187)) ;
#188051 = CARTESIAN_POINT('Ctrl Pts',(-13.3490417585328,-12.3366700448471,
117.91540460405)) ;
#188052 = CARTESIAN_POINT('Ctrl Pts',(-13.4228456326664,-12.3366700837602,
117.891173655913)) ;
#188053 = CARTESIAN_POINT('Ctrl Pts',(-13.4139738325163,-12.4070470358761,
117.864151582069)) ;
#188054 = CARTESIAN_POINT('Ctrl Pts',(-13.3156962558462,-12.336806735375,
117.60014657944)) ;
#188055 = CARTESIAN_POINT('Ctrl Pts',(-13.3129416529795,-12.4121923869935,
117.591756501563)) ;
#188056 = CARTESIAN_POINT('Ctrl Pts',(-13.2391377775031,-12.4121923758419,
117.61598744561)) ;
#188057 = CARTESIAN_POINT('Ctrl Pts',(-13.1653339020268,-12.4121923646903,
117.640218389657)) ;
#188058 = CARTESIAN_POINT('Ctrl Pts',(-13.1680885048935,-12.3368067130718,
117.648608467534)) ;
#188059 = CARTESIAN_POINT('Ctrl Pts',(-13.1708431077602,-12.2614210614532,
117.656998545411)) ;
#188060 = CARTESIAN_POINT('Ctrl Pts',(-13.2446469832366,-12.2614210726048,
117.632767601364)) ;
#188061 = CARTESIAN_POINT('Ctrl Pts',(-13.3184508587129,-12.2614210837564,
117.608536657317)) ;
#188062 = CARTESIAN_POINT('Ctrl Pts',(-13.3156962558462,-12.336806735375,
117.60014657944)) ;
#188063 = CARTESIAN_POINT('Ctrl Pts',(-13.2143094352689,-12.343454815208,
117.326830151226)) ;
#188064 = CARTESIAN_POINT('Ctrl Pts',(-13.2178948502753,-12.4184892364302,
117.337750744908)) ;
#188065 = CARTESIAN_POINT('Ctrl Pts',(-13.1440909762376,-12.4184892524871,
117.361981693338)) ;
#188066 = CARTESIAN_POINT('Ctrl Pts',(-13.0702871022,-12.418489268544,117.386212641767)) ;
#188067 = CARTESIAN_POINT('Ctrl Pts',(-13.0667016871936,-12.3434548473218,
117.375292048084)) ;
#188068 = CARTESIAN_POINT('Ctrl Pts',(-13.0631162721871,-12.2684204260996,
117.364371454402)) ;
#188069 = CARTESIAN_POINT('Ctrl Pts',(-13.1369201462248,-12.2684204100427,
117.340140505973)) ;
#188070 = CARTESIAN_POINT('Ctrl Pts',(-13.2107240202625,-12.2684203939858,
117.315909557544)) ;
#188071 = CARTESIAN_POINT('Ctrl Pts',(-13.2143094352689,-12.343454815208,
117.326830151226)) ;
#188072 = CARTESIAN_POINT('Ctrl Pts',(-13.1166976808709,-12.4274004694333,
117.065026003125)) ;
#188073 = CARTESIAN_POINT('Ctrl Pts',(-13.1263688309921,-12.4966868092395,
117.094482764137)) ;
#188074 = CARTESIAN_POINT('Ctrl Pts',(-13.052564960866,-12.4966868487172,
117.11871372448)) ;
#188075 = CARTESIAN_POINT('Ctrl Pts',(-12.9787610907399,-12.496686888195,
117.142944684823)) ;
#188076 = CARTESIAN_POINT('Ctrl Pts',(-12.9690899406187,-12.4274005483888,
117.113487923811)) ;
#188077 = CARTESIAN_POINT('Ctrl Pts',(-12.9594187904974,-12.3581142085826,
117.084031162799)) ;
#188078 = CARTESIAN_POINT('Ctrl Pts',(-13.0332226606235,-12.3581141691049,
117.059800202456)) ;
#188079 = CARTESIAN_POINT('Ctrl Pts',(-13.1070265307496,-12.3581141296271,
117.035569242112)) ;
#188080 = CARTESIAN_POINT('Ctrl Pts',(-13.1166976808709,-12.4274004694333,
117.065026003125)) ;
#188081 = CARTESIAN_POINT('Ctrl Pts',(-13.029296249753,-12.5821548538746,
116.83426577371)) ;
#188082 = CARTESIAN_POINT('Ctrl Pts',(-13.0443506263033,-12.6407407748519,
116.880118973957)) ;
#188083 = CARTESIAN_POINT('Ctrl Pts',(-12.9705467617918,-12.6407408319528,
116.904349951401)) ;
#188084 = CARTESIAN_POINT('Ctrl Pts',(-12.8967428972803,-12.6407408890538,
116.928580928845)) ;
#188085 = CARTESIAN_POINT('Ctrl Pts',(-12.88168852073,-12.5821549680765,116.882727728599)) ;
#188086 = CARTESIAN_POINT('Ctrl Pts',(-12.8666341441797,-12.5235690470992,
116.836874528352)) ;
#188087 = CARTESIAN_POINT('Ctrl Pts',(-12.9404380086912,-12.5235689899983,
116.812643550908)) ;
#188088 = CARTESIAN_POINT('Ctrl Pts',(-13.0142418732027,-12.5235689328973,
116.788412573463)) ;
#188089 = CARTESIAN_POINT('Ctrl Pts',(-13.029296249753,-12.5821548538746,
116.83426577371)) ;
#188090 = CARTESIAN_POINT('Ctrl Pts',(-12.957469185764,-12.7965584285917,
116.650922402553)) ;
#188091 = CARTESIAN_POINT('Ctrl Pts',(-12.9768279961232,-12.8402632676504,
116.709886213787)) ;
#188092 = CARTESIAN_POINT('Ctrl Pts',(-12.903024138244,-12.8402633354297,
116.734117211432)) ;
#188093 = CARTESIAN_POINT('Ctrl Pts',(-12.8292202803647,-12.8402634032089,
116.758348209077)) ;
#188094 = CARTESIAN_POINT('Ctrl Pts',(-12.8098614700054,-12.7965585641502,
116.699384397843)) ;
#188095 = CARTESIAN_POINT('Ctrl Pts',(-12.7905026596461,-12.7528537250914,
116.640420586608)) ;
#188096 = CARTESIAN_POINT('Ctrl Pts',(-12.8643065175254,-12.7528536573122,
116.616189588963)) ;
#188097 = CARTESIAN_POINT('Ctrl Pts',(-12.9381103754047,-12.752853589533,
116.591958591318)) ;
#188098 = CARTESIAN_POINT('Ctrl Pts',(-12.957469185764,-12.7965584285917,
116.650922402553)) ;
#188099 = CARTESIAN_POINT('Ctrl Pts',(-12.9054874508914,-13.0557769277784,
116.528074736688)) ;
#188100 = CARTESIAN_POINT('Ctrl Pts',(-12.9277706871717,-13.0814494476449,
116.595945877568)) ;
#188101 = CARTESIAN_POINT('Ctrl Pts',(-12.8539668362307,-13.0814495182785,
116.620176896346)) ;
#188102 = CARTESIAN_POINT('Ctrl Pts',(-12.7801629852898,-13.0814495889122,
116.644407915124)) ;
#188103 = CARTESIAN_POINT('Ctrl Pts',(-12.7578797490096,-13.0557770690457,
116.576536774244)) ;
#188104 = CARTESIAN_POINT('Ctrl Pts',(-12.7355965127293,-13.0301045491793,
116.508665633364)) ;
#188105 = CARTESIAN_POINT('Ctrl Pts',(-12.8094003636702,-13.0301044785456,
116.484434614586)) ;
#188106 = CARTESIAN_POINT('Ctrl Pts',(-12.8832042146112,-13.030104407912,
116.460203595808)) ;
#188107 = CARTESIAN_POINT('Ctrl Pts',(-12.9054874508914,-13.0557769277784,
116.528074736688)) ;
#188108 = CARTESIAN_POINT('Ctrl Pts',(-12.8764554614161,-13.3412469909538,
116.475159277175)) ;
#188109 = CARTESIAN_POINT('Ctrl Pts',(-12.9000646743804,-13.3470269436932,
116.547069129252)) ;
#188110 = CARTESIAN_POINT('Ctrl Pts',(-12.826260829751,-13.3470270098198,
116.571300167254)) ;
#188111 = CARTESIAN_POINT('Ctrl Pts',(-12.7524569851216,-13.3470270759464,
116.595531205256)) ;
#188112 = CARTESIAN_POINT('Ctrl Pts',(-12.7288477721572,-13.341247123207,
116.523621353179)) ;
#188113 = CARTESIAN_POINT('Ctrl Pts',(-12.7052385591928,-13.3354671704675,
116.451711501102)) ;
#188114 = CARTESIAN_POINT('Ctrl Pts',(-12.7790424038223,-13.335467104341,
116.4274804631)) ;
#188115 = CARTESIAN_POINT('Ctrl Pts',(-12.8528462484517,-13.3354670382144,
116.403249425098)) ;
#188116 = CARTESIAN_POINT('Ctrl Pts',(-12.8764554614161,-13.3412469909538,
116.475159277175)) ;
#188117 = CARTESIAN_POINT('Ctrl Pts',(-12.8717225081288,-13.6316256256215,
116.496181890224)) ;
#188118 = CARTESIAN_POINT('Ctrl Pts',(-12.8949646242832,-13.6171399155478,
116.566973624807)) ;
#188119 = CARTESIAN_POINT('Ctrl Pts',(-12.8211607846619,-13.6171399723523,
116.591204678062)) ;
#188120 = CARTESIAN_POINT('Ctrl Pts',(-12.7473569450405,-13.6171400291567,
116.615435731318)) ;
#188121 = CARTESIAN_POINT('Ctrl Pts',(-12.7241148288861,-13.6316257392305,
116.544643996736)) ;
#188122 = CARTESIAN_POINT('Ctrl Pts',(-12.7008727127316,-13.6461114493042,
116.473852262154)) ;
#188123 = CARTESIAN_POINT('Ctrl Pts',(-12.7746765523529,-13.6461113924997,
116.449621208898)) ;
#188124 = CARTESIAN_POINT('Ctrl Pts',(-12.8484803919743,-13.6461113356952,
116.425390155642)) ;
#188125 = CARTESIAN_POINT('Ctrl Pts',(-12.8717225081288,-13.6316256256215,
116.496181890224)) ;
#188126 = CARTESIAN_POINT('Ctrl Pts',(-12.8907909191923,-13.9070076933881,
116.589733690393)) ;
#188127 = CARTESIAN_POINT('Ctrl Pts',(-12.9120028931781,-13.8732725053054,
116.65434193966)) ;
#188128 = CARTESIAN_POINT('Ctrl Pts',(-12.8381990569256,-13.8732725490148,
116.678573003177)) ;
#188129 = CARTESIAN_POINT('Ctrl Pts',(-12.7643952206731,-13.8732725927241,
116.702804066694)) ;
#188130 = CARTESIAN_POINT('Ctrl Pts',(-12.7431832466874,-13.9070077808067,
116.638195817426)) ;
#188131 = CARTESIAN_POINT('Ctrl Pts',(-12.7219712727016,-13.9407429688894,
116.573587568159)) ;
#188132 = CARTESIAN_POINT('Ctrl Pts',(-12.7957751089541,-13.9407429251801,
116.549356504642)) ;
#188133 = CARTESIAN_POINT('Ctrl Pts',(-12.8695789452066,-13.9407428814708,
116.525125441125)) ;
#188134 = CARTESIAN_POINT('Ctrl Pts',(-12.8907909191923,-13.9070076933881,
116.589733690393)) ;
#188135 = CARTESIAN_POINT('Ctrl Pts',(-12.9317044536525,-14.1476875757229,
116.749883763998)) ;
#188136 = CARTESIAN_POINT('Ctrl Pts',(-12.94935668604,-14.0970962848469,116.803649614901)) ;
#188137 = CARTESIAN_POINT('Ctrl Pts',(-12.8755528511703,-14.0970963139386,
116.82788068263)) ;
#188138 = CARTESIAN_POINT('Ctrl Pts',(-12.8017490163005,-14.0970963430303,
116.852111750358)) ;
#188139 = CARTESIAN_POINT('Ctrl Pts',(-12.7840967839129,-14.1476876339063,
116.798345899455)) ;
#188140 = CARTESIAN_POINT('Ctrl Pts',(-12.7664445515254,-14.1982789247823,
116.744580048552)) ;
#188141 = CARTESIAN_POINT('Ctrl Pts',(-12.8402483863952,-14.1982788956906,
116.720348980823)) ;
#188142 = CARTESIAN_POINT('Ctrl Pts',(-12.9140522212649,-14.1982788665989,
116.696117913095)) ;
#188143 = CARTESIAN_POINT('Ctrl Pts',(-12.9317044536525,-14.1476875757229,
116.749883763998)) ;
#188144 = CARTESIAN_POINT('Ctrl Pts',(-12.9904518256849,-14.3351652655006,
116.964206833377)) ;
#188145 = CARTESIAN_POINT('Ctrl Pts',(-13.0032965612653,-14.2714071859544,
117.003329824843)) ;
#188146 = CARTESIAN_POINT('Ctrl Pts',(-12.9294927264181,-14.2714072026928,
117.02756089264)) ;
#188147 = CARTESIAN_POINT('Ctrl Pts',(-12.8556888915708,-14.2714072194312,
117.051791960437)) ;
#188148 = CARTESIAN_POINT('Ctrl Pts',(-12.8428441559903,-14.3351652989775,
117.012668968971)) ;
#188149 = CARTESIAN_POINT('Ctrl Pts',(-12.8299994204098,-14.3989233785238,
116.973545977504)) ;
#188150 = CARTESIAN_POINT('Ctrl Pts',(-12.9038032552571,-14.3989233617854,
116.949314909707)) ;
#188151 = CARTESIAN_POINT('Ctrl Pts',(-12.9776070901044,-14.3989233450469,
116.92508384191)) ;
#188152 = CARTESIAN_POINT('Ctrl Pts',(-12.9904518256849,-14.3351652655006,
116.964206833377)) ;
#188153 = CARTESIAN_POINT('Ctrl Pts',(-13.0621987371074,-14.4575099619995,
117.218132519493)) ;
#188154 = CARTESIAN_POINT('Ctrl Pts',(-13.0693208431459,-14.3851129420045,
117.239825304866)) ;
#188155 = CARTESIAN_POINT('Ctrl Pts',(-12.9955170071031,-14.38511294846,117.264056369021)) ;
#188156 = CARTESIAN_POINT('Ctrl Pts',(-12.9217131710604,-14.3851129549154,
117.288287433177)) ;
#188157 = CARTESIAN_POINT('Ctrl Pts',(-12.9145910650219,-14.4575099749105,
117.266594647805)) ;
#188158 = CARTESIAN_POINT('Ctrl Pts',(-12.9074689589835,-14.5299069949055,
117.244901862432)) ;
#188159 = CARTESIAN_POINT('Ctrl Pts',(-12.9812727950263,-14.52990698845,117.220670798277)) ;
#188160 = CARTESIAN_POINT('Ctrl Pts',(-13.055076631069,-14.5299069819946,
117.196439734121)) ;
#188161 = CARTESIAN_POINT('Ctrl Pts',(-13.0621987371074,-14.4575099619995,
117.218132519493)) ;
#188162 = CARTESIAN_POINT('Ctrl Pts',(-13.1416934201426,-14.5055206620573,
117.495908283019)) ;
#188163 = CARTESIAN_POINT('Ctrl Pts',(-13.1425378898428,-14.4296611949973,
117.498480401175)) ;
#188164 = CARTESIAN_POINT('Ctrl Pts',(-13.0687340512145,-14.4296611947843,
117.522711457456)) ;
#188165 = CARTESIAN_POINT('Ctrl Pts',(-12.9949302125861,-14.4296611945714,
117.546942513736)) ;
#188166 = CARTESIAN_POINT('Ctrl Pts',(-12.9940857428859,-14.5055206616315,
117.54437039558)) ;
#188167 = CARTESIAN_POINT('Ctrl Pts',(-12.9932412731857,-14.5813801286916,
117.541798277423)) ;
#188168 = CARTESIAN_POINT('Ctrl Pts',(-13.067045111814,-14.5813801289045,
117.517567221143)) ;
#188169 = CARTESIAN_POINT('Ctrl Pts',(-13.1408489504423,-14.5813801291174,
117.493336164862)) ;
#188170 = CARTESIAN_POINT('Ctrl Pts',(-13.1416934201426,-14.5055206620573,
117.495908283019)) ;
#188171 = CARTESIAN_POINT('Ctrl Pts',(-13.2212073264965,-14.4754288487564,
117.773416266333)) ;
#188172 = CARTESIAN_POINT('Ctrl Pts',(-13.2157700751089,-14.4015565166022,
117.756855275716)) ;
#188173 = CARTESIAN_POINT('Ctrl Pts',(-13.1419662346049,-14.4015565138437,
117.781086326283)) ;
#188174 = CARTESIAN_POINT('Ctrl Pts',(-13.0681623941008,-14.4015565110851,
117.805317376851)) ;
#188175 = CARTESIAN_POINT('Ctrl Pts',(-13.0735996454884,-14.4754288432393,
117.821878367468)) ;
#188176 = CARTESIAN_POINT('Ctrl Pts',(-13.0790368968761,-14.5493011753935,
117.838439358085)) ;
#188177 = CARTESIAN_POINT('Ctrl Pts',(-13.1528407373801,-14.5493011781521,
117.814208307518)) ;
#188178 = CARTESIAN_POINT('Ctrl Pts',(-13.2266445778842,-14.5493011809106,
117.78997725695)) ;
#188179 = CARTESIAN_POINT('Ctrl Pts',(-13.2212073264965,-14.4754288487564,
117.773416266333)) ;
#188180 = CARTESIAN_POINT('Ctrl Pts',(-13.2954245315983,-14.3696969300058,
118.034975562768)) ;
#188181 = CARTESIAN_POINT('Ctrl Pts',(-13.2840619904211,-14.3030961668257,
118.00036709561)) ;
#188182 = CARTESIAN_POINT('Ctrl Pts',(-13.2102581479488,-14.3030961645972,
118.024598140183)) ;
#188183 = CARTESIAN_POINT('Ctrl Pts',(-13.1364543054765,-14.3030961623686,
118.048829184755)) ;
#188184 = CARTESIAN_POINT('Ctrl Pts',(-13.1478168466536,-14.3696969255486,
118.083437651913)) ;
#188185 = CARTESIAN_POINT('Ctrl Pts',(-13.1591793878308,-14.4362976887287,
118.118046119071)) ;
#188186 = CARTESIAN_POINT('Ctrl Pts',(-13.2329832303031,-14.4362976909572,
118.093815074498)) ;
#188187 = CARTESIAN_POINT('Ctrl Pts',(-13.3067870727754,-14.4362976931858,
118.069584029926)) ;
#188188 = CARTESIAN_POINT('Ctrl Pts',(-13.2954245315983,-14.3696969300058,
118.034975562768)) ;
#188189 = CARTESIAN_POINT('Ctrl Pts',(-13.3577857668099,-14.1954536297215,
118.260415901486)) ;
#188190 = CARTESIAN_POINT('Ctrl Pts',(-13.3413169958214,-14.1409200386093,
118.210254682291)) ;
#188191 = CARTESIAN_POINT('Ctrl Pts',(-13.2675131522284,-14.1409200387787,
118.23448572345)) ;
#188192 = CARTESIAN_POINT('Ctrl Pts',(-13.1937093086354,-14.1409200389481,
118.258716764609)) ;
#188193 = CARTESIAN_POINT('Ctrl Pts',(-13.2101780796239,-14.1954536300603,
118.308877983803)) ;
#188194 = CARTESIAN_POINT('Ctrl Pts',(-13.2266468506125,-14.2499872211724,
118.359039202998)) ;
#188195 = CARTESIAN_POINT('Ctrl Pts',(-13.3004506942055,-14.249987221003,
118.334808161839)) ;
#188196 = CARTESIAN_POINT('Ctrl Pts',(-13.3742545377985,-14.2499872208336,
118.31057712068)) ;
#188197 = CARTESIAN_POINT('Ctrl Pts',(-13.3577857668099,-14.1954536297215,
118.260415901486)) ;
#188198 = CARTESIAN_POINT('Ctrl Pts',(-13.4030472404078,-13.9663067477415,
118.433665970609)) ;
#188199 = CARTESIAN_POINT('Ctrl Pts',(-13.3826610350393,-13.9276927071092,
118.371572878415)) ;
#188200 = CARTESIAN_POINT('Ctrl Pts',(-13.308857191142,-13.9276927095559,
118.395803918647)) ;
#188201 = CARTESIAN_POINT('Ctrl Pts',(-13.2350533472446,-13.9276927120025,
118.420034958879)) ;
#188202 = CARTESIAN_POINT('Ctrl Pts',(-13.255439552613,-13.9663067526349,
118.482128051073)) ;
#188203 = CARTESIAN_POINT('Ctrl Pts',(-13.2758257579814,-14.0049207932672,
118.544221143267)) ;
#188204 = CARTESIAN_POINT('Ctrl Pts',(-13.3496296018788,-14.0049207908205,
118.519990103035)) ;
#188205 = CARTESIAN_POINT('Ctrl Pts',(-13.4234334457761,-14.0049207883739,
118.495759062804)) ;
#188206 = CARTESIAN_POINT('Ctrl Pts',(-13.4030472404078,-13.9663067477415,
118.433665970609)) ;
#188207 = CARTESIAN_POINT('Ctrl Pts',(-13.4274257673163,-13.6964880977043,
118.543501361886)) ;
#188208 = CARTESIAN_POINT('Ctrl Pts',(-13.4045704519705,-13.6766583743927,
118.473887759096)) ;
#188209 = CARTESIAN_POINT('Ctrl Pts',(-13.3307666083207,-13.6766583775101,
118.498118800081)) ;
#188210 = CARTESIAN_POINT('Ctrl Pts',(-13.2569627646708,-13.6766583806274,
118.522349841067)) ;
#188211 = CARTESIAN_POINT('Ctrl Pts',(-13.2798180800167,-13.696488103939,
118.591963443857)) ;
#188212 = CARTESIAN_POINT('Ctrl Pts',(-13.3026733953625,-13.7163178272505,
118.661577046648)) ;
#188213 = CARTESIAN_POINT('Ctrl Pts',(-13.3764772390123,-13.7163178241332,
118.637346005662)) ;
#188214 = CARTESIAN_POINT('Ctrl Pts',(-13.4502810826622,-13.7163178210159,
118.613114964676)) ;
#188215 = CARTESIAN_POINT('Ctrl Pts',(-13.4274257673163,-13.6964880977043,
118.543501361886)) ;
#188216 = CARTESIAN_POINT('Ctrl Pts',(-13.4282463775527,-13.4086720240795,
118.581326099254)) ;
#188217 = CARTESIAN_POINT('Ctrl Pts',(-13.4045691840501,-13.4089104896533,
118.509209188176)) ;
#188218 = CARTESIAN_POINT('Ctrl Pts',(-13.3307653407294,-13.4089104912241,
118.533440230164)) ;
#188219 = CARTESIAN_POINT('Ctrl Pts',(-13.2569614974086,-13.408910492795,
118.557671272153)) ;
#188220 = CARTESIAN_POINT('Ctrl Pts',(-13.2806386909112,-13.4086720272212,
118.62978818323)) ;
#188221 = CARTESIAN_POINT('Ctrl Pts',(-13.3043158844138,-13.4084335616475,
118.701905094307)) ;
#188222 = CARTESIAN_POINT('Ctrl Pts',(-13.3781197277346,-13.4084335600766,
118.677674052319)) ;
#188223 = CARTESIAN_POINT('Ctrl Pts',(-13.4519235710553,-13.4084335585058,
118.653443010331)) ;
#188224 = CARTESIAN_POINT('Ctrl Pts',(-13.4282463775527,-13.4086720240795,
118.581326099254)) ;
#188225 = CARTESIAN_POINT('Ctrl Pts',(-13.4047342363666,-13.1198463580562,
118.545258189768)) ;
#188226 = CARTESIAN_POINT('Ctrl Pts',(-13.3819284192765,-13.1402531049797,
118.475795350571)) ;
#188227 = CARTESIAN_POINT('Ctrl Pts',(-13.3081245757733,-13.1402531026116,
118.500026392003)) ;
#188228 = CARTESIAN_POINT('Ctrl Pts',(-13.2343207322702,-13.1402531002435,
118.524257433436)) ;
#188229 = CARTESIAN_POINT('Ctrl Pts',(-13.2571265493602,-13.1198463533199,
118.593720272633)) ;
#188230 = CARTESIAN_POINT('Ctrl Pts',(-13.2799323664503,-13.0994396063964,
118.663183111831)) ;
#188231 = CARTESIAN_POINT('Ctrl Pts',(-13.3537362099535,-13.0994396087645,
118.638952070398)) ;
#188232 = CARTESIAN_POINT('Ctrl Pts',(-13.4275400534566,-13.0994396111326,
118.614721028966)) ;
#188233 = CARTESIAN_POINT('Ctrl Pts',(-13.4047342363666,-13.1198463580562,
118.545258189768)) ;
#188234 = CARTESIAN_POINT('Ctrl Pts',(-13.3580365344568,-12.8536440540051,
118.438389162205)) ;
#188235 = CARTESIAN_POINT('Ctrl Pts',(-13.3377263303549,-12.8926679376459,
118.376527557416)) ;
#188236 = CARTESIAN_POINT('Ctrl Pts',(-13.2639224859729,-12.8926679313973,
118.400758596172)) ;
#188237 = CARTESIAN_POINT('Ctrl Pts',(-13.1901186415909,-12.8926679251486,
118.424989634928)) ;
#188238 = CARTESIAN_POINT('Ctrl Pts',(-13.2104288456928,-12.8536440415079,
118.486851239717)) ;
#188239 = CARTESIAN_POINT('Ctrl Pts',(-13.2307390497946,-12.8146201578671,
118.548712844506)) ;
#188240 = CARTESIAN_POINT('Ctrl Pts',(-13.3045428941766,-12.8146201641158,
118.52448180575)) ;
#188241 = CARTESIAN_POINT('Ctrl Pts',(-13.3783467385586,-12.8146201703644,
118.500250766995)) ;
#188242 = CARTESIAN_POINT('Ctrl Pts',(-13.3580365344568,-12.8536440540051,
118.438389162205)) ;
#188243 = CARTESIAN_POINT('Ctrl Pts',(-13.2900338474699,-12.6260691585523,
118.266921417924)) ;
#188244 = CARTESIAN_POINT('Ctrl Pts',(-13.2737043319057,-12.6810405314409,
118.217184347987)) ;
#188245 = CARTESIAN_POINT('Ctrl Pts',(-13.19990048528,-12.6810405208292,118.241415379908)) ;
#188246 = CARTESIAN_POINT('Ctrl Pts',(-13.1260966386543,-12.6810405102175,
118.26564641183)) ;
#188247 = CARTESIAN_POINT('Ctrl Pts',(-13.1424261542185,-12.6260691373289,
118.315383481767)) ;
#188248 = CARTESIAN_POINT('Ctrl Pts',(-13.1587556697827,-12.5710977644403,
118.365120551704)) ;
#188249 = CARTESIAN_POINT('Ctrl Pts',(-13.2325595164084,-12.571097775052,
118.340889519783)) ;
#188250 = CARTESIAN_POINT('Ctrl Pts',(-13.3063633630341,-12.5710977856637,
118.316658487861)) ;
#188251 = CARTESIAN_POINT('Ctrl Pts',(-13.2900338474699,-12.6260691585523,
118.266921417924)) ;
#188252 = CARTESIAN_POINT('Ctrl Pts',(-13.2058856946641,-12.4569456938658,
118.045990431136)) ;
#188253 = CARTESIAN_POINT('Ctrl Pts',(-13.1946760329366,-12.5238051277268,
118.01184760977)) ;
#188254 = CARTESIAN_POINT('Ctrl Pts',(-13.1208721836935,-12.5238051170314,
118.03607863372)) ;
#188255 = CARTESIAN_POINT('Ctrl Pts',(-13.0470683344505,-12.523805106336,
118.06030965767)) ;
#188256 = CARTESIAN_POINT('Ctrl Pts',(-13.058277996178,-12.4569456724751,
118.094452479035)) ;
#188257 = CARTESIAN_POINT('Ctrl Pts',(-13.0694876579055,-12.3900862386142,
118.128595300401)) ;
#188258 = CARTESIAN_POINT('Ctrl Pts',(-13.1432915071485,-12.3900862493095,
118.104364276451)) ;
#188259 = CARTESIAN_POINT('Ctrl Pts',(-13.2170953563916,-12.3900862600049,
118.080133252501)) ;
#188260 = CARTESIAN_POINT('Ctrl Pts',(-13.2058856946641,-12.4569456938658,
118.045990431136)) ;
#188261 = CARTESIAN_POINT('Ctrl Pts',(-13.1099984077294,-12.3560371763605,
117.789461557574)) ;
#188262 = CARTESIAN_POINT('Ctrl Pts',(-13.1047323153025,-12.4300391766208,
117.773421889139)) ;
#188263 = CARTESIAN_POINT('Ctrl Pts',(-13.0309284627601,-12.43003916942,117.79765290304)) ;
#188264 = CARTESIAN_POINT('Ctrl Pts',(-12.9571246102177,-12.4300391622191,
117.82188391694)) ;
#188265 = CARTESIAN_POINT('Ctrl Pts',(-12.9623907026446,-12.3560371619588,
117.837923585375)) ;
#188266 = CARTESIAN_POINT('Ctrl Pts',(-12.9676567950715,-12.2820351616984,
117.853963253809)) ;
#188267 = CARTESIAN_POINT('Ctrl Pts',(-13.0414606476139,-12.2820351688993,
117.829732239909)) ;
#188268 = CARTESIAN_POINT('Ctrl Pts',(-13.1152645001563,-12.2820351761001,
117.805501226008)) ;
#188269 = CARTESIAN_POINT('Ctrl Pts',(-13.1099984077294,-12.3560371763605,
117.789461557574)) ;
#188270 = CARTESIAN_POINT('Ctrl Pts',(-13.0093871644828,-12.3312869891021,
117.518335932488)) ;
#188271 = CARTESIAN_POINT('Ctrl Pts',(-13.0104073119892,-12.407123602134,
117.521443136472)) ;
#188272 = CARTESIAN_POINT('Ctrl Pts',(-12.9366034569471,-12.4071236031691,
117.545674142759)) ;
#188273 = CARTESIAN_POINT('Ctrl Pts',(-12.862799601905,-12.4071236042042,
117.569905149046)) ;
#188274 = CARTESIAN_POINT('Ctrl Pts',(-12.8617794543986,-12.3312869911723,
117.566797945062)) ;
#188275 = CARTESIAN_POINT('Ctrl Pts',(-12.8607593068922,-12.2554503781403,
117.563690741078)) ;
#188276 = CARTESIAN_POINT('Ctrl Pts',(-12.9345631619343,-12.2554503771052,
117.539459734791)) ;
#188277 = CARTESIAN_POINT('Ctrl Pts',(-13.0083670169764,-12.2554503760701,
117.515228728505)) ;
#188278 = CARTESIAN_POINT('Ctrl Pts',(-13.0093871644828,-12.3312869891021,
117.518335932488)) ;
#188279 = CARTESIAN_POINT('Ctrl Pts',(-12.9090497943827,-12.384579728798,
117.248374706076)) ;
#188280 = CARTESIAN_POINT('Ctrl Pts',(-12.916339277386,-12.4568056181836,
117.270577294226)) ;
#188281 = CARTESIAN_POINT('Ctrl Pts',(-12.8425354197324,-12.4568056323219,
117.294808292558)) ;
#188282 = CARTESIAN_POINT('Ctrl Pts',(-12.7687315620788,-12.4568056464601,
117.319039290891)) ;
#188283 = CARTESIAN_POINT('Ctrl Pts',(-12.7614420790756,-12.3845797570745,
117.296836702741)) ;
#188284 = CARTESIAN_POINT('Ctrl Pts',(-12.7541525960724,-12.3123538676888,
117.274634114591)) ;
#188285 = CARTESIAN_POINT('Ctrl Pts',(-12.8279564537259,-12.3123538535506,
117.250403116258)) ;
#188286 = CARTESIAN_POINT('Ctrl Pts',(-12.9017603113795,-12.3123538394123,
117.226172117926)) ;
#188287 = CARTESIAN_POINT('Ctrl Pts',(-12.9090497943827,-12.384579728798,
117.248374706076)) ;
#188288 = CARTESIAN_POINT('Ctrl Pts',(-12.8169551777731,-12.5118388251457,
117.003294087217)) ;
#188289 = CARTESIAN_POINT('Ctrl Pts',(-12.8299521097154,-12.5752838792253,
117.042880643781)) ;
#188290 = CARTESIAN_POINT('Ctrl Pts',(-12.7561482516071,-12.5752839097083,
117.067111640729)) ;
#188291 = CARTESIAN_POINT('Ctrl Pts',(-12.6823443934988,-12.5752839401913,
117.091342637677)) ;
#188292 = CARTESIAN_POINT('Ctrl Pts',(-12.6693474615566,-12.5118388861117,
117.051756081112)) ;
#188293 = CARTESIAN_POINT('Ctrl Pts',(-12.6563505296143,-12.448393832032,
117.012169524548)) ;
#188294 = CARTESIAN_POINT('Ctrl Pts',(-12.7301543877226,-12.4483938015491,
116.9879385276)) ;
#188295 = CARTESIAN_POINT('Ctrl Pts',(-12.8039582458309,-12.4483937710661,
116.963707530652)) ;
#188296 = CARTESIAN_POINT('Ctrl Pts',(-12.8169551777731,-12.5118388251457,
117.003294087217)) ;
#188297 = CARTESIAN_POINT('Ctrl Pts',(-12.7382168138023,-12.7038857020727,
116.798924647324)) ;
#188298 = CARTESIAN_POINT('Ctrl Pts',(-12.755996265204,-12.7540141068732,
116.853077986343)) ;
#188299 = CARTESIAN_POINT('Ctrl Pts',(-12.6821924084334,-12.7540141550584,
116.877308987365)) ;
#188300 = CARTESIAN_POINT('Ctrl Pts',(-12.6083885516627,-12.7540142032436,
116.901539988387)) ;
#188301 = CARTESIAN_POINT('Ctrl Pts',(-12.5906091002609,-12.7038857984431,
116.847386649367)) ;
#188302 = CARTESIAN_POINT('Ctrl Pts',(-12.5728296488592,-12.6537573936426,
116.793233310347)) ;
#188303 = CARTESIAN_POINT('Ctrl Pts',(-12.6466335056298,-12.6537573454574,
116.769002309326)) ;
#188304 = CARTESIAN_POINT('Ctrl Pts',(-12.7204373624006,-12.6537572972722,
116.744771308304)) ;
#188305 = CARTESIAN_POINT('Ctrl Pts',(-12.7382168138023,-12.7038857020727,
116.798924647324)) ;
#188306 = CARTESIAN_POINT('Ctrl Pts',(-12.6778922634921,-12.9467051649881,
116.650586228922)) ;
#188307 = CARTESIAN_POINT('Ctrl Pts',(-12.6991766219081,-12.9799528972862,
116.715414949048)) ;
#188308 = CARTESIAN_POINT('Ctrl Pts',(-12.6253727686005,-12.9799529618983,
116.739645960617)) ;
#188309 = CARTESIAN_POINT('Ctrl Pts',(-12.5515689152929,-12.9799530265103,
116.763876972187)) ;
#188310 = CARTESIAN_POINT('Ctrl Pts',(-12.5302845568768,-12.9467052942123,
116.699048252061)) ;
#188311 = CARTESIAN_POINT('Ctrl Pts',(-12.5090001984607,-12.9134575619143,
116.634219531935)) ;
#188312 = CARTESIAN_POINT('Ctrl Pts',(-12.5828040517684,-12.9134574973022,
116.609988520366)) ;
#188313 = CARTESIAN_POINT('Ctrl Pts',(-12.656607905076,-12.9134574326901,
116.585757508796)) ;
#188314 = CARTESIAN_POINT('Ctrl Pts',(-12.6778922634921,-12.9467051649881,
116.650586228922)) ;
#188315 = CARTESIAN_POINT('Ctrl Pts',(-12.6393672663025,-13.2232753780377,
116.568664349212)) ;
#188316 = CARTESIAN_POINT('Ctrl Pts',(-12.6626392596797,-13.237261879662,
116.639547084586)) ;
#188317 = CARTESIAN_POINT('Ctrl Pts',(-12.588835411666,-13.237261957473,116.66377811228)) ;
#188318 = CARTESIAN_POINT('Ctrl Pts',(-12.5150315636522,-13.237262035284,
116.688009139974)) ;
#188319 = CARTESIAN_POINT('Ctrl Pts',(-12.4917595702749,-13.2232755336597,
116.617126404599)) ;
#188320 = CARTESIAN_POINT('Ctrl Pts',(-12.4684875768976,-13.2092890320355,
116.546243669225)) ;
#188321 = CARTESIAN_POINT('Ctrl Pts',(-12.5422914249114,-13.2092889542245,
116.522012641531)) ;
#188322 = CARTESIAN_POINT('Ctrl Pts',(-12.6160952729252,-13.2092888764135,
116.497781613838)) ;
#188323 = CARTESIAN_POINT('Ctrl Pts',(-12.6393672663025,-13.2232753780377,
116.568664349212)) ;
#188324 = CARTESIAN_POINT('Ctrl Pts',(-12.6246970514702,-13.5141286997517,
116.5594436943)) ;
#188325 = CARTESIAN_POINT('Ctrl Pts',(-12.6482932870681,-13.5078290678433,
116.631314019028)) ;
#188326 = CARTESIAN_POINT('Ctrl Pts',(-12.5744894458595,-13.5078291537003,
116.655545067449)) ;
#188327 = CARTESIAN_POINT('Ctrl Pts',(-12.500685604651,-13.5078292395572,
116.679776115871)) ;
#188328 = CARTESIAN_POINT('Ctrl Pts',(-12.4770893690531,-13.5141288714655,
116.607905791143)) ;
#188329 = CARTESIAN_POINT('Ctrl Pts',(-12.4534931334552,-13.5204285033738,
116.536035466415)) ;
#188330 = CARTESIAN_POINT('Ctrl Pts',(-12.5272969746638,-13.5204284175169,
116.511804417994)) ;
#188331 = CARTESIAN_POINT('Ctrl Pts',(-12.6011008158723,-13.52042833166,116.487573369573)) ;
#188332 = CARTESIAN_POINT('Ctrl Pts',(-12.6246970514702,-13.5141286997517,
116.5594436943)) ;
#188333 = CARTESIAN_POINT('Ctrl Pts',(-12.6342523291232,-13.7984771926956,
116.624052868779)) ;
#188334 = CARTESIAN_POINT('Ctrl Pts',(-12.6564811749019,-13.7723162248091,
116.69175834462)) ;
#188335 = CARTESIAN_POINT('Ctrl Pts',(-12.5826773414463,-13.7723163117777,
116.715989416656)) ;
#188336 = CARTESIAN_POINT('Ctrl Pts',(-12.5088735079907,-13.7723163987464,
116.740220488691)) ;
#188337 = CARTESIAN_POINT('Ctrl Pts',(-12.486644662212,-13.7984773666329,
116.672515012851)) ;
#188338 = CARTESIAN_POINT('Ctrl Pts',(-12.4644158164333,-13.8246383345194,
116.60480953701)) ;
#188339 = CARTESIAN_POINT('Ctrl Pts',(-12.5382196498889,-13.8246382475507,
116.580578464974)) ;
#188340 = CARTESIAN_POINT('Ctrl Pts',(-12.6120234833445,-13.8246381605821,
116.556347392938)) ;
#188341 = CARTESIAN_POINT('Ctrl Pts',(-12.6342523291232,-13.7984771926956,
116.624052868779)) ;
#188342 = CARTESIAN_POINT('Ctrl Pts',(-12.6667338754881,-14.0556517682192,
116.758530399118)) ;
#188343 = CARTESIAN_POINT('Ctrl Pts',(-12.6859920465302,-14.0114975765456,
116.817187678919)) ;
#188344 = CARTESIAN_POINT('Ctrl Pts',(-12.6121882209902,-14.011497656322,
116.841418775065)) ;
#188345 = CARTESIAN_POINT('Ctrl Pts',(-12.5383843954502,-14.0114977360984,
116.86564987121)) ;
#188346 = CARTESIAN_POINT('Ctrl Pts',(-12.5191262244081,-14.055651927772,
116.806992591408)) ;
#188347 = CARTESIAN_POINT('Ctrl Pts',(-12.4998680533661,-14.0998061194455,
116.748335311607)) ;
#188348 = CARTESIAN_POINT('Ctrl Pts',(-12.5736718789061,-14.0998060396691,
116.724104215462)) ;
#188349 = CARTESIAN_POINT('Ctrl Pts',(-12.6474757044461,-14.0998059598928,
116.699873119317)) ;
#188350 = CARTESIAN_POINT('Ctrl Pts',(-12.6667338754881,-14.0556517682192,
116.758530399118)) ;
#188351 = CARTESIAN_POINT('Ctrl Pts',(-12.7185614877042,-14.2658619034502,
116.951700772076)) ;
#188352 = CARTESIAN_POINT('Ctrl Pts',(-12.7334986348115,-14.206967241119,
116.997196910099)) ;
#188353 = CARTESIAN_POINT('Ctrl Pts',(-12.6596948160871,-14.2069673051098,
117.021428027003)) ;
#188354 = CARTESIAN_POINT('Ctrl Pts',(-12.5858909973627,-14.2069673691006,
117.045659143907)) ;
#188355 = CARTESIAN_POINT('Ctrl Pts',(-12.5709538502553,-14.2658620314317,
117.000163005885)) ;
#188356 = CARTESIAN_POINT('Ctrl Pts',(-12.5560167031479,-14.3247566937629,
116.954666867862)) ;
#188357 = CARTESIAN_POINT('Ctrl Pts',(-12.6298205218724,-14.3247566297721,
116.930435750958)) ;
#188358 = CARTESIAN_POINT('Ctrl Pts',(-12.7036243405968,-14.3247565657813,
116.906204634054)) ;
#188359 = CARTESIAN_POINT('Ctrl Pts',(-12.7185614877042,-14.2658619034502,
116.951700772076)) ;
#188360 = CARTESIAN_POINT('Ctrl Pts',(-12.7861042651264,-14.4169100671748,
117.193039609464)) ;
#188361 = CARTESIAN_POINT('Ctrl Pts',(-12.7956109926747,-14.3473831262014,
117.221995565631)) ;
#188362 = CARTESIAN_POINT('Ctrl Pts',(-12.721807179474,-14.3473831682741,
117.246226699359)) ;
#188363 = CARTESIAN_POINT('Ctrl Pts',(-12.6480033662733,-14.3473832103469,
117.270457833088)) ;
#188364 = CARTESIAN_POINT('Ctrl Pts',(-12.638496638725,-14.4169101513204,
117.241501876921)) ;
#188365 = CARTESIAN_POINT('Ctrl Pts',(-12.6289899111766,-14.4864370922939,
117.212545920754)) ;
#188366 = CARTESIAN_POINT('Ctrl Pts',(-12.7027937243773,-14.4864370502211,
117.188314787025)) ;
#188367 = CARTESIAN_POINT('Ctrl Pts',(-12.776597537578,-14.4864370081483,
117.164083653297)) ;
#188368 = CARTESIAN_POINT('Ctrl Pts',(-12.7861042651264,-14.4169100671748,
117.193039609464)) ;
#188369 = CARTESIAN_POINT('Ctrl Pts',(-12.8630657685899,-14.4953742453793,
117.462914929122)) ;
#188370 = CARTESIAN_POINT('Ctrl Pts',(-12.8664795502472,-14.4202668072197,
117.473312755161)) ;
#188371 = CARTESIAN_POINT('Ctrl Pts',(-12.7926757400385,-14.4202668221935,
117.497543898003)) ;
#188372 = CARTESIAN_POINT('Ctrl Pts',(-12.7188719298299,-14.4202668371673,
117.521775040845)) ;
#188373 = CARTESIAN_POINT('Ctrl Pts',(-12.7154581481725,-14.495374275327,
117.511377214806)) ;
#188374 = CARTESIAN_POINT('Ctrl Pts',(-12.7120443665152,-14.5704817134867,
117.500979388766)) ;
#188375 = CARTESIAN_POINT('Ctrl Pts',(-12.7858481767239,-14.5704816985128,
117.476748245924)) ;
#188376 = CARTESIAN_POINT('Ctrl Pts',(-12.8596519869325,-14.570481683539,
117.452517103082)) ;
#188377 = CARTESIAN_POINT('Ctrl Pts',(-12.8630657685899,-14.4953742453793,
117.462914929122)) ;
#188378 = CARTESIAN_POINT('Ctrl Pts',(-12.9430874779425,-14.4969828286805,
117.741985737709)) ;
#188379 = CARTESIAN_POINT('Ctrl Pts',(-12.9401882473644,-14.4216525600046,
117.733155147064)) ;
#188380 = CARTESIAN_POINT('Ctrl Pts',(-12.8663844374637,-14.4216525461531,
117.757386290844)) ;
#188381 = CARTESIAN_POINT('Ctrl Pts',(-12.7925806275628,-14.4216525323015,
117.781617434623)) ;
#188382 = CARTESIAN_POINT('Ctrl Pts',(-12.7954798581409,-14.4969828009775,
117.790448025268)) ;
#188383 = CARTESIAN_POINT('Ctrl Pts',(-12.7983790887189,-14.5723130696534,
117.799278615913)) ;
#188384 = CARTESIAN_POINT('Ctrl Pts',(-12.8721828986197,-14.5723130835049,
117.775047472134)) ;
#188385 = CARTESIAN_POINT('Ctrl Pts',(-12.9459867085205,-14.5723130973564,
117.750816328354)) ;
#188386 = CARTESIAN_POINT('Ctrl Pts',(-12.9430874779425,-14.4969828286805,
117.741985737709)) ;
#188387 = CARTESIAN_POINT('Ctrl Pts',(-13.0203177415346,-14.421551875411,
118.012685171403)) ;
#188388 = CARTESIAN_POINT('Ctrl Pts',(-13.0112884091571,-14.3513763125925,
117.985183279766)) ;
#188389 = CARTESIAN_POINT('Ctrl Pts',(-12.9374845968934,-14.3513762706419,
118.009414416348)) ;
#188390 = CARTESIAN_POINT('Ctrl Pts',(-12.8636807846298,-14.3513762286912,
118.033645552931)) ;
#188391 = CARTESIAN_POINT('Ctrl Pts',(-12.8727101170073,-14.4215517915098,
118.061147444569)) ;
#188392 = CARTESIAN_POINT('Ctrl Pts',(-12.8817394493848,-14.4917273543283,
118.088649336206)) ;
#188393 = CARTESIAN_POINT('Ctrl Pts',(-12.9555432616484,-14.491727396279,
118.064418199623)) ;
#188394 = CARTESIAN_POINT('Ctrl Pts',(-13.029347073912,-14.4917274382296,
118.04018706304)) ;
#188395 = CARTESIAN_POINT('Ctrl Pts',(-13.0203177415346,-14.421551875411,
118.012685171403)) ;
#188396 = CARTESIAN_POINT('Ctrl Pts',(-13.0883258543975,-14.2735000710325,
118.255405538239)) ;
#188397 = CARTESIAN_POINT('Ctrl Pts',(-13.0737988185205,-14.213556255384,
118.211158528823)) ;
#188398 = CARTESIAN_POINT('Ctrl Pts',(-12.9999950012594,-14.2135561892348,
118.235389650184)) ;
#188399 = CARTESIAN_POINT('Ctrl Pts',(-12.9261911839982,-14.2135561230857,
118.259620771545)) ;
#188400 = CARTESIAN_POINT('Ctrl Pts',(-12.9407182198752,-14.2734999387342,
118.303867780962)) ;
#188401 = CARTESIAN_POINT('Ctrl Pts',(-12.9552452557522,-14.3334437543827,
118.348114790378)) ;
#188402 = CARTESIAN_POINT('Ctrl Pts',(-13.0290490730134,-14.3334438205319,
118.323883669017)) ;
#188403 = CARTESIAN_POINT('Ctrl Pts',(-13.1028528902745,-14.3334438866811,
118.299652547656)) ;
#188404 = CARTESIAN_POINT('Ctrl Pts',(-13.0883258543975,-14.2735000710325,
118.255405538239)) ;
#188405 = CARTESIAN_POINT('Ctrl Pts',(-13.141058050103,-14.0646532706665,
118.451466458674)) ;
#188406 = CARTESIAN_POINT('Ctrl Pts',(-13.1220942972562,-14.019201123048,
118.393705925278)) ;
#188407 = CARTESIAN_POINT('Ctrl Pts',(-13.0482904731012,-14.0192010389841,
118.417937025641)) ;
#188408 = CARTESIAN_POINT('Ctrl Pts',(-12.9744866489462,-14.0192009549201,
118.442168126005)) ;
#188409 = CARTESIAN_POINT('Ctrl Pts',(-12.9934504017929,-14.0646531025386,
118.499928659402)) ;
#188410 = CARTESIAN_POINT('Ctrl Pts',(-13.0124141546397,-14.110105250157,
118.557689192798)) ;
#188411 = CARTESIAN_POINT('Ctrl Pts',(-13.0862179787947,-14.110105334221,
118.533458092435)) ;
#188412 = CARTESIAN_POINT('Ctrl Pts',(-13.1600218029498,-14.1101054182849,
118.509226992071)) ;
#188413 = CARTESIAN_POINT('Ctrl Pts',(-13.141058050103,-14.0646532706665,
118.451466458674)) ;
#188414 = CARTESIAN_POINT('Ctrl Pts',(-13.174281067565,-13.8091818841456,
118.588155479857)) ;
#188415 = CARTESIAN_POINT('Ctrl Pts',(-13.1522348887302,-13.7814979528365,
118.521006374321)) ;
#188416 = CARTESIAN_POINT('Ctrl Pts',(-13.0784310564862,-13.7814978588796,
118.545237450047)) ;
#188417 = CARTESIAN_POINT('Ctrl Pts',(-13.0046272242423,-13.7814977649226,
118.569468525773)) ;
#188418 = CARTESIAN_POINT('Ctrl Pts',(-13.0266734030771,-13.8091816962316,
118.636617631309)) ;
#188419 = CARTESIAN_POINT('Ctrl Pts',(-13.048719581912,-13.8368656275406,
118.703766736846)) ;
#188420 = CARTESIAN_POINT('Ctrl Pts',(-13.1225234141559,-13.8368657214976,
118.679535661119)) ;
#188421 = CARTESIAN_POINT('Ctrl Pts',(-13.1963272463998,-13.8368658154546,
118.655304585393)) ;
#188422 = CARTESIAN_POINT('Ctrl Pts',(-13.174281067565,-13.8091818841456,
118.588155479857)) ;
#188423 = CARTESIAN_POINT('Ctrl Pts',(-13.1847943926898,-13.5266904596517,
118.655545948521)) ;
#188424 = CARTESIAN_POINT('Ctrl Pts',(-13.1612493680941,-13.5186880514058,
118.583831600714)) ;
#188425 = CARTESIAN_POINT('Ctrl Pts',(-13.0874455275475,-13.5186879553988,
118.608062651152)) ;
#188426 = CARTESIAN_POINT('Ctrl Pts',(-13.0136416870009,-13.5186878593918,
118.632293701589)) ;
#188427 = CARTESIAN_POINT('Ctrl Pts',(-13.0371867115966,-13.5266902676377,
118.704008049396)) ;
#188428 = CARTESIAN_POINT('Ctrl Pts',(-13.0607317361924,-13.5346926758837,
118.775722397203)) ;
#188429 = CARTESIAN_POINT('Ctrl Pts',(-13.134535576739,-13.5346927718906,
118.751491346766)) ;
#188430 = CARTESIAN_POINT('Ctrl Pts',(-13.2083394172856,-13.5346928678976,
118.727260296328)) ;
#188431 = CARTESIAN_POINT('Ctrl Pts',(-13.1847943926898,-13.5266904596517,
118.655545948521)) ;
#188432 = CARTESIAN_POINT('Ctrl Pts',(-13.1711799492058,-13.2352604395114,
118.649594190874)) ;
#188433 = CARTESIAN_POINT('Ctrl Pts',(-13.1478151112943,-13.2475929455495,
118.578428662746)) ;
#188434 = CARTESIAN_POINT('Ctrl Pts',(-13.0740112629422,-13.2475928562787,
118.602659689409)) ;
#188435 = CARTESIAN_POINT('Ctrl Pts',(-13.0002074145902,-13.2475927670079,
118.626890716073)) ;
#188436 = CARTESIAN_POINT('Ctrl Pts',(-13.0235722525017,-13.2352602609698,
118.698056244201)) ;
#188437 = CARTESIAN_POINT('Ctrl Pts',(-13.0469370904133,-13.2229277549316,
118.769221772329)) ;
#188438 = CARTESIAN_POINT('Ctrl Pts',(-13.1207409387653,-13.2229278442025,
118.744990745665)) ;
#188439 = CARTESIAN_POINT('Ctrl Pts',(-13.1945447871174,-13.2229279334733,
118.720759719002)) ;
#188440 = CARTESIAN_POINT('Ctrl Pts',(-13.1711799492058,-13.2352604395114,
118.649594190874)) ;
#188441 = CARTESIAN_POINT('Ctrl Pts',(-13.1334389030405,-12.9567404114365,
118.570185916102)) ;
#188442 = CARTESIAN_POINT('Ctrl Pts',(-13.1119382741817,-12.9885373907524,
118.504698468097)) ;
#188443 = CARTESIAN_POINT('Ctrl Pts',(-13.0381344195311,-12.9885373153284,
118.528929475576)) ;
#188444 = CARTESIAN_POINT('Ctrl Pts',(-12.9643305648806,-12.9885372399044,
118.553160483055)) ;
#188445 = CARTESIAN_POINT('Ctrl Pts',(-12.9858311937394,-12.9567402605885,
118.618647931061)) ;
#188446 = CARTESIAN_POINT('Ctrl Pts',(-13.0073318225981,-12.9249432812726,
118.684135379066)) ;
#188447 = CARTESIAN_POINT('Ctrl Pts',(-13.0811356772487,-12.9249433566966,
118.659904371587)) ;
#188448 = CARTESIAN_POINT('Ctrl Pts',(-13.1549395318993,-12.9249434321206,
118.635673364108)) ;
#188449 = CARTESIAN_POINT('Ctrl Pts',(-13.1334389030405,-12.9567404114365,
118.570185916102)) ;
#188450 = CARTESIAN_POINT('Ctrl Pts',(-13.0738178620181,-12.7122106250869,
118.424014225001)) ;
#188451 = CARTESIAN_POINT('Ctrl Pts',(-13.0557144644975,-12.7611284974195,
118.368874195644)) ;
#188452 = CARTESIAN_POINT('Ctrl Pts',(-12.9819106054213,-12.7611284394827,
118.393105189643)) ;
#188453 = CARTESIAN_POINT('Ctrl Pts',(-12.9081067463451,-12.7611283815459,
118.417336183643)) ;
#188454 = CARTESIAN_POINT('Ctrl Pts',(-12.9262101438657,-12.7122105092134,
118.472476213)) ;
#188455 = CARTESIAN_POINT('Ctrl Pts',(-12.9443135413864,-12.6632926368809,
118.527616242358)) ;
#188456 = CARTESIAN_POINT('Ctrl Pts',(-13.0181174004625,-12.6632926948177,
118.503385248358)) ;
#188457 = CARTESIAN_POINT('Ctrl Pts',(-13.0919212595387,-12.6632927527544,
118.479154254359)) ;
#188458 = CARTESIAN_POINT('Ctrl Pts',(-13.0738178620181,-12.7122106250869,
118.424014225001)) ;
#188459 = CARTESIAN_POINT('Ctrl Pts',(-12.9958498760682,-12.5182289407429,
118.221927525614)) ;
#188460 = CARTESIAN_POINT('Ctrl Pts',(-12.9824305092123,-12.5807644314872,
118.181054298033)) ;
#188461 = CARTESIAN_POINT('Ctrl Pts',(-12.9086266477341,-12.5807643929597,
118.205285284716)) ;
#188462 = CARTESIAN_POINT('Ctrl Pts',(-12.8348227862559,-12.5807643544323,
118.2295162714)) ;
#188463 = CARTESIAN_POINT('Ctrl Pts',(-12.8482421531118,-12.518228863688,
118.27038949898)) ;
#188464 = CARTESIAN_POINT('Ctrl Pts',(-12.8616615199678,-12.4556933729437,
118.311262726561)) ;
#188465 = CARTESIAN_POINT('Ctrl Pts',(-12.9354653814459,-12.4556934114712,
118.287031739878)) ;
#188466 = CARTESIAN_POINT('Ctrl Pts',(-13.0092692429241,-12.4556934499986,
118.262800753194)) ;
#188467 = CARTESIAN_POINT('Ctrl Pts',(-12.9958498760682,-12.5182289407429,
118.221927525614)) ;
#188468 = CARTESIAN_POINT('Ctrl Pts',(-12.903982147102,-12.3880154836096,
117.97761106073)) ;
#188469 = CARTESIAN_POINT('Ctrl Pts',(-12.8962220934696,-12.4597373427525,
117.953975188267)) ;
#188470 = CARTESIAN_POINT('Ctrl Pts',(-12.8224182319584,-12.4597373239449,
117.97820617485)) ;
#188471 = CARTESIAN_POINT('Ctrl Pts',(-12.7486143704472,-12.4597373051373,
118.002437161433)) ;
#188472 = CARTESIAN_POINT('Ctrl Pts',(-12.7563744240796,-12.3880154459944,
118.026073033896)) ;
#188473 = CARTESIAN_POINT('Ctrl Pts',(-12.764134477712,-12.3162935868514,
118.049708906359)) ;
#188474 = CARTESIAN_POINT('Ctrl Pts',(-12.8379383392232,-12.316293605659,
118.025477919776)) ;
#188475 = CARTESIAN_POINT('Ctrl Pts',(-12.9117422007343,-12.3162936244666,
118.001246933193)) ;
#188476 = CARTESIAN_POINT('Ctrl Pts',(-12.903982147102,-12.3880154836096,
117.97761106073)) ;
#188477 = CARTESIAN_POINT('Ctrl Pts',(-12.8039707728634,-12.3319594983171,
117.708586088061)) ;
#188478 = CARTESIAN_POINT('Ctrl Pts',(-12.8024453054662,-12.4077044418995,
117.703939759514)) ;
#188479 = CARTESIAN_POINT('Ctrl Pts',(-12.7286414461199,-12.407704439621,
117.728170752691)) ;
#188480 = CARTESIAN_POINT('Ctrl Pts',(-12.6548375867736,-12.4077044373425,
117.752401745868)) ;
#188481 = CARTESIAN_POINT('Ctrl Pts',(-12.6563630541708,-12.33195949376,117.757048074414)) ;
#188482 = CARTESIAN_POINT('Ctrl Pts',(-12.6578885215679,-12.2562145501775,
117.761694402961)) ;
#188483 = CARTESIAN_POINT('Ctrl Pts',(-12.7316923809142,-12.2562145524561,
117.737463409784)) ;
#188484 = CARTESIAN_POINT('Ctrl Pts',(-12.8054962402605,-12.2562145547346,
117.713232416607)) ;
#188485 = CARTESIAN_POINT('Ctrl Pts',(-12.8039707728634,-12.3319594983171,
117.708586088061)) ;
#188486 = CARTESIAN_POINT('Ctrl Pts',(-12.7034974125508,-12.3535606969818,
117.437807953422)) ;
#188487 = CARTESIAN_POINT('Ctrl Pts',(-12.7082554753366,-12.4279116529158,
117.452300244096)) ;
#188488 = CARTESIAN_POINT('Ctrl Pts',(-12.6344516183772,-12.4279116627694,
117.476531244543)) ;
#188489 = CARTESIAN_POINT('Ctrl Pts',(-12.5606477614179,-12.427911672623,
117.50076224499)) ;
#188490 = CARTESIAN_POINT('Ctrl Pts',(-12.5558896986321,-12.3535607166891,
117.486269954316)) ;
#188491 = CARTESIAN_POINT('Ctrl Pts',(-12.5511316358463,-12.2792097607552,
117.471777663643)) ;
#188492 = CARTESIAN_POINT('Ctrl Pts',(-12.6249354928057,-12.2792097509015,
117.447546663196)) ;
#188493 = CARTESIAN_POINT('Ctrl Pts',(-12.698739349765,-12.2792097410479,
117.423315662748)) ;
#188494 = CARTESIAN_POINT('Ctrl Pts',(-12.7034974125508,-12.3535606969818,
117.437807953422)) ;
#188495 = CARTESIAN_POINT('Ctrl Pts',(-12.6073331725263,-12.451253883518,
117.180405293082)) ;
#188496 = CARTESIAN_POINT('Ctrl Pts',(-12.6180782994954,-12.5188965599117,
117.213133215423)) ;
#188497 = CARTESIAN_POINT('Ctrl Pts',(-12.5442744463408,-12.5188965769681,
117.237364227459)) ;
#188498 = CARTESIAN_POINT('Ctrl Pts',(-12.4704705931862,-12.5188965940245,
117.261595239495)) ;
#188499 = CARTESIAN_POINT('Ctrl Pts',(-12.4597254662172,-12.4512539176309,
117.228867317154)) ;
#188500 = CARTESIAN_POINT('Ctrl Pts',(-12.4489803392481,-12.3836112412372,
117.196139394813)) ;
#188501 = CARTESIAN_POINT('Ctrl Pts',(-12.5227841924027,-12.3836112241808,
117.171908382778)) ;
#188502 = CARTESIAN_POINT('Ctrl Pts',(-12.5965880455573,-12.3836112071243,
117.147677370742)) ;
#188503 = CARTESIAN_POINT('Ctrl Pts',(-12.6073331725263,-12.451253883518,
117.180405293082)) ;
#188504 = CARTESIAN_POINT('Ctrl Pts',(-12.5223846797122,-12.618326669095,
116.957138731185)) ;
#188505 = CARTESIAN_POINT('Ctrl Pts',(-12.538343432535,-12.6744063613934,
117.005746516825)) ;
#188506 = CARTESIAN_POINT('Ctrl Pts',(-12.4645395830942,-12.6744063803127,
117.029977540172)) ;
#188507 = CARTESIAN_POINT('Ctrl Pts',(-12.3907357336533,-12.6744063992319,
117.054208563519)) ;
#188508 = CARTESIAN_POINT('Ctrl Pts',(-12.3747769808305,-12.6183267069335,
117.005600777879)) ;
#188509 = CARTESIAN_POINT('Ctrl Pts',(-12.3588182280077,-12.5622470146351,
116.956992992239)) ;
#188510 = CARTESIAN_POINT('Ctrl Pts',(-12.4326220774486,-12.5622469957158,
116.932761968892)) ;
#188511 = CARTESIAN_POINT('Ctrl Pts',(-12.5064259268894,-12.5622469767965,
116.908530945545)) ;
#188512 = CARTESIAN_POINT('Ctrl Pts',(-12.5223846797122,-12.618326669095,
116.957138731185)) ;
#188513 = CARTESIAN_POINT('Ctrl Pts',(-12.4538138970697,-12.8433532834822,
116.783847061127)) ;
#188514 = CARTESIAN_POINT('Ctrl Pts',(-12.4738488524153,-12.883805650216,
116.844870302127)) ;
#188515 = CARTESIAN_POINT('Ctrl Pts',(-12.4000450061609,-12.8838056661619,
116.86910133518)) ;
#188516 = CARTESIAN_POINT('Ctrl Pts',(-12.3262411599065,-12.8838056821078,
116.893332368233)) ;
#188517 = CARTESIAN_POINT('Ctrl Pts',(-12.306206204561,-12.843353315374,116.832309127233)) ;
#188518 = CARTESIAN_POINT('Ctrl Pts',(-12.2861712492154,-12.8029009486403,
116.771285886233)) ;
#188519 = CARTESIAN_POINT('Ctrl Pts',(-12.3599750954699,-12.8029009326944,
116.74705485318)) ;
#188520 = CARTESIAN_POINT('Ctrl Pts',(-12.4337789417243,-12.8029009167485,
116.722823820128)) ;
#188521 = CARTESIAN_POINT('Ctrl Pts',(-12.4538138970697,-12.8433532834822,
116.783847061127)) ;
#188522 = CARTESIAN_POINT('Ctrl Pts',(-12.4061377499022,-13.1083703127966,
116.674020302438)) ;
#188523 = CARTESIAN_POINT('Ctrl Pts',(-12.4287995875301,-13.1303789495469,
116.74304460315)) ;
#188524 = CARTESIAN_POINT('Ctrl Pts',(-12.3549957432582,-13.1303789610419,
116.767275642241)) ;
#188525 = CARTESIAN_POINT('Ctrl Pts',(-12.2811918989863,-13.130378972537,
116.791506681332)) ;
#188526 = CARTESIAN_POINT('Ctrl Pts',(-12.2585300613583,-13.1083703357867,
116.72248238062)) ;
#188527 = CARTESIAN_POINT('Ctrl Pts',(-12.2358682237303,-13.0863616990364,
116.653458079908)) ;
#188528 = CARTESIAN_POINT('Ctrl Pts',(-12.3096720680023,-13.0863616875414,
116.629227040817)) ;
#188529 = CARTESIAN_POINT('Ctrl Pts',(-12.3834759122742,-13.0863616760463,
116.604996001726)) ;
#188530 = CARTESIAN_POINT('Ctrl Pts',(-12.4061377499022,-13.1083703127966,
116.674020302438)) ;
#188531 = CARTESIAN_POINT('Ctrl Pts',(-12.3816337942229,-13.3973093025061,
116.635000519371)) ;
#188532 = CARTESIAN_POINT('Ctrl Pts',(-12.4053038929574,-13.3991753907739,
116.707095820866)) ;
#188533 = CARTESIAN_POINT('Ctrl Pts',(-12.3315000496693,-13.399175395662,
116.731326862953)) ;
#188534 = CARTESIAN_POINT('Ctrl Pts',(-12.2576962063811,-13.39917540055,116.755557905041)) ;
#188535 = CARTESIAN_POINT('Ctrl Pts',(-12.2340261076466,-13.3973093122823,
116.683462603546)) ;
#188536 = CARTESIAN_POINT('Ctrl Pts',(-12.2103560089121,-13.3954432240146,
116.611367302051)) ;
#188537 = CARTESIAN_POINT('Ctrl Pts',(-12.2841598522002,-13.3954432191265,
116.587136259963)) ;
#188538 = CARTESIAN_POINT('Ctrl Pts',(-12.3579636954884,-13.3954432142384,
116.562905217876)) ;
#188539 = CARTESIAN_POINT('Ctrl Pts',(-12.3816337942229,-13.3973093025061,
116.635000519371)) ;
#188540 = CARTESIAN_POINT('Ctrl Pts',(-12.381503672392,-13.685052446536,116.669875319027)) ;
#188541 = CARTESIAN_POINT('Ctrl Pts',(-12.4044882857984,-13.666829482395,
116.739882742886)) ;
#188542 = CARTESIAN_POINT('Ctrl Pts',(-12.3306844425751,-13.6668294834514,
116.764113785171)) ;
#188543 = CARTESIAN_POINT('Ctrl Pts',(-12.2568805993519,-13.6668294845077,
116.788344827456)) ;
#188544 = CARTESIAN_POINT('Ctrl Pts',(-12.2338959859455,-13.6850524486487,
116.718337403597)) ;
#188545 = CARTESIAN_POINT('Ctrl Pts',(-12.2109113725392,-13.7032754127896,
116.648329979738)) ;
#188546 = CARTESIAN_POINT('Ctrl Pts',(-12.2847152157624,-13.7032754117333,
116.624098937453)) ;
#188547 = CARTESIAN_POINT('Ctrl Pts',(-12.3585190589856,-13.7032754106769,
116.599867895168)) ;
#188548 = CARTESIAN_POINT('Ctrl Pts',(-12.381503672392,-13.685052446536,116.669875319027)) ;
#188549 = CARTESIAN_POINT('Ctrl Pts',(-12.4049796303941,-13.9562925901238,
116.776990471733)) ;
#188550 = CARTESIAN_POINT('Ctrl Pts',(-12.425622446726,-13.9191017880253,
116.839865159623)) ;
#188551 = CARTESIAN_POINT('Ctrl Pts',(-12.3518186029917,-13.9191017857383,
116.864096200351)) ;
#188552 = CARTESIAN_POINT('Ctrl Pts',(-12.2780147592573,-13.9191017834513,
116.88832724108)) ;
#188553 = CARTESIAN_POINT('Ctrl Pts',(-12.2573719429255,-13.9562925855498,
116.82545255319)) ;
#188554 = CARTESIAN_POINT('Ctrl Pts',(-12.2367291265936,-13.9934833876483,
116.762577865301)) ;
#188555 = CARTESIAN_POINT('Ctrl Pts',(-12.3105329703279,-13.9934833899353,
116.738346824573)) ;
#188556 = CARTESIAN_POINT('Ctrl Pts',(-12.3843368140622,-13.9934833922223,
116.714115783844)) ;
#188557 = CARTESIAN_POINT('Ctrl Pts',(-12.4049796303941,-13.9562925901238,
116.776990471733)) ;
#188558 = CARTESIAN_POINT('Ctrl Pts',(-12.4494947820984,-14.1872893194723,
116.947967301945)) ;
#188559 = CARTESIAN_POINT('Ctrl Pts',(-12.4663273310332,-14.1339131286007,
116.999236530143)) ;
#188560 = CARTESIAN_POINT('Ctrl Pts',(-12.3925234868813,-14.1339131262424,
117.023467569599)) ;
#188561 = CARTESIAN_POINT('Ctrl Pts',(-12.3187196427294,-14.1339131238842,
117.047698609056)) ;
#188562 = CARTESIAN_POINT('Ctrl Pts',(-12.3018870937946,-14.1872893147558,
116.996429380858)) ;
#188563 = CARTESIAN_POINT('Ctrl Pts',(-12.2850545448598,-14.2406655056274,
116.94516015266)) ;
#188564 = CARTESIAN_POINT('Ctrl Pts',(-12.3588583890117,-14.2406655079856,
116.920929113203)) ;
#188565 = CARTESIAN_POINT('Ctrl Pts',(-12.4326622331636,-14.2406655103439,
116.896698073747)) ;
#188566 = CARTESIAN_POINT('Ctrl Pts',(-12.4494947820984,-14.1872893194723,
116.947967301945)) ;
#188567 = CARTESIAN_POINT('Ctrl Pts',(-12.5111240358726,-14.3636852679792,
117.17110246923)) ;
#188568 = CARTESIAN_POINT('Ctrl Pts',(-12.5229448664094,-14.2979128675593,
117.207106811808)) ;
#188569 = CARTESIAN_POINT('Ctrl Pts',(-12.4491410223146,-14.2979128665308,
117.231337851438)) ;
#188570 = CARTESIAN_POINT('Ctrl Pts',(-12.3753371782198,-14.2979128655022,
117.255568891069)) ;
#188571 = CARTESIAN_POINT('Ctrl Pts',(-12.3635163476831,-14.3636852659222,
117.219564548491)) ;
#188572 = CARTESIAN_POINT('Ctrl Pts',(-12.3516955171463,-14.4294576663421,
117.183560205913)) ;
#188573 = CARTESIAN_POINT('Ctrl Pts',(-12.4254993612411,-14.4294576673706,
117.159329166283)) ;
#188574 = CARTESIAN_POINT('Ctrl Pts',(-12.4993032053359,-14.4294576683991,
117.135098126652)) ;
#188575 = CARTESIAN_POINT('Ctrl Pts',(-12.5111240358726,-14.3636852679792,
117.17110246923)) ;
#188576 = CARTESIAN_POINT('Ctrl Pts',(-12.5849595606455,-14.4725504618335,
117.431499846562)) ;
#188577 = CARTESIAN_POINT('Ctrl Pts',(-12.5909072144408,-14.3990795841732,
117.449615440357)) ;
#188578 = CARTESIAN_POINT('Ctrl Pts',(-12.5171033712477,-14.3990795846932,
117.473846482734)) ;
#188579 = CARTESIAN_POINT('Ctrl Pts',(-12.4432995280546,-14.3990795852131,
117.498077525111)) ;
#188580 = CARTESIAN_POINT('Ctrl Pts',(-12.4373518742593,-14.4725504628734,
117.479961931316)) ;
#188581 = CARTESIAN_POINT('Ctrl Pts',(-12.431404220464,-14.5460213405337,
117.461846337522)) ;
#188582 = CARTESIAN_POINT('Ctrl Pts',(-12.5052080636571,-14.5460213400138,
117.437615295145)) ;
#188583 = CARTESIAN_POINT('Ctrl Pts',(-12.5790119068502,-14.5460213394938,
117.413384252768)) ;
#188584 = CARTESIAN_POINT('Ctrl Pts',(-12.5849595606455,-14.4725504618335,
117.431499846562)) ;
#188585 = CARTESIAN_POINT('Ctrl Pts',(-12.6644929453121,-14.505767100085,
117.709124162451)) ;
#188586 = CARTESIAN_POINT('Ctrl Pts',(-12.664163724492,-14.4298697296846,
117.708121408856)) ;
#188587 = CARTESIAN_POINT('Ctrl Pts',(-12.5903598826455,-14.429869730049,
117.732352455334)) ;
#188588 = CARTESIAN_POINT('Ctrl Pts',(-12.516556040799,-14.4298697304134,
117.756583501813)) ;
#188589 = CARTESIAN_POINT('Ctrl Pts',(-12.5168852616191,-14.5057671008138,
117.757586255408)) ;
#188590 = CARTESIAN_POINT('Ctrl Pts',(-12.5172144824392,-14.5816644712143,
117.758589009003)) ;
#188591 = CARTESIAN_POINT('Ctrl Pts',(-12.5910183242857,-14.5816644708498,
117.734357962524)) ;
#188592 = CARTESIAN_POINT('Ctrl Pts',(-12.6648221661322,-14.5816644704854,
117.710126916046)) ;
#188593 = CARTESIAN_POINT('Ctrl Pts',(-12.6644929453121,-14.505767100085,
117.709124162451)) ;
#188594 = CARTESIAN_POINT('Ctrl Pts',(-12.7438560906552,-14.461184023194,
117.986366449058)) ;
#188595 = CARTESIAN_POINT('Ctrl Pts',(-12.7372499374125,-14.388288943336,
117.966245171962)) ;
#188596 = CARTESIAN_POINT('Ctrl Pts',(-12.6634460974251,-14.3882889407252,
117.990476224103)) ;
#188597 = CARTESIAN_POINT('Ctrl Pts',(-12.5896422574376,-14.3882889381144,
118.014707276243)) ;
#188598 = CARTESIAN_POINT('Ctrl Pts',(-12.5962484106803,-14.4611840179724,
118.034828553339)) ;
#188599 = CARTESIAN_POINT('Ctrl Pts',(-12.6028545639229,-14.5340790978304,
118.054949830435)) ;
#188600 = CARTESIAN_POINT('Ctrl Pts',(-12.6766584039103,-14.5340791004412,
118.030718778294)) ;
#188601 = CARTESIAN_POINT('Ctrl Pts',(-12.7504622438978,-14.534079103052,
118.006487726153)) ;
#188602 = CARTESIAN_POINT('Ctrl Pts',(-12.7438560906552,-14.461184023194,
117.986366449058)) ;
#188603 = CARTESIAN_POINT('Ctrl Pts',(-12.8161888293578,-14.3417566878776,
118.242145226587)) ;
#188604 = CARTESIAN_POINT('Ctrl Pts',(-12.8037886916051,-14.2770945733709,
118.204376407392)) ;
#188605 = CARTESIAN_POINT('Ctrl Pts',(-12.7299848531598,-14.2770945642116,
118.22860746423)) ;
#188606 = CARTESIAN_POINT('Ctrl Pts',(-12.6561810147145,-14.2770945550524,
118.252838521068)) ;
#188607 = CARTESIAN_POINT('Ctrl Pts',(-12.6685811524673,-14.3417566695591,
118.290607340263)) ;
#188608 = CARTESIAN_POINT('Ctrl Pts',(-12.68098129022,-14.4064187840659,118.328376159457)) ;
#188609 = CARTESIAN_POINT('Ctrl Pts',(-12.7547851286653,-14.4064187932251,
118.304145102619)) ;
#188610 = CARTESIAN_POINT('Ctrl Pts',(-12.8285889671106,-14.4064188023844,
118.279914045781)) ;
#188611 = CARTESIAN_POINT('Ctrl Pts',(-12.8161888293578,-14.3417566878776,
118.242145226587)) ;
#188612 = CARTESIAN_POINT('Ctrl Pts',(-12.8756299425708,-14.1564991842471,
118.458617084048)) ;
#188613 = CARTESIAN_POINT('Ctrl Pts',(-12.8583285484173,-14.104678506832,
118.405919828527)) ;
#188614 = CARTESIAN_POINT('Ctrl Pts',(-12.7845247106298,-14.1046784883743,
118.430150887369)) ;
#188615 = CARTESIAN_POINT('Ctrl Pts',(-12.7107208728424,-14.1046784699167,
118.454381946211)) ;
#188616 = CARTESIAN_POINT('Ctrl Pts',(-12.7280222669959,-14.1564991473318,
118.507079201731)) ;
#188617 = CARTESIAN_POINT('Ctrl Pts',(-12.7453236611495,-14.208319824747,
118.559776457252)) ;
#188618 = CARTESIAN_POINT('Ctrl Pts',(-12.8191274989369,-14.2083198432046,
118.53554539841)) ;
#188619 = CARTESIAN_POINT('Ctrl Pts',(-12.8929313367243,-14.2083198616622,
118.511314339568)) ;
#188620 = CARTESIAN_POINT('Ctrl Pts',(-12.8756299425708,-14.1564991842471,
118.458617084048)) ;
#188621 = CARTESIAN_POINT('Ctrl Pts',(-12.9173366092664,-13.9178865274089,
118.621150963458)) ;
#188622 = CARTESIAN_POINT('Ctrl Pts',(-12.8963635167268,-13.8826509917796,
118.557270306911)) ;
#188623 = CARTESIAN_POINT('Ctrl Pts',(-12.8225596784781,-13.8826509615156,
118.581501364348)) ;
#188624 = CARTESIAN_POINT('Ctrl Pts',(-12.7487558402295,-13.8826509312515,
118.605732421785)) ;
#188625 = CARTESIAN_POINT('Ctrl Pts',(-12.7697289327691,-13.9178864668808,
118.669613078332)) ;
#188626 = CARTESIAN_POINT('Ctrl Pts',(-12.7907020253087,-13.9531220025101,
118.733493734878)) ;
#188627 = CARTESIAN_POINT('Ctrl Pts',(-12.8645058635573,-13.9531220327742,
118.709262677441)) ;
#188628 = CARTESIAN_POINT('Ctrl Pts',(-12.9383097018059,-13.9531220630382,
118.685031620004)) ;
#188629 = CARTESIAN_POINT('Ctrl Pts',(-12.9173366092664,-13.9178865274089,
118.621150963458)) ;
#188630 = CARTESIAN_POINT('Ctrl Pts',(-12.9373830489153,-13.643415658276,
118.717703562338)) ;
#188631 = CARTESIAN_POINT('Ctrl Pts',(-12.9142455039955,-13.6272927364366,
118.647230332902)) ;
#188632 = CARTESIAN_POINT('Ctrl Pts',(-12.8404416636247,-13.627292694101,
118.671461383875)) ;
#188633 = CARTESIAN_POINT('Ctrl Pts',(-12.7666378232539,-13.6272926517654,
118.695692434849)) ;
#188634 = CARTESIAN_POINT('Ctrl Pts',(-12.7897753681737,-13.6434155736048,
118.766165664285)) ;
#188635 = CARTESIAN_POINT('Ctrl Pts',(-12.8129129130935,-13.6595384954442,
118.836638893721)) ;
#188636 = CARTESIAN_POINT('Ctrl Pts',(-12.8867167534643,-13.6595385377798,
118.812407842748)) ;
#188637 = CARTESIAN_POINT('Ctrl Pts',(-12.9605205938351,-13.6595385801154,
118.788176791774)) ;
#188638 = CARTESIAN_POINT('Ctrl Pts',(-12.9373830489153,-13.643415658276,
118.717703562338)) ;
#188639 = CARTESIAN_POINT('Ctrl Pts',(-12.933631988452,-13.3531854263633,
118.741726098941)) ;
#188640 = CARTESIAN_POINT('Ctrl Pts',(-12.9099894296058,-13.3573028544331,
118.669714678404)) ;
#188641 = CARTESIAN_POINT('Ctrl Pts',(-12.8361855854579,-13.3573028025058,
118.693945717873)) ;
#188642 = CARTESIAN_POINT('Ctrl Pts',(-12.76238174131,-13.3573027505784,118.718176757342)) ;
#188643 = CARTESIAN_POINT('Ctrl Pts',(-12.7860243001563,-13.3531853225086,
118.790188177879)) ;
#188644 = CARTESIAN_POINT('Ctrl Pts',(-12.8096668590025,-13.3490678944388,
118.862199598417)) ;
#188645 = CARTESIAN_POINT('Ctrl Pts',(-12.8834707031504,-13.3490679463661,
118.837968558948)) ;
#188646 = CARTESIAN_POINT('Ctrl Pts',(-12.9572745472983,-13.3490679982935,
118.813737519479)) ;
#188647 = CARTESIAN_POINT('Ctrl Pts',(-12.933631988452,-13.3531854263633,
118.741726098941)) ;
#188648 = CARTESIAN_POINT('Ctrl Pts',(-12.9056359229119,-13.0673885224611,
118.691923781968)) ;
#188649 = CARTESIAN_POINT('Ctrl Pts',(-12.8831798942909,-13.0914657876093,
118.623526340883)) ;
#188650 = CARTESIAN_POINT('Ctrl Pts',(-12.8093760450123,-13.0914657299476,
118.647757364725)) ;
#188651 = CARTESIAN_POINT('Ctrl Pts',(-12.7355721957337,-13.0914656722859,
118.671988388566)) ;
#188652 = CARTESIAN_POINT('Ctrl Pts',(-12.7580282243547,-13.0673884071377,
118.740385829651)) ;
#188653 = CARTESIAN_POINT('Ctrl Pts',(-12.7804842529757,-13.0433111419895,
118.808783270735)) ;
#188654 = CARTESIAN_POINT('Ctrl Pts',(-12.8542881022543,-13.0433111996512,
118.784552246894)) ;
#188655 = CARTESIAN_POINT('Ctrl Pts',(-12.9280919515329,-13.0433112573129,
118.760321223052)) ;
#188656 = CARTESIAN_POINT('Ctrl Pts',(-12.9056359229119,-13.0673885224611,
118.691923781968)) ;
#188657 = CARTESIAN_POINT('Ctrl Pts',(-12.854527427208,-12.8066409255768,
118.571752043509)) ;
#188658 = CARTESIAN_POINT('Ctrl Pts',(-12.8348726791899,-12.8489579270799,
118.511886850991)) ;
#188659 = CARTESIAN_POINT('Ctrl Pts',(-12.7610688238133,-12.8489578695406,
118.536117856259)) ;
#188660 = CARTESIAN_POINT('Ctrl Pts',(-12.6872649684367,-12.8489578120014,
118.560348861527)) ;
#188661 = CARTESIAN_POINT('Ctrl Pts',(-12.7069197164548,-12.8066408104982,
118.620214054045)) ;
#188662 = CARTESIAN_POINT('Ctrl Pts',(-12.7265744644729,-12.7643238089951,
118.680079246563)) ;
#188663 = CARTESIAN_POINT('Ctrl Pts',(-12.8003783198495,-12.7643238665344,
118.655848241295)) ;
#188664 = CARTESIAN_POINT('Ctrl Pts',(-12.8741821752261,-12.7643239240736,
118.631617236027)) ;
#188665 = CARTESIAN_POINT('Ctrl Pts',(-12.854527427208,-12.8066409255768,
118.571752043509)) ;
#188666 = CARTESIAN_POINT('Ctrl Pts',(-12.7836941512798,-12.5904014103484,
118.391342109483)) ;
#188667 = CARTESIAN_POINT('Ctrl Pts',(-12.7682252464874,-12.6478767369269,
118.344226319916)) ;
#188668 = CARTESIAN_POINT('Ctrl Pts',(-12.6944213851999,-12.6478766870741,
118.368457307181)) ;
#188669 = CARTESIAN_POINT('Ctrl Pts',(-12.6206175239125,-12.6478766372212,
118.392688294445)) ;
#188670 = CARTESIAN_POINT('Ctrl Pts',(-12.6360864287049,-12.5904013106426,
118.439804084012)) ;
#188671 = CARTESIAN_POINT('Ctrl Pts',(-12.6515553334974,-12.5329259840641,
118.486919873579)) ;
#188672 = CARTESIAN_POINT('Ctrl Pts',(-12.7253591947849,-12.5329260339169,
118.462688886314)) ;
#188673 = CARTESIAN_POINT('Ctrl Pts',(-12.7991630560723,-12.5329260837698,
118.43845789905)) ;
#188674 = CARTESIAN_POINT('Ctrl Pts',(-12.7836941512798,-12.5904014103484,
118.391342109483)) ;
#188675 = CARTESIAN_POINT('Ctrl Pts',(-12.6961467508586,-12.4318423089519,
118.160410562632)) ;
#188676 = CARTESIAN_POINT('Ctrl Pts',(-12.6860283059274,-12.500471718984,
118.12959141033)) ;
#188677 = CARTESIAN_POINT('Ctrl Pts',(-12.6122244385164,-12.5004716824447,
118.153822378943)) ;
#188678 = CARTESIAN_POINT('Ctrl Pts',(-12.5384205711053,-12.5004716459054,
118.178053347556)) ;
#188679 = CARTESIAN_POINT('Ctrl Pts',(-12.5485390160365,-12.4318422358733,
118.208872499858)) ;
#188680 = CARTESIAN_POINT('Ctrl Pts',(-12.5586574609676,-12.3632128258413,
118.239691652159)) ;
#188681 = CARTESIAN_POINT('Ctrl Pts',(-12.6324613283787,-12.3632128623805,
118.215460683547)) ;
#188682 = CARTESIAN_POINT('Ctrl Pts',(-12.7062651957898,-12.3632128989198,
118.191229714934)) ;
#188683 = CARTESIAN_POINT('Ctrl Pts',(-12.6961467508586,-12.4318423089519,
118.160410562632)) ;
#188684 = CARTESIAN_POINT('Ctrl Pts',(-12.5994432623834,-12.3456712150683,
117.901136629197)) ;
#188685 = CARTESIAN_POINT('Ctrl Pts',(-12.5953319588446,-12.4204161323536,
117.888614260233)) ;
#188686 = CARTESIAN_POINT('Ctrl Pts',(-12.5215280877492,-12.4204161168077,
117.912845217624)) ;
#188687 = CARTESIAN_POINT('Ctrl Pts',(-12.4477242166539,-12.4204161012619,
117.937076175015)) ;
#188688 = CARTESIAN_POINT('Ctrl Pts',(-12.4518355201927,-12.3456711839767,
117.949598543979)) ;
#188689 = CARTESIAN_POINT('Ctrl Pts',(-12.4559468237315,-12.2709262666914,
117.962120912943)) ;
#188690 = CARTESIAN_POINT('Ctrl Pts',(-12.5297506948269,-12.2709262822373,
117.937889955552)) ;
#188691 = CARTESIAN_POINT('Ctrl Pts',(-12.6035545659222,-12.2709262977831,
117.913658998161)) ;
#188692 = CARTESIAN_POINT('Ctrl Pts',(-12.5994432623834,-12.3456712150683,
117.901136629197)) ;
#188693 = CARTESIAN_POINT('Ctrl Pts',(-12.4981428620814,-12.3353742164119,
117.628067921489)) ;
#188694 = CARTESIAN_POINT('Ctrl Pts',(-12.5003639216367,-12.4109469942247,
117.634832908676)) ;
#188695 = CARTESIAN_POINT('Ctrl Pts',(-12.4265600484705,-12.4109470032869,
117.659063859759)) ;
#188696 = CARTESIAN_POINT('Ctrl Pts',(-12.3527561753044,-12.410947012349,
117.683294810843)) ;
#188697 = CARTESIAN_POINT('Ctrl Pts',(-12.3505351157491,-12.3353742345363,
117.676529823657)) ;
#188698 = CARTESIAN_POINT('Ctrl Pts',(-12.3483140561938,-12.2598014567236,
117.66976483647)) ;
#188699 = CARTESIAN_POINT('Ctrl Pts',(-12.42211792936,-12.2598014476614,117.645533885386)) ;
#188700 = CARTESIAN_POINT('Ctrl Pts',(-12.4959218025261,-12.2598014385992,
117.621302934303)) ;
#188701 = CARTESIAN_POINT('Ctrl Pts',(-12.4981428620814,-12.3353742164119,
117.628067921489)) ;
#188702 = CARTESIAN_POINT('Ctrl Pts',(-12.3992898679553,-12.402733699683,
117.362430521718)) ;
#188703 = CARTESIAN_POINT('Ctrl Pts',(-12.4076821390233,-12.473714122898,
117.387992023362)) ;
#188704 = CARTESIAN_POINT('Ctrl Pts',(-12.3338782663327,-12.4737141587005,
117.412222975894)) ;
#188705 = CARTESIAN_POINT('Ctrl Pts',(-12.2600743936421,-12.473714194503,
117.436453928426)) ;
#188706 = CARTESIAN_POINT('Ctrl Pts',(-12.2516821225741,-12.402733771288,
117.410892426782)) ;
#188707 = CARTESIAN_POINT('Ctrl Pts',(-12.243289851506,-12.331753348073,117.385330925138)) ;
#188708 = CARTESIAN_POINT('Ctrl Pts',(-12.3170937241966,-12.3317533122705,
117.361099972606)) ;
#188709 = CARTESIAN_POINT('Ctrl Pts',(-12.3908975968872,-12.331753276468,
117.336869020074)) ;
#188710 = CARTESIAN_POINT('Ctrl Pts',(-12.3992898679553,-12.402733699683,
117.362430521718)) ;
#188711 = CARTESIAN_POINT('Ctrl Pts',(-12.3089264322979,-12.5432714498278,
117.122757256205)) ;
#188712 = CARTESIAN_POINT('Ctrl Pts',(-12.3229040621412,-12.6045444668254,
117.165330859406)) ;
#188713 = CARTESIAN_POINT('Ctrl Pts',(-12.2491001924915,-12.6045445287426,
117.1895618212)) ;
#188714 = CARTESIAN_POINT('Ctrl Pts',(-12.1752963228417,-12.6045445906598,
117.213792782994)) ;
#188715 = CARTESIAN_POINT('Ctrl Pts',(-12.1613186929985,-12.5432715736621,
117.171219179793)) ;
#188716 = CARTESIAN_POINT('Ctrl Pts',(-12.1473410631552,-12.4819985566645,
117.128645576591)) ;
#188717 = CARTESIAN_POINT('Ctrl Pts',(-12.2211449328049,-12.4819984947474,
117.104414614797)) ;
#188718 = CARTESIAN_POINT('Ctrl Pts',(-12.2949488024546,-12.4819984328302,
117.080183653003)) ;
#188719 = CARTESIAN_POINT('Ctrl Pts',(-12.3089264322979,-12.5432714498278,
117.122757256205)) ;
#188720 = CARTESIAN_POINT('Ctrl Pts',(-12.2333037274479,-12.7462375607508,
116.92788225993)) ;
#188721 = CARTESIAN_POINT('Ctrl Pts',(-12.2518478945764,-12.7934303811122,
116.984364798848)) ;
#188722 = CARTESIAN_POINT('Ctrl Pts',(-12.1780440305619,-12.7934304650843,
117.008595777806)) ;
#188723 = CARTESIAN_POINT('Ctrl Pts',(-12.1042401665475,-12.7934305490564,
117.032826756764)) ;
#188724 = CARTESIAN_POINT('Ctrl Pts',(-12.0856959994191,-12.746237728695,
116.976344217846)) ;
#188725 = CARTESIAN_POINT('Ctrl Pts',(-12.0671518322907,-12.6990449083337,
116.919861678928)) ;
#188726 = CARTESIAN_POINT('Ctrl Pts',(-12.1409556963051,-12.6990448243616,
116.89563069997)) ;
#188727 = CARTESIAN_POINT('Ctrl Pts',(-12.2147595603195,-12.6990447403895,
116.871399721012)) ;
#188728 = CARTESIAN_POINT('Ctrl Pts',(-12.2333037274479,-12.7462375607508,
116.92788225993)) ;
#188729 = CARTESIAN_POINT('Ctrl Pts',(-12.1768490292264,-12.9968255702811,
116.791336954581)) ;
#188730 = CARTESIAN_POINT('Ctrl Pts',(-12.1986293527966,-13.0265927652578,
116.857676303844)) ;
#188731 = CARTESIAN_POINT('Ctrl Pts',(-12.1248254963235,-13.0265928649381,
116.881907305772)) ;
#188732 = CARTESIAN_POINT('Ctrl Pts',(-12.0510216398503,-13.0265929646183,
116.9061383077)) ;
#188733 = CARTESIAN_POINT('Ctrl Pts',(-12.0292413162801,-12.9968257696416,
116.839798958437)) ;
#188734 = CARTESIAN_POINT('Ctrl Pts',(-12.0074609927098,-12.9670585746648,
116.773459609174)) ;
#188735 = CARTESIAN_POINT('Ctrl Pts',(-12.081264849183,-12.9670584749846,
116.749228607246)) ;
#188736 = CARTESIAN_POINT('Ctrl Pts',(-12.1550687056562,-12.9670583753043,
116.724997605318)) ;
#188737 = CARTESIAN_POINT('Ctrl Pts',(-12.1768490292264,-12.9968255702811,
116.791336954581)) ;
#188738 = CARTESIAN_POINT('Ctrl Pts',(-12.1427051117451,-13.2777710794654,
116.722782478303)) ;
#188739 = CARTESIAN_POINT('Ctrl Pts',(-12.1661680895721,-13.2879677234676,
116.794246920931)) ;
#188740 = CARTESIAN_POINT('Ctrl Pts',(-12.0923642418223,-13.2879678309871,
116.818477949429)) ;
#188741 = CARTESIAN_POINT('Ctrl Pts',(-12.0185603940725,-13.2879679385065,
116.842708977927)) ;
#188742 = CARTESIAN_POINT('Ctrl Pts',(-11.9950974162455,-13.2777712945044,
116.771244535298)) ;
#188743 = CARTESIAN_POINT('Ctrl Pts',(-11.9716344384184,-13.2675746505022,
116.69978009267)) ;
#188744 = CARTESIAN_POINT('Ctrl Pts',(-12.0454382861683,-13.2675745429828,
116.675549064172)) ;
#188745 = CARTESIAN_POINT('Ctrl Pts',(-12.1192421339181,-13.2675744354633,
116.651318035675)) ;
#188746 = CARTESIAN_POINT('Ctrl Pts',(-12.1427051117451,-13.2777710794654,
116.722782478303)) ;
#188747 = CARTESIAN_POINT('Ctrl Pts',(-12.132619814381,-13.5692121151867,
116.72755803208)) ;
#188748 = CARTESIAN_POINT('Ctrl Pts',(-12.1560873514429,-13.5590766136152,
116.799036361418)) ;
#188749 = CARTESIAN_POINT('Ctrl Pts',(-12.0822835127583,-13.5590767201184,
116.823267417527)) ;
#188750 = CARTESIAN_POINT('Ctrl Pts',(-12.0084796740738,-13.5590768266217,
116.847498473636)) ;
#188751 = CARTESIAN_POINT('Ctrl Pts',(-11.9850121370119,-13.5692123281932,
116.776020144298)) ;
#188752 = CARTESIAN_POINT('Ctrl Pts',(-11.9615445999501,-13.5793478297647,
116.70454181496)) ;
#188753 = CARTESIAN_POINT('Ctrl Pts',(-12.0353484386346,-13.5793477232615,
116.680310758851)) ;
#188754 = CARTESIAN_POINT('Ctrl Pts',(-12.1091522773192,-13.5793476167582,
116.656079702742)) ;
#188755 = CARTESIAN_POINT('Ctrl Pts',(-12.132619814381,-13.5692121151867,
116.72755803208)) ;
#188756 = CARTESIAN_POINT('Ctrl Pts',(-12.1467639143516,-13.8503430324929,
116.806211060665)) ;
#188757 = CARTESIAN_POINT('Ctrl Pts',(-12.1685429840334,-13.8205648157971,
116.872546590843)) ;
#188758 = CARTESIAN_POINT('Ctrl Pts',(-12.094739153736,-13.8205649121888,
116.896777672498)) ;
#188759 = CARTESIAN_POINT('Ctrl Pts',(-12.0209353234386,-13.8205650085804,
116.921008754153)) ;
#188760 = CARTESIAN_POINT('Ctrl Pts',(-11.9991562537568,-13.8503432252762,
116.854673223975)) ;
#188761 = CARTESIAN_POINT('Ctrl Pts',(-11.977377184075,-13.880121441972,116.788337693796)) ;
#188762 = CARTESIAN_POINT('Ctrl Pts',(-12.0511810143725,-13.8801213455804,
116.764106612141)) ;
#188763 = CARTESIAN_POINT('Ctrl Pts',(-12.1249848446699,-13.8801212491888,
116.739875530486)) ;
#188764 = CARTESIAN_POINT('Ctrl Pts',(-12.1467639143516,-13.8503430324929,
116.806211060665)) ;
#188765 = CARTESIAN_POINT('Ctrl Pts',(-12.1829893801448,-14.0986233529731,
116.951857724496)) ;
#188766 = CARTESIAN_POINT('Ctrl Pts',(-12.2015410509572,-14.0514664875456,
117.008363118508)) ;
#188767 = CARTESIAN_POINT('Ctrl Pts',(-12.1277372276301,-14.0514665673178,
117.032594221393)) ;
#188768 = CARTESIAN_POINT('Ctrl Pts',(-12.0539334043031,-14.05146664709,117.056825324279)) ;
#188769 = CARTESIAN_POINT('Ctrl Pts',(-12.0353817334907,-14.0986235125175,
117.000319930267)) ;
#188770 = CARTESIAN_POINT('Ctrl Pts',(-12.0168300626784,-14.145780377945,
116.943814536255)) ;
#188771 = CARTESIAN_POINT('Ctrl Pts',(-12.0906338860054,-14.1457802981728,
116.919583433369)) ;
#188772 = CARTESIAN_POINT('Ctrl Pts',(-12.1644377093324,-14.1457802184006,
116.895352330483)) ;
#188773 = CARTESIAN_POINT('Ctrl Pts',(-12.1829893801448,-14.0986233529731,
116.951857724496)) ;
#188774 = CARTESIAN_POINT('Ctrl Pts',(-12.2382733903879,-14.2995832696182,
117.155728549187)) ;
#188775 = CARTESIAN_POINT('Ctrl Pts',(-12.2522588615321,-14.2383253097085,
117.198326035843)) ;
#188776 = CARTESIAN_POINT('Ctrl Pts',(-12.1784550430804,-14.2383253669594,
117.222557153578)) ;
#188777 = CARTESIAN_POINT('Ctrl Pts',(-12.1046512246287,-14.2383254242103,
117.246788271313)) ;
#188778 = CARTESIAN_POINT('Ctrl Pts',(-12.0906657534845,-14.29958338412,117.204190784657)) ;
#188779 = CARTESIAN_POINT('Ctrl Pts',(-12.0766802823402,-14.3608413440297,
117.161593298)) ;
#188780 = CARTESIAN_POINT('Ctrl Pts',(-12.1504841007919,-14.3608412867788,
117.137362180265)) ;
#188781 = CARTESIAN_POINT('Ctrl Pts',(-12.2242879192436,-14.3608412295279,
117.11313106253)) ;
#188782 = CARTESIAN_POINT('Ctrl Pts',(-12.2382733903879,-14.2995832696182,
117.155728549187)) ;
#188783 = CARTESIAN_POINT('Ctrl Pts',(-12.3080272802778,-14.4373031232107,
117.403743324184)) ;
#188784 = CARTESIAN_POINT('Ctrl Pts',(-12.3164280476558,-14.3663375815008,
117.42933070437)) ;
#188785 = CARTESIAN_POINT('Ctrl Pts',(-12.2426242313647,-14.3663376133963,
117.453561828685)) ;
#188786 = CARTESIAN_POINT('Ctrl Pts',(-12.1688204150736,-14.3663376452917,
117.477792953001)) ;
#188787 = CARTESIAN_POINT('Ctrl Pts',(-12.1604196476955,-14.4373031870016,
117.452205572816)) ;
#188788 = CARTESIAN_POINT('Ctrl Pts',(-12.1520188803175,-14.5082687287115,
117.426618192631)) ;
#188789 = CARTESIAN_POINT('Ctrl Pts',(-12.2258226966086,-14.5082686968161,
117.402387068315)) ;
#188790 = CARTESIAN_POINT('Ctrl Pts',(-12.2996265128997,-14.5082686649206,
117.378155943999)) ;
#188791 = CARTESIAN_POINT('Ctrl Pts',(-12.3080272802778,-14.4373031232107,
117.403743324184)) ;
#188792 = CARTESIAN_POINT('Ctrl Pts',(-12.3858324941963,-14.5016051754735,
117.676070811341)) ;
#188793 = CARTESIAN_POINT('Ctrl Pts',(-12.3880822552564,-14.4260436157556,
117.682923218844)) ;
#188794 = CARTESIAN_POINT('Ctrl Pts',(-12.3142784389973,-14.4260436229732,
117.707154343258)) ;
#188795 = CARTESIAN_POINT('Ctrl Pts',(-12.2404746227383,-14.4260436301907,
117.731385467671)) ;
#188796 = CARTESIAN_POINT('Ctrl Pts',(-12.2382248616783,-14.5016051899087,
117.724533060168)) ;
#188797 = CARTESIAN_POINT('Ctrl Pts',(-12.2359751006182,-14.5771667496267,
117.717680652665)) ;
#188798 = CARTESIAN_POINT('Ctrl Pts',(-12.3097789168773,-14.5771667424091,
117.693449528252)) ;
#188799 = CARTESIAN_POINT('Ctrl Pts',(-12.3835827331363,-14.5771667351915,
117.669218403838)) ;
#188800 = CARTESIAN_POINT('Ctrl Pts',(-12.3858324941963,-14.5016051754735,
117.676070811341)) ;
#188801 = CARTESIAN_POINT('Ctrl Pts',(-12.4662324280866,-14.4885235205326,
117.956501349458)) ;
#188802 = CARTESIAN_POINT('Ctrl Pts',(-12.4621366687095,-14.4137610040608,
117.9440263257)) ;
#188803 = CARTESIAN_POINT('Ctrl Pts',(-12.3883328497861,-14.4137609891403,
117.968257441998)) ;
#188804 = CARTESIAN_POINT('Ctrl Pts',(-12.3145290308627,-14.4137609742198,
117.992488558297)) ;
#188805 = CARTESIAN_POINT('Ctrl Pts',(-12.3186247902397,-14.4885234906916,
118.004963582055)) ;
#188806 = CARTESIAN_POINT('Ctrl Pts',(-12.3227205496168,-14.5632860071634,
118.017438605813)) ;
#188807 = CARTESIAN_POINT('Ctrl Pts',(-12.3965243685402,-14.5632860220839,
117.993207489514)) ;
#188808 = CARTESIAN_POINT('Ctrl Pts',(-12.4703281874636,-14.5632860370044,
117.968976373216)) ;
#188809 = CARTESIAN_POINT('Ctrl Pts',(-12.4662324280866,-14.4885235205326,
117.956501349458)) ;
#188810 = CARTESIAN_POINT('Ctrl Pts',(-12.542015891352,-14.3988909925641,
118.222731825387)) ;
#188811 = CARTESIAN_POINT('Ctrl Pts',(-12.5318901459169,-14.3302736656516,
118.191890437167)) ;
#188812 = CARTESIAN_POINT('Ctrl Pts',(-12.4580863228816,-14.3302736334562,
118.216121540941)) ;
#188813 = CARTESIAN_POINT('Ctrl Pts',(-12.3842824998462,-14.3302736012609,
118.240352644715)) ;
#188814 = CARTESIAN_POINT('Ctrl Pts',(-12.3944082452813,-14.3988909281734,
118.271194032935)) ;
#188815 = CARTESIAN_POINT('Ctrl Pts',(-12.4045339907163,-14.4675082550859,
118.302035421155)) ;
#188816 = CARTESIAN_POINT('Ctrl Pts',(-12.4783378137517,-14.4675082872812,
118.277804317381)) ;
#188817 = CARTESIAN_POINT('Ctrl Pts',(-12.552141636787,-14.4675083194766,
118.253573213606)) ;
#188818 = CARTESIAN_POINT('Ctrl Pts',(-12.542015891352,-14.3988909925641,
118.222731825387)) ;
#188819 = CARTESIAN_POINT('Ctrl Pts',(-12.6075687803781,-14.2382785177405,
118.457972969816)) ;
#188820 = CARTESIAN_POINT('Ctrl Pts',(-12.5921145495609,-14.1807709154062,
118.410901875046)) ;
#188821 = CARTESIAN_POINT('Ctrl Pts',(-12.5183107209811,-14.180770872992,
118.435132961933)) ;
#188822 = CARTESIAN_POINT('Ctrl Pts',(-12.4445068924013,-14.1807708305777,
118.459364048819)) ;
#188823 = CARTESIAN_POINT('Ctrl Pts',(-12.4599611232185,-14.2382784329119,
118.506435143589)) ;
#188824 = CARTESIAN_POINT('Ctrl Pts',(-12.4754153540358,-14.2957860352462,
118.553506238358)) ;
#188825 = CARTESIAN_POINT('Ctrl Pts',(-12.5492191826155,-14.2957860776604,
118.529275151471)) ;
#188826 = CARTESIAN_POINT('Ctrl Pts',(-12.6230230111953,-14.2957861200747,
118.505044064585)) ;
#188827 = CARTESIAN_POINT('Ctrl Pts',(-12.6075687803781,-14.2382785177405,
118.457972969816)) ;
#188828 = CARTESIAN_POINT('Ctrl Pts',(-12.6567934735026,-14.0201835577284,
118.643239416327)) ;
#188829 = CARTESIAN_POINT('Ctrl Pts',(-12.6371477842982,-13.9778166138277,
118.58340181574)) ;
#188830 = CARTESIAN_POINT('Ctrl Pts',(-12.5633439504344,-13.9778165664169,
118.607632886532)) ;
#188831 = CARTESIAN_POINT('Ctrl Pts',(-12.4895401165705,-13.9778165190061,
118.631863957324)) ;
#188832 = CARTESIAN_POINT('Ctrl Pts',(-12.5091858057748,-14.0201834629068,
118.691701557911)) ;
#188833 = CARTESIAN_POINT('Ctrl Pts',(-12.5288314949792,-14.0625504068075,
118.751539158498)) ;
#188834 = CARTESIAN_POINT('Ctrl Pts',(-12.6026353288431,-14.0625504542183,
118.727308087706)) ;
#188835 = CARTESIAN_POINT('Ctrl Pts',(-12.6764391627069,-14.0625505016291,
118.703077016914)) ;
#188836 = CARTESIAN_POINT('Ctrl Pts',(-12.6567934735026,-14.0201835577284,
118.643239416327)) ;
#188837 = CARTESIAN_POINT('Ctrl Pts',(-12.6860528811102,-13.7575805640437,
118.767919765883)) ;
#188838 = CARTESIAN_POINT('Ctrl Pts',(-12.6635985131685,-13.7334844884055,
118.699527383226)) ;
#188839 = CARTESIAN_POINT('Ctrl Pts',(-12.5897946740628,-13.7334844436557,
118.723758438053)) ;
#188840 = CARTESIAN_POINT('Ctrl Pts',(-12.515990834957,-13.7334843989059,
118.747989492879)) ;
#188841 = CARTESIAN_POINT('Ctrl Pts',(-12.5384452028988,-13.7575804745442,
118.816381875535)) ;
#188842 = CARTESIAN_POINT('Ctrl Pts',(-12.5608995708405,-13.7816765501825,
118.884774258192)) ;
#188843 = CARTESIAN_POINT('Ctrl Pts',(-12.6347034099462,-13.7816765949322,
118.860543203365)) ;
#188844 = CARTESIAN_POINT('Ctrl Pts',(-12.7085072490519,-13.781676639682,
118.836312148539)) ;
#188845 = CARTESIAN_POINT('Ctrl Pts',(-12.6860528811102,-13.7575805640437,
118.767919765883)) ;
#188846 = CARTESIAN_POINT('Ctrl Pts',(-12.6920563199496,-13.4715356144856,
118.821634228625)) ;
#188847 = CARTESIAN_POINT('Ctrl Pts',(-12.6684156000948,-13.467375361388,
118.74962840962)) ;
#188848 = CARTESIAN_POINT('Ctrl Pts',(-12.5946117570558,-13.4673753229371,
118.773859452466)) ;
#188849 = CARTESIAN_POINT('Ctrl Pts',(-12.5208079140168,-13.4673752844861,
118.798090495312)) ;
#188850 = CARTESIAN_POINT('Ctrl Pts',(-12.5444486338716,-13.4715355375837,
118.870096314318)) ;
#188851 = CARTESIAN_POINT('Ctrl Pts',(-12.5680893537264,-13.4756957906813,
118.942102133323)) ;
#188852 = CARTESIAN_POINT('Ctrl Pts',(-12.6418931967654,-13.4756958291323,
118.917871090476)) ;
#188853 = CARTESIAN_POINT('Ctrl Pts',(-12.7156970398044,-13.4756958675833,
118.89364004763)) ;
#188854 = CARTESIAN_POINT('Ctrl Pts',(-12.6920563199496,-13.4715356144856,
118.821634228625)) ;
#188855 = CARTESIAN_POINT('Ctrl Pts',(-12.6739055959979,-13.1815808813972,
118.801789101295)) ;
#188856 = CARTESIAN_POINT('Ctrl Pts',(-12.650763023528,-13.1976597435624,
118.731300559009)) ;
#188857 = CARTESIAN_POINT('Ctrl Pts',(-12.5769591778132,-13.1976597143198,
118.755531593705)) ;
#188858 = CARTESIAN_POINT('Ctrl Pts',(-12.5031553320983,-13.1976596850772,
118.779762628401)) ;
#188859 = CARTESIAN_POINT('Ctrl Pts',(-12.5262979045681,-13.1815808229121,
118.850251170687)) ;
#188860 = CARTESIAN_POINT('Ctrl Pts',(-12.549440477038,-13.1655019607469,
118.920739712973)) ;
#188861 = CARTESIAN_POINT('Ctrl Pts',(-12.6232443227529,-13.1655019899895,
118.896508678276)) ;
#188862 = CARTESIAN_POINT('Ctrl Pts',(-12.6970481684677,-13.1655020192321,
118.872277643581)) ;
#188863 = CARTESIAN_POINT('Ctrl Pts',(-12.6739055959979,-13.1815808813972,
118.801789101295)) ;
#188864 = CARTESIAN_POINT('Ctrl Pts',(-12.6316959301711,-12.9071949482228,
118.708856292433)) ;
#188865 = CARTESIAN_POINT('Ctrl Pts',(-12.6107280772881,-12.9424572144763,
118.644991595303)) ;
#188866 = CARTESIAN_POINT('Ctrl Pts',(-12.5369242306686,-12.9424571966172,
118.669222627244)) ;
#188867 = CARTESIAN_POINT('Ctrl Pts',(-12.4631203840491,-12.9424571787581,
118.693453659185)) ;
#188868 = CARTESIAN_POINT('Ctrl Pts',(-12.4840882369321,-12.9071949125046,
118.757318356314)) ;
#188869 = CARTESIAN_POINT('Ctrl Pts',(-12.5050560898151,-12.8719326462511,
118.821183053443)) ;
#188870 = CARTESIAN_POINT('Ctrl Pts',(-12.5788599364347,-12.8719326641102,
118.796952021502)) ;
#188871 = CARTESIAN_POINT('Ctrl Pts',(-12.6526637830542,-12.8719326819694,
118.772720989562)) ;
#188872 = CARTESIAN_POINT('Ctrl Pts',(-12.6316959301711,-12.9071949482228,
118.708856292433)) ;
#188873 = CARTESIAN_POINT('Ctrl Pts',(-12.5685224634978,-12.6718251326146,
118.551729535265)) ;
#188874 = CARTESIAN_POINT('Ctrl Pts',(-12.5512038301306,-12.723574947821,
118.498979772095)) ;
#188875 = CARTESIAN_POINT('Ctrl Pts',(-12.4773999834557,-12.7235749374657,
118.523210803867)) ;
#188876 = CARTESIAN_POINT('Ctrl Pts',(-12.4035961367808,-12.7235749271105,
118.547441835638)) ;
#188877 = CARTESIAN_POINT('Ctrl Pts',(-12.420914770148,-12.6718251119041,
118.600191598809)) ;
#188878 = CARTESIAN_POINT('Ctrl Pts',(-12.4382334035152,-12.6200752966978,
118.652941361979)) ;
#188879 = CARTESIAN_POINT('Ctrl Pts',(-12.5120372501901,-12.620075307053,
118.628710330207)) ;
#188880 = CARTESIAN_POINT('Ctrl Pts',(-12.585841096865,-12.6200753174082,
118.604479298435)) ;
#188881 = CARTESIAN_POINT('Ctrl Pts',(-12.5685224634978,-12.6718251326146,
118.551729535265)) ;
#188882 = CARTESIAN_POINT('Ctrl Pts',(-12.4874902277502,-12.4884732056212,
118.340373479315)) ;
#188883 = CARTESIAN_POINT('Ctrl Pts',(-12.4750698575582,-12.553103678643,
118.302543035572)) ;
#188884 = CARTESIAN_POINT('Ctrl Pts',(-12.4012660118782,-12.5531036749217,
118.326774070374)) ;
#188885 = CARTESIAN_POINT('Ctrl Pts',(-12.3274621661981,-12.5531036712005,
118.351005105176)) ;
#188886 = CARTESIAN_POINT('Ctrl Pts',(-12.33988253639,-12.4884731981787,118.388835548919)) ;
#188887 = CARTESIAN_POINT('Ctrl Pts',(-12.3523029065819,-12.4238427251569,
118.426665992661)) ;
#188888 = CARTESIAN_POINT('Ctrl Pts',(-12.426106752262,-12.4238427288782,
118.402434957859)) ;
#188889 = CARTESIAN_POINT('Ctrl Pts',(-12.4999105979421,-12.4238427325995,
118.378203923057)) ;
#188890 = CARTESIAN_POINT('Ctrl Pts',(-12.4874902277502,-12.4884732056212,
118.340373479315)) ;
#188891 = CARTESIAN_POINT('Ctrl Pts',(-12.3934765958688,-12.3715751089405,
118.089586721581)) ;
#188892 = CARTESIAN_POINT('Ctrl Pts',(-12.3868662577331,-12.4444657268571,
118.06945269815)) ;
#188893 = CARTESIAN_POINT('Ctrl Pts',(-12.3130624136099,-12.4444657266469,
118.093683737694)) ;
#188894 = CARTESIAN_POINT('Ctrl Pts',(-12.2392585694866,-12.4444657264366,
118.117914777237)) ;
#188895 = CARTESIAN_POINT('Ctrl Pts',(-12.2458689076223,-12.3715751085199,
118.138048800668)) ;
#188896 = CARTESIAN_POINT('Ctrl Pts',(-12.2524792457579,-12.2986844906033,
118.158182824099)) ;
#188897 = CARTESIAN_POINT('Ctrl Pts',(-12.3262830898812,-12.2986844908136,
118.133951784556)) ;
#188898 = CARTESIAN_POINT('Ctrl Pts',(-12.4000869340045,-12.2986844910239,
118.109720745012)) ;
#188899 = CARTESIAN_POINT('Ctrl Pts',(-12.3934765958688,-12.3715751089405,
118.089586721581)) ;
#188900 = CARTESIAN_POINT('Ctrl Pts',(-12.293164555208,-12.3301226383043,
117.819480325447)) ;
#188901 = CARTESIAN_POINT('Ctrl Pts',(-12.292815707975,-12.4060167548224,
117.818417793086)) ;
#188902 = CARTESIAN_POINT('Ctrl Pts',(-12.2190118649512,-12.4060167550604,
117.842648835978)) ;
#188903 = CARTESIAN_POINT('Ctrl Pts',(-12.1452080219273,-12.4060167552985,
117.866879878871)) ;
#188904 = CARTESIAN_POINT('Ctrl Pts',(-12.1455568691603,-12.3301226387804,
117.867942411232)) ;
#188905 = CARTESIAN_POINT('Ctrl Pts',(-12.1459057163933,-12.2542285222622,
117.869004943594)) ;
#188906 = CARTESIAN_POINT('Ctrl Pts',(-12.2197095594172,-12.2542285220242,
117.844773900702)) ;
#188907 = CARTESIAN_POINT('Ctrl Pts',(-12.293513402441,-12.2542285217862,
117.820542857809)) ;
#188908 = CARTESIAN_POINT('Ctrl Pts',(-12.293164555208,-12.3301226383043,
117.819480325447)) ;
#188909 = CARTESIAN_POINT('Ctrl Pts',(-12.19274645429,-12.3662578527564,117.549013076406)) ;
#188910 = CARTESIAN_POINT('Ctrl Pts',(-12.1986766714654,-12.4397415757967,
117.567075561145)) ;
#188911 = CARTESIAN_POINT('Ctrl Pts',(-12.1248728290033,-12.4397415751055,
117.591306605748)) ;
#188912 = CARTESIAN_POINT('Ctrl Pts',(-12.0510689865413,-12.4397415744144,
117.615537650352)) ;
#188913 = CARTESIAN_POINT('Ctrl Pts',(-12.0451387693659,-12.366257851374,
117.597475165613)) ;
#188914 = CARTESIAN_POINT('Ctrl Pts',(-12.0392085521905,-12.2927741283337,
117.579412680873)) ;
#188915 = CARTESIAN_POINT('Ctrl Pts',(-12.1130123946526,-12.2927741290249,
117.55518163627)) ;
#188916 = CARTESIAN_POINT('Ctrl Pts',(-12.1868162371146,-12.2927741297161,
117.530950591666)) ;
#188917 = CARTESIAN_POINT('Ctrl Pts',(-12.19274645429,-12.3662578527564,117.549013076406)) ;
#188918 = CARTESIAN_POINT('Ctrl Pts',(-12.0982790904957,-12.4776432814408,
117.296753345716)) ;
#188919 = CARTESIAN_POINT('Ctrl Pts',(-12.1100806154141,-12.5434578807603,
117.33269888651)) ;
#188920 = CARTESIAN_POINT('Ctrl Pts',(-12.0362767728468,-12.5434578790229,
117.356929930793)) ;
#188921 = CARTESIAN_POINT('Ctrl Pts',(-11.9624729302794,-12.5434578772856,
117.381160975076)) ;
#188922 = CARTESIAN_POINT('Ctrl Pts',(-11.950671405361,-12.477643277966,117.345215434282)) ;
#188923 = CARTESIAN_POINT('Ctrl Pts',(-11.9388698804425,-12.4118286786465,
117.309269893487)) ;
#188924 = CARTESIAN_POINT('Ctrl Pts',(-12.0126737230099,-12.4118286803839,
117.285038849205)) ;
#188925 = CARTESIAN_POINT('Ctrl Pts',(-12.0864775655773,-12.4118286821212,
117.260807804922)) ;
#188926 = CARTESIAN_POINT('Ctrl Pts',(-12.0982790904957,-12.4776432814408,
117.296753345716)) ;
#188927 = CARTESIAN_POINT('Ctrl Pts',(-12.0157313689232,-12.6576066827307,
117.080968227054)) ;
#188928 = CARTESIAN_POINT('Ctrl Pts',(-12.0325769790524,-12.71095179343,117.132277237482)) ;
#188929 = CARTESIAN_POINT('Ctrl Pts',(-11.9587731356166,-12.7109517930547,
117.15650827912)) ;
#188930 = CARTESIAN_POINT('Ctrl Pts',(-11.8849692921809,-12.7109517926794,
117.180739320758)) ;
#188931 = CARTESIAN_POINT('Ctrl Pts',(-11.8681236820516,-12.6576066819802,
117.12943031033)) ;
#188932 = CARTESIAN_POINT('Ctrl Pts',(-11.8512780719223,-12.604261571281,
117.078121299901)) ;
#188933 = CARTESIAN_POINT('Ctrl Pts',(-11.9250819153581,-12.6042615716562,
117.053890258263)) ;
#188934 = CARTESIAN_POINT('Ctrl Pts',(-11.9988857587939,-12.6042615720315,
117.029659216626)) ;
#188935 = CARTESIAN_POINT('Ctrl Pts',(-12.0157313689232,-12.6576066827307,
117.080968227054)) ;
#188936 = CARTESIAN_POINT('Ctrl Pts',(-11.9512285219355,-12.8904240369604,
116.919843926317)) ;
#188937 = CARTESIAN_POINT('Ctrl Pts',(-11.9718712658943,-12.9275904125638,
116.982718393653)) ;
#188938 = CARTESIAN_POINT('Ctrl Pts',(-11.8980674218478,-12.9275904154763,
117.00694943343)) ;
#188939 = CARTESIAN_POINT('Ctrl Pts',(-11.8242635778013,-12.9275904183888,
117.031180473208)) ;
#188940 = CARTESIAN_POINT('Ctrl Pts',(-11.8036208338425,-12.8904240427854,
116.968306005872)) ;
#188941 = CARTESIAN_POINT('Ctrl Pts',(-11.7829780898837,-12.853257667182,
116.905431538537)) ;
#188942 = CARTESIAN_POINT('Ctrl Pts',(-11.8567819339302,-12.8532576642695,
116.881200498759)) ;
#188943 = CARTESIAN_POINT('Ctrl Pts',(-11.9305857779767,-12.853257661357,
116.856969458981)) ;
#188944 = CARTESIAN_POINT('Ctrl Pts',(-11.9512285219355,-12.8904240369604,
116.919843926317)) ;
#188945 = CARTESIAN_POINT('Ctrl Pts',(-11.9077036102862,-13.1612401483887,
116.822691378443)) ;
#188946 = CARTESIAN_POINT('Ctrl Pts',(-11.9306826023252,-13.1795510816038,
116.892681680379)) ;
#188947 = CARTESIAN_POINT('Ctrl Pts',(-11.8568787581112,-13.1795510898929,
116.916912719647)) ;
#188948 = CARTESIAN_POINT('Ctrl Pts',(-11.7830749138971,-13.1795510981819,
116.941143758914)) ;
#188949 = CARTESIAN_POINT('Ctrl Pts',(-11.7600959218581,-13.1612401649668,
116.871153456977)) ;
#188950 = CARTESIAN_POINT('Ctrl Pts',(-11.737116929819,-13.1429292317516,
116.80116315504)) ;
#188951 = CARTESIAN_POINT('Ctrl Pts',(-11.8109207740331,-13.1429292234626,
116.776932115773)) ;
#188952 = CARTESIAN_POINT('Ctrl Pts',(-11.8847246182471,-13.1429292151735,
116.752701076506)) ;
#188953 = CARTESIAN_POINT('Ctrl Pts',(-11.9077036102862,-13.1612401483887,
116.822691378443)) ;
#188954 = CARTESIAN_POINT('Ctrl Pts',(-11.8877528191562,-13.4512163582634,
116.79743209915)) ;
#188955 = CARTESIAN_POINT('Ctrl Pts',(-11.9114235075367,-13.4493066869731,
116.869529196403)) ;
#188956 = CARTESIAN_POINT('Ctrl Pts',(-11.8376196640733,-13.4493067026551,
116.893760237956)) ;
#188957 = CARTESIAN_POINT('Ctrl Pts',(-11.76381582061,-13.4493067183372,116.91799127951)) ;
#188958 = CARTESIAN_POINT('Ctrl Pts',(-11.7401451322294,-13.4512163896275,
116.845894182257)) ;
#188959 = CARTESIAN_POINT('Ctrl Pts',(-11.7164744438488,-13.4531260609178,
116.773797085004)) ;
#188960 = CARTESIAN_POINT('Ctrl Pts',(-11.7902782873122,-13.4531260452357,
116.74956604345)) ;
#188961 = CARTESIAN_POINT('Ctrl Pts',(-11.8640821307756,-13.4531260295536,
116.725335001897)) ;
#188962 = CARTESIAN_POINT('Ctrl Pts',(-11.8877528191562,-13.4512163582634,
116.79743209915)) ;
#188963 = CARTESIAN_POINT('Ctrl Pts',(-11.8921420096609,-13.7384260494091,
116.846260536763)) ;
#188964 = CARTESIAN_POINT('Ctrl Pts',(-11.9148067679452,-13.7164599573725,
116.915293733103)) ;
#188965 = CARTESIAN_POINT('Ctrl Pts',(-11.8410029264598,-13.7164599797673,
116.939524780681)) ;
#188966 = CARTESIAN_POINT('Ctrl Pts',(-11.7671990849745,-13.7164600021621,
116.963755828259)) ;
#188967 = CARTESIAN_POINT('Ctrl Pts',(-11.7445343266902,-13.7384260941987,
116.89472263192)) ;
#188968 = CARTESIAN_POINT('Ctrl Pts',(-11.721869568406,-13.7603921862353,
116.82568943558)) ;
#188969 = CARTESIAN_POINT('Ctrl Pts',(-11.7956734098913,-13.7603921638405,
116.801458388001)) ;
#188970 = CARTESIAN_POINT('Ctrl Pts',(-11.8694772513767,-13.7603921414456,
116.777227340423)) ;
#188971 = CARTESIAN_POINT('Ctrl Pts',(-11.8921420096609,-13.7384260494091,
116.846260536763)) ;
#188972 = CARTESIAN_POINT('Ctrl Pts',(-11.9197697611465,-14.0027479972631,
116.965881508677)) ;
#188973 = CARTESIAN_POINT('Ctrl Pts',(-11.939804311693,-13.9622948022858,
117.02690351647)) ;
#188974 = CARTESIAN_POINT('Ctrl Pts',(-11.8660004733724,-13.962294829201,
117.051134573688)) ;
#188975 = CARTESIAN_POINT('Ctrl Pts',(-11.7921966350518,-13.9622948561163,
117.075365630906)) ;
#188976 = CARTESIAN_POINT('Ctrl Pts',(-11.7721620845053,-14.0027480510937,
117.014343623112)) ;
#188977 = CARTESIAN_POINT('Ctrl Pts',(-11.7521275339589,-14.0432012460711,
116.953321615319)) ;
#188978 = CARTESIAN_POINT('Ctrl Pts',(-11.8259313722795,-14.0432012191558,
116.929090558101)) ;
#188979 = CARTESIAN_POINT('Ctrl Pts',(-11.8997352106001,-14.0432011922405,
116.904859500883)) ;
#188980 = CARTESIAN_POINT('Ctrl Pts',(-11.9197697611465,-14.0027479972631,
116.965881508677)) ;
#188981 = CARTESIAN_POINT('Ctrl Pts',(-11.9678037086644,-14.2248634912547,
117.147598095)) ;
#188982 = CARTESIAN_POINT('Ctrl Pts',(-11.9837806505396,-14.1688437545673,
117.196261281318)) ;
#188983 = CARTESIAN_POINT('Ctrl Pts',(-11.9099768161194,-14.1688437816251,
117.220492350416)) ;
#188984 = CARTESIAN_POINT('Ctrl Pts',(-11.8361729816992,-14.168843808683,
117.244723419513)) ;
#188985 = CARTESIAN_POINT('Ctrl Pts',(-11.820196039824,-14.2248635453705,
117.196060233195)) ;
#188986 = CARTESIAN_POINT('Ctrl Pts',(-11.8042190979487,-14.2808832820579,
117.147397046877)) ;
#188987 = CARTESIAN_POINT('Ctrl Pts',(-11.8780229323689,-14.2808832550001,
117.123165977779)) ;
#188988 = CARTESIAN_POINT('Ctrl Pts',(-11.9518267667891,-14.2808832279422,
117.098934908682)) ;
#188989 = CARTESIAN_POINT('Ctrl Pts',(-11.9678037086644,-14.2248634912547,
117.147598095)) ;
#188990 = CARTESIAN_POINT('Ctrl Pts',(-12.0322684953334,-14.3897502001773,
117.379450247852)) ;
#188991 = CARTESIAN_POINT('Ctrl Pts',(-12.0430330101594,-14.3221371212432,
117.412237222224)) ;
#188992 = CARTESIAN_POINT('Ctrl Pts',(-11.9692291801814,-14.3221371438564,
117.436468304852)) ;
#188993 = CARTESIAN_POINT('Ctrl Pts',(-11.8954253502033,-14.3221371664696,
117.460699387479)) ;
#188994 = CARTESIAN_POINT('Ctrl Pts',(-11.8846608353774,-14.3897502454037,
117.427912413107)) ;
#188995 = CARTESIAN_POINT('Ctrl Pts',(-11.8738963205514,-14.4573633243378,
117.395125438735)) ;
#188996 = CARTESIAN_POINT('Ctrl Pts',(-11.9477001505294,-14.4573633017246,
117.370894356107)) ;
#188997 = CARTESIAN_POINT('Ctrl Pts',(-12.0215039805075,-14.4573632791114,
117.34666327348)) ;
#188998 = CARTESIAN_POINT('Ctrl Pts',(-12.0322684953334,-14.3897502001773,
117.379450247852)) ;
#188999 = CARTESIAN_POINT('Ctrl Pts',(-12.107744276387,-14.4847583322739,
117.644855028012)) ;
#189000 = CARTESIAN_POINT('Ctrl Pts',(-12.1125197986048,-14.4104140333925,
117.659400497042)) ;
#189001 = CARTESIAN_POINT('Ctrl Pts',(-12.0387159728293,-14.4104140454356,
117.68363159247)) ;
#189002 = CARTESIAN_POINT('Ctrl Pts',(-11.9649121470538,-14.4104140574787,
117.707862687898)) ;
#189003 = CARTESIAN_POINT('Ctrl Pts',(-11.960136624836,-14.4847583563601,
117.693317218868)) ;
#189004 = CARTESIAN_POINT('Ctrl Pts',(-11.9553611026181,-14.5591026552415,
117.678771749837)) ;
#189005 = CARTESIAN_POINT('Ctrl Pts',(-12.0291649283937,-14.5591026431984,
117.654540654409)) ;
#189006 = CARTESIAN_POINT('Ctrl Pts',(-12.1029687541692,-14.5591026311553,
117.630309558981)) ;
#189007 = CARTESIAN_POINT('Ctrl Pts',(-12.107744276387,-14.4847583322739,
117.644855028012)) ;
#189008 = CARTESIAN_POINT('Ctrl Pts',(-12.1876872494525,-14.5032991769,117.923727178985)) ;
#189009 = CARTESIAN_POINT('Ctrl Pts',(-12.1861561390636,-14.4275531479525,
117.91906366252)) ;
#189010 = CARTESIAN_POINT('Ctrl Pts',(-12.1123523160226,-14.4275531440522,
117.943294766276)) ;
#189011 = CARTESIAN_POINT('Ctrl Pts',(-12.0385484929815,-14.427553140152,
117.967525870033)) ;
#189012 = CARTESIAN_POINT('Ctrl Pts',(-12.0400796033704,-14.5032991690996,
117.972189386498)) ;
#189013 = CARTESIAN_POINT('Ctrl Pts',(-12.0416107137593,-14.5790451980471,
117.976852902963)) ;
#189014 = CARTESIAN_POINT('Ctrl Pts',(-12.1154145368004,-14.5790452019473,
117.952621799206)) ;
#189015 = CARTESIAN_POINT('Ctrl Pts',(-12.1892183598415,-14.5790452058476,
117.928390695449)) ;
#189016 = CARTESIAN_POINT('Ctrl Pts',(-12.1876872494525,-14.5032991769,117.923727178985)) ;
#189017 = CARTESIAN_POINT('Ctrl Pts',(-12.26622892562,-14.4441301859155,118.198469361747)) ;
#189018 = CARTESIAN_POINT('Ctrl Pts',(-12.2584771052313,-14.3724053611762,
118.174858566166)) ;
#189019 = CARTESIAN_POINT('Ctrl Pts',(-12.1846732836344,-14.3724053372545,
118.199089674322)) ;
#189020 = CARTESIAN_POINT('Ctrl Pts',(-12.1108694620375,-14.3724053133327,
118.223320782477)) ;
#189021 = CARTESIAN_POINT('Ctrl Pts',(-12.1186212824263,-14.444130138072,
118.246931578058)) ;
#189022 = CARTESIAN_POINT('Ctrl Pts',(-12.1263731028151,-14.5158549628113,
118.270542373639)) ;
#189023 = CARTESIAN_POINT('Ctrl Pts',(-12.2001769244119,-14.5158549867331,
118.246311265484)) ;
#189024 = CARTESIAN_POINT('Ctrl Pts',(-12.2739807460088,-14.5158550106548,
118.222080157328)) ;
#189025 = CARTESIAN_POINT('Ctrl Pts',(-12.26622892562,-14.4441301859155,118.198469361747)) ;
#189026 = CARTESIAN_POINT('Ctrl Pts',(-12.3365380163311,-14.3114937407021,
118.448066596164)) ;
#189027 = CARTESIAN_POINT('Ctrl Pts',(-12.3231327195336,-14.2489252476856,
118.407236223487)) ;
#189028 = CARTESIAN_POINT('Ctrl Pts',(-12.2493288970295,-14.2489252018326,
118.431467328879)) ;
#189029 = CARTESIAN_POINT('Ctrl Pts',(-12.1755250745255,-14.2489251559797,
118.455698434271)) ;
#189030 = CARTESIAN_POINT('Ctrl Pts',(-12.1889303713229,-14.3114936489961,
118.496528806949)) ;
#189031 = CARTESIAN_POINT('Ctrl Pts',(-12.2023356681204,-14.3740621420126,
118.537359179626)) ;
#189032 = CARTESIAN_POINT('Ctrl Pts',(-12.2761394906244,-14.3740621878656,
118.513128074234)) ;
#189033 = CARTESIAN_POINT('Ctrl Pts',(-12.3499433131285,-14.3740622337185,
118.488896968842)) ;
#189034 = CARTESIAN_POINT('Ctrl Pts',(-12.3365380163311,-14.3114937407021,
118.448066596164)) ;
#189035 = CARTESIAN_POINT('Ctrl Pts',(-12.3930354443869,-14.114774307687,
118.655627115153)) ;
#189036 = CARTESIAN_POINT('Ctrl Pts',(-12.3749320945125,-14.0658491597741,
118.600487230699)) ;
#189037 = CARTESIAN_POINT('Ctrl Pts',(-12.30112826882,-14.0658490924885,118.624718326379)) ;
#189038 = CARTESIAN_POINT('Ctrl Pts',(-12.2273244431275,-14.0658490252028,
118.64894942206)) ;
#189039 = CARTESIAN_POINT('Ctrl Pts',(-12.245427793002,-14.1147741731156,
118.704089306515)) ;
#189040 = CARTESIAN_POINT('Ctrl Pts',(-12.2635311428765,-14.1636993210285,
118.75922919097)) ;
#189041 = CARTESIAN_POINT('Ctrl Pts',(-12.3373349685689,-14.1636993883142,
118.734998095289)) ;
#189042 = CARTESIAN_POINT('Ctrl Pts',(-12.4111387942614,-14.1636994555999,
118.710766999608)) ;
#189043 = CARTESIAN_POINT('Ctrl Pts',(-12.3930354443869,-14.114774307687,
118.655627115153)) ;
#189044 = CARTESIAN_POINT('Ctrl Pts',(-12.4308165590885,-13.8682921869894,
118.806151894352)) ;
#189045 = CARTESIAN_POINT('Ctrl Pts',(-12.4093156019594,-13.8365043277557,
118.740663446289)) ;
#189046 = CARTESIAN_POINT('Ctrl Pts',(-12.3355117707898,-13.8365042424835,
118.764894525288)) ;
#189047 = CARTESIAN_POINT('Ctrl Pts',(-12.2617079396203,-13.8365041572113,
118.789125604286)) ;
#189048 = CARTESIAN_POINT('Ctrl Pts',(-12.2832088967495,-13.868292016445,
118.854614052349)) ;
#189049 = CARTESIAN_POINT('Ctrl Pts',(-12.3047098538786,-13.9000798756787,
118.920102500412)) ;
#189050 = CARTESIAN_POINT('Ctrl Pts',(-12.3785136850481,-13.9000799609509,
118.895871421414)) ;
#189051 = CARTESIAN_POINT('Ctrl Pts',(-12.4523175162177,-13.9000800462231,
118.871640342415)) ;
#189052 = CARTESIAN_POINT('Ctrl Pts',(-12.4308165590885,-13.8682921869894,
118.806151894352)) ;
#189053 = CARTESIAN_POINT('Ctrl Pts',(-12.4465020803455,-13.5896536678714,
118.889371904184)) ;
#189054 = CARTESIAN_POINT('Ctrl Pts',(-12.4231412470967,-13.5772729173919,
118.818218573456)) ;
#189055 = CARTESIAN_POINT('Ctrl Pts',(-12.3493374086623,-13.5772728198901,
118.842449630327)) ;
#189056 = CARTESIAN_POINT('Ctrl Pts',(-12.2755335702279,-13.5772727223883,
118.866680687197)) ;
#189057 = CARTESIAN_POINT('Ctrl Pts',(-12.2988944034766,-13.5896534728677,
118.937834017926)) ;
#189058 = CARTESIAN_POINT('Ctrl Pts',(-12.3222552367254,-13.6020342233472,
119.008987348655)) ;
#189059 = CARTESIAN_POINT('Ctrl Pts',(-12.3960590751598,-13.6020343208491,
118.984756291784)) ;
#189060 = CARTESIAN_POINT('Ctrl Pts',(-12.4698629135942,-13.6020344183509,
118.960525234913)) ;
#189061 = CARTESIAN_POINT('Ctrl Pts',(-12.4465020803455,-13.5896536678714,
118.889371904184)) ;
#189062 = CARTESIAN_POINT('Ctrl Pts',(-12.4381763312558,-13.2982167701219,
118.899517978675)) ;
#189063 = CARTESIAN_POINT('Ctrl Pts',(-12.4146278754705,-13.3061648042617,
118.827793179891)) ;
#189064 = CARTESIAN_POINT('Ctrl Pts',(-12.3408240286096,-13.3061647018305,
118.852024211096)) ;
#189065 = CARTESIAN_POINT('Ctrl Pts',(-12.2670201817487,-13.3061645993992,
118.876255242301)) ;
#189066 = CARTESIAN_POINT('Ctrl Pts',(-12.290568637534,-13.2982165652594,
118.947980041085)) ;
#189067 = CARTESIAN_POINT('Ctrl Pts',(-12.3141170933193,-13.2902685311196,
119.019704839869)) ;
#189068 = CARTESIAN_POINT('Ctrl Pts',(-12.3879209401802,-13.2902686335509,
118.995473808664)) ;
#189069 = CARTESIAN_POINT('Ctrl Pts',(-12.4617247870411,-13.2902687359821,
118.971242777458)) ;
#189070 = CARTESIAN_POINT('Ctrl Pts',(-12.4381763312558,-13.2982167701219,
118.899517978675)) ;
#189071 = CARTESIAN_POINT('Ctrl Pts',(-12.4056299449732,-13.0155927262678,
118.835868127191)) ;
#189072 = CARTESIAN_POINT('Ctrl Pts',(-12.3835849842552,-13.0432841492844,
118.768722731737)) ;
#189073 = CARTESIAN_POINT('Ctrl Pts',(-12.3097811286645,-13.0432840507906,
118.792953736353)) ;
#189074 = CARTESIAN_POINT('Ctrl Pts',(-12.2359772730738,-13.0432839522968,
118.817184740968)) ;
#189075 = CARTESIAN_POINT('Ctrl Pts',(-12.2580222337918,-13.0155925292803,
118.884330136422)) ;
#189076 = CARTESIAN_POINT('Ctrl Pts',(-12.2800671945098,-12.9879011062637,
118.951475531876)) ;
#189077 = CARTESIAN_POINT('Ctrl Pts',(-12.3538710501005,-12.9879012047575,
118.92724452726)) ;
#189078 = CARTESIAN_POINT('Ctrl Pts',(-12.4276749056913,-12.9879013032513,
118.903013522645)) ;
#189079 = CARTESIAN_POINT('Ctrl Pts',(-12.4056299449732,-13.0155927262678,
118.835868127191)) ;
#189080 = CARTESIAN_POINT('Ctrl Pts',(-12.3507015426636,-12.7625129426041,
118.703939374418)) ;
#189081 = CARTESIAN_POINT('Ctrl Pts',(-12.3317271438295,-12.8079141772025,
118.646146414998)) ;
#189082 = CARTESIAN_POINT('Ctrl Pts',(-12.2579232802105,-12.8079140912617,
118.67037739516)) ;
#189083 = CARTESIAN_POINT('Ctrl Pts',(-12.1841194165914,-12.8079140053209,
118.694608375323)) ;
#189084 = CARTESIAN_POINT('Ctrl Pts',(-12.2030938154255,-12.7625127707225,
118.752401334743)) ;
#189085 = CARTESIAN_POINT('Ctrl Pts',(-12.2220682142596,-12.7171115361241,
118.810194294164)) ;
#189086 = CARTESIAN_POINT('Ctrl Pts',(-12.2958720778787,-12.7171116220649,
118.785963314002)) ;
#189087 = CARTESIAN_POINT('Ctrl Pts',(-12.3696759414977,-12.7171117080057,
118.761732333839)) ;
#189088 = CARTESIAN_POINT('Ctrl Pts',(-12.3507015426636,-12.7625129426041,
118.703939374418)) ;
#189089 = CARTESIAN_POINT('Ctrl Pts',(-12.276179464868,-12.5553594059935,
118.512465785977)) ;
#189090 = CARTESIAN_POINT('Ctrl Pts',(-12.2616450921185,-12.6152904005215,
118.468196429597)) ;
#189091 = CARTESIAN_POINT('Ctrl Pts',(-12.1878412218671,-12.6152903344179,
118.492427389559)) ;
#189092 = CARTESIAN_POINT('Ctrl Pts',(-12.1140373516158,-12.6152902683143,
118.516658349521)) ;
#189093 = CARTESIAN_POINT('Ctrl Pts',(-12.1285717243653,-12.5553592737864,
118.5609277059)) ;
#189094 = CARTESIAN_POINT('Ctrl Pts',(-12.1431060971148,-12.4954282792585,
118.60519706228)) ;
#189095 = CARTESIAN_POINT('Ctrl Pts',(-12.2169099673661,-12.4954283453621,
118.580966102318)) ;
#189096 = CARTESIAN_POINT('Ctrl Pts',(-12.2907138376175,-12.4954284114656,
118.556735142357)) ;
#189097 = CARTESIAN_POINT('Ctrl Pts',(-12.276179464868,-12.5553594059935,
118.512465785977)) ;
#189098 = CARTESIAN_POINT('Ctrl Pts',(-12.1866037708491,-12.4101759250027,
118.275199832939)) ;
#189099 = CARTESIAN_POINT('Ctrl Pts',(-12.1775656705167,-12.4803322250042,
118.247671235534)) ;
#189100 = CARTESIAN_POINT('Ctrl Pts',(-12.1037617959182,-12.4803321844946,
118.271902182255)) ;
#189101 = CARTESIAN_POINT('Ctrl Pts',(-12.0299579213197,-12.4803321439849,
118.296133128976)) ;
#189102 = CARTESIAN_POINT('Ctrl Pts',(-12.0389960216522,-12.4101758439834,
118.323661726381)) ;
#189103 = CARTESIAN_POINT('Ctrl Pts',(-12.0480341219847,-12.3400195439819,
118.351190323787)) ;
#189104 = CARTESIAN_POINT('Ctrl Pts',(-12.1218379965832,-12.3400195844916,
118.326959377066)) ;
#189105 = CARTESIAN_POINT('Ctrl Pts',(-12.1956418711816,-12.3400196250012,
118.302728430345)) ;
#189106 = CARTESIAN_POINT('Ctrl Pts',(-12.1866037708491,-12.4101759250027,
118.275199832939)) ;
#189107 = CARTESIAN_POINT('Ctrl Pts',(-12.0884786810735,-12.3376963152453,
118.011668844001)) ;
#189108 = CARTESIAN_POINT('Ctrl Pts',(-12.085546690365,-12.4130169374688,
118.002738471319)) ;
#189109 = CARTESIAN_POINT('Ctrl Pts',(-12.0117428139613,-12.4130169250925,
118.026969412542)) ;
#189110 = CARTESIAN_POINT('Ctrl Pts',(-11.9379389375575,-12.4130169127163,
118.051200353765)) ;
#189111 = CARTESIAN_POINT('Ctrl Pts',(-11.940870928266,-12.3376962904928,
118.060130726446)) ;
#189112 = CARTESIAN_POINT('Ctrl Pts',(-11.9438029189746,-12.2623756682694,
118.069061099127)) ;
#189113 = CARTESIAN_POINT('Ctrl Pts',(-12.0176067953783,-12.2623756806456,
118.044830157905)) ;
#189114 = CARTESIAN_POINT('Ctrl Pts',(-12.091410671782,-12.2623756930219,
118.020599216682)) ;
#189115 = CARTESIAN_POINT('Ctrl Pts',(-12.0884786810735,-12.3376963152453,
118.011668844001)) ;
#189116 = CARTESIAN_POINT('Ctrl Pts',(-11.9868042804343,-12.3422639933637,
117.737570588473)) ;
#189117 = CARTESIAN_POINT('Ctrl Pts',(-11.9902301097811,-12.4173784848516,
117.748005109908)) ;
#189118 = CARTESIAN_POINT('Ctrl Pts',(-11.9164262344824,-12.4173785007626,
117.772236054496)) ;
#189119 = CARTESIAN_POINT('Ctrl Pts',(-11.8426223591838,-12.4173785166736,
117.796466999085)) ;
#189120 = CARTESIAN_POINT('Ctrl Pts',(-11.8391965298369,-12.3422640251856,
117.786032477649)) ;
#189121 = CARTESIAN_POINT('Ctrl Pts',(-11.83577070049,-12.2671495336977,117.775597956213)) ;
#189122 = CARTESIAN_POINT('Ctrl Pts',(-11.9095745757887,-12.2671495177867,
117.751367011625)) ;
#189123 = CARTESIAN_POINT('Ctrl Pts',(-11.9833784510874,-12.2671495018757,
117.727136067037)) ;
#189124 = CARTESIAN_POINT('Ctrl Pts',(-11.9868042804343,-12.3422639933637,
117.737570588473)) ;
#189125 = CARTESIAN_POINT('Ctrl Pts',(-11.8890994352425,-12.4243537888734,
117.475457869454)) ;
#189126 = CARTESIAN_POINT('Ctrl Pts',(-11.8986177488891,-12.4938495197523,
117.504449115127)) ;
#189127 = CARTESIAN_POINT('Ctrl Pts',(-11.8248138772114,-12.4938495605533,
117.528680070744)) ;
#189128 = CARTESIAN_POINT('Ctrl Pts',(-11.7510100055337,-12.4938496013543,
117.552911026361)) ;
#189129 = CARTESIAN_POINT('Ctrl Pts',(-11.7414916918871,-12.4243538704754,
117.523919780688)) ;
#189130 = CARTESIAN_POINT('Ctrl Pts',(-11.7319733782405,-12.3548581395965,
117.494928535016)) ;
#189131 = CARTESIAN_POINT('Ctrl Pts',(-11.8057772499182,-12.3548580987955,
117.470697579399)) ;
#189132 = CARTESIAN_POINT('Ctrl Pts',(-11.879581121596,-12.3548580579945,
117.446466623782)) ;
#189133 = CARTESIAN_POINT('Ctrl Pts',(-11.8890994352425,-12.4243537888734,
117.475457869454)) ;
#189134 = CARTESIAN_POINT('Ctrl Pts',(-11.8017044319056,-12.5764990896273,
117.244563346778)) ;
#189135 = CARTESIAN_POINT('Ctrl Pts',(-11.8166083589498,-12.6354761389067,
117.289958301969)) ;
#189136 = CARTESIAN_POINT('Ctrl Pts',(-11.7428044925836,-12.6354761997948,
117.314189273764)) ;
#189137 = CARTESIAN_POINT('Ctrl Pts',(-11.6690006262173,-12.6354762606829,
117.338420245559)) ;
#189138 = CARTESIAN_POINT('Ctrl Pts',(-11.6540966991731,-12.5764992114035,
117.293025290368)) ;
#189139 = CARTESIAN_POINT('Ctrl Pts',(-11.6391927721289,-12.5175221621241,
117.247630335178)) ;
#189140 = CARTESIAN_POINT('Ctrl Pts',(-11.7129966384952,-12.517522101236,
117.223399363383)) ;
#189141 = CARTESIAN_POINT('Ctrl Pts',(-11.7868005048614,-12.5175220403479,
117.199168391588)) ;
#189142 = CARTESIAN_POINT('Ctrl Pts',(-11.8017044319056,-12.5764990896273,
117.244563346778)) ;
#189143 = CARTESIAN_POINT('Ctrl Pts',(-11.7291135872937,-12.7898749801387,
117.058995916747)) ;
#189144 = CARTESIAN_POINT('Ctrl Pts',(-11.7483728632372,-12.8340435200322,
117.117656562069)) ;
#189145 = CARTESIAN_POINT('Ctrl Pts',(-11.6745690038856,-12.834043593478,
117.14188755523)) ;
#189146 = CARTESIAN_POINT('Ctrl Pts',(-11.600765144534,-12.8340436669238,
117.16611854839)) ;
#189147 = CARTESIAN_POINT('Ctrl Pts',(-11.5815058685905,-12.7898751270303,
117.107457903068)) ;
#189148 = CARTESIAN_POINT('Ctrl Pts',(-11.5622465926471,-12.7457065871368,
117.048797257746)) ;
#189149 = CARTESIAN_POINT('Ctrl Pts',(-11.6360504519986,-12.745706513691,
117.024566264585)) ;
#189150 = CARTESIAN_POINT('Ctrl Pts',(-11.7098543113502,-12.7457064402452,
117.000335271425)) ;
#189151 = CARTESIAN_POINT('Ctrl Pts',(-11.7291135872937,-12.7898749801387,
117.058995916747)) ;
#189152 = CARTESIAN_POINT('Ctrl Pts',(-11.6764341261523,-13.0489854290901,
116.934128082032)) ;
#189153 = CARTESIAN_POINT('Ctrl Pts',(-11.6986642223819,-13.0751301371368,
117.001837366752)) ;
#189154 = CARTESIAN_POINT('Ctrl Pts',(-11.6248603705172,-13.0751302144171,
117.026068382717)) ;
#189155 = CARTESIAN_POINT('Ctrl Pts',(-11.5510565186525,-13.0751302916973,
117.050299398681)) ;
#189156 = CARTESIAN_POINT('Ctrl Pts',(-11.5288264224229,-13.0489855836505,
116.982590113961)) ;
#189157 = CARTESIAN_POINT('Ctrl Pts',(-11.5065963261933,-13.0228408756037,
116.914880829242)) ;
#189158 = CARTESIAN_POINT('Ctrl Pts',(-11.580400178058,-13.0228407983235,
116.890649813277)) ;
#189159 = CARTESIAN_POINT('Ctrl Pts',(-11.6542040299227,-13.0228407210433,
116.866418797313)) ;
#189160 = CARTESIAN_POINT('Ctrl Pts',(-11.6764341261523,-13.0489854290901,
116.934128082032)) ;
#189161 = CARTESIAN_POINT('Ctrl Pts',(-11.6468794476633,-13.3335116646803,
116.879553756773)) ;
#189162 = CARTESIAN_POINT('Ctrl Pts',(-11.6704731941443,-13.3398303944034,
116.951416500274)) ;
#189163 = CARTESIAN_POINT('Ctrl Pts',(-11.5966693491189,-13.3398304688619,
116.97564753707)) ;
#189164 = CARTESIAN_POINT('Ctrl Pts',(-11.5228655040934,-13.3398305433204,
116.999878573866)) ;
#189165 = CARTESIAN_POINT('Ctrl Pts',(-11.4992717576124,-13.3335118135973,
116.928015830364)) ;
#189166 = CARTESIAN_POINT('Ctrl Pts',(-11.4756780111314,-13.3271930838743,
116.856153086863)) ;
#189167 = CARTESIAN_POINT('Ctrl Pts',(-11.5494818561569,-13.3271930094158,
116.831922050067)) ;
#189168 = CARTESIAN_POINT('Ctrl Pts',(-11.6232857011823,-13.3271929349573,
116.807691013271)) ;
#189169 = CARTESIAN_POINT('Ctrl Pts',(-11.6468794476633,-13.3335116646803,
116.879553756773)) ;
#189170 = CARTESIAN_POINT('Ctrl Pts',(-11.6414627303795,-13.6230727255243,
116.898378600556)) ;
#189171 = CARTESIAN_POINT('Ctrl Pts',(-11.6647393194538,-13.6091838535946,
116.969275333898)) ;
#189172 = CARTESIAN_POINT('Ctrl Pts',(-11.5909354802481,-13.6091839202508,
116.99350638842)) ;
#189173 = CARTESIAN_POINT('Ctrl Pts',(-11.5171316410424,-13.6091839869071,
117.017737442942)) ;
#189174 = CARTESIAN_POINT('Ctrl Pts',(-11.4938550519681,-13.6230728588367,
116.9468407096)) ;
#189175 = CARTESIAN_POINT('Ctrl Pts',(-11.4705784628939,-13.6369617307664,
116.875943976258)) ;
#189176 = CARTESIAN_POINT('Ctrl Pts',(-11.5443823020996,-13.6369616641102,
116.851712921736)) ;
#189177 = CARTESIAN_POINT('Ctrl Pts',(-11.6181861413053,-13.6369615974539,
116.827481867214)) ;
#189178 = CARTESIAN_POINT('Ctrl Pts',(-11.6414627303795,-13.6230727255243,
116.898378600556)) ;
#189179 = CARTESIAN_POINT('Ctrl Pts',(-11.6598233366193,-13.8991091738745,
116.989763695794)) ;
#189180 = CARTESIAN_POINT('Ctrl Pts',(-11.681119458354,-13.8659263158171,
117.054628245326)) ;
#189181 = CARTESIAN_POINT('Ctrl Pts',(-11.6073156234127,-13.8659263690519,
117.078859312837)) ;
#189182 = CARTESIAN_POINT('Ctrl Pts',(-11.5335117884714,-13.8659264222868,
117.103090380348)) ;
#189183 = CARTESIAN_POINT('Ctrl Pts',(-11.5122156667368,-13.8991092803442,
117.038225830815)) ;
#189184 = CARTESIAN_POINT('Ctrl Pts',(-11.4909195450021,-13.9322921384017,
116.973361281282)) ;
#189185 = CARTESIAN_POINT('Ctrl Pts',(-11.5647233799434,-13.9322920851668,
116.949130213771)) ;
#189186 = CARTESIAN_POINT('Ctrl Pts',(-11.6385272148846,-13.9322920319319,
116.924899146261)) ;
#189187 = CARTESIAN_POINT('Ctrl Pts',(-11.6598233366193,-13.8991091738745,
116.989763695794)) ;
#189188 = CARTESIAN_POINT('Ctrl Pts',(-11.70011193344,-14.1412745978093,117.148019110991)) ;
#189189 = CARTESIAN_POINT('Ctrl Pts',(-11.7178919586761,-14.0911330408888,
117.202174198091)) ;
#189190 = CARTESIAN_POINT('Ctrl Pts',(-11.6440881259211,-14.0911330778526,
117.22640527226)) ;
#189191 = CARTESIAN_POINT('Ctrl Pts',(-11.5702842931661,-14.0911331148164,
117.25063634643)) ;
#189192 = CARTESIAN_POINT('Ctrl Pts',(-11.55250426793,-14.141274671737,117.19648125933)) ;
#189193 = CARTESIAN_POINT('Ctrl Pts',(-11.5347242426939,-14.1914162286575,
117.14232617223)) ;
#189194 = CARTESIAN_POINT('Ctrl Pts',(-11.6085280754489,-14.1914161916937,
117.118095098061)) ;
#189195 = CARTESIAN_POINT('Ctrl Pts',(-11.6823319082039,-14.1914161547299,
117.093864023891)) ;
#189196 = CARTESIAN_POINT('Ctrl Pts',(-11.70011193344,-14.1412745978093,117.148019110991)) ;
#189197 = CARTESIAN_POINT('Ctrl Pts',(-11.7587869921287,-14.3313662237517,
117.362325380269)) ;
#189198 = CARTESIAN_POINT('Ctrl Pts',(-11.7717607368277,-14.2678756388728,
117.401841312536)) ;
#189199 = CARTESIAN_POINT('Ctrl Pts',(-11.6979569041075,-14.2678756602265,
117.426072386812)) ;
#189200 = CARTESIAN_POINT('Ctrl Pts',(-11.6241530713873,-14.2678756815801,
117.450303461088)) ;
#189201 = CARTESIAN_POINT('Ctrl Pts',(-11.6111793266882,-14.331366266459,
117.41078752882)) ;
#189202 = CARTESIAN_POINT('Ctrl Pts',(-11.5982055819891,-14.3948568513378,
117.371271596553)) ;
#189203 = CARTESIAN_POINT('Ctrl Pts',(-11.6720094147093,-14.3948568299842,
117.347040522277)) ;
#189204 = CARTESIAN_POINT('Ctrl Pts',(-11.7458132474296,-14.3948568086305,
117.322809448002)) ;
#189205 = CARTESIAN_POINT('Ctrl Pts',(-11.7587869921287,-14.3313662237517,
117.362325380269)) ;
#189206 = CARTESIAN_POINT('Ctrl Pts',(-11.8298919850122,-14.4547660222928,
117.614104425803)) ;
#189207 = CARTESIAN_POINT('Ctrl Pts',(-11.8371920680467,-14.3825637894308,
117.6363393002)) ;
#189208 = CARTESIAN_POINT('Ctrl Pts',(-11.7633882348918,-14.3825637991791,
117.660570373151)) ;
#189209 = CARTESIAN_POINT('Ctrl Pts',(-11.6895844017367,-14.3825638089273,
117.684801446103)) ;
#189210 = CARTESIAN_POINT('Ctrl Pts',(-11.6822843187022,-14.4547660417892,
117.662566571706)) ;
#189211 = CARTESIAN_POINT('Ctrl Pts',(-11.6749842356676,-14.5269682746512,
117.64033169731)) ;
#189212 = CARTESIAN_POINT('Ctrl Pts',(-11.7487880688226,-14.526968264903,
117.616100624358)) ;
#189213 = CARTESIAN_POINT('Ctrl Pts',(-11.8225919019776,-14.5269682551548,
117.591869551407)) ;
#189214 = CARTESIAN_POINT('Ctrl Pts',(-11.8298919850122,-14.4547660222928,
117.614104425803)) ;
#189215 = CARTESIAN_POINT('Ctrl Pts',(-11.9091252270702,-14.5053328691454,
117.891029238867)) ;
#189216 = CARTESIAN_POINT('Ctrl Pts',(-11.9101675159898,-14.4294900381805,
117.894203882266)) ;
#189217 = CARTESIAN_POINT('Ctrl Pts',(-11.8363636802989,-14.4294900382422,
117.918434947493)) ;
#189218 = CARTESIAN_POINT('Ctrl Pts',(-11.762559844608,-14.4294900383039,
117.942666012721)) ;
#189219 = CARTESIAN_POINT('Ctrl Pts',(-11.7615175556885,-14.5053328692688,
117.939491369322)) ;
#189220 = CARTESIAN_POINT('Ctrl Pts',(-11.7604752667689,-14.5811757002337,
117.936316725924)) ;
#189221 = CARTESIAN_POINT('Ctrl Pts',(-11.8342791024598,-14.581175700172,
117.912085660696)) ;
#189222 = CARTESIAN_POINT('Ctrl Pts',(-11.9080829381506,-14.5811757001103,
117.887854595469)) ;
#189223 = CARTESIAN_POINT('Ctrl Pts',(-11.9091252270702,-14.5053328691454,
117.891029238867)) ;
#189224 = CARTESIAN_POINT('Ctrl Pts',(-11.9891525457306,-14.4771328889757,
118.170301722369)) ;
#189225 = CARTESIAN_POINT('Ctrl Pts',(-11.9838733903065,-14.4031442032382,
118.154222266415)) ;
#189226 = CARTESIAN_POINT('Ctrl Pts',(-11.9100695518998,-14.4031441988983,
118.17845332337)) ;
#189227 = CARTESIAN_POINT('Ctrl Pts',(-11.8362657134931,-14.4031441945584,
118.202684380326)) ;
#189228 = CARTESIAN_POINT('Ctrl Pts',(-11.8415448689172,-14.4771328802959,
118.21876383628)) ;
#189229 = CARTESIAN_POINT('Ctrl Pts',(-11.8468240243413,-14.5511215660333,
118.234843292234)) ;
#189230 = CARTESIAN_POINT('Ctrl Pts',(-11.920627862748,-14.5511215703732,
118.210612235279)) ;
#189231 = CARTESIAN_POINT('Ctrl Pts',(-11.9944317011547,-14.5511215747131,
118.186381178323)) ;
#189232 = CARTESIAN_POINT('Ctrl Pts',(-11.9891525457306,-14.4771328889757,
118.170301722369)) ;
#189233 = CARTESIAN_POINT('Ctrl Pts',(-12.0631580436741,-14.3740575561619,
118.430997938471)) ;
#189234 = CARTESIAN_POINT('Ctrl Pts',(-12.0519733519711,-14.3071548458452,
118.396931171973)) ;
#189235 = CARTESIAN_POINT('Ctrl Pts',(-11.9781695115022,-14.307154840074,
118.421162222647)) ;
#189236 = CARTESIAN_POINT('Ctrl Pts',(-11.9043656710333,-14.3071548343027,
118.445393273322)) ;
#189237 = CARTESIAN_POINT('Ctrl Pts',(-11.9155503627364,-14.3740575446194,
118.479460039819)) ;
#189238 = CARTESIAN_POINT('Ctrl Pts',(-11.9267350544394,-14.4409602549361,
118.513526806317)) ;
#189239 = CARTESIAN_POINT('Ctrl Pts',(-12.0005388949083,-14.4409602607073,
118.489295755643)) ;
#189240 = CARTESIAN_POINT('Ctrl Pts',(-12.0743427353772,-14.4409602664786,
118.465064704968)) ;
#189241 = CARTESIAN_POINT('Ctrl Pts',(-12.0631580436741,-14.3740575561619,
118.430997938471)) ;
#189242 = CARTESIAN_POINT('Ctrl Pts',(-12.1262287274815,-14.2012582823737,
118.658729046755)) ;
#189243 = CARTESIAN_POINT('Ctrl Pts',(-12.1098857541428,-14.1463204404916,
118.608950986816)) ;
#189244 = CARTESIAN_POINT('Ctrl Pts',(-12.0360819115211,-14.1463204373001,
118.633182030934)) ;
#189245 = CARTESIAN_POINT('Ctrl Pts',(-11.9622780688994,-14.1463204341086,
118.657413075051)) ;
#189246 = CARTESIAN_POINT('Ctrl Pts',(-11.9786210422382,-14.2012582759907,
118.70719113499)) ;
#189247 = CARTESIAN_POINT('Ctrl Pts',(-11.9949640155769,-14.2561961178728,
118.756969194928)) ;
#189248 = CARTESIAN_POINT('Ctrl Pts',(-12.0687678581985,-14.2561961210643,
118.732738150811)) ;
#189249 = CARTESIAN_POINT('Ctrl Pts',(-12.1425717008202,-14.2561961242558,
118.708507106693)) ;
#189250 = CARTESIAN_POINT('Ctrl Pts',(-12.1262287274815,-14.2012582823737,
118.658729046755)) ;
#189251 = CARTESIAN_POINT('Ctrl Pts',(-12.1720317469942,-13.9726608385018,
118.833715114846)) ;
#189252 = CARTESIAN_POINT('Ctrl Pts',(-12.1517317413815,-13.9336031304971,
118.771884573146)) ;
#189253 = CARTESIAN_POINT('Ctrl Pts',(-12.0779278978753,-13.9336031304968,
118.79611561457)) ;
#189254 = CARTESIAN_POINT('Ctrl Pts',(-12.0041240543692,-13.9336031304964,
118.820346655993)) ;
#189255 = CARTESIAN_POINT('Ctrl Pts',(-12.0244240599819,-13.9726608385011,
118.882177197693)) ;
#189256 = CARTESIAN_POINT('Ctrl Pts',(-12.0447240655947,-14.0117185465058,
118.944007739393)) ;
#189257 = CARTESIAN_POINT('Ctrl Pts',(-12.1185279091008,-14.0117185465062,
118.919776697969)) ;
#189258 = CARTESIAN_POINT('Ctrl Pts',(-12.192331752607,-14.0117185465065,
118.895545656546)) ;
#189259 = CARTESIAN_POINT('Ctrl Pts',(-12.1720317469942,-13.9726608385018,
118.833715114846)) ;
#189260 = CARTESIAN_POINT('Ctrl Pts',(-12.1969356507805,-13.7058102020006,
118.944880479442)) ;
#189261 = CARTESIAN_POINT('Ctrl Pts',(-12.1741357371113,-13.6853276622156,
118.875435621207)) ;
#189262 = CARTESIAN_POINT('Ctrl Pts',(-12.1003318934442,-13.685327664635,
118.899666662141)) ;
#189263 = CARTESIAN_POINT('Ctrl Pts',(-12.0265280497771,-13.6853276670543,
118.923897703074)) ;
#189264 = CARTESIAN_POINT('Ctrl Pts',(-12.0493279634463,-13.7058102068394,
118.993342561308)) ;
#189265 = CARTESIAN_POINT('Ctrl Pts',(-12.0721278771155,-13.7262927466244,
119.062787419543)) ;
#189266 = CARTESIAN_POINT('Ctrl Pts',(-12.1459317207826,-13.726292744205,
119.03855637861)) ;
#189267 = CARTESIAN_POINT('Ctrl Pts',(-12.2197355644497,-13.7262927417856,
119.014325337677)) ;
#189268 = CARTESIAN_POINT('Ctrl Pts',(-12.1969356507805,-13.7058102020006,
118.944880479442)) ;
#189269 = CARTESIAN_POINT('Ctrl Pts',(-12.1984748836622,-13.4160016672544,
118.985181508571)) ;
#189270 = CARTESIAN_POINT('Ctrl Pts',(-12.1747964593274,-13.4157263085417,
118.913060848612)) ;
#189271 = CARTESIAN_POINT('Ctrl Pts',(-12.100992615932,-13.4157263119192,
118.937291890373)) ;
#189272 = CARTESIAN_POINT('Ctrl Pts',(-12.0271887725366,-13.4157263152968,
118.961522932133)) ;
#189273 = CARTESIAN_POINT('Ctrl Pts',(-12.0508671968713,-13.4160016740095,
119.033643592092)) ;
#189274 = CARTESIAN_POINT('Ctrl Pts',(-12.074545621206,-13.4162770327222,
119.105764252051)) ;
#189275 = CARTESIAN_POINT('Ctrl Pts',(-12.1483494646015,-13.4162770293446,
119.08153321029)) ;
#189276 = CARTESIAN_POINT('Ctrl Pts',(-12.2221533079969,-13.4162770259671,
119.057302168529)) ;
#189277 = CARTESIAN_POINT('Ctrl Pts',(-12.1984748836622,-13.4160016672544,
118.985181508571)) ;
#189278 = CARTESIAN_POINT('Ctrl Pts',(-12.1757274731677,-13.1285751860039,
118.9512289621)) ;
#189279 = CARTESIAN_POINT('Ctrl Pts',(-12.1528714753158,-13.1483696405658,
118.881613280481)) ;
#189280 = CARTESIAN_POINT('Ctrl Pts',(-12.0790676321189,-13.1483696423267,
118.905844322846)) ;
#189281 = CARTESIAN_POINT('Ctrl Pts',(-12.0052637889219,-13.1483696440876,
118.930075365211)) ;
#189282 = CARTESIAN_POINT('Ctrl Pts',(-12.0281197867738,-13.1285751895257,
118.99969104683)) ;
#189283 = CARTESIAN_POINT('Ctrl Pts',(-12.0509757846257,-13.1087807349637,
119.06930672845)) ;
#189284 = CARTESIAN_POINT('Ctrl Pts',(-12.1247796278227,-13.1087807332029,
119.045075686085)) ;
#189285 = CARTESIAN_POINT('Ctrl Pts',(-12.1985834710196,-13.108780731442,
119.020844643719)) ;
#189286 = CARTESIAN_POINT('Ctrl Pts',(-12.1757274731677,-13.1285751860039,
118.9512289621)) ;
#189287 = CARTESIAN_POINT('Ctrl Pts',(-12.1296371270561,-12.8607655160009,
118.846298221329)) ;
#189288 = CARTESIAN_POINT('Ctrl Pts',(-12.1092322366569,-12.8992892822013,
118.784148217467)) ;
#189289 = CARTESIAN_POINT('Ctrl Pts',(-12.0354283931757,-12.8992892809573,
118.808379258966)) ;
#189290 = CARTESIAN_POINT('Ctrl Pts',(-11.9616245496946,-12.8992892797133,
118.832610300466)) ;
#189291 = CARTESIAN_POINT('Ctrl Pts',(-11.9820294400938,-12.8607655135129,
118.894760304328)) ;
#189292 = CARTESIAN_POINT('Ctrl Pts',(-12.0024343304931,-12.8222417473126,
118.95691030819)) ;
#189293 = CARTESIAN_POINT('Ctrl Pts',(-12.0762381739742,-12.8222417485565,
118.932679266691)) ;
#189294 = CARTESIAN_POINT('Ctrl Pts',(-12.1500420174553,-12.8222417498005,
118.908448225191)) ;
#189295 = CARTESIAN_POINT('Ctrl Pts',(-12.1296371270561,-12.8607655160009,
118.846298221329)) ;
#189296 = CARTESIAN_POINT('Ctrl Pts',(-12.0621098926496,-12.6316532711116,
118.676300392897)) ;
#189297 = CARTESIAN_POINT('Ctrl Pts',(-12.0456518862887,-12.686231857174,
118.626171960866)) ;
#189298 = CARTESIAN_POINT('Ctrl Pts',(-11.9718480413066,-12.6862318515475,
118.650402997794)) ;
#189299 = CARTESIAN_POINT('Ctrl Pts',(-11.8980441963246,-12.6862318459211,
118.674634034722)) ;
#189300 = CARTESIAN_POINT('Ctrl Pts',(-11.9145022026855,-12.6316532598588,
118.724762466754)) ;
#189301 = CARTESIAN_POINT('Ctrl Pts',(-11.9309602090465,-12.5770746737964,
118.774890898785)) ;
#189302 = CARTESIAN_POINT('Ctrl Pts',(-12.0047640540285,-12.5770746794228,
118.750659861857)) ;
#189303 = CARTESIAN_POINT('Ctrl Pts',(-12.0785678990105,-12.5770746850493,
118.726428824929)) ;
#189304 = CARTESIAN_POINT('Ctrl Pts',(-12.0621098926496,-12.6316532711116,
118.676300392897)) ;
#189305 = CARTESIAN_POINT('Ctrl Pts',(-11.978269028545,-12.460718041819,118.456338381467)) ;
#189306 = CARTESIAN_POINT('Ctrl Pts',(-11.9669085684669,-12.5273111609863,
118.42173625281)) ;
#189307 = CARTESIAN_POINT('Ctrl Pts',(-11.8931047213999,-12.5273111540266,
118.445967283387)) ;
#189308 = CARTESIAN_POINT('Ctrl Pts',(-11.8193008743329,-12.5273111470668,
118.470198313965)) ;
#189309 = CARTESIAN_POINT('Ctrl Pts',(-11.830661334411,-12.4607180278995,
118.504800442623)) ;
#189310 = CARTESIAN_POINT('Ctrl Pts',(-11.8420217944891,-12.3941249087322,
118.53940257128)) ;
#189311 = CARTESIAN_POINT('Ctrl Pts',(-11.915825641556,-12.394124915692,118.515171540702)) ;
#189312 = CARTESIAN_POINT('Ctrl Pts',(-11.989629488623,-12.3941249226517,
118.490940510125)) ;
#189313 = CARTESIAN_POINT('Ctrl Pts',(-11.978269028545,-12.460718041819,118.456338381467)) ;
#189314 = CARTESIAN_POINT('Ctrl Pts',(-11.8829561531315,-12.3580087732105,
118.201435967149)) ;
#189315 = CARTESIAN_POINT('Ctrl Pts',(-11.8775015614734,-12.4318697519678,
118.184822160659)) ;
#189316 = CARTESIAN_POINT('Ctrl Pts',(-11.8036977119076,-12.4318697467782,
118.209053183626)) ;
#189317 = CARTESIAN_POINT('Ctrl Pts',(-11.7298938623419,-12.4318697415885,
118.233284206593)) ;
#189318 = CARTESIAN_POINT('Ctrl Pts',(-11.735348454,-12.3580087628311,118.249898013083)) ;
#189319 = CARTESIAN_POINT('Ctrl Pts',(-11.7408030456581,-12.2841477840738,
118.266511819573)) ;
#189320 = CARTESIAN_POINT('Ctrl Pts',(-11.8146068952239,-12.2841477892635,
118.242280796606)) ;
#189321 = CARTESIAN_POINT('Ctrl Pts',(-11.8884107447897,-12.2841477944531,
118.218049773639)) ;
#189322 = CARTESIAN_POINT('Ctrl Pts',(-11.8829561531315,-12.3580087732105,
118.201435967149)) ;
#189323 = CARTESIAN_POINT('Ctrl Pts',(-11.7821952753084,-12.3309308762199,
117.929933042971)) ;
#189324 = CARTESIAN_POINT('Ctrl Pts',(-11.7830355643032,-12.4067892276866,
117.932492427132)) ;
#189325 = CARTESIAN_POINT('Ctrl Pts',(-11.7092317122289,-12.4067892280987,
117.956723442458)) ;
#189326 = CARTESIAN_POINT('Ctrl Pts',(-11.6354278601546,-12.4067892285108,
117.980954457785)) ;
#189327 = CARTESIAN_POINT('Ctrl Pts',(-11.6345875711599,-12.330930877044,
117.978395073623)) ;
#189328 = CARTESIAN_POINT('Ctrl Pts',(-11.6337472821651,-12.2550725255773,
117.975835689462)) ;
#189329 = CARTESIAN_POINT('Ctrl Pts',(-11.7075511342394,-12.2550725251652,
117.951604674136)) ;
#189330 = CARTESIAN_POINT('Ctrl Pts',(-11.7813549863137,-12.2550725247531,
117.92737365881)) ;
#189331 = CARTESIAN_POINT('Ctrl Pts',(-11.7821952753084,-12.3309308762199,
117.929933042971)) ;
#189332 = CARTESIAN_POINT('Ctrl Pts',(-11.6820920733114,-12.3817530522947,
117.660553623845)) ;
#189333 = CARTESIAN_POINT('Ctrl Pts',(-11.6891878850714,-12.4541728296822,
117.682166320851)) ;
#189334 = CARTESIAN_POINT('Ctrl Pts',(-11.6153840306775,-12.454172840125,
117.706397329112)) ;
#189335 = CARTESIAN_POINT('Ctrl Pts',(-11.5415801762836,-12.4541728505679,
117.730628337373)) ;
#189336 = CARTESIAN_POINT('Ctrl Pts',(-11.5344843645237,-12.3817530731804,
117.709015640367)) ;
#189337 = CARTESIAN_POINT('Ctrl Pts',(-11.5273885527638,-12.3093332957928,
117.687402943361)) ;
#189338 = CARTESIAN_POINT('Ctrl Pts',(-11.6011924071576,-12.30933328535,117.6631719351)) ;
#189339 = CARTESIAN_POINT('Ctrl Pts',(-11.6749962615515,-12.3093332749072,
117.638940926839)) ;
#189340 = CARTESIAN_POINT('Ctrl Pts',(-11.6820920733114,-12.3817530522947,
117.660553623845)) ;
#189341 = CARTESIAN_POINT('Ctrl Pts',(-11.5895815929449,-12.506826084586,
117.414237666503)) ;
#189342 = CARTESIAN_POINT('Ctrl Pts',(-11.6024130459701,-12.5706179101752,
117.453320201195)) ;
#189343 = CARTESIAN_POINT('Ctrl Pts',(-11.5286091905944,-12.5706179343356,
117.477551206465)) ;
#189344 = CARTESIAN_POINT('Ctrl Pts',(-11.4548053352187,-12.5706179584961,
117.501782211736)) ;
#189345 = CARTESIAN_POINT('Ctrl Pts',(-11.4419738821936,-12.5068261329069,
117.462699677045)) ;
#189346 = CARTESIAN_POINT('Ctrl Pts',(-11.4291424291684,-12.4430343073178,
117.423617142354)) ;
#189347 = CARTESIAN_POINT('Ctrl Pts',(-11.5029462845441,-12.4430342831573,
117.399386137083)) ;
#189348 = CARTESIAN_POINT('Ctrl Pts',(-11.5767501399198,-12.4430342589969,
117.375155131812)) ;
#189349 = CARTESIAN_POINT('Ctrl Pts',(-11.5895815929449,-12.506826084586,
117.414237666503)) ;
#189350 = CARTESIAN_POINT('Ctrl Pts',(-11.5103184193888,-12.6970626230436,
117.208275910696)) ;
#189351 = CARTESIAN_POINT('Ctrl Pts',(-11.5279687114292,-12.7476645000542,
117.262035851343)) ;
#189352 = CARTESIAN_POINT('Ctrl Pts',(-11.4541648566701,-12.7476645399719,
117.286266858491)) ;
#189353 = CARTESIAN_POINT('Ctrl Pts',(-11.380361001911,-12.7476645798895,
117.31049786564)) ;
#189354 = CARTESIAN_POINT('Ctrl Pts',(-11.3627107098707,-12.6970627028788,
117.256737924993)) ;
#189355 = CARTESIAN_POINT('Ctrl Pts',(-11.3450604178303,-12.6464608258682,
117.202977984346)) ;
#189356 = CARTESIAN_POINT('Ctrl Pts',(-11.4188642725894,-12.6464607859506,
117.178746977197)) ;
#189357 = CARTESIAN_POINT('Ctrl Pts',(-11.4926681273484,-12.646460746033,
117.154515970049)) ;
#189358 = CARTESIAN_POINT('Ctrl Pts',(-11.5103184193888,-12.6970626230436,
117.208275910696)) ;
#189359 = CARTESIAN_POINT('Ctrl Pts',(-11.4490956702002,-12.9398196291384,
117.057375370954)) ;
#189360 = CARTESIAN_POINT('Ctrl Pts',(-11.4703099251282,-12.9735460220805,
117.121990567328)) ;
#189361 = CARTESIAN_POINT('Ctrl Pts',(-11.3965060727708,-12.9735460788729,
117.146221581792)) ;
#189362 = CARTESIAN_POINT('Ctrl Pts',(-11.3227022204133,-12.9735461356652,
117.170452596256)) ;
#189363 = CARTESIAN_POINT('Ctrl Pts',(-11.3014879654853,-12.9398197427232,
117.105837399882)) ;
#189364 = CARTESIAN_POINT('Ctrl Pts',(-11.2802737105573,-12.9060933497811,
117.041222203508)) ;
#189365 = CARTESIAN_POINT('Ctrl Pts',(-11.3540775629148,-12.9060932929888,
117.016991189044)) ;
#189366 = CARTESIAN_POINT('Ctrl Pts',(-11.4278814152722,-12.9060932361964,
116.99276017458)) ;
#189367 = CARTESIAN_POINT('Ctrl Pts',(-11.4490956702002,-12.9398196291384,
117.057375370954)) ;
#189368 = CARTESIAN_POINT('Ctrl Pts',(-11.4099894577055,-13.2163226304817,
116.973745461531)) ;
#189369 = CARTESIAN_POINT('Ctrl Pts',(-11.4332305688274,-13.2307930159817,
117.04453413468)) ;
#189370 = CARTESIAN_POINT('Ctrl Pts',(-11.3594267210954,-13.2307930864604,
117.068765163233)) ;
#189371 = CARTESIAN_POINT('Ctrl Pts',(-11.2856228733634,-13.2307931569392,
117.092996191785)) ;
#189372 = CARTESIAN_POINT('Ctrl Pts',(-11.2623817622415,-13.2163227714392,
117.022207518635)) ;
#189373 = CARTESIAN_POINT('Ctrl Pts',(-11.2391406511197,-13.2018523859393,
116.951418845486)) ;
#189374 = CARTESIAN_POINT('Ctrl Pts',(-11.3129444988516,-13.2018523154605,
116.927187816934)) ;
#189375 = CARTESIAN_POINT('Ctrl Pts',(-11.3867483465836,-13.2018522449817,
116.902956788382)) ;
#189376 = CARTESIAN_POINT('Ctrl Pts',(-11.4099894577055,-13.2163226304817,
116.973745461531)) ;
#189377 = CARTESIAN_POINT('Ctrl Pts',(-11.3947104282053,-13.5056990228868,
116.962500660225)) ;
#189378 = CARTESIAN_POINT('Ctrl Pts',(-11.4183215240288,-13.4999868027269,
117.034416246959)) ;
#189379 = CARTESIAN_POINT('Ctrl Pts',(-11.344517682384,-13.4999868805839,
117.058647294052)) ;
#189380 = CARTESIAN_POINT('Ctrl Pts',(-11.2707138407393,-13.499986958441,
117.082878341144)) ;
#189381 = CARTESIAN_POINT('Ctrl Pts',(-11.2471027449158,-13.5056991786008,
117.010962754411)) ;
#189382 = CARTESIAN_POINT('Ctrl Pts',(-11.2234916490923,-13.5114113987607,
116.939047167677)) ;
#189383 = CARTESIAN_POINT('Ctrl Pts',(-11.2972954907371,-13.5114113209037,
116.914816120584)) ;
#189384 = CARTESIAN_POINT('Ctrl Pts',(-11.3710993323818,-13.5114112430466,
116.890585073491)) ;
#189385 = CARTESIAN_POINT('Ctrl Pts',(-11.3947104282053,-13.5056990228868,
116.962500660225)) ;
#189386 = CARTESIAN_POINT('Ctrl Pts',(-11.4036668088478,-13.7916926696265,
117.025439420547)) ;
#189387 = CARTESIAN_POINT('Ctrl Pts',(-11.4259492352715,-13.7660050582146,
117.093308094503)) ;
#189388 = CARTESIAN_POINT('Ctrl Pts',(-11.3521454009588,-13.7660051397553,
117.117539163929)) ;
#189389 = CARTESIAN_POINT('Ctrl Pts',(-11.2783415666462,-13.766005221296,
117.141770233354)) ;
#189390 = CARTESIAN_POINT('Ctrl Pts',(-11.2560591402225,-13.791692832708,
117.073901559397)) ;
#189391 = CARTESIAN_POINT('Ctrl Pts',(-11.2337767137989,-13.81738044412,117.006032885441)) ;
#189392 = CARTESIAN_POINT('Ctrl Pts',(-11.3075805481115,-13.8173803625793,
116.981801816016)) ;
#189393 = CARTESIAN_POINT('Ctrl Pts',(-11.3813843824241,-13.8173802810385,
116.95757074659)) ;
#189394 = CARTESIAN_POINT('Ctrl Pts',(-11.4036668088478,-13.7916926696265,
117.025439420547)) ;
#189395 = CARTESIAN_POINT('Ctrl Pts',(-11.4354180827992,-14.0485418604028,
117.157509418095)) ;
#189396 = CARTESIAN_POINT('Ctrl Pts',(-11.4547844005631,-14.0048845368929,
117.216496095483)) ;
#189397 = CARTESIAN_POINT('Ctrl Pts',(-11.3809805736863,-14.0048846120398,
117.240727187556)) ;
#189398 = CARTESIAN_POINT('Ctrl Pts',(-11.3071767468095,-14.0048846871867,
117.26495827963)) ;
#189399 = CARTESIAN_POINT('Ctrl Pts',(-11.2878104290456,-14.0485420106967,
117.205971602242)) ;
#189400 = CARTESIAN_POINT('Ctrl Pts',(-11.2684441112818,-14.0921993342066,
117.146984924854)) ;
#189401 = CARTESIAN_POINT('Ctrl Pts',(-11.3422479381586,-14.0921992590597,
117.122753832781)) ;
#189402 = CARTESIAN_POINT('Ctrl Pts',(-11.4160517650354,-14.0921991839128,
117.098522740707)) ;
#189403 = CARTESIAN_POINT('Ctrl Pts',(-11.4354180827992,-14.0485418604028,
117.157509418095)) ;
#189404 = CARTESIAN_POINT('Ctrl Pts',(-11.4868177885781,-14.2607963084926,
117.349453433615)) ;
#189405 = CARTESIAN_POINT('Ctrl Pts',(-11.5018915030736,-14.2022566312554,
117.39536553396)) ;
#189406 = CARTESIAN_POINT('Ctrl Pts',(-11.4280876830046,-14.2022566928803,
117.419596646769)) ;
#189407 = CARTESIAN_POINT('Ctrl Pts',(-11.3542838629355,-14.2022567545052,
117.443827759578)) ;
#189408 = CARTESIAN_POINT('Ctrl Pts',(-11.33921014844,-14.2607964317425,117.397915659233)) ;
#189409 = CARTESIAN_POINT('Ctrl Pts',(-11.3241364339445,-14.3193361089797,
117.352003558888)) ;
#189410 = CARTESIAN_POINT('Ctrl Pts',(-11.3979402540135,-14.3193360473548,
117.327772446079)) ;
#189411 = CARTESIAN_POINT('Ctrl Pts',(-11.4717440740825,-14.3193359857299,
117.30354133327)) ;
#189412 = CARTESIAN_POINT('Ctrl Pts',(-11.4868177885781,-14.2607963084926,
117.349453433615)) ;
#189413 = CARTESIAN_POINT('Ctrl Pts',(-11.5538956508532,-14.4133855037132,
117.589310677699)) ;
#189414 = CARTESIAN_POINT('Ctrl Pts',(-11.563572812887,-14.3441068413642,
117.618785749883)) ;
#189415 = CARTESIAN_POINT('Ctrl Pts',(-11.489768998477,-14.3441068827324,
117.643016879929)) ;
#189416 = CARTESIAN_POINT('Ctrl Pts',(-11.415965184067,-14.3441069241007,
117.667248009974)) ;
#189417 = CARTESIAN_POINT('Ctrl Pts',(-11.4062880220333,-14.4133855864497,
117.63777293779)) ;
#189418 = CARTESIAN_POINT('Ctrl Pts',(-11.3966108599995,-14.4826642487988,
117.608297865606)) ;
#189419 = CARTESIAN_POINT('Ctrl Pts',(-11.4704146744095,-14.4826642074306,
117.584066735561)) ;
#189420 = CARTESIAN_POINT('Ctrl Pts',(-11.5442184888195,-14.4826641660623,
117.559835605515)) ;
#189421 = CARTESIAN_POINT('Ctrl Pts',(-11.5538956508532,-14.4133855037132,
117.589310677699)) ;
#189422 = CARTESIAN_POINT('Ctrl Pts',(-11.6305563612239,-14.4941554742073,
117.858230229529)) ;
#189423 = CARTESIAN_POINT('Ctrl Pts',(-11.6341625811807,-14.4191362246067,
117.869214191629)) ;
#189424 = CARTESIAN_POINT('Ctrl Pts',(-11.5603587701322,-14.4191362402107,
117.893445331912)) ;
#189425 = CARTESIAN_POINT('Ctrl Pts',(-11.4865549590836,-14.4191362558146,
117.917676472196)) ;
#189426 = CARTESIAN_POINT('Ctrl Pts',(-11.4829487391268,-14.4941555054153,
117.906692510097)) ;
#189427 = CARTESIAN_POINT('Ctrl Pts',(-11.4793425191701,-14.5691747550159,
117.895708547997)) ;
#189428 = CARTESIAN_POINT('Ctrl Pts',(-11.5531463302186,-14.5691747394119,
117.871477407714)) ;
#189429 = CARTESIAN_POINT('Ctrl Pts',(-11.6269501412672,-14.5691747238079,
117.84724626743)) ;
#189430 = CARTESIAN_POINT('Ctrl Pts',(-11.6305563612239,-14.4941554742073,
117.858230229529)) ;
#189431 = CARTESIAN_POINT('Ctrl Pts',(-11.7109172218611,-14.4980202636657,
118.138483857812)) ;
#189432 = CARTESIAN_POINT('Ctrl Pts',(-11.7081839997789,-14.4226207212898,
118.130158902281)) ;
#189433 = CARTESIAN_POINT('Ctrl Pts',(-11.6343801895775,-14.4226207084362,
118.154390045145)) ;
#189434 = CARTESIAN_POINT('Ctrl Pts',(-11.5605763793761,-14.4226206955826,
118.178621188009)) ;
#189435 = CARTESIAN_POINT('Ctrl Pts',(-11.5633096014583,-14.4980202379585,
118.186946143541)) ;
#189436 = CARTESIAN_POINT('Ctrl Pts',(-11.5660428235405,-14.5734197803344,
118.195271099072)) ;
#189437 = CARTESIAN_POINT('Ctrl Pts',(-11.6398466337419,-14.573419793188,
118.171039956207)) ;
#189438 = CARTESIAN_POINT('Ctrl Pts',(-11.7136504439433,-14.5734198060416,
118.146808813343)) ;
#189439 = CARTESIAN_POINT('Ctrl Pts',(-11.7109172218611,-14.4980202636657,
118.138483857812)) ;
#189440 = CARTESIAN_POINT('Ctrl Pts',(-11.7882117517516,-14.4245044594768,
118.409341495335)) ;
#189441 = CARTESIAN_POINT('Ctrl Pts',(-11.7793449549404,-14.3541263042152,
118.382334660807)) ;
#189442 = CARTESIAN_POINT('Ctrl Pts',(-11.7055411427768,-14.3541262631264,
118.406565797695)) ;
#189443 = CARTESIAN_POINT('Ctrl Pts',(-11.6317373306133,-14.3541262220375,
118.430796934583)) ;
#189444 = CARTESIAN_POINT('Ctrl Pts',(-11.6406041274246,-14.4245043772991,
118.45780376911)) ;
#189445 = CARTESIAN_POINT('Ctrl Pts',(-11.6494709242359,-14.4948825325607,
118.484810603637)) ;
#189446 = CARTESIAN_POINT('Ctrl Pts',(-11.7232747363994,-14.4948825736496,
118.46057946675)) ;
#189447 = CARTESIAN_POINT('Ctrl Pts',(-11.797078548563,-14.4948826147384,
118.436348329862)) ;
#189448 = CARTESIAN_POINT('Ctrl Pts',(-11.7882117517516,-14.4245044594768,
118.409341495335)) ;
#189449 = CARTESIAN_POINT('Ctrl Pts',(-11.8562827938217,-14.279297376843,
118.65208243579)) ;
#189450 = CARTESIAN_POINT('Ctrl Pts',(-11.8419177852559,-14.2189530105724,
118.608328935389)) ;
#189451 = CARTESIAN_POINT('Ctrl Pts',(-11.7681139685888,-14.2189529442762,
118.63256005856)) ;
#189452 = CARTESIAN_POINT('Ctrl Pts',(-11.6943101519217,-14.2189528779799,
118.65679118173)) ;
#189453 = CARTESIAN_POINT('Ctrl Pts',(-11.7086751604876,-14.2792972442505,
118.700544682131)) ;
#189454 = CARTESIAN_POINT('Ctrl Pts',(-11.7230401690534,-14.3396416105211,
118.744298182531)) ;
#189455 = CARTESIAN_POINT('Ctrl Pts',(-11.7968439857205,-14.3396416768173,
118.720067059361)) ;
#189456 = CARTESIAN_POINT('Ctrl Pts',(-11.8706478023876,-14.3396417431136,
118.69583593619)) ;
#189457 = CARTESIAN_POINT('Ctrl Pts',(-11.8562827938217,-14.279297376843,
118.65208243579)) ;
#189458 = CARTESIAN_POINT('Ctrl Pts',(-11.9097428090595,-14.0713598205673,
118.85049429419)) ;
#189459 = CARTESIAN_POINT('Ctrl Pts',(-11.8908877918867,-14.0254428843111,
118.793064952058)) ;
#189460 = CARTESIAN_POINT('Ctrl Pts',(-11.8170839684841,-14.0254427985769,
118.817296054714)) ;
#189461 = CARTESIAN_POINT('Ctrl Pts',(-11.7432801450815,-14.0254427128428,
118.841527157369)) ;
#189462 = CARTESIAN_POINT('Ctrl Pts',(-11.7621351622542,-14.0713596490991,
118.898956499501)) ;
#189463 = CARTESIAN_POINT('Ctrl Pts',(-11.780990179427,-14.1172765853553,
118.956385841632)) ;
#189464 = CARTESIAN_POINT('Ctrl Pts',(-11.8547940028297,-14.1172766710895,
118.932154738977)) ;
#189465 = CARTESIAN_POINT('Ctrl Pts',(-11.9285978262323,-14.1172767568236,
118.907923636322)) ;
#189466 = CARTESIAN_POINT('Ctrl Pts',(-11.9097428090595,-14.0713598205673,
118.85049429419)) ;
#189467 = CARTESIAN_POINT('Ctrl Pts',(-11.9435103312939,-13.8176789860274,
118.988744092681)) ;
#189468 = CARTESIAN_POINT('Ctrl Pts',(-11.9215372338277,-13.7894049725344,
118.921817581118)) ;
#189469 = CARTESIAN_POINT('Ctrl Pts',(-11.8477334023547,-13.7894048748747,
118.946048659193)) ;
#189470 = CARTESIAN_POINT('Ctrl Pts',(-11.7739295708818,-13.789404777215,
118.970279737267)) ;
#189471 = CARTESIAN_POINT('Ctrl Pts',(-11.795902668348,-13.8176787907079,
119.03720624883)) ;
#189472 = CARTESIAN_POINT('Ctrl Pts',(-11.8178757658143,-13.8459528042009,
119.104132760393)) ;
#189473 = CARTESIAN_POINT('Ctrl Pts',(-11.8916795972872,-13.8459529018606,
119.079901682319)) ;
#189474 = CARTESIAN_POINT('Ctrl Pts',(-11.9654834287601,-13.8459529995203,
119.055670604245)) ;
#189475 = CARTESIAN_POINT('Ctrl Pts',(-11.9435103312939,-13.8176789860274,
118.988744092681)) ;
#189476 = CARTESIAN_POINT('Ctrl Pts',(-11.9547796677016,-13.5347545509982,
119.058563970788)) ;
#189477 = CARTESIAN_POINT('Ctrl Pts',(-11.931252448714,-13.526191139526,118.986903855894)) ;
#189478 = CARTESIAN_POINT('Ctrl Pts',(-11.8574486085768,-13.5261910386332,
119.011134907579)) ;
#189479 = CARTESIAN_POINT('Ctrl Pts',(-11.7836447684397,-13.5261909377405,
119.035365959264)) ;
#189480 = CARTESIAN_POINT('Ctrl Pts',(-11.8071719874273,-13.5347543492127,
119.107026074158)) ;
#189481 = CARTESIAN_POINT('Ctrl Pts',(-11.8306992064149,-13.5433177606849,
119.178686189051)) ;
#189482 = CARTESIAN_POINT('Ctrl Pts',(-11.9045030465521,-13.5433178615776,
119.154455137367)) ;
#189483 = CARTESIAN_POINT('Ctrl Pts',(-11.9783068866892,-13.5433179624704,
119.130224085682)) ;
#189484 = CARTESIAN_POINT('Ctrl Pts',(-11.9547796677016,-13.5347545509982,
119.058563970788)) ;
#189485 = CARTESIAN_POINT('Ctrl Pts',(-11.9418285130168,-13.2436560304018,
119.054582905373)) ;
#189486 = CARTESIAN_POINT('Ctrl Pts',(-11.9184363705024,-13.2554035564965,
118.983334211708)) ;
#189487 = CARTESIAN_POINT('Ctrl Pts',(-11.8446325221026,-13.2554034608617,
119.007565238226)) ;
#189488 = CARTESIAN_POINT('Ctrl Pts',(-11.7708286737027,-13.2554033652269,
119.031796264744)) ;
#189489 = CARTESIAN_POINT('Ctrl Pts',(-11.7942208162171,-13.2436558391322,
119.103044958408)) ;
#189490 = CARTESIAN_POINT('Ctrl Pts',(-11.8176129587315,-13.2319083130375,
119.174293652073)) ;
#189491 = CARTESIAN_POINT('Ctrl Pts',(-11.8914168071314,-13.2319084086723,
119.150062625555)) ;
#189492 = CARTESIAN_POINT('Ctrl Pts',(-11.9652206555312,-13.2319085043071,
119.125831599037)) ;
#189493 = CARTESIAN_POINT('Ctrl Pts',(-11.9418285130168,-13.2436560304018,
119.054582905373)) ;
#189494 = CARTESIAN_POINT('Ctrl Pts',(-11.9049261358387,-12.9652204672347,
118.977628691884)) ;
#189495 = CARTESIAN_POINT('Ctrl Pts',(-11.8833418779651,-12.9964254468849,
118.911886523235)) ;
#189496 = CARTESIAN_POINT('Ctrl Pts',(-11.8095380224967,-12.9964253637305,
118.936117528223)) ;
#189497 = CARTESIAN_POINT('Ctrl Pts',(-11.7357341670283,-12.996425280576,
118.960348533212)) ;
#189498 = CARTESIAN_POINT('Ctrl Pts',(-11.7573184249019,-12.9652203009257,
119.02609070186)) ;
#189499 = CARTESIAN_POINT('Ctrl Pts',(-11.7789026827756,-12.9340153212755,
119.091832870508)) ;
#189500 = CARTESIAN_POINT('Ctrl Pts',(-11.852706538244,-12.93401540443,119.06760186552)) ;
#189501 = CARTESIAN_POINT('Ctrl Pts',(-11.9265103937124,-12.9340154875845,
119.043370860532)) ;
#189502 = CARTESIAN_POINT('Ctrl Pts',(-11.9049261358387,-12.9652204672347,
118.977628691884)) ;
#189503 = CARTESIAN_POINT('Ctrl Pts',(-11.8458933110122,-12.7189935301929,
118.833296067848)) ;
#189504 = CARTESIAN_POINT('Ctrl Pts',(-11.827664106781,-12.7674367069974,
118.777772851381)) ;
#189505 = CARTESIAN_POINT('Ctrl Pts',(-11.7538602461059,-12.7674366419676,
118.80200384051)) ;
#189506 = CARTESIAN_POINT('Ctrl Pts',(-11.6800563854307,-12.7674365769377,
118.826234829639)) ;
#189507 = CARTESIAN_POINT('Ctrl Pts',(-11.698285589662,-12.7189934001331,
118.881758046107)) ;
#189508 = CARTESIAN_POINT('Ctrl Pts',(-11.7165147938932,-12.6705502233285,
118.937281262574)) ;
#189509 = CARTESIAN_POINT('Ctrl Pts',(-11.7903186545683,-12.6705502883584,
118.913050273445)) ;
#189510 = CARTESIAN_POINT('Ctrl Pts',(-11.8641225152435,-12.6705503533883,
118.888819284315)) ;
#189511 = CARTESIAN_POINT('Ctrl Pts',(-11.8458933110122,-12.7189935301929,
118.833296067848)) ;
#189512 = CARTESIAN_POINT('Ctrl Pts',(-11.768187928547,-12.5228013953796,
118.632102371038)) ;
#189513 = CARTESIAN_POINT('Ctrl Pts',(-11.7546222310584,-12.585015703863,
118.590783443794)) ;
#189514 = CARTESIAN_POINT('Ctrl Pts',(-11.6808183674585,-12.5850156600089,
118.615014424014)) ;
#189515 = CARTESIAN_POINT('Ctrl Pts',(-11.6070145038585,-12.5850156161548,
118.639245404235)) ;
#189516 = CARTESIAN_POINT('Ctrl Pts',(-11.6205802013471,-12.5228013076713,
118.680564331479)) ;
#189517 = CARTESIAN_POINT('Ctrl Pts',(-11.6341458988357,-12.4605869991879,
118.721883258723)) ;
#189518 = CARTESIAN_POINT('Ctrl Pts',(-11.7079497624357,-12.460587043042,
118.697652278502)) ;
#189519 = CARTESIAN_POINT('Ctrl Pts',(-11.7817536260356,-12.4605870868961,
118.673421298282)) ;
#189520 = CARTESIAN_POINT('Ctrl Pts',(-11.768187928547,-12.5228013953796,
118.632102371038)) ;
#189521 = CARTESIAN_POINT('Ctrl Pts',(-11.6766862938013,-12.3908781186536,
118.388873969626)) ;
#189522 = CARTESIAN_POINT('Ctrl Pts',(-11.6687546982478,-12.462397411453,
118.364715607968)) ;
#189523 = CARTESIAN_POINT('Ctrl Pts',(-11.5949508340276,-12.4623973889088,
118.388946586299)) ;
#189524 = CARTESIAN_POINT('Ctrl Pts',(-11.5211469698073,-12.4623973663647,
118.413177564631)) ;
#189525 = CARTESIAN_POINT('Ctrl Pts',(-11.5290785653608,-12.3908780735653,
118.437335926289)) ;
#189526 = CARTESIAN_POINT('Ctrl Pts',(-11.5370101609142,-12.3193587807659,
118.461494287948)) ;
#189527 = CARTESIAN_POINT('Ctrl Pts',(-11.6108140251345,-12.3193588033101,
118.437263309616)) ;
#189528 = CARTESIAN_POINT('Ctrl Pts',(-11.6846178893547,-12.3193588258542,
118.413032331285)) ;
#189529 = CARTESIAN_POINT('Ctrl Pts',(-11.6766862938013,-12.3908781186536,
118.388873969626)) ;
#189530 = CARTESIAN_POINT('Ctrl Pts',(-11.5772683011683,-12.3325103501403,
118.121499206796)) ;
#189531 = CARTESIAN_POINT('Ctrl Pts',(-11.5755328069561,-12.4082131688575,
118.116213170239)) ;
#189532 = CARTESIAN_POINT('Ctrl Pts',(-11.5017289440862,-12.4082131654103,
118.140444152683)) ;
#189533 = CARTESIAN_POINT('Ctrl Pts',(-11.4279250812163,-12.4082131619632,
118.164675135128)) ;
#189534 = CARTESIAN_POINT('Ctrl Pts',(-11.4296605754286,-12.332510343246,
118.169961171685)) ;
#189535 = CARTESIAN_POINT('Ctrl Pts',(-11.4313960696408,-12.2568075245288,
118.175247208242)) ;
#189536 = CARTESIAN_POINT('Ctrl Pts',(-11.5051999325107,-12.2568075279759,
118.151016225798)) ;
#189537 = CARTESIAN_POINT('Ctrl Pts',(-11.5790037953806,-12.2568075314231,
118.126785243353)) ;
#189538 = CARTESIAN_POINT('Ctrl Pts',(-11.5772683011683,-12.3325103501403,
118.121499206796)) ;
#189539 = CARTESIAN_POINT('Ctrl Pts',(-11.4760325891554,-12.3519340314614,
117.848650931793)) ;
#189540 = CARTESIAN_POINT('Ctrl Pts',(-11.4806282527326,-12.4263955875959,
117.862648580506)) ;
#189541 = CARTESIAN_POINT('Ctrl Pts',(-11.4068243929883,-12.4263955990476,
117.886879572471)) ;
#189542 = CARTESIAN_POINT('Ctrl Pts',(-11.3330205332441,-12.4263956104993,
117.911110564435)) ;
#189543 = CARTESIAN_POINT('Ctrl Pts',(-11.3284248696669,-12.3519340543648,
117.897112915723)) ;
#189544 = CARTESIAN_POINT('Ctrl Pts',(-11.3238292060898,-12.2774724982303,
117.88311526701)) ;
#189545 = CARTESIAN_POINT('Ctrl Pts',(-11.397633065834,-12.2774724867786,
117.858884275046)) ;
#189546 = CARTESIAN_POINT('Ctrl Pts',(-11.4714369255783,-12.2774724753269,
117.834653283081)) ;
#189547 = CARTESIAN_POINT('Ctrl Pts',(-11.4760325891554,-12.3519340314614,
117.848650931793)) ;
#189548 = CARTESIAN_POINT('Ctrl Pts',(-11.3799644765095,-12.4474402254027,
117.591425257479)) ;
#189549 = CARTESIAN_POINT('Ctrl Pts',(-11.3905425586945,-12.5153461039576,
117.623644388164)) ;
#189550 = CARTESIAN_POINT('Ctrl Pts',(-11.31673870267,-12.5153461252544,117.647875391459)) ;
#189551 = CARTESIAN_POINT('Ctrl Pts',(-11.2429348466455,-12.5153461465513,
117.672106394753)) ;
#189552 = CARTESIAN_POINT('Ctrl Pts',(-11.2323567644604,-12.4474402679963,
117.639887264068)) ;
#189553 = CARTESIAN_POINT('Ctrl Pts',(-11.2217786822754,-12.3795343894413,
117.607668133383)) ;
#189554 = CARTESIAN_POINT('Ctrl Pts',(-11.2955825382999,-12.3795343681445,
117.583437130089)) ;
#189555 = CARTESIAN_POINT('Ctrl Pts',(-11.3693863943245,-12.3795343468477,
117.559206126794)) ;
#189556 = CARTESIAN_POINT('Ctrl Pts',(-11.3799644765095,-12.4474402254027,
117.591425257479)) ;
#189557 = CARTESIAN_POINT('Ctrl Pts',(-11.2946200779385,-12.6124878626438,
117.366945500947)) ;
#189558 = CARTESIAN_POINT('Ctrl Pts',(-11.3104392464365,-12.6689727866278,
117.415128135064)) ;
#189559 = CARTESIAN_POINT('Ctrl Pts',(-11.2366353946611,-12.6689728121277,
117.4393591513)) ;
#189560 = CARTESIAN_POINT('Ctrl Pts',(-11.1628315428857,-12.6689728376277,
117.463590167537)) ;
#189561 = CARTESIAN_POINT('Ctrl Pts',(-11.1470123743877,-12.6124879136438,
117.41540753342)) ;
#189562 = CARTESIAN_POINT('Ctrl Pts',(-11.1311932058897,-12.5560029896598,
117.367224899304)) ;
#189563 = CARTESIAN_POINT('Ctrl Pts',(-11.2049970576651,-12.5560029641598,
117.342993883067)) ;
#189564 = CARTESIAN_POINT('Ctrl Pts',(-11.2788009094405,-12.5560029386599,
117.318762866831)) ;
#189565 = CARTESIAN_POINT('Ctrl Pts',(-11.2946200779385,-12.6124878626438,
117.366945500947)) ;
#189566 = CARTESIAN_POINT('Ctrl Pts',(-11.2254931800816,-12.8359789539693,
117.191951388043)) ;
#189567 = CARTESIAN_POINT('Ctrl Pts',(-11.2454273142253,-12.8769447916209,
117.252667543749)) ;
#189568 = CARTESIAN_POINT('Ctrl Pts',(-11.1716234664004,-12.8769448154243,
117.276898572018)) ;
#189569 = CARTESIAN_POINT('Ctrl Pts',(-11.0978196185755,-12.8769448392277,
117.301129600287)) ;
#189570 = CARTESIAN_POINT('Ctrl Pts',(-11.0778854844318,-12.8359790015761,
117.240413444581)) ;
#189571 = CARTESIAN_POINT('Ctrl Pts',(-11.0579513502882,-12.7950131639245,
117.179697288875)) ;
#189572 = CARTESIAN_POINT('Ctrl Pts',(-11.131755198113,-12.7950131401211,
117.155466260606)) ;
#189573 = CARTESIAN_POINT('Ctrl Pts',(-11.2055590459379,-12.7950131163177,
117.131235232337)) ;
#189574 = CARTESIAN_POINT('Ctrl Pts',(-11.2254931800816,-12.8359789539693,
117.191951388043)) ;
#189575 = CARTESIAN_POINT('Ctrl Pts',(-11.1771457608799,-13.1004046039055,
117.080125851854)) ;
#189576 = CARTESIAN_POINT('Ctrl Pts',(-11.1997526258493,-13.1229691360916,
117.148982714559)) ;
#189577 = CARTESIAN_POINT('Ctrl Pts',(-11.1259487808142,-13.1229691554338,
117.173213751326)) ;
#189578 = CARTESIAN_POINT('Ctrl Pts',(-11.052144935779,-13.1229691747759,
117.197444788092)) ;
#189579 = CARTESIAN_POINT('Ctrl Pts',(-11.0295380708096,-13.1004046425898,
117.128587925387)) ;
#189580 = CARTESIAN_POINT('Ctrl Pts',(-11.0069312058402,-13.0778401104037,
117.059731062681)) ;
#189581 = CARTESIAN_POINT('Ctrl Pts',(-11.0807350508753,-13.0778400910615,
117.035500025915)) ;
#189582 = CARTESIAN_POINT('Ctrl Pts',(-11.1545388959105,-13.0778400717194,
117.011268989148)) ;
#189583 = CARTESIAN_POINT('Ctrl Pts',(-11.1771457608799,-13.1004046039055,
117.080125851854)) ;
#189584 = CARTESIAN_POINT('Ctrl Pts',(-11.1519710721537,-13.3877822848103,
117.038914256933)) ;
#189585 = CARTESIAN_POINT('Ctrl Pts',(-11.1756359825419,-13.3903147860949,
117.11099375541)) ;
#189586 = CARTESIAN_POINT('Ctrl Pts',(-11.1018321392159,-13.3903147988625,
117.135224797382)) ;
#189587 = CARTESIAN_POINT('Ctrl Pts',(-11.0280282958898,-13.3903148116302,
117.159455839354)) ;
#189588 = CARTESIAN_POINT('Ctrl Pts',(-11.0043633855016,-13.3877823103455,
117.087376340877)) ;
#189589 = CARTESIAN_POINT('Ctrl Pts',(-10.9806984751134,-13.3852498090609,
117.0152968424)) ;
#189590 = CARTESIAN_POINT('Ctrl Pts',(-11.0545023184394,-13.3852497962932,
116.991065800428)) ;
#189591 = CARTESIAN_POINT('Ctrl Pts',(-11.1283061617654,-13.3852497835256,
116.966834758456)) ;
#189592 = CARTESIAN_POINT('Ctrl Pts',(-11.1519710721537,-13.3877822848103,
117.038914256933)) ;
#189593 = CARTESIAN_POINT('Ctrl Pts',(-11.1511192899988,-13.6773386169807,
117.071787370231)) ;
#189594 = CARTESIAN_POINT('Ctrl Pts',(-11.1741453692937,-13.6596563698358,
117.141921092393)) ;
#189595 = CARTESIAN_POINT('Ctrl Pts',(-11.1003415265199,-13.659656376027,
117.166152136048)) ;
#189596 = CARTESIAN_POINT('Ctrl Pts',(-11.0265376837462,-13.6596563822181,
117.190383179702)) ;
#189597 = CARTESIAN_POINT('Ctrl Pts',(-11.0035116044512,-13.6773386293631,
117.120249457539)) ;
#189598 = CARTESIAN_POINT('Ctrl Pts',(-10.9804855251563,-13.695020876508,
117.050115735377)) ;
#189599 = CARTESIAN_POINT('Ctrl Pts',(-11.0542893679301,-13.6950208703168,
117.025884691723)) ;
#189600 = CARTESIAN_POINT('Ctrl Pts',(-11.1280932107038,-13.6950208641256,
117.001653648069)) ;
#189601 = CARTESIAN_POINT('Ctrl Pts',(-11.1511192899988,-13.6773386169807,
117.071787370231)) ;
#189602 = CARTESIAN_POINT('Ctrl Pts',(-11.1738411493158,-13.9481535278235,
117.176435570806)) ;
#189603 = CARTESIAN_POINT('Ctrl Pts',(-11.1945817658723,-13.9115346180425,
117.23960814232)) ;
#189604 = CARTESIAN_POINT('Ctrl Pts',(-11.1207779228081,-13.9115346192683,
117.263839185089)) ;
#189605 = CARTESIAN_POINT('Ctrl Pts',(-11.0469740797439,-13.9115346204941,
117.288070227859)) ;
#189606 = CARTESIAN_POINT('Ctrl Pts',(-11.0262334631874,-13.948153530275,
117.224897656345)) ;
#189607 = CARTESIAN_POINT('Ctrl Pts',(-11.0054928466309,-13.984772440056,
117.161725084831)) ;
#189608 = CARTESIAN_POINT('Ctrl Pts',(-11.0792966896951,-13.9847724388302,
117.137494042062)) ;
#189609 = CARTESIAN_POINT('Ctrl Pts',(-11.1531005327593,-13.9847724376044,
117.113262999292)) ;
#189610 = CARTESIAN_POINT('Ctrl Pts',(-11.1738411493158,-13.9481535278235,
117.176435570806)) ;
#189611 = CARTESIAN_POINT('Ctrl Pts',(-11.2178302810653,-14.1811353756388,
117.345891952531)) ;
#189612 = CARTESIAN_POINT('Ctrl Pts',(-11.234796139088,-14.1281930358969,
117.397567218671)) ;
#189613 = CARTESIAN_POINT('Ctrl Pts',(-11.1609922953461,-14.1281930344687,
117.421798259377)) ;
#189614 = CARTESIAN_POINT('Ctrl Pts',(-11.0871884516043,-14.1281930330404,
117.446029300082)) ;
#189615 = CARTESIAN_POINT('Ctrl Pts',(-11.0702225935816,-14.1811353727823,
117.394354033942)) ;
#189616 = CARTESIAN_POINT('Ctrl Pts',(-11.0532567355589,-14.2340777125242,
117.342678767802)) ;
#189617 = CARTESIAN_POINT('Ctrl Pts',(-11.1270605793008,-14.2340777139524,
117.318447727097)) ;
#189618 = CARTESIAN_POINT('Ctrl Pts',(-11.2008644230427,-14.2340777153806,
117.294216686391)) ;
#189619 = CARTESIAN_POINT('Ctrl Pts',(-11.2178302810653,-14.1811353756388,
117.345891952531)) ;
#189620 = CARTESIAN_POINT('Ctrl Pts',(-11.2789434257265,-14.3592804603128,
117.567414573632)) ;
#189621 = CARTESIAN_POINT('Ctrl Pts',(-11.2909348548221,-14.2938199374356,
117.603938531914)) ;
#189622 = CARTESIAN_POINT('Ctrl Pts',(-11.2171310104801,-14.2938199356805,
117.628169570792)) ;
#189623 = CARTESIAN_POINT('Ctrl Pts',(-11.1433271661381,-14.2938199339254,
117.652400609669)) ;
#189624 = CARTESIAN_POINT('Ctrl Pts',(-11.1313357370424,-14.3592804568026,
117.615876651387)) ;
#189625 = CARTESIAN_POINT('Ctrl Pts',(-11.1193443079467,-14.4247409796798,
117.579352693104)) ;
#189626 = CARTESIAN_POINT('Ctrl Pts',(-11.1931481522888,-14.4247409814349,
117.555121654227)) ;
#189627 = CARTESIAN_POINT('Ctrl Pts',(-11.2669519966308,-14.4247409831899,
117.530890615349)) ;
#189628 = CARTESIAN_POINT('Ctrl Pts',(-11.2789434257265,-14.3592804603128,
117.567414573632)) ;
#189629 = CARTESIAN_POINT('Ctrl Pts',(-11.3529530376374,-14.4707867328028,
117.82855139819)) ;
#189630 = CARTESIAN_POINT('Ctrl Pts',(-11.3590548784153,-14.3974420670784,
117.847136620716)) ;
#189631 = CARTESIAN_POINT('Ctrl Pts',(-11.285251034286,-14.3974420666518,
117.871367660241)) ;
#189632 = CARTESIAN_POINT('Ctrl Pts',(-11.2114471901566,-14.3974420662252,
117.895598699767)) ;
#189633 = CARTESIAN_POINT('Ctrl Pts',(-11.2053453493787,-14.4707867319496,
117.87701347724)) ;
#189634 = CARTESIAN_POINT('Ctrl Pts',(-11.1992435086008,-14.5441313976739,
117.858428254714)) ;
#189635 = CARTESIAN_POINT('Ctrl Pts',(-11.2730473527302,-14.5441313981005,
117.834197215189)) ;
#189636 = CARTESIAN_POINT('Ctrl Pts',(-11.3468511968595,-14.5441313985271,
117.809966175664)) ;
#189637 = CARTESIAN_POINT('Ctrl Pts',(-11.3529530376374,-14.4707867328028,
117.82855139819)) ;
#189638 = CARTESIAN_POINT('Ctrl Pts',(-11.4321384096907,-14.5057904984994,
118.104989650374)) ;
#189639 = CARTESIAN_POINT('Ctrl Pts',(-11.4319904956564,-14.429894649573,
118.104539128091)) ;
#189640 = CARTESIAN_POINT('Ctrl Pts',(-11.3581866522587,-14.4298946498541,
118.128770169845)) ;
#189641 = CARTESIAN_POINT('Ctrl Pts',(-11.284382808861,-14.4298946501351,
118.153001211598)) ;
#189642 = CARTESIAN_POINT('Ctrl Pts',(-11.2845307228953,-14.5057904990616,
118.153451733882)) ;
#189643 = CARTESIAN_POINT('Ctrl Pts',(-11.2846786369295,-14.581686347988,
118.153902256165)) ;
#189644 = CARTESIAN_POINT('Ctrl Pts',(-11.3584824803272,-14.5816863477069,
118.129671214411)) ;
#189645 = CARTESIAN_POINT('Ctrl Pts',(-11.4322863237249,-14.5816863474258,
118.105440172657)) ;
#189646 = CARTESIAN_POINT('Ctrl Pts',(-11.4321384096907,-14.5057904984994,
118.104989650374)) ;
#189647 = CARTESIAN_POINT('Ctrl Pts',(-11.5115346995745,-14.4636194148643,
118.382300113082)) ;
#189648 = CARTESIAN_POINT('Ctrl Pts',(-11.5051083611355,-14.3905570608512,
118.362726522999)) ;
#189649 = CARTESIAN_POINT('Ctrl Pts',(-11.4313045190715,-14.3905570601267,
118.386957568815)) ;
#189650 = CARTESIAN_POINT('Ctrl Pts',(-11.3575006770075,-14.3905570594022,
118.411188614631)) ;
#189651 = CARTESIAN_POINT('Ctrl Pts',(-11.3639270154464,-14.4636194134152,
118.430762204714)) ;
#189652 = CARTESIAN_POINT('Ctrl Pts',(-11.3703533538854,-14.5366817674283,
118.450335794797)) ;
#189653 = CARTESIAN_POINT('Ctrl Pts',(-11.4441571959494,-14.5366817681528,
118.426104748981)) ;
#189654 = CARTESIAN_POINT('Ctrl Pts',(-11.5179610380134,-14.5366817688773,
118.401873703165)) ;
#189655 = CARTESIAN_POINT('Ctrl Pts',(-11.5115346995745,-14.4636194148643,
118.382300113082)) ;
#189656 = CARTESIAN_POINT('Ctrl Pts',(-11.5841867566869,-14.3461280489561,
118.639074111226)) ;
#189657 = CARTESIAN_POINT('Ctrl Pts',(-11.5719437539166,-14.2811630148822,
118.601783899988)) ;
#189658 = CARTESIAN_POINT('Ctrl Pts',(-11.4981399133463,-14.2811630098894,
118.626014950353)) ;
#189659 = CARTESIAN_POINT('Ctrl Pts',(-11.4243360727761,-14.2811630048965,
118.650246000719)) ;
#189660 = CARTESIAN_POINT('Ctrl Pts',(-11.4365790755464,-14.3461280389704,
118.687536211957)) ;
#189661 = CARTESIAN_POINT('Ctrl Pts',(-11.4488220783168,-14.4110930730442,
118.724826423195)) ;
#189662 = CARTESIAN_POINT('Ctrl Pts',(-11.522625918887,-14.4110930780371,
118.70059537283)) ;
#189663 = CARTESIAN_POINT('Ctrl Pts',(-11.5964297594572,-14.41109308303,118.676364322464)) ;
#189664 = CARTESIAN_POINT('Ctrl Pts',(-11.5841867566869,-14.3461280489561,
118.639074111226)) ;
#189665 = CARTESIAN_POINT('Ctrl Pts',(-11.6440388517106,-14.1630186070769,
118.856745565544)) ;
#189666 = CARTESIAN_POINT('Ctrl Pts',(-11.6268671158057,-14.1107446176607,
118.80444322831)) ;
#189667 = CARTESIAN_POINT('Ctrl Pts',(-11.5530632760904,-14.1107446061865,
118.828674281279)) ;
#189668 = CARTESIAN_POINT('Ctrl Pts',(-11.4792594363752,-14.1107445947124,
118.852905334249)) ;
#189669 = CARTESIAN_POINT('Ctrl Pts',(-11.49643117228,-14.1630185841287,118.905207671484)) ;
#189670 = CARTESIAN_POINT('Ctrl Pts',(-11.5136029081849,-14.215292573545,
118.957510008719)) ;
#189671 = CARTESIAN_POINT('Ctrl Pts',(-11.5874067479002,-14.2152925850191,
118.933278955749)) ;
#189672 = CARTESIAN_POINT('Ctrl Pts',(-11.6612105876154,-14.2152925964932,
118.909047902779)) ;
#189673 = CARTESIAN_POINT('Ctrl Pts',(-11.6440388517106,-14.1630186070769,
118.856745565544)) ;
#189674 = CARTESIAN_POINT('Ctrl Pts',(-11.6865201020579,-13.9239936072657,
119.021875248409)) ;
#189675 = CARTESIAN_POINT('Ctrl Pts',(-11.6656175469763,-13.8883328136029,
118.95820943773)) ;
#189676 = CARTESIAN_POINT('Ctrl Pts',(-11.591813707628,-13.8883327903774,
118.982440491818)) ;
#189677 = CARTESIAN_POINT('Ctrl Pts',(-11.5180098682797,-13.8883327671519,
119.006671545905)) ;
#189678 = CARTESIAN_POINT('Ctrl Pts',(-11.5389124233613,-13.9239935608147,
119.070337356584)) ;
#189679 = CARTESIAN_POINT('Ctrl Pts',(-11.5598149784429,-13.9596543544774,
119.134003167263)) ;
#189680 = CARTESIAN_POINT('Ctrl Pts',(-11.6336188177912,-13.9596543777029,
119.109772113175)) ;
#189681 = CARTESIAN_POINT('Ctrl Pts',(-11.7074226571395,-13.9596544009284,
119.085541059088)) ;
#189682 = CARTESIAN_POINT('Ctrl Pts',(-11.6865201020579,-13.9239936072657,
119.021875248409)) ;
#189683 = CARTESIAN_POINT('Ctrl Pts',(-11.7070382005163,-13.6520857920573,
119.119617519121)) ;
#189684 = CARTESIAN_POINT('Ctrl Pts',(-11.6839436556647,-13.6353584241277,
119.049275261158)) ;
#189685 = CARTESIAN_POINT('Ctrl Pts',(-11.6101398146794,-13.6353583920573,
119.073506310259)) ;
#189686 = CARTESIAN_POINT('Ctrl Pts',(-11.5363359736941,-13.635358359987,
119.09773735936)) ;
#189687 = CARTESIAN_POINT('Ctrl Pts',(-11.5594305185456,-13.6520857279166,
119.168079617324)) ;
#189688 = CARTESIAN_POINT('Ctrl Pts',(-11.5825250633972,-13.6688130958462,
119.238421875288)) ;
#189689 = CARTESIAN_POINT('Ctrl Pts',(-11.6563289043825,-13.6688131279166,
119.214190826187)) ;
#189690 = CARTESIAN_POINT('Ctrl Pts',(-11.7301327453678,-13.668813159987,
119.189959777085)) ;
#189691 = CARTESIAN_POINT('Ctrl Pts',(-11.7070382005163,-13.6520857920573,
119.119617519121)) ;
#189692 = CARTESIAN_POINT('Ctrl Pts',(-11.7039900854668,-13.3607989189298,
119.145938172776)) ;
#189693 = CARTESIAN_POINT('Ctrl Pts',(-11.6803380884392,-13.3643850289944,
119.073898005236)) ;
#189694 = CARTESIAN_POINT('Ctrl Pts',(-11.6065342445709,-13.3643849861059,
119.098129045556)) ;
#189695 = CARTESIAN_POINT('Ctrl Pts',(-11.5327304007025,-13.3643849432174,
119.122360085876)) ;
#189696 = CARTESIAN_POINT('Ctrl Pts',(-11.5563823977301,-13.3607988331528,
119.194400253416)) ;
#189697 = CARTESIAN_POINT('Ctrl Pts',(-11.5800343947576,-13.3572127230881,
119.266440420956)) ;
#189698 = CARTESIAN_POINT('Ctrl Pts',(-11.653838238626,-13.3572127659766,
119.242209380636)) ;
#189699 = CARTESIAN_POINT('Ctrl Pts',(-11.7276420824943,-13.3572128088652,
119.217978340316)) ;
#189700 = CARTESIAN_POINT('Ctrl Pts',(-11.7039900854668,-13.3607989189298,
119.145938172776)) ;
#189701 = CARTESIAN_POINT('Ctrl Pts',(-11.6767330335314,-13.0758433976518,
119.098233907499)) ;
#189702 = CARTESIAN_POINT('Ctrl Pts',(-11.6542192956397,-13.0993300266372,
119.029660693489)) ;
#189703 = CARTESIAN_POINT('Ctrl Pts',(-11.5804154474959,-13.0993299787843,
119.053891720787)) ;
#189704 = CARTESIAN_POINT('Ctrl Pts',(-11.5066115993522,-13.0993299309314,
119.078122748085)) ;
#189705 = CARTESIAN_POINT('Ctrl Pts',(-11.529125337244,-13.075843301946,119.146695962096)) ;
#189706 = CARTESIAN_POINT('Ctrl Pts',(-11.5516390751357,-13.0523566729605,
119.215269176106)) ;
#189707 = CARTESIAN_POINT('Ctrl Pts',(-11.6254429232794,-13.0523567208134,
119.191038148808)) ;
#189708 = CARTESIAN_POINT('Ctrl Pts',(-11.6992467714231,-13.0523567686663,
119.166807121509)) ;
#189709 = CARTESIAN_POINT('Ctrl Pts',(-11.6767330335314,-13.0758433976518,
119.098233907499)) ;
#189710 = CARTESIAN_POINT('Ctrl Pts',(-11.6263549017493,-12.8137701829539,
118.980301130087)) ;
#189711 = CARTESIAN_POINT('Ctrl Pts',(-11.606591109743,-12.8555883335488,
118.920103807366)) ;
#189712 = CARTESIAN_POINT('Ctrl Pts',(-11.5327872562889,-12.8555882837421,
118.944334818489)) ;
#189713 = CARTESIAN_POINT('Ctrl Pts',(-11.4589834028348,-12.8555882339354,
118.968565829613)) ;
#189714 = CARTESIAN_POINT('Ctrl Pts',(-11.4787471948412,-12.8137700833405,
119.028763152334)) ;
#189715 = CARTESIAN_POINT('Ctrl Pts',(-11.4985109868476,-12.7719519327456,
119.088960475056)) ;
#189716 = CARTESIAN_POINT('Ctrl Pts',(-11.5723148403017,-12.7719519825523,
119.064729463932)) ;
#189717 = CARTESIAN_POINT('Ctrl Pts',(-11.6461186937557,-12.771952032359,
119.040498452808)) ;
#189718 = CARTESIAN_POINT('Ctrl Pts',(-11.6263549017493,-12.8137701829539,
118.980301130087)) ;
#189719 = CARTESIAN_POINT('Ctrl Pts',(-11.5554224404524,-12.5948352961054,
118.79984493087)) ;
#189720 = CARTESIAN_POINT('Ctrl Pts',(-11.5398458335298,-12.6519997752805,
118.75240109813)) ;
#189721 = CARTESIAN_POINT('Ctrl Pts',(-11.4660419740139,-12.6519997298115,
118.776632090791)) ;
#189722 = CARTESIAN_POINT('Ctrl Pts',(-11.392238114498,-12.6519996843424,
118.800863083451)) ;
#189723 = CARTESIAN_POINT('Ctrl Pts',(-11.4078147214206,-12.5948352051674,
118.848306916191)) ;
#189724 = CARTESIAN_POINT('Ctrl Pts',(-11.4233913283432,-12.5376707259923,
118.89575074893)) ;
#189725 = CARTESIAN_POINT('Ctrl Pts',(-11.4971951878591,-12.5376707714613,
118.87151975627)) ;
#189726 = CARTESIAN_POINT('Ctrl Pts',(-11.570999047375,-12.5376708169303,
118.84728876361)) ;
#189727 = CARTESIAN_POINT('Ctrl Pts',(-11.5554224404524,-12.5948352961054,
118.79984493087)) ;
#189728 = CARTESIAN_POINT('Ctrl Pts',(-11.4693499814157,-12.4363827345609,
118.57295586756)) ;
#189729 = CARTESIAN_POINT('Ctrl Pts',(-11.4590304335375,-12.5046923403289,
118.541524188328)) ;
#189730 = CARTESIAN_POINT('Ctrl Pts',(-11.3852265691063,-12.5046923075435,
118.565755166016)) ;
#189731 = CARTESIAN_POINT('Ctrl Pts',(-11.311422704675,-12.5046922747581,
118.589986143705)) ;
#189732 = CARTESIAN_POINT('Ctrl Pts',(-11.3217422525532,-12.4363826689901,
118.621417822938)) ;
#189733 = CARTESIAN_POINT('Ctrl Pts',(-11.3320618004314,-12.368073063222,
118.65284950217)) ;
#189734 = CARTESIAN_POINT('Ctrl Pts',(-11.4058656648627,-12.3680730960074,
118.628618524481)) ;
#189735 = CARTESIAN_POINT('Ctrl Pts',(-11.4796695292939,-12.3680731287928,
118.604387546793)) ;
#189736 = CARTESIAN_POINT('Ctrl Pts',(-11.4693499814157,-12.4363827345609,
118.57295586756)) ;
#189737 = CARTESIAN_POINT('Ctrl Pts',(-11.372312899221,-12.3469185629382,
118.312891406487)) ;
#189738 = CARTESIAN_POINT('Ctrl Pts',(-11.3680187374058,-12.4215734203002,
118.299812080862)) ;
#189739 = CARTESIAN_POINT('Ctrl Pts',(-11.2942148686676,-12.4215734050828,
118.324043045432)) ;
#189740 = CARTESIAN_POINT('Ctrl Pts',(-11.2204109999293,-12.4215733898654,
118.348274010003)) ;
#189741 = CARTESIAN_POINT('Ctrl Pts',(-11.2247051617446,-12.3469185325034,
118.361353335628)) ;
#189742 = CARTESIAN_POINT('Ctrl Pts',(-11.2289993235598,-12.2722636751415,
118.374432661253)) ;
#189743 = CARTESIAN_POINT('Ctrl Pts',(-11.302803192298,-12.2722636903589,
118.350201696683)) ;
#189744 = CARTESIAN_POINT('Ctrl Pts',(-11.3766070610363,-12.2722637055763,
118.325970732112)) ;
#189745 = CARTESIAN_POINT('Ctrl Pts',(-11.372312899221,-12.3469185629382,
118.312891406487)) ;
#189746 = CARTESIAN_POINT('Ctrl Pts',(-11.270758988364,-12.3346897142696,
118.039141827272)) ;
#189747 = CARTESIAN_POINT('Ctrl Pts',(-11.272812768128,-12.410307219777,118.04539730732)) ;
#189748 = CARTESIAN_POINT('Ctrl Pts',(-11.1990088967919,-12.4103072275808,
118.069628263978)) ;
#189749 = CARTESIAN_POINT('Ctrl Pts',(-11.1252050254558,-12.4103072353845,
118.093859220636)) ;
#189750 = CARTESIAN_POINT('Ctrl Pts',(-11.1231512456917,-12.3346897298771,
118.087603740587)) ;
#189751 = CARTESIAN_POINT('Ctrl Pts',(-11.1210974659277,-12.2590722243697,
118.081348260539)) ;
#189752 = CARTESIAN_POINT('Ctrl Pts',(-11.1949013372638,-12.259072216566,
118.057117303881)) ;
#189753 = CARTESIAN_POINT('Ctrl Pts',(-11.2687052085999,-12.2590722087622,
118.032886347224)) ;
#189754 = CARTESIAN_POINT('Ctrl Pts',(-11.270758988364,-12.3346897142696,
118.039141827272)) ;
#189755 = CARTESIAN_POINT('Ctrl Pts',(-11.1721007998187,-12.3996707792268,
117.77397409113)) ;
#189756 = CARTESIAN_POINT('Ctrl Pts',(-11.1803145318333,-12.470861286488,
117.798991791736)) ;
#189757 = CARTESIAN_POINT('Ctrl Pts',(-11.1065106607222,-12.4708613194526,
117.823222749078)) ;
#189758 = CARTESIAN_POINT('Ctrl Pts',(-11.032706789611,-12.4708613524172,
117.847453706421)) ;
#189759 = CARTESIAN_POINT('Ctrl Pts',(-11.0244930575963,-12.3996708451561,
117.822436005816)) ;
#189760 = CARTESIAN_POINT('Ctrl Pts',(-11.0162793255817,-12.3284803378949,
117.797418305211)) ;
#189761 = CARTESIAN_POINT('Ctrl Pts',(-11.0900831966928,-12.3284803049303,
117.773187347868)) ;
#189762 = CARTESIAN_POINT('Ctrl Pts',(-11.163887067804,-12.3284802719657,
117.748956390525)) ;
#189763 = CARTESIAN_POINT('Ctrl Pts',(-11.1721007998187,-12.3996707792268,
117.77397409113)) ;
#189764 = CARTESIAN_POINT('Ctrl Pts',(-11.0813833295911,-12.5380776390174,
117.5332221053)) ;
#189765 = CARTESIAN_POINT('Ctrl Pts',(-11.0952068472566,-12.5997094329327,
117.575326307758)) ;
#189766 = CARTESIAN_POINT('Ctrl Pts',(-11.0214029785273,-12.5997094914945,
117.599557272356)) ;
#189767 = CARTESIAN_POINT('Ctrl Pts',(-10.9475991097979,-12.5997095500564,
117.623788236953)) ;
#189768 = CARTESIAN_POINT('Ctrl Pts',(-10.9337755921324,-12.5380777561411,
117.581684034495)) ;
#189769 = CARTESIAN_POINT('Ctrl Pts',(-10.9199520744669,-12.4764459622258,
117.539579832036)) ;
#189770 = CARTESIAN_POINT('Ctrl Pts',(-10.9937559431962,-12.476445903664,
117.515348867439)) ;
#189771 = CARTESIAN_POINT('Ctrl Pts',(-11.0675598119255,-12.4764458451021,
117.491117902841)) ;
#189772 = CARTESIAN_POINT('Ctrl Pts',(-11.0813833295911,-12.5380776390174,
117.5332221053)) ;
#189773 = CARTESIAN_POINT('Ctrl Pts',(-11.0052275153054,-12.739380812412,
117.336728726965)) ;
#189774 = CARTESIAN_POINT('Ctrl Pts',(-11.0236543762053,-12.7870487344557,
117.392853970097)) ;
#189775 = CARTESIAN_POINT('Ctrl Pts',(-10.9498505125397,-12.7870488154654,
117.417084950118)) ;
#189776 = CARTESIAN_POINT('Ctrl Pts',(-10.876046648874,-12.7870488964751,
117.441315930138)) ;
#189777 = CARTESIAN_POINT('Ctrl Pts',(-10.8576197879741,-12.7393809744314,
117.385190687007)) ;
#189778 = CARTESIAN_POINT('Ctrl Pts',(-10.8391929270742,-12.6917130523877,
117.329065443875)) ;
#189779 = CARTESIAN_POINT('Ctrl Pts',(-10.9129967907399,-12.691712971378,
117.304834463854)) ;
#189780 = CARTESIAN_POINT('Ctrl Pts',(-10.9868006544055,-12.6917128903682,
117.280603483834)) ;
#189781 = CARTESIAN_POINT('Ctrl Pts',(-11.0052275153054,-12.739380812412,
117.336728726965)) ;
#189782 = CARTESIAN_POINT('Ctrl Pts',(-10.9480638418633,-12.9893867745162,
117.198103000491)) ;
#189783 = CARTESIAN_POINT('Ctrl Pts',(-10.9697745011554,-13.0196703754918,
117.264230163634)) ;
#189784 = CARTESIAN_POINT('Ctrl Pts',(-10.8959706446165,-13.0196704733174,
117.288461165362)) ;
#189785 = CARTESIAN_POINT('Ctrl Pts',(-10.8221667880775,-13.019670571143,
117.312692167089)) ;
#189786 = CARTESIAN_POINT('Ctrl Pts',(-10.8004561287854,-12.9893869701674,
117.246565003946)) ;
#189787 = CARTESIAN_POINT('Ctrl Pts',(-10.7787454694932,-12.9591033691919,
117.180437840802)) ;
#189788 = CARTESIAN_POINT('Ctrl Pts',(-10.8525493260322,-12.9591032713663,
117.156206839075)) ;
#189789 = CARTESIAN_POINT('Ctrl Pts',(-10.9263531825711,-12.9591031735407,
117.131975837347)) ;
#189790 = CARTESIAN_POINT('Ctrl Pts',(-10.9480638418633,-12.9893867745162,
117.198103000491)) ;
#189791 = CARTESIAN_POINT('Ctrl Pts',(-10.91326793993,-13.2694171615401,117.12751697522)) ;
#189792 = CARTESIAN_POINT('Ctrl Pts',(-10.9367074543696,-13.2801946819997,
117.198909952163)) ;
#189793 = CARTESIAN_POINT('Ctrl Pts',(-10.8629036063477,-13.2801947890163,
117.223140979832)) ;
#189794 = CARTESIAN_POINT('Ctrl Pts',(-10.7890997583258,-13.2801948960329,
117.247372007501)) ;
#189795 = CARTESIAN_POINT('Ctrl Pts',(-10.7656602438862,-13.2694173755733,
117.175979030557)) ;
#189796 = CARTESIAN_POINT('Ctrl Pts',(-10.7422207294466,-13.2586398551137,
117.104586053614)) ;
#189797 = CARTESIAN_POINT('Ctrl Pts',(-10.8160245774685,-13.2586397480971,
117.080355025945)) ;
#189798 = CARTESIAN_POINT('Ctrl Pts',(-10.8898284254904,-13.2586396410806,
117.056123998276)) ;
#189799 = CARTESIAN_POINT('Ctrl Pts',(-10.91326793993,-13.2694171615401,117.12751697522)) ;
#189800 = CARTESIAN_POINT('Ctrl Pts',(-10.9025452534367,-13.5619468890867,
117.130491501621)) ;
#189801 = CARTESIAN_POINT('Ctrl Pts',(-10.9260309116402,-13.5523172456924,
117.202025025017)) ;
#189802 = CARTESIAN_POINT('Ctrl Pts',(-10.8522270727192,-13.5523173531236,
117.226256080406)) ;
#189803 = CARTESIAN_POINT('Ctrl Pts',(-10.7784232337981,-13.5523174605549,
117.250487135794)) ;
#189804 = CARTESIAN_POINT('Ctrl Pts',(-10.7549375755945,-13.5619471039492,
117.178953612398)) ;
#189805 = CARTESIAN_POINT('Ctrl Pts',(-10.7314519173909,-13.5715767473435,
117.107420089002)) ;
#189806 = CARTESIAN_POINT('Ctrl Pts',(-10.805255756312,-13.5715766399123,
117.083189033613)) ;
#189807 = CARTESIAN_POINT('Ctrl Pts',(-10.8790595952331,-13.5715765324811,
117.058957978225)) ;
#189808 = CARTESIAN_POINT('Ctrl Pts',(-10.9025452534367,-13.5619468890867,
117.130491501621)) ;
#189809 = CARTESIAN_POINT('Ctrl Pts',(-10.915841183644,-13.8411213292838,
117.206227086059)) ;
#189810 = CARTESIAN_POINT('Ctrl Pts',(-10.937704050494,-13.8119862931275,
117.272817848839)) ;
#189811 = CARTESIAN_POINT('Ctrl Pts',(-10.8639002202108,-13.8119863923944,
117.297048930537)) ;
#189812 = CARTESIAN_POINT('Ctrl Pts',(-10.7900963899276,-13.8119864916613,
117.321280012236)) ;
#189813 = CARTESIAN_POINT('Ctrl Pts',(-10.7682335230776,-13.8411215278176,
117.254689249455)) ;
#189814 = CARTESIAN_POINT('Ctrl Pts',(-10.7463706562276,-13.870256563974,
117.188098486674)) ;
#189815 = CARTESIAN_POINT('Ctrl Pts',(-10.8201744865108,-13.8702564647071,
117.163867404976)) ;
#189816 = CARTESIAN_POINT('Ctrl Pts',(-10.893978316794,-13.8702563654402,
117.139636323278)) ;
#189817 = CARTESIAN_POINT('Ctrl Pts',(-10.915841183644,-13.8411213292838,
117.206227086059)) ;
#189818 = CARTESIAN_POINT('Ctrl Pts',(-10.9516849884551,-14.0928083771544,
117.351013070944)) ;
#189819 = CARTESIAN_POINT('Ctrl Pts',(-10.9703412062463,-14.0460580395473,
117.407836898122)) ;
#189820 = CARTESIAN_POINT('Ctrl Pts',(-10.8965373833647,-14.0460581223417,
117.432068002364)) ;
#189821 = CARTESIAN_POINT('Ctrl Pts',(-10.822733560483,-14.0460582051361,
117.456299106607)) ;
#189822 = CARTESIAN_POINT('Ctrl Pts',(-10.8040773426918,-14.0928085427432,
117.399475279428)) ;
#189823 = CARTESIAN_POINT('Ctrl Pts',(-10.7854211249006,-14.1395588803503,
117.34265145225)) ;
#189824 = CARTESIAN_POINT('Ctrl Pts',(-10.8592249477822,-14.1395587975559,
117.318420348007)) ;
#189825 = CARTESIAN_POINT('Ctrl Pts',(-10.9330287706639,-14.1395587147615,
117.294189243765)) ;
#189826 = CARTESIAN_POINT('Ctrl Pts',(-10.9516849884551,-14.0928083771544,
117.351013070944)) ;
#189827 = CARTESIAN_POINT('Ctrl Pts',(-11.0064738727342,-14.2946225939457,
117.553299701914)) ;
#189828 = CARTESIAN_POINT('Ctrl Pts',(-11.0206000342901,-14.2337123839225,
117.596325708778)) ;
#189829 = CARTESIAN_POINT('Ctrl Pts',(-10.9467962167889,-14.2337124445756,
117.620556829408)) ;
#189830 = CARTESIAN_POINT('Ctrl Pts',(-10.8729923992877,-14.2337125052288,
117.644787950038)) ;
#189831 = CARTESIAN_POINT('Ctrl Pts',(-10.8588662377318,-14.2946227152521,
117.601761943175)) ;
#189832 = CARTESIAN_POINT('Ctrl Pts',(-10.8447400761759,-14.3555329252753,
117.558735936311)) ;
#189833 = CARTESIAN_POINT('Ctrl Pts',(-10.9185438936771,-14.3555328646222,
117.534504815681)) ;
#189834 = CARTESIAN_POINT('Ctrl Pts',(-10.9923477111784,-14.355532803969,
117.510273695051)) ;
#189835 = CARTESIAN_POINT('Ctrl Pts',(-11.0064738727342,-14.2946225939457,
117.553299701914)) ;
#189836 = CARTESIAN_POINT('Ctrl Pts',(-11.0756251998262,-14.4342154714355,
117.79936755511)) ;
#189837 = CARTESIAN_POINT('Ctrl Pts',(-11.0842111585001,-14.3634681415102,
117.825518997977)) ;
#189838 = CARTESIAN_POINT('Ctrl Pts',(-11.0104073439954,-14.3634681764234,
117.849750127735)) ;
#189839 = CARTESIAN_POINT('Ctrl Pts',(-10.9366035294908,-14.3634682113365,
117.873981257492)) ;
#189840 = CARTESIAN_POINT('Ctrl Pts',(-10.9280175708169,-14.4342155412618,
117.847829814624)) ;
#189841 = CARTESIAN_POINT('Ctrl Pts',(-10.919431612143,-14.5049628711871,
117.821678371757)) ;
#189842 = CARTESIAN_POINT('Ctrl Pts',(-10.9932354266477,-14.5049628362739,
117.797447241999)) ;
#189843 = CARTESIAN_POINT('Ctrl Pts',(-11.0670392411523,-14.5049628013607,
117.773216112242)) ;
#189844 = CARTESIAN_POINT('Ctrl Pts',(-11.0756251998262,-14.4342154714355,
117.79936755511)) ;
#189845 = CARTESIAN_POINT('Ctrl Pts',(-11.153880257495,-14.5009486089819,
118.073339050419)) ;
#189846 = CARTESIAN_POINT('Ctrl Pts',(-11.156278566929,-14.4254353908754,
118.080643912192)) ;
#189847 = CARTESIAN_POINT('Ctrl Pts',(-11.0824747524078,-14.4254353992881,
118.104875041898)) ;
#189848 = CARTESIAN_POINT('Ctrl Pts',(-11.0086709378866,-14.4254354077009,
118.129106171605)) ;
#189849 = CARTESIAN_POINT('Ctrl Pts',(-11.0062726284526,-14.5009486258073,
118.121801309832)) ;
#189850 = CARTESIAN_POINT('Ctrl Pts',(-11.0038743190187,-14.5764618439138,
118.114496448059)) ;
#189851 = CARTESIAN_POINT('Ctrl Pts',(-11.0776781335399,-14.5764618355011,
118.090265318352)) ;
#189852 = CARTESIAN_POINT('Ctrl Pts',(-11.1514819480611,-14.5764618270883,
118.066034188645)) ;
#189853 = CARTESIAN_POINT('Ctrl Pts',(-11.153880257495,-14.5009486089819,
118.073339050419)) ;
#189854 = CARTESIAN_POINT('Ctrl Pts',(-11.2337163322941,-14.4900601303297,
118.351780652459)) ;
#189855 = CARTESIAN_POINT('Ctrl Pts',(-11.2298142925024,-14.4151940072696,
118.339895667138)) ;
#189856 = CARTESIAN_POINT('Ctrl Pts',(-11.1560104761921,-14.4151939916633,
118.364126791396)) ;
#189857 = CARTESIAN_POINT('Ctrl Pts',(-11.0822066598818,-14.4151939760569,
118.388357915653)) ;
#189858 = CARTESIAN_POINT('Ctrl Pts',(-11.0861086996736,-14.490060099117,
118.400242900973)) ;
#189859 = CARTESIAN_POINT('Ctrl Pts',(-11.0900107394653,-14.564926222177,
118.412127886294)) ;
#189860 = CARTESIAN_POINT('Ctrl Pts',(-11.1638145557756,-14.5649262377834,
118.387896762036)) ;
#189861 = CARTESIAN_POINT('Ctrl Pts',(-11.2376183720859,-14.5649262533898,
118.363665637779)) ;
#189862 = CARTESIAN_POINT('Ctrl Pts',(-11.2337163322941,-14.4900601303297,
118.351780652459)) ;
#189863 = CARTESIAN_POINT('Ctrl Pts',(-11.3100721441772,-14.4021465802023,
118.619936605905)) ;
#189864 = CARTESIAN_POINT('Ctrl Pts',(-11.3000967501311,-14.3333051056759,
118.589553163606)) ;
#189865 = CARTESIAN_POINT('Ctrl Pts',(-11.2262929293861,-14.3333050707066,
118.613784274357)) ;
#189866 = CARTESIAN_POINT('Ctrl Pts',(-11.1524891086412,-14.3333050357374,
118.638015385107)) ;
#189867 = CARTESIAN_POINT('Ctrl Pts',(-11.1624645026873,-14.4021465102638,
118.668398827405)) ;
#189868 = CARTESIAN_POINT('Ctrl Pts',(-11.1724398967335,-14.4709879847903,
118.698782269704)) ;
#189869 = CARTESIAN_POINT('Ctrl Pts',(-11.2462437174784,-14.4709880197595,
118.674551158953)) ;
#189870 = CARTESIAN_POINT('Ctrl Pts',(-11.3200475382233,-14.4709880547288,
118.650320048203)) ;
#189871 = CARTESIAN_POINT('Ctrl Pts',(-11.3100721441772,-14.4021465802023,
118.619936605905)) ;
#189872 = CARTESIAN_POINT('Ctrl Pts',(-11.37566907483,-14.2443882215466,118.855102173573)) ;
#189873 = CARTESIAN_POINT('Ctrl Pts',(-11.3603668518626,-14.1864574930971,
118.80849406999)) ;
#189874 = CARTESIAN_POINT('Ctrl Pts',(-11.2865630258025,-14.1864574444021,
118.832725164551)) ;
#189875 = CARTESIAN_POINT('Ctrl Pts',(-11.2127591997423,-14.1864573957072,
118.856956259112)) ;
#189876 = CARTESIAN_POINT('Ctrl Pts',(-11.2280614227097,-14.2443881241568,
118.903564362695)) ;
#189877 = CARTESIAN_POINT('Ctrl Pts',(-11.2433636456771,-14.3023188526063,
118.950172466279)) ;
#189878 = CARTESIAN_POINT('Ctrl Pts',(-11.3171674717372,-14.3023189013012,
118.925941371718)) ;
#189879 = CARTESIAN_POINT('Ctrl Pts',(-11.3909712977974,-14.3023189499961,
118.901710277157)) ;
#189880 = CARTESIAN_POINT('Ctrl Pts',(-11.37566907483,-14.2443882215466,118.855102173573)) ;
#189881 = CARTESIAN_POINT('Ctrl Pts',(-11.4258059802253,-14.0257063779415,
119.043473900735)) ;
#189882 = CARTESIAN_POINT('Ctrl Pts',(-11.4062419396678,-13.9829558305902,
118.983884988605)) ;
#189883 = CARTESIAN_POINT('Ctrl Pts',(-11.3324381072493,-13.9829557770323,
119.008116063799)) ;
#189884 = CARTESIAN_POINT('Ctrl Pts',(-11.2586342748308,-13.9829557234744,
119.032347138994)) ;
#189885 = CARTESIAN_POINT('Ctrl Pts',(-11.2781983153884,-14.0257062708258,
119.091936051124)) ;
#189886 = CARTESIAN_POINT('Ctrl Pts',(-11.2977623559459,-14.0684568181771,
119.151524963255)) ;
#189887 = CARTESIAN_POINT('Ctrl Pts',(-11.3715661883644,-14.068456871735,
119.12729388806)) ;
#189888 = CARTESIAN_POINT('Ctrl Pts',(-11.4453700207828,-14.0684569252929,
119.103062812865)) ;
#189889 = CARTESIAN_POINT('Ctrl Pts',(-11.4258059802253,-14.0257063779415,
119.043473900735)) ;
#189890 = CARTESIAN_POINT('Ctrl Pts',(-11.4553454834867,-13.7667943185538,
119.168622081409)) ;
#189891 = CARTESIAN_POINT('Ctrl Pts',(-11.4329616627383,-13.7420568683352,
119.100444573897)) ;
#189892 = CARTESIAN_POINT('Ctrl Pts',(-11.359157824951,-13.7420568128391,
119.124675632739)) ;
#189893 = CARTESIAN_POINT('Ctrl Pts',(-11.2853539871637,-13.7420567573429,
119.148906691581)) ;
#189894 = CARTESIAN_POINT('Ctrl Pts',(-11.3077378079121,-13.7667942075616,
119.217084199093)) ;
#189895 = CARTESIAN_POINT('Ctrl Pts',(-11.3301216286606,-13.7915316577803,
119.285261706605)) ;
#189896 = CARTESIAN_POINT('Ctrl Pts',(-11.4039254664479,-13.7915317132764,
119.261030647763)) ;
#189897 = CARTESIAN_POINT('Ctrl Pts',(-11.4777293042352,-13.7915317687725,
119.236799588921)) ;
#189898 = CARTESIAN_POINT('Ctrl Pts',(-11.4553454834867,-13.7667943185538,
119.168622081409)) ;
#189899 = CARTESIAN_POINT('Ctrl Pts',(-11.4621777273754,-13.4796298971122,
119.225070200418)) ;
#189900 = CARTESIAN_POINT('Ctrl Pts',(-11.438545300536,-13.4749049518927,
119.153089640415)) ;
#189901 = CARTESIAN_POINT('Ctrl Pts',(-11.3647414577201,-13.4749049038309,
119.177320683941)) ;
#189902 = CARTESIAN_POINT('Ctrl Pts',(-11.2909376149041,-13.474904855769,
119.201551727466)) ;
#189903 = CARTESIAN_POINT('Ctrl Pts',(-11.3145700417435,-13.4796298009885,
119.27353228747)) ;
#189904 = CARTESIAN_POINT('Ctrl Pts',(-11.3382024685828,-13.4843547462079,
119.345512847473)) ;
#189905 = CARTESIAN_POINT('Ctrl Pts',(-11.4120063113988,-13.4843547942698,
119.321281803947)) ;
#189906 = CARTESIAN_POINT('Ctrl Pts',(-11.4858101542147,-13.4843548423316,
119.297050760422)) ;
#189907 = CARTESIAN_POINT('Ctrl Pts',(-11.4621777273754,-13.4796298971122,
119.225070200418)) ;
#189908 = CARTESIAN_POINT('Ctrl Pts',(-11.4447439616591,-13.1904267551927,
119.207288539011)) ;
#189909 = CARTESIAN_POINT('Ctrl Pts',(-11.4215622116791,-13.2058873743104,
119.136680668146)) ;
#189910 = CARTESIAN_POINT('Ctrl Pts',(-11.3477583653682,-13.2058873346672,
119.160911701027)) ;
#189911 = CARTESIAN_POINT('Ctrl Pts',(-11.2739545190573,-13.205887295024,
119.185142733907)) ;
#189912 = CARTESIAN_POINT('Ctrl Pts',(-11.2971362690373,-13.1904266759062,
119.255750604772)) ;
#189913 = CARTESIAN_POINT('Ctrl Pts',(-11.3203180190173,-13.1749660567885,
119.326358475637)) ;
#189914 = CARTESIAN_POINT('Ctrl Pts',(-11.3941218653282,-13.1749660964317,
119.302127442757)) ;
#189915 = CARTESIAN_POINT('Ctrl Pts',(-11.4679257116391,-13.1749661360749,
119.277896409876)) ;
#189916 = CARTESIAN_POINT('Ctrl Pts',(-11.4447439616591,-13.1904267551927,
119.207288539011)) ;
#189917 = CARTESIAN_POINT('Ctrl Pts',(-11.4032367595843,-12.9149395489465,
119.11653118219)) ;
#189918 = CARTESIAN_POINT('Ctrl Pts',(-11.3821797578339,-12.9496591977343,
119.052394951809)) ;
#189919 = CARTESIAN_POINT('Ctrl Pts',(-11.3083759098325,-12.9496591712855,
119.076625979541)) ;
#189920 = CARTESIAN_POINT('Ctrl Pts',(-11.2345720618312,-12.9496591448368,
119.100857007273)) ;
#189921 = CARTESIAN_POINT('Ctrl Pts',(-11.2556290635817,-12.914939496049,
119.164993237654)) ;
#189922 = CARTESIAN_POINT('Ctrl Pts',(-11.2766860653321,-12.8802198472613,
119.229129468036)) ;
#189923 = CARTESIAN_POINT('Ctrl Pts',(-11.3504899133335,-12.88021987371,119.204898440304)) ;
#189924 = CARTESIAN_POINT('Ctrl Pts',(-11.4242937613348,-12.8802199001588,
119.180667412572)) ;
#189925 = CARTESIAN_POINT('Ctrl Pts',(-11.4032367595843,-12.9149395489465,
119.11653118219)) ;
#189926 = CARTESIAN_POINT('Ctrl Pts',(-11.34057571108,-12.6780026906519,118.960998194151)) ;
#189927 = CARTESIAN_POINT('Ctrl Pts',(-11.3231311967939,-12.7293185102392,
118.907865017845)) ;
#189928 = CARTESIAN_POINT('Ctrl Pts',(-11.2493273482835,-12.7293184935026,
118.932096044026)) ;
#189929 = CARTESIAN_POINT('Ctrl Pts',(-11.1755234997732,-12.729318476766,
118.956327070207)) ;
#189930 = CARTESIAN_POINT('Ctrl Pts',(-11.1929680140592,-12.6780026571787,
119.009460246513)) ;
#189931 = CARTESIAN_POINT('Ctrl Pts',(-11.2104125283453,-12.6266868375913,
119.062593422819)) ;
#189932 = CARTESIAN_POINT('Ctrl Pts',(-11.2842163768557,-12.6266868543279,
119.038362396638)) ;
#189933 = CARTESIAN_POINT('Ctrl Pts',(-11.3580202253661,-12.6266868710645,
119.014131370457)) ;
#189934 = CARTESIAN_POINT('Ctrl Pts',(-11.34057571108,-12.6780026906519,118.960998194151)) ;
#189935 = CARTESIAN_POINT('Ctrl Pts',(-11.2599568255112,-12.492912372698,
118.750912408693)) ;
#189936 = CARTESIAN_POINT('Ctrl Pts',(-11.2473811529661,-12.5572296336134,
118.712608938893)) ;
#189937 = CARTESIAN_POINT('Ctrl Pts',(-11.173577305252,-12.5572296258791,
118.736839967499)) ;
#189938 = CARTESIAN_POINT('Ctrl Pts',(-11.099773457538,-12.5572296181447,
118.761070996106)) ;
#189939 = CARTESIAN_POINT('Ctrl Pts',(-11.1123491300831,-12.4929123572293,
118.799374465907)) ;
#189940 = CARTESIAN_POINT('Ctrl Pts',(-11.1249248026282,-12.4285950963139,
118.837677935707)) ;
#189941 = CARTESIAN_POINT('Ctrl Pts',(-11.1987286503423,-12.4285951040482,
118.8134469071)) ;
#189942 = CARTESIAN_POINT('Ctrl Pts',(-11.2725324980563,-12.4285951117825,
118.789215878493)) ;
#189943 = CARTESIAN_POINT('Ctrl Pts',(-11.2599568255112,-12.492912372698,
118.750912408693)) ;
#189944 = CARTESIAN_POINT('Ctrl Pts',(-11.1664274260683,-12.3740385950698,
118.501529078933)) ;
#189945 = CARTESIAN_POINT('Ctrl Pts',(-11.1596290262187,-12.446753464716,
118.480822249738)) ;
#189946 = CARTESIAN_POINT('Ctrl Pts',(-11.0858251801177,-12.4467534627922,
118.505053283258)) ;
#189947 = CARTESIAN_POINT('Ctrl Pts',(-11.0120213340167,-12.4467534608683,
118.529284316778)) ;
#189948 = CARTESIAN_POINT('Ctrl Pts',(-11.0188197338663,-12.374038591222,
118.549991145973)) ;
#189949 = CARTESIAN_POINT('Ctrl Pts',(-11.0256181337159,-12.3013237215758,
118.570697975168)) ;
#189950 = CARTESIAN_POINT('Ctrl Pts',(-11.0994219798169,-12.3013237234996,
118.546466941648)) ;
#189951 = CARTESIAN_POINT('Ctrl Pts',(-11.1732258259179,-12.3013237254235,
118.522235908128)) ;
#189952 = CARTESIAN_POINT('Ctrl Pts',(-11.1664274260683,-12.3740385950698,
118.501529078933)) ;
#189953 = CARTESIAN_POINT('Ctrl Pts',(-11.0659273383696,-12.3302346237977,
118.230957628629)) ;
#189954 = CARTESIAN_POINT('Ctrl Pts',(-11.0654009453968,-12.406117742521,
118.229354320508)) ;
#189955 = CARTESIAN_POINT('Ctrl Pts',(-10.991597101039,-12.4061177428899,
118.253585359338)) ;
#189956 = CARTESIAN_POINT('Ctrl Pts',(-10.9177932566812,-12.4061177432587,
118.277816398167)) ;
#189957 = CARTESIAN_POINT('Ctrl Pts',(-10.918319649654,-12.3302346245354,
118.279419706287)) ;
#189958 = CARTESIAN_POINT('Ctrl Pts',(-10.9188460426267,-12.2543515058121,
118.281023014408)) ;
#189959 = CARTESIAN_POINT('Ctrl Pts',(-10.9926498869845,-12.2543515054432,
118.256791975578)) ;
#189960 = CARTESIAN_POINT('Ctrl Pts',(-11.0664537313423,-12.2543515050743,
118.232560936749)) ;
#189961 = CARTESIAN_POINT('Ctrl Pts',(-11.0659273383696,-12.3302346237977,
118.230957628629)) ;
#189962 = CARTESIAN_POINT('Ctrl Pts',(-10.9655287020424,-12.3639942142519,
117.960502448918)) ;
#189963 = CARTESIAN_POINT('Ctrl Pts',(-10.9712805841424,-12.4376333996041,
117.978021753744)) ;
#189964 = CARTESIAN_POINT('Ctrl Pts',(-10.8974767409502,-12.4376333997196,
118.002252796123)) ;
#189965 = CARTESIAN_POINT('Ctrl Pts',(-10.8236728977579,-12.4376333998351,
118.026483838503)) ;
#189966 = CARTESIAN_POINT('Ctrl Pts',(-10.8179210156579,-12.3639942144829,
118.008964533677)) ;
#189967 = CARTESIAN_POINT('Ctrl Pts',(-10.8121691335578,-12.2903550291307,
117.99144522885)) ;
#189968 = CARTESIAN_POINT('Ctrl Pts',(-10.8859729767501,-12.2903550290152,
117.967214186471)) ;
#189969 = CARTESIAN_POINT('Ctrl Pts',(-10.9597768199423,-12.2903550288997,
117.942983144091)) ;
#189970 = CARTESIAN_POINT('Ctrl Pts',(-10.9655287020424,-12.3639942142519,
117.960502448918)) ;
#189971 = CARTESIAN_POINT('Ctrl Pts',(-10.8702494346859,-12.4744699305646,
117.706006023523)) ;
#189972 = CARTESIAN_POINT('Ctrl Pts',(-10.8819243834061,-12.5405049323792,
117.741566033642)) ;
#189973 = CARTESIAN_POINT('Ctrl Pts',(-10.8081205408963,-12.5405049308727,
117.7657970781)) ;
#189974 = CARTESIAN_POINT('Ctrl Pts',(-10.7343166983866,-12.5405049293662,
117.790028122558)) ;
#189975 = CARTESIAN_POINT('Ctrl Pts',(-10.7226417496664,-12.4744699275516,
117.75446811244)) ;
#189976 = CARTESIAN_POINT('Ctrl Pts',(-10.7109668009462,-12.408434925737,
117.718908102322)) ;
#189977 = CARTESIAN_POINT('Ctrl Pts',(-10.784770643456,-12.4084349272435,
117.694677057863)) ;
#189978 = CARTESIAN_POINT('Ctrl Pts',(-10.8585744859657,-12.40843492875,117.670446013405)) ;
#189979 = CARTESIAN_POINT('Ctrl Pts',(-10.8702494346859,-12.4744699305646,
117.706006023523)) ;
#189980 = CARTESIAN_POINT('Ctrl Pts',(-10.7883722736656,-12.6502203530517,
117.491779654815)) ;
#189981 = CARTESIAN_POINT('Ctrl Pts',(-10.8050539911803,-12.7040802804882,
117.542589474842)) ;
#189982 = CARTESIAN_POINT('Ctrl Pts',(-10.7312501484571,-12.7040802781189,
117.56682051865)) ;
#189983 = CARTESIAN_POINT('Ctrl Pts',(-10.6574463057339,-12.7040802757496,
117.591051562459)) ;
#189984 = CARTESIAN_POINT('Ctrl Pts',(-10.6407645882193,-12.6502203483131,
117.540241742432)) ;
#189985 = CARTESIAN_POINT('Ctrl Pts',(-10.6240828707046,-12.5963604208767,
117.489431922405)) ;
#189986 = CARTESIAN_POINT('Ctrl Pts',(-10.6978867134277,-12.596360423246,
117.465200878597)) ;
#189987 = CARTESIAN_POINT('Ctrl Pts',(-10.7716905561509,-12.5963604256153,
117.440969834788)) ;
#189988 = CARTESIAN_POINT('Ctrl Pts',(-10.7883722736656,-12.6502203530517,
117.491779654815)) ;
#189989 = CARTESIAN_POINT('Ctrl Pts',(-10.7226751288005,-12.8831101738135,
117.32729459891)) ;
#189990 = CARTESIAN_POINT('Ctrl Pts',(-10.7432320047121,-12.9207872316337,
117.389907526118)) ;
#189991 = CARTESIAN_POINT('Ctrl Pts',(-10.669428161409,-12.9207872305233,
117.41413856816)) ;
#189992 = CARTESIAN_POINT('Ctrl Pts',(-10.5956243181059,-12.9207872294128,
117.438369610202)) ;
#189993 = CARTESIAN_POINT('Ctrl Pts',(-10.5750674421944,-12.8831101715926,
117.375756682994)) ;
#189994 = CARTESIAN_POINT('Ctrl Pts',(-10.5545105662828,-12.8454331137723,
117.313143755785)) ;
#189995 = CARTESIAN_POINT('Ctrl Pts',(-10.6283144095859,-12.8454331148828,
117.288912713743)) ;
#189996 = CARTESIAN_POINT('Ctrl Pts',(-10.702118252889,-12.8454331159932,
117.264681671701)) ;
#189997 = CARTESIAN_POINT('Ctrl Pts',(-10.7226751288005,-12.8831101738135,
117.32729459891)) ;
#189998 = CARTESIAN_POINT('Ctrl Pts',(-10.6785821123709,-13.1530763913863,
117.228387939344)) ;
#189999 = CARTESIAN_POINT('Ctrl Pts',(-10.7015154333077,-13.1719578711027,
117.298239134592)) ;
#190000 = CARTESIAN_POINT('Ctrl Pts',(-10.6277115895755,-13.1719578734333,
117.322470175327)) ;
#190001 = CARTESIAN_POINT('Ctrl Pts',(-10.5539077458432,-13.1719578757638,
117.346701216061)) ;
#190002 = CARTESIAN_POINT('Ctrl Pts',(-10.5309744249064,-13.1530763960474,
117.276850020814)) ;
#190003 = CARTESIAN_POINT('Ctrl Pts',(-10.5080411039696,-13.134194916331,
117.206998825567)) ;
#190004 = CARTESIAN_POINT('Ctrl Pts',(-10.5818449477019,-13.1341949140004,
117.182767784832)) ;
#190005 = CARTESIAN_POINT('Ctrl Pts',(-10.6556487914341,-13.1341949116699,
117.158536744097)) ;
#190006 = CARTESIAN_POINT('Ctrl Pts',(-10.6785821123709,-13.1530763913863,
117.228387939344)) ;
#190007 = CARTESIAN_POINT('Ctrl Pts',(-10.6579116055234,-13.4431032907692,
117.20097789324)) ;
#190008 = CARTESIAN_POINT('Ctrl Pts',(-10.6815861390285,-13.4417610754161,
117.273086702264)) ;
#190009 = CARTESIAN_POINT('Ctrl Pts',(-10.6077822955129,-13.4417610837383,
117.297317743659)) ;
#190010 = CARTESIAN_POINT('Ctrl Pts',(-10.5339784519973,-13.4417610920606,
117.321548785054)) ;
#190011 = CARTESIAN_POINT('Ctrl Pts',(-10.5103039184922,-13.4431033074138,
117.24943997603)) ;
#190012 = CARTESIAN_POINT('Ctrl Pts',(-10.486629384987,-13.4444455227669,
117.177331167006)) ;
#190013 = CARTESIAN_POINT('Ctrl Pts',(-10.5604332285026,-13.4444455144446,
117.153100125611)) ;
#190014 = CARTESIAN_POINT('Ctrl Pts',(-10.6342370720182,-13.4444455061224,
117.128869084216)) ;
#190015 = CARTESIAN_POINT('Ctrl Pts',(-10.6579116055234,-13.4431032907692,
117.20097789324)) ;
#190016 = CARTESIAN_POINT('Ctrl Pts',(-10.6616166491097,-13.7301505723016,
117.247656025822)) ;
#190017 = CARTESIAN_POINT('Ctrl Pts',(-10.684334421916,-13.7087638139034,
117.316850696012)) ;
#190018 = CARTESIAN_POINT('Ctrl Pts',(-10.6105305796162,-13.7087638278677,
117.34108174111)) ;
#190019 = CARTESIAN_POINT('Ctrl Pts',(-10.5367267373163,-13.7087638418319,
117.365312786208)) ;
#190020 = CARTESIAN_POINT('Ctrl Pts',(-10.5140089645101,-13.7301506002301,
117.296118116017)) ;
#190021 = CARTESIAN_POINT('Ctrl Pts',(-10.4912911917038,-13.7515373586284,
117.226923445826)) ;
#190022 = CARTESIAN_POINT('Ctrl Pts',(-10.5650950340036,-13.7515373446641,
117.202692400729)) ;
#190023 = CARTESIAN_POINT('Ctrl Pts',(-10.6388988763035,-13.7515373306999,
117.178461355631)) ;
#190024 = CARTESIAN_POINT('Ctrl Pts',(-10.6616166491097,-13.7301505723016,
117.247656025822)) ;
#190025 = CARTESIAN_POINT('Ctrl Pts',(-10.6885692655636,-13.9953629945928,
117.365213136604)) ;
#190026 = CARTESIAN_POINT('Ctrl Pts',(-10.708704220682,-13.9554274129798,
117.426540960711)) ;
#190027 = CARTESIAN_POINT('Ctrl Pts',(-10.6349003807089,-13.9554274317702,
117.450772012895)) ;
#190028 = CARTESIAN_POINT('Ctrl Pts',(-10.5610965407357,-13.9554274505607,
117.47500306508)) ;
#190029 = CARTESIAN_POINT('Ctrl Pts',(-10.5409615856173,-13.9953630321736,
117.413675240973)) ;
#190030 = CARTESIAN_POINT('Ctrl Pts',(-10.5208266304989,-14.0352986137866,
117.352347416867)) ;
#190031 = CARTESIAN_POINT('Ctrl Pts',(-10.5946304704721,-14.0352985949962,
117.328116364682)) ;
#190032 = CARTESIAN_POINT('Ctrl Pts',(-10.6684343104452,-14.0352985762058,
117.303885312498)) ;
#190033 = CARTESIAN_POINT('Ctrl Pts',(-10.6885692655636,-13.9953629945928,
117.365213136604)) ;
#190034 = CARTESIAN_POINT('Ctrl Pts',(-10.7360390503692,-14.2191243988368,
117.545218751564)) ;
#190035 = CARTESIAN_POINT('Ctrl Pts',(-10.7521557686961,-14.1635077763497,
117.594307674595)) ;
#190036 = CARTESIAN_POINT('Ctrl Pts',(-10.6783519318786,-14.1635077969098,
117.618538736391)) ;
#190037 = CARTESIAN_POINT('Ctrl Pts',(-10.604548095061,-14.16350781747,117.642769798187)) ;
#190038 = CARTESIAN_POINT('Ctrl Pts',(-10.5884313767342,-14.2191244399571,
117.593680875156)) ;
#190039 = CARTESIAN_POINT('Ctrl Pts',(-10.5723146584073,-14.2747410624442,
117.544591952124)) ;
#190040 = CARTESIAN_POINT('Ctrl Pts',(-10.6461184952249,-14.2747410418841,
117.520360890328)) ;
#190041 = CARTESIAN_POINT('Ctrl Pts',(-10.7199223320424,-14.2747410213239,
117.496129828532)) ;
#190042 = CARTESIAN_POINT('Ctrl Pts',(-10.7360390503692,-14.2191243988368,
117.545218751564)) ;
#190043 = CARTESIAN_POINT('Ctrl Pts',(-10.8004224513246,-14.3863702551061,
117.77697919627)) ;
#190044 = CARTESIAN_POINT('Ctrl Pts',(-10.8113293964078,-14.318995498507,
117.810199990393)) ;
#190045 = CARTESIAN_POINT('Ctrl Pts',(-10.7375255639529,-14.3189955173641,
117.834431065477)) ;
#190046 = CARTESIAN_POINT('Ctrl Pts',(-10.6637217314981,-14.3189955362211,
117.858662140561)) ;
#190047 = CARTESIAN_POINT('Ctrl Pts',(-10.6528147864148,-14.3863702928201,
117.825441346437)) ;
#190048 = CARTESIAN_POINT('Ctrl Pts',(-10.6419078413316,-14.4537450494192,
117.792220552313)) ;
#190049 = CARTESIAN_POINT('Ctrl Pts',(-10.7157116737865,-14.4537450305621,
117.76798947723)) ;
#190050 = CARTESIAN_POINT('Ctrl Pts',(-10.7895155062413,-14.4537450117051,
117.743758402146)) ;
#190051 = CARTESIAN_POINT('Ctrl Pts',(-10.8004224513246,-14.3863702551061,
117.77697919627)) ;
#190052 = CARTESIAN_POINT('Ctrl Pts',(-10.8752502952428,-14.4829184358348,
118.040206328883)) ;
#190053 = CARTESIAN_POINT('Ctrl Pts',(-10.8802177774422,-14.408705819493,
118.055336477252)) ;
#190054 = CARTESIAN_POINT('Ctrl Pts',(-10.8064139483773,-14.4087058298003,
118.079567562661)) ;
#190055 = CARTESIAN_POINT('Ctrl Pts',(-10.7326101193124,-14.4087058401076,
118.10379864807)) ;
#190056 = CARTESIAN_POINT('Ctrl Pts',(-10.727642637113,-14.4829184564494,
118.088668499701)) ;
#190057 = CARTESIAN_POINT('Ctrl Pts',(-10.7226751549136,-14.5571310727912,
118.073538351333)) ;
#190058 = CARTESIAN_POINT('Ctrl Pts',(-10.7964789839785,-14.5571310624839,
118.049307265924)) ;
#190059 = CARTESIAN_POINT('Ctrl Pts',(-10.8702828130435,-14.5571310521766,
118.025076180515)) ;
#190060 = CARTESIAN_POINT('Ctrl Pts',(-10.8752502952428,-14.4829184358348,
118.040206328883)) ;
#190061 = CARTESIAN_POINT('Ctrl Pts',(-10.9554503612226,-14.5038609743369,
118.320003608547)) ;
#190062 = CARTESIAN_POINT('Ctrl Pts',(-10.9540905544359,-14.4280787626501,
118.31586185539)) ;
#190063 = CARTESIAN_POINT('Ctrl Pts',(-10.8802867285745,-14.4280787598768,
118.340092950556)) ;
#190064 = CARTESIAN_POINT('Ctrl Pts',(-10.806482902713,-14.4280787571034,
118.364324045722)) ;
#190065 = CARTESIAN_POINT('Ctrl Pts',(-10.8078427094997,-14.5038609687901,
118.36846579888)) ;
#190066 = CARTESIAN_POINT('Ctrl Pts',(-10.8092025162864,-14.5796431804768,
118.372607552037)) ;
#190067 = CARTESIAN_POINT('Ctrl Pts',(-10.8830063421479,-14.5796431832502,
118.34837645687)) ;
#190068 = CARTESIAN_POINT('Ctrl Pts',(-10.9568101680093,-14.5796431860236,
118.324145361704)) ;
#190069 = CARTESIAN_POINT('Ctrl Pts',(-10.9554503612226,-14.5038609743369,
118.320003608547)) ;
#190070 = CARTESIAN_POINT('Ctrl Pts',(-11.0338946450071,-14.4469649885374,
118.594339392381)) ;
#190071 = CARTESIAN_POINT('Ctrl Pts',(-11.0263233894398,-14.3750457551338,
118.571278568299)) ;
#190072 = CARTESIAN_POINT('Ctrl Pts',(-10.9525195650589,-14.3750457349022,
118.595509667975)) ;
#190073 = CARTESIAN_POINT('Ctrl Pts',(-10.878715740678,-14.3750457146707,
118.619740767651)) ;
#190074 = CARTESIAN_POINT('Ctrl Pts',(-10.8862869962453,-14.4469649480743,
118.642801591733)) ;
#190075 = CARTESIAN_POINT('Ctrl Pts',(-10.8938582518126,-14.5188841814779,
118.665862415815)) ;
#190076 = CARTESIAN_POINT('Ctrl Pts',(-10.9676620761935,-14.5188842017095,
118.641631316139)) ;
#190077 = CARTESIAN_POINT('Ctrl Pts',(-11.0414659005744,-14.518884221941,
118.617400216464)) ;
#190078 = CARTESIAN_POINT('Ctrl Pts',(-11.0338946450071,-14.4469649885374,
118.594339392381)) ;
#190079 = CARTESIAN_POINT('Ctrl Pts',(-11.1046254927112,-14.3162777489947,
118.845269515741)) ;
#190080 = CARTESIAN_POINT('Ctrl Pts',(-11.0913705484774,-14.2533785894399,
118.804897092878)) ;
#190081 = CARTESIAN_POINT('Ctrl Pts',(-11.0175667238931,-14.2533785490254,
118.829128191934)) ;
#190082 = CARTESIAN_POINT('Ctrl Pts',(-10.9437628993088,-14.253378508611,
118.853359290991)) ;
#190083 = CARTESIAN_POINT('Ctrl Pts',(-10.9570178435427,-14.3162776681657,
118.893731713853)) ;
#190084 = CARTESIAN_POINT('Ctrl Pts',(-10.9702727877766,-14.3791768277205,
118.934104136716)) ;
#190085 = CARTESIAN_POINT('Ctrl Pts',(-11.0440766123608,-14.379176868135,
118.90987303766)) ;
#190086 = CARTESIAN_POINT('Ctrl Pts',(-11.1178804369451,-14.3791769085495,
118.885641938604)) ;
#190087 = CARTESIAN_POINT('Ctrl Pts',(-11.1046254927112,-14.3162777489947,
118.845269515741)) ;
#190088 = CARTESIAN_POINT('Ctrl Pts',(-11.1615630301732,-14.1213118802641,
119.054150344886)) ;
#190089 = CARTESIAN_POINT('Ctrl Pts',(-11.1435799622605,-14.0719335115926,
118.999376820032)) ;
#190090 = CARTESIAN_POINT('Ctrl Pts',(-11.0697761351519,-14.0719334508548,
119.0236079114)) ;
#190091 = CARTESIAN_POINT('Ctrl Pts',(-10.9959723080433,-14.0719333901169,
119.047839002768)) ;
#190092 = CARTESIAN_POINT('Ctrl Pts',(-11.013955375956,-14.1213117587884,
119.102612527621)) ;
#190093 = CARTESIAN_POINT('Ctrl Pts',(-11.0319384438687,-14.1706901274599,
119.157386052474)) ;
#190094 = CARTESIAN_POINT('Ctrl Pts',(-11.1057422709773,-14.1706901881977,
119.133154961106)) ;
#190095 = CARTESIAN_POINT('Ctrl Pts',(-11.1795460980859,-14.1706902489356,
119.108923869739)) ;
#190096 = CARTESIAN_POINT('Ctrl Pts',(-11.1615630301732,-14.1213118802641,
119.054150344886)) ;
#190097 = CARTESIAN_POINT('Ctrl Pts',(-11.2000141105456,-13.8756723338256,
119.206771292959)) ;
#190098 = CARTESIAN_POINT('Ctrl Pts',(-11.1785857096267,-13.8433718742573,
119.141503839532)) ;
#190099 = CARTESIAN_POINT('Ctrl Pts',(-11.1047818778379,-13.8433717952861,
119.165734916645)) ;
#190100 = CARTESIAN_POINT('Ctrl Pts',(-11.0309780460491,-13.8433717163149,
119.189965993757)) ;
#190101 = CARTESIAN_POINT('Ctrl Pts',(-11.0524064469679,-13.8756721758832,
119.255233447184)) ;
#190102 = CARTESIAN_POINT('Ctrl Pts',(-11.0738348478868,-13.9079726354515,
119.32050090061)) ;
#190103 = CARTESIAN_POINT('Ctrl Pts',(-11.1476386796756,-13.9079727144228,
119.296269823498)) ;
#190104 = CARTESIAN_POINT('Ctrl Pts',(-11.2214425114645,-13.907972793394,
119.272038746385)) ;
#190105 = CARTESIAN_POINT('Ctrl Pts',(-11.2000141105456,-13.8756723338256,
119.206771292959)) ;
#190106 = CARTESIAN_POINT('Ctrl Pts',(-11.2163100996261,-13.597140902686,
119.291910614714)) ;
#190107 = CARTESIAN_POINT('Ctrl Pts',(-11.1929780886912,-13.584239435371,
119.220845072204)) ;
#190108 = CARTESIAN_POINT('Ctrl Pts',(-11.1191742502117,-13.5842393431877,
119.245076128938)) ;
#190109 = CARTESIAN_POINT('Ctrl Pts',(-11.0453704117322,-13.5842392510044,
119.269307185671)) ;
#190110 = CARTESIAN_POINT('Ctrl Pts',(-11.068702422667,-13.5971407183194,
119.340372728181)) ;
#190111 = CARTESIAN_POINT('Ctrl Pts',(-11.0920344336019,-13.6100421856345,
119.41143827069)) ;
#190112 = CARTESIAN_POINT('Ctrl Pts',(-11.1658382720815,-13.6100422778178,
119.387207213956)) ;
#190113 = CARTESIAN_POINT('Ctrl Pts',(-11.239642110561,-13.6100423700011,
119.362976157223)) ;
#190114 = CARTESIAN_POINT('Ctrl Pts',(-11.2163100996261,-13.597140902686,
119.291910614714)) ;
#190115 = CARTESIAN_POINT('Ctrl Pts',(-11.2087112550923,-13.3072582096283,
119.304089569254)) ;
#190116 = CARTESIAN_POINT('Ctrl Pts',(-11.1851449455377,-13.3145766205793,
119.23231039087)) ;
#190117 = CARTESIAN_POINT('Ctrl Pts',(-11.1113410991254,-13.3145765231922,
119.256541423441)) ;
#190118 = CARTESIAN_POINT('Ctrl Pts',(-11.0375372527131,-13.3145764258051,
119.280772456013)) ;
#190119 = CARTESIAN_POINT('Ctrl Pts',(-11.0611035622676,-13.3072580148542,
119.352551634397)) ;
#190120 = CARTESIAN_POINT('Ctrl Pts',(-11.0846698718222,-13.2999396039032,
119.424330812782)) ;
#190121 = CARTESIAN_POINT('Ctrl Pts',(-11.1584737182345,-13.2999397012903,
119.40009978021)) ;
#190122 = CARTESIAN_POINT('Ctrl Pts',(-11.2322775646468,-13.2999397986774,
119.375868747639)) ;
#190123 = CARTESIAN_POINT('Ctrl Pts',(-11.2087112550923,-13.3072582096283,
119.304089569254)) ;
#190124 = CARTESIAN_POINT('Ctrl Pts',(-11.176929955516,-13.023884652308,119.242788774443)) ;
#190125 = CARTESIAN_POINT('Ctrl Pts',(-11.1548134261834,-13.0509977629016,
119.175425392607)) ;
#190126 = CARTESIAN_POINT('Ctrl Pts',(-11.0810095713045,-13.0509976674412,
119.199656399391)) ;
#190127 = CARTESIAN_POINT('Ctrl Pts',(-11.0072057164255,-13.0509975719808,
119.223887406175)) ;
#190128 = CARTESIAN_POINT('Ctrl Pts',(-11.0293222457582,-13.0238844613873,
119.29125078801)) ;
#190129 = CARTESIAN_POINT('Ctrl Pts',(-11.0514387750908,-12.9967713507938,
119.358614169846)) ;
#190130 = CARTESIAN_POINT('Ctrl Pts',(-11.1252426299697,-12.9967714462542,
119.334383163062)) ;
#190131 = CARTESIAN_POINT('Ctrl Pts',(-11.1990464848487,-12.9967715417145,
119.310152156278)) ;
#190132 = CARTESIAN_POINT('Ctrl Pts',(-11.176929955516,-13.023884652308,119.242788774443)) ;
#190133 = CARTESIAN_POINT('Ctrl Pts',(-11.122465034715,-12.7690113233817,
119.112365611642)) ;
#190134 = CARTESIAN_POINT('Ctrl Pts',(-11.1033846730978,-12.8139584952445,
119.054249906723)) ;
#190135 = CARTESIAN_POINT('Ctrl Pts',(-11.0295808101122,-12.813958410504,
119.078480888815)) ;
#190136 = CARTESIAN_POINT('Ctrl Pts',(-10.9557769471266,-12.8139583257634,
119.102711870907)) ;
#190137 = CARTESIAN_POINT('Ctrl Pts',(-10.9748573087438,-12.7690111539007,
119.160827575826)) ;
#190138 = CARTESIAN_POINT('Ctrl Pts',(-10.9939376703611,-12.7240639820379,
119.218943280745)) ;
#190139 = CARTESIAN_POINT('Ctrl Pts',(-11.0677415333467,-12.7240640667784,
119.194712298653)) ;
#190140 = CARTESIAN_POINT('Ctrl Pts',(-11.1415453963323,-12.724064151519,
119.170481316561)) ;
#190141 = CARTESIAN_POINT('Ctrl Pts',(-11.122465034715,-12.7690113233817,
119.112365611642)) ;
#190142 = CARTESIAN_POINT('Ctrl Pts',(-11.0484836538836,-12.5606194771078,
118.922504182192)) ;
#190143 = CARTESIAN_POINT('Ctrl Pts',(-11.0338062707941,-12.6201819472302,
118.877799239411)) ;
#190144 = CARTESIAN_POINT('Ctrl Pts',(-10.9600024009755,-12.6201818809856,
118.902030200691)) ;
#190145 = CARTESIAN_POINT('Ctrl Pts',(-10.8861985311569,-12.620181814741,
118.92626116197)) ;
#190146 = CARTESIAN_POINT('Ctrl Pts',(-10.9008759142464,-12.5606193446187,
118.970966104751)) ;
#190147 = CARTESIAN_POINT('Ctrl Pts',(-10.9155532973358,-12.5010568744963,
119.015671047533)) ;
#190148 = CARTESIAN_POINT('Ctrl Pts',(-10.9893571671545,-12.5010569407409,
118.991440086253)) ;
#190149 = CARTESIAN_POINT('Ctrl Pts',(-11.0631610369731,-12.5010570069855,
118.967209124973)) ;
#190150 = CARTESIAN_POINT('Ctrl Pts',(-11.0484836538836,-12.5606194771078,
118.922504182192)) ;
#190151 = CARTESIAN_POINT('Ctrl Pts',(-10.9596194230083,-12.413760463827,
118.687278216149)) ;
#190152 = CARTESIAN_POINT('Ctrl Pts',(-10.9503912303216,-12.4836640016496,
118.659170628094)) ;
#190153 = CARTESIAN_POINT('Ctrl Pts',(-10.8765873557,-12.4836639599655,118.683401574745)) ;
#190154 = CARTESIAN_POINT('Ctrl Pts',(-10.8027834810785,-12.4836639182814,
118.707632521395)) ;
#190155 = CARTESIAN_POINT('Ctrl Pts',(-10.8120116737651,-12.4137603804588,
118.73574010945)) ;
#190156 = CARTESIAN_POINT('Ctrl Pts',(-10.8212398664518,-12.3438568426362,
118.763847697506)) ;
#190157 = CARTESIAN_POINT('Ctrl Pts',(-10.8950437410734,-12.3438568843203,
118.739616750855)) ;
#190158 = CARTESIAN_POINT('Ctrl Pts',(-10.968847615695,-12.3438569260044,
118.715385804204)) ;
#190159 = CARTESIAN_POINT('Ctrl Pts',(-10.9596194230083,-12.413760463827,
118.687278216149)) ;
#190160 = CARTESIAN_POINT('Ctrl Pts',(-10.861301775566,-12.3386970972896,
118.42329982477)) ;
#190161 = CARTESIAN_POINT('Ctrl Pts',(-10.8581899088794,-12.4139449164538,
118.41382157885)) ;
#190162 = CARTESIAN_POINT('Ctrl Pts',(-10.7843860319931,-12.4139449029389,
118.438052518602)) ;
#190163 = CARTESIAN_POINT('Ctrl Pts',(-10.7105821551067,-12.4139448894239,
118.462283458355)) ;
#190164 = CARTESIAN_POINT('Ctrl Pts',(-10.7136940217933,-12.3386970702597,
118.471761704275)) ;
#190165 = CARTESIAN_POINT('Ctrl Pts',(-10.71680588848,-12.2634492510955,118.481239950195)) ;
#190166 = CARTESIAN_POINT('Ctrl Pts',(-10.7906097653663,-12.2634492646105,
118.457009010442)) ;
#190167 = CARTESIAN_POINT('Ctrl Pts',(-10.8644136422527,-12.2634492781254,
118.43277807069)) ;
#190168 = CARTESIAN_POINT('Ctrl Pts',(-10.861301775566,-12.3386970972896,
118.42329982477)) ;
#190169 = CARTESIAN_POINT('Ctrl Pts',(-10.7600017865258,-12.3409867725706,
118.150207238855)) ;
#190170 = CARTESIAN_POINT('Ctrl Pts',(-10.7632241796794,-12.4161865646984,
118.160022126406)) ;
#190171 = CARTESIAN_POINT('Ctrl Pts',(-10.6894203032958,-12.4161865800311,
118.18425306769)) ;
#190172 = CARTESIAN_POINT('Ctrl Pts',(-10.6156164269123,-12.4161865953639,
118.208484008974)) ;
#190173 = CARTESIAN_POINT('Ctrl Pts',(-10.6123940337586,-12.3409868032361,
118.198669121423)) ;
#190174 = CARTESIAN_POINT('Ctrl Pts',(-10.609171640605,-12.2657870111083,
118.188854233873)) ;
#190175 = CARTESIAN_POINT('Ctrl Pts',(-10.6829755169886,-12.2657869957756,
118.164623292589)) ;
#190176 = CARTESIAN_POINT('Ctrl Pts',(-10.7567793933721,-12.2657869804429,
118.140392351305)) ;
#190177 = CARTESIAN_POINT('Ctrl Pts',(-10.7600017865258,-12.3409867725706,
118.150207238855)) ;
#190178 = CARTESIAN_POINT('Ctrl Pts',(-10.6620478041179,-12.4204578395528,
117.88734093994)) ;
#190179 = CARTESIAN_POINT('Ctrl Pts',(-10.6713795731896,-12.4902214392955,
117.915764000842)) ;
#190180 = CARTESIAN_POINT('Ctrl Pts',(-10.5975756999991,-12.4902214812087,
117.939994951852)) ;
#190181 = CARTESIAN_POINT('Ctrl Pts',(-10.5237718268086,-12.4902215231219,
117.964225902861)) ;
#190182 = CARTESIAN_POINT('Ctrl Pts',(-10.514440057737,-12.4204579233792,
117.93580284196)) ;
#190183 = CARTESIAN_POINT('Ctrl Pts',(-10.5051082886654,-12.3506943236366,
117.907379781058)) ;
#190184 = CARTESIAN_POINT('Ctrl Pts',(-10.5789121618558,-12.3506942817234,
117.883148830048)) ;
#190185 = CARTESIAN_POINT('Ctrl Pts',(-10.6527160350463,-12.3506942398102,
117.858917879039)) ;
#190186 = CARTESIAN_POINT('Ctrl Pts',(-10.6620478041179,-12.4204578395528,
117.88734093994)) ;
#190187 = CARTESIAN_POINT('Ctrl Pts',(-10.573847688419,-12.5714299256093,
117.654168216919)) ;
#190188 = CARTESIAN_POINT('Ctrl Pts',(-10.5886173544689,-12.6307574701192,
117.699154234686)) ;
#190189 = CARTESIAN_POINT('Ctrl Pts',(-10.514813486715,-12.6307575336333,
117.723385202254)) ;
#190190 = CARTESIAN_POINT('Ctrl Pts',(-10.441009618961,-12.6307575971475,
117.747616169822)) ;
#190191 = CARTESIAN_POINT('Ctrl Pts',(-10.4262399529111,-12.5714300526376,
117.702630152056)) ;
#190192 = CARTESIAN_POINT('Ctrl Pts',(-10.4114702868613,-12.5121025081277,
117.65764413429)) ;
#190193 = CARTESIAN_POINT('Ctrl Pts',(-10.4852741546152,-12.5121024446135,
117.633413166721)) ;
#190194 = CARTESIAN_POINT('Ctrl Pts',(-10.5590780223691,-12.5121023810993,
117.609182199153)) ;
#190195 = CARTESIAN_POINT('Ctrl Pts',(-10.573847688419,-12.5714299256093,
117.654168216919)) ;
#190196 = CARTESIAN_POINT('Ctrl Pts',(-10.5009899435521,-12.7828129113163,
117.467691180829)) ;
#190197 = CARTESIAN_POINT('Ctrl Pts',(-10.520135271516,-12.8274711161602,
117.526004758861)) ;
#190198 = CARTESIAN_POINT('Ctrl Pts',(-10.446331410711,-12.82747119449,117.550235747595)) ;
#190199 = CARTESIAN_POINT('Ctrl Pts',(-10.3725275499061,-12.8274712728199,
117.574466736329)) ;
#190200 = CARTESIAN_POINT('Ctrl Pts',(-10.3533822219422,-12.782813067976,
117.516153158297)) ;
#190201 = CARTESIAN_POINT('Ctrl Pts',(-10.3342368939783,-12.7381548631321,
117.457839580264)) ;
#190202 = CARTESIAN_POINT('Ctrl Pts',(-10.4080407547832,-12.7381547848022,
117.43360859153)) ;
#190203 = CARTESIAN_POINT('Ctrl Pts',(-10.4818446155882,-12.7381547064724,
117.409377602796)) ;
#190204 = CARTESIAN_POINT('Ctrl Pts',(-10.5009899435521,-12.7828129113163,
117.467691180829)) ;
#190205 = CARTESIAN_POINT('Ctrl Pts',(-10.4477866958819,-13.0396896566704,
117.341091891166)) ;
#190206 = CARTESIAN_POINT('Ctrl Pts',(-10.4699418299774,-13.0664804040034,
117.40857285315)) ;
#190207 = CARTESIAN_POINT('Ctrl Pts',(-10.3961379769048,-13.0664804892966,
117.432803865435)) ;
#190208 = CARTESIAN_POINT('Ctrl Pts',(-10.3223341238321,-13.0664805745898,
117.457034877721)) ;
#190209 = CARTESIAN_POINT('Ctrl Pts',(-10.3001789897366,-13.0396898272568,
117.389553915737)) ;
#190210 = CARTESIAN_POINT('Ctrl Pts',(-10.278023855641,-13.0128990799238,
117.322072953753)) ;
#190211 = CARTESIAN_POINT('Ctrl Pts',(-10.3518277087136,-13.0128989946306,
117.297841941468)) ;
#190212 = CARTESIAN_POINT('Ctrl Pts',(-10.4256315617863,-13.0128989093375,
117.273610929183)) ;
#190213 = CARTESIAN_POINT('Ctrl Pts',(-10.4477866958819,-13.0396896566704,
117.341091891166)) ;
#190214 = CARTESIAN_POINT('Ctrl Pts',(-10.4173299629953,-13.3246405733811,
117.283892429125)) ;
#190215 = CARTESIAN_POINT('Ctrl Pts',(-10.4409090851197,-13.3315770270648,
117.355710629024)) ;
#190216 = CARTESIAN_POINT('Ctrl Pts',(-10.3671052396779,-13.331577110356,
117.379941664552)) ;
#190217 = CARTESIAN_POINT('Ctrl Pts',(-10.2933013942362,-13.3315771936471,
117.40417270008)) ;
#190218 = CARTESIAN_POINT('Ctrl Pts',(-10.2697222721119,-13.3246407399634,
117.332354500181)) ;
#190219 = CARTESIAN_POINT('Ctrl Pts',(-10.2461431499876,-13.3177042862798,
117.260536300282)) ;
#190220 = CARTESIAN_POINT('Ctrl Pts',(-10.3199469954293,-13.3177042029886,
117.236305264754)) ;
#190221 = CARTESIAN_POINT('Ctrl Pts',(-10.393750840871,-13.3177041196975,
117.212074229227)) ;
#190222 = CARTESIAN_POINT('Ctrl Pts',(-10.4173299629953,-13.3246405733811,
117.283892429125)) ;
#190223 = CARTESIAN_POINT('Ctrl Pts',(-10.4112128032642,-13.6149949699245,
117.300663470431)) ;
#190224 = CARTESIAN_POINT('Ctrl Pts',(-10.4345220214507,-13.6016695488901,
117.371659586614)) ;
#190225 = CARTESIAN_POINT('Ctrl Pts',(-10.3607181825812,-13.6016696242958,
117.39589064216)) ;
#190226 = CARTESIAN_POINT('Ctrl Pts',(-10.2869143437116,-13.6016696997014,
117.420121697705)) ;
#190227 = CARTESIAN_POINT('Ctrl Pts',(-10.2636051255251,-13.6149951207358,
117.349125581522)) ;
#190228 = CARTESIAN_POINT('Ctrl Pts',(-10.2402959073386,-13.6283205417703,
117.278129465339)) ;
#190229 = CARTESIAN_POINT('Ctrl Pts',(-10.3140997462082,-13.6283204663646,
117.253898409794)) ;
#190230 = CARTESIAN_POINT('Ctrl Pts',(-10.3879035850777,-13.6283203909589,
117.229667354248)) ;
#190231 = CARTESIAN_POINT('Ctrl Pts',(-10.4112128032642,-13.6149949699245,
117.300663470431)) ;
#190232 = CARTESIAN_POINT('Ctrl Pts',(-10.4289381058465,-13.8916396903177,
117.39010694689)) ;
#190233 = CARTESIAN_POINT('Ctrl Pts',(-10.4503113588195,-13.8589788645426,
117.455206425549)) ;
#190234 = CARTESIAN_POINT('Ctrl Pts',(-10.3765075249951,-13.8589789264578,
117.479437496461)) ;
#190235 = CARTESIAN_POINT('Ctrl Pts',(-10.3027036911708,-13.858978988373,
117.503668567374)) ;
#190236 = CARTESIAN_POINT('Ctrl Pts',(-10.2813304381978,-13.891639814148,
117.438569088715)) ;
#190237 = CARTESIAN_POINT('Ctrl Pts',(-10.2599571852247,-13.9243006399231,
117.373469610057)) ;
#190238 = CARTESIAN_POINT('Ctrl Pts',(-10.3337610190491,-13.9243005780079,
117.349238539144)) ;
#190239 = CARTESIAN_POINT('Ctrl Pts',(-10.4075648528735,-13.9243005160927,
117.325007468232)) ;
#190240 = CARTESIAN_POINT('Ctrl Pts',(-10.4289381058465,-13.8916396903177,
117.39010694689)) ;
#190241 = CARTESIAN_POINT('Ctrl Pts',(-10.468506753606,-14.1343825887975,
117.546066895377)) ;
#190242 = CARTESIAN_POINT('Ctrl Pts',(-10.4864163346107,-14.0847239411806,
117.600616588237)) ;
#190243 = CARTESIAN_POINT('Ctrl Pts',(-10.4126125039408,-14.0847239865753,
117.624847668757)) ;
#190244 = CARTESIAN_POINT('Ctrl Pts',(-10.3388086732709,-14.0847240319701,
117.649078749278)) ;
#190245 = CARTESIAN_POINT('Ctrl Pts',(-10.3208990922662,-14.134382679587,
117.594529056418)) ;
#190246 = CARTESIAN_POINT('Ctrl Pts',(-10.3029895112616,-14.1840413272039,
117.539979363559)) ;
#190247 = CARTESIAN_POINT('Ctrl Pts',(-10.3767933419314,-14.1840412818091,
117.515748283038)) ;
#190248 = CARTESIAN_POINT('Ctrl Pts',(-10.4505971726013,-14.1840412364144,
117.491517202517)) ;
#190249 = CARTESIAN_POINT('Ctrl Pts',(-10.468506753606,-14.1343825887975,
117.546066895377)) ;
#190250 = CARTESIAN_POINT('Ctrl Pts',(-10.5266399323651,-14.3263844089833,
117.758714791445)) ;
#190251 = CARTESIAN_POINT('Ctrl Pts',(-10.539781502399,-14.2632443878997,
117.798741892392)) ;
#190252 = CARTESIAN_POINT('Ctrl Pts',(-10.4659776724899,-14.263244415508,
117.82297297523)) ;
#190253 = CARTESIAN_POINT('Ctrl Pts',(-10.3921738425808,-14.2632444431164,
117.847204058068)) ;
#190254 = CARTESIAN_POINT('Ctrl Pts',(-10.3790322725469,-14.3263844642,117.807176957121)) ;
#190255 = CARTESIAN_POINT('Ctrl Pts',(-10.3658907025129,-14.3895244852836,
117.767149856173)) ;
#190256 = CARTESIAN_POINT('Ctrl Pts',(-10.439694532422,-14.3895244576753,
117.742918773336)) ;
#190257 = CARTESIAN_POINT('Ctrl Pts',(-10.5134983623311,-14.3895244300669,
117.718687690498)) ;
#190258 = CARTESIAN_POINT('Ctrl Pts',(-10.5266399323651,-14.3263844089833,
117.758714791445)) ;
#190259 = CARTESIAN_POINT('Ctrl Pts',(-10.5977223470439,-14.4524065463604,
118.010565142517)) ;
#190260 = CARTESIAN_POINT('Ctrl Pts',(-10.6051893156736,-14.3803719566858,
118.033308323326)) ;
#190261 = CARTESIAN_POINT('Ctrl Pts',(-10.5313854853145,-14.3803719694669,
118.057539404794)) ;
#190262 = CARTESIAN_POINT('Ctrl Pts',(-10.4575816549555,-14.3803719822481,
118.081770486261)) ;
#190263 = CARTESIAN_POINT('Ctrl Pts',(-10.4501146863257,-14.4524065719227,
118.059027305451)) ;
#190264 = CARTESIAN_POINT('Ctrl Pts',(-10.442647717696,-14.5244411615974,
118.036284124642)) ;
#190265 = CARTESIAN_POINT('Ctrl Pts',(-10.5164515480551,-14.5244411488162,
118.012053043175)) ;
#190266 = CARTESIAN_POINT('Ctrl Pts',(-10.5902553784142,-14.5244411360351,
117.987821961707)) ;
#190267 = CARTESIAN_POINT('Ctrl Pts',(-10.5977223470439,-14.4524065463604,
118.010565142517)) ;
#190268 = CARTESIAN_POINT('Ctrl Pts',(-10.6769157709103,-14.5048820459499,
118.287401592442)) ;
#190269 = CARTESIAN_POINT('Ctrl Pts',(-10.6781273667279,-14.4290737092712,
118.291091917164)) ;
#190270 = CARTESIAN_POINT('Ctrl Pts',(-10.6043235337896,-14.4290737099999,
118.315322990775)) ;
#190271 = CARTESIAN_POINT('Ctrl Pts',(-10.5305197008513,-14.4290737107285,
118.339554064386)) ;
#190272 = CARTESIAN_POINT('Ctrl Pts',(-10.5293081050337,-14.5048820474072,
118.335863739665)) ;
#190273 = CARTESIAN_POINT('Ctrl Pts',(-10.5280965092161,-14.5806903840858,
118.332173414943)) ;
#190274 = CARTESIAN_POINT('Ctrl Pts',(-10.6019003421544,-14.5806903833572,
118.307942341331)) ;
#190275 = CARTESIAN_POINT('Ctrl Pts',(-10.6757041750927,-14.5806903826285,
118.28371126772)) ;
#190276 = CARTESIAN_POINT('Ctrl Pts',(-10.6769157709103,-14.5048820459499,
118.287401592442)) ;
#190277 = CARTESIAN_POINT('Ctrl Pts',(-10.7565713057278,-14.4792643387988,
118.565341880977)) ;
#190278 = CARTESIAN_POINT('Ctrl Pts',(-10.7514919843651,-14.4051302441696,
118.549871087139)) ;
#190279 = CARTESIAN_POINT('Ctrl Pts',(-10.6776881489865,-14.4051302376983,
118.574102153317)) ;
#190280 = CARTESIAN_POINT('Ctrl Pts',(-10.603884313608,-14.405130231227,118.598333219496)) ;
#190281 = CARTESIAN_POINT('Ctrl Pts',(-10.6089636349707,-14.4792643258562,
118.613804013335)) ;
#190282 = CARTESIAN_POINT('Ctrl Pts',(-10.6140429563333,-14.5533984204853,
118.629274807173)) ;
#190283 = CARTESIAN_POINT('Ctrl Pts',(-10.6878467917119,-14.5533984269566,
118.605043740994)) ;
#190284 = CARTESIAN_POINT('Ctrl Pts',(-10.7616506270905,-14.5533984334279,
118.580812674816)) ;
#190285 = CARTESIAN_POINT('Ctrl Pts',(-10.7565713057278,-14.4792643387988,
118.565341880977)) ;
#190286 = CARTESIAN_POINT('Ctrl Pts',(-10.8312394732339,-14.3777623982077,
118.828257574301)) ;
#190287 = CARTESIAN_POINT('Ctrl Pts',(-10.8202044172732,-14.3106033154662,
118.794646573987)) ;
#190288 = CARTESIAN_POINT('Ctrl Pts',(-10.7464005788549,-14.3106033061414,
118.818877630907)) ;
#190289 = CARTESIAN_POINT('Ctrl Pts',(-10.6725967404366,-14.3106032968165,
118.843108687828)) ;
#190290 = CARTESIAN_POINT('Ctrl Pts',(-10.6836317963974,-14.377762379558,
118.876719688142)) ;
#190291 = CARTESIAN_POINT('Ctrl Pts',(-10.6946668523581,-14.4449214622994,
118.910330688456)) ;
#190292 = CARTESIAN_POINT('Ctrl Pts',(-10.7684706907764,-14.4449214716243,
118.886099631536)) ;
#190293 = CARTESIAN_POINT('Ctrl Pts',(-10.8422745291946,-14.4449214809491,
118.861868574615)) ;
#190294 = CARTESIAN_POINT('Ctrl Pts',(-10.8312394732339,-14.3777623982077,
118.828257574301)) ;
#190295 = CARTESIAN_POINT('Ctrl Pts',(-10.8943486068065,-14.2077004202751,
119.055900281951)) ;
#190296 = CARTESIAN_POINT('Ctrl Pts',(-10.8781572711893,-14.1523145589373,
119.006584085897)) ;
#190297 = CARTESIAN_POINT('Ctrl Pts',(-10.8043534303052,-14.1523145504394,
119.030815135306)) ;
#190298 = CARTESIAN_POINT('Ctrl Pts',(-10.7305495894211,-14.1523145419415,
119.055046184716)) ;
#190299 = CARTESIAN_POINT('Ctrl Pts',(-10.7467409250382,-14.2077004032793,
119.10436238077)) ;
#190300 = CARTESIAN_POINT('Ctrl Pts',(-10.7629322606553,-14.2630862646171,
119.153678576825)) ;
#190301 = CARTESIAN_POINT('Ctrl Pts',(-10.8367361015395,-14.2630862731151,
119.129447527415)) ;
#190302 = CARTESIAN_POINT('Ctrl Pts',(-10.9105399424236,-14.263086281613,
119.105216478005)) ;
#190303 = CARTESIAN_POINT('Ctrl Pts',(-10.8943486068065,-14.2077004202751,
119.055900281951)) ;
#190304 = CARTESIAN_POINT('Ctrl Pts',(-10.9409131008362,-13.980362420234,
119.23327739182)) ;
#190305 = CARTESIAN_POINT('Ctrl Pts',(-10.9207102013615,-13.9407671671798,
119.171742619647)) ;
#190306 = CARTESIAN_POINT('Ctrl Pts',(-10.8469063586303,-13.9407671625387,
119.195973663431)) ;
#190307 = CARTESIAN_POINT('Ctrl Pts',(-10.7731025158991,-13.9407671578977,
119.220204707215)) ;
#190308 = CARTESIAN_POINT('Ctrl Pts',(-10.7933054153738,-13.980362410952,
119.281739479387)) ;
#190309 = CARTESIAN_POINT('Ctrl Pts',(-10.8135083148485,-14.0199576640062,
119.34327425156)) ;
#190310 = CARTESIAN_POINT('Ctrl Pts',(-10.8873121575797,-14.0199576686472,
119.319043207776)) ;
#190311 = CARTESIAN_POINT('Ctrl Pts',(-10.9611160003109,-14.0199576732883,
119.294812163993)) ;
#190312 = CARTESIAN_POINT('Ctrl Pts',(-10.9409131008362,-13.980362420234,
119.23327739182)) ;
#190313 = CARTESIAN_POINT('Ctrl Pts',(-10.9665178595046,-13.7128487430244,
119.346765660867)) ;
#190314 = CARTESIAN_POINT('Ctrl Pts',(-10.9437620232542,-13.6918738812675,
119.277455055282)) ;
#190315 = CARTESIAN_POINT('Ctrl Pts',(-10.8699581797813,-13.6918738808366,
119.301686096807)) ;
#190316 = CARTESIAN_POINT('Ctrl Pts',(-10.7961543363084,-13.6918738804057,
119.325917138332)) ;
#190317 = CARTESIAN_POINT('Ctrl Pts',(-10.8189101725589,-13.7128487421626,
119.395227743917)) ;
#190318 = CARTESIAN_POINT('Ctrl Pts',(-10.8416660088093,-13.7338236039195,
119.464538349502)) ;
#190319 = CARTESIAN_POINT('Ctrl Pts',(-10.9154698522822,-13.7338236043504,
119.440307307977)) ;
#190320 = CARTESIAN_POINT('Ctrl Pts',(-10.9892736957551,-13.7338236047813,
119.416076266453)) ;
#190321 = CARTESIAN_POINT('Ctrl Pts',(-10.9665178595046,-13.7128487430244,
119.346765660867)) ;
#190322 = CARTESIAN_POINT('Ctrl Pts',(-10.9686843945112,-13.4250762896625,
119.388764927315)) ;
#190323 = CARTESIAN_POINT('Ctrl Pts',(-10.9450107520713,-13.4241646281582,
119.316658832214)) ;
#190324 = CARTESIAN_POINT('Ctrl Pts',(-10.8712069085982,-13.424164630414,
119.340889873738)) ;
#190325 = CARTESIAN_POINT('Ctrl Pts',(-10.7974030651251,-13.4241646326699,
119.365120915263)) ;
#190326 = CARTESIAN_POINT('Ctrl Pts',(-10.821076707565,-13.4250762941742,
119.437227010363)) ;
#190327 = CARTESIAN_POINT('Ctrl Pts',(-10.844750350005,-13.4259879556785,
119.509333105464)) ;
#190328 = CARTESIAN_POINT('Ctrl Pts',(-10.9185541934781,-13.4259879534226,
119.48510206394)) ;
#190329 = CARTESIAN_POINT('Ctrl Pts',(-10.9923580369512,-13.4259879511667,
119.460871022416)) ;
#190330 = CARTESIAN_POINT('Ctrl Pts',(-10.9686843945112,-13.4250762896625,
119.388764927315)) ;
#190331 = CARTESIAN_POINT('Ctrl Pts',(-10.9467663089628,-13.1369898154444,
119.357371205815)) ;
#190332 = CARTESIAN_POINT('Ctrl Pts',(-10.92385617065,-13.1561933535751,119.28759062112)) ;
#190333 = CARTESIAN_POINT('Ctrl Pts',(-10.8500523275358,-13.1561933570076,
119.311821663738)) ;
#190334 = CARTESIAN_POINT('Ctrl Pts',(-10.7762484844217,-13.15619336044,119.336052706355)) ;
#190335 = CARTESIAN_POINT('Ctrl Pts',(-10.7991586227345,-13.1369898223093,
119.40583329105)) ;
#190336 = CARTESIAN_POINT('Ctrl Pts',(-10.8220687610474,-13.1177862841786,
119.475613875745)) ;
#190337 = CARTESIAN_POINT('Ctrl Pts',(-10.8958726041615,-13.1177862807461,
119.451382833128)) ;
#190338 = CARTESIAN_POINT('Ctrl Pts',(-10.9696764472756,-13.1177862773137,
119.42715179051)) ;
#190339 = CARTESIAN_POINT('Ctrl Pts',(-10.9467663089628,-13.1369898154444,
119.357371205815)) ;
#190340 = CARTESIAN_POINT('Ctrl Pts',(-10.9008150940902,-12.8663855366991,
119.253146965752)) ;
#190341 = CARTESIAN_POINT('Ctrl Pts',(-10.8803401623047,-12.9045144387046,
119.190783627186)) ;
#190342 = CARTESIAN_POINT('Ctrl Pts',(-10.8065363192358,-12.9045144401406,
119.215014669941)) ;
#190343 = CARTESIAN_POINT('Ctrl Pts',(-10.732732476167,-12.9045144415766,
119.239245712697)) ;
#190344 = CARTESIAN_POINT('Ctrl Pts',(-10.7532074079525,-12.8663855395711,
119.301609051263)) ;
#190345 = CARTESIAN_POINT('Ctrl Pts',(-10.7736823397381,-12.8282566375656,
119.36397238983)) ;
#190346 = CARTESIAN_POINT('Ctrl Pts',(-10.8474861828069,-12.8282566361296,
119.339741347074)) ;
#190347 = CARTESIAN_POINT('Ctrl Pts',(-10.9212900258757,-12.8282566346936,
119.315510304319)) ;
#190348 = CARTESIAN_POINT('Ctrl Pts',(-10.9008150940902,-12.8663855366991,
119.253146965752)) ;
#190349 = CARTESIAN_POINT('Ctrl Pts',(-10.8345412319917,-12.6384940512534,
119.086571197061)) ;
#190350 = CARTESIAN_POINT('Ctrl Pts',(-10.817933850772,-12.6925911695923,
119.035987793437)) ;
#190351 = CARTESIAN_POINT('Ctrl Pts',(-10.7441300072107,-12.6925911686239,
119.060218834692)) ;
#190352 = CARTESIAN_POINT('Ctrl Pts',(-10.6703261636495,-12.6925911676555,
119.084449875948)) ;
#190353 = CARTESIAN_POINT('Ctrl Pts',(-10.6869335448692,-12.6384940493165,
119.135033279572)) ;
#190354 = CARTESIAN_POINT('Ctrl Pts',(-10.7035409260888,-12.5843969309776,
119.185616683196)) ;
#190355 = CARTESIAN_POINT('Ctrl Pts',(-10.7773447696501,-12.584396931946,
119.16138564194)) ;
#190356 = CARTESIAN_POINT('Ctrl Pts',(-10.8511486132114,-12.5843969329144,
119.137154600685)) ;
#190357 = CARTESIAN_POINT('Ctrl Pts',(-10.8345412319917,-12.6384940512534,
119.086571197061)) ;
#190358 = CARTESIAN_POINT('Ctrl Pts',(-10.7508843645138,-12.4647340958094,
118.867309476952)) ;
#190359 = CARTESIAN_POINT('Ctrl Pts',(-10.7393585365561,-12.5310434351584,
118.832203664559)) ;
#190360 = CARTESIAN_POINT('Ctrl Pts',(-10.6655546915337,-12.5310434317377,
118.856434701364)) ;
#190361 = CARTESIAN_POINT('Ctrl Pts',(-10.5917508465113,-12.5310434283171,
118.880665738169)) ;
#190362 = CARTESIAN_POINT('Ctrl Pts',(-10.603276674469,-12.4647340889681,
118.915771550563)) ;
#190363 = CARTESIAN_POINT('Ctrl Pts',(-10.6148025024268,-12.3984247496191,
118.950877362956)) ;
#190364 = CARTESIAN_POINT('Ctrl Pts',(-10.6886063474492,-12.3984247530398,
118.926646326151)) ;
#190365 = CARTESIAN_POINT('Ctrl Pts',(-10.7624101924716,-12.3984247564605,
118.902415289346)) ;
#190366 = CARTESIAN_POINT('Ctrl Pts',(-10.7508843645138,-12.4647340958094,
118.867309476952)) ;
#190367 = CARTESIAN_POINT('Ctrl Pts',(-10.65582614901,-12.3600064377204,118.613172394745)) ;
#190368 = CARTESIAN_POINT('Ctrl Pts',(-10.6501884550795,-12.4337245690079,
118.59600088844)) ;
#190369 = CARTESIAN_POINT('Ctrl Pts',(-10.5763846080915,-12.4337245657129,
118.620231919259)) ;
#190370 = CARTESIAN_POINT('Ctrl Pts',(-10.5025807611034,-12.4337245624179,
118.644462950077)) ;
#190371 = CARTESIAN_POINT('Ctrl Pts',(-10.5082184550339,-12.3600064311304,
118.661634456381)) ;
#190372 = CARTESIAN_POINT('Ctrl Pts',(-10.5138561489644,-12.286288299843,
118.678805962685)) ;
#190373 = CARTESIAN_POINT('Ctrl Pts',(-10.5876599959525,-12.286288303138,
118.654574931867)) ;
#190374 = CARTESIAN_POINT('Ctrl Pts',(-10.6614638429405,-12.286288306433,
118.630343901049)) ;
#190375 = CARTESIAN_POINT('Ctrl Pts',(-10.65582614901,-12.3600064377204,118.613172394745)) ;
#190376 = CARTESIAN_POINT('Ctrl Pts',(-10.5550274625865,-12.3305764766961,
118.341594134656)) ;
#190377 = CARTESIAN_POINT('Ctrl Pts',(-10.5556862943649,-12.4064564353267,
118.343600829588)) ;
#190378 = CARTESIAN_POINT('Ctrl Pts',(-10.4818824450957,-12.4064564352426,
118.367831853458)) ;
#190379 = CARTESIAN_POINT('Ctrl Pts',(-10.4080785958265,-12.4064564351584,
118.392062877328)) ;
#190380 = CARTESIAN_POINT('Ctrl Pts',(-10.4074197640481,-12.3305764765278,
118.390056182396)) ;
#190381 = CARTESIAN_POINT('Ctrl Pts',(-10.4067609322696,-12.2546965178971,
118.388049487464)) ;
#190382 = CARTESIAN_POINT('Ctrl Pts',(-10.4805647815389,-12.2546965179813,
118.363818463594)) ;
#190383 = CARTESIAN_POINT('Ctrl Pts',(-10.5543686308081,-12.2546965180655,
118.339587439724)) ;
#190384 = CARTESIAN_POINT('Ctrl Pts',(-10.5550274625865,-12.3305764766961,
118.341594134656)) ;
#190385 = CARTESIAN_POINT('Ctrl Pts',(-10.4547480010087,-12.3793274592069,
118.071699282546)) ;
#190386 = CARTESIAN_POINT('Ctrl Pts',(-10.4616740800548,-12.4519136571081,
118.092795001273)) ;
#190387 = CARTESIAN_POINT('Ctrl Pts',(-10.3878702284318,-12.4519136645641,
118.117026017974)) ;
#190388 = CARTESIAN_POINT('Ctrl Pts',(-10.3140663768089,-12.4519136720201,
118.141257034675)) ;
#190389 = CARTESIAN_POINT('Ctrl Pts',(-10.3071402977628,-12.379327474119,
118.120161315948)) ;
#190390 = CARTESIAN_POINT('Ctrl Pts',(-10.3002142187167,-12.3067412762178,
118.099065597221)) ;
#190391 = CARTESIAN_POINT('Ctrl Pts',(-10.3740180703397,-12.3067412687618,
118.07483458052)) ;
#190392 = CARTESIAN_POINT('Ctrl Pts',(-10.4478219219626,-12.3067412613058,
118.050603563819)) ;
#190393 = CARTESIAN_POINT('Ctrl Pts',(-10.4547480010087,-12.3793274592069,
118.071699282546)) ;
#190394 = CARTESIAN_POINT('Ctrl Pts',(-10.3621291537513,-12.5020990421703,
117.824980763251)) ;
#190395 = CARTESIAN_POINT('Ctrl Pts',(-10.3747997470748,-12.5662179845147,
117.863573345446)) ;
#190396 = CARTESIAN_POINT('Ctrl Pts',(-10.3009958943635,-12.5662180028208,
117.887804358831)) ;
#190397 = CARTESIAN_POINT('Ctrl Pts',(-10.2271920416521,-12.5662180211268,
117.912035372217)) ;
#190398 = CARTESIAN_POINT('Ctrl Pts',(-10.2145214483286,-12.5020990787824,
117.873442790023)) ;
#190399 = CARTESIAN_POINT('Ctrl Pts',(-10.2018508550051,-12.4379801364379,
117.834850207828)) ;
#190400 = CARTESIAN_POINT('Ctrl Pts',(-10.2756547077164,-12.4379801181319,
117.810619194442)) ;
#190401 = CARTESIAN_POINT('Ctrl Pts',(-10.3494585604278,-12.4379800998258,
117.786388181056)) ;
#190402 = CARTESIAN_POINT('Ctrl Pts',(-10.3621291537513,-12.5020990421703,
117.824980763251)) ;
#190403 = CARTESIAN_POINT('Ctrl Pts',(-10.28233167392,-12.6906392671464,117.617412412838)) ;
#190404 = CARTESIAN_POINT('Ctrl Pts',(-10.2998578268941,-12.7416870715668,
117.670794246116)) ;
#190405 = CARTESIAN_POINT('Ctrl Pts',(-10.226053974148,-12.7416871035792,
117.695025259396)) ;
#190406 = CARTESIAN_POINT('Ctrl Pts',(-10.1522501214019,-12.7416871355915,
117.719256272676)) ;
#190407 = CARTESIAN_POINT('Ctrl Pts',(-10.1347239684278,-12.6906393311711,
117.665874439398)) ;
#190408 = CARTESIAN_POINT('Ctrl Pts',(-10.1171978154537,-12.6395915267507,
117.61249260612)) ;
#190409 = CARTESIAN_POINT('Ctrl Pts',(-10.1910016681997,-12.6395914947383,
117.58826159284)) ;
#190410 = CARTESIAN_POINT('Ctrl Pts',(-10.2648055209459,-12.639591462726,
117.564030579559)) ;
#190411 = CARTESIAN_POINT('Ctrl Pts',(-10.28233167392,-12.6906392671464,117.617412412838)) ;
#190412 = CARTESIAN_POINT('Ctrl Pts',(-10.2205479280091,-12.9321841999642,
117.464807021943)) ;
#190413 = CARTESIAN_POINT('Ctrl Pts',(-10.2416769947665,-12.9664415034876,
117.529162749087)) ;
#190414 = CARTESIAN_POINT('Ctrl Pts',(-10.1678731436798,-12.9664415511475,
117.553393767422)) ;
#190415 = CARTESIAN_POINT('Ctrl Pts',(-10.0940692925932,-12.9664415988073,
117.577624785756)) ;
#190416 = CARTESIAN_POINT('Ctrl Pts',(-10.0729402258358,-12.9321842952839,
117.513269058612)) ;
#190417 = CARTESIAN_POINT('Ctrl Pts',(-10.0518111590785,-12.8979269917605,
117.448913331469)) ;
#190418 = CARTESIAN_POINT('Ctrl Pts',(-10.1256150101652,-12.8979269441006,
117.424682313134)) ;
#190419 = CARTESIAN_POINT('Ctrl Pts',(-10.1994188612518,-12.8979268964408,
117.4004512948)) ;
#190420 = CARTESIAN_POINT('Ctrl Pts',(-10.2205479280091,-12.9321841999642,
117.464807021943)) ;
#190421 = CARTESIAN_POINT('Ctrl Pts',(-10.1807928433781,-13.2070342064579,
117.379088560202)) ;
#190422 = CARTESIAN_POINT('Ctrl Pts',(-10.2039961426259,-13.2221513251204,
117.449762064688)) ;
#190423 = CARTESIAN_POINT('Ctrl Pts',(-10.1301922952923,-13.2221513851254,
117.473993094454)) ;
#190424 = CARTESIAN_POINT('Ctrl Pts',(-10.0563884479586,-13.2221514451304,
117.498224124219)) ;
#190425 = CARTESIAN_POINT('Ctrl Pts',(-10.0331851487109,-13.2070343264679,
117.427550619733)) ;
#190426 = CARTESIAN_POINT('Ctrl Pts',(-10.0099818494631,-13.1919172078054,
117.356877115248)) ;
#190427 = CARTESIAN_POINT('Ctrl Pts',(-10.0837856967967,-13.1919171478004,
117.332646085482)) ;
#190428 = CARTESIAN_POINT('Ctrl Pts',(-10.1575895441303,-13.1919170877954,
117.308415055717)) ;
#190429 = CARTESIAN_POINT('Ctrl Pts',(-10.1807928433781,-13.2070342064579,
117.379088560202)) ;
#190430 = CARTESIAN_POINT('Ctrl Pts',(-10.1647556271092,-13.4981307625057,
117.365766560135)) ;
#190431 = CARTESIAN_POINT('Ctrl Pts',(-10.1883771632764,-13.4929460625343,
117.437713946625)) ;
#190432 = CARTESIAN_POINT('Ctrl Pts',(-10.1145733212772,-13.492946132437,
117.461944992639)) ;
#190433 = CARTESIAN_POINT('Ctrl Pts',(-10.040769479278,-13.4929462023397,
117.486176038652)) ;
#190434 = CARTESIAN_POINT('Ctrl Pts',(-10.0171479431107,-13.4981309023111,
117.414228652161)) ;
#190435 = CARTESIAN_POINT('Ctrl Pts',(-9.99352640694351,-13.5033156022825,
117.342281265671)) ;
#190436 = CARTESIAN_POINT('Ctrl Pts',(-10.0673302489427,-13.5033155323798,
117.318050219658)) ;
#190437 = CARTESIAN_POINT('Ctrl Pts',(-10.1411340909419,-13.5033154624771,
117.293819173644)) ;
#190438 = CARTESIAN_POINT('Ctrl Pts',(-10.1647556271092,-13.4981307625057,
117.365766560135)) ;
#190439 = CARTESIAN_POINT('Ctrl Pts',(-10.1729059089313,-13.7819922849582,
117.425914749233)) ;
#190440 = CARTESIAN_POINT('Ctrl Pts',(-10.1952615851707,-13.7569816324817,
117.494006530502)) ;
#190441 = CARTESIAN_POINT('Ctrl Pts',(-10.121457749576,-13.7569817049211,
117.518237596022)) ;
#190442 = CARTESIAN_POINT('Ctrl Pts',(-10.0476539139814,-13.7569817773604,
117.542468661543)) ;
#190443 = CARTESIAN_POINT('Ctrl Pts',(-10.025298237742,-13.7819924298369,
117.474376880274)) ;
#190444 = CARTESIAN_POINT('Ctrl Pts',(-10.0029425615027,-13.8070030823134,
117.406285099005)) ;
#190445 = CARTESIAN_POINT('Ctrl Pts',(-10.0767463970973,-13.807003009874,
117.382054033484)) ;
#190446 = CARTESIAN_POINT('Ctrl Pts',(-10.150550232692,-13.8070029374347,
117.357822967964)) ;
#190447 = CARTESIAN_POINT('Ctrl Pts',(-10.1729059089313,-13.7819922849582,
117.425914749233)) ;
#190448 = CARTESIAN_POINT('Ctrl Pts',(-10.2041166916304,-14.041794726603,
117.55658075774)) ;
#190449 = CARTESIAN_POINT('Ctrl Pts',(-10.2235892247858,-13.9986090894959,
117.61589095021)) ;
#190450 = CARTESIAN_POINT('Ctrl Pts',(-10.1497853964037,-13.998609159369,
117.640122037698)) ;
#190451 = CARTESIAN_POINT('Ctrl Pts',(-10.0759815680215,-13.998609229242,
117.664353125187)) ;
#190452 = CARTESIAN_POINT('Ctrl Pts',(-10.0565090348661,-14.0417948663491,
117.605042932717)) ;
#190453 = CARTESIAN_POINT('Ctrl Pts',(-10.0370365017106,-14.0849805034562,
117.545732740248)) ;
#190454 = CARTESIAN_POINT('Ctrl Pts',(-10.1108403300928,-14.0849804335832,
117.52150165276)) ;
#190455 = CARTESIAN_POINT('Ctrl Pts',(-10.1846441584749,-14.0849803637101,
117.497270565271)) ;
#190456 = CARTESIAN_POINT('Ctrl Pts',(-10.2041166916304,-14.041794726603,
117.55658075774)) ;
#190457 = CARTESIAN_POINT('Ctrl Pts',(-10.2550233033811,-14.255449164482,
117.747005840351)) ;
#190458 = CARTESIAN_POINT('Ctrl Pts',(-10.2702380565919,-14.197284228839,
117.793347521988)) ;
#190459 = CARTESIAN_POINT('Ctrl Pts',(-10.1964342348443,-14.197284287096,
117.817578629684)) ;
#190460 = CARTESIAN_POINT('Ctrl Pts',(-10.1226304130967,-14.197284345353,
117.84180973738)) ;
#190461 = CARTESIAN_POINT('Ctrl Pts',(-10.1074156598859,-14.2554492809961,
117.795468055743)) ;
#190462 = CARTESIAN_POINT('Ctrl Pts',(-10.0922009066752,-14.3136142166391,
117.749126374106)) ;
#190463 = CARTESIAN_POINT('Ctrl Pts',(-10.1660047284228,-14.3136141583821,
117.72489526641)) ;
#190464 = CARTESIAN_POINT('Ctrl Pts',(-10.2398085501704,-14.313614100125,
117.700664158713)) ;
#190465 = CARTESIAN_POINT('Ctrl Pts',(-10.2550233033811,-14.255449164482,
117.747005840351)) ;
#190466 = CARTESIAN_POINT('Ctrl Pts',(-10.3219217787568,-14.4102492008634,
117.986414030523)) ;
#190467 = CARTESIAN_POINT('Ctrl Pts',(-10.3317506903204,-14.3411914994799,
118.016351307379)) ;
#190468 = CARTESIAN_POINT('Ctrl Pts',(-10.2579468745014,-14.3411915397154,
118.040582433133)) ;
#190469 = CARTESIAN_POINT('Ctrl Pts',(-10.1841430586823,-14.3411915799509,
118.064813558886)) ;
#190470 = CARTESIAN_POINT('Ctrl Pts',(-10.1743141471187,-14.4102492813345,
118.034876282031)) ;
#190471 = CARTESIAN_POINT('Ctrl Pts',(-10.1644852355551,-14.4793069827181,
118.004939005175)) ;
#190472 = CARTESIAN_POINT('Ctrl Pts',(-10.2382890513741,-14.4793069424825,
117.980707879422)) ;
#190473 = CARTESIAN_POINT('Ctrl Pts',(-10.3120928671932,-14.479306902247,
117.956476753668)) ;
#190474 = CARTESIAN_POINT('Ctrl Pts',(-10.3219217787568,-14.4102492008634,
117.986414030523)) ;
#190475 = CARTESIAN_POINT('Ctrl Pts',(-10.3980811903642,-14.4927425304254,
118.253658438679)) ;
#190476 = CARTESIAN_POINT('Ctrl Pts',(-10.401877290509,-14.4178249477771,
118.265220745276)) ;
#190477 = CARTESIAN_POINT('Ctrl Pts',(-10.3280734781105,-14.4178249636249,
118.289451881448)) ;
#190478 = CARTESIAN_POINT('Ctrl Pts',(-10.254269665712,-14.4178249794727,
118.31368301762)) ;
#190479 = CARTESIAN_POINT('Ctrl Pts',(-10.2504735655672,-14.4927425621209,
118.302120711023)) ;
#190480 = CARTESIAN_POINT('Ctrl Pts',(-10.2466774654224,-14.5676601447692,
118.290558404426)) ;
#190481 = CARTESIAN_POINT('Ctrl Pts',(-10.3204812778209,-14.5676601289214,
118.266327268254)) ;
#190482 = CARTESIAN_POINT('Ctrl Pts',(-10.3942850902194,-14.5676601130736,
118.242096132082)) ;
#190483 = CARTESIAN_POINT('Ctrl Pts',(-10.3980811903642,-14.4927425304254,
118.253658438679)) ;
#190484 = CARTESIAN_POINT('Ctrl Pts',(-10.4784322706411,-14.4990616510816,
118.533888978582)) ;
#190485 = CARTESIAN_POINT('Ctrl Pts',(-10.4758897404157,-14.4235929848165,
118.526144839733)) ;
#190486 = CARTESIAN_POINT('Ctrl Pts',(-10.4020859293724,-14.4235929732871,
118.550375980033)) ;
#190487 = CARTESIAN_POINT('Ctrl Pts',(-10.3282821183291,-14.4235929617576,
118.574607120333)) ;
#190488 = CARTESIAN_POINT('Ctrl Pts',(-10.3308246485545,-14.4990616280226,
118.582351259182)) ;
#190489 = CARTESIAN_POINT('Ctrl Pts',(-10.3333671787799,-14.5745302942877,
118.59009539803)) ;
#190490 = CARTESIAN_POINT('Ctrl Pts',(-10.4071709898231,-14.5745303058172,
118.56586425773)) ;
#190491 = CARTESIAN_POINT('Ctrl Pts',(-10.4809748008665,-14.5745303173466,
118.541633117431)) ;
#190492 = CARTESIAN_POINT('Ctrl Pts',(-10.4784322706411,-14.4990616510816,
118.533888978582)) ;
#190493 = CARTESIAN_POINT('Ctrl Pts',(-10.5559396621602,-14.4278621718276,
118.805402129203)) ;
#190494 = CARTESIAN_POINT('Ctrl Pts',(-10.5472488614899,-14.3572534635398,
118.778931350552)) ;
#190495 = CARTESIAN_POINT('Ctrl Pts',(-10.4734450490211,-14.357253423911,
118.80316248651)) ;
#190496 = CARTESIAN_POINT('Ctrl Pts',(-10.3996412365523,-14.3572533842822,
118.827393622468)) ;
#190497 = CARTESIAN_POINT('Ctrl Pts',(-10.4083320372227,-14.4278620925699,
118.853864401119)) ;
#190498 = CARTESIAN_POINT('Ctrl Pts',(-10.4170228378929,-14.4984708008576,
118.880335179769)) ;
#190499 = CARTESIAN_POINT('Ctrl Pts',(-10.4908266503617,-14.4984708404865,
118.856104043811)) ;
#190500 = CARTESIAN_POINT('Ctrl Pts',(-10.5646304628305,-14.4984708801153,
118.831872907853)) ;
#190501 = CARTESIAN_POINT('Ctrl Pts',(-10.5559396621602,-14.4278621718276,
118.805402129203)) ;
#190502 = CARTESIAN_POINT('Ctrl Pts',(-10.6246350611719,-14.2839264835508,
119.050194569323)) ;
#190503 = CARTESIAN_POINT('Ctrl Pts',(-10.6103996640293,-14.2232622888904,
119.006835844406)) ;
#190504 = CARTESIAN_POINT('Ctrl Pts',(-10.5365958475133,-14.2232622233179,
119.031066968037)) ;
#190505 = CARTESIAN_POINT('Ctrl Pts',(-10.4627920309972,-14.2232621577455,
119.055298091668)) ;
#190506 = CARTESIAN_POINT('Ctrl Pts',(-10.4770274281398,-14.2839263524059,
119.098656816584)) ;
#190507 = CARTESIAN_POINT('Ctrl Pts',(-10.4912628252824,-14.3445905470663,
119.142015541501)) ;
#190508 = CARTESIAN_POINT('Ctrl Pts',(-10.5650666417984,-14.3445906126388,
119.11778441787)) ;
#190509 = CARTESIAN_POINT('Ctrl Pts',(-10.6388704583145,-14.3445906782112,
119.09355329424)) ;
#190510 = CARTESIAN_POINT('Ctrl Pts',(-10.6246350611719,-14.2839264835508,
119.050194569323)) ;
#190511 = CARTESIAN_POINT('Ctrl Pts',(-10.6784414228845,-14.0776636855761,
119.249607301814)) ;
#190512 = CARTESIAN_POINT('Ctrl Pts',(-10.6596932344536,-14.0313099788708,
119.19250334277)) ;
#190513 = CARTESIAN_POINT('Ctrl Pts',(-10.5858894115044,-14.0313098927161,
119.216734446806)) ;
#190514 = CARTESIAN_POINT('Ctrl Pts',(-10.5120855885552,-14.0313098065613,
119.240965550842)) ;
#190515 = CARTESIAN_POINT('Ctrl Pts',(-10.5308337769861,-14.0776635132666,
119.298069509887)) ;
#190516 = CARTESIAN_POINT('Ctrl Pts',(-10.549581965417,-14.1240172199719,
119.355173468931)) ;
#190517 = CARTESIAN_POINT('Ctrl Pts',(-10.6233857883662,-14.1240173061266,
119.330942364894)) ;
#190518 = CARTESIAN_POINT('Ctrl Pts',(-10.6971896113153,-14.1240173922814,
119.306711260858)) ;
#190519 = CARTESIAN_POINT('Ctrl Pts',(-10.6784414228845,-14.0776636855761,
119.249607301814)) ;
#190520 = CARTESIAN_POINT('Ctrl Pts',(-10.7127437309599,-13.825817961869,
119.38938959783)) ;
#190521 = CARTESIAN_POINT('Ctrl Pts',(-10.6908424609061,-13.7969788395993,
119.322681860926)) ;
#190522 = CARTESIAN_POINT('Ctrl Pts',(-10.6170386300113,-13.7969787399069,
119.346912940761)) ;
#190523 = CARTESIAN_POINT('Ctrl Pts',(-10.5432347991165,-13.7969786402144,
119.371144020597)) ;
#190524 = CARTESIAN_POINT('Ctrl Pts',(-10.5651360691703,-13.8258177624841,
119.437851757501)) ;
#190525 = CARTESIAN_POINT('Ctrl Pts',(-10.5870373392241,-13.8546568847537,
119.504559494405)) ;
#190526 = CARTESIAN_POINT('Ctrl Pts',(-10.6608411701189,-13.8546569844462,
119.48032841457)) ;
#190527 = CARTESIAN_POINT('Ctrl Pts',(-10.7346450010137,-13.8546570841386,
119.456097334734)) ;
#190528 = CARTESIAN_POINT('Ctrl Pts',(-10.7127437309599,-13.825817961869,
119.38938959783)) ;
#190529 = CARTESIAN_POINT('Ctrl Pts',(-10.7247246250284,-13.5431962708422,
119.461411594824)) ;
#190530 = CARTESIAN_POINT('Ctrl Pts',(-10.7012190404884,-13.5340457388908,
119.389817374893)) ;
#190531 = CARTESIAN_POINT('Ctrl Pts',(-10.6274152007733,-13.5340456342861,
119.414048427863)) ;
#190532 = CARTESIAN_POINT('Ctrl Pts',(-10.5536113610583,-13.5340455296813,
119.438279480834)) ;
#190533 = CARTESIAN_POINT('Ctrl Pts',(-10.5771169455982,-13.5431960616327,
119.509873700765)) ;
#190534 = CARTESIAN_POINT('Ctrl Pts',(-10.6006225301382,-13.5523465935841,
119.581467920696)) ;
#190535 = CARTESIAN_POINT('Ctrl Pts',(-10.6744263698533,-13.5523466981889,
119.557236867726)) ;
#190536 = CARTESIAN_POINT('Ctrl Pts',(-10.7482302095684,-13.5523468027936,
119.533005814755)) ;
#190537 = CARTESIAN_POINT('Ctrl Pts',(-10.7247246250284,-13.5431962708422,
119.461411594824)) ;
#190538 = CARTESIAN_POINT('Ctrl Pts',(-10.712517892844,-13.2523620051609,
119.45965594129)) ;
#190539 = CARTESIAN_POINT('Ctrl Pts',(-10.6890964715402,-13.2635030369063,
119.388318069056)) ;
#190540 = CARTESIAN_POINT('Ctrl Pts',(-10.6152926231585,-13.2635029359697,
119.412549095629)) ;
#190541 = CARTESIAN_POINT('Ctrl Pts',(-10.5414887747767,-13.2635028350331,
119.436780122202)) ;
#190542 = CARTESIAN_POINT('Ctrl Pts',(-10.5649101960805,-13.2523618032878,
119.508117994436)) ;
#190543 = CARTESIAN_POINT('Ctrl Pts',(-10.5883316173843,-13.2412207715424,
119.57945586667)) ;
#190544 = CARTESIAN_POINT('Ctrl Pts',(-10.6621354657661,-13.241220872479,
119.555224840097)) ;
#190545 = CARTESIAN_POINT('Ctrl Pts',(-10.7359393141478,-13.2412209734156,
119.530993813524)) ;
#190546 = CARTESIAN_POINT('Ctrl Pts',(-10.712517892844,-13.2523620051609,
119.45965594129)) ;
#190547 = CARTESIAN_POINT('Ctrl Pts',(-10.6762276498122,-12.972854005055,
119.384625156595)) ;
#190548 = CARTESIAN_POINT('Ctrl Pts',(-10.6545701505956,-13.0035262645876,
119.318659906517)) ;
#190549 = CARTESIAN_POINT('Ctrl Pts',(-10.5807662945932,-13.0035261755681,
119.342890909878)) ;
#190550 = CARTESIAN_POINT('Ctrl Pts',(-10.5069624385908,-13.0035260865486,
119.36712191324)) ;
#190551 = CARTESIAN_POINT('Ctrl Pts',(-10.5286199378074,-12.9728538270159,
119.433087163318)) ;
#190552 = CARTESIAN_POINT('Ctrl Pts',(-10.5502774370239,-12.9421815674833,
119.499052413396)) ;
#190553 = CARTESIAN_POINT('Ctrl Pts',(-10.6240812930263,-12.9421816565028,
119.474821410034)) ;
#190554 = CARTESIAN_POINT('Ctrl Pts',(-10.6978851490287,-12.9421817455224,
119.450590406672)) ;
#190555 = CARTESIAN_POINT('Ctrl Pts',(-10.6762276498122,-12.972854005055,
119.384625156595)) ;
#190556 = CARTESIAN_POINT('Ctrl Pts',(-10.6180038705804,-12.7260422771964,
119.242651094908)) ;
#190557 = CARTESIAN_POINT('Ctrl Pts',(-10.5996471848408,-12.7739923813095,
119.186739590185)) ;
#190558 = CARTESIAN_POINT('Ctrl Pts',(-10.5258433228096,-12.7739923097986,
119.210970575184)) ;
#190559 = CARTESIAN_POINT('Ctrl Pts',(-10.4520394607784,-12.7739922382878,
119.235201560183)) ;
#190560 = CARTESIAN_POINT('Ctrl Pts',(-10.470396146518,-12.7260421341746,
119.291113064906)) ;
#190561 = CARTESIAN_POINT('Ctrl Pts',(-10.4887528322575,-12.6780920300614,
119.347024569628)) ;
#190562 = CARTESIAN_POINT('Ctrl Pts',(-10.5625566942887,-12.6780921015723,
119.32279358463)) ;
#190563 = CARTESIAN_POINT('Ctrl Pts',(-10.6363605563199,-12.6780921730832,
119.298562599631)) ;
#190564 = CARTESIAN_POINT('Ctrl Pts',(-10.6180038705804,-12.7260422771964,
119.242651094908)) ;
#190565 = CARTESIAN_POINT('Ctrl Pts',(-10.5404232380422,-12.5272823112894,
119.04200368921)) ;
#190566 = CARTESIAN_POINT('Ctrl Pts',(-10.5267175930382,-12.5891820336003,
119.000258504269)) ;
#190567 = CARTESIAN_POINT('Ctrl Pts',(-10.4529137276197,-12.5891819848851,
119.02448947895)) ;
#190568 = CARTESIAN_POINT('Ctrl Pts',(-10.3791098622012,-12.58918193617,119.048720453632)) ;
#190569 = CARTESIAN_POINT('Ctrl Pts',(-10.3928155072053,-12.5272822138591,
119.090465638574)) ;
#190570 = CARTESIAN_POINT('Ctrl Pts',(-10.4065211522092,-12.4653824915483,
119.132210823515)) ;
#190571 = CARTESIAN_POINT('Ctrl Pts',(-10.4803250176277,-12.4653825402634,
119.107979848833)) ;
#190572 = CARTESIAN_POINT('Ctrl Pts',(-10.5541288830462,-12.4653825889786,
119.083748874151)) ;
#190573 = CARTESIAN_POINT('Ctrl Pts',(-10.5404232380422,-12.5272823112894,
119.04200368921)) ;
#190574 = CARTESIAN_POINT('Ctrl Pts',(-10.4495581259175,-12.3938739809445,
118.800583074419)) ;
#190575 = CARTESIAN_POINT('Ctrl Pts',(-10.44144472112,-12.4651813337181,118.775870950958)) ;
#190576 = CARTESIAN_POINT('Ctrl Pts',(-10.3676408542443,-12.4651813074342,
118.800101921202)) ;
#190577 = CARTESIAN_POINT('Ctrl Pts',(-10.2938369873686,-12.4651812811503,
118.824332891445)) ;
#190578 = CARTESIAN_POINT('Ctrl Pts',(-10.3019503921661,-12.3938739283766,
118.849045014906)) ;
#190579 = CARTESIAN_POINT('Ctrl Pts',(-10.3100637969636,-12.322566575603,
118.873757138366)) ;
#190580 = CARTESIAN_POINT('Ctrl Pts',(-10.3838676638393,-12.3225666018869,
118.849526168123)) ;
#190581 = CARTESIAN_POINT('Ctrl Pts',(-10.4576715307149,-12.3225666281708,
118.825295197879)) ;
#190582 = CARTESIAN_POINT('Ctrl Pts',(-10.4495581259175,-12.3938739809445,
118.800583074419)) ;
#190583 = CARTESIAN_POINT('Ctrl Pts',(-10.3500894578653,-12.3331330123649,
118.53313055352)) ;
#190584 = CARTESIAN_POINT('Ctrl Pts',(-10.348173757062,-12.4087892430706,
118.527295636584)) ;
#190585 = CARTESIAN_POINT('Ctrl Pts',(-10.2743698913232,-12.408789238365,
118.551526610291)) ;
#190586 = CARTESIAN_POINT('Ctrl Pts',(-10.2005660255843,-12.4087892336594,
118.575757583997)) ;
#190587 = CARTESIAN_POINT('Ctrl Pts',(-10.2024817263876,-12.3331330029537,
118.581592500933)) ;
#190588 = CARTESIAN_POINT('Ctrl Pts',(-10.2043974271909,-12.257476772248,
118.587427417868)) ;
#190589 = CARTESIAN_POINT('Ctrl Pts',(-10.2782012929297,-12.2574767769536,
118.563196444162)) ;
#190590 = CARTESIAN_POINT('Ctrl Pts',(-10.3520051586686,-12.2574767816592,
118.538965470456)) ;
#190591 = CARTESIAN_POINT('Ctrl Pts',(-10.3500894578653,-12.3331330123649,
118.53313055352)) ;
#190592 = CARTESIAN_POINT('Ctrl Pts',(-10.2491542011391,-12.3500900604043,
118.261071608061)) ;
#190593 = CARTESIAN_POINT('Ctrl Pts',(-10.2535509429431,-12.4246766699504,
118.274463372938)) ;
#190594 = CARTESIAN_POINT('Ctrl Pts',(-10.1797470798509,-12.4246766830339,
118.298694354706)) ;
#190595 = CARTESIAN_POINT('Ctrl Pts',(-10.1059432167588,-12.4246766961173,
118.322925336473)) ;
#190596 = CARTESIAN_POINT('Ctrl Pts',(-10.1015464749548,-12.3500900865712,
118.309533571596)) ;
#190597 = CARTESIAN_POINT('Ctrl Pts',(-10.0971497331507,-12.2755034770251,
118.296141806718)) ;
#190598 = CARTESIAN_POINT('Ctrl Pts',(-10.1709535962429,-12.2755034639416,
118.27191082495)) ;
#190599 = CARTESIAN_POINT('Ctrl Pts',(-10.2447574593351,-12.2755034508582,
118.247679843183)) ;
#190600 = CARTESIAN_POINT('Ctrl Pts',(-10.2491542011391,-12.3500900604043,
118.261071608061)) ;
#190601 = CARTESIAN_POINT('Ctrl Pts',(-10.1522204522322,-12.4439523224458,
118.001438639181)) ;
#190602 = CARTESIAN_POINT('Ctrl Pts',(-10.1626549630217,-12.5120989674076,
118.033220474389)) ;
#190603 = CARTESIAN_POINT('Ctrl Pts',(-10.0888511045098,-12.5120989925412,
118.057451470107)) ;
#190604 = CARTESIAN_POINT('Ctrl Pts',(-10.0150472459978,-12.5120990176749,
118.081682465826)) ;
#190605 = CARTESIAN_POINT('Ctrl Pts',(-10.0046127352084,-12.4439523727131,
118.049900630617)) ;
#190606 = CARTESIAN_POINT('Ctrl Pts',(-9.99417822441887,-12.3758057277512,
118.018118795408)) ;
#190607 = CARTESIAN_POINT('Ctrl Pts',(-10.0679820829308,-12.3758057026176,
117.99388779969)) ;
#190608 = CARTESIAN_POINT('Ctrl Pts',(-10.1417859414427,-12.3758056774839,
117.969656803972)) ;
#190609 = CARTESIAN_POINT('Ctrl Pts',(-10.1522204522322,-12.4439523224458,
118.001438639181)) ;
#190610 = CARTESIAN_POINT('Ctrl Pts',(-10.0665263018171,-12.607738556858,
117.775916927757)) ;
#190611 = CARTESIAN_POINT('Ctrl Pts',(-10.0822256130435,-12.6645527953263,
117.823734495797)) ;
#190612 = CARTESIAN_POINT('Ctrl Pts',(-10.0084217591895,-12.6645528262529,
117.847965505703)) ;
#190613 = CARTESIAN_POINT('Ctrl Pts',(-9.93461790533546,-12.6645528571796,
117.872196515608)) ;
#190614 = CARTESIAN_POINT('Ctrl Pts',(-9.91891859410901,-12.6077386187113,
117.824378947568)) ;
#190615 = CARTESIAN_POINT('Ctrl Pts',(-9.90321928288255,-12.5509243802431,
117.776561379528)) ;
#190616 = CARTESIAN_POINT('Ctrl Pts',(-9.97702313673659,-12.5509243493165,
117.752330369622)) ;
#190617 = CARTESIAN_POINT('Ctrl Pts',(-10.0508269905906,-12.5509243183898,
117.728099359717)) ;
#190618 = CARTESIAN_POINT('Ctrl Pts',(-10.0665263018171,-12.607738556858,
117.775916927757)) ;
#190619 = CARTESIAN_POINT('Ctrl Pts',(-9.9973141738669,-12.8282760815645,
117.600428827391)) ;
#190620 = CARTESIAN_POINT('Ctrl Pts',(-10.0171388338787,-12.8697778180786,
117.660811542349)) ;
#190621 = CARTESIAN_POINT('Ctrl Pts',(-9.94333498419105,-12.8697778506645,
117.685042564945)) ;
#190622 = CARTESIAN_POINT('Ctrl Pts',(-9.86953113450339,-12.8697778832504,
117.70927358754)) ;
#190623 = CARTESIAN_POINT('Ctrl Pts',(-9.84970647449161,-12.8282761467363,
117.648890872582)) ;
#190624 = CARTESIAN_POINT('Ctrl Pts',(-9.8298818144798,-12.7867744102223,
117.588508157623)) ;
#190625 = CARTESIAN_POINT('Ctrl Pts',(-9.90368566416747,-12.7867743776364,
117.564277135028)) ;
#190626 = CARTESIAN_POINT('Ctrl Pts',(-9.97748951385512,-12.7867743450505,
117.540046112432)) ;
#190627 = CARTESIAN_POINT('Ctrl Pts',(-9.9973141738669,-12.8282760815645,
117.600428827391)) ;
#190628 = CARTESIAN_POINT('Ctrl Pts',(-9.94813424492341,-13.0924261676405,
117.486171962013)) ;
#190629 = CARTESIAN_POINT('Ctrl Pts',(-9.97068753593406,-13.1155471529824,
117.554865646909)) ;
#190630 = CARTESIAN_POINT('Ctrl Pts',(-9.8968836900418,-13.1155471809982,
117.579096681065)) ;
#190631 = CARTESIAN_POINT('Ctrl Pts',(-9.82307984414954,-13.1155472090139,
117.60332771522)) ;
#190632 = CARTESIAN_POINT('Ctrl Pts',(-9.80052655313887,-13.092426223672,
117.534634030324)) ;
#190633 = CARTESIAN_POINT('Ctrl Pts',(-9.7779732621282,-13.06930523833,117.465940345428)) ;
#190634 = CARTESIAN_POINT('Ctrl Pts',(-9.85177710802046,-13.0693052103143,
117.441709311273)) ;
#190635 = CARTESIAN_POINT('Ctrl Pts',(-9.9255809539127,-13.0693051822985,
117.417478277117)) ;
#190636 = CARTESIAN_POINT('Ctrl Pts',(-9.94813424492341,-13.0924261676405,
117.486171962013)) ;
#190637 = CARTESIAN_POINT('Ctrl Pts',(-9.92229665695523,-13.3792544087802,
117.442915109267)) ;
#190638 = CARTESIAN_POINT('Ctrl Pts',(-9.94595477750255,-13.3823829246599,
117.514973926819)) ;
#190639 = CARTESIAN_POINT('Ctrl Pts',(-9.87215093408175,-13.3823829459244,
117.539204968502)) ;
#190640 = CARTESIAN_POINT('Ctrl Pts',(-9.79834709066094,-13.3823829671888,
117.563436010186)) ;
#190641 = CARTESIAN_POINT('Ctrl Pts',(-9.77468897011363,-13.3792544513091,
117.491377192633)) ;
#190642 = CARTESIAN_POINT('Ctrl Pts',(-9.75103084956629,-13.3761259354293,
117.419318375081)) ;
#190643 = CARTESIAN_POINT('Ctrl Pts',(-9.82483469298709,-13.3761259141649,
117.395087333397)) ;
#190644 = CARTESIAN_POINT('Ctrl Pts',(-9.8986385364079,-13.3761258929005,
117.370856291714)) ;
#190645 = CARTESIAN_POINT('Ctrl Pts',(-9.92229665695523,-13.3792544087802,
117.442915109267)) ;
#190646 = CARTESIAN_POINT('Ctrl Pts',(-9.9207435467235,-13.6698091146606,
117.47374538968)) ;
#190647 = CARTESIAN_POINT('Ctrl Pts',(-9.94381007459405,-13.6526542862593,
117.54400231155)) ;
#190648 = CARTESIAN_POINT('Ctrl Pts',(-9.87000623233327,-13.6526542988554,
117.568233356767)) ;
#190649 = CARTESIAN_POINT('Ctrl Pts',(-9.79620239007249,-13.6526543114514,
117.592464401983)) ;
#190650 = CARTESIAN_POINT('Ctrl Pts',(-9.77313586220196,-13.6698091398527,
117.522207480113)) ;
#190651 = CARTESIAN_POINT('Ctrl Pts',(-9.75006933433139,-13.686963968254,
117.451950558243)) ;
#190652 = CARTESIAN_POINT('Ctrl Pts',(-9.82387317659218,-13.686963955658,
117.427719513027)) ;
#190653 = CARTESIAN_POINT('Ctrl Pts',(-9.89767701885295,-13.6869639430619,
117.40348846781)) ;
#190654 = CARTESIAN_POINT('Ctrl Pts',(-9.9207435467235,-13.6698091146606,
117.47374538968)) ;
#190655 = CARTESIAN_POINT('Ctrl Pts',(-9.94290969392009,-13.9412445098837,
117.576695883073)) ;
#190656 = CARTESIAN_POINT('Ctrl Pts',(-9.96372985878011,-13.9051106030385,
117.640110745778)) ;
#190657 = CARTESIAN_POINT('Ctrl Pts',(-9.88992601655304,-13.9051106090347,
117.664341791097)) ;
#190658 = CARTESIAN_POINT('Ctrl Pts',(-9.81612217432595,-13.905110615031,
117.688572836417)) ;
#190659 = CARTESIAN_POINT('Ctrl Pts',(-9.79530200946594,-13.9412445218762,
117.625157973711)) ;
#190660 = CARTESIAN_POINT('Ctrl Pts',(-9.7744818446059,-13.9773784287214,
117.561743111006)) ;
#190661 = CARTESIAN_POINT('Ctrl Pts',(-9.84828568683299,-13.9773784227252,
117.537512065686)) ;
#190662 = CARTESIAN_POINT('Ctrl Pts',(-9.92208952906005,-13.9773784167289,
117.513281020367)) ;
#190663 = CARTESIAN_POINT('Ctrl Pts',(-9.94290969392009,-13.9412445098837,
117.576695883073)) ;
#190664 = CARTESIAN_POINT('Ctrl Pts',(-9.9861032646117,-14.1747166899893,
117.74357571091)) ;
#190665 = CARTESIAN_POINT('Ctrl Pts',(-10.0032076914057,-14.1222263839683,
117.795673035085)) ;
#190666 = CARTESIAN_POINT('Ctrl Pts',(-9.92940384865615,-14.1222263855747,
117.819904078812)) ;
#190667 = CARTESIAN_POINT('Ctrl Pts',(-9.85560000590656,-14.122226387181,
117.84413512254)) ;
#190668 = CARTESIAN_POINT('Ctrl Pts',(-9.8384955791125,-14.1747166932021,
117.792037798365)) ;
#190669 = CARTESIAN_POINT('Ctrl Pts',(-9.82139115231847,-14.2272069992232,
117.739940474191)) ;
#190670 = CARTESIAN_POINT('Ctrl Pts',(-9.89519499506806,-14.2272069976168,
117.715709430463)) ;
#190671 = CARTESIAN_POINT('Ctrl Pts',(-9.96899883781767,-14.2272069960104,
117.691478386735)) ;
#190672 = CARTESIAN_POINT('Ctrl Pts',(-9.9861032646117,-14.1747166899893,
117.74357571091)) ;
#190673 = CARTESIAN_POINT('Ctrl Pts',(-10.0471796021649,-14.355514528968,
117.96520267545)) ;
#190674 = CARTESIAN_POINT('Ctrl Pts',(-10.0593081194111,-14.2903204554486,
118.002144182084)) ;
#190675 = CARTESIAN_POINT('Ctrl Pts',(-9.98550427561081,-14.2903204543728,
118.026375222612)) ;
#190676 = CARTESIAN_POINT('Ctrl Pts',(-9.91170043181045,-14.290320453297,
118.050606263139)) ;
#190677 = CARTESIAN_POINT('Ctrl Pts',(-9.89957191456421,-14.3555145268165,
118.013664756505)) ;
#190678 = CARTESIAN_POINT('Ctrl Pts',(-9.88744339731793,-14.4207086003359,
117.97672324987)) ;
#190679 = CARTESIAN_POINT('Ctrl Pts',(-9.96124724111826,-14.4207086014117,
117.952492209343)) ;
#190680 = CARTESIAN_POINT('Ctrl Pts',(-10.0350510849186,-14.4207086024875,
117.928261168815)) ;
#190681 = CARTESIAN_POINT('Ctrl Pts',(-10.0471796021649,-14.355514528968,
117.96520267545)) ;
#190682 = CARTESIAN_POINT('Ctrl Pts',(-10.1202605083237,-14.4682461385157,
118.223189643421)) ;
#190683 = CARTESIAN_POINT('Ctrl Pts',(-10.1265714543446,-14.3950833007867,
118.242411766797)) ;
#190684 = CARTESIAN_POINT('Ctrl Pts',(-10.0527676099358,-14.3950832998909,
118.266642805471)) ;
#190685 = CARTESIAN_POINT('Ctrl Pts',(-9.97896376552697,-14.395083298995,
118.290873844145)) ;
#190686 = CARTESIAN_POINT('Ctrl Pts',(-9.97265281950605,-14.468246136724,
118.271651720769)) ;
#190687 = CARTESIAN_POINT('Ctrl Pts',(-9.96634187348515,-14.5414089744529,
118.252429597393)) ;
#190688 = CARTESIAN_POINT('Ctrl Pts',(-10.040145717894,-14.5414089753487,
118.228198558719)) ;
#190689 = CARTESIAN_POINT('Ctrl Pts',(-10.1139495623028,-14.5414089762446,
118.203967520045)) ;
#190690 = CARTESIAN_POINT('Ctrl Pts',(-10.1202605083237,-14.4682461385157,
118.223189643421)) ;
#190691 = CARTESIAN_POINT('Ctrl Pts',(-10.2000975446143,-14.5059599121584,
118.501953451591)) ;
#190692 = CARTESIAN_POINT('Ctrl Pts',(-10.2001061244579,-14.4300548891346,
118.501979584462)) ;
#190693 = CARTESIAN_POINT('Ctrl Pts',(-10.1263022802071,-14.4300548892677,
118.526210623618)) ;
#190694 = CARTESIAN_POINT('Ctrl Pts',(-10.0524984359563,-14.4300548894008,
118.550441662773)) ;
#190695 = CARTESIAN_POINT('Ctrl Pts',(-10.0524898561127,-14.5059599124246,
118.550415529902)) ;
#190696 = CARTESIAN_POINT('Ctrl Pts',(-10.0524812762691,-14.5818649354484,
118.55038939703)) ;
#190697 = CARTESIAN_POINT('Ctrl Pts',(-10.1262851205199,-14.5818649353153,
118.526158357875)) ;
#190698 = CARTESIAN_POINT('Ctrl Pts',(-10.2000889647707,-14.5818649351822,
118.50192731872)) ;
#190699 = CARTESIAN_POINT('Ctrl Pts',(-10.2000975446143,-14.5059599121584,
118.501953451591)) ;
#190700 = CARTESIAN_POINT('Ctrl Pts',(-10.279142301007,-14.4658731530402,
118.777992572)) ;
#190701 = CARTESIAN_POINT('Ctrl Pts',(-10.2729014028888,-14.3926562072765,
118.758983803308)) ;
#190702 = CARTESIAN_POINT('Ctrl Pts',(-10.1990975593153,-14.3926562077147,
118.783214844527)) ;
#190703 = CARTESIAN_POINT('Ctrl Pts',(-10.1252937157419,-14.3926562081529,
118.807445885745)) ;
#190704 = CARTESIAN_POINT('Ctrl Pts',(-10.1315346138602,-14.4658731539167,
118.826454654437)) ;
#190705 = CARTESIAN_POINT('Ctrl Pts',(-10.1377755119784,-14.5390900996804,
118.845463423128)) ;
#190706 = CARTESIAN_POINT('Ctrl Pts',(-10.2115793555519,-14.5390900992422,
118.821232381909)) ;
#190707 = CARTESIAN_POINT('Ctrl Pts',(-10.2853831991253,-14.539090098804,
118.797001340691)) ;
#190708 = CARTESIAN_POINT('Ctrl Pts',(-10.279142301007,-14.4658731530402,
118.777992572)) ;
#190709 = CARTESIAN_POINT('Ctrl Pts',(-10.352240241271,-14.3505784504634,
119.036184934344)) ;
#190710 = CARTESIAN_POINT('Ctrl Pts',(-10.3401503369545,-14.2853046871927,
118.999361036421)) ;
#190711 = CARTESIAN_POINT('Ctrl Pts',(-10.266346494636,-14.2853046856717,
119.023592081462)) ;
#190712 = CARTESIAN_POINT('Ctrl Pts',(-10.1925426523175,-14.2853046841507,
119.047823126503)) ;
#190713 = CARTESIAN_POINT('Ctrl Pts',(-10.204632556634,-14.3505784474213,
119.084647024426)) ;
#190714 = CARTESIAN_POINT('Ctrl Pts',(-10.2167224609505,-14.4158522106919,
119.121470922348)) ;
#190715 = CARTESIAN_POINT('Ctrl Pts',(-10.290526303269,-14.4158522122129,
119.097239877307)) ;
#190716 = CARTESIAN_POINT('Ctrl Pts',(-10.3643301455875,-14.415852213734,
119.073008832266)) ;
#190717 = CARTESIAN_POINT('Ctrl Pts',(-10.352240241271,-14.3505784504634,
119.036184934344)) ;
#190718 = CARTESIAN_POINT('Ctrl Pts',(-10.4126879463665,-14.1680509006919,
119.255822408057)) ;
#190719 = CARTESIAN_POINT('Ctrl Pts',(-10.3956244954864,-14.1154268840112,
119.203849889661)) ;
#190720 = CARTESIAN_POINT('Ctrl Pts',(-10.3218206543467,-14.1154268771774,
119.228080938293)) ;
#190721 = CARTESIAN_POINT('Ctrl Pts',(-10.248016813207,-14.1154268703437,
119.252311986924)) ;
#190722 = CARTESIAN_POINT('Ctrl Pts',(-10.2650802640871,-14.1680508870244,
119.30428450532)) ;
#190723 = CARTESIAN_POINT('Ctrl Pts',(-10.2821437149672,-14.220674903705,
119.356257023716)) ;
#190724 = CARTESIAN_POINT('Ctrl Pts',(-10.3559475561069,-14.2206749105388,
119.332025975084)) ;
#190725 = CARTESIAN_POINT('Ctrl Pts',(-10.4297513972466,-14.2206749173726,
119.307794926453)) ;
#190726 = CARTESIAN_POINT('Ctrl Pts',(-10.4126879463665,-14.1680509006919,
119.255822408057)) ;
#190727 = CARTESIAN_POINT('Ctrl Pts',(-10.4553302025288,-13.9327426687889,
119.421085323347)) ;
#190728 = CARTESIAN_POINT('Ctrl Pts',(-10.4345324484994,-13.8964722980425,
119.357738719966)) ;
#190729 = CARTESIAN_POINT('Ctrl Pts',(-10.3607286076222,-13.8964722840852,
119.381969769397)) ;
#190730 = CARTESIAN_POINT('Ctrl Pts',(-10.286924766745,-13.896472270128,119.406200818828)) ;
#190731 = CARTESIAN_POINT('Ctrl Pts',(-10.3077225207744,-13.9327426408744,
119.469547422208)) ;
#190732 = CARTESIAN_POINT('Ctrl Pts',(-10.3285202748037,-13.9690130116207,
119.532894025589)) ;
#190733 = CARTESIAN_POINT('Ctrl Pts',(-10.4023241156809,-13.969013025578,
119.508662976158)) ;
#190734 = CARTESIAN_POINT('Ctrl Pts',(-10.4761279565581,-13.9690130395352,
119.484431926727)) ;
#190735 = CARTESIAN_POINT('Ctrl Pts',(-10.4553302025288,-13.9327426687889,
119.421085323347)) ;
#190736 = CARTESIAN_POINT('Ctrl Pts',(-10.4767300292865,-13.660519783253,
119.521681152881)) ;
#190737 = CARTESIAN_POINT('Ctrl Pts',(-10.4536751293628,-13.6432040400609,
119.451459647159)) ;
#190738 = CARTESIAN_POINT('Ctrl Pts',(-10.3798712878056,-13.6432040175434,
119.475690694518)) ;
#190739 = CARTESIAN_POINT('Ctrl Pts',(-10.3060674462484,-13.643203995026,
119.499921741878)) ;
#190740 = CARTESIAN_POINT('Ctrl Pts',(-10.329122346172,-13.6605197382181,
119.570143247601)) ;
#190741 = CARTESIAN_POINT('Ctrl Pts',(-10.3521772460956,-13.6778354814103,
119.640364753323)) ;
#190742 = CARTESIAN_POINT('Ctrl Pts',(-10.4259810876529,-13.6778355039277,
119.616133705964)) ;
#190743 = CARTESIAN_POINT('Ctrl Pts',(-10.4997849292101,-13.6778355264452,
119.591902658604)) ;
#190744 = CARTESIAN_POINT('Ctrl Pts',(-10.4767300292865,-13.660519783253,
119.521681152881)) ;
#190745 = CARTESIAN_POINT('Ctrl Pts',(-10.4743674522874,-13.3693405601706,
119.550093043289)) ;
#190746 = CARTESIAN_POINT('Ctrl Pts',(-10.4507071759646,-13.3723302960764,
119.478027658547)) ;
#190747 = CARTESIAN_POINT('Ctrl Pts',(-10.3769033323417,-13.3723302632285,
119.502258699615)) ;
#190748 = CARTESIAN_POINT('Ctrl Pts',(-10.3030994887188,-13.3723302303806,
119.526489740682)) ;
#190749 = CARTESIAN_POINT('Ctrl Pts',(-10.3267597650416,-13.3693404944748,
119.598555125425)) ;
#190750 = CARTESIAN_POINT('Ctrl Pts',(-10.3504200413644,-13.3663507585691,
119.670620510168)) ;
#190751 = CARTESIAN_POINT('Ctrl Pts',(-10.4242238849873,-13.366350791417,
119.6463894691)) ;
#190752 = CARTESIAN_POINT('Ctrl Pts',(-10.4980277286102,-13.3663508242649,
119.622158428032)) ;
#190753 = CARTESIAN_POINT('Ctrl Pts',(-10.4743674522874,-13.3693405601706,
119.550093043289)) ;
#190754 = CARTESIAN_POINT('Ctrl Pts',(-10.4477380288771,-13.0834454323783,
119.504368831108)) ;
#190755 = CARTESIAN_POINT('Ctrl Pts',(-10.4251707000769,-13.1064007088209,
119.435632388021)) ;
#190756 = CARTESIAN_POINT('Ctrl Pts',(-10.3513668529602,-13.1064006698969,
119.459863418448)) ;
#190757 = CARTESIAN_POINT('Ctrl Pts',(-10.2775630058435,-13.1064006309729,
119.484094448874)) ;
#190758 = CARTESIAN_POINT('Ctrl Pts',(-10.3001303346437,-13.0834453545303,
119.552830891961)) ;
#190759 = CARTESIAN_POINT('Ctrl Pts',(-10.3226976634438,-13.0604900780877,
119.621567335047)) ;
#190760 = CARTESIAN_POINT('Ctrl Pts',(-10.3965015105605,-13.0604901170117,
119.597336304621)) ;
#190761 = CARTESIAN_POINT('Ctrl Pts',(-10.4703053576772,-13.0604901559357,
119.573105274194)) ;
#190762 = CARTESIAN_POINT('Ctrl Pts',(-10.4477380288771,-13.0834454323783,
119.504368831108)) ;
#190763 = CARTESIAN_POINT('Ctrl Pts',(-10.3980917229495,-12.8212149019315,
119.388565275558)) ;
#190764 = CARTESIAN_POINT('Ctrl Pts',(-10.3782253674531,-12.8625120463937,
119.328055561196)) ;
#190765 = CARTESIAN_POINT('Ctrl Pts',(-10.3044215158748,-12.8625120051449,
119.352286578033)) ;
#190766 = CARTESIAN_POINT('Ctrl Pts',(-10.2306176642965,-12.8625119638961,
119.37651759487)) ;
#190767 = CARTESIAN_POINT('Ctrl Pts',(-10.250484019793,-12.8212148194339,
119.437027309232)) ;
#190768 = CARTESIAN_POINT('Ctrl Pts',(-10.2703503752895,-12.7799176749718,
119.497537023594)) ;
#190769 = CARTESIAN_POINT('Ctrl Pts',(-10.3441542268677,-12.7799177162206,
119.473306006757)) ;
#190770 = CARTESIAN_POINT('Ctrl Pts',(-10.417958078446,-12.7799177574694,
119.44907498992)) ;
#190771 = CARTESIAN_POINT('Ctrl Pts',(-10.3980917229495,-12.8212149019315,
119.388565275558)) ;
#190772 = CARTESIAN_POINT('Ctrl Pts',(-10.3280493110319,-12.6012650290221,
119.21069278713)) ;
#190773 = CARTESIAN_POINT('Ctrl Pts',(-10.3123106560122,-12.6579784616352,
119.16275538225)) ;
#190774 = CARTESIAN_POINT('Ctrl Pts',(-10.2385067992872,-12.6579784230308,
119.186986383411)) ;
#190775 = CARTESIAN_POINT('Ctrl Pts',(-10.164702942562,-12.6579783844264,
119.211217384571)) ;
#190776 = CARTESIAN_POINT('Ctrl Pts',(-10.1804415975817,-12.6012649518134,
119.259154789451)) ;
#190777 = CARTESIAN_POINT('Ctrl Pts',(-10.1961802526014,-12.5445515192003,
119.30709219433)) ;
#190778 = CARTESIAN_POINT('Ctrl Pts',(-10.2699841093265,-12.5445515578047,
119.28286119317)) ;
#190779 = CARTESIAN_POINT('Ctrl Pts',(-10.3437879660516,-12.5445515964091,
119.258630192009)) ;
#190780 = CARTESIAN_POINT('Ctrl Pts',(-10.3280493110319,-12.6012650290221,
119.21069278713)) ;
#190781 = CARTESIAN_POINT('Ctrl Pts',(-10.2417633229291,-12.4396335453714,
118.983410941354)) ;
#190782 = CARTESIAN_POINT('Ctrl Pts',(-10.2312909677737,-12.5077139487023,
118.951513835972)) ;
#190783 = CARTESIAN_POINT('Ctrl Pts',(-10.1574871057891,-12.5077139189152,
118.975744821113)) ;
#190784 = CARTESIAN_POINT('Ctrl Pts',(-10.0836832438045,-12.5077138891282,
118.999975806254)) ;
#190785 = CARTESIAN_POINT('Ctrl Pts',(-10.0941555989599,-12.4396334857973,
119.031872911636)) ;
#190786 = CARTESIAN_POINT('Ctrl Pts',(-10.1046279541153,-12.3715530824664,
119.063770017018)) ;
#190787 = CARTESIAN_POINT('Ctrl Pts',(-10.1784318160999,-12.3715531122535,
119.039539031877)) ;
#190788 = CARTESIAN_POINT('Ctrl Pts',(-10.2522356780844,-12.3715531420405,
119.015308046736)) ;
#190789 = CARTESIAN_POINT('Ctrl Pts',(-10.2417633229291,-12.4396335453714,
118.983410941354)) ;
#190790 = CARTESIAN_POINT('Ctrl Pts',(-10.1449346240586,-12.3483868402897,
118.723968564828)) ;
#190791 = CARTESIAN_POINT('Ctrl Pts',(-10.1404732357698,-12.4229364888091,
118.710379894499)) ;
#190792 = CARTESIAN_POINT('Ctrl Pts',(-10.0666693694827,-12.4229364744478,
118.734610866535)) ;
#190793 = CARTESIAN_POINT('Ctrl Pts',(-9.99286550319555,-12.4229364600866,
118.758841838571)) ;
#190794 = CARTESIAN_POINT('Ctrl Pts',(-9.99732689148439,-12.3483868115671,
118.772430508901)) ;
#190795 = CARTESIAN_POINT('Ctrl Pts',(-10.0017882797732,-12.2738371630477,
118.78601917923)) ;
#190796 = CARTESIAN_POINT('Ctrl Pts',(-10.0755921460604,-12.2738371774089,
118.761788207194)) ;
#190797 = CARTESIAN_POINT('Ctrl Pts',(-10.1493960123475,-12.2738371917702,
118.737557235158)) ;
#190798 = CARTESIAN_POINT('Ctrl Pts',(-10.1449346240586,-12.3483868402897,
118.723968564828)) ;
#190799 = CARTESIAN_POINT('Ctrl Pts',(-10.0435893086032,-12.3339887574785,
118.450796152108)) ;
#190800 = CARTESIAN_POINT('Ctrl Pts',(-10.0454623318421,-12.4096519181944,
118.45650107709)) ;
#190801 = CARTESIAN_POINT('Ctrl Pts',(-9.97165846281568,-12.4096519246285,
118.480732040783)) ;
#190802 = CARTESIAN_POINT('Ctrl Pts',(-9.89785459378927,-12.4096519310626,
118.504963004476)) ;
#190803 = CARTESIAN_POINT('Ctrl Pts',(-9.89598157055043,-12.3339887703467,
118.499258079494)) ;
#190804 = CARTESIAN_POINT('Ctrl Pts',(-9.89410854731156,-12.2583256096307,
118.493553154512)) ;
#190805 = CARTESIAN_POINT('Ctrl Pts',(-9.96791241633798,-12.2583256031966,
118.469322190819)) ;
#190806 = CARTESIAN_POINT('Ctrl Pts',(-10.0417162853644,-12.2583255967626,
118.445091227126)) ;
#190807 = CARTESIAN_POINT('Ctrl Pts',(-10.0435893086032,-12.3339887574785,
118.450796152108)) ;
#190808 = CARTESIAN_POINT('Ctrl Pts',(-9.94475629597229,-12.3966946761742,
118.185097834847)) ;
#190809 = CARTESIAN_POINT('Ctrl Pts',(-9.95280117473567,-12.4680894419109,
118.209601235821)) ;
#190810 = CARTESIAN_POINT('Ctrl Pts',(-9.8789973054581,-12.4680894717794,
118.233832198748)) ;
#190811 = CARTESIAN_POINT('Ctrl Pts',(-9.80519343618053,-12.4680895016479,
118.258063161676)) ;
#190812 = CARTESIAN_POINT('Ctrl Pts',(-9.79714855741716,-12.3966947359113,
118.233559760702)) ;
#190813 = CARTESIAN_POINT('Ctrl Pts',(-9.78910367865378,-12.3252999701746,
118.209056359728)) ;
#190814 = CARTESIAN_POINT('Ctrl Pts',(-9.86290754793137,-12.3252999403061,
118.184825396801)) ;
#190815 = CARTESIAN_POINT('Ctrl Pts',(-9.93671141720893,-12.3252999104375,
118.160594433873)) ;
#190816 = CARTESIAN_POINT('Ctrl Pts',(-9.94475629597229,-12.3966946761742,
118.185097834847)) ;
#190817 = CARTESIAN_POINT('Ctrl Pts',(-9.85341967036429,-12.5338429010278,
117.942589305257)) ;
#190818 = CARTESIAN_POINT('Ctrl Pts',(-9.8671146551736,-12.5957672263305,
117.984302017465)) ;
#190819 = CARTESIAN_POINT('Ctrl Pts',(-9.79331078750242,-12.5957672815326,
118.008532985286)) ;
#190820 = CARTESIAN_POINT('Ctrl Pts',(-9.71950691983124,-12.5957673367347,
118.032763953106)) ;
#190821 = CARTESIAN_POINT('Ctrl Pts',(-9.70581193502193,-12.533843011432,
117.991051240898)) ;
#190822 = CARTESIAN_POINT('Ctrl Pts',(-9.69211695021262,-12.4719186861293,
117.94933852869)) ;
#190823 = CARTESIAN_POINT('Ctrl Pts',(-9.7659208178838,-12.4719186309272,
117.92510756087)) ;
#190824 = CARTESIAN_POINT('Ctrl Pts',(-9.83972468555498,-12.4719185757251,
117.900876593049)) ;
#190825 = CARTESIAN_POINT('Ctrl Pts',(-9.85341967036429,-12.5338429010278,
117.942589305257)) ;
#190826 = CARTESIAN_POINT('Ctrl Pts',(-9.77721000168019,-12.7326606979156,
117.745753431851)) ;
#190827 = CARTESIAN_POINT('Ctrl Pts',(-9.79551548151559,-12.780794213553,
117.801508967934)) ;
#190828 = CARTESIAN_POINT('Ctrl Pts',(-9.72171161855032,-12.7807942904156,
117.825739950088)) ;
#190829 = CARTESIAN_POINT('Ctrl Pts',(-9.64790775558505,-12.7807943672782,
117.849970932242)) ;
#190830 = CARTESIAN_POINT('Ctrl Pts',(-9.62960227574966,-12.7326608516408,
117.794215396159)) ;
#190831 = CARTESIAN_POINT('Ctrl Pts',(-9.61129679591425,-12.6845273360034,
117.738459860075)) ;
#190832 = CARTESIAN_POINT('Ctrl Pts',(-9.68510065887952,-12.6845272591408,
117.714228877921)) ;
#190833 = CARTESIAN_POINT('Ctrl Pts',(-9.75890452184478,-12.6845271822782,
117.689997895767)) ;
#190834 = CARTESIAN_POINT('Ctrl Pts',(-9.77721000168019,-12.7326606979156,
117.745753431851)) ;
#190835 = CARTESIAN_POINT('Ctrl Pts',(-9.71941528284546,-12.9811862243396,
117.605182017047)) ;
#190836 = CARTESIAN_POINT('Ctrl Pts',(-9.74104880236432,-13.0120391573078,
117.671074224952)) ;
#190837 = CARTESIAN_POINT('Ctrl Pts',(-9.66724494595711,-13.0120392516688,
117.69530522708)) ;
#190838 = CARTESIAN_POINT('Ctrl Pts',(-9.5934410895499,-13.0120393460298,
117.719536229209)) ;
#190839 = CARTESIAN_POINT('Ctrl Pts',(-9.57180757003104,-12.9811864130616,
117.653644021304)) ;
#190840 = CARTESIAN_POINT('Ctrl Pts',(-9.55017405051217,-12.9503334800935,
117.587751813399)) ;
#190841 = CARTESIAN_POINT('Ctrl Pts',(-9.62397790691939,-12.9503333857324,
117.56352081127)) ;
#190842 = CARTESIAN_POINT('Ctrl Pts',(-9.6977817633266,-12.9503332913714,
117.539289809141)) ;
#190843 = CARTESIAN_POINT('Ctrl Pts',(-9.71941528284546,-12.9811862243396,
117.605182017047)) ;
#190844 = CARTESIAN_POINT('Ctrl Pts',(-9.68389597109276,-13.260918115125,
117.532433827482)) ;
#190845 = CARTESIAN_POINT('Ctrl Pts',(-9.70730780262489,-13.2722865612631,
117.603742486795)) ;
#190846 = CARTESIAN_POINT('Ctrl Pts',(-9.63350395438863,-13.2722866661501,
117.627973513811)) ;
#190847 = CARTESIAN_POINT('Ctrl Pts',(-9.55970010615233,-13.2722867710372,
117.652204540827)) ;
#190848 = CARTESIAN_POINT('Ctrl Pts',(-9.53628827462019,-13.2609183248991,
117.580895881514)) ;
#190849 = CARTESIAN_POINT('Ctrl Pts',(-9.51287644308806,-13.249549878761,
117.509587222201)) ;
#190850 = CARTESIAN_POINT('Ctrl Pts',(-9.58668029132435,-13.249549773874,
117.485356195185)) ;
#190851 = CARTESIAN_POINT('Ctrl Pts',(-9.66048413956062,-13.249549668987,
117.461125168169)) ;
#190852 = CARTESIAN_POINT('Ctrl Pts',(-9.68389597109276,-13.260918115125,
117.532433827482)) ;
#190853 = CARTESIAN_POINT('Ctrl Pts',(-9.67242963948662,-13.5531074788782,
117.533099665877)) ;
#190854 = CARTESIAN_POINT('Ctrl Pts',(-9.69594021851786,-13.5440933427765,
117.604709094102)) ;
#190855 = CARTESIAN_POINT('Ctrl Pts',(-9.62213637927301,-13.5440934499071,
117.628940148505)) ;
#190856 = CARTESIAN_POINT('Ctrl Pts',(-9.54833254002818,-13.5440935570377,
117.653171202907)) ;
#190857 = CARTESIAN_POINT('Ctrl Pts',(-9.52482196099694,-13.5531076931393,
117.581561774682)) ;
#190858 = CARTESIAN_POINT('Ctrl Pts',(-9.5013113819657,-13.5621218292409,
117.509952346458)) ;
#190859 = CARTESIAN_POINT('Ctrl Pts',(-9.57511522121055,-13.5621217221104,
117.485721292055)) ;
#190860 = CARTESIAN_POINT('Ctrl Pts',(-9.64891906045538,-13.5621216149798,
117.461490237653)) ;
#190861 = CARTESIAN_POINT('Ctrl Pts',(-9.67242963948662,-13.5531074788782,
117.533099665877)) ;
#190862 = CARTESIAN_POINT('Ctrl Pts',(-9.68511244301849,-13.8336246591284,
117.607072550047)) ;
#190863 = CARTESIAN_POINT('Ctrl Pts',(-9.70704089076989,-13.8050124160848,
117.673863061661)) ;
#190864 = CARTESIAN_POINT('Ctrl Pts',(-9.63323706028518,-13.805012516226,
117.698094142745)) ;
#190865 = CARTESIAN_POINT('Ctrl Pts',(-9.55943322980046,-13.8050126163672,
117.72232522383)) ;
#190866 = CARTESIAN_POINT('Ctrl Pts',(-9.53750478204908,-13.8336248594109,
117.655534712216)) ;
#190867 = CARTESIAN_POINT('Ctrl Pts',(-9.51557633429766,-13.8622371024545,
117.588744200601)) ;
#190868 = CARTESIAN_POINT('Ctrl Pts',(-9.58938016478238,-13.8622370023133,
117.564513119517)) ;
#190869 = CARTESIAN_POINT('Ctrl Pts',(-9.66318399526709,-13.8622369021721,
117.540282038433)) ;
#190870 = CARTESIAN_POINT('Ctrl Pts',(-9.68511244301849,-13.8336246591284,
117.607072550047)) ;
#190871 = CARTESIAN_POINT('Ctrl Pts',(-9.7201246877408,-14.0853767704005,
117.749151870546)) ;
#190872 = CARTESIAN_POINT('Ctrl Pts',(-9.73890794499503,-14.0391458019482,
117.806362639386)) ;
#190873 = CARTESIAN_POINT('Ctrl Pts',(-9.66510412230631,-14.0391458872152,
117.830593744216)) ;
#190874 = CARTESIAN_POINT('Ctrl Pts',(-9.59130029961758,-14.0391459724823,
117.854824849046)) ;
#190875 = CARTESIAN_POINT('Ctrl Pts',(-9.57251704236337,-14.0853769409346,
117.797614080206)) ;
#190876 = CARTESIAN_POINT('Ctrl Pts',(-9.55373378510916,-14.131607909387,
117.740403311365)) ;
#190877 = CARTESIAN_POINT('Ctrl Pts',(-9.62753760779788,-14.1316078241199,
117.716172206536)) ;
#190878 = CARTESIAN_POINT('Ctrl Pts',(-9.70134143048658,-14.1316077388528,
117.691941101706)) ;
#190879 = CARTESIAN_POINT('Ctrl Pts',(-9.7201246877408,-14.0853767704005,
117.749151870546)) ;
#190880 = CARTESIAN_POINT('Ctrl Pts',(-9.77484710365909,-14.2903978532202,
117.951517261547)) ;
#190881 = CARTESIAN_POINT('Ctrl Pts',(-9.7890995255308,-14.2297838798409,
117.994927836903)) ;
#190882 = CARTESIAN_POINT('Ctrl Pts',(-9.71529570863531,-14.2297839428811,
118.019158959378)) ;
#190883 = CARTESIAN_POINT('Ctrl Pts',(-9.6414918917398,-14.2297840059213,
118.043390081853)) ;
#190884 = CARTESIAN_POINT('Ctrl Pts',(-9.62723946986811,-14.2903979793006,
117.999979506497)) ;
#190885 = CARTESIAN_POINT('Ctrl Pts',(-9.61298704799638,-14.3510119526798,
117.95656893114)) ;
#190886 = CARTESIAN_POINT('Ctrl Pts',(-9.68679086489188,-14.3510118896396,
117.932337808665)) ;
#190887 = CARTESIAN_POINT('Ctrl Pts',(-9.76059468178738,-14.3510118265994,
117.90810668619)) ;
#190888 = CARTESIAN_POINT('Ctrl Pts',(-9.77484710365909,-14.2903978532202,
117.951517261547)) ;
#190889 = CARTESIAN_POINT('Ctrl Pts',(-9.84334910457871,-14.430884933304,
118.195415358412)) ;
#190890 = CARTESIAN_POINT('Ctrl Pts',(-9.8521105935028,-14.36037249955,118.222101438012)) ;
#190891 = CARTESIAN_POINT('Ctrl Pts',(-9.77830678021269,-14.3603725370538,
118.246332571468)) ;
#190892 = CARTESIAN_POINT('Ctrl Pts',(-9.70450296692257,-14.3603725745575,
118.270563704924)) ;
#190893 = CARTESIAN_POINT('Ctrl Pts',(-9.69574147799849,-14.4308850083114,
118.243877625325)) ;
#190894 = CARTESIAN_POINT('Ctrl Pts',(-9.6869799890744,-14.5013974420654,
118.217191545725)) ;
#190895 = CARTESIAN_POINT('Ctrl Pts',(-9.76078380236452,-14.5013974045617,
118.192960412269)) ;
#190896 = CARTESIAN_POINT('Ctrl Pts',(-9.83458761565463,-14.501397367058,
118.168729278813)) ;
#190897 = CARTESIAN_POINT('Ctrl Pts',(-9.84334910457871,-14.430884933304,
118.195415358412)) ;
#190898 = CARTESIAN_POINT('Ctrl Pts',(-9.92122616212989,-14.5000545452193,
118.468156118046)) ;
#190899 = CARTESIAN_POINT('Ctrl Pts',(-9.92382827917419,-14.4246071586731,
118.47608174479)) ;
#190900 = CARTESIAN_POINT('Ctrl Pts',(-9.85002446664451,-14.4246071686467,
118.500312880563)) ;
#190901 = CARTESIAN_POINT('Ctrl Pts',(-9.77622065411485,-14.4246071786203,
118.524544016335)) ;
#190902 = CARTESIAN_POINT('Ctrl Pts',(-9.77361853707056,-14.5000545651665,
118.516618389591)) ;
#190903 = CARTESIAN_POINT('Ctrl Pts',(-9.77101642002627,-14.5755019517128,
118.508692762847)) ;
#190904 = CARTESIAN_POINT('Ctrl Pts',(-9.84482023255593,-14.5755019417391,
118.484461627074)) ;
#190905 = CARTESIAN_POINT('Ctrl Pts',(-9.9186240450856,-14.5755019317655,
118.460230491302)) ;
#190906 = CARTESIAN_POINT('Ctrl Pts',(-9.92122616212989,-14.5000545452193,
118.468156118046)) ;
#190907 = CARTESIAN_POINT('Ctrl Pts',(-10.0013588136134,-14.4915166284975,
118.74761997857)) ;
#190908 = CARTESIAN_POINT('Ctrl Pts',(-9.99763779706234,-14.4165522893736,
118.736286360703)) ;
#190909 = CARTESIAN_POINT('Ctrl Pts',(-9.9238339828673,-14.4165522733908,
118.760517491403)) ;
#190910 = CARTESIAN_POINT('Ctrl Pts',(-9.85003016867226,-14.4165522574081,
118.784748622103)) ;
#190911 = CARTESIAN_POINT('Ctrl Pts',(-9.85375118522337,-14.491516596532,
118.796082239971)) ;
#190912 = CARTESIAN_POINT('Ctrl Pts',(-9.85747220177447,-14.566480935656,
118.807415857838)) ;
#190913 = CARTESIAN_POINT('Ctrl Pts',(-9.93127601596952,-14.5664809516387,
118.783184727138)) ;
#190914 = CARTESIAN_POINT('Ctrl Pts',(-10.0050798301646,-14.5664809676215,
118.758953596437)) ;
#190915 = CARTESIAN_POINT('Ctrl Pts',(-10.0013588136134,-14.4915166284975,
118.74761997857)) ;
#190916 = CARTESIAN_POINT('Ctrl Pts',(-10.0779474866917,-14.4057133919849,
119.016492386824)) ;
#190917 = CARTESIAN_POINT('Ctrl Pts',(-10.0681370537657,-14.3366264116548,
118.986611389331)) ;
#190918 = CARTESIAN_POINT('Ctrl Pts',(-9.99433323529747,-14.3366263740412,
119.010842507016)) ;
#190919 = CARTESIAN_POINT('Ctrl Pts',(-9.92052941682924,-14.3366263364276,
119.035073624701)) ;
#190920 = CARTESIAN_POINT('Ctrl Pts',(-9.93033984975523,-14.4057133167577,
119.064954622193)) ;
#190921 = CARTESIAN_POINT('Ctrl Pts',(-9.94015028268123,-14.4748002970877,
119.094835619686)) ;
#190922 = CARTESIAN_POINT('Ctrl Pts',(-10.0139541011495,-14.4748003347014,
119.070604502001)) ;
#190923 = CARTESIAN_POINT('Ctrl Pts',(-10.0877579196177,-14.474800372315,
119.046373384316)) ;
#190924 = CARTESIAN_POINT('Ctrl Pts',(-10.0779474866917,-14.4057133919849,
119.016492386824)) ;
#190925 = CARTESIAN_POINT('Ctrl Pts',(-10.1439356362234,-14.2496052022137,
119.252877640221)) ;
#190926 = CARTESIAN_POINT('Ctrl Pts',(-10.1287707813893,-14.1913134689692,
119.206687937649)) ;
#190927 = CARTESIAN_POINT('Ctrl Pts',(-10.0549669574364,-14.1913134155293,
119.230919038628)) ;
#190928 = CARTESIAN_POINT('Ctrl Pts',(-9.98116313348346,-14.1913133620894,
119.255150139607)) ;
#190929 = CARTESIAN_POINT('Ctrl Pts',(-9.9963279883176,-14.2496050953339,
119.30133984218)) ;
#190930 = CARTESIAN_POINT('Ctrl Pts',(-10.0114928431517,-14.3078968285784,
119.347529544752)) ;
#190931 = CARTESIAN_POINT('Ctrl Pts',(-10.0852966671046,-14.3078968820183,
119.323298443772)) ;
#190932 = CARTESIAN_POINT('Ctrl Pts',(-10.1591004910575,-14.3078969354582,
119.299067342793)) ;
#190933 = CARTESIAN_POINT('Ctrl Pts',(-10.1439356362234,-14.2496052022137,
119.252877640221)) ;
#190934 = CARTESIAN_POINT('Ctrl Pts',(-10.1943912071192,-14.0337448610519,
119.442029357324)) ;
#190935 = CARTESIAN_POINT('Ctrl Pts',(-10.1749466541285,-13.9904362158164,
119.382804384838)) ;
#190936 = CARTESIAN_POINT('Ctrl Pts',(-10.1011428237473,-13.9904361538178,
119.407035466237)) ;
#190937 = CARTESIAN_POINT('Ctrl Pts',(-10.027338993366,-13.9904360918192,
119.431266547637)) ;
#190938 = CARTESIAN_POINT('Ctrl Pts',(-10.0467835463566,-14.0337447370547,
119.490491520124)) ;
#190939 = CARTESIAN_POINT('Ctrl Pts',(-10.0662280993472,-14.0770533822902,
119.54971649261)) ;
#190940 = CARTESIAN_POINT('Ctrl Pts',(-10.1400319297285,-14.0770534442888,
119.525485411211)) ;
#190941 = CARTESIAN_POINT('Ctrl Pts',(-10.2138357601098,-14.0770535062874,
119.501254329811)) ;
#190942 = CARTESIAN_POINT('Ctrl Pts',(-10.1943912071192,-14.0337448610519,
119.442029357324)) ;
#190943 = CARTESIAN_POINT('Ctrl Pts',(-10.2248051700175,-13.774289830103,
119.570067049263)) ;
#190944 = CARTESIAN_POINT('Ctrl Pts',(-10.2024751831986,-13.7490307967716,
119.50205351104)) ;
#190945 = CARTESIAN_POINT('Ctrl Pts',(-10.1286713464233,-13.7490307328435,
119.526284572964)) ;
#190946 = CARTESIAN_POINT('Ctrl Pts',(-10.0548675096479,-13.7490306689154,
119.550515634889)) ;
#190947 = CARTESIAN_POINT('Ctrl Pts',(-10.0771974964669,-13.7742897022469,
119.618529173111)) ;
#190948 = CARTESIAN_POINT('Ctrl Pts',(-10.0995274832858,-13.7995487355784,
119.686542711334)) ;
#190949 = CARTESIAN_POINT('Ctrl Pts',(-10.1733313200612,-13.7995487995064,
119.66231164941)) ;
#190950 = CARTESIAN_POINT('Ctrl Pts',(-10.2471351568365,-13.7995488634345,
119.638080587485)) ;
#190951 = CARTESIAN_POINT('Ctrl Pts',(-10.2248051700175,-13.774289830103,
119.570067049263)) ;
#190952 = CARTESIAN_POINT('Ctrl Pts',(-10.2322343776425,-13.4875484100679,
119.628322764206)) ;
#190953 = CARTESIAN_POINT('Ctrl Pts',(-10.2086144448205,-13.4822714043299,
119.556380258782)) ;
#190954 = CARTESIAN_POINT('Ctrl Pts',(-10.1348106023241,-13.4822713469427,
119.580611303281)) ;
#190955 = CARTESIAN_POINT('Ctrl Pts',(-10.0610067598278,-13.4822712895556,
119.60484234778)) ;
#190956 = CARTESIAN_POINT('Ctrl Pts',(-10.0846266926498,-13.4875482952936,
119.676784853204)) ;
#190957 = CARTESIAN_POINT('Ctrl Pts',(-10.1082466254719,-13.4928253010316,
119.748727358628)) ;
#190958 = CARTESIAN_POINT('Ctrl Pts',(-10.1820504679682,-13.4928253584187,
119.724496314129)) ;
#190959 = CARTESIAN_POINT('Ctrl Pts',(-10.2558543104646,-13.4928254158059,
119.70026526963)) ;
#190960 = CARTESIAN_POINT('Ctrl Pts',(-10.2322343776425,-13.4875484100679,
119.628322764206)) ;
#190961 = CARTESIAN_POINT('Ctrl Pts',(-10.2155030787286,-13.1987144632943,
119.612621471267)) ;
#190962 = CARTESIAN_POINT('Ctrl Pts',(-10.1922860890302,-13.2135962190273,
119.541906265711)) ;
#190963 = CARTESIAN_POINT('Ctrl Pts',(-10.1184822422072,-13.2135961694435,
119.566137297032)) ;
#190964 = CARTESIAN_POINT('Ctrl Pts',(-10.0446783953842,-13.2135961198597,
119.590368328353)) ;
#190965 = CARTESIAN_POINT('Ctrl Pts',(-10.0678953850826,-13.1987143641267,
119.661083533908)) ;
#190966 = CARTESIAN_POINT('Ctrl Pts',(-10.091112374781,-13.1838326083937,
119.731798739464)) ;
#190967 = CARTESIAN_POINT('Ctrl Pts',(-10.164916221604,-13.1838326579775,
119.707567708143)) ;
#190968 = CARTESIAN_POINT('Ctrl Pts',(-10.238720068427,-13.1838327075613,
119.683336676822)) ;
#190969 = CARTESIAN_POINT('Ctrl Pts',(-10.2155030787286,-13.1987144632943,
119.612621471267)) ;
#190970 = CARTESIAN_POINT('Ctrl Pts',(-10.1748040815892,-12.9229602452279,
119.524251932971)) ;
#190971 = CARTESIAN_POINT('Ctrl Pts',(-10.1536568930331,-12.9571183444642,
119.459841007927)) ;
#190972 = CARTESIAN_POINT('Ctrl Pts',(-10.0798530435771,-12.9571183085152,
119.484072031228)) ;
#190973 = CARTESIAN_POINT('Ctrl Pts',(-10.0060491941211,-12.9571182725662,
119.508303054529)) ;
#190974 = CARTESIAN_POINT('Ctrl Pts',(-10.0271963826772,-12.9229601733299,
119.572713979573)) ;
#190975 = CARTESIAN_POINT('Ctrl Pts',(-10.0483435712333,-12.8888020740936,
119.637124904618)) ;
#190976 = CARTESIAN_POINT('Ctrl Pts',(-10.1221474206893,-12.8888021100426,
119.612893881317)) ;
#190977 = CARTESIAN_POINT('Ctrl Pts',(-10.1959512701453,-12.8888021459916,
119.588662858015)) ;
#190978 = CARTESIAN_POINT('Ctrl Pts',(-10.1748040815892,-12.9229602452279,
119.524251932971)) ;
#190979 = CARTESIAN_POINT('Ctrl Pts',(-10.1124465818058,-12.6836290013039,
119.36980293551)) ;
#190980 = CARTESIAN_POINT('Ctrl Pts',(-10.0948870427062,-12.7345497889164,
119.316319412014)) ;
#190981 = CARTESIAN_POINT('Ctrl Pts',(-10.0210831923806,-12.7345497658022,
119.340550432667)) ;
#190982 = CARTESIAN_POINT('Ctrl Pts',(-9.94727934205508,-12.734549742688,
119.36478145332)) ;
#190983 = CARTESIAN_POINT('Ctrl Pts',(-9.9648388811547,-12.6836289550754,
119.418264976815)) ;
#190984 = CARTESIAN_POINT('Ctrl Pts',(-9.98239842025433,-12.6327081674629,
119.471748500311)) ;
#190985 = CARTESIAN_POINT('Ctrl Pts',(-10.0562022705799,-12.6327081905771,
119.447517479658)) ;
#190986 = CARTESIAN_POINT('Ctrl Pts',(-10.1300061209054,-12.6327082136913,
119.423286459006)) ;
#190987 = CARTESIAN_POINT('Ctrl Pts',(-10.1124465818058,-12.6836290013039,
119.36980293551)) ;
#190988 = CARTESIAN_POINT('Ctrl Pts',(-10.032243567432,-12.4971808863818,
119.160966196631)) ;
#190989 = CARTESIAN_POINT('Ctrl Pts',(-10.0195239505098,-12.5611972883497,
119.122224295324)) ;
#190990 = CARTESIAN_POINT('Ctrl Pts',(-9.94572010065391,-12.5611972760957,
119.146455317408)) ;
#190991 = CARTESIAN_POINT('Ctrl Pts',(-9.87191625079806,-12.5611972638417,
119.170686339491)) ;
#190992 = CARTESIAN_POINT('Ctrl Pts',(-9.88463586772028,-12.4971808618738,
119.209428240797)) ;
#190993 = CARTESIAN_POINT('Ctrl Pts',(-9.89735548464251,-12.4331644599059,
119.248170142104)) ;
#190994 = CARTESIAN_POINT('Ctrl Pts',(-9.97115933449836,-12.4331644721599,
119.22393912002)) ;
#190995 = CARTESIAN_POINT('Ctrl Pts',(-10.0449631843542,-12.4331644844139,
119.199708097937)) ;
#190996 = CARTESIAN_POINT('Ctrl Pts',(-10.032243567432,-12.4971808863818,
119.160966196631)) ;
#190997 = CARTESIAN_POINT('Ctrl Pts',(-9.93941244595383,-12.3766482309411,
118.91356140389)) ;
#190998 = CARTESIAN_POINT('Ctrl Pts',(-9.93242405862038,-12.4491772372763,
118.89227590331)) ;
#190999 = CARTESIAN_POINT('Ctrl Pts',(-9.85862020998783,-12.4491772329469,
118.916506929119)) ;
#191000 = CARTESIAN_POINT('Ctrl Pts',(-9.78481636135525,-12.4491772286174,
118.940737954929)) ;
#191001 = CARTESIAN_POINT('Ctrl Pts',(-9.7918047486887,-12.3766482222823,
118.962023455509)) ;
#191002 = CARTESIAN_POINT('Ctrl Pts',(-9.79879313602213,-12.3041192159472,
118.983308956088)) ;
#191003 = CARTESIAN_POINT('Ctrl Pts',(-9.87259698465468,-12.3041192202766,
118.959077930279)) ;
#191004 = CARTESIAN_POINT('Ctrl Pts',(-9.94640083328725,-12.304119224606,
118.93484690447)) ;
#191005 = CARTESIAN_POINT('Ctrl Pts',(-9.93941244595383,-12.3766482309411,
118.91356140389)) ;
#191006 = CARTESIAN_POINT('Ctrl Pts',(-9.83867669766088,-12.3303160635296,
118.642394997812)) ;
#191007 = CARTESIAN_POINT('Ctrl Pts',(-9.83797380881755,-12.406190350598,
118.640254111632)) ;
#191008 = CARTESIAN_POINT('Ctrl Pts',(-9.76416996259023,-12.4061903509704,
118.664485144767)) ;
#191009 = CARTESIAN_POINT('Ctrl Pts',(-9.69036611636291,-12.4061903513427,
118.688716177902)) ;
#191010 = CARTESIAN_POINT('Ctrl Pts',(-9.69106900520625,-12.3303160642744,
118.690857064083)) ;
#191011 = CARTESIAN_POINT('Ctrl Pts',(-9.69177189404958,-12.254441777206,
118.692997950263)) ;
#191012 = CARTESIAN_POINT('Ctrl Pts',(-9.7655757402769,-12.2544417768337,
118.668766917128)) ;
#191013 = CARTESIAN_POINT('Ctrl Pts',(-9.8393795865042,-12.2544417764613,
118.644535883993)) ;
#191014 = CARTESIAN_POINT('Ctrl Pts',(-9.83867669766088,-12.3303160635296,
118.642394997812)) ;
#191015 = CARTESIAN_POINT('Ctrl Pts',(-9.73837574668705,-12.3620878034078,
118.372182541714)) ;
#191016 = CARTESIAN_POINT('Ctrl Pts',(-9.74394510030878,-12.4358572257211,
118.389145894146)) ;
#191017 = CARTESIAN_POINT('Ctrl Pts',(-9.67014125555776,-12.435857227174,
118.413376931778)) ;
#191018 = CARTESIAN_POINT('Ctrl Pts',(-9.59633741080671,-12.4358572286269,
118.43760796941)) ;
#191019 = CARTESIAN_POINT('Ctrl Pts',(-9.59076805718501,-12.3620878063136,
118.420644616978)) ;
#191020 = CARTESIAN_POINT('Ctrl Pts',(-9.58519870356327,-12.2883183840004,
118.403681264546)) ;
#191021 = CARTESIAN_POINT('Ctrl Pts',(-9.65900254831429,-12.2883183825475,
118.379450226914)) ;
#191022 = CARTESIAN_POINT('Ctrl Pts',(-9.73280639306531,-12.2883183810946,
118.355219189282)) ;
#191023 = CARTESIAN_POINT('Ctrl Pts',(-9.73837574668705,-12.3620878034078,
118.372182541714)) ;
#191024 = CARTESIAN_POINT('Ctrl Pts',(-9.64331761099955,-12.4693107333451,
118.118151143645)) ;
#191025 = CARTESIAN_POINT('Ctrl Pts',(-9.65479830623516,-12.5357038324563,
118.153119488932)) ;
#191026 = CARTESIAN_POINT('Ctrl Pts',(-9.58099446292707,-12.5357038327128,
118.177350530959)) ;
#191027 = CARTESIAN_POINT('Ctrl Pts',(-9.50719061961899,-12.5357038329694,
118.201581572986)) ;
#191028 = CARTESIAN_POINT('Ctrl Pts',(-9.49570992438338,-12.4693107338582,
118.166613227698)) ;
#191029 = CARTESIAN_POINT('Ctrl Pts',(-9.48422922914777,-12.402917634747,
118.131644882411)) ;
#191030 = CARTESIAN_POINT('Ctrl Pts',(-9.55803307245587,-12.4029176344904,
118.107413840384)) ;
#191031 = CARTESIAN_POINT('Ctrl Pts',(-9.63183691576394,-12.4029176342339,
118.083182798358)) ;
#191032 = CARTESIAN_POINT('Ctrl Pts',(-9.64331761099955,-12.4693107333451,
118.118151143645)) ;
#191033 = CARTESIAN_POINT('Ctrl Pts',(-9.56006119087889,-12.645191135036,
117.900125999057)) ;
#191034 = CARTESIAN_POINT('Ctrl Pts',(-9.57663687909926,-12.6994019736038,
117.950612870956)) ;
#191035 = CARTESIAN_POINT('Ctrl Pts',(-9.50283303638179,-12.6994019715653,
117.974843914782)) ;
#191036 = CARTESIAN_POINT('Ctrl Pts',(-9.42902919366433,-12.6994019695268,
117.999074958608)) ;
#191037 = CARTESIAN_POINT('Ctrl Pts',(-9.41245350544398,-12.6451911309591,
117.948588086708)) ;
#191038 = CARTESIAN_POINT('Ctrl Pts',(-9.39587781722363,-12.5909802923914,
117.898101214808)) ;
#191039 = CARTESIAN_POINT('Ctrl Pts',(-9.46968165994109,-12.5909802944298,
117.873870170982)) ;
#191040 = CARTESIAN_POINT('Ctrl Pts',(-9.54348550265856,-12.5909802964683,
117.849639127157)) ;
#191041 = CARTESIAN_POINT('Ctrl Pts',(-9.56006119087889,-12.645191135036,
117.900125999057)) ;
#191042 = CARTESIAN_POINT('Ctrl Pts',(-9.49421241414551,-12.8761323945115,
117.735033267654)) ;
#191043 = CARTESIAN_POINT('Ctrl Pts',(-9.51467678263965,-12.9142969383445,
117.797364432234)) ;
#191044 = CARTESIAN_POINT('Ctrl Pts',(-9.44087293971269,-12.9142969355883,
117.821595475422)) ;
#191045 = CARTESIAN_POINT('Ctrl Pts',(-9.3670690967857,-12.9142969328321,
117.84582651861)) ;
#191046 = CARTESIAN_POINT('Ctrl Pts',(-9.34660472829156,-12.8761323889991,
117.783495354029)) ;
#191047 = CARTESIAN_POINT('Ctrl Pts',(-9.32614035979739,-12.8379678451661,
117.721164189449)) ;
#191048 = CARTESIAN_POINT('Ctrl Pts',(-9.39994420272437,-12.8379678479223,
117.696933146261)) ;
#191049 = CARTESIAN_POINT('Ctrl Pts',(-9.47374804565133,-12.8379678506785,
117.672702103074)) ;
#191050 = CARTESIAN_POINT('Ctrl Pts',(-9.49421241414551,-12.8761323945115,
117.735033267654)) ;
#191051 = CARTESIAN_POINT('Ctrl Pts',(-9.44952047826331,-13.1443073603244,
117.634195686389)) ;
#191052 = CARTESIAN_POINT('Ctrl Pts',(-9.47240530569183,-13.1638021990363,
117.703899178321)) ;
#191053 = CARTESIAN_POINT('Ctrl Pts',(-9.39860146235271,-13.16380219707,117.728130220253)) ;
#191054 = CARTESIAN_POINT('Ctrl Pts',(-9.32479761901359,-13.1638021951038,
117.752361262185)) ;
#191055 = CARTESIAN_POINT('Ctrl Pts',(-9.30191279158505,-13.1443073563919,
117.682657770253)) ;
#191056 = CARTESIAN_POINT('Ctrl Pts',(-9.27902796415653,-13.12481251768,117.612954278321)) ;
#191057 = CARTESIAN_POINT('Ctrl Pts',(-9.35283180749566,-13.1248125196462,
117.588723236389)) ;
#191058 = CARTESIAN_POINT('Ctrl Pts',(-9.42663565083478,-13.1248125216125,
117.564492194457)) ;
#191059 = CARTESIAN_POINT('Ctrl Pts',(-9.44952047826331,-13.1443073603244,
117.634195686389)) ;
#191060 = CARTESIAN_POINT('Ctrl Pts',(-9.42806301659363,-13.4354170804365,
117.604552144975)) ;
#191061 = CARTESIAN_POINT('Ctrl Pts',(-9.45174090939818,-13.4346128293488,
117.676671185992)) ;
#191062 = CARTESIAN_POINT('Ctrl Pts',(-9.37793706587032,-13.4346128319822,
117.70090222735)) ;
#191063 = CARTESIAN_POINT('Ctrl Pts',(-9.30413322234245,-13.4346128346157,
117.725133268707)) ;
#191064 = CARTESIAN_POINT('Ctrl Pts',(-9.28045532953792,-13.4354170857033,
117.653014227689)) ;
#191065 = CARTESIAN_POINT('Ctrl Pts',(-9.25677743673337,-13.436221336791,
117.580895186672)) ;
#191066 = CARTESIAN_POINT('Ctrl Pts',(-9.33058128026124,-13.4362213341576,
117.556664145314)) ;
#191067 = CARTESIAN_POINT('Ctrl Pts',(-9.40438512378909,-13.4362213315242,
117.532433103957)) ;
#191068 = CARTESIAN_POINT('Ctrl Pts',(-9.42806301659363,-13.4354170804365,
117.604552144975)) ;
#191069 = CARTESIAN_POINT('Ctrl Pts',(-9.43113345781473,-13.7221366616439,
117.649216366819)) ;
#191070 = CARTESIAN_POINT('Ctrl Pts',(-9.45390061019574,-13.7013113003572,
117.718561439368)) ;
#191071 = CARTESIAN_POINT('Ctrl Pts',(-9.38009676726755,-13.7013113073341,
117.742792482551)) ;
#191072 = CARTESIAN_POINT('Ctrl Pts',(-9.30629292433936,-13.7013113143109,
117.767023525735)) ;
#191073 = CARTESIAN_POINT('Ctrl Pts',(-9.28352577195833,-13.7221366755976,
117.697678453187)) ;
#191074 = CARTESIAN_POINT('Ctrl Pts',(-9.26075861957731,-13.7429620368844,
117.628333380638)) ;
#191075 = CARTESIAN_POINT('Ctrl Pts',(-9.3345624625055,-13.7429620299075,
117.604102337454)) ;
#191076 = CARTESIAN_POINT('Ctrl Pts',(-9.4083663054337,-13.7429620229307,
117.57987129427)) ;
#191077 = CARTESIAN_POINT('Ctrl Pts',(-9.43113345781473,-13.7221366616439,
117.649216366819)) ;
#191078 = CARTESIAN_POINT('Ctrl Pts',(-9.45742319346762,-13.9882040306806,
117.764746473513)) ;
#191079 = CARTESIAN_POINT('Ctrl Pts',(-9.47765409992438,-13.948770536174,
117.826366550077)) ;
#191080 = CARTESIAN_POINT('Ctrl Pts',(-9.40385025854739,-13.9487705477941,
117.850597597986)) ;
#191081 = CARTESIAN_POINT('Ctrl Pts',(-9.33004641717041,-13.9487705594142,
117.874828645894)) ;
#191082 = CARTESIAN_POINT('Ctrl Pts',(-9.30981551071365,-13.9882040539209,
117.81320856933)) ;
#191083 = CARTESIAN_POINT('Ctrl Pts',(-9.28958460425689,-14.0276375484275,
117.751588492765)) ;
#191084 = CARTESIAN_POINT('Ctrl Pts',(-9.36338844563387,-14.0276375368073,
117.727357444856)) ;
#191085 = CARTESIAN_POINT('Ctrl Pts',(-9.43719228701085,-14.0276375251872,
117.703126396948)) ;
#191086 = CARTESIAN_POINT('Ctrl Pts',(-9.45742319346762,-13.9882040306806,
117.764746473513)) ;
#191087 = CARTESIAN_POINT('Ctrl Pts',(-9.50431469901294,-14.2132831582582,
117.942967310221)) ;
#191088 = CARTESIAN_POINT('Ctrl Pts',(-9.52056835396493,-14.1580769970448,
117.9924733203)) ;
#191089 = CARTESIAN_POINT('Ctrl Pts',(-9.44676451495778,-14.1580770113055,
118.016704375426)) ;
#191090 = CARTESIAN_POINT('Ctrl Pts',(-9.37296067595063,-14.1580770255661,
118.040935430553)) ;
#191091 = CARTESIAN_POINT('Ctrl Pts',(-9.35670702099861,-14.2132831867795,
117.991429420474)) ;
#191092 = CARTESIAN_POINT('Ctrl Pts',(-9.34045336604661,-14.2684893479928,
117.941923410395)) ;
#191093 = CARTESIAN_POINT('Ctrl Pts',(-9.41425720505376,-14.2684893337322,
117.917692355268)) ;
#191094 = CARTESIAN_POINT('Ctrl Pts',(-9.48806104406092,-14.2684893194715,
117.893461300141)) ;
#191095 = CARTESIAN_POINT('Ctrl Pts',(-9.50431469901294,-14.2132831582582,
117.942967310221)) ;
#191096 = CARTESIAN_POINT('Ctrl Pts',(-9.56833785438296,-14.3825130038358,
118.17365809311)) ;
#191097 = CARTESIAN_POINT('Ctrl Pts',(-9.57940645753599,-14.3154103550948,
118.20737127182)) ;
#191098 = CARTESIAN_POINT('Ctrl Pts',(-9.50560262233898,-14.3154103696642,
118.231602338552)) ;
#191099 = CARTESIAN_POINT('Ctrl Pts',(-9.43179878714198,-14.3154103842335,
118.255833405283)) ;
#191100 = CARTESIAN_POINT('Ctrl Pts',(-9.42073018398896,-14.3825130329745,
118.222120226574)) ;
#191101 = CARTESIAN_POINT('Ctrl Pts',(-9.40966158083592,-14.4496156817154,
118.188407047864)) ;
#191102 = CARTESIAN_POINT('Ctrl Pts',(-9.48346541603292,-14.4496156671461,
118.164175981132)) ;
#191103 = CARTESIAN_POINT('Ctrl Pts',(-9.55726925122993,-14.4496156525767,
118.1399449144)) ;
#191104 = CARTESIAN_POINT('Ctrl Pts',(-9.56833785438296,-14.3825130038358,
118.17365809311)) ;
#191105 = CARTESIAN_POINT('Ctrl Pts',(-9.64282625620299,-14.4810713491466,
118.435803129355)) ;
#191106 = CARTESIAN_POINT('Ctrl Pts',(-9.64798025335909,-14.4069908889082,
118.451501372389)) ;
#191107 = CARTESIAN_POINT('Ctrl Pts',(-9.57417642109813,-14.4069908973545,
118.475732448064)) ;
#191108 = CARTESIAN_POINT('Ctrl Pts',(-9.50037258883717,-14.4069909058008,
118.499963523738)) ;
#191109 = CARTESIAN_POINT('Ctrl Pts',(-9.49521859168107,-14.4810713660392,
118.484265280704)) ;
#191110 = CARTESIAN_POINT('Ctrl Pts',(-9.49006459452497,-14.5551518262776,
118.468567037671)) ;
#191111 = CARTESIAN_POINT('Ctrl Pts',(-9.56386842678596,-14.5551518178313,
118.444335961996)) ;
#191112 = CARTESIAN_POINT('Ctrl Pts',(-9.6376722590469,-14.555151809385,118.420104886322)) ;
#191113 = CARTESIAN_POINT('Ctrl Pts',(-9.64282625620299,-14.4810713491466,
118.435803129355)) ;
#191114 = CARTESIAN_POINT('Ctrl Pts',(-9.72303088811142,-14.5044054817918,
118.715641377644)) ;
#191115 = CARTESIAN_POINT('Ctrl Pts',(-9.72185690535189,-14.4285885279282,
118.712065614687)) ;
#191116 = CARTESIAN_POINT('Ctrl Pts',(-9.64805307633812,-14.4285885262166,
118.736296700252)) ;
#191117 = CARTESIAN_POINT('Ctrl Pts',(-9.57424924732434,-14.4285885245051,
118.760527785817)) ;
#191118 = CARTESIAN_POINT('Ctrl Pts',(-9.57542323008388,-14.5044054783686,
118.764103548774)) ;
#191119 = CARTESIAN_POINT('Ctrl Pts',(-9.57659721284341,-14.5802224322322,
118.767679311731)) ;
#191120 = CARTESIAN_POINT('Ctrl Pts',(-9.65040104185718,-14.5802224339438,
118.743448226166)) ;
#191121 = CARTESIAN_POINT('Ctrl Pts',(-9.72420487087096,-14.5802224356554,
118.719217140601)) ;
#191122 = CARTESIAN_POINT('Ctrl Pts',(-9.72303088811142,-14.5044054817918,
118.715641377644)) ;
#191123 = CARTESIAN_POINT('Ctrl Pts',(-9.80169380240826,-14.4496129795719,
118.990681507836)) ;
#191124 = CARTESIAN_POINT('Ctrl Pts',(-9.79429250812283,-14.377512086332,
118.96813835858)) ;
#191125 = CARTESIAN_POINT('Ctrl Pts',(-9.72048868096979,-14.3775120696296,
118.992369449812)) ;
#191126 = CARTESIAN_POINT('Ctrl Pts',(-9.64668485381674,-14.3775120529272,
119.016600541045)) ;
#191127 = CARTESIAN_POINT('Ctrl Pts',(-9.65408614810217,-14.449612946167,
119.039143690301)) ;
#191128 = CARTESIAN_POINT('Ctrl Pts',(-9.66148744238758,-14.5217138394069,
119.061686839557)) ;
#191129 = CARTESIAN_POINT('Ctrl Pts',(-9.73529126954064,-14.5217138561093,
119.037455748325)) ;
#191130 = CARTESIAN_POINT('Ctrl Pts',(-9.80909509669367,-14.5217138728117,
119.013224657093)) ;
#191131 = CARTESIAN_POINT('Ctrl Pts',(-9.80169380240826,-14.4496129795719,
118.990681507836)) ;
#191132 = CARTESIAN_POINT('Ctrl Pts',(-9.87269202902114,-14.3209948065222,
119.242404449809)) ;
#191133 = CARTESIAN_POINT('Ctrl Pts',(-9.85958903526633,-14.2577695417982,
119.202494843768)) ;
#191134 = CARTESIAN_POINT('Ctrl Pts',(-9.78578520837554,-14.257769507085,
119.226725935799)) ;
#191135 = CARTESIAN_POINT('Ctrl Pts',(-9.71198138148474,-14.2577694723718,
119.25095702783)) ;
#191136 = CARTESIAN_POINT('Ctrl Pts',(-9.72508437523955,-14.3209947370958,
119.290866633871)) ;
#191137 = CARTESIAN_POINT('Ctrl Pts',(-9.73818736899434,-14.3842200018198,
119.330776239912)) ;
#191138 = CARTESIAN_POINT('Ctrl Pts',(-9.81199119588514,-14.384220036533,
119.306545147881)) ;
#191139 = CARTESIAN_POINT('Ctrl Pts',(-9.88579502277594,-14.3842200712462,
119.28231405585)) ;
#191140 = CARTESIAN_POINT('Ctrl Pts',(-9.87269202902114,-14.3209948065222,
119.242404449809)) ;
#191141 = CARTESIAN_POINT('Ctrl Pts',(-9.93011353231494,-14.1276267553148,
119.452772844541)) ;
#191142 = CARTESIAN_POINT('Ctrl Pts',(-9.91224855578811,-14.0778104825488,
119.398359007162)) ;
#191143 = CARTESIAN_POINT('Ctrl Pts',(-9.83844472708885,-14.077810428769,
119.422590093684)) ;
#191144 = CARTESIAN_POINT('Ctrl Pts',(-9.7646408983896,-14.0778103749893,
119.446821180207)) ;
#191145 = CARTESIAN_POINT('Ctrl Pts',(-9.78250587491643,-14.1276266477552,
119.501235017587)) ;
#191146 = CARTESIAN_POINT('Ctrl Pts',(-9.80037085144328,-14.1774429205212,
119.555648854967)) ;
#191147 = CARTESIAN_POINT('Ctrl Pts',(-9.87417468014253,-14.177442974301,
119.531417768444)) ;
#191148 = CARTESIAN_POINT('Ctrl Pts',(-9.94797850884177,-14.1774430280807,
119.507186681921)) ;
#191149 = CARTESIAN_POINT('Ctrl Pts',(-9.93011353231494,-14.1276267553148,
119.452772844541)) ;
#191150 = CARTESIAN_POINT('Ctrl Pts',(-9.96912456086633,-13.88341485216,119.607067761314)) ;
#191151 = CARTESIAN_POINT('Ctrl Pts',(-9.94777603635157,-13.8505765249219,
119.542043598682)) ;
#191152 = CARTESIAN_POINT('Ctrl Pts',(-9.8739722037022,-13.8505764535514,
119.566274673173)) ;
#191153 = CARTESIAN_POINT('Ctrl Pts',(-9.80016837105283,-13.850576382181,
119.590505747665)) ;
#191154 = CARTESIAN_POINT('Ctrl Pts',(-9.82151689556758,-13.8834147094192,
119.655529910297)) ;
#191155 = CARTESIAN_POINT('Ctrl Pts',(-9.84286542008233,-13.9162530366573,
119.720554072928)) ;
#191156 = CARTESIAN_POINT('Ctrl Pts',(-9.9166692527317,-13.9162531080278,
119.696322998437)) ;
#191157 = CARTESIAN_POINT('Ctrl Pts',(-9.99047308538107,-13.9162531793982,
119.672091923946)) ;
#191158 = CARTESIAN_POINT('Ctrl Pts',(-9.96912456086633,-13.88341485216,119.607067761314)) ;
#191159 = CARTESIAN_POINT('Ctrl Pts',(-9.98608738662717,-13.605636693064,
119.694232674666)) ;
#191160 = CARTESIAN_POINT('Ctrl Pts',(-9.96278900243976,-13.5921442428259,
119.623269553942)) ;
#191161 = CARTESIAN_POINT('Ctrl Pts',(-9.88898516382017,-13.5921441578331,
119.647500610249)) ;
#191162 = CARTESIAN_POINT('Ctrl Pts',(-9.81518132520059,-13.5921440728403,
119.671731666556)) ;
#191163 = CARTESIAN_POINT('Ctrl Pts',(-9.83847970938801,-13.6056365230784,
119.74269478728)) ;
#191164 = CARTESIAN_POINT('Ctrl Pts',(-9.86177809357544,-13.6191289733166,
119.813657908004)) ;
#191165 = CARTESIAN_POINT('Ctrl Pts',(-9.93558193219503,-13.6191290583094,
119.789426851697)) ;
#191166 = CARTESIAN_POINT('Ctrl Pts',(-10.0093857708146,-13.6191291433021,
119.76519579539)) ;
#191167 = CARTESIAN_POINT('Ctrl Pts',(-9.98608738662717,-13.605636693064,
119.694232674666)) ;
#191168 = CARTESIAN_POINT('Ctrl Pts',(-9.97927918663981,-13.3159385103922,
119.708801041575)) ;
#191169 = CARTESIAN_POINT('Ctrl Pts',(-9.95569186707513,-13.3226522577716,
119.636957870211)) ;
#191170 = CARTESIAN_POINT('Ctrl Pts',(-9.88188802115178,-13.3226521665054,
119.661188904272)) ;
#191171 = CARTESIAN_POINT('Ctrl Pts',(-9.80808417522844,-13.3226520752392,
119.685419938333)) ;
#191172 = CARTESIAN_POINT('Ctrl Pts',(-9.83167149479313,-13.3159383278597,
119.757263109697)) ;
#191173 = CARTESIAN_POINT('Ctrl Pts',(-9.85525881435782,-13.3092245804803,
119.829106281061)) ;
#191174 = CARTESIAN_POINT('Ctrl Pts',(-9.92906266028116,-13.3092246717465,
119.804875247)) ;
#191175 = CARTESIAN_POINT('Ctrl Pts',(-10.0028665062045,-13.3092247630127,
119.780644212939)) ;
#191176 = CARTESIAN_POINT('Ctrl Pts',(-9.97927918663981,-13.3159385103922,
119.708801041575)) ;
#191177 = CARTESIAN_POINT('Ctrl Pts',(-9.947822664236,-13.0300093756574,119.6487613202)) ;
#191178 = CARTESIAN_POINT('Ctrl Pts',(-9.92565661232397,-13.0566953178852,
119.581247100649)) ;
#191179 = CARTESIAN_POINT('Ctrl Pts',(-9.85185275806088,-13.0566952256386,
119.605478109308)) ;
#191180 = CARTESIAN_POINT('Ctrl Pts',(-9.7780489037978,-13.0566951333921,
119.629709117968)) ;
#191181 = CARTESIAN_POINT('Ctrl Pts',(-9.80021495570981,-13.0300091911643,
119.697223337518)) ;
#191182 = CARTESIAN_POINT('Ctrl Pts',(-9.82238100762185,-13.0033232489365,
119.764737557069)) ;
#191183 = CARTESIAN_POINT('Ctrl Pts',(-9.89618486188495,-13.003323341183,
119.74050654841)) ;
#191184 = CARTESIAN_POINT('Ctrl Pts',(-9.96998871614802,-13.0033234334296,
119.71627553975)) ;
#191185 = CARTESIAN_POINT('Ctrl Pts',(-9.947822664236,-13.0300093756574,119.6487613202)) ;
#191186 = CARTESIAN_POINT('Ctrl Pts',(-9.8944105320407,-12.7764992730081,
119.521214509144)) ;
#191187 = CARTESIAN_POINT('Ctrl Pts',(-9.87521436237714,-12.820923286975,
119.462746071682)) ;
#191188 = CARTESIAN_POINT('Ctrl Pts',(-9.80141050039616,-12.8209232050731,
119.486977056834)) ;
#191189 = CARTESIAN_POINT('Ctrl Pts',(-9.72760663841516,-12.8209231231712,
119.511208041986)) ;
#191190 = CARTESIAN_POINT('Ctrl Pts',(-9.74680280807871,-12.7764991092043,
119.569676479447)) ;
#191191 = CARTESIAN_POINT('Ctrl Pts',(-9.76599897774222,-12.7320750952375,
119.628144916909)) ;
#191192 = CARTESIAN_POINT('Ctrl Pts',(-9.83980283972324,-12.7320751771394,
119.603913931757)) ;
#191193 = CARTESIAN_POINT('Ctrl Pts',(-9.91360670170422,-12.7320752590413,
119.579682946605)) ;
#191194 = CARTESIAN_POINT('Ctrl Pts',(-9.8944105320407,-12.7764992730081,
119.521214509144)) ;
#191195 = CARTESIAN_POINT('Ctrl Pts',(-9.82070657807217,-12.5655360581605,
119.33234328729)) ;
#191196 = CARTESIAN_POINT('Ctrl Pts',(-9.80589079521809,-12.6247539701097,
119.2872168012)) ;
#191197 = CARTESIAN_POINT('Ctrl Pts',(-9.73208692613494,-12.6247539044987,
119.31144776472)) ;
#191198 = CARTESIAN_POINT('Ctrl Pts',(-9.65828305705181,-12.6247538388877,
119.335678728239)) ;
#191199 = CARTESIAN_POINT('Ctrl Pts',(-9.67309883990591,-12.5655359269385,
119.38080521433)) ;
#191200 = CARTESIAN_POINT('Ctrl Pts',(-9.68791462276,-12.5063180149893,119.42593170042)) ;
#191201 = CARTESIAN_POINT('Ctrl Pts',(-9.76171849184312,-12.5063180806004,
119.4017007369)) ;
#191202 = CARTESIAN_POINT('Ctrl Pts',(-9.83552236092627,-12.5063181462114,
119.37746977338)) ;
#191203 = CARTESIAN_POINT('Ctrl Pts',(-9.82070657807217,-12.5655360581605,
119.33234328729)) ;
#191204 = CARTESIAN_POINT('Ctrl Pts',(-9.73221917304687,-12.4169761529621,
119.098239780795)) ;
#191205 = CARTESIAN_POINT('Ctrl Pts',(-9.72282668729767,-12.4866530449287,
119.069631782602)) ;
#191206 = CARTESIAN_POINT('Ctrl Pts',(-9.649022813112,-12.4866530028469,119.093862730581)) ;
#191207 = CARTESIAN_POINT('Ctrl Pts',(-9.5752189389263,-12.4866529607651,
119.118093678559)) ;
#191208 = CARTESIAN_POINT('Ctrl Pts',(-9.58461142467551,-12.4169760687985,
119.146701676752)) ;
#191209 = CARTESIAN_POINT('Ctrl Pts',(-9.59400391042471,-12.3472991768318,
119.175309674945)) ;
#191210 = CARTESIAN_POINT('Ctrl Pts',(-9.6678077846104,-12.3472992189136,
119.151078726967)) ;
#191211 = CARTESIAN_POINT('Ctrl Pts',(-9.74161165879609,-12.3472992609954,
119.126847778988)) ;
#191212 = CARTESIAN_POINT('Ctrl Pts',(-9.73221917304687,-12.4169761529621,
119.098239780795)) ;
#191213 = CARTESIAN_POINT('Ctrl Pts',(-9.63396562356762,-12.339692635442,
118.834500805048)) ;
#191214 = CARTESIAN_POINT('Ctrl Pts',(-9.63068383128753,-12.4148681964576,
118.824504993183)) ;
#191215 = CARTESIAN_POINT('Ctrl Pts',(-9.55687995436833,-12.4148681820189,
118.848735932836)) ;
#191216 = CARTESIAN_POINT('Ctrl Pts',(-9.48307607744914,-12.4148681675802,
118.872966872488)) ;
#191217 = CARTESIAN_POINT('Ctrl Pts',(-9.48635786972923,-12.3396926065646,
118.882962684353)) ;
#191218 = CARTESIAN_POINT('Ctrl Pts',(-9.48963966200935,-12.264517045549,
118.892958496218)) ;
#191219 = CARTESIAN_POINT('Ctrl Pts',(-9.56344353892853,-12.2645170599877,
118.868727556566)) ;
#191220 = CARTESIAN_POINT('Ctrl Pts',(-9.63724741584773,-12.2645170744263,
118.844496616913)) ;
#191221 = CARTESIAN_POINT('Ctrl Pts',(-9.63396562356762,-12.339692635442,
118.834500805048)) ;
#191222 = CARTESIAN_POINT('Ctrl Pts',(-9.53271625870816,-12.3399218128255,
118.561543074817)) ;
#191223 = CARTESIAN_POINT('Ctrl Pts',(-9.53576535287959,-12.4151926619622,
118.570830121603)) ;
#191224 = CARTESIAN_POINT('Ctrl Pts',(-9.46196147602193,-12.4151926765907,
118.595061061442)) ;
#191225 = CARTESIAN_POINT('Ctrl Pts',(-9.38815759916426,-12.4151926912192,
118.619292001282)) ;
#191226 = CARTESIAN_POINT('Ctrl Pts',(-9.38510850499285,-12.3399218420826,
118.610004954497)) ;
#191227 = CARTESIAN_POINT('Ctrl Pts',(-9.38205941082139,-12.2646509929459,
118.600717907712)) ;
#191228 = CARTESIAN_POINT('Ctrl Pts',(-9.45586328767907,-12.2646509783174,
118.576486967872)) ;
#191229 = CARTESIAN_POINT('Ctrl Pts',(-9.52966716453673,-12.2646509636889,
118.552256028032)) ;
#191230 = CARTESIAN_POINT('Ctrl Pts',(-9.53271625870816,-12.3399218128255,
118.561543074817)) ;
#191231 = CARTESIAN_POINT('Ctrl Pts',(-9.43473348009199,-12.4170982893213,
118.298531776641)) ;
#191232 = CARTESIAN_POINT('Ctrl Pts',(-9.44389485074115,-12.4870926783877,
118.326435831388)) ;
#191233 = CARTESIAN_POINT('Ctrl Pts',(-9.37009097662917,-12.4870927205449,
118.35066677959)) ;
#191234 = CARTESIAN_POINT('Ctrl Pts',(-9.2962871025172,-12.4870927627021,
118.374897727793)) ;
#191235 = CARTESIAN_POINT('Ctrl Pts',(-9.28712573186802,-12.4170983736357,
118.346993673047)) ;
#191236 = CARTESIAN_POINT('Ctrl Pts',(-9.27796436121887,-12.3471039845693,
118.319089618301)) ;
#191237 = CARTESIAN_POINT('Ctrl Pts',(-9.35176823533084,-12.3471039424121,
118.294858670098)) ;
#191238 = CARTESIAN_POINT('Ctrl Pts',(-9.42557210944283,-12.3471039002549,
118.270627721895)) ;
#191239 = CARTESIAN_POINT('Ctrl Pts',(-9.43473348009199,-12.4170982893213,
118.298531776641)) ;
#191240 = CARTESIAN_POINT('Ctrl Pts',(-9.34612142005041,-12.5661915214183,
118.064123452786)) ;
#191241 = CARTESIAN_POINT('Ctrl Pts',(-9.36074871887772,-12.6258811352282,
118.108675842885)) ;
#191242 = CARTESIAN_POINT('Ctrl Pts',(-9.28694484996586,-12.6258812005672,
118.132906806927)) ;
#191243 = CARTESIAN_POINT('Ctrl Pts',(-9.21314098105396,-12.6258812659061,
118.157137770968)) ;
#191244 = CARTESIAN_POINT('Ctrl Pts',(-9.19851368222664,-12.5661916520963,
118.112585380869)) ;
#191245 = CARTESIAN_POINT('Ctrl Pts',(-9.1838863833993,-12.5065020382865,
118.068032990769)) ;
#191246 = CARTESIAN_POINT('Ctrl Pts',(-9.25769025231121,-12.5065019729475,
118.043802026728)) ;
#191247 = CARTESIAN_POINT('Ctrl Pts',(-9.33149412122307,-12.5065019076085,
118.019571062686)) ;
#191248 = CARTESIAN_POINT('Ctrl Pts',(-9.34612142005041,-12.5661915214183,
118.064123452786)) ;
#191249 = CARTESIAN_POINT('Ctrl Pts',(-9.27272433522268,-12.7760910985915,
117.876015426606)) ;
#191250 = CARTESIAN_POINT('Ctrl Pts',(-9.29176439552139,-12.8212153371298,
117.934008376216)) ;
#191251 = CARTESIAN_POINT('Ctrl Pts',(-9.2179605335698,-12.8212154191497,
117.958239361457)) ;
#191252 = CARTESIAN_POINT('Ctrl Pts',(-9.14415667161822,-12.8212155011696,
117.982470346699)) ;
#191253 = CARTESIAN_POINT('Ctrl Pts',(-9.12511661131953,-12.7760912626314,
117.924477397089)) ;
#191254 = CARTESIAN_POINT('Ctrl Pts',(-9.10607655102083,-12.7309670240931,
117.866484447479)) ;
#191255 = CARTESIAN_POINT('Ctrl Pts',(-9.1798804129724,-12.7309669420732,
117.842253462237)) ;
#191256 = CARTESIAN_POINT('Ctrl Pts',(-9.25368427492398,-12.7309668600532,
117.818022476996)) ;
#191257 = CARTESIAN_POINT('Ctrl Pts',(-9.27272433522268,-12.7760910985915,
117.876015426606)) ;
#191258 = CARTESIAN_POINT('Ctrl Pts',(-9.21878702259048,-13.0327329322163,
117.747284173735)) ;
#191259 = CARTESIAN_POINT('Ctrl Pts',(-9.24088580050292,-13.0600070239695,
117.81459348377)) ;
#191260 = CARTESIAN_POINT('Ctrl Pts',(-9.1670819466148,-13.0600071142797,
117.838824493571)) ;
#191261 = CARTESIAN_POINT('Ctrl Pts',(-9.09327809272665,-13.0600072045899,
117.863055503372)) ;
#191262 = CARTESIAN_POINT('Ctrl Pts',(-9.07117931481421,-13.0327331128366,
117.795746193338)) ;
#191263 = CARTESIAN_POINT('Ctrl Pts',(-9.04908053690176,-13.0054590210833,
117.728436883303)) ;
#191264 = CARTESIAN_POINT('Ctrl Pts',(-9.12288439078989,-13.0054589307732,
117.704205873502)) ;
#191265 = CARTESIAN_POINT('Ctrl Pts',(-9.19668824467802,-13.005458840463,
117.679974863701)) ;
#191266 = CARTESIAN_POINT('Ctrl Pts',(-9.21878702259048,-13.0327329322163,
117.747284173735)) ;
#191267 = CARTESIAN_POINT('Ctrl Pts',(-9.18778602878387,-13.3169814944794,
117.688392704249)) ;
#191268 = CARTESIAN_POINT('Ctrl Pts',(-9.21134730464771,-13.3244510016564,
117.760156547187)) ;
#191269 = CARTESIAN_POINT('Ctrl Pts',(-9.13754345877924,-13.3244510916003,
117.784387581415)) ;
#191270 = CARTESIAN_POINT('Ctrl Pts',(-9.06373961291076,-13.3244511815443,
117.808618615643)) ;
#191271 = CARTESIAN_POINT('Ctrl Pts',(-9.04017833704691,-13.3169816743673,
117.736854772705)) ;
#191272 = CARTESIAN_POINT('Ctrl Pts',(-9.01661706118305,-13.3095121671903,
117.665090929766)) ;
#191273 = CARTESIAN_POINT('Ctrl Pts',(-9.09042090705155,-13.3095120772463,
117.640859895538)) ;
#191274 = CARTESIAN_POINT('Ctrl Pts',(-9.16422475292001,-13.3095119873024,
117.61662886131)) ;
#191275 = CARTESIAN_POINT('Ctrl Pts',(-9.18778602878387,-13.3169814944794,
117.688392704249)) ;
#191276 = CARTESIAN_POINT('Ctrl Pts',(-9.18098202319864,-13.6065319682423,
117.70296148096)) ;
#191277 = CARTESIAN_POINT('Ctrl Pts',(-9.20432341160334,-13.593796615994,
117.774055582276)) ;
#191278 = CARTESIAN_POINT('Ctrl Pts',(-9.13051957298211,-13.5937966997554,
117.798286638578)) ;
#191279 = CARTESIAN_POINT('Ctrl Pts',(-9.05671573436087,-13.5937967835168,
117.82251769488)) ;
#191280 = CARTESIAN_POINT('Ctrl Pts',(-9.03337434595617,-13.6065321357651,
117.751423593564)) ;
#191281 = CARTESIAN_POINT('Ctrl Pts',(-9.01003295755148,-13.6192674880133,
117.680329492249)) ;
#191282 = CARTESIAN_POINT('Ctrl Pts',(-9.08383679617271,-13.6192674042519,
117.656098435947)) ;
#191283 = CARTESIAN_POINT('Ctrl Pts',(-9.15764063479395,-13.6192673204905,
117.631867379645)) ;
#191284 = CARTESIAN_POINT('Ctrl Pts',(-9.18098202319864,-13.6065319682423,
117.70296148096)) ;
#191285 = CARTESIAN_POINT('Ctrl Pts',(-9.19808875904426,-13.8845186470045,
117.790606361168)) ;
#191286 = CARTESIAN_POINT('Ctrl Pts',(-9.21953568780673,-13.8523553116745,
117.855930244232)) ;
#191287 = CARTESIAN_POINT('Ctrl Pts',(-9.14573185495254,-13.852355381399,
117.880161318099)) ;
#191288 = CARTESIAN_POINT('Ctrl Pts',(-9.07192802209835,-13.8523554511235,
117.904392391967)) ;
#191289 = CARTESIAN_POINT('Ctrl Pts',(-9.0504810933359,-13.8845187864536,
117.839068508903)) ;
#191290 = CARTESIAN_POINT('Ctrl Pts',(-9.02903416457341,-13.9166821217837,
117.773744625839)) ;
#191291 = CARTESIAN_POINT('Ctrl Pts',(-9.10283799742762,-13.9166820520591,
117.749513551972)) ;
#191292 = CARTESIAN_POINT('Ctrl Pts',(-9.17664183028178,-13.9166819823346,
117.725282478104)) ;
#191293 = CARTESIAN_POINT('Ctrl Pts',(-9.19808875904426,-13.8845186470045,
117.790606361168)) ;
#191294 = CARTESIAN_POINT('Ctrl Pts',(-9.23700591797465,-14.1277890814299,
117.944490651807)) ;
#191295 = CARTESIAN_POINT('Ctrl Pts',(-9.25503655471375,-14.0785921493268,
117.999409060714)) ;
#191296 = CARTESIAN_POINT('Ctrl Pts',(-9.1812327258708,-14.0785922024829,
118.0236401468)) ;
#191297 = CARTESIAN_POINT('Ctrl Pts',(-9.10742889702784,-14.0785922556391,
118.047871232885)) ;
#191298 = CARTESIAN_POINT('Ctrl Pts',(-9.08939826028874,-14.1277891877422,
117.992952823977)) ;
#191299 = CARTESIAN_POINT('Ctrl Pts',(-9.07136762354965,-14.1769861198453,
117.93803441507)) ;
#191300 = CARTESIAN_POINT('Ctrl Pts',(-9.14517145239261,-14.1769860666892,
117.913803328985)) ;
#191301 = CARTESIAN_POINT('Ctrl Pts',(-9.21897528123558,-14.1769860135331,
117.8895722429)) ;
#191302 = CARTESIAN_POINT('Ctrl Pts',(-9.23700591797465,-14.1277890814299,
117.944490651807)) ;
#191303 = CARTESIAN_POINT('Ctrl Pts',(-9.29456875476075,-14.3214999944636,
118.155368644358)) ;
#191304 = CARTESIAN_POINT('Ctrl Pts',(-9.30787208960374,-14.2587034430882,
118.195888454611)) ;
#191305 = CARTESIAN_POINT('Ctrl Pts',(-9.23406826234362,-14.2587034768352,
118.220119545517)) ;
#191306 = CARTESIAN_POINT('Ctrl Pts',(-9.16026443508352,-14.2587035105822,
118.244350636423)) ;
#191307 = CARTESIAN_POINT('Ctrl Pts',(-9.14696110024054,-14.3215000619577,
118.203830826171)) ;
#191308 = CARTESIAN_POINT('Ctrl Pts',(-9.13365776539753,-14.3842966133332,
118.163311015918)) ;
#191309 = CARTESIAN_POINT('Ctrl Pts',(-9.20746159265764,-14.3842965795861,
118.139079925012)) ;
#191310 = CARTESIAN_POINT('Ctrl Pts',(-9.28126541991776,-14.3842965458391,
118.114848834105)) ;
#191311 = CARTESIAN_POINT('Ctrl Pts',(-9.29456875476075,-14.3214999944636,
118.155368644358)) ;
#191312 = CARTESIAN_POINT('Ctrl Pts',(-9.36558798569984,-14.4499114443817,
118.40714452843)) ;
#191313 = CARTESIAN_POINT('Ctrl Pts',(-9.37321903855488,-14.3780538242765,
118.430387483132)) ;
#191314 = CARTESIAN_POINT('Ctrl Pts',(-9.29941521096486,-14.37805384036,118.454618573033)) ;
#191315 = CARTESIAN_POINT('Ctrl Pts',(-9.22561138337483,-14.3780538564435,
118.478849662934)) ;
#191316 = CARTESIAN_POINT('Ctrl Pts',(-9.2179803305198,-14.4499114765488,
118.455606708232)) ;
#191317 = CARTESIAN_POINT('Ctrl Pts',(-9.21034927766476,-14.521769096654,
118.43236375353)) ;
#191318 = CARTESIAN_POINT('Ctrl Pts',(-9.28415310525479,-14.5217690805705,
118.408132663629)) ;
#191319 = CARTESIAN_POINT('Ctrl Pts',(-9.3579569328448,-14.521769064487,118.383901573727)) ;
#191320 = CARTESIAN_POINT('Ctrl Pts',(-9.36558798569984,-14.4499114443817,
118.40714452843)) ;
#191321 = CARTESIAN_POINT('Ctrl Pts',(-9.44439581983412,-14.5043711676863,
118.682688731011)) ;
#191322 = CARTESIAN_POINT('Ctrl Pts',(-9.44580117430657,-14.4286019200682,
118.686969213129)) ;
#191323 = CARTESIAN_POINT('Ctrl Pts',(-9.37199734464163,-14.4286019216996,
118.71120029671)) ;
#191324 = CARTESIAN_POINT('Ctrl Pts',(-9.29819351497668,-14.4286019233309,
118.735431380292)) ;
#191325 = CARTESIAN_POINT('Ctrl Pts',(-9.29678816050424,-14.504371170949,
118.731150898174)) ;
#191326 = CARTESIAN_POINT('Ctrl Pts',(-9.29538280603177,-14.5801404185671,
118.726870416056)) ;
#191327 = CARTESIAN_POINT('Ctrl Pts',(-9.36918663569673,-14.5801404169357,
118.702639332474)) ;
#191328 = CARTESIAN_POINT('Ctrl Pts',(-9.44299046536166,-14.5801404153043,
118.678408248893)) ;
#191329 = CARTESIAN_POINT('Ctrl Pts',(-9.44439581983412,-14.5043711676863,
118.682688731011)) ;
#191330 = CARTESIAN_POINT('Ctrl Pts',(-9.5241527941287,-14.481209763182,118.960955450656)) ;
#191331 = CARTESIAN_POINT('Ctrl Pts',(-9.51926017308425,-14.4069431255803,
118.946053315668)) ;
#191332 = CARTESIAN_POINT('Ctrl Pts',(-9.44545634078204,-14.4069431170847,
118.970284391217)) ;
#191333 = CARTESIAN_POINT('Ctrl Pts',(-9.37165250847984,-14.4069431085892,
118.994515466766)) ;
#191334 = CARTESIAN_POINT('Ctrl Pts',(-9.37654512952428,-14.4812097461908,
119.009417601753)) ;
#191335 = CARTESIAN_POINT('Ctrl Pts',(-9.38143775056871,-14.5554763837924,
119.024319736741)) ;
#191336 = CARTESIAN_POINT('Ctrl Pts',(-9.45524158287093,-14.555476392288,
119.000088661192)) ;
#191337 = CARTESIAN_POINT('Ctrl Pts',(-9.52904541517314,-14.5554764007836,
118.975857585643)) ;
#191338 = CARTESIAN_POINT('Ctrl Pts',(-9.5241527941287,-14.481209763182,118.960955450656)) ;
#191339 = CARTESIAN_POINT('Ctrl Pts',(-9.59915417164219,-14.3816923411007,
119.22493046164)) ;
#191340 = CARTESIAN_POINT('Ctrl Pts',(-9.58828196244955,-14.3142615616255,
119.191815466132)) ;
#191341 = CARTESIAN_POINT('Ctrl Pts',(-9.51447812654902,-14.3142615481585,
119.216046530721)) ;
#191342 = CARTESIAN_POINT('Ctrl Pts',(-9.44067429064847,-14.3142615346915,
119.240277595309)) ;
#191343 = CARTESIAN_POINT('Ctrl Pts',(-9.45154649984112,-14.3816923141668,
119.273392590818)) ;
#191344 = CARTESIAN_POINT('Ctrl Pts',(-9.46241870903376,-14.449123093642,
119.306507586327)) ;
#191345 = CARTESIAN_POINT('Ctrl Pts',(-9.5362225449343,-14.449123107109,119.282276521738)) ;
#191346 = CARTESIAN_POINT('Ctrl Pts',(-9.61002638083482,-14.4491231205759,
119.258045457149)) ;
#191347 = CARTESIAN_POINT('Ctrl Pts',(-9.59915417164219,-14.3816923411007,
119.22493046164)) ;
#191348 = CARTESIAN_POINT('Ctrl Pts',(-9.66271309070694,-14.2134896291755,
119.453949550053)) ;
#191349 = CARTESIAN_POINT('Ctrl Pts',(-9.64665334575257,-14.1577013578714,
119.405034157769)) ;
#191350 = CARTESIAN_POINT('Ctrl Pts',(-9.57284950669676,-14.1577013437741,
119.429265212747)) ;
#191351 = CARTESIAN_POINT('Ctrl Pts',(-9.49904566764095,-14.1577013296769,
119.453496267726)) ;
#191352 = CARTESIAN_POINT('Ctrl Pts',(-9.51510541259531,-14.2134896009809,
119.50241166001)) ;
#191353 = CARTESIAN_POINT('Ctrl Pts',(-9.53116515754968,-14.269277872285,
119.551327052294)) ;
#191354 = CARTESIAN_POINT('Ctrl Pts',(-9.60496899660549,-14.2692778863823,
119.527095997316)) ;
#191355 = CARTESIAN_POINT('Ctrl Pts',(-9.6787728356613,-14.2692779004795,
119.502864942338)) ;
#191356 = CARTESIAN_POINT('Ctrl Pts',(-9.66271309070694,-14.2134896291755,
119.453949550053)) ;
#191357 = CARTESIAN_POINT('Ctrl Pts',(-9.70990503125504,-13.9864989351748,
119.633376033993)) ;
#191358 = CARTESIAN_POINT('Ctrl Pts',(-9.68978709639809,-13.9464758835493,
119.572100050222)) ;
#191359 = CARTESIAN_POINT('Ctrl Pts',(-9.61598325463275,-13.9464758738248,
119.596331096948)) ;
#191360 = CARTESIAN_POINT('Ctrl Pts',(-9.54217941286741,-13.9464758641003,
119.620562143673)) ;
#191361 = CARTESIAN_POINT('Ctrl Pts',(-9.56229734772436,-13.9864989157259,
119.681838127444)) ;
#191362 = CARTESIAN_POINT('Ctrl Pts',(-9.5824152825813,-14.0265219673515,
119.743114111215)) ;
#191363 = CARTESIAN_POINT('Ctrl Pts',(-9.65621912434665,-14.0265219770759,
119.718883064489)) ;
#191364 = CARTESIAN_POINT('Ctrl Pts',(-9.73002296611199,-14.0265219868004,
119.694652017763)) ;
#191365 = CARTESIAN_POINT('Ctrl Pts',(-9.70990503125504,-13.9864989351748,
119.633376033993)) ;
#191366 = CARTESIAN_POINT('Ctrl Pts',(-9.73598202444326,-13.7220237261921,
119.748017635008)) ;
#191367 = CARTESIAN_POINT('Ctrl Pts',(-9.71328442430442,-13.7004075787871,
119.678884407102)) ;
#191368 = CARTESIAN_POINT('Ctrl Pts',(-9.6394805813284,-13.7004075723778,
119.70311545014)) ;
#191369 = CARTESIAN_POINT('Ctrl Pts',(-9.5656767383524,-13.7004075659685,
119.727346493179)) ;
#191370 = CARTESIAN_POINT('Ctrl Pts',(-9.58837433849125,-13.7220237133736,
119.796479721084)) ;
#191371 = CARTESIAN_POINT('Ctrl Pts',(-9.61107193863009,-13.7436398607786,
119.86561294899)) ;
#191372 = CARTESIAN_POINT('Ctrl Pts',(-9.6848757816061,-13.7436398671878,
119.841381905952)) ;
#191373 = CARTESIAN_POINT('Ctrl Pts',(-9.75867962458211,-13.7436398735971,
119.817150862914)) ;
#191374 = CARTESIAN_POINT('Ctrl Pts',(-9.73598202444326,-13.7220237261921,
119.748017635008)) ;
#191375 = CARTESIAN_POINT('Ctrl Pts',(-9.73888236422256,-13.4322464163541,
119.792546805507)) ;
#191376 = CARTESIAN_POINT('Ctrl Pts',(-9.71520923913131,-13.4308324436495,
119.720442286112)) ;
#191377 = CARTESIAN_POINT('Ctrl Pts',(-9.64140539559821,-13.4308324430486,
119.744673327453)) ;
#191378 = CARTESIAN_POINT('Ctrl Pts',(-9.56760155206506,-13.4308324424476,
119.768904368795)) ;
#191379 = CARTESIAN_POINT('Ctrl Pts',(-9.59127467715629,-13.4322464151522,
119.841008888189)) ;
#191380 = CARTESIAN_POINT('Ctrl Pts',(-9.61494780224751,-13.4336603878567,
119.913113407584)) ;
#191381 = CARTESIAN_POINT('Ctrl Pts',(-9.68875164578064,-13.4336603884577,
119.888882366242)) ;
#191382 = CARTESIAN_POINT('Ctrl Pts',(-9.76255548931378,-13.4336603890586,
119.864651324901)) ;
#191383 = CARTESIAN_POINT('Ctrl Pts',(-9.73888236422256,-13.4322464163541,
119.792546805507)) ;
#191384 = CARTESIAN_POINT('Ctrl Pts',(-9.71766042455426,-13.1452897052538,
119.763098775571)) ;
#191385 = CARTESIAN_POINT('Ctrl Pts',(-9.69470574929104,-13.1639105046461,
119.693182538477)) ;
#191386 = CARTESIAN_POINT('Ctrl Pts',(-9.62090190597256,-13.1639105064164,
119.717413580472)) ;
#191387 = CARTESIAN_POINT('Ctrl Pts',(-9.54709806265407,-13.1639105081867,
119.741644622467)) ;
#191388 = CARTESIAN_POINT('Ctrl Pts',(-9.57005273791729,-13.1452897087944,
119.811560859561)) ;
#191389 = CARTESIAN_POINT('Ctrl Pts',(-9.59300741318051,-13.1266689094021,
119.881477096656)) ;
#191390 = CARTESIAN_POINT('Ctrl Pts',(-9.666811256499,-13.1266689076317,119.857246054661)) ;
#191391 = CARTESIAN_POINT('Ctrl Pts',(-9.74061509981748,-13.1266689058614,
119.833015012666)) ;
#191392 = CARTESIAN_POINT('Ctrl Pts',(-9.71766042455426,-13.1452897052538,
119.763098775571)) ;
#191393 = CARTESIAN_POINT('Ctrl Pts',(-9.67235419941848,-12.8735307541799,
119.660876832314)) ;
#191394 = CARTESIAN_POINT('Ctrl Pts',(-9.65178857018535,-12.9111570713961,
119.598237243989)) ;
#191395 = CARTESIAN_POINT('Ctrl Pts',(-9.57798472730891,-12.9111570744422,
119.622468287331)) ;
#191396 = CARTESIAN_POINT('Ctrl Pts',(-9.5041808844325,-12.9111570774884,
119.646699330672)) ;
#191397 = CARTESIAN_POINT('Ctrl Pts',(-9.52474651366562,-12.8735307602723,
119.709338918997)) ;
#191398 = CARTESIAN_POINT('Ctrl Pts',(-9.54531214289875,-12.8359044430562,
119.771978507321)) ;
#191399 = CARTESIAN_POINT('Ctrl Pts',(-9.61911598577518,-12.83590444001,119.74774746398)) ;
#191400 = CARTESIAN_POINT('Ctrl Pts',(-9.6929198286516,-12.8359044369638,
119.723516420638)) ;
#191401 = CARTESIAN_POINT('Ctrl Pts',(-9.67235419941848,-12.8735307541799,
119.660876832314)) ;
#191402 = CARTESIAN_POINT('Ctrl Pts',(-9.60679604063529,-12.6449175335016,
119.496385341549)) ;
#191403 = CARTESIAN_POINT('Ctrl Pts',(-9.59004978947933,-12.6985622170396,
119.445378962574)) ;
#191404 = CARTESIAN_POINT('Ctrl Pts',(-9.51624594666137,-12.698562218704,
119.469610006093)) ;
#191405 = CARTESIAN_POINT('Ctrl Pts',(-9.44244210384339,-12.6985622203683,
119.493841049613)) ;
#191406 = CARTESIAN_POINT('Ctrl Pts',(-9.45918835499932,-12.6449175368303,
119.544847428588)) ;
#191407 = CARTESIAN_POINT('Ctrl Pts',(-9.47593460615524,-12.5912728532923,
119.595853807563)) ;
#191408 = CARTESIAN_POINT('Ctrl Pts',(-9.54973844897323,-12.5912728516279,
119.571622764043)) ;
#191409 = CARTESIAN_POINT('Ctrl Pts',(-9.6235422917912,-12.5912728499636,
119.547391720524)) ;
#191410 = CARTESIAN_POINT('Ctrl Pts',(-9.60679604063529,-12.6449175335016,
119.496385341549)) ;
#191411 = CARTESIAN_POINT('Ctrl Pts',(-9.52374541645956,-12.4692026417619,
119.278925596776)) ;
#191412 = CARTESIAN_POINT('Ctrl Pts',(-9.51203907941057,-12.5351960145383,
119.243269982934)) ;
#191413 = CARTESIAN_POINT('Ctrl Pts',(-9.43823523604837,-12.5351960141678,
119.267501024796)) ;
#191414 = CARTESIAN_POINT('Ctrl Pts',(-9.36443139268619,-12.5351960137972,
119.291732066658)) ;
#191415 = CARTESIAN_POINT('Ctrl Pts',(-9.3761377297352,-12.4692026410208,
119.3273876805)) ;
#191416 = CARTESIAN_POINT('Ctrl Pts',(-9.38784406678419,-12.4032092682444,
119.363043294341)) ;
#191417 = CARTESIAN_POINT('Ctrl Pts',(-9.46164791014638,-12.4032092686149,
119.33881225248)) ;
#191418 = CARTESIAN_POINT('Ctrl Pts',(-9.53545175350857,-12.4032092689855,
119.314581210618)) ;
#191419 = CARTESIAN_POINT('Ctrl Pts',(-9.52374541645956,-12.4692026417619,
119.278925596776)) ;
#191420 = CARTESIAN_POINT('Ctrl Pts',(-9.42830467125578,-12.3617390442732,
119.023858845481)) ;
#191421 = CARTESIAN_POINT('Ctrl Pts',(-9.42250815332207,-12.4353332114667,
119.006203587009)) ;
#191422 = CARTESIAN_POINT('Ctrl Pts',(-9.34870430822669,-12.4353332096564,
119.030434623592)) ;
#191423 = CARTESIAN_POINT('Ctrl Pts',(-9.27490046313128,-12.4353332078462,
119.054665660175)) ;
#191424 = CARTESIAN_POINT('Ctrl Pts',(-9.28069698106498,-12.3617390406526,
119.072320918647)) ;
#191425 = CARTESIAN_POINT('Ctrl Pts',(-9.28649349899868,-12.2881448734591,
119.089976177118)) ;
#191426 = CARTESIAN_POINT('Ctrl Pts',(-9.36029734409406,-12.2881448752694,
119.065745140535)) ;
#191427 = CARTESIAN_POINT('Ctrl Pts',(-9.43410118918947,-12.2881448770796,
119.041514103952)) ;
#191428 = CARTESIAN_POINT('Ctrl Pts',(-9.42830467125578,-12.3617390442732,
119.023858845481)) ;
#191429 = CARTESIAN_POINT('Ctrl Pts',(-9.32805694090023,-12.3304471936261,
118.753786408682)) ;
#191430 = CARTESIAN_POINT('Ctrl Pts',(-9.32852185600717,-12.4063328156575,
118.755202464884)) ;
#191431 = CARTESIAN_POINT('Ctrl Pts',(-9.25471800936834,-12.4063328154178,
118.779433496766)) ;
#191432 = CARTESIAN_POINT('Ctrl Pts',(-9.18091416272954,-12.4063328151781,
118.803664528648)) ;
#191433 = CARTESIAN_POINT('Ctrl Pts',(-9.18044924762258,-12.3304471931467,
118.802248472446)) ;
#191434 = CARTESIAN_POINT('Ctrl Pts',(-9.17998433251566,-12.2545615711153,
118.800832416244)) ;
#191435 = CARTESIAN_POINT('Ctrl Pts',(-9.25378817915447,-12.254561571355,
118.776601384362)) ;
#191436 = CARTESIAN_POINT('Ctrl Pts',(-9.32759202579329,-12.2545615715947,
118.75237035248)) ;
#191437 = CARTESIAN_POINT('Ctrl Pts',(-9.32805694090023,-12.3304471936261,
118.753786408682)) ;
#191438 = CARTESIAN_POINT('Ctrl Pts',(-9.22771837840066,-12.376595059269,
118.483689651131)) ;
#191439 = CARTESIAN_POINT('Ctrl Pts',(-9.23445495121477,-12.4493688880087,
118.50420816464)) ;
#191440 = CARTESIAN_POINT('Ctrl Pts',(-9.16065110249134,-12.4493688924278,
118.528439190173)) ;
#191441 = CARTESIAN_POINT('Ctrl Pts',(-9.08684725376789,-12.4493688968469,
118.552670215705)) ;
#191442 = CARTESIAN_POINT('Ctrl Pts',(-9.0801106809538,-12.3765950681072,
118.532151702196)) ;
#191443 = CARTESIAN_POINT('Ctrl Pts',(-9.07337410813971,-12.3038212393674,
118.511633188686)) ;
#191444 = CARTESIAN_POINT('Ctrl Pts',(-9.14717795686315,-12.3038212349483,
118.487402163154)) ;
#191445 = CARTESIAN_POINT('Ctrl Pts',(-9.22098180558658,-12.3038212305292,
118.463171137621)) ;
#191446 = CARTESIAN_POINT('Ctrl Pts',(-9.22771837840066,-12.376595059269,
118.483689651131)) ;
#191447 = CARTESIAN_POINT('Ctrl Pts',(-9.13441934511046,-12.4977240769561,
118.235035472375)) ;
#191448 = CARTESIAN_POINT('Ctrl Pts',(-9.14694502691882,-12.5621460088863,
118.273186677651)) ;
#191449 = CARTESIAN_POINT('Ctrl Pts',(-9.07314117653568,-12.5621460220276,
118.297417698128)) ;
#191450 = CARTESIAN_POINT('Ctrl Pts',(-8.99933732615257,-12.5621460351689,
118.321648718606)) ;
#191451 = CARTESIAN_POINT('Ctrl Pts',(-8.9868116443442,-12.4977241032387,
118.283497513329)) ;
#191452 = CARTESIAN_POINT('Ctrl Pts',(-8.97428596253584,-12.4333021713085,
118.245346308053)) ;
#191453 = CARTESIAN_POINT('Ctrl Pts',(-9.04808981291898,-12.4333021581672,
118.221115287576)) ;
#191454 = CARTESIAN_POINT('Ctrl Pts',(-9.12189366330211,-12.4333021450259,
118.196884267098)) ;
#191455 = CARTESIAN_POINT('Ctrl Pts',(-9.13441934511046,-12.4977240769561,
118.235035472375)) ;
#191456 = CARTESIAN_POINT('Ctrl Pts',(-9.05412590445871,-12.6852356935121,
118.026023195874)) ;
#191457 = CARTESIAN_POINT('Ctrl Pts',(-9.07154033274177,-12.736658719336,
118.079064733939)) ;
#191458 = CARTESIAN_POINT('Ctrl Pts',(-8.99773648181564,-12.7366587448055,
118.103295752762)) ;
#191459 = CARTESIAN_POINT('Ctrl Pts',(-8.92393263088948,-12.7366587702751,
118.127526771585)) ;
#191460 = CARTESIAN_POINT('Ctrl Pts',(-8.90651820260644,-12.6852357444512,
118.074485233521)) ;
#191461 = CARTESIAN_POINT('Ctrl Pts',(-8.88910377432337,-12.6338127186274,
118.021443695456)) ;
#191462 = CARTESIAN_POINT('Ctrl Pts',(-8.96290762524951,-12.6338126931579,
117.997212676633)) ;
#191463 = CARTESIAN_POINT('Ctrl Pts',(-9.03671147617565,-12.6338126676883,
117.972981657809)) ;
#191464 = CARTESIAN_POINT('Ctrl Pts',(-9.05412590445871,-12.6852356935121,
118.026023195874)) ;
#191465 = CARTESIAN_POINT('Ctrl Pts',(-8.99222443458086,-12.9233901911912,
117.872760424297)) ;
#191466 = CARTESIAN_POINT('Ctrl Pts',(-9.01325581855126,-12.9582592987456,
117.93681862566)) ;
#191467 = CARTESIAN_POINT('Ctrl Pts',(-8.93945196899214,-12.958259335733,
117.961049648647)) ;
#191468 = CARTESIAN_POINT('Ctrl Pts',(-8.86564811943302,-12.9582593727203,
117.985280671634)) ;
#191469 = CARTESIAN_POINT('Ctrl Pts',(-8.84461673546261,-12.9233902651659,
117.921222470271)) ;
#191470 = CARTESIAN_POINT('Ctrl Pts',(-8.82358535149221,-12.8885211576114,
117.857164268908)) ;
#191471 = CARTESIAN_POINT('Ctrl Pts',(-8.89738920105133,-12.8885211206241,
117.832933245921)) ;
#191472 = CARTESIAN_POINT('Ctrl Pts',(-8.97119305061046,-12.8885210836367,
117.808702222934)) ;
#191473 = CARTESIAN_POINT('Ctrl Pts',(-8.99222443458086,-12.9233901911912,
117.872760424297)) ;
#191474 = CARTESIAN_POINT('Ctrl Pts',(-8.95143036020703,-13.1995574427629,
117.78415630209)) ;
#191475 = CARTESIAN_POINT('Ctrl Pts',(-8.97460286631076,-13.2151953803477,
117.854736015799)) ;
#191476 = CARTESIAN_POINT('Ctrl Pts',(-8.90079901934515,-13.2151954315295,
117.878967046685)) ;
#191477 = CARTESIAN_POINT('Ctrl Pts',(-8.82699517237954,-13.2151954827113,
117.903198077571)) ;
#191478 = CARTESIAN_POINT('Ctrl Pts',(-8.80382266627582,-13.1995575451265,
117.832618363863)) ;
#191479 = CARTESIAN_POINT('Ctrl Pts',(-8.7806501601721,-13.1839196075417,
117.762038650154)) ;
#191480 = CARTESIAN_POINT('Ctrl Pts',(-8.8544540071377,-13.1839195563599,
117.737807619268)) ;
#191481 = CARTESIAN_POINT('Ctrl Pts',(-8.92825785410331,-13.1839195051781,
117.713576588382)) ;
#191482 = CARTESIAN_POINT('Ctrl Pts',(-8.95143036020703,-13.1995574427629,
117.78415630209)) ;
#191483 = CARTESIAN_POINT('Ctrl Pts',(-8.93482201587667,-13.4900175633602,
117.769023857071)) ;
#191484 = CARTESIAN_POINT('Ctrl Pts',(-8.95845396264376,-13.4853985697917,
117.841002952746)) ;
#191485 = CARTESIAN_POINT('Ctrl Pts',(-8.88465012030017,-13.4853986306042,
117.86523399771)) ;
#191486 = CARTESIAN_POINT('Ctrl Pts',(-8.81084627795657,-13.4853986914167,
117.889465042674)) ;
#191487 = CARTESIAN_POINT('Ctrl Pts',(-8.7872143311895,-13.4900176849852,
117.817485946999)) ;
#191488 = CARTESIAN_POINT('Ctrl Pts',(-8.7635823844224,-13.4946366785538,
117.745506851324)) ;
#191489 = CARTESIAN_POINT('Ctrl Pts',(-8.837386226766,-13.4946366177413,117.72127580636)) ;
#191490 = CARTESIAN_POINT('Ctrl Pts',(-8.91119006910959,-13.4946365569288,
117.697044761396)) ;
#191491 = CARTESIAN_POINT('Ctrl Pts',(-8.93482201587667,-13.4900175633602,
117.769023857071)) ;
#191492 = CARTESIAN_POINT('Ctrl Pts',(-8.94231588505226,-13.7743854626431,
117.827189380347)) ;
#191493 = CARTESIAN_POINT('Ctrl Pts',(-8.96472742648635,-13.7499058485971,
117.895451318152)) ;
#191494 = CARTESIAN_POINT('Ctrl Pts',(-8.89092358984129,-13.7499059130724,
117.919682380473)) ;
#191495 = CARTESIAN_POINT('Ctrl Pts',(-8.81711975319624,-13.7499059775478,
117.943913442794)) ;
#191496 = CARTESIAN_POINT('Ctrl Pts',(-8.79470821176214,-13.7743855915938,
117.875651504989)) ;
#191497 = CARTESIAN_POINT('Ctrl Pts',(-8.77229667032804,-13.7988652056398,
117.807389567185)) ;
#191498 = CARTESIAN_POINT('Ctrl Pts',(-8.84610050697309,-13.7988651411644,
117.783158504863)) ;
#191499 = CARTESIAN_POINT('Ctrl Pts',(-8.91990434361816,-13.7988650766891,
117.758927442542)) ;
#191500 = CARTESIAN_POINT('Ctrl Pts',(-8.94231588505226,-13.7743854626431,
117.827189380347)) ;
#191501 = CARTESIAN_POINT('Ctrl Pts',(-8.97275889862437,-14.034295085312,
117.955380252604)) ;
#191502 = CARTESIAN_POINT('Ctrl Pts',(-8.99234358787894,-13.9916338194208,
118.015032054628)) ;
#191503 = CARTESIAN_POINT('Ctrl Pts',(-8.91853975771521,-13.9916338823601,
118.03926313669)) ;
#191504 = CARTESIAN_POINT('Ctrl Pts',(-8.84473592755146,-13.9916339452994,
118.063494218752)) ;
#191505 = CARTESIAN_POINT('Ctrl Pts',(-8.82515123829691,-14.0342952111906,
118.003842416728)) ;
#191506 = CARTESIAN_POINT('Ctrl Pts',(-8.80556654904233,-14.0769564770818,
117.944190614704)) ;
#191507 = CARTESIAN_POINT('Ctrl Pts',(-8.87937037920607,-14.0769564141425,
117.919959532642)) ;
#191508 = CARTESIAN_POINT('Ctrl Pts',(-8.9531742093698,-14.0769563512032,
117.89572845058)) ;
#191509 = CARTESIAN_POINT('Ctrl Pts',(-8.97275889862437,-14.034295085312,
117.955380252604)) ;
#191510 = CARTESIAN_POINT('Ctrl Pts',(-9.02327149966453,-14.2500983716934,
118.144707533452)) ;
#191511 = CARTESIAN_POINT('Ctrl Pts',(-9.0386239611536,-14.1923084690493,
118.191468652428)) ;
#191512 = CARTESIAN_POINT('Ctrl Pts',(-8.96482013749476,-14.1923085231576,
118.215699754303)) ;
#191513 = CARTESIAN_POINT('Ctrl Pts',(-8.89101631383591,-14.192308577266,
118.239930856178)) ;
#191514 = CARTESIAN_POINT('Ctrl Pts',(-8.87566385234682,-14.2500984799102,
118.193169737202)) ;
#191515 = CARTESIAN_POINT('Ctrl Pts',(-8.86031139085772,-14.3078883825543,
118.146408618226)) ;
#191516 = CARTESIAN_POINT('Ctrl Pts',(-8.93411521451657,-14.307888328446,
118.122177516351)) ;
#191517 = CARTESIAN_POINT('Ctrl Pts',(-9.00791903817544,-14.3078882743376,
118.097946414476)) ;
#191518 = CARTESIAN_POINT('Ctrl Pts',(-9.02327149966453,-14.2500983716934,
118.144707533452)) ;
#191519 = CARTESIAN_POINT('Ctrl Pts',(-9.08946157962158,-14.4061684747286,
118.381787624125)) ;
#191520 = CARTESIAN_POINT('Ctrl Pts',(-9.0994811477014,-14.3373982174877,
118.412305610108)) ;
#191521 = CARTESIAN_POINT('Ctrl Pts',(-9.02567732968049,-14.3373982554781,
118.436536729156)) ;
#191522 = CARTESIAN_POINT('Ctrl Pts',(-8.95187351165958,-14.3373982934686,
118.460767848203)) ;
#191523 = CARTESIAN_POINT('Ctrl Pts',(-8.94185394357977,-14.4061685507095,
118.430249862219)) ;
#191524 = CARTESIAN_POINT('Ctrl Pts',(-8.93183437549992,-14.4749388079505,
118.399731876235)) ;
#191525 = CARTESIAN_POINT('Ctrl Pts',(-9.00563819352086,-14.47493876996,118.375500757188)) ;
#191526 = CARTESIAN_POINT('Ctrl Pts',(-9.07944201154175,-14.4749387319696,
118.351269638141)) ;
#191527 = CARTESIAN_POINT('Ctrl Pts',(-9.08946157962158,-14.4061684747286,
118.381787624125)) ;
#191528 = CARTESIAN_POINT('Ctrl Pts',(-9.16561443892928,-14.4915146282391,
118.649122210678)) ;
#191529 = CARTESIAN_POINT('Ctrl Pts',(-9.1695996827275,-14.4166858315879,
118.661260618433)) ;
#191530 = CARTESIAN_POINT('Ctrl Pts',(-9.09579586856763,-14.4166858475525,
118.68549174924)) ;
#191531 = CARTESIAN_POINT('Ctrl Pts',(-9.02199205440779,-14.4166858635172,
118.709722880047)) ;
#191532 = CARTESIAN_POINT('Ctrl Pts',(-9.01800681060956,-14.4915146601683,
118.697584472293)) ;
#191533 = CARTESIAN_POINT('Ctrl Pts',(-9.01402156681139,-14.5663434568195,
118.685446064538)) ;
#191534 = CARTESIAN_POINT('Ctrl Pts',(-9.08782538097122,-14.5663434408549,
118.661214933731)) ;
#191535 = CARTESIAN_POINT('Ctrl Pts',(-9.16162919513109,-14.5663434248902,
118.636983802923)) ;
#191536 = CARTESIAN_POINT('Ctrl Pts',(-9.16561443892928,-14.4915146282391,
118.649122210678)) ;
#191537 = CARTESIAN_POINT('Ctrl Pts',(-9.24634855912068,-14.4998611303634,
118.930692891984)) ;
#191538 = CARTESIAN_POINT('Ctrl Pts',(-9.2439651474815,-14.4243396117057,
118.923433402744)) ;
#191539 = CARTESIAN_POINT('Ctrl Pts',(-9.17016133536057,-14.4243396013487,
118.947664539761)) ;
#191540 = CARTESIAN_POINT('Ctrl Pts',(-9.09635752323964,-14.4243395909917,
118.971895676779)) ;
#191541 = CARTESIAN_POINT('Ctrl Pts',(-9.09874093487882,-14.4998611096494,
118.979155166019)) ;
#191542 = CARTESIAN_POINT('Ctrl Pts',(-9.10112434651799,-14.5753826283071,
118.986414655258)) ;
#191543 = CARTESIAN_POINT('Ctrl Pts',(-9.17492815863893,-14.5753826386642,
118.962183518241)) ;
#191544 = CARTESIAN_POINT('Ctrl Pts',(-9.24873197075985,-14.5753826490212,
118.937952381223)) ;
#191545 = CARTESIAN_POINT('Ctrl Pts',(-9.24634855912068,-14.4998611303634,
118.930692891984)) ;
#191546 = CARTESIAN_POINT('Ctrl Pts',(-9.32363756664781,-14.4309678249663,
119.201372357098)) ;
#191547 = CARTESIAN_POINT('Ctrl Pts',(-9.31512481565251,-14.3601461164253,
119.17544388909)) ;
#191548 = CARTESIAN_POINT('Ctrl Pts',(-9.24132100236167,-14.3601460788116,
119.199675022545)) ;
#191549 = CARTESIAN_POINT('Ctrl Pts',(-9.16751718907081,-14.3601460411978,
119.223906155999)) ;
#191550 = CARTESIAN_POINT('Ctrl Pts',(-9.1760299400661,-14.4309677497388,
119.249834624006)) ;
#191551 = CARTESIAN_POINT('Ctrl Pts',(-9.1845426910614,-14.5017894582798,
119.275763092013)) ;
#191552 = CARTESIAN_POINT('Ctrl Pts',(-9.25834650435227,-14.5017894958936,
119.251531958559)) ;
#191553 = CARTESIAN_POINT('Ctrl Pts',(-9.33215031764312,-14.5017895335074,
119.227300825105)) ;
#191554 = CARTESIAN_POINT('Ctrl Pts',(-9.32363756664781,-14.4309678249663,
119.201372357098)) ;
#191555 = CARTESIAN_POINT('Ctrl Pts',(-9.39258979887019,-14.2895356443573,
119.446881447834)) ;
#191556 = CARTESIAN_POINT('Ctrl Pts',(-9.37851621544446,-14.2284839799428,
119.404015581425)) ;
#191557 = CARTESIAN_POINT('Ctrl Pts',(-9.30471239868478,-14.228483916303,
119.428246704314)) ;
#191558 = CARTESIAN_POINT('Ctrl Pts',(-9.23090858192508,-14.2284838526632,
119.452477827202)) ;
#191559 = CARTESIAN_POINT('Ctrl Pts',(-9.24498216535079,-14.2895355170776,
119.495343693611)) ;
#191560 = CARTESIAN_POINT('Ctrl Pts',(-9.25905574877654,-14.3505871814921,
119.538209560021)) ;
#191561 = CARTESIAN_POINT('Ctrl Pts',(-9.33285956553622,-14.3505872451319,
119.513978437132)) ;
#191562 = CARTESIAN_POINT('Ctrl Pts',(-9.40666338229591,-14.3505873087717,
119.489747314244)) ;
#191563 = CARTESIAN_POINT('Ctrl Pts',(-9.39258979887019,-14.2895356443573,
119.446881447834)) ;
#191564 = CARTESIAN_POINT('Ctrl Pts',(-9.4470024036837,-14.0847982621001,
119.648180996783)) ;
#191565 = CARTESIAN_POINT('Ctrl Pts',(-9.42837319306047,-14.0379502045981,
119.591439424947)) ;
#191566 = CARTESIAN_POINT('Ctrl Pts',(-9.35456937033141,-14.0379501191932,
119.615670529654)) ;
#191567 = CARTESIAN_POINT('Ctrl Pts',(-9.28076554760235,-14.0379500337882,
119.639901634361)) ;
#191568 = CARTESIAN_POINT('Ctrl Pts',(-9.29939475822559,-14.0847980912902,
119.696643206197)) ;
#191569 = CARTESIAN_POINT('Ctrl Pts',(-9.31802396884881,-14.1316461487922,
119.753384778032)) ;
#191570 = CARTESIAN_POINT('Ctrl Pts',(-9.39182779157788,-14.1316462341972,
119.729153673326)) ;
#191571 = CARTESIAN_POINT('Ctrl Pts',(-9.46563161430695,-14.1316463196022,
119.704922568619)) ;
#191572 = CARTESIAN_POINT('Ctrl Pts',(-9.4470024036837,-14.0847982621001,
119.648180996783)) ;
#191573 = CARTESIAN_POINT('Ctrl Pts',(-9.48202871648516,-13.8335759567493,
119.790243958502)) ;
#191574 = CARTESIAN_POINT('Ctrl Pts',(-9.46019456732522,-13.8041981863265,
119.723740660991)) ;
#191575 = CARTESIAN_POINT('Ctrl Pts',(-9.38639073681574,-13.8041980860306,
119.747971742)) ;
#191576 = CARTESIAN_POINT('Ctrl Pts',(-9.31258690630627,-13.8041979857347,
119.772202823009)) ;
#191577 = CARTESIAN_POINT('Ctrl Pts',(-9.33442105546621,-13.8335757561575,
119.83870612052)) ;
#191578 = CARTESIAN_POINT('Ctrl Pts',(-9.35625520462616,-13.8629535265802,
119.905209418031)) ;
#191579 = CARTESIAN_POINT('Ctrl Pts',(-9.43005903513562,-13.8629536268761,
119.880978337022)) ;
#191580 = CARTESIAN_POINT('Ctrl Pts',(-9.5038628656451,-13.8629537271721,
119.856747256013)) ;
#191581 = CARTESIAN_POINT('Ctrl Pts',(-9.48202871648516,-13.8335759567493,
119.790243958502)) ;
#191582 = CARTESIAN_POINT('Ctrl Pts',(-9.49463933409684,-13.5504534645936,
119.86430996683)) ;
#191583 = CARTESIAN_POINT('Ctrl Pts',(-9.4711543977437,-13.5407982837148,
119.792778637903)) ;
#191584 = CARTESIAN_POINT('Ctrl Pts',(-9.39735055836403,-13.540798177125,
119.817009691895)) ;
#191585 = CARTESIAN_POINT('Ctrl Pts',(-9.32354671898437,-13.5407980705352,
119.841240745887)) ;
#191586 = CARTESIAN_POINT('Ctrl Pts',(-9.34703165533753,-13.5504532514139,
119.912772074813)) ;
#191587 = CARTESIAN_POINT('Ctrl Pts',(-9.37051659169066,-13.5601084322927,
119.98430340374)) ;
#191588 = CARTESIAN_POINT('Ctrl Pts',(-9.44432043107033,-13.5601085388825,
119.960072349748)) ;
#191589 = CARTESIAN_POINT('Ctrl Pts',(-9.51812427045,-13.5601086454724,119.935841295756)) ;
#191590 = CARTESIAN_POINT('Ctrl Pts',(-9.49463933409684,-13.5504534645936,
119.86430996683)) ;
#191591 = CARTESIAN_POINT('Ctrl Pts',(-9.48316140353234,-13.261274370137,
119.864568700158)) ;
#191592 = CARTESIAN_POINT('Ctrl Pts',(-9.45971434880432,-13.2717947138784,
119.793152752578)) ;
#191593 = CARTESIAN_POINT('Ctrl Pts',(-9.38591050056251,-13.2717946091373,
119.817383779577)) ;
#191594 = CARTESIAN_POINT('Ctrl Pts',(-9.31210665232066,-13.2717945043963,
119.841614806576)) ;
#191595 = CARTESIAN_POINT('Ctrl Pts',(-9.33555370704867,-13.2612741606549,
119.913030754156)) ;
#191596 = CARTESIAN_POINT('Ctrl Pts',(-9.35900076177666,-13.2507538169135,
119.984446701736)) ;
#191597 = CARTESIAN_POINT('Ctrl Pts',(-9.4328046100185,-13.2507539216545,
119.960215674737)) ;
#191598 = CARTESIAN_POINT('Ctrl Pts',(-9.50660845826033,-13.2507540263956,
119.935984647738)) ;
#191599 = CARTESIAN_POINT('Ctrl Pts',(-9.48316140353234,-13.261274370137,
119.864568700158)) ;
#191600 = CARTESIAN_POINT('Ctrl Pts',(-9.44760475251543,-12.9807689853667,
119.791808570075)) ;
#191601 = CARTESIAN_POINT('Ctrl Pts',(-9.42586969078854,-13.0108889686765,
119.725607077008)) ;
#191602 = CARTESIAN_POINT('Ctrl Pts',(-9.35206583439519,-13.0108888747282,
119.749838079179)) ;
#191603 = CARTESIAN_POINT('Ctrl Pts',(-9.27826197800183,-13.0108887807799,
119.77406908135)) ;
#191604 = CARTESIAN_POINT('Ctrl Pts',(-9.29999703972874,-12.9807687974702,
119.840270574417)) ;
#191605 = CARTESIAN_POINT('Ctrl Pts',(-9.32173210145563,-12.9506488141604,
119.906472067483)) ;
#191606 = CARTESIAN_POINT('Ctrl Pts',(-9.39553595784899,-12.9506489081087,
119.882241065313)) ;
#191607 = CARTESIAN_POINT('Ctrl Pts',(-9.46933981424234,-12.950649002057,
119.858010063142)) ;
#191608 = CARTESIAN_POINT('Ctrl Pts',(-9.44760475251543,-12.9807689853667,
119.791808570075)) ;
#191609 = CARTESIAN_POINT('Ctrl Pts',(-9.38982768745498,-12.7323944980461,
119.651262965745)) ;
#191610 = CARTESIAN_POINT('Ctrl Pts',(-9.37136074583974,-12.7799004526929,
119.595015639306)) ;
#191611 = CARTESIAN_POINT('Ctrl Pts',(-9.29755688290444,-12.7799003762679,
119.619246621551)) ;
#191612 = CARTESIAN_POINT('Ctrl Pts',(-9.22375301996916,-12.7799002998429,
119.643477603796)) ;
#191613 = CARTESIAN_POINT('Ctrl Pts',(-9.24221996158439,-12.7323943451961,
119.699724930235)) ;
#191614 = CARTESIAN_POINT('Ctrl Pts',(-9.26068690319964,-12.6848883905494,
119.755972256675)) ;
#191615 = CARTESIAN_POINT('Ctrl Pts',(-9.33449076613494,-12.6848884669744,
119.73174127443)) ;
#191616 = CARTESIAN_POINT('Ctrl Pts',(-9.4082946290702,-12.6848885433994,
119.707510292184)) ;
#191617 = CARTESIAN_POINT('Ctrl Pts',(-9.38982768745498,-12.7323944980461,
119.651262965745)) ;
#191618 = CARTESIAN_POINT('Ctrl Pts',(-9.31302269296055,-12.5325218808407,
119.452855618209)) ;
#191619 = CARTESIAN_POINT('Ctrl Pts',(-9.29915514898113,-12.594053905958,
119.410617314963)) ;
#191620 = CARTESIAN_POINT('Ctrl Pts',(-9.22535128175568,-12.5940538521665,
119.434848284141)) ;
#191621 = CARTESIAN_POINT('Ctrl Pts',(-9.15154741453021,-12.594053798375,
119.459079253319)) ;
#191622 = CARTESIAN_POINT('Ctrl Pts',(-9.16541495850962,-12.5325217732577,
119.501317556565)) ;
#191623 = CARTESIAN_POINT('Ctrl Pts',(-9.17928250248903,-12.4709897481403,
119.543555859811)) ;
#191624 = CARTESIAN_POINT('Ctrl Pts',(-9.2530863697145,-12.4709898019318,
119.519324890633)) ;
#191625 = CARTESIAN_POINT('Ctrl Pts',(-9.32689023693996,-12.4709898557234,
119.495093921455)) ;
#191626 = CARTESIAN_POINT('Ctrl Pts',(-9.31302269296055,-12.5325218808407,
119.452855618209)) ;
#191627 = CARTESIAN_POINT('Ctrl Pts',(-9.2220091378968,-12.3964669498525,
119.211168926867)) ;
#191628 = CARTESIAN_POINT('Ctrl Pts',(-9.21373997527486,-12.4675909509527,
119.185982390066)) ;
#191629 = CARTESIAN_POINT('Ctrl Pts',(-9.13993610636165,-12.4675909216126,
119.210213354104)) ;
#191630 = CARTESIAN_POINT('Ctrl Pts',(-9.06613223744845,-12.4675908922725,
119.234444318141)) ;
#191631 = CARTESIAN_POINT('Ctrl Pts',(-9.07440140007039,-12.3964668911723,
119.259630854942)) ;
#191632 = CARTESIAN_POINT('Ctrl Pts',(-9.08267056269233,-12.3253428900721,
119.284817391743)) ;
#191633 = CARTESIAN_POINT('Ctrl Pts',(-9.15647443160554,-12.3253429194122,
119.260586427706)) ;
#191634 = CARTESIAN_POINT('Ctrl Pts',(-9.23027830051874,-12.3253429487523,
119.236355463668)) ;
#191635 = CARTESIAN_POINT('Ctrl Pts',(-9.2220091378968,-12.3964669498525,
119.211168926867)) ;
#191636 = CARTESIAN_POINT('Ctrl Pts',(-9.12316400642471,-12.3339203423186,
118.945439966049)) ;
#191637 = CARTESIAN_POINT('Ctrl Pts',(-9.12105247455863,-12.4095182646376,
118.939008579113)) ;
#191638 = CARTESIAN_POINT('Ctrl Pts',(-9.04724860595158,-12.4095182584409,
118.963239544083)) ;
#191639 = CARTESIAN_POINT('Ctrl Pts',(-8.97344473734454,-12.4095182522441,
118.987470509053)) ;
#191640 = CARTESIAN_POINT('Ctrl Pts',(-8.97555626921059,-12.3339203299251,
118.993901895989)) ;
#191641 = CARTESIAN_POINT('Ctrl Pts',(-8.97766780107668,-12.2583224076062,
119.000333282924)) ;
#191642 = CARTESIAN_POINT('Ctrl Pts',(-9.05147166968372,-12.2583224138029,
118.976102317954)) ;
#191643 = CARTESIAN_POINT('Ctrl Pts',(-9.12527553829077,-12.2583224199996,
118.951871352984)) ;
#191644 = CARTESIAN_POINT('Ctrl Pts',(-9.12316400642471,-12.3339203423186,
118.945439966049)) ;
#191645 = CARTESIAN_POINT('Ctrl Pts',(-9.02196719116671,-12.3484596551531,
118.672664621969)) ;
#191646 = CARTESIAN_POINT('Ctrl Pts',(-9.02618431696446,-12.4231567143316,
118.685509305294)) ;
#191647 = CARTESIAN_POINT('Ctrl Pts',(-8.95238045100166,-12.423156728635,
118.709740278318)) ;
#191648 = CARTESIAN_POINT('Ctrl Pts',(-8.87857658503889,-12.4231567429385,
118.733971251342)) ;
#191649 = CARTESIAN_POINT('Ctrl Pts',(-8.87435945924114,-12.34845968376,118.721126568017)) ;
#191650 = CARTESIAN_POINT('Ctrl Pts',(-8.87014233344338,-12.2737626245815,
118.708281884692)) ;
#191651 = CARTESIAN_POINT('Ctrl Pts',(-8.94394619940617,-12.2737626102781,
118.684050911668)) ;
#191652 = CARTESIAN_POINT('Ctrl Pts',(-9.01775006536895,-12.2737625959746,
118.659819938644)) ;
#191653 = CARTESIAN_POINT('Ctrl Pts',(-9.02196719116671,-12.3484596551531,
118.672664621969)) ;
#191654 = CARTESIAN_POINT('Ctrl Pts',(-8.9249315758202,-12.44015832593,118.412680001706)) ;
#191655 = CARTESIAN_POINT('Ctrl Pts',(-8.93519409242402,-12.5085664478243,
118.443937970181)) ;
#191656 = CARTESIAN_POINT('Ctrl Pts',(-8.86139023098923,-12.508566476899,
118.468168956996)) ;
#191657 = CARTESIAN_POINT('Ctrl Pts',(-8.78758636955445,-12.5085665059736,
118.492399943812)) ;
#191658 = CARTESIAN_POINT('Ctrl Pts',(-8.77732385295063,-12.4401583840793,
118.461141975338)) ;
#191659 = CARTESIAN_POINT('Ctrl Pts',(-8.76706133634684,-12.371750262185,
118.429884006863)) ;
#191660 = CARTESIAN_POINT('Ctrl Pts',(-8.84086519778162,-12.3717502331104,
118.405653020048)) ;
#191661 = CARTESIAN_POINT('Ctrl Pts',(-8.9146690592164,-12.3717502040357,
118.381422033232)) ;
#191662 = CARTESIAN_POINT('Ctrl Pts',(-8.9249315758202,-12.44015832593,118.412680001706)) ;
#191663 = CARTESIAN_POINT('Ctrl Pts',(-8.83885025035531,-12.6016814204418,
118.185950248879)) ;
#191664 = CARTESIAN_POINT('Ctrl Pts',(-8.85440481641178,-12.6589156114348,
118.23332694628)) ;
#191665 = CARTESIAN_POINT('Ctrl Pts',(-8.78060096001723,-12.6589156492429,
118.257557948447)) ;
#191666 = CARTESIAN_POINT('Ctrl Pts',(-8.70679710362268,-12.6589156870509,
118.281788950615)) ;
#191667 = CARTESIAN_POINT('Ctrl Pts',(-8.69124253756622,-12.6016814960579,
118.234412253214)) ;
#191668 = CARTESIAN_POINT('Ctrl Pts',(-8.67568797150973,-12.5444473050649,
118.187035555813)) ;
#191669 = CARTESIAN_POINT('Ctrl Pts',(-8.7494918279043,-12.5444472672568,
118.162804553645)) ;
#191670 = CARTESIAN_POINT('Ctrl Pts',(-8.82329568429883,-12.5444472294488,
118.138573551478)) ;
#191671 = CARTESIAN_POINT('Ctrl Pts',(-8.83885025035531,-12.6016814204418,
118.185950248879)) ;
#191672 = CARTESIAN_POINT('Ctrl Pts',(-8.76869825092151,-12.8223735055108,
118.007837352754)) ;
#191673 = CARTESIAN_POINT('Ctrl Pts',(-8.78843878657979,-12.8642856579198,
118.067963838344)) ;
#191674 = CARTESIAN_POINT('Ctrl Pts',(-8.71463493540657,-12.8642856973606,
118.092194856415)) ;
#191675 = CARTESIAN_POINT('Ctrl Pts',(-8.64083108423339,-12.8642857368014,
118.116425874486)) ;
#191676 = CARTESIAN_POINT('Ctrl Pts',(-8.6210905485751,-12.8223735843924,
118.056299388895)) ;
#191677 = CARTESIAN_POINT('Ctrl Pts',(-8.60135001291686,-12.7804614319833,
117.996172903305)) ;
#191678 = CARTESIAN_POINT('Ctrl Pts',(-8.67515386409004,-12.7804613925425,
117.971941885234)) ;
#191679 = CARTESIAN_POINT('Ctrl Pts',(-8.74895771526325,-12.7804613531017,
117.947710867163)) ;
#191680 = CARTESIAN_POINT('Ctrl Pts',(-8.76869825092151,-12.8223735055108,
118.007837352754)) ;
#191681 = CARTESIAN_POINT('Ctrl Pts',(-8.71926001658606,-13.0840251447648,
117.892569881876)) ;
#191682 = CARTESIAN_POINT('Ctrl Pts',(-8.74175151045566,-13.1077315684995,
117.961075342452)) ;
#191683 = CARTESIAN_POINT('Ctrl Pts',(-8.6679476634762,-13.1077316062093,
117.985306373297)) ;
#191684 = CARTESIAN_POINT('Ctrl Pts',(-8.59414381649674,-13.1077316439191,
118.009537404141)) ;
#191685 = CARTESIAN_POINT('Ctrl Pts',(-8.57165232262716,-13.0840252201844,
117.941031943565)) ;
#191686 = CARTESIAN_POINT('Ctrl Pts',(-8.54916082875752,-13.0603187964498,
117.872526482989)) ;
#191687 = CARTESIAN_POINT('Ctrl Pts',(-8.62296467573699,-13.06031875874,117.848295452145)) ;
#191688 = CARTESIAN_POINT('Ctrl Pts',(-8.69676852271643,-13.0603187210301,
117.8240644213)) ;
#191689 = CARTESIAN_POINT('Ctrl Pts',(-8.71926001658606,-13.0840251447648,
117.892569881876)) ;
#191690 = CARTESIAN_POINT('Ctrl Pts',(-8.69264272124601,-13.370624374638,
117.846967346644)) ;
#191691 = CARTESIAN_POINT('Ctrl Pts',(-8.7162928406045,-13.3743556073404,
117.919001793682)) ;
#191692 = CARTESIAN_POINT('Ctrl Pts',(-8.64248899702783,-13.3743556381557,
117.943232834891)) ;
#191693 = CARTESIAN_POINT('Ctrl Pts',(-8.56868515345113,-13.3743556689709,
117.967463876099)) ;
#191694 = CARTESIAN_POINT('Ctrl Pts',(-8.54503503409265,-13.3706244362685,
117.895429429062)) ;
#191695 = CARTESIAN_POINT('Ctrl Pts',(-8.52138491473414,-13.3668932035661,
117.823394982024)) ;
#191696 = CARTESIAN_POINT('Ctrl Pts',(-8.59518875831084,-13.3668931727509,
117.799163940815)) ;
#191697 = CARTESIAN_POINT('Ctrl Pts',(-8.66899260188751,-13.3668931419356,
117.774932899606)) ;
#191698 = CARTESIAN_POINT('Ctrl Pts',(-8.69264272124601,-13.370624374638,
117.846967346644)) ;
#191699 = CARTESIAN_POINT('Ctrl Pts',(-8.69038448104888,-13.6607958553262,
117.875577804038)) ;
#191700 = CARTESIAN_POINT('Ctrl Pts',(-8.71349373520954,-13.6442717980086,
117.945964863113)) ;
#191701 = CARTESIAN_POINT('Ctrl Pts',(-8.63968989357253,-13.6442718197528,
117.970195910229)) ;
#191702 = CARTESIAN_POINT('Ctrl Pts',(-8.56588605193551,-13.6442718414971,
117.994426957346)) ;
#191703 = CARTESIAN_POINT('Ctrl Pts',(-8.54277679777483,-13.6607958988147,
117.924039898271)) ;
#191704 = CARTESIAN_POINT('Ctrl Pts',(-8.51966754361415,-13.6773199561323,
117.853652839196)) ;
#191705 = CARTESIAN_POINT('Ctrl Pts',(-8.59347138525118,-13.6773199343881,
117.82942179208)) ;
#191706 = CARTESIAN_POINT('Ctrl Pts',(-8.6672752268882,-13.6773199126438,
117.805190744963)) ;
#191707 = CARTESIAN_POINT('Ctrl Pts',(-8.69038448104888,-13.6607958553262,
117.875577804038)) ;
#191708 = CARTESIAN_POINT('Ctrl Pts',(-8.711753214821,-13.9332273193549,117.976096242106)) ;
#191709 = CARTESIAN_POINT('Ctrl Pts',(-8.73267209967682,-13.8976559253995,
118.039811789834)) ;
#191710 = CARTESIAN_POINT('Ctrl Pts',(-8.65886825869564,-13.8976559384048,
118.064042838948)) ;
#191711 = CARTESIAN_POINT('Ctrl Pts',(-8.58506441771443,-13.8976559514102,
118.088273888062)) ;
#191712 = CARTESIAN_POINT('Ctrl Pts',(-8.56414553285862,-13.9332273453655,
118.024558340334)) ;
#191713 = CARTESIAN_POINT('Ctrl Pts',(-8.54322664800276,-13.9687987393209,
117.960842792606)) ;
#191714 = CARTESIAN_POINT('Ctrl Pts',(-8.61703048898397,-13.9687987263155,
117.936611743492)) ;
#191715 = CARTESIAN_POINT('Ctrl Pts',(-8.69083432996515,-13.9687987133102,
117.912380694378)) ;
#191716 = CARTESIAN_POINT('Ctrl Pts',(-8.711753214821,-13.9332273193549,117.976096242106)) ;
#191717 = CARTESIAN_POINT('Ctrl Pts',(-8.75479531072491,-14.1696161307288,
118.142792114175)) ;
#191718 = CARTESIAN_POINT('Ctrl Pts',(-8.77200370839762,-14.117484643747,
118.195206116772)) ;
#191719 = CARTESIAN_POINT('Ctrl Pts',(-8.6981998667684,-14.1174846489895,
118.219437163913)) ;
#191720 = CARTESIAN_POINT('Ctrl Pts',(-8.62439602513918,-14.117484654232,
118.243668211053)) ;
#191721 = CARTESIAN_POINT('Ctrl Pts',(-8.60718762746647,-14.1696161412137,
118.191254208456)) ;
#191722 = CARTESIAN_POINT('Ctrl Pts',(-8.58997922979378,-14.2217476281955,
118.138840205859)) ;
#191723 = CARTESIAN_POINT('Ctrl Pts',(-8.66378307142299,-14.221747622953,
118.114609158719)) ;
#191724 = CARTESIAN_POINT('Ctrl Pts',(-8.73758691305221,-14.2217476177105,
118.090378111578)) ;
#191725 = CARTESIAN_POINT('Ctrl Pts',(-8.75479531072491,-14.1696161307288,
118.142792114175)) ;
#191726 = CARTESIAN_POINT('Ctrl Pts',(-8.8148406701214,-14.3504842744957,
118.360928178299)) ;
#191727 = CARTESIAN_POINT('Ctrl Pts',(-8.82715272549973,-14.285645743084,
118.39842871237)) ;
#191728 = CARTESIAN_POINT('Ctrl Pts',(-8.75334888310061,-14.2856457445399,
118.422659757166)) ;
#191729 = CARTESIAN_POINT('Ctrl Pts',(-8.67954504070153,-14.2856457459958,
118.446890801961)) ;
#191730 = CARTESIAN_POINT('Ctrl Pts',(-8.6672329853232,-14.3504842774075,
118.40939026789)) ;
#191731 = CARTESIAN_POINT('Ctrl Pts',(-8.65492092994486,-14.4153228088192,
118.371889733819)) ;
#191732 = CARTESIAN_POINT('Ctrl Pts',(-8.72872477234397,-14.4153228073633,
118.347658689024)) ;
#191733 = CARTESIAN_POINT('Ctrl Pts',(-8.80252861474306,-14.4153228059074,
118.323427644228)) ;
#191734 = CARTESIAN_POINT('Ctrl Pts',(-8.8148406701214,-14.3504842744957,
118.360928178299)) ;
#191735 = CARTESIAN_POINT('Ctrl Pts',(-8.88828842378017,-14.4664314373378,
118.620362245209)) ;
#191736 = CARTESIAN_POINT('Ctrl Pts',(-8.89475089159606,-14.393398523113,
118.640045879492)) ;
#191737 = CARTESIAN_POINT('Ctrl Pts',(-8.82094704774123,-14.3933985223856,
118.664276919853)) ;
#191738 = CARTESIAN_POINT('Ctrl Pts',(-8.74714320388638,-14.3933985216583,
118.688507960215)) ;
#191739 = CARTESIAN_POINT('Ctrl Pts',(-8.7406807360705,-14.4664314358832,
118.668824325932)) ;
#191740 = CARTESIAN_POINT('Ctrl Pts',(-8.73421826825462,-14.539464350108,
118.64914069165)) ;
#191741 = CARTESIAN_POINT('Ctrl Pts',(-8.80802211210946,-14.5394643508353,
118.624909651288)) ;
#191742 = CARTESIAN_POINT('Ctrl Pts',(-8.88182595596429,-14.5394643515627,
118.600678610927)) ;
#191743 = CARTESIAN_POINT('Ctrl Pts',(-8.88828842378017,-14.4664314373378,
118.620362245209)) ;
#191744 = CARTESIAN_POINT('Ctrl Pts',(-8.96751292468527,-14.505814940549,
118.8970150562)) ;
#191745 = CARTESIAN_POINT('Ctrl Pts',(-8.96772137448786,-14.4299235771365,
118.897649960723)) ;
#191746 = CARTESIAN_POINT('Ctrl Pts',(-8.89391753013919,-14.4299235770663,
118.92188099958)) ;
#191747 = CARTESIAN_POINT('Ctrl Pts',(-8.82011368579049,-14.429923576996,
118.946112038437)) ;
#191748 = CARTESIAN_POINT('Ctrl Pts',(-8.81990523598791,-14.5058149404085,
118.945477133914)) ;
#191749 = CARTESIAN_POINT('Ctrl Pts',(-8.81969678618531,-14.5817063038209,
118.944842229391)) ;
#191750 = CARTESIAN_POINT('Ctrl Pts',(-8.893500630534,-14.5817063038912,118.920611190534)) ;
#191751 = CARTESIAN_POINT('Ctrl Pts',(-8.96730447488267,-14.5817063039614,
118.896380151676)) ;
#191752 = CARTESIAN_POINT('Ctrl Pts',(-8.96751292468527,-14.505814940549,
118.8970150562)) ;
#191753 = CARTESIAN_POINT('Ctrl Pts',(-9.04680096010112,-14.46830400306,119.173859350138)) ;
#191754 = CARTESIAN_POINT('Ctrl Pts',(-9.04074169525011,-14.3949198444241,
119.155403807125)) ;
#191755 = CARTESIAN_POINT('Ctrl Pts',(-8.96693785085317,-14.3949198453838,
119.179634845835)) ;
#191756 = CARTESIAN_POINT('Ctrl Pts',(-8.89313400645622,-14.3949198463436,
119.203865884545)) ;
#191757 = CARTESIAN_POINT('Ctrl Pts',(-8.89919327130725,-14.4683040049795,
119.222321427559)) ;
#191758 = CARTESIAN_POINT('Ctrl Pts',(-8.90525253615825,-14.5416881636154,
119.240776970572)) ;
#191759 = CARTESIAN_POINT('Ctrl Pts',(-8.9790563805552,-14.5416881626556,
119.216545931862)) ;
#191760 = CARTESIAN_POINT('Ctrl Pts',(-9.05286022495216,-14.5416881616959,
119.192314893152)) ;
#191761 = CARTESIAN_POINT('Ctrl Pts',(-9.04680096010112,-14.46830400306,119.173859350138)) ;
#191762 = CARTESIAN_POINT('Ctrl Pts',(-9.12041342587677,-14.3544455833434,
119.433744666185)) ;
#191763 = CARTESIAN_POINT('Ctrl Pts',(-9.10846654169691,-14.28890351008,119.397356384606)) ;
#191764 = CARTESIAN_POINT('Ctrl Pts',(-9.03466269818544,-14.2889035106551,
119.421587426014)) ;
#191765 = CARTESIAN_POINT('Ctrl Pts',(-8.96085885467401,-14.2889035112301,
119.445818467421)) ;
#191766 = CARTESIAN_POINT('Ctrl Pts',(-8.97280573885388,-14.3544455844935,
119.482206748999)) ;
#191767 = CARTESIAN_POINT('Ctrl Pts',(-8.98475262303375,-14.4199876577569,
119.518595030578)) ;
#191768 = CARTESIAN_POINT('Ctrl Pts',(-9.05855646654521,-14.4199876571819,
119.49436398917)) ;
#191769 = CARTESIAN_POINT('Ctrl Pts',(-9.13236031005665,-14.4199876566068,
119.470132947763)) ;
#191770 = CARTESIAN_POINT('Ctrl Pts',(-9.12041342587677,-14.3544455833434,
119.433744666185)) ;
#191771 = CARTESIAN_POINT('Ctrl Pts',(-9.1810115636041,-14.1743504235921,
119.653691355209)) ;
#191772 = CARTESIAN_POINT('Ctrl Pts',(-9.16408389144678,-14.1212879349947,
119.602132397024)) ;
#191773 = CARTESIAN_POINT('Ctrl Pts',(-9.09028004882841,-14.121287932882,
119.626363441152)) ;
#191774 = CARTESIAN_POINT('Ctrl Pts',(-9.01647620621002,-14.1212879307693,
119.650594485279)) ;
#191775 = CARTESIAN_POINT('Ctrl Pts',(-9.03340387836735,-14.1743504193667,
119.702153443464)) ;
#191776 = CARTESIAN_POINT('Ctrl Pts',(-9.05033155052467,-14.2274129079642,
119.753712401649)) ;
#191777 = CARTESIAN_POINT('Ctrl Pts',(-9.12413539314305,-14.2274129100769,
119.729481357522)) ;
#191778 = CARTESIAN_POINT('Ctrl Pts',(-9.19793923576142,-14.2274129121895,
119.705250313394)) ;
#191779 = CARTESIAN_POINT('Ctrl Pts',(-9.1810115636041,-14.1743504235921,
119.653691355209)) ;
#191780 = CARTESIAN_POINT('Ctrl Pts',(-9.22434028506487,-13.9404023706078,
119.821067847651)) ;
#191781 = CARTESIAN_POINT('Ctrl Pts',(-9.20362990504079,-13.9035978670998,
119.757987371546)) ;
#191782 = CARTESIAN_POINT('Ctrl Pts',(-9.12982606302781,-13.903597860184,
119.782218417518)) ;
#191783 = CARTESIAN_POINT('Ctrl Pts',(-9.05602222101485,-13.9035978532681,
119.806449463489)) ;
#191784 = CARTESIAN_POINT('Ctrl Pts',(-9.07673260103893,-13.940402356776,
119.869529939594)) ;
#191785 = CARTESIAN_POINT('Ctrl Pts',(-9.09744298106302,-13.977206860284,
119.932610415698)) ;
#191786 = CARTESIAN_POINT('Ctrl Pts',(-9.17124682307598,-13.9772068671999,
119.908379369727)) ;
#191787 = CARTESIAN_POINT('Ctrl Pts',(-9.24505066508896,-13.9772068741157,
119.884148323755)) ;
#191788 = CARTESIAN_POINT('Ctrl Pts',(-9.22434028506487,-13.9404023706078,
119.821067847651)) ;
#191789 = CARTESIAN_POINT('Ctrl Pts',(-9.24641752481561,-13.6671888266285,
119.923944245978)) ;
#191790 = CARTESIAN_POINT('Ctrl Pts',(-9.22339798409645,-13.6494076085659,
119.853830438823)) ;
#191791 = CARTESIAN_POINT('Ctrl Pts',(-9.14959414204322,-13.6494075929638,
119.878061484672)) ;
#191792 = CARTESIAN_POINT('Ctrl Pts',(-9.07579029998996,-13.6494075773616,
119.902292530521)) ;
#191793 = CARTESIAN_POINT('Ctrl Pts',(-9.09880984070912,-13.6671887954242,
119.972406337675)) ;
#191794 = CARTESIAN_POINT('Ctrl Pts',(-9.12182938142827,-13.6849700134867,
120.042520144829)) ;
#191795 = CARTESIAN_POINT('Ctrl Pts',(-9.19563322348152,-13.6849700290889,
120.018289098981)) ;
#191796 = CARTESIAN_POINT('Ctrl Pts',(-9.26943706553476,-13.684970044691,
119.994058053132)) ;
#191797 = CARTESIAN_POINT('Ctrl Pts',(-9.24641752481561,-13.6671888266285,
119.923944245978)) ;
#191798 = CARTESIAN_POINT('Ctrl Pts',(-9.24470708760251,-13.3783758394987,
119.954073987494)) ;
#191799 = CARTESIAN_POINT('Ctrl Pts',(-9.22104244183216,-13.3807343880949,
119.881995294314)) ;
#191800 = CARTESIAN_POINT('Ctrl Pts',(-9.14723859835509,-13.3807343653365,
119.906226335826)) ;
#191801 = CARTESIAN_POINT('Ctrl Pts',(-9.07343475487802,-13.3807343425781,
119.930457377338)) ;
#191802 = CARTESIAN_POINT('Ctrl Pts',(-9.09709940064837,-13.3783757939819,
120.002536070518)) ;
#191803 = CARTESIAN_POINT('Ctrl Pts',(-9.12076404641873,-13.3760172453858,
120.074614763697)) ;
#191804 = CARTESIAN_POINT('Ctrl Pts',(-9.19456788989579,-13.3760172681442,
120.050383722185)) ;
#191805 = CARTESIAN_POINT('Ctrl Pts',(-9.26837173337287,-13.3760172909026,
120.026152680673)) ;
#191806 = CARTESIAN_POINT('Ctrl Pts',(-9.24470708760251,-13.3783758394987,
119.954073987494)) ;
#191807 = CARTESIAN_POINT('Ctrl Pts',(-9.21880682278639,-13.0914976589315,
119.910642708643)) ;
#191808 = CARTESIAN_POINT('Ctrl Pts',(-9.19618261652847,-13.1138898142191,
119.841733026189)) ;
#191809 = CARTESIAN_POINT('Ctrl Pts',(-9.12237877045627,-13.113889784642,
119.865964059796)) ;
#191810 = CARTESIAN_POINT('Ctrl Pts',(-9.04857492438406,-13.1138897550648,
119.890195093404)) ;
#191811 = CARTESIAN_POINT('Ctrl Pts',(-9.07119913064198,-13.0914975997771,
119.959104775858)) ;
#191812 = CARTESIAN_POINT('Ctrl Pts',(-9.09382333689987,-13.0691054444894,
120.028014458313)) ;
#191813 = CARTESIAN_POINT('Ctrl Pts',(-9.1676271829721,-13.0691054740666,
120.003783424705)) ;
#191814 = CARTESIAN_POINT('Ctrl Pts',(-9.24143102904429,-13.0691055036438,
119.979552391098)) ;
#191815 = CARTESIAN_POINT('Ctrl Pts',(-9.21880682278639,-13.0914976589315,
119.910642708643)) ;
#191816 = CARTESIAN_POINT('Ctrl Pts',(-9.16970010340457,-12.827936357185,
119.796531141099)) ;
#191817 = CARTESIAN_POINT('Ctrl Pts',(-9.14973808973235,-12.8687628272745,
119.735730067553)) ;
#191818 = CARTESIAN_POINT('Ctrl Pts',(-9.07593423988325,-12.8687627938338,
119.759961089656)) ;
#191819 = CARTESIAN_POINT('Ctrl Pts',(-9.00213039003418,-12.868762760393,
119.78419211176)) ;
#191820 = CARTESIAN_POINT('Ctrl Pts',(-9.02209240370642,-12.8279362903035,
119.844993185306)) ;
#191821 = CARTESIAN_POINT('Ctrl Pts',(-9.04205441737867,-12.7871098202139,
119.905794258852)) ;
#191822 = CARTESIAN_POINT('Ctrl Pts',(-9.11585826722775,-12.7871098536547,
119.881563236748)) ;
#191823 = CARTESIAN_POINT('Ctrl Pts',(-9.18966211707683,-12.7871098870954,
119.857332214645)) ;
#191824 = CARTESIAN_POINT('Ctrl Pts',(-9.16970010340457,-12.827936357185,
119.796531141099)) ;
#191825 = CARTESIAN_POINT('Ctrl Pts',(-9.09997329978592,-12.6061166858968,
119.619706123168)) ;
#191826 = CARTESIAN_POINT('Ctrl Pts',(-9.08411501804255,-12.662489659223,
119.571404354757)) ;
#191827 = CARTESIAN_POINT('Ctrl Pts',(-9.01031116342983,-12.6624896260607,
119.595635362352)) ;
#191828 = CARTESIAN_POINT('Ctrl Pts',(-8.93650730881713,-12.6624895928983,
119.619866369947)) ;
#191829 = CARTESIAN_POINT('Ctrl Pts',(-8.95236559056048,-12.6061166195721,
119.668168138357)) ;
#191830 = CARTESIAN_POINT('Ctrl Pts',(-8.96822387230382,-12.5497436462459,
119.716469906768)) ;
#191831 = CARTESIAN_POINT('Ctrl Pts',(-9.04202772691654,-12.5497436794083,
119.692238899173)) ;
#191832 = CARTESIAN_POINT('Ctrl Pts',(-9.11583158152926,-12.5497437125706,
119.668007891578)) ;
#191833 = CARTESIAN_POINT('Ctrl Pts',(-9.09997329978592,-12.6061166858968,
119.619706123168)) ;
#191834 = CARTESIAN_POINT('Ctrl Pts',(-9.01413184976296,-12.4431271546039,
119.393730189171)) ;
#191835 = CARTESIAN_POINT('Ctrl Pts',(-9.0035097601658,-12.5109613838961,
119.361377017011)) ;
#191836 = CARTESIAN_POINT('Ctrl Pts',(-8.92970590071719,-12.510961357698,
119.385608009876)) ;
#191837 = CARTESIAN_POINT('Ctrl Pts',(-8.85590204126855,-12.5109613315,119.409839002741)) ;
#191838 = CARTESIAN_POINT('Ctrl Pts',(-8.86652413086572,-12.4431271022078,
119.442192174902)) ;
#191839 = CARTESIAN_POINT('Ctrl Pts',(-8.87714622046288,-12.3752928729157,
119.474545347062)) ;
#191840 = CARTESIAN_POINT('Ctrl Pts',(-8.95095007991151,-12.3752928991138,
119.450314354197)) ;
#191841 = CARTESIAN_POINT('Ctrl Pts',(-9.02475393936012,-12.3752929253118,
119.426083361332)) ;
#191842 = CARTESIAN_POINT('Ctrl Pts',(-9.01413184976296,-12.4431271546039,
119.393730189171)) ;
#191843 = CARTESIAN_POINT('Ctrl Pts',(-8.91797994965442,-12.3502094912987,
119.136186372322)) ;
#191844 = CARTESIAN_POINT('Ctrl Pts',(-8.91332488011852,-12.4246287371788,
119.122007780357)) ;
#191845 = CARTESIAN_POINT('Ctrl Pts',(-8.83952101692612,-12.4246287241844,
119.14623876182)) ;
#191846 = CARTESIAN_POINT('Ctrl Pts',(-8.76571715373373,-12.42462871119,119.170469743282)) ;
#191847 = CARTESIAN_POINT('Ctrl Pts',(-8.77037222326963,-12.35020946531,119.184648335247)) ;
#191848 = CARTESIAN_POINT('Ctrl Pts',(-8.77502729280552,-12.2757902194299,
119.198826927212)) ;
#191849 = CARTESIAN_POINT('Ctrl Pts',(-8.84883115599792,-12.2757902324242,
119.174595945749)) ;
#191850 = CARTESIAN_POINT('Ctrl Pts',(-8.92263501919031,-12.2757902454186,
119.150364964287)) ;
#191851 = CARTESIAN_POINT('Ctrl Pts',(-8.91797994965442,-12.3502094912987,
119.136186372322)) ;
#191852 = CARTESIAN_POINT('Ctrl Pts',(-8.81678556357941,-12.3330949628537,
118.863432839579)) ;
#191853 = CARTESIAN_POINT('Ctrl Pts',(-8.81845498558905,-12.4088168292008,
118.868517628251)) ;
#191854 = CARTESIAN_POINT('Ctrl Pts',(-8.744651119493,-12.4088168339974,118.892748600869)) ;
#191855 = CARTESIAN_POINT('Ctrl Pts',(-8.67084725339693,-12.408816838794,
118.916979573487)) ;
#191856 = CARTESIAN_POINT('Ctrl Pts',(-8.66917783138726,-12.3330949724469,
118.911894784815)) ;
#191857 = CARTESIAN_POINT('Ctrl Pts',(-8.66750840937762,-12.2573731060998,
118.906809996142)) ;
#191858 = CARTESIAN_POINT('Ctrl Pts',(-8.74131227547369,-12.2573731013032,
118.882579023524)) ;
#191859 = CARTESIAN_POINT('Ctrl Pts',(-8.81511614156976,-12.2573730965066,
118.858348050906)) ;
#191860 = CARTESIAN_POINT('Ctrl Pts',(-8.81678556357941,-12.3330949628537,
118.863432839579)) ;
#191861 = CARTESIAN_POINT('Ctrl Pts',(-8.71722634028701,-12.3941323979468,
118.595736689137)) ;
#191862 = CARTESIAN_POINT('Ctrl Pts',(-8.72511363131764,-12.4657028650143,
118.619760103441)) ;
#191863 = CARTESIAN_POINT('Ctrl Pts',(-8.65130976405657,-12.4657028918637,
118.64399107251)) ;
#191864 = CARTESIAN_POINT('Ctrl Pts',(-8.57750589679551,-12.4657029187131,
118.66822204158)) ;
#191865 = CARTESIAN_POINT('Ctrl Pts',(-8.56961860576491,-12.3941324516456,
118.644198627277)) ;
#191866 = CARTESIAN_POINT('Ctrl Pts',(-8.56173131473427,-12.3225619845781,
118.620175212973)) ;
#191867 = CARTESIAN_POINT('Ctrl Pts',(-8.63553518199533,-12.3225619577287,
118.595944243904)) ;
#191868 = CARTESIAN_POINT('Ctrl Pts',(-8.70933904925639,-12.3225619308793,
118.571713274834)) ;
#191869 = CARTESIAN_POINT('Ctrl Pts',(-8.71722634028701,-12.3941323979468,
118.595736689137)) ;
#191870 = CARTESIAN_POINT('Ctrl Pts',(-8.62633858589104,-12.5280047279255,
118.354282868859)) ;
#191871 = CARTESIAN_POINT('Ctrl Pts',(-8.63985083191165,-12.5903323506603,
118.395438988361)) ;
#191872 = CARTESIAN_POINT('Ctrl Pts',(-8.56604696618086,-12.5903324003766,
118.419669962092)) ;
#191873 = CARTESIAN_POINT('Ctrl Pts',(-8.49224310045005,-12.5903324500929,
118.443900935822)) ;
#191874 = CARTESIAN_POINT('Ctrl Pts',(-8.47873085442944,-12.5280048273581,
118.40274481632)) ;
#191875 = CARTESIAN_POINT('Ctrl Pts',(-8.46521860840883,-12.4656772046233,
118.361588696818)) ;
#191876 = CARTESIAN_POINT('Ctrl Pts',(-8.53902247413964,-12.465677154907,
118.337357723088)) ;
#191877 = CARTESIAN_POINT('Ctrl Pts',(-8.61282633987043,-12.4656771051907,
118.313126749357)) ;
#191878 = CARTESIAN_POINT('Ctrl Pts',(-8.62633858589104,-12.5280047279255,
118.354282868859)) ;
#191879 = CARTESIAN_POINT('Ctrl Pts',(-8.54913265153816,-12.725823043926,
118.15460227813)) ;
#191880 = CARTESIAN_POINT('Ctrl Pts',(-8.56732074945708,-12.7744304923816,
118.210000287949)) ;
#191881 = CARTESIAN_POINT('Ctrl Pts',(-8.49351688740926,-12.7744305640523,
118.234231272897)) ;
#191882 = CARTESIAN_POINT('Ctrl Pts',(-8.41971302536143,-12.7744306357229,
118.258462257845)) ;
#191883 = CARTESIAN_POINT('Ctrl Pts',(-8.40152492744251,-12.7258231872673,
118.203064248026)) ;
#191884 = CARTESIAN_POINT('Ctrl Pts',(-8.38333682952358,-12.6772157388117,
118.147666238207)) ;
#191885 = CARTESIAN_POINT('Ctrl Pts',(-8.45714069157141,-12.677215667141,
118.123435253259)) ;
#191886 = CARTESIAN_POINT('Ctrl Pts',(-8.53094455361923,-12.6772155954704,
118.099204268311)) ;
#191887 = CARTESIAN_POINT('Ctrl Pts',(-8.54913265153816,-12.725823043926,
118.15460227813)) ;
#191888 = CARTESIAN_POINT('Ctrl Pts',(-8.49060543502265,-12.9740366931117,
118.011903735962)) ;
#191889 = CARTESIAN_POINT('Ctrl Pts',(-8.51217039092456,-13.0053860395,118.077587110234)) ;
#191890 = CARTESIAN_POINT('Ctrl Pts',(-8.43836653480978,-13.0053861296798,
118.101818113253)) ;
#191891 = CARTESIAN_POINT('Ctrl Pts',(-8.36456267869501,-13.0053862198596,
118.126049116273)) ;
#191892 = CARTESIAN_POINT('Ctrl Pts',(-8.3429977227931,-12.9740368734713,
118.060365742)) ;
#191893 = CARTESIAN_POINT('Ctrl Pts',(-8.3214327668912,-12.942687527083,117.994682367728)) ;
#191894 = CARTESIAN_POINT('Ctrl Pts',(-8.39523662300597,-12.9426874369032,
117.970451364709)) ;
#191895 = CARTESIAN_POINT('Ctrl Pts',(-8.46904047912075,-12.9426873467234,
117.94622036169)) ;
#191896 = CARTESIAN_POINT('Ctrl Pts',(-8.49060543502265,-12.9740366931117,
118.011903735962)) ;
#191897 = CARTESIAN_POINT('Ctrl Pts',(-8.45445954867268,-13.2534633118697,
117.93728020588)) ;
#191898 = CARTESIAN_POINT('Ctrl Pts',(-8.47784570948945,-13.2653501074278,
118.008510676394)) ;
#191899 = CARTESIAN_POINT('Ctrl Pts',(-8.40404186114072,-13.2653502091921,
118.032741703068)) ;
#191900 = CARTESIAN_POINT('Ctrl Pts',(-8.33023801279197,-13.2653503109564,
118.056972729741)) ;
#191901 = CARTESIAN_POINT('Ctrl Pts',(-8.30685185197521,-13.2534635153983,
117.985742259227)) ;
#191902 = CARTESIAN_POINT('Ctrl Pts',(-8.28346569115844,-13.2415767198401,
117.914511788712)) ;
#191903 = CARTESIAN_POINT('Ctrl Pts',(-8.35726953950717,-13.2415766180759,
117.890280762039)) ;
#191904 = CARTESIAN_POINT('Ctrl Pts',(-8.4310733878559,-13.2415765163116,
117.866049735365)) ;
#191905 = CARTESIAN_POINT('Ctrl Pts',(-8.45445954867268,-13.2534633118697,
117.93728020588)) ;
#191906 = CARTESIAN_POINT('Ctrl Pts',(-8.44237507272009,-13.5448240416985,
117.935968379582)) ;
#191907 = CARTESIAN_POINT('Ctrl Pts',(-8.46590485409652,-13.5363866538712,
118.007636295091)) ;
#191908 = CARTESIAN_POINT('Ctrl Pts',(-8.39210101449033,-13.5363867591239,
118.031867348393)) ;
#191909 = CARTESIAN_POINT('Ctrl Pts',(-8.31829717488412,-13.5363868643766,
118.056098401694)) ;
#191910 = CARTESIAN_POINT('Ctrl Pts',(-8.29476739350768,-13.544824252204,
117.984430486186)) ;
#191911 = CARTESIAN_POINT('Ctrl Pts',(-8.27123761213126,-13.5532616400314,
117.912762570677)) ;
#191912 = CARTESIAN_POINT('Ctrl Pts',(-8.34504145173747,-13.5532615347787,
117.888531517376)) ;
#191913 = CARTESIAN_POINT('Ctrl Pts',(-8.41884529134366,-13.553261429526,
117.864300464074)) ;
#191914 = CARTESIAN_POINT('Ctrl Pts',(-8.44237507272009,-13.5448240416985,
117.935968379582)) ;
#191915 = CARTESIAN_POINT('Ctrl Pts',(-8.45433167813838,-13.8260554927979,
118.007737132418)) ;
#191916 = CARTESIAN_POINT('Ctrl Pts',(-8.47632978159744,-13.7979711605236,
118.074739804093)) ;
#191917 = CARTESIAN_POINT('Ctrl Pts',(-8.4025259507639,-13.7979712603347,
118.098970884115)) ;
#191918 = CARTESIAN_POINT('Ctrl Pts',(-8.32872211993039,-13.7979713601458,
118.123201964137)) ;
#191919 = CARTESIAN_POINT('Ctrl Pts',(-8.30672401647134,-13.8260556924201,
118.056199292462)) ;
#191920 = CARTESIAN_POINT('Ctrl Pts',(-8.2847259130123,-13.8541400246944,
117.989196620786)) ;
#191921 = CARTESIAN_POINT('Ctrl Pts',(-8.35852974384581,-13.8541399248833,
117.964965540765)) ;
#191922 = CARTESIAN_POINT('Ctrl Pts',(-8.43233357467934,-13.8541398250722,
117.940734460743)) ;
#191923 = CARTESIAN_POINT('Ctrl Pts',(-8.45433167813838,-13.8260554927979,
118.007737132418)) ;
#191924 = CARTESIAN_POINT('Ctrl Pts',(-8.4890114847467,-14.0796928172426,
118.148954260656)) ;
#191925 = CARTESIAN_POINT('Ctrl Pts',(-8.50788465162799,-14.0338589352342,
118.206438879706)) ;
#191926 = CARTESIAN_POINT('Ctrl Pts',(-8.43408082879524,-14.033859021297,
118.230669984097)) ;
#191927 = CARTESIAN_POINT('Ctrl Pts',(-8.36027700596246,-14.0338591073598,
118.254901088488)) ;
#191928 = CARTESIAN_POINT('Ctrl Pts',(-8.34140383908118,-14.0796929893683,
118.197416469438)) ;
#191929 = CARTESIAN_POINT('Ctrl Pts',(-8.32253067219987,-14.1255268713768,
118.139931850387)) ;
#191930 = CARTESIAN_POINT('Ctrl Pts',(-8.39633449503265,-14.1255267853139,
118.115700745996)) ;
#191931 = CARTESIAN_POINT('Ctrl Pts',(-8.47013831786541,-14.1255266992511,
118.091469641605)) ;
#191932 = CARTESIAN_POINT('Ctrl Pts',(-8.4890114847467,-14.0796928172426,
118.148954260656)) ;
#191933 = CARTESIAN_POINT('Ctrl Pts',(-8.54257172063092,-14.2840883967328,
118.347363105514)) ;
#191934 = CARTESIAN_POINT('Ctrl Pts',(-8.55700344248699,-14.223916620712,
118.391319799648)) ;
#191935 = CARTESIAN_POINT('Ctrl Pts',(-8.48319962595063,-14.2239166860408,
118.415550923217)) ;
#191936 = CARTESIAN_POINT('Ctrl Pts',(-8.4093958094143,-14.2239167513696,
118.439782046786)) ;
#191937 = CARTESIAN_POINT('Ctrl Pts',(-8.39496408755824,-14.2840885273904,
118.395825352652)) ;
#191938 = CARTESIAN_POINT('Ctrl Pts',(-8.38053236570218,-14.3442603034112,
118.351868658518)) ;
#191939 = CARTESIAN_POINT('Ctrl Pts',(-8.45433618223852,-14.3442602380824,
118.327637534949)) ;
#191940 = CARTESIAN_POINT('Ctrl Pts',(-8.52813999877486,-14.3442601727535,
118.30340641138)) ;
#191941 = CARTESIAN_POINT('Ctrl Pts',(-8.54257172063092,-14.2840883967328,
118.347363105514)) ;
#191942 = CARTESIAN_POINT('Ctrl Pts',(-8.61125485980821,-14.4281001590278,
118.59212459814)) ;
#191943 = CARTESIAN_POINT('Ctrl Pts',(-8.62017704976491,-14.3577843512303,
118.619300147099)) ;
#191944 = CARTESIAN_POINT('Ctrl Pts',(-8.54637323724559,-14.3577843906291,
118.643531282903)) ;
#191945 = CARTESIAN_POINT('Ctrl Pts',(-8.47256942472626,-14.357784430028,
118.667762418707)) ;
#191946 = CARTESIAN_POINT('Ctrl Pts',(-8.46364723476955,-14.4281002378256,
118.640586869749)) ;
#191947 = CARTESIAN_POINT('Ctrl Pts',(-8.45472504481283,-14.4984160456232,
118.61341132079)) ;
#191948 = CARTESIAN_POINT('Ctrl Pts',(-8.52852885733216,-14.4984160062243,
118.589180184986)) ;
#191949 = CARTESIAN_POINT('Ctrl Pts',(-8.6023326698515,-14.4984159668254,
118.564949049182)) ;
#191950 = CARTESIAN_POINT('Ctrl Pts',(-8.61125485980821,-14.4281001590278,
118.59212459814)) ;
#191951 = CARTESIAN_POINT('Ctrl Pts',(-8.68881511671028,-14.4990916302809,
118.863813337563)) ;
#191952 = CARTESIAN_POINT('Ctrl Pts',(-8.69160201611696,-14.4237145145617,
118.872301781483)) ;
#191953 = CARTESIAN_POINT('Ctrl Pts',(-8.61779820492839,-14.4237145258999,
118.89653292134)) ;
#191954 = CARTESIAN_POINT('Ctrl Pts',(-8.5439943937398,-14.4237145372381,
118.920764061198)) ;
#191955 = CARTESIAN_POINT('Ctrl Pts',(-8.54120749433315,-14.4990916529572,
118.912275617278)) ;
#191956 = CARTESIAN_POINT('Ctrl Pts',(-8.53842059492649,-14.5744687686764,
118.903787173358)) ;
#191957 = CARTESIAN_POINT('Ctrl Pts',(-8.61222440611505,-14.5744687573382,
118.879556033501)) ;
#191958 = CARTESIAN_POINT('Ctrl Pts',(-8.68602821730362,-14.574468746,118.855324893643)) ;
#191959 = CARTESIAN_POINT('Ctrl Pts',(-8.68881511671028,-14.4990916302809,
118.863813337563)) ;
#191960 = CARTESIAN_POINT('Ctrl Pts',(-8.76912430296958,-14.4927693074735,
119.143894083316)) ;
#191961 = CARTESIAN_POINT('Ctrl Pts',(-8.76557443984321,-14.4177207882231,
119.133081771065)) ;
#191962 = CARTESIAN_POINT('Ctrl Pts',(-8.69177062728724,-14.4177207722467,
119.157312906758)) ;
#191963 = CARTESIAN_POINT('Ctrl Pts',(-8.61796681473128,-14.4177207562703,
119.18154404245)) ;
#191964 = CARTESIAN_POINT('Ctrl Pts',(-8.62151667785764,-14.4927692755206,
119.192356354701)) ;
#191965 = CARTESIAN_POINT('Ctrl Pts',(-8.62506654098401,-14.567817794771,
119.203168666952)) ;
#191966 = CARTESIAN_POINT('Ctrl Pts',(-8.69887035353998,-14.5678178107474,
119.17893753126)) ;
#191967 = CARTESIAN_POINT('Ctrl Pts',(-8.77267416609596,-14.5678178267238,
119.154706395567)) ;
#191968 = CARTESIAN_POINT('Ctrl Pts',(-8.76912430296958,-14.4927693074735,
119.143894083316)) ;
#191969 = CARTESIAN_POINT('Ctrl Pts',(-8.84564499663558,-14.4094376546516,
119.412427388764)) ;
#191970 = CARTESIAN_POINT('Ctrl Pts',(-8.83601350712255,-14.3400945271198,
119.383091423897)) ;
#191971 = CARTESIAN_POINT('Ctrl Pts',(-8.76220969078333,-14.3400944873417,
119.407322548066)) ;
#191972 = CARTESIAN_POINT('Ctrl Pts',(-8.68840587444411,-14.3400944475637,
119.431553672236)) ;
#191973 = CARTESIAN_POINT('Ctrl Pts',(-8.69803736395715,-14.4094375750955,
119.460889637102)) ;
#191974 = CARTESIAN_POINT('Ctrl Pts',(-8.70766885347021,-14.4787807026274,
119.490225601969)) ;
#191975 = CARTESIAN_POINT('Ctrl Pts',(-8.78147266980941,-14.4787807424054,
119.4659944778)) ;
#191976 = CARTESIAN_POINT('Ctrl Pts',(-8.85527648614863,-14.4787807821835,
119.44176335363)) ;
#191977 = CARTESIAN_POINT('Ctrl Pts',(-8.84564499663558,-14.4094376546516,
119.412427388764)) ;
#191978 = CARTESIAN_POINT('Ctrl Pts',(-8.91218973923486,-14.2549673486149,
119.650598079917)) ;
#191979 = CARTESIAN_POINT('Ctrl Pts',(-8.89716344705603,-14.1963046294673,
119.604830416691)) ;
#191980 = CARTESIAN_POINT('Ctrl Pts',(-8.82335962503793,-14.1963045717546,
119.629061523563)) ;
#191981 = CARTESIAN_POINT('Ctrl Pts',(-8.74955580301983,-14.1963045140418,
119.653292630436)) ;
#191982 = CARTESIAN_POINT('Ctrl Pts',(-8.76458209519867,-14.2549672331893,
119.699060293662)) ;
#191983 = CARTESIAN_POINT('Ctrl Pts',(-8.77960838737749,-14.3136299523368,
119.744827956887)) ;
#191984 = CARTESIAN_POINT('Ctrl Pts',(-8.85341220939561,-14.3136300100496,
119.720596850015)) ;
#191985 = CARTESIAN_POINT('Ctrl Pts',(-8.9272160314137,-14.3136300677624,
119.696365743142)) ;
#191986 = CARTESIAN_POINT('Ctrl Pts',(-8.91218973923486,-14.2549673486149,
119.650598079917)) ;
#191987 = CARTESIAN_POINT('Ctrl Pts',(-8.96309326723311,-14.0408502140836,
119.841068283191)) ;
#191988 = CARTESIAN_POINT('Ctrl Pts',(-8.94375726638346,-13.9970485144641,
119.782173942844)) ;
#191989 = CARTESIAN_POINT('Ctrl Pts',(-8.86995343771673,-13.9970484457834,
119.806405029466)) ;
#191990 = CARTESIAN_POINT('Ctrl Pts',(-8.79614960904997,-13.9970483771027,
119.830636116088)) ;
#191991 = CARTESIAN_POINT('Ctrl Pts',(-8.81548560989961,-14.0408500767222,
119.889530456434)) ;
#191992 = CARTESIAN_POINT('Ctrl Pts',(-8.83482161074924,-14.0846517763417,
119.948424796781)) ;
#191993 = CARTESIAN_POINT('Ctrl Pts',(-8.908625439416,-14.0846518450224,119.92419371016)) ;
#191994 = CARTESIAN_POINT('Ctrl Pts',(-8.98242926808274,-14.0846519137031,
119.899962623538)) ;
#191995 = CARTESIAN_POINT('Ctrl Pts',(-8.96309326723311,-14.0408502140836,
119.841068283191)) ;
#191996 = CARTESIAN_POINT('Ctrl Pts',(-8.99415259582093,-13.7824650273217,
119.971073817574)) ;
#191997 = CARTESIAN_POINT('Ctrl Pts',(-8.97188631073203,-13.7566374523408,
119.903254304363)) ;
#191998 = CARTESIAN_POINT('Ctrl Pts',(-8.89808247511074,-13.7566373798381,
119.927485369803)) ;
#191999 = CARTESIAN_POINT('Ctrl Pts',(-8.82427863948944,-13.7566373073354,
119.951716435242)) ;
#192000 = CARTESIAN_POINT('Ctrl Pts',(-8.84654492457835,-13.7824648823164,
120.019535948453)) ;
#192001 = CARTESIAN_POINT('Ctrl Pts',(-8.86881120966723,-13.8082924572973,
120.087355461664)) ;
#192002 = CARTESIAN_POINT('Ctrl Pts',(-8.94261504528854,-13.8082925298,120.063124396225)) ;
#192003 = CARTESIAN_POINT('Ctrl Pts',(-9.01641888090982,-13.8082926023027,
120.038893330785)) ;
#192004 = CARTESIAN_POINT('Ctrl Pts',(-8.99415259582093,-13.7824650273217,
119.971073817574)) ;
#192005 = CARTESIAN_POINT('Ctrl Pts',(-9.0023120554926,-13.4963851494492,
120.031528435387)) ;
#192006 = CARTESIAN_POINT('Ctrl Pts',(-8.97870554701302,-13.4904923432814,
119.959626818148)) ;
#192007 = CARTESIAN_POINT('Ctrl Pts',(-8.90490170488797,-13.4904922758106,
119.983857863778)) ;
#192008 = CARTESIAN_POINT('Ctrl Pts',(-8.83109786276295,-13.4904922083398,
120.008088909408)) ;
#192009 = CARTESIAN_POINT('Ctrl Pts',(-8.85470437124252,-13.4963850145077,
120.079990526647)) ;
#192010 = CARTESIAN_POINT('Ctrl Pts',(-8.87831087972213,-13.5022778206756,
120.151892143886)) ;
#192011 = CARTESIAN_POINT('Ctrl Pts',(-8.95211472184715,-13.5022778881464,
120.127661098256)) ;
#192012 = CARTESIAN_POINT('Ctrl Pts',(-9.02591856397219,-13.5022779556171,
120.103430052626)) ;
#192013 = CARTESIAN_POINT('Ctrl Pts',(-9.0023120554926,-13.4963851494492,
120.031528435387)) ;
#192014 = CARTESIAN_POINT('Ctrl Pts',(-8.98624034471568,-13.2068554623175,
120.017906636824)) ;
#192015 = CARTESIAN_POINT('Ctrl Pts',(-8.96298924945921,-13.2211688965324,
119.947087551054)) ;
#192016 = CARTESIAN_POINT('Ctrl Pts',(-8.88918540217969,-13.2211688373046,
119.971318580984)) ;
#192017 = CARTESIAN_POINT('Ctrl Pts',(-8.81538155490015,-13.2211687780768,
119.995549610914)) ;
#192018 = CARTESIAN_POINT('Ctrl Pts',(-8.83863265015661,-13.2068553438618,
120.066368696685)) ;
#192019 = CARTESIAN_POINT('Ctrl Pts',(-8.86188374541307,-13.1925419096468,
120.137187782455)) ;
#192020 = CARTESIAN_POINT('Ctrl Pts',(-8.93568759269262,-13.1925419688746,
120.112956752525)) ;
#192021 = CARTESIAN_POINT('Ctrl Pts',(-9.00949143997215,-13.1925420281025,
120.088725722595)) ;
#192022 = CARTESIAN_POINT('Ctrl Pts',(-8.98624034471568,-13.2068554623175,
120.017906636824)) ;
#192023 = CARTESIAN_POINT('Ctrl Pts',(-8.946364301955,-12.9311896303103,119.931928817403)) ;
#192024 = CARTESIAN_POINT('Ctrl Pts',(-8.9251279617825,-12.9647719930566,
119.867246350707)) ;
#192025 = CARTESIAN_POINT('Ctrl Pts',(-8.85132411089623,-12.9647719471212,
119.891477369652)) ;
#192026 = CARTESIAN_POINT('Ctrl Pts',(-8.77752026000998,-12.9647719011858,
119.915708388597)) ;
#192027 = CARTESIAN_POINT('Ctrl Pts',(-8.79875660018247,-12.9311895384395,
119.980390855293)) ;
#192028 = CARTESIAN_POINT('Ctrl Pts',(-8.81999294035498,-12.8976071756931,
120.045073321988)) ;
#192029 = CARTESIAN_POINT('Ctrl Pts',(-8.89379679124124,-12.8976072216285,
120.020842303044)) ;
#192030 = CARTESIAN_POINT('Ctrl Pts',(-8.9676006421275,-12.8976072675639,
119.996611284099)) ;
#192031 = CARTESIAN_POINT('Ctrl Pts',(-8.946364301955,-12.9311896303103,119.931928817403)) ;
#192032 = CARTESIAN_POINT('Ctrl Pts',(-8.88452827451557,-12.6901579122719,
119.779127065873)) ;
#192033 = CARTESIAN_POINT('Ctrl Pts',(-8.86684171688226,-12.7406206917642,
119.72525666422)) ;
#192034 = CARTESIAN_POINT('Ctrl Pts',(-8.79303786446268,-12.7406206607923,
119.749487678494)) ;
#192035 = CARTESIAN_POINT('Ctrl Pts',(-8.71923401204311,-12.7406206298204,
119.773718692769)) ;
#192036 = CARTESIAN_POINT('Ctrl Pts',(-8.73692056967643,-12.6901578503282,
119.827589094422)) ;
#192037 = CARTESIAN_POINT('Ctrl Pts',(-8.75460712730975,-12.639695070836,
119.881459496076)) ;
#192038 = CARTESIAN_POINT('Ctrl Pts',(-8.82841097972933,-12.6396951018078,
119.857228481802)) ;
#192039 = CARTESIAN_POINT('Ctrl Pts',(-8.9022148321489,-12.6396951327797,
119.832997467527)) ;
#192040 = CARTESIAN_POINT('Ctrl Pts',(-8.88452827451557,-12.6901579122719,
119.779127065873)) ;
#192041 = CARTESIAN_POINT('Ctrl Pts',(-8.80498155763684,-12.5020099307821,
119.572221904851)) ;
#192042 = CARTESIAN_POINT('Ctrl Pts',(-8.79209020285993,-12.5656860202673,
119.532956917547)) ;
#192043 = CARTESIAN_POINT('Ctrl Pts',(-8.71828635025744,-12.565686002392,
119.557187931264)) ;
#192044 = CARTESIAN_POINT('Ctrl Pts',(-8.64448249765493,-12.5656859845167,
119.581418944981)) ;
#192045 = CARTESIAN_POINT('Ctrl Pts',(-8.65737385243184,-12.5020098950315,
119.620683932286)) ;
#192046 = CARTESIAN_POINT('Ctrl Pts',(-8.67026520720871,-12.4383338055463,
119.65994891959)) ;
#192047 = CARTESIAN_POINT('Ctrl Pts',(-8.74406905981123,-12.4383338234216,
119.635717905873)) ;
#192048 = CARTESIAN_POINT('Ctrl Pts',(-8.81787291241371,-12.4383338412968,
119.611486892155)) ;
#192049 = CARTESIAN_POINT('Ctrl Pts',(-8.80498155763684,-12.5020099307821,
119.572221904851)) ;
#192050 = CARTESIAN_POINT('Ctrl Pts',(-8.7115619119402,-12.3786471033838,
119.32335220504)) ;
#192051 = CARTESIAN_POINT('Ctrl Pts',(-8.70443569741749,-12.451033969766,
119.301646904946)) ;
#192052 = CARTESIAN_POINT('Ctrl Pts',(-8.630631846706,-12.4510339632927,119.325877924423)) ;
#192053 = CARTESIAN_POINT('Ctrl Pts',(-8.55682799599452,-12.4510339568193,
119.3501089439)) ;
#192054 = CARTESIAN_POINT('Ctrl Pts',(-8.56395421051721,-12.378647090437,
119.371814243995)) ;
#192055 = CARTESIAN_POINT('Ctrl Pts',(-8.57108042503996,-12.3062602240548,
119.393519544089)) ;
#192056 = CARTESIAN_POINT('Ctrl Pts',(-8.64488427575143,-12.3062602305281,
119.369288524612)) ;
#192057 = CARTESIAN_POINT('Ctrl Pts',(-8.71868812646292,-12.3062602370015,
119.345057505135)) ;
#192058 = CARTESIAN_POINT('Ctrl Pts',(-8.7115619119402,-12.3786471033838,
119.32335220504)) ;
#192059 = CARTESIAN_POINT('Ctrl Pts',(-8.61202742108512,-12.3306796608346,
119.055450282701)) ;
#192060 = CARTESIAN_POINT('Ctrl Pts',(-8.61111059814198,-12.4065247391554,
119.052657787592)) ;
#192061 = CARTESIAN_POINT('Ctrl Pts',(-8.53730674903535,-12.4065247391449,
119.076888811957)) ;
#192062 = CARTESIAN_POINT('Ctrl Pts',(-8.46350289992872,-12.4065247391344,
119.101119836322)) ;
#192063 = CARTESIAN_POINT('Ctrl Pts',(-8.46441972287187,-12.3306796608136,
119.103912331432)) ;
#192064 = CARTESIAN_POINT('Ctrl Pts',(-8.46533654581499,-12.2548345824928,
119.106704826541)) ;
#192065 = CARTESIAN_POINT('Ctrl Pts',(-8.53914039492163,-12.2548345825033,
119.082473802176)) ;
#192066 = CARTESIAN_POINT('Ctrl Pts',(-8.61294424402827,-12.2548345825139,
119.05824277781)) ;
#192067 = CARTESIAN_POINT('Ctrl Pts',(-8.61202742108512,-12.3306796608346,
119.055450282701)) ;
#192068 = CARTESIAN_POINT('Ctrl Pts',(-8.51084890152702,-12.360155377245,
118.782851948086)) ;
#192069 = CARTESIAN_POINT('Ctrl Pts',(-8.51625934876444,-12.4340571826112,
118.799331297198)) ;
#192070 = CARTESIAN_POINT('Ctrl Pts',(-8.44245550224552,-12.4340571856698,
118.823562329445)) ;
#192071 = CARTESIAN_POINT('Ctrl Pts',(-8.36865165572661,-12.4340571887285,
118.847793361692)) ;
#192072 = CARTESIAN_POINT('Ctrl Pts',(-8.36324120848917,-12.3601553833623,
118.83131401258)) ;
#192073 = CARTESIAN_POINT('Ctrl Pts',(-8.35783076125176,-12.2862535779961,
118.814834663468)) ;
#192074 = CARTESIAN_POINT('Ctrl Pts',(-8.43163460777068,-12.2862535749374,
118.790603631221)) ;
#192075 = CARTESIAN_POINT('Ctrl Pts',(-8.5054384542896,-12.2862535718788,
118.766372598974)) ;
#192076 = CARTESIAN_POINT('Ctrl Pts',(-8.51084890152702,-12.360155377245,
118.782851948086)) ;
#192077 = CARTESIAN_POINT('Ctrl Pts',(-8.41582654585043,-12.4653999327267,
118.52883086794)) ;
#192078 = CARTESIAN_POINT('Ctrl Pts',(-8.42714754368904,-12.5320640126139,
118.563312800623)) ;
#192079 = CARTESIAN_POINT('Ctrl Pts',(-8.35334369898756,-12.5320640153815,
118.587543838406)) ;
#192080 = CARTESIAN_POINT('Ctrl Pts',(-8.27953985428609,-12.5320640181491,
118.611774876189)) ;
#192081 = CARTESIAN_POINT('Ctrl Pts',(-8.26821885644749,-12.4653999382619,
118.577292943505)) ;
#192082 = CARTESIAN_POINT('Ctrl Pts',(-8.25689785860889,-12.3987358583746,
118.542811010821)) ;
#192083 = CARTESIAN_POINT('Ctrl Pts',(-8.33070170331036,-12.398735855607,
118.518579973038)) ;
#192084 = CARTESIAN_POINT('Ctrl Pts',(-8.40450554801183,-12.3987358528394,
118.494348935256)) ;
#192085 = CARTESIAN_POINT('Ctrl Pts',(-8.41582654585043,-12.4653999327267,
118.52883086794)) ;
#192086 = CARTESIAN_POINT('Ctrl Pts',(-8.33239181332137,-12.6388027493961,
118.310157345988)) ;
#192087 = CARTESIAN_POINT('Ctrl Pts',(-8.34882205720498,-12.6934585985942,
118.360201217838)) ;
#192088 = CARTESIAN_POINT('Ctrl Pts',(-8.2750182137703,-12.6934585991624,
118.38443225948)) ;
#192089 = CARTESIAN_POINT('Ctrl Pts',(-8.20121437033563,-12.6934585997305,
118.408663301121)) ;
#192090 = CARTESIAN_POINT('Ctrl Pts',(-8.18478412645201,-12.6388027505324,
118.35861942927)) ;
#192091 = CARTESIAN_POINT('Ctrl Pts',(-8.1683538825684,-12.5841469013344,
118.308575557419)) ;
#192092 = CARTESIAN_POINT('Ctrl Pts',(-8.24215772600308,-12.5841469007662,
118.284344515778)) ;
#192093 = CARTESIAN_POINT('Ctrl Pts',(-8.31596156943775,-12.584146900198,
118.260113474137)) ;
#192094 = CARTESIAN_POINT('Ctrl Pts',(-8.33239181332137,-12.6388027493961,
118.310157345988)) ;
#192095 = CARTESIAN_POINT('Ctrl Pts',(-8.26591621181812,-12.8679196576227,
118.143124187206)) ;
#192096 = CARTESIAN_POINT('Ctrl Pts',(-8.28627939353487,-12.9066583901742,
118.205147153176)) ;
#192097 = CARTESIAN_POINT('Ctrl Pts',(-8.21247555056549,-12.9066583881138,
118.229378196234)) ;
#192098 = CARTESIAN_POINT('Ctrl Pts',(-8.13867170759611,-12.9066583860534,
118.253609239292)) ;
#192099 = CARTESIAN_POINT('Ctrl Pts',(-8.11830852587934,-12.8679196535019,
118.191586273322)) ;
#192100 = CARTESIAN_POINT('Ctrl Pts',(-8.09794534416259,-12.8291809209503,
118.129563307352)) ;
#192101 = CARTESIAN_POINT('Ctrl Pts',(-8.17174918713197,-12.8291809230107,
118.105332264294)) ;
#192102 = CARTESIAN_POINT('Ctrl Pts',(-8.24555303010134,-12.8291809250711,
118.081101221236)) ;
#192103 = CARTESIAN_POINT('Ctrl Pts',(-8.26591621181812,-12.8679196576227,
118.143124187206)) ;
#192104 = CARTESIAN_POINT('Ctrl Pts',(-8.22030810185899,-13.1373001966588,
118.039762360663)) ;
#192105 = CARTESIAN_POINT('Ctrl Pts',(-8.24315064156721,-13.1572855705815,
118.109337051049)) ;
#192106 = CARTESIAN_POINT('Ctrl Pts',(-8.16934679842566,-13.1572855672865,
118.133568093583)) ;
#192107 = CARTESIAN_POINT('Ctrl Pts',(-8.0955429552841,-13.1572855639915,
118.157799136117)) ;
#192108 = CARTESIAN_POINT('Ctrl Pts',(-8.07270041557589,-13.1373001900688,
118.08822444573)) ;
#192109 = CARTESIAN_POINT('Ctrl Pts',(-8.04985787586767,-13.1173148161461,
118.018649755344)) ;
#192110 = CARTESIAN_POINT('Ctrl Pts',(-8.12366171900923,-13.1173148194411,
117.99441871281)) ;
#192111 = CARTESIAN_POINT('Ctrl Pts',(-8.19746556215078,-13.1173148227361,
117.970187670276)) ;
#192112 = CARTESIAN_POINT('Ctrl Pts',(-8.22030810185899,-13.1373001966588,
118.039762360663)) ;
#192113 = CARTESIAN_POINT('Ctrl Pts',(-8.19835036718157,-13.4255234275119,
118.008268887877)) ;
#192114 = CARTESIAN_POINT('Ctrl Pts',(-8.22202747304424,-13.425412168657,
118.080385532087)) ;
#192115 = CARTESIAN_POINT('Ctrl Pts',(-8.14822362956311,-13.4254121666008,
118.104616573587)) ;
#192116 = CARTESIAN_POINT('Ctrl Pts',(-8.07441978608198,-13.4254121645446,
118.128847615087)) ;
#192117 = CARTESIAN_POINT('Ctrl Pts',(-8.05074268021931,-13.4255234233994,
118.056730970876)) ;
#192118 = CARTESIAN_POINT('Ctrl Pts',(-8.02706557435661,-13.4256346822543,
117.984614326666)) ;
#192119 = CARTESIAN_POINT('Ctrl Pts',(-8.10086941783775,-13.4256346843105,
117.960383285166)) ;
#192120 = CARTESIAN_POINT('Ctrl Pts',(-8.17467326131888,-13.4256346863667,
117.936152243667)) ;
#192121 = CARTESIAN_POINT('Ctrl Pts',(-8.19835036718157,-13.4255234275119,
118.008268887877)) ;
#192122 = CARTESIAN_POINT('Ctrl Pts',(-8.20061003959541,-13.7140381962048,
118.050644598093)) ;
#192123 = CARTESIAN_POINT('Ctrl Pts',(-8.22342961676016,-13.6937806023833,
118.120149348188)) ;
#192124 = CARTESIAN_POINT('Ctrl Pts',(-8.14962577334613,-13.6937806037046,
118.144380389892)) ;
#192125 = CARTESIAN_POINT('Ctrl Pts',(-8.07582192993207,-13.6937806050258,
118.168611431595)) ;
#192126 = CARTESIAN_POINT('Ctrl Pts',(-8.05300235276731,-13.7140381988474,
118.099106681501)) ;
#192127 = CARTESIAN_POINT('Ctrl Pts',(-8.03018277560256,-13.7342957926689,
118.029601931407)) ;
#192128 = CARTESIAN_POINT('Ctrl Pts',(-8.10398661901661,-13.7342957913476,
118.005370889703)) ;
#192129 = CARTESIAN_POINT('Ctrl Pts',(-8.17779046243066,-13.7342957900263,
117.981139847999)) ;
#192130 = CARTESIAN_POINT('Ctrl Pts',(-8.20061003959541,-13.7140381962048,
118.050644598093)) ;
#192131 = CARTESIAN_POINT('Ctrl Pts',(-8.2262886533452,-13.981013641758,118.164309383492)) ;
#192132 = CARTESIAN_POINT('Ctrl Pts',(-8.2466148823236,-13.9420847851826,
118.226219797217)) ;
#192133 = CARTESIAN_POINT('Ctrl Pts',(-8.17281103977456,-13.9420847906692,
118.250450841556)) ;
#192134 = CARTESIAN_POINT('Ctrl Pts',(-8.09900719722553,-13.9420847961559,
118.274681885894)) ;
#192135 = CARTESIAN_POINT('Ctrl Pts',(-8.07868096824714,-13.9810136527313,
118.21277147217)) ;
#192136 = CARTESIAN_POINT('Ctrl Pts',(-8.05835473926874,-14.0199425093067,
118.150861058445)) ;
#192137 = CARTESIAN_POINT('Ctrl Pts',(-8.13215858181778,-14.01994250382,118.126630014106)) ;
#192138 = CARTESIAN_POINT('Ctrl Pts',(-8.2059624243668,-14.0199424983334,
118.102398969767)) ;
#192139 = CARTESIAN_POINT('Ctrl Pts',(-8.2262886533452,-13.981013641758,118.164309383492)) ;
#192140 = CARTESIAN_POINT('Ctrl Pts',(-8.27273205955447,-14.2077526521797,
118.341223296335)) ;
#192141 = CARTESIAN_POINT('Ctrl Pts',(-8.28911130746513,-14.1529353062713,
118.391111842453)) ;
#192142 = CARTESIAN_POINT('Ctrl Pts',(-8.21530746668232,-14.1529353151086,
118.415342892171)) ;
#192143 = CARTESIAN_POINT('Ctrl Pts',(-8.14150362589951,-14.1529353239459,
118.43957394189)) ;
#192144 = CARTESIAN_POINT('Ctrl Pts',(-8.12512437798886,-14.2077526698542,
118.389685395771)) ;
#192145 = CARTESIAN_POINT('Ctrl Pts',(-8.10874513007819,-14.2625700157626,
118.339796849653)) ;
#192146 = CARTESIAN_POINT('Ctrl Pts',(-8.182548970861,-14.2625700069253,118.315565799935)) ;
#192147 = CARTESIAN_POINT('Ctrl Pts',(-8.25635281164381,-14.2625699980881,
118.291334750216)) ;
#192148 = CARTESIAN_POINT('Ctrl Pts',(-8.27273205955447,-14.2077526521797,
118.341223296335)) ;
#192149 = CARTESIAN_POINT('Ctrl Pts',(-8.33605388433727,-14.3782190485839,
118.569622801418)) ;
#192150 = CARTESIAN_POINT('Ctrl Pts',(-8.347300341461,-14.3114194784183,118.603877694822)) ;
#192151 = CARTESIAN_POINT('Ctrl Pts',(-8.27349650343915,-14.3114194884178,
118.62810875295)) ;
#192152 = CARTESIAN_POINT('Ctrl Pts',(-8.19969266541728,-14.3114194984174,
118.652339811078)) ;
#192153 = CARTESIAN_POINT('Ctrl Pts',(-8.18844620829354,-14.378219068583,
118.618084917674)) ;
#192154 = CARTESIAN_POINT('Ctrl Pts',(-8.1771997511698,-14.4450186387486,
118.583830024269)) ;
#192155 = CARTESIAN_POINT('Ctrl Pts',(-8.25100358919167,-14.445018628749,
118.559598966142)) ;
#192156 = CARTESIAN_POINT('Ctrl Pts',(-8.32480742721352,-14.4450186187495,
118.535367908014)) ;
#192157 = CARTESIAN_POINT('Ctrl Pts',(-8.33605388433727,-14.3782190485839,
118.569622801418)) ;
#192158 = CARTESIAN_POINT('Ctrl Pts',(-8.41067546930047,-14.4794481619843,
118.832358521227)) ;
#192159 = CARTESIAN_POINT('Ctrl Pts',(-8.41599441965751,-14.4054839121495,
118.848559185268)) ;
#192160 = CARTESIAN_POINT('Ctrl Pts',(-8.34219058465964,-14.4054839189219,
118.872790252606)) ;
#192161 = CARTESIAN_POINT('Ctrl Pts',(-8.26838674966178,-14.4054839256943,
118.897021319945)) ;
#192162 = CARTESIAN_POINT('Ctrl Pts',(-8.26306779930477,-14.4794481755291,
118.880820655904)) ;
#192163 = CARTESIAN_POINT('Ctrl Pts',(-8.25774884894772,-14.5534124253639,
118.864619991863)) ;
#192164 = CARTESIAN_POINT('Ctrl Pts',(-8.33155268394558,-14.5534124185915,
118.840388924525)) ;
#192165 = CARTESIAN_POINT('Ctrl Pts',(-8.40535651894344,-14.5534124118191,
118.816157857186)) ;
#192166 = CARTESIAN_POINT('Ctrl Pts',(-8.41067546930047,-14.4794481619843,
118.832358521227)) ;
#192167 = CARTESIAN_POINT('Ctrl Pts',(-8.49060294650496,-14.5047934992133,
119.111248928823)) ;
#192168 = CARTESIAN_POINT('Ctrl Pts',(-8.48961555716104,-14.4289527181918,
119.1082414995)) ;
#192169 = CARTESIAN_POINT('Ctrl Pts',(-8.41581172498398,-14.4289527172552,
119.13247257543)) ;
#192170 = CARTESIAN_POINT('Ctrl Pts',(-8.34200789280688,-14.4289527163185,
119.15670365136)) ;
#192171 = CARTESIAN_POINT('Ctrl Pts',(-8.34299528215081,-14.5047934973399,
119.159711080683)) ;
#192172 = CARTESIAN_POINT('Ctrl Pts',(-8.34398267149472,-14.5806342783613,
119.162718510006)) ;
#192173 = CARTESIAN_POINT('Ctrl Pts',(-8.41778650367179,-14.580634279298,
119.138487434076)) ;
#192174 = CARTESIAN_POINT('Ctrl Pts',(-8.49159033584886,-14.5806342802347,
119.114256358146)) ;
#192175 = CARTESIAN_POINT('Ctrl Pts',(-8.49060294650496,-14.5047934992133,
119.111248928823)) ;
#192176 = CARTESIAN_POINT('Ctrl Pts',(-8.56952664834317,-14.4522183736054,
119.387142880941)) ;
#192177 = CARTESIAN_POINT('Ctrl Pts',(-8.56229269511265,-14.3799386549208,
119.365109425723)) ;
#192178 = CARTESIAN_POINT('Ctrl Pts',(-8.48848886515389,-14.3799386416776,
119.38934050841)) ;
#192179 = CARTESIAN_POINT('Ctrl Pts',(-8.41468503519511,-14.3799386284344,
119.413571591096)) ;
#192180 = CARTESIAN_POINT('Ctrl Pts',(-8.42191898842563,-14.452218347119,
119.435605046314)) ;
#192181 = CARTESIAN_POINT('Ctrl Pts',(-8.42915294165614,-14.5244980658035,
119.457638501531)) ;
#192182 = CARTESIAN_POINT('Ctrl Pts',(-8.50295677161491,-14.5244980790467,
119.433407418845)) ;
#192183 = CARTESIAN_POINT('Ctrl Pts',(-8.57676060157369,-14.5244980922899,
119.409176336158)) ;
#192184 = CARTESIAN_POINT('Ctrl Pts',(-8.56952664834317,-14.4522183736054,
119.387142880941)) ;
#192185 = CARTESIAN_POINT('Ctrl Pts',(-8.64082192792583,-14.3254100791536,
119.639777714158)) ;
#192186 = CARTESIAN_POINT('Ctrl Pts',(-8.62786556152258,-14.2618795112896,
119.600314711553)) ;
#192187 = CARTESIAN_POINT('Ctrl Pts',(-8.5540617322727,-14.2618794820993,
119.624545796399)) ;
#192188 = CARTESIAN_POINT('Ctrl Pts',(-8.48025790302279,-14.261879452909,
119.648776881244)) ;
#192189 = CARTESIAN_POINT('Ctrl Pts',(-8.49321426942607,-14.325410020773,
119.68823988385)) ;
#192190 = CARTESIAN_POINT('Ctrl Pts',(-8.50617063582931,-14.3889405886369,
119.727702886455)) ;
#192191 = CARTESIAN_POINT('Ctrl Pts',(-8.57997446507921,-14.3889406178272,
119.703471801609)) ;
#192192 = CARTESIAN_POINT('Ctrl Pts',(-8.6537782943291,-14.3889406470175,
119.679240716764)) ;
#192193 = CARTESIAN_POINT('Ctrl Pts',(-8.64082192792583,-14.3254100791536,
119.639777714158)) ;
#192194 = CARTESIAN_POINT('Ctrl Pts',(-8.69855299299028,-14.1342773327245,
119.850992494174)) ;
#192195 = CARTESIAN_POINT('Ctrl Pts',(-8.68081527062798,-14.0839997344191,
119.796966252638)) ;
#192196 = CARTESIAN_POINT('Ctrl Pts',(-8.60701144003505,-14.0839996884698,
119.821197333393)) ;
#192197 = CARTESIAN_POINT('Ctrl Pts',(-8.53320760944215,-14.0839996425206,
119.845428414148)) ;
#192198 = CARTESIAN_POINT('Ctrl Pts',(-8.55094533180445,-14.134277240826,
119.899454655684)) ;
#192199 = CARTESIAN_POINT('Ctrl Pts',(-8.56868305416677,-14.1845548391315,
119.95348089722)) ;
#192200 = CARTESIAN_POINT('Ctrl Pts',(-8.64248688475969,-14.1845548850807,
119.929249816465)) ;
#192201 = CARTESIAN_POINT('Ctrl Pts',(-8.7162907153526,-14.18455493103,119.90501873571)) ;
#192202 = CARTESIAN_POINT('Ctrl Pts',(-8.69855299299028,-14.1342773327245,
119.850992494174)) ;
#192203 = CARTESIAN_POINT('Ctrl Pts',(-8.73823026219567,-13.8911855385649,
120.007348076147)) ;
#192204 = CARTESIAN_POINT('Ctrl Pts',(-8.71696200923995,-13.8578071985554,
119.942568407905)) ;
#192205 = CARTESIAN_POINT('Ctrl Pts',(-8.64315817558926,-13.8578071355948,
119.966799479347)) ;
#192206 = CARTESIAN_POINT('Ctrl Pts',(-8.56935434193856,-13.8578070726341,
119.991030550788)) ;
#192207 = CARTESIAN_POINT('Ctrl Pts',(-8.59062259489427,-13.8911854126436,
120.05581021903)) ;
#192208 = CARTESIAN_POINT('Ctrl Pts',(-8.61189084784997,-13.9245637526531,
120.120589887271)) ;
#192209 = CARTESIAN_POINT('Ctrl Pts',(-8.68569468150069,-13.9245638156137,
120.09635881583)) ;
#192210 = CARTESIAN_POINT('Ctrl Pts',(-8.75949851515137,-13.9245638785744,
120.072127744389)) ;
#192211 = CARTESIAN_POINT('Ctrl Pts',(-8.73823026219567,-13.8911855385649,
120.007348076147)) ;
#192212 = CARTESIAN_POINT('Ctrl Pts',(-8.75589442615831,-13.6134122049751,
120.096730914448)) ;
#192213 = CARTESIAN_POINT('Ctrl Pts',(-8.73262575513511,-13.5993787020081,
120.025858295372)) ;
#192214 = CARTESIAN_POINT('Ctrl Pts',(-8.65882191632523,-13.5993786244693,
120.050089351099)) ;
#192215 = CARTESIAN_POINT('Ctrl Pts',(-8.58501807751536,-13.5993785469305,
120.074320406827)) ;
#192216 = CARTESIAN_POINT('Ctrl Pts',(-8.60828674853857,-13.6134120498975,
120.145193025903)) ;
#192217 = CARTESIAN_POINT('Ctrl Pts',(-8.63155541956179,-13.6274455528644,
120.216065644979)) ;
#192218 = CARTESIAN_POINT('Ctrl Pts',(-8.70535925837165,-13.6274456304033,
120.191834589251)) ;
#192219 = CARTESIAN_POINT('Ctrl Pts',(-8.77916309718153,-13.6274457079421,
120.167603533524)) ;
#192220 = CARTESIAN_POINT('Ctrl Pts',(-8.75589442615831,-13.6134122049751,
120.096730914448)) ;
#192221 = CARTESIAN_POINT('Ctrl Pts',(-8.74967783452186,-13.3239481087795,
120.113088049486)) ;
#192222 = CARTESIAN_POINT('Ctrl Pts',(-8.72607932381083,-13.3301038926875,
120.041210791831)) ;
#192223 = CARTESIAN_POINT('Ctrl Pts',(-8.65227547827315,-13.3301038083537,
120.065441827067)) ;
#192224 = CARTESIAN_POINT('Ctrl Pts',(-8.57847163273545,-13.3301037240199,
120.089672862302)) ;
#192225 = CARTESIAN_POINT('Ctrl Pts',(-8.60207014344647,-13.3239479401119,
120.161550119957)) ;
#192226 = CARTESIAN_POINT('Ctrl Pts',(-8.62566865415748,-13.3177921562039,
120.233427377612)) ;
#192227 = CARTESIAN_POINT('Ctrl Pts',(-8.69947249969519,-13.3177922405377,
120.209196342377)) ;
#192228 = CARTESIAN_POINT('Ctrl Pts',(-8.77327634523286,-13.3177923248715,
120.184965307141)) ;
#192229 = CARTESIAN_POINT('Ctrl Pts',(-8.74967783452186,-13.3239481087795,
120.113088049486)) ;
#192230 = CARTESIAN_POINT('Ctrl Pts',(-8.71923606193324,-13.0394391601657,
120.05588628759)) ;
#192231 = CARTESIAN_POINT('Ctrl Pts',(-8.69699356662627,-13.0654672913968,
119.988139233932)) ;
#192232 = CARTESIAN_POINT('Ctrl Pts',(-8.62318971345324,-13.0654672055952,
120.012370245912)) ;
#192233 = CARTESIAN_POINT('Ctrl Pts',(-8.54938586028022,-13.0654671197937,
120.036601257892)) ;
#192234 = CARTESIAN_POINT('Ctrl Pts',(-8.57162835558722,-13.0394389885626,
120.104348311549)) ;
#192235 = CARTESIAN_POINT('Ctrl Pts',(-8.59387085089422,-13.0134108573315,
120.172095365206)) ;
#192236 = CARTESIAN_POINT('Ctrl Pts',(-8.66767470406722,-13.0134109431331,
120.147864353226)) ;
#192237 = CARTESIAN_POINT('Ctrl Pts',(-8.74147855724025,-13.0134110289346,
120.123633341247)) ;
#192238 = CARTESIAN_POINT('Ctrl Pts',(-8.71923606193324,-13.0394391601657,
120.05588628759)) ;
#192239 = CARTESIAN_POINT('Ctrl Pts',(-8.66606319630121,-12.7825526473998,
119.929370423015)) ;
#192240 = CARTESIAN_POINT('Ctrl Pts',(-8.64676730794358,-12.8265535642734,
119.870598258589)) ;
#192241 = CARTESIAN_POINT('Ctrl Pts',(-8.57296344702554,-12.8265534855134,
119.894829246979)) ;
#192242 = CARTESIAN_POINT('Ctrl Pts',(-8.49915958610749,-12.8265534067534,
119.919060235368)) ;
#192243 = CARTESIAN_POINT('Ctrl Pts',(-8.5184554744651,-12.7825524898798,
119.977832399794)) ;
#192244 = CARTESIAN_POINT('Ctrl Pts',(-8.53775136282272,-12.7385515730062,
120.03660456422)) ;
#192245 = CARTESIAN_POINT('Ctrl Pts',(-8.61155522374078,-12.7385516517662,
120.012373575831)) ;
#192246 = CARTESIAN_POINT('Ctrl Pts',(-8.68535908465883,-12.7385517305262,
119.988142587441)) ;
#192247 = CARTESIAN_POINT('Ctrl Pts',(-8.66606319630121,-12.7825526473998,
119.929370423015)) ;
#192248 = CARTESIAN_POINT('Ctrl Pts',(-8.59271043085412,-12.5702685769134,
119.741585147016)) ;
#192249 = CARTESIAN_POINT('Ctrl Pts',(-8.57777001188604,-12.6291549421708,
119.696079039497)) ;
#192250 = CARTESIAN_POINT('Ctrl Pts',(-8.50396614376988,-12.629154878069,
119.720310005963)) ;
#192251 = CARTESIAN_POINT('Ctrl Pts',(-8.43016227565372,-12.6291548139673,
119.744540972428)) ;
#192252 = CARTESIAN_POINT('Ctrl Pts',(-8.44510269462181,-12.57026844871,119.790047079946)) ;
#192253 = CARTESIAN_POINT('Ctrl Pts',(-8.46004311358988,-12.5113820834526,
119.835553187465)) ;
#192254 = CARTESIAN_POINT('Ctrl Pts',(-8.53384698170604,-12.5113821475544,
119.811322221)) ;
#192255 = CARTESIAN_POINT('Ctrl Pts',(-8.6076508498222,-12.5113822116561,
119.787091254535)) ;
#192256 = CARTESIAN_POINT('Ctrl Pts',(-8.59271043085412,-12.5702685769134,
119.741585147016)) ;
#192257 = CARTESIAN_POINT('Ctrl Pts',(-8.50491328859232,-12.4204037087553,
119.509450907549)) ;
#192258 = CARTESIAN_POINT('Ctrl Pts',(-8.4953507374057,-12.4898390976006,
119.480324917526)) ;
#192259 = CARTESIAN_POINT('Ctrl Pts',(-8.42154686411292,-12.4898390557385,
119.504555868224)) ;
#192260 = CARTESIAN_POINT('Ctrl Pts',(-8.34774299082012,-12.4898390138765,
119.528786818922)) ;
#192261 = CARTESIAN_POINT('Ctrl Pts',(-8.35730554200674,-12.4204036250312,
119.557912808945)) ;
#192262 = CARTESIAN_POINT('Ctrl Pts',(-8.36686809319335,-12.3509682361859,
119.587038798968)) ;
#192263 = CARTESIAN_POINT('Ctrl Pts',(-8.44067196648614,-12.3509682780479,
119.56280784827)) ;
#192264 = CARTESIAN_POINT('Ctrl Pts',(-8.51447583977895,-12.35096831991,119.538576897572)) ;
#192265 = CARTESIAN_POINT('Ctrl Pts',(-8.50491328859232,-12.4204037087553,
119.509450907549)) ;
#192266 = CARTESIAN_POINT('Ctrl Pts',(-8.40683399712527,-12.3408608148814,
119.246251031593)) ;
#192267 = CARTESIAN_POINT('Ctrl Pts',(-8.4033695857143,-12.4159518832881,
119.235698991346)) ;
#192268 = CARTESIAN_POINT('Ctrl Pts',(-8.32956570922843,-12.4159518680668,
119.259929932318)) ;
#192269 = CARTESIAN_POINT('Ctrl Pts',(-8.25576183274256,-12.4159518528455,
119.28416087329)) ;
#192270 = CARTESIAN_POINT('Ctrl Pts',(-8.25922624415353,-12.3408607844389,
119.294712913538)) ;
#192271 = CARTESIAN_POINT('Ctrl Pts',(-8.2626906555645,-12.2657697160322,
119.305264953785)) ;
#192272 = CARTESIAN_POINT('Ctrl Pts',(-8.33649453205038,-12.2657697312535,
119.281034012813)) ;
#192273 = CARTESIAN_POINT('Ctrl Pts',(-8.41029840853624,-12.2657697464747,
119.256803071841)) ;
#192274 = CARTESIAN_POINT('Ctrl Pts',(-8.40683399712527,-12.3408608148814,
119.246251031593)) ;
#192275 = CARTESIAN_POINT('Ctrl Pts',(-8.30571590982397,-12.3387915853932,
118.973648699883)) ;
#192276 = CARTESIAN_POINT('Ctrl Pts',(-8.30857389731344,-12.414137720195,
118.98235366655)) ;
#192277 = CARTESIAN_POINT('Ctrl Pts',(-8.23477002042433,-12.4141377338266,
119.006584606295)) ;
#192278 = CARTESIAN_POINT('Ctrl Pts',(-8.16096614353523,-12.4141377474583,
119.030815546039)) ;
#192279 = CARTESIAN_POINT('Ctrl Pts',(-8.15810815604576,-12.3387916126566,
119.022110579371)) ;
#192280 = CARTESIAN_POINT('Ctrl Pts',(-8.15525016855628,-12.2634454778548,
119.013405612704)) ;
#192281 = CARTESIAN_POINT('Ctrl Pts',(-8.22905404544539,-12.2634454642232,
118.98917467296)) ;
#192282 = CARTESIAN_POINT('Ctrl Pts',(-8.3028579223345,-12.2634454505915,
118.964943733216)) ;
#192283 = CARTESIAN_POINT('Ctrl Pts',(-8.30571590982397,-12.3387915853932,
118.973648699883)) ;
#192284 = CARTESIAN_POINT('Ctrl Pts',(-8.20736927607411,-12.4137122483728,
118.709584594176)) ;
#192285 = CARTESIAN_POINT('Ctrl Pts',(-8.2163634416192,-12.4839393117036,
118.736979369127)) ;
#192286 = CARTESIAN_POINT('Ctrl Pts',(-8.14255956699891,-12.4839393535464,
118.761210315782)) ;
#192287 = CARTESIAN_POINT('Ctrl Pts',(-8.06875569237863,-12.4839393953892,
118.785441262436)) ;
#192288 = CARTESIAN_POINT('Ctrl Pts',(-8.05976152683357,-12.4137123320584,
118.758046487485)) ;
#192289 = CARTESIAN_POINT('Ctrl Pts',(-8.05076736128849,-12.3434852687276,
118.730651712534)) ;
#192290 = CARTESIAN_POINT('Ctrl Pts',(-8.12457123590877,-12.3434852268848,
118.706420765879)) ;
#192291 = CARTESIAN_POINT('Ctrl Pts',(-8.19837511052905,-12.343485185042,
118.682189819225)) ;
#192292 = CARTESIAN_POINT('Ctrl Pts',(-8.20736927607411,-12.4137122483728,
118.709584594176)) ;
#192293 = CARTESIAN_POINT('Ctrl Pts',(-8.11806988347709,-12.5618189977429,
118.473239800089)) ;
#192294 = CARTESIAN_POINT('Ctrl Pts',(-8.13257443790471,-12.6218107314417,
118.517418330508)) ;
#192295 = CARTESIAN_POINT('Ctrl Pts',(-8.05877056827575,-12.6218107975561,
118.541649292365)) ;
#192296 = CARTESIAN_POINT('Ctrl Pts',(-7.98496669864682,-12.6218108636706,
118.565880254222)) ;
#192297 = CARTESIAN_POINT('Ctrl Pts',(-7.97046214421921,-12.5618191299718,
118.521701723804)) ;
#192298 = CARTESIAN_POINT('Ctrl Pts',(-7.95595758979159,-12.501827396273,
118.477523193385)) ;
#192299 = CARTESIAN_POINT('Ctrl Pts',(-8.02976145942054,-12.5018273301586,
118.453292231528)) ;
#192300 = CARTESIAN_POINT('Ctrl Pts',(-8.10356532904949,-12.5018272640442,
118.42906126967)) ;
#192301 = CARTESIAN_POINT('Ctrl Pts',(-8.11806988347709,-12.5618189977429,
118.473239800089)) ;
#192302 = CARTESIAN_POINT('Ctrl Pts',(-8.04465640581912,-12.7689119270669,
118.284855280658)) ;
#192303 = CARTESIAN_POINT('Ctrl Pts',(-8.06357919075944,-12.814533735282,
118.34249102837)) ;
#192304 = CARTESIAN_POINT('Ctrl Pts',(-7.98977532782009,-12.8145338199658,
118.366722010603)) ;
#192305 = CARTESIAN_POINT('Ctrl Pts',(-7.91597146488071,-12.8145339046497,
118.390952992836)) ;
#192306 = CARTESIAN_POINT('Ctrl Pts',(-7.8970486799404,-12.7689120964346,
118.333317245123)) ;
#192307 = CARTESIAN_POINT('Ctrl Pts',(-7.87812589500005,-12.7232902882195,
118.275681497411)) ;
#192308 = CARTESIAN_POINT('Ctrl Pts',(-7.95192975793942,-12.7232902035356,
118.251450515178)) ;
#192309 = CARTESIAN_POINT('Ctrl Pts',(-8.02573362087878,-12.7232901188518,
118.227219532945)) ;
#192310 = CARTESIAN_POINT('Ctrl Pts',(-8.04465640581912,-12.7689119270669,
118.284855280658)) ;
#192311 = CARTESIAN_POINT('Ctrl Pts',(-7.98990681541494,-13.0251682484426,
118.1537612682)) ;
#192312 = CARTESIAN_POINT('Ctrl Pts',(-8.01194249189055,-13.052967781727,
118.220878381343)) ;
#192313 = CARTESIAN_POINT('Ctrl Pts',(-7.93813863719427,-13.0529678764172,
118.245109388683)) ;
#192314 = CARTESIAN_POINT('Ctrl Pts',(-7.86433478249799,-13.0529679711075,
118.269340396023)) ;
#192315 = CARTESIAN_POINT('Ctrl Pts',(-7.84229910602238,-13.025168437823,
118.20222328288)) ;
#192316 = CARTESIAN_POINT('Ctrl Pts',(-7.82026342954678,-12.9973689045386,
118.135106169737)) ;
#192317 = CARTESIAN_POINT('Ctrl Pts',(-7.89406728424306,-12.9973688098484,
118.110875162397)) ;
#192318 = CARTESIAN_POINT('Ctrl Pts',(-7.96787113893935,-12.9973687151582,
118.086644155057)) ;
#192319 = CARTESIAN_POINT('Ctrl Pts',(-7.98990681541494,-13.0251682484426,
118.1537612682)) ;
#192320 = CARTESIAN_POINT('Ctrl Pts',(-7.95830518848991,-13.3082750938872,
118.092954291203)) ;
#192321 = CARTESIAN_POINT('Ctrl Pts',(-7.98184680689377,-13.3163504016851,
118.164658260563)) ;
#192322 = CARTESIAN_POINT('Ctrl Pts',(-7.90804296057227,-13.3163504980826,
118.188889293411)) ;
#192323 = CARTESIAN_POINT('Ctrl Pts',(-7.83423911425076,-13.31635059448,118.213120326259)) ;
#192324 = CARTESIAN_POINT('Ctrl Pts',(-7.81069749584691,-13.3082752866821,
118.141416356899)) ;
#192325 = CARTESIAN_POINT('Ctrl Pts',(-7.78715587744302,-13.3001999788842,
118.069712387539)) ;
#192326 = CARTESIAN_POINT('Ctrl Pts',(-7.86095972376454,-13.3001998824867,
118.045481354691)) ;
#192327 = CARTESIAN_POINT('Ctrl Pts',(-7.93476357008601,-13.3001997860893,
118.021250321843)) ;
#192328 = CARTESIAN_POINT('Ctrl Pts',(-7.95830518848991,-13.3082750938872,
118.092954291203)) ;
#192329 = CARTESIAN_POINT('Ctrl Pts',(-7.95079241587088,-13.5983478962611,
118.105425292295)) ;
#192330 = CARTESIAN_POINT('Ctrl Pts',(-7.97416229673392,-13.5861829357955,
118.176606176905)) ;
#192331 = CARTESIAN_POINT('Ctrl Pts',(-7.90035845823514,-13.5861830266329,
118.20083723358)) ;
#192332 = CARTESIAN_POINT('Ctrl Pts',(-7.82655461973636,-13.5861831174704,
118.225068290255)) ;
#192333 = CARTESIAN_POINT('Ctrl Pts',(-7.80318473887331,-13.5983480779361,
118.153887405644)) ;
#192334 = CARTESIAN_POINT('Ctrl Pts',(-7.77981485801028,-13.6105130384017,
118.082706521034)) ;
#192335 = CARTESIAN_POINT('Ctrl Pts',(-7.85361869650906,-13.6105129475642,
118.058475464359)) ;
#192336 = CARTESIAN_POINT('Ctrl Pts',(-7.92742253500785,-13.6105128567267,
118.034244407684)) ;
#192337 = CARTESIAN_POINT('Ctrl Pts',(-7.95079241587088,-13.5983478962611,
118.105425292295)) ;
#192338 = CARTESIAN_POINT('Ctrl Pts',(-7.96711105691976,-13.8761876349326,
118.190549865602)) ;
#192339 = CARTESIAN_POINT('Ctrl Pts',(-7.98864383656382,-13.8446061027284,
118.256135236427)) ;
#192340 = CARTESIAN_POINT('Ctrl Pts',(-7.91484000469734,-13.8446061808087,
118.280366313303)) ;
#192341 = CARTESIAN_POINT('Ctrl Pts',(-7.84103617283086,-13.8446062588889,
118.304597390179)) ;
#192342 = CARTESIAN_POINT('Ctrl Pts',(-7.81950339318683,-13.8761877910931,
118.239012019354)) ;
#192343 = CARTESIAN_POINT('Ctrl Pts',(-7.79797061354276,-13.9077693232973,
118.173426648529)) ;
#192344 = CARTESIAN_POINT('Ctrl Pts',(-7.87177444540925,-13.907769245217,
118.149195571653)) ;
#192345 = CARTESIAN_POINT('Ctrl Pts',(-7.94557827727571,-13.9077691671368,
118.124964494777)) ;
#192346 = CARTESIAN_POINT('Ctrl Pts',(-7.96711105691976,-13.8761876349326,
118.190549865602)) ;
#192347 = CARTESIAN_POINT('Ctrl Pts',(-8.00577117627182,-14.1226645874526,
118.343946067148)) ;
#192348 = CARTESIAN_POINT('Ctrl Pts',(-8.0238998963966,-14.0738264529784,
118.399163222083)) ;
#192349 = CARTESIAN_POINT('Ctrl Pts',(-7.95009606892581,-14.0738265118824,
118.423394312347)) ;
#192350 = CARTESIAN_POINT('Ctrl Pts',(-7.87629224145502,-14.0738265707863,
118.447625402612)) ;
#192351 = CARTESIAN_POINT('Ctrl Pts',(-7.85816352133023,-14.1226647052604,
118.392408247677)) ;
#192352 = CARTESIAN_POINT('Ctrl Pts',(-7.84003480120545,-14.1715028397345,
118.337191092741)) ;
#192353 = CARTESIAN_POINT('Ctrl Pts',(-7.91383862867624,-14.1715027808306,
118.312960002477)) ;
#192354 = CARTESIAN_POINT('Ctrl Pts',(-7.98764245614702,-14.1715027219267,
118.288728912213)) ;
#192355 = CARTESIAN_POINT('Ctrl Pts',(-8.00577117627182,-14.1226645874526,
118.343946067148)) ;
#192356 = CARTESIAN_POINT('Ctrl Pts',(-8.06283714233654,-14.3171342011777,
118.553214565647)) ;
#192357 = CARTESIAN_POINT('Ctrl Pts',(-8.07627530082243,-14.2546443269057,
118.594145026798)) ;
#192358 = CARTESIAN_POINT('Ctrl Pts',(-8.0024714756415,-14.2546443659289,
118.618376124037)) ;
#192359 = CARTESIAN_POINT('Ctrl Pts',(-7.92866765046057,-14.2546444049521,
118.642607221276)) ;
#192360 = CARTESIAN_POINT('Ctrl Pts',(-7.9152294919747,-14.3171342792242,
118.601676760125)) ;
#192361 = CARTESIAN_POINT('Ctrl Pts',(-7.90179133348882,-14.3796241534962,
118.560746298974)) ;
#192362 = CARTESIAN_POINT('Ctrl Pts',(-7.97559515866974,-14.379624114473,
118.536515201735)) ;
#192363 = CARTESIAN_POINT('Ctrl Pts',(-8.04939898385068,-14.3796240754498,
118.512284104496)) ;
#192364 = CARTESIAN_POINT('Ctrl Pts',(-8.06283714233654,-14.3171342011777,
118.553214565647)) ;
#192365 = CARTESIAN_POINT('Ctrl Pts',(-8.13328894628417,-14.4470643657725,
118.803140602869)) ;
#192366 = CARTESIAN_POINT('Ctrl Pts',(-8.14109712925884,-14.375408398759,
118.826923067142)) ;
#192367 = CARTESIAN_POINT('Ctrl Pts',(-8.06729330458394,-14.3754084186234,
118.851154165922)) ;
#192368 = CARTESIAN_POINT('Ctrl Pts',(-7.99348947990904,-14.3754084384878,
118.875385264702)) ;
#192369 = CARTESIAN_POINT('Ctrl Pts',(-7.98568129693438,-14.4470644055013,
118.85160280043)) ;
#192370 = CARTESIAN_POINT('Ctrl Pts',(-7.97787311395969,-14.5187203725148,
118.827820336157)) ;
#192371 = CARTESIAN_POINT('Ctrl Pts',(-8.0516769386346,-14.5187203526504,
118.803589237377)) ;
#192372 = CARTESIAN_POINT('Ctrl Pts',(-8.12548076330949,-14.5187203327861,
118.779358138597)) ;
#192373 = CARTESIAN_POINT('Ctrl Pts',(-8.13328894628417,-14.4470643657725,
118.803140602869)) ;
#192374 = CARTESIAN_POINT('Ctrl Pts',(-8.21185565403187,-14.503923953364,
119.077904388302)) ;
#192375 = CARTESIAN_POINT('Ctrl Pts',(-8.21345628147345,-14.4281893560193,
119.082779640171)) ;
#192376 = CARTESIAN_POINT('Ctrl Pts',(-8.13965245513209,-14.4281893585944,
119.107010733875)) ;
#192377 = CARTESIAN_POINT('Ctrl Pts',(-8.06584862879074,-14.4281893611695,
119.13124182758)) ;
#192378 = CARTESIAN_POINT('Ctrl Pts',(-8.06424800134915,-14.5039239585142,
119.126366575712)) ;
#192379 = CARTESIAN_POINT('Ctrl Pts',(-8.06264737390758,-14.5796585558589,
119.121491323843)) ;
#192380 = CARTESIAN_POINT('Ctrl Pts',(-8.13645120024894,-14.5796585532838,
119.097260230139)) ;
#192381 = CARTESIAN_POINT('Ctrl Pts',(-8.21025502659029,-14.5796585507087,
119.073029136434)) ;
#192382 = CARTESIAN_POINT('Ctrl Pts',(-8.21185565403187,-14.503923953364,
119.077904388302)) ;
#192383 = CARTESIAN_POINT('Ctrl Pts',(-8.2919897821839,-14.4828378904359,
119.357469635026)) ;
#192384 = CARTESIAN_POINT('Ctrl Pts',(-8.28726335063194,-14.4084605775559,
119.34307368624)) ;
#192385 = CARTESIAN_POINT('Ctrl Pts',(-8.21345952116713,-14.4084605673929,
119.367304770431)) ;
#192386 = CARTESIAN_POINT('Ctrl Pts',(-8.13965569170231,-14.40846055723,119.391535854622)) ;
#192387 = CARTESIAN_POINT('Ctrl Pts',(-8.14438212325429,-14.48283787011,119.405931803408)) ;
#192388 = CARTESIAN_POINT('Ctrl Pts',(-8.14910855480624,-14.5572151829901,
119.420327752194)) ;
#192389 = CARTESIAN_POINT('Ctrl Pts',(-8.22291238427106,-14.557215193153,
119.396096668003)) ;
#192390 = CARTESIAN_POINT('Ctrl Pts',(-8.29671621373586,-14.557215203316,
119.371865583812)) ;
#192391 = CARTESIAN_POINT('Ctrl Pts',(-8.2919897821839,-14.4828378904359,
119.357469635026)) ;
#192392 = CARTESIAN_POINT('Ctrl Pts',(-8.3671164306326,-14.385601171439,119.621760366738)) ;
#192393 = CARTESIAN_POINT('Ctrl Pts',(-8.35640339197924,-14.3179002562645,
119.589130178826)) ;
#192394 = CARTESIAN_POINT('Ctrl Pts',(-8.28259955872094,-14.3179002385077,
119.613361251462)) ;
#192395 = CARTESIAN_POINT('Ctrl Pts',(-8.20879572546266,-14.3179002207509,
119.637592324099)) ;
#192396 = CARTESIAN_POINT('Ctrl Pts',(-8.21950876411601,-14.3856011359254,
119.670222512011)) ;
#192397 = CARTESIAN_POINT('Ctrl Pts',(-8.23022180276934,-14.4533020510999,
119.702852699924)) ;
#192398 = CARTESIAN_POINT('Ctrl Pts',(-8.30402563602765,-14.4533020688567,
119.678621627287)) ;
#192399 = CARTESIAN_POINT('Ctrl Pts',(-8.37782946928592,-14.4533020866135,
119.65439055465)) ;
#192400 = CARTESIAN_POINT('Ctrl Pts',(-8.3671164306326,-14.385601171439,119.621760366738)) ;
#192401 = CARTESIAN_POINT('Ctrl Pts',(-8.43129354623971,-14.2179717447503,
119.852851556862)) ;
#192402 = CARTESIAN_POINT('Ctrl Pts',(-8.41534602136537,-14.1618723407489,
119.804277968692)) ;
#192403 = CARTESIAN_POINT('Ctrl Pts',(-8.34154218406632,-14.161872321804,
119.828509029022)) ;
#192404 = CARTESIAN_POINT('Ctrl Pts',(-8.26773834676728,-14.1618723028591,
119.852740089351)) ;
#192405 = CARTESIAN_POINT('Ctrl Pts',(-8.28368587164164,-14.2179717068605,
119.901313677521)) ;
#192406 = CARTESIAN_POINT('Ctrl Pts',(-8.299633396516,-14.2740711108619,119.94988726569)) ;
#192407 = CARTESIAN_POINT('Ctrl Pts',(-8.37343723381503,-14.2740711298068,
119.925656205361)) ;
#192408 = CARTESIAN_POINT('Ctrl Pts',(-8.44724107111407,-14.2740711487517,
119.901425145032)) ;
#192409 = CARTESIAN_POINT('Ctrl Pts',(-8.43129354623971,-14.2179717447503,
119.852851556862)) ;
#192410 = CARTESIAN_POINT('Ctrl Pts',(-8.47844463780643,-13.9957363810985,
120.031646358861)) ;
#192411 = CARTESIAN_POINT('Ctrl Pts',(-8.45845292588495,-13.9550697800569,
119.970754829578)) ;
#192412 = CARTESIAN_POINT('Ctrl Pts',(-8.38464908591199,-13.95506976129,119.994985881762)) ;
#192413 = CARTESIAN_POINT('Ctrl Pts',(-8.31084524593901,-13.9550697425231,
120.019216933947)) ;
#192414 = CARTESIAN_POINT('Ctrl Pts',(-8.33083695786049,-13.9957363435648,
120.08010846323)) ;
#192415 = CARTESIAN_POINT('Ctrl Pts',(-8.35082866978197,-14.0364029446064,
120.140999992513)) ;
#192416 = CARTESIAN_POINT('Ctrl Pts',(-8.42463250975494,-14.0364029633733,
120.116768940328)) ;
#192417 = CARTESIAN_POINT('Ctrl Pts',(-8.4984363497279,-14.0364029821402,
120.092537888144)) ;
#192418 = CARTESIAN_POINT('Ctrl Pts',(-8.47844463780643,-13.9957363810985,
120.031646358861)) ;
#192419 = CARTESIAN_POINT('Ctrl Pts',(-8.50554208777262,-13.7291995183929,
120.149825509069)) ;
#192420 = CARTESIAN_POINT('Ctrl Pts',(-8.48289027006436,-13.707082237132,
120.080831726937)) ;
#192421 = CARTESIAN_POINT('Ctrl Pts',(-8.40908642760036,-13.7070822245354,
120.105062771535)) ;
#192422 = CARTESIAN_POINT('Ctrl Pts',(-8.33528258513637,-13.7070822119389,
120.129293816133)) ;
#192423 = CARTESIAN_POINT('Ctrl Pts',(-8.35793440284465,-13.7291994931998,
120.198287598264)) ;
#192424 = CARTESIAN_POINT('Ctrl Pts',(-8.38058622055291,-13.7513167744608,
120.267281380396)) ;
#192425 = CARTESIAN_POINT('Ctrl Pts',(-8.45439006301691,-13.7513167870574,
120.243050335798)) ;
#192426 = CARTESIAN_POINT('Ctrl Pts',(-8.52819390548089,-13.7513167996539,
120.2188192912)) ;
#192427 = CARTESIAN_POINT('Ctrl Pts',(-8.50554208777262,-13.7291995183929,
120.149825509069)) ;
#192428 = CARTESIAN_POINT('Ctrl Pts',(-8.50912632410288,-13.4423294051305,
120.196103041933)) ;
#192429 = CARTESIAN_POINT('Ctrl Pts',(-8.48545842126137,-13.440209694869,
120.124014428538)) ;
#192430 = CARTESIAN_POINT('Ctrl Pts',(-8.41165457775546,-13.4402096875426,
120.148245469962)) ;
#192431 = CARTESIAN_POINT('Ctrl Pts',(-8.33785073424954,-13.4402096802161,
120.172476511386)) ;
#192432 = CARTESIAN_POINT('Ctrl Pts',(-8.36151863709104,-13.4423293904776,
120.244565124781)) ;
#192433 = CARTESIAN_POINT('Ctrl Pts',(-8.38518653993252,-13.444449100739,
120.316653738176)) ;
#192434 = CARTESIAN_POINT('Ctrl Pts',(-8.45899038343846,-13.4444491080655,
120.292422696752)) ;
#192435 = CARTESIAN_POINT('Ctrl Pts',(-8.53279422694436,-13.444449115392,
120.268191655328)) ;
#192436 = CARTESIAN_POINT('Ctrl Pts',(-8.50912632410288,-13.4423294051305,
120.196103041933)) ;
#192437 = CARTESIAN_POINT('Ctrl Pts',(-8.48842339088641,-13.1524216120436,
120.168582375125)) ;
#192438 = CARTESIAN_POINT('Ctrl Pts',(-8.46543005559105,-13.1705421865172,
120.098548385741)) ;
#192439 = CARTESIAN_POINT('Ctrl Pts',(-8.39162621191911,-13.1705421848694,
120.12277942666)) ;
#192440 = CARTESIAN_POINT('Ctrl Pts',(-8.31782236824715,-13.1705421832215,
120.147010467578)) ;
#192441 = CARTESIAN_POINT('Ctrl Pts',(-8.34081570354252,-13.1524216087479,
120.217044456961)) ;
#192442 = CARTESIAN_POINT('Ctrl Pts',(-8.36380903883786,-13.1343010342744,
120.287078446345)) ;
#192443 = CARTESIAN_POINT('Ctrl Pts',(-8.43761288250982,-13.1343010359222,
120.262847405426)) ;
#192444 = CARTESIAN_POINT('Ctrl Pts',(-8.51141672618176,-13.1343010375701,
120.238616364508)) ;
#192445 = CARTESIAN_POINT('Ctrl Pts',(-8.48842339088641,-13.1524216120436,
120.168582375125)) ;
#192446 = CARTESIAN_POINT('Ctrl Pts',(-8.44428324962565,-12.8827428706973,
120.06951076432)) ;
#192447 = CARTESIAN_POINT('Ctrl Pts',(-8.42360575544995,-12.9197213640829,
120.00653045339)) ;
#192448 = CARTESIAN_POINT('Ctrl Pts',(-8.3498019121995,-12.9197213654279,
120.030761495592)) ;
#192449 = CARTESIAN_POINT('Ctrl Pts',(-8.27599806894903,-12.919721366773,
120.054992537794)) ;
#192450 = CARTESIAN_POINT('Ctrl Pts',(-8.29667556312474,-12.8827428733873,
120.117972848725)) ;
#192451 = CARTESIAN_POINT('Ctrl Pts',(-8.31735305730044,-12.8457643800017,
120.180953159656)) ;
#192452 = CARTESIAN_POINT('Ctrl Pts',(-8.3911569005509,-12.8457643786566,
120.156722117453)) ;
#192453 = CARTESIAN_POINT('Ctrl Pts',(-8.46496074380135,-12.8457643773116,
120.132491075251)) ;
#192454 = CARTESIAN_POINT('Ctrl Pts',(-8.44428324962565,-12.8827428706973,
120.06951076432)) ;
#192455 = CARTESIAN_POINT('Ctrl Pts',(-8.37882269029488,-12.6504179680888,
119.905639294763)) ;
#192456 = CARTESIAN_POINT('Ctrl Pts',(-8.36195051844518,-12.7036746706006,
119.854249381688)) ;
#192457 = CARTESIAN_POINT('Ctrl Pts',(-8.28814667575038,-12.7036746730312,
119.878480425583)) ;
#192458 = CARTESIAN_POINT('Ctrl Pts',(-8.21434283305557,-12.7036746754618,
119.902711469478)) ;
#192459 = CARTESIAN_POINT('Ctrl Pts',(-8.23121500490527,-12.65041797295,119.954101382553)) ;
#192460 = CARTESIAN_POINT('Ctrl Pts',(-8.24808717675496,-12.5971612704382,
120.005491295628)) ;
#192461 = CARTESIAN_POINT('Ctrl Pts',(-8.32189101944977,-12.5971612680076,
119.981260251733)) ;
#192462 = CARTESIAN_POINT('Ctrl Pts',(-8.39569486214457,-12.597161265577,
119.957029207838)) ;
#192463 = CARTESIAN_POINT('Ctrl Pts',(-8.37882269029488,-12.6504179680888,
119.905639294763)) ;
#192464 = CARTESIAN_POINT('Ctrl Pts',(-8.29622142005809,-12.4733695384466,
119.689502394773)) ;
#192465 = CARTESIAN_POINT('Ctrl Pts',(-8.28435858733497,-12.5390682481556,
119.653370120416)) ;
#192466 = CARTESIAN_POINT('Ctrl Pts',(-8.21055474474865,-12.5390682494468,
119.677601164641)) ;
#192467 = CARTESIAN_POINT('Ctrl Pts',(-8.13675090216231,-12.5390682507379,
119.701832208866)) ;
#192468 = CARTESIAN_POINT('Ctrl Pts',(-8.14861373488543,-12.4733695410289,
119.737964483223)) ;
#192469 = CARTESIAN_POINT('Ctrl Pts',(-8.16047656760854,-12.4076708313198,
119.77409675758)) ;
#192470 = CARTESIAN_POINT('Ctrl Pts',(-8.23428041019488,-12.4076708300287,
119.749865713355)) ;
#192471 = CARTESIAN_POINT('Ctrl Pts',(-8.30808425278119,-12.4076708287375,
119.72563466913)) ;
#192472 = CARTESIAN_POINT('Ctrl Pts',(-8.29622142005809,-12.4733695384466,
119.689502394773)) ;
#192473 = CARTESIAN_POINT('Ctrl Pts',(-8.20108241127664,-12.3637277646619,
119.435348643595)) ;
#192474 = CARTESIAN_POINT('Ctrl Pts',(-8.19510827341861,-12.4371796156444,
119.417152383597)) ;
#192475 = CARTESIAN_POINT('Ctrl Pts',(-8.12130442993599,-12.4371796152465,
119.441383425092)) ;
#192476 = CARTESIAN_POINT('Ctrl Pts',(-8.04750058645336,-12.4371796148486,
119.465614466587)) ;
#192477 = CARTESIAN_POINT('Ctrl Pts',(-8.0534747243114,-12.3637277638662,
119.483810726586)) ;
#192478 = CARTESIAN_POINT('Ctrl Pts',(-8.05944886216942,-12.2902759128838,
119.502006986584)) ;
#192479 = CARTESIAN_POINT('Ctrl Pts',(-8.13325270565205,-12.2902759132816,
119.477775945089)) ;
#192480 = CARTESIAN_POINT('Ctrl Pts',(-8.20705654913468,-12.2902759136795,
119.453544903594)) ;
#192481 = CARTESIAN_POINT('Ctrl Pts',(-8.20108241127664,-12.3637277646619,
119.435348643595)) ;
#192482 = CARTESIAN_POINT('Ctrl Pts',(-8.10069311267931,-12.3302633026411,
119.164918199571)) ;
#192483 = CARTESIAN_POINT('Ctrl Pts',(-8.10098863908321,-12.4061588446246,
119.165818325233)) ;
#192484 = CARTESIAN_POINT('Ctrl Pts',(-8.02718479434802,-12.406158844275,
119.190049362913)) ;
#192485 = CARTESIAN_POINT('Ctrl Pts',(-7.95338094961285,-12.4061588439253,
119.214280400593)) ;
#192486 = CARTESIAN_POINT('Ctrl Pts',(-7.95308542320895,-12.3302633019418,
119.213380274931)) ;
#192487 = CARTESIAN_POINT('Ctrl Pts',(-7.95278989680505,-12.2543677599582,
119.21248014927)) ;
#192488 = CARTESIAN_POINT('Ctrl Pts',(-8.02659374154021,-12.2543677603079,
119.18824911159)) ;
#192489 = CARTESIAN_POINT('Ctrl Pts',(-8.10039758627541,-12.2543677606575,
119.16401807391)) ;
#192490 = CARTESIAN_POINT('Ctrl Pts',(-8.10069311267931,-12.3302633026411,
119.164918199571)) ;
#192491 = CARTESIAN_POINT('Ctrl Pts',(-8.00044993799628,-12.3743151570883,
118.895045920248)) ;
#192492 = CARTESIAN_POINT('Ctrl Pts',(-8.00701167902443,-12.4472453738058,
118.915031924497)) ;
#192493 = CARTESIAN_POINT('Ctrl Pts',(-7.93320783263552,-12.4472453760978,
118.93926295714)) ;
#192494 = CARTESIAN_POINT('Ctrl Pts',(-7.85940398624658,-12.4472453783898,
118.963493989783)) ;
#192495 = CARTESIAN_POINT('Ctrl Pts',(-7.85284224521843,-12.3743151616723,
118.943507985534)) ;
#192496 = CARTESIAN_POINT('Ctrl Pts',(-7.84628050419029,-12.3013849449547,
118.923521981286)) ;
#192497 = CARTESIAN_POINT('Ctrl Pts',(-7.92008435057921,-12.3013849426627,
118.899290948643)) ;
#192498 = CARTESIAN_POINT('Ctrl Pts',(-7.99388819696813,-12.3013849403707,
118.875059916)) ;
#192499 = CARTESIAN_POINT('Ctrl Pts',(-8.00044993799628,-12.3743151570883,
118.895045920248)) ;
#192500 = CARTESIAN_POINT('Ctrl Pts',(-7.90710319884704,-12.4928395526405,
118.64614258601)) ;
#192501 = CARTESIAN_POINT('Ctrl Pts',(-7.91945933895386,-12.5575998714036,
118.683777394806)) ;
#192502 = CARTESIAN_POINT('Ctrl Pts',(-7.84565549110987,-12.5575998792926,
118.708008423017)) ;
#192503 = CARTESIAN_POINT('Ctrl Pts',(-7.7718516432659,-12.5575998871817,
118.732239451228)) ;
#192504 = CARTESIAN_POINT('Ctrl Pts',(-7.7594955031591,-12.4928395684187,
118.694604642432)) ;
#192505 = CARTESIAN_POINT('Ctrl Pts',(-7.74713936305227,-12.4280792496557,
118.656969833636)) ;
#192506 = CARTESIAN_POINT('Ctrl Pts',(-7.82094321089625,-12.4280792417666,
118.632738805425)) ;
#192507 = CARTESIAN_POINT('Ctrl Pts',(-7.89474705874023,-12.4280792338775,
118.608507777214)) ;
#192508 = CARTESIAN_POINT('Ctrl Pts',(-7.90710319884704,-12.4928395526405,
118.64614258601)) ;
#192509 = CARTESIAN_POINT('Ctrl Pts',(-7.82605565543513,-12.6792484033362,
118.434964572872)) ;
#192510 = CARTESIAN_POINT('Ctrl Pts',(-7.84335047013331,-12.7310874670911,
118.487641787435)) ;
#192511 = CARTESIAN_POINT('Ctrl Pts',(-7.76954662110735,-12.7310874856029,
118.511872812046)) ;
#192512 = CARTESIAN_POINT('Ctrl Pts',(-7.69574277208138,-12.7310875041147,
118.536103836657)) ;
#192513 = CARTESIAN_POINT('Ctrl Pts',(-7.67844795738318,-12.6792484403597,
118.483426622094)) ;
#192514 = CARTESIAN_POINT('Ctrl Pts',(-7.66115314268502,-12.6274093766048,
118.430749407531)) ;
#192515 = CARTESIAN_POINT('Ctrl Pts',(-7.73495699171098,-12.627409358093,
118.40651838292)) ;
#192516 = CARTESIAN_POINT('Ctrl Pts',(-7.80876084073694,-12.6274093395813,
118.382287358309)) ;
#192517 = CARTESIAN_POINT('Ctrl Pts',(-7.82605565543513,-12.6792484033362,
118.434964572872)) ;
#192518 = CARTESIAN_POINT('Ctrl Pts',(-7.76370923303463,-12.9157037711306,
118.280276167893)) ;
#192519 = CARTESIAN_POINT('Ctrl Pts',(-7.78465336230621,-12.9511079256509,
118.344068605718)) ;
#192520 = CARTESIAN_POINT('Ctrl Pts',(-7.71084951411926,-12.9511079534963,
118.368299632885)) ;
#192521 = CARTESIAN_POINT('Ctrl Pts',(-7.63704566593232,-12.9511079813417,
118.392530660051)) ;
#192522 = CARTESIAN_POINT('Ctrl Pts',(-7.61610153666074,-12.9157038268213,
118.328738222226)) ;
#192523 = CARTESIAN_POINT('Ctrl Pts',(-7.59515740738914,-12.880299672301,
118.264945784401)) ;
#192524 = CARTESIAN_POINT('Ctrl Pts',(-7.6689612555761,-12.8802996444556,
118.240714757234)) ;
#192525 = CARTESIAN_POINT('Ctrl Pts',(-7.74276510376304,-12.8802996166102,
118.216483730068)) ;
#192526 = CARTESIAN_POINT('Ctrl Pts',(-7.76370923303463,-12.9157037711306,
118.280276167893)) ;
#192527 = CARTESIAN_POINT('Ctrl Pts',(-7.7222130498299,-13.1914441677562,
118.189580023527)) ;
#192528 = CARTESIAN_POINT('Ctrl Pts',(-7.74534632640251,-13.2076474543041,
118.260040250604)) ;
#192529 = CARTESIAN_POINT('Ctrl Pts',(-7.67154247998087,-13.2076474957357,
118.284271283147)) ;
#192530 = CARTESIAN_POINT('Ctrl Pts',(-7.59773863355922,-13.2076475371673,
118.30850231569)) ;
#192531 = CARTESIAN_POINT('Ctrl Pts',(-7.57460535698663,-13.1914442506193,
118.238042088613)) ;
#192532 = CARTESIAN_POINT('Ctrl Pts',(-7.55147208041403,-13.1752409640713,
118.167581861536)) ;
#192533 = CARTESIAN_POINT('Ctrl Pts',(-7.62527592683567,-13.1752409226398,
118.143350828993)) ;
#192534 = CARTESIAN_POINT('Ctrl Pts',(-7.69907977325731,-13.1752408812082,
118.119119796449)) ;
#192535 = CARTESIAN_POINT('Ctrl Pts',(-7.7222130498299,-13.1914441677562,
118.189580023527)) ;
#192536 = CARTESIAN_POINT('Ctrl Pts',(-7.70493031502856,-13.4802992555045,
118.172216171245)) ;
#192537 = CARTESIAN_POINT('Ctrl Pts',(-7.72857354727237,-13.4763581958197,
118.244229640883)) ;
#192538 = CARTESIAN_POINT('Ctrl Pts',(-7.65476970455688,-13.4763582452253,
118.268460684714)) ;
#192539 = CARTESIAN_POINT('Ctrl Pts',(-7.58096586184136,-13.4763582946309,
118.292691728546)) ;
#192540 = CARTESIAN_POINT('Ctrl Pts',(-7.55732262959753,-13.4802993543157,
118.220678258908)) ;
#192541 = CARTESIAN_POINT('Ctrl Pts',(-7.53367939735367,-13.4842404140005,
118.14866478927)) ;
#192542 = CARTESIAN_POINT('Ctrl Pts',(-7.60748324006919,-13.4842403645949,
118.124433745439)) ;
#192543 = CARTESIAN_POINT('Ctrl Pts',(-7.6812870827847,-13.4842403151893,
118.100202701607)) ;
#192544 = CARTESIAN_POINT('Ctrl Pts',(-7.70493031502856,-13.4802992555045,
118.172216171245)) ;
#192545 = CARTESIAN_POINT('Ctrl Pts',(-7.71165791300415,-13.7664087624137,
118.228202531316)) ;
#192546 = CARTESIAN_POINT('Ctrl Pts',(-7.73413116046454,-13.7424862734231,
118.296652415907)) ;
#192547 = CARTESIAN_POINT('Ctrl Pts',(-7.66032732263785,-13.7424863290053,
118.320883474629)) ;
#192548 = CARTESIAN_POINT('Ctrl Pts',(-7.58652348481117,-13.7424863845875,
118.345114533351)) ;
#192549 = CARTESIAN_POINT('Ctrl Pts',(-7.5640502373508,-13.766408873578,118.276664648761)) ;
#192550 = CARTESIAN_POINT('Ctrl Pts',(-7.54157698989042,-13.7903313625685,
118.20821476417)) ;
#192551 = CARTESIAN_POINT('Ctrl Pts',(-7.61538082771709,-13.7903313069864,
118.183983705448)) ;
#192552 = CARTESIAN_POINT('Ctrl Pts',(-7.68918466554377,-13.7903312514042,
118.159752646726)) ;
#192553 = CARTESIAN_POINT('Ctrl Pts',(-7.71165791300415,-13.7664087624137,
118.228202531316)) ;
#192554 = CARTESIAN_POINT('Ctrl Pts',(-7.74161114589191,-14.0278445854345,
118.354981969349)) ;
#192555 = CARTESIAN_POINT('Ctrl Pts',(-7.76129016724846,-13.98563446645,118.414921091898)) ;
#192556 = CARTESIAN_POINT('Ctrl Pts',(-7.68748633547243,-13.9856345227655,
118.439152169049)) ;
#192557 = CARTESIAN_POINT('Ctrl Pts',(-7.61368250369641,-13.985634579081,
118.463383246201)) ;
#192558 = CARTESIAN_POINT('Ctrl Pts',(-7.59400348233985,-14.0278446980655,
118.403444123652)) ;
#192559 = CARTESIAN_POINT('Ctrl Pts',(-7.57432446098331,-14.07005481705,118.343505001104)) ;
#192560 = CARTESIAN_POINT('Ctrl Pts',(-7.64812829275933,-14.0700547607345,
118.319273923952)) ;
#192561 = CARTESIAN_POINT('Ctrl Pts',(-7.72193212453537,-14.070054704419,
118.295042846801)) ;
#192562 = CARTESIAN_POINT('Ctrl Pts',(-7.74161114589191,-14.0278445854345,
118.354981969349)) ;
#192563 = CARTESIAN_POINT('Ctrl Pts',(-7.79147735941891,-14.2444016591037,
118.542237068999)) ;
#192564 = CARTESIAN_POINT('Ctrl Pts',(-7.80697137655135,-14.1870110797581,
118.589429343793)) ;
#192565 = CARTESIAN_POINT('Ctrl Pts',(-7.73316755069903,-14.1870111286872,
118.613660438987)) ;
#192566 = CARTESIAN_POINT('Ctrl Pts',(-7.6593637248467,-14.1870111776162,
118.637891534181)) ;
#192567 = CARTESIAN_POINT('Ctrl Pts',(-7.64386970771426,-14.2444017569618,
118.590699259387)) ;
#192568 = CARTESIAN_POINT('Ctrl Pts',(-7.6283756905818,-14.3017923363074,
118.543506984594)) ;
#192569 = CARTESIAN_POINT('Ctrl Pts',(-7.70217951643413,-14.3017922873783,
118.5192758894)) ;
#192570 = CARTESIAN_POINT('Ctrl Pts',(-7.77598334228645,-14.3017922384493,
118.495044794206)) ;
#192571 = CARTESIAN_POINT('Ctrl Pts',(-7.79147735941891,-14.2444016591037,
118.542237068999)) ;
#192572 = CARTESIAN_POINT('Ctrl Pts',(-7.85719638681783,-14.4026063876543,
118.777859695063)) ;
#192573 = CARTESIAN_POINT('Ctrl Pts',(-7.86739098952979,-14.3340872602138,
118.808910808447)) ;
#192574 = CARTESIAN_POINT('Ctrl Pts',(-7.79358716916343,-14.3340872957345,
118.83314192035)) ;
#192575 = CARTESIAN_POINT('Ctrl Pts',(-7.71978334879709,-14.3340873312552,
118.857373032254)) ;
#192576 = CARTESIAN_POINT('Ctrl Pts',(-7.70958874608515,-14.4026064586957,
118.82632191887)) ;
#192577 = CARTESIAN_POINT('Ctrl Pts',(-7.69939414337321,-14.4711255861363,
118.795270805486)) ;
#192578 = CARTESIAN_POINT('Ctrl Pts',(-7.77319796373955,-14.4711255506156,
118.771039693583)) ;
#192579 = CARTESIAN_POINT('Ctrl Pts',(-7.84700178410591,-14.4711255150949,
118.74680858168)) ;
#192580 = CARTESIAN_POINT('Ctrl Pts',(-7.85719638681783,-14.4026063876543,
118.777859695063)) ;
#192581 = CARTESIAN_POINT('Ctrl Pts',(-7.93377264099751,-14.4903817315252,
119.046765235563)) ;
#192582 = CARTESIAN_POINT('Ctrl Pts',(-7.93789788343907,-14.4156342594261,
119.059330056695)) ;
#192583 = CARTESIAN_POINT('Ctrl Pts',(-7.86409406767712,-14.4156342751567,
119.083561182623)) ;
#192584 = CARTESIAN_POINT('Ctrl Pts',(-7.79029025191515,-14.4156342908872,
119.10779230855)) ;
#192585 = CARTESIAN_POINT('Ctrl Pts',(-7.7861650094736,-14.4903817629863,
119.095227487418)) ;
#192586 = CARTESIAN_POINT('Ctrl Pts',(-7.78203976703203,-14.5651292350854,
119.082662666287)) ;
#192587 = CARTESIAN_POINT('Ctrl Pts',(-7.85584358279399,-14.5651292193548,
119.058431540359)) ;
#192588 = CARTESIAN_POINT('Ctrl Pts',(-7.92964739855593,-14.5651292036242,
119.034200414431)) ;
#192589 = CARTESIAN_POINT('Ctrl Pts',(-7.93377264099751,-14.4903817315252,
119.046765235563)) ;
#192590 = CARTESIAN_POINT('Ctrl Pts',(-8.01373210317338,-14.5006966747965,
119.325637975014)) ;
#192591 = CARTESIAN_POINT('Ctrl Pts',(-8.0115497988902,-14.4251205193326,
119.318991026449)) ;
#192592 = CARTESIAN_POINT('Ctrl Pts',(-7.93774598491779,-14.425120510433,
119.343222157827)) ;
#192593 = CARTESIAN_POINT('Ctrl Pts',(-7.86394217094539,-14.4251205015334,
119.367453289206)) ;
#192594 = CARTESIAN_POINT('Ctrl Pts',(-7.86612447522857,-14.5006966569974,
119.374100237771)) ;
#192595 = CARTESIAN_POINT('Ctrl Pts',(-7.86830677951178,-14.5762728124613,
119.380747186336)) ;
#192596 = CARTESIAN_POINT('Ctrl Pts',(-7.94211059348418,-14.5762728213609,
119.356516054957)) ;
#192597 = CARTESIAN_POINT('Ctrl Pts',(-8.01591440745658,-14.5762728302605,
119.332284923579)) ;
#192598 = CARTESIAN_POINT('Ctrl Pts',(-8.01373210317338,-14.5006966747965,
119.325637975014)) ;
#192599 = CARTESIAN_POINT('Ctrl Pts',(-8.09161196909389,-14.4339382681578,
119.598307168471)) ;
#192600 = CARTESIAN_POINT('Ctrl Pts',(-8.08325550424145,-14.3629125582236,
119.572854722915)) ;
#192601 = CARTESIAN_POINT('Ctrl Pts',(-8.00945168990967,-14.3629125229021,
119.597085853198)) ;
#192602 = CARTESIAN_POINT('Ctrl Pts',(-7.93564787557786,-14.3629124875806,
119.621316983482)) ;
#192603 = CARTESIAN_POINT('Ctrl Pts',(-7.94400434043028,-14.4339381975148,
119.646769429038)) ;
#192604 = CARTESIAN_POINT('Ctrl Pts',(-7.9523608052827,-14.504963907449,119.672221874595)) ;
#192605 = CARTESIAN_POINT('Ctrl Pts',(-8.02616461961452,-14.5049639427705,
119.647990744311)) ;
#192606 = CARTESIAN_POINT('Ctrl Pts',(-8.0999684339463,-14.504963978092,119.623759614027)) ;
#192607 = CARTESIAN_POINT('Ctrl Pts',(-8.09161196909389,-14.4339382681578,
119.598307168471)) ;
#192608 = CARTESIAN_POINT('Ctrl Pts',(-8.16098641912054,-14.293783753758,
119.845172580273)) ;
#192609 = CARTESIAN_POINT('Ctrl Pts',(-8.14703842436003,-14.2324386627931,
119.802689236725)) ;
#192610 = CARTESIAN_POINT('Ctrl Pts',(-8.07323460709228,-14.2324386013355,
119.826920358066)) ;
#192611 = CARTESIAN_POINT('Ctrl Pts',(-7.99943078982447,-14.2324385398779,
119.851151479407)) ;
#192612 = CARTESIAN_POINT('Ctrl Pts',(-8.01337878458499,-14.2937836308428,
119.893634822955)) ;
#192613 = CARTESIAN_POINT('Ctrl Pts',(-8.0273267793455,-14.3551287218076,
119.936118166504)) ;
#192614 = CARTESIAN_POINT('Ctrl Pts',(-8.10113059661327,-14.3551287832652,
119.911887045163)) ;
#192615 = CARTESIAN_POINT('Ctrl Pts',(-8.17493441388104,-14.3551288447229,
119.887655923821)) ;
#192616 = CARTESIAN_POINT('Ctrl Pts',(-8.16098641912054,-14.293783753758,
119.845172580273)) ;
#192617 = CARTESIAN_POINT('Ctrl Pts',(-8.21570971002611,-14.0908689343358,
120.047346649353)) ;
#192618 = CARTESIAN_POINT('Ctrl Pts',(-8.19718615656026,-14.0436003014087,
119.990926892202)) ;
#192619 = CARTESIAN_POINT('Ctrl Pts',(-8.12338233373114,-14.0436002177779,
120.015157996604)) ;
#192620 = CARTESIAN_POINT('Ctrl Pts',(-8.04957851090201,-14.0436001341472,
120.039389101006)) ;
#192621 = CARTESIAN_POINT('Ctrl Pts',(-8.06810206436785,-14.0908687670742,
120.095808858157)) ;
#192622 = CARTESIAN_POINT('Ctrl Pts',(-8.08662561783368,-14.1381374000013,
120.152228615309)) ;
#192623 = CARTESIAN_POINT('Ctrl Pts',(-8.16042944066284,-14.1381374836321,
120.127997510907)) ;
#192624 = CARTESIAN_POINT('Ctrl Pts',(-8.23423326349196,-14.1381375672628,
120.103766406505)) ;
#192625 = CARTESIAN_POINT('Ctrl Pts',(-8.21570971002611,-14.0908689343358,
120.047346649353)) ;
#192626 = CARTESIAN_POINT('Ctrl Pts',(-8.25119308463164,-13.8416080598376,
120.190682254416)) ;
#192627 = CARTESIAN_POINT('Ctrl Pts',(-8.22943548398096,-13.8116727384737,
120.124412111326)) ;
#192628 = CARTESIAN_POINT('Ctrl Pts',(-8.15563165367641,-13.8116726391883,
120.148643192959)) ;
#192629 = CARTESIAN_POINT('Ctrl Pts',(-8.08182782337186,-13.8116725399028,
120.172874274592)) ;
#192630 = CARTESIAN_POINT('Ctrl Pts',(-8.10358542402254,-13.8416078612666,
120.239144417682)) ;
#192631 = CARTESIAN_POINT('Ctrl Pts',(-8.12534302467321,-13.8715431826305,
120.305414560772)) ;
#192632 = CARTESIAN_POINT('Ctrl Pts',(-8.19914685497777,-13.871543281916,
120.281183479139)) ;
#192633 = CARTESIAN_POINT('Ctrl Pts',(-8.27295068528229,-13.8715433812015,
120.256952397506)) ;
#192634 = CARTESIAN_POINT('Ctrl Pts',(-8.25119308463164,-13.8416080598376,
120.190682254416)) ;
#192635 = CARTESIAN_POINT('Ctrl Pts',(-8.26455274508899,-13.5600342116363,
120.266919542768)) ;
#192636 = CARTESIAN_POINT('Ctrl Pts',(-8.24109469557833,-13.5497128461305,
120.195470106805)) ;
#192637 = CARTESIAN_POINT('Ctrl Pts',(-8.16729085657722,-13.5497127385965,
120.21970116195)) ;
#192638 = CARTESIAN_POINT('Ctrl Pts',(-8.09348701757607,-13.5497126310626,
120.243932217095)) ;
#192639 = CARTESIAN_POINT('Ctrl Pts',(-8.11694506708672,-13.5600339965684,
120.315381653058)) ;
#192640 = CARTESIAN_POINT('Ctrl Pts',(-8.14040311659736,-13.5703553620741,
120.386831089021)) ;
#192641 = CARTESIAN_POINT('Ctrl Pts',(-8.2142069555985,-13.5703554696081,
120.362600033876)) ;
#192642 = CARTESIAN_POINT('Ctrl Pts',(-8.28801079459963,-13.570355577142,
120.338368978732)) ;
#192643 = CARTESIAN_POINT('Ctrl Pts',(-8.26455274508899,-13.5600342116363,
120.266919542768)) ;
#192644 = CARTESIAN_POINT('Ctrl Pts',(-8.25379252720853,-13.2694053226454,
120.269537469826)) ;
#192645 = CARTESIAN_POINT('Ctrl Pts',(-8.23031867646663,-13.2793593921655,
120.198039905872)) ;
#192646 = CARTESIAN_POINT('Ctrl Pts',(-8.15651482840728,-13.2793592852709,
120.222270933427)) ;
#192647 = CARTESIAN_POINT('Ctrl Pts',(-8.08271098034794,-13.2793591783763,
120.246501960982)) ;
#192648 = CARTESIAN_POINT('Ctrl Pts',(-8.10618483108986,-13.2694051088563,
120.317999524935)) ;
#192649 = CARTESIAN_POINT('Ctrl Pts',(-8.12965868183175,-13.2594510393362,
120.389497088889)) ;
#192650 = CARTESIAN_POINT('Ctrl Pts',(-8.2034625298911,-13.2594511462308,
120.365266061334)) ;
#192651 = CARTESIAN_POINT('Ctrl Pts',(-8.27726637795044,-13.2594512531254,
120.341035033779)) ;
#192652 = CARTESIAN_POINT('Ctrl Pts',(-8.25379252720853,-13.2694053226454,
120.269537469826)) ;
#192653 = CARTESIAN_POINT('Ctrl Pts',(-8.21877794635093,-12.9879324368107,
120.198480845472)) ;
#192654 = CARTESIAN_POINT('Ctrl Pts',(-8.19697716664803,-13.0175527392448,
120.132079185993)) ;
#192655 = CARTESIAN_POINT('Ctrl Pts',(-8.12317331011067,-13.0175526420622,
120.156310187725)) ;
#192656 = CARTESIAN_POINT('Ctrl Pts',(-8.04936945357328,-13.0175525448795,
120.180541189457)) ;
#192657 = CARTESIAN_POINT('Ctrl Pts',(-8.07117023327617,-12.9879322424453,
120.246942848936)) ;
#192658 = CARTESIAN_POINT('Ctrl Pts',(-8.09297101297905,-12.9583119400111,
120.313344508415)) ;
#192659 = CARTESIAN_POINT('Ctrl Pts',(-8.16677486951643,-12.9583120371938,
120.289113506683)) ;
#192660 = CARTESIAN_POINT('Ctrl Pts',(-8.24057872605381,-12.9583121343765,
120.264882504951)) ;
#192661 = CARTESIAN_POINT('Ctrl Pts',(-8.21877794635093,-12.9879324368107,
120.198480845472)) ;
#192662 = CARTESIAN_POINT('Ctrl Pts',(-8.1617475280646,-12.7391527795793,
120.060108032395)) ;
#192663 = CARTESIAN_POINT('Ctrl Pts',(-8.14316493865999,-12.786186317019,
120.003508461359)) ;
#192664 = CARTESIAN_POINT('Ctrl Pts',(-8.06936107504735,-12.7861862364123,
120.027739441541)) ;
#192665 = CARTESIAN_POINT('Ctrl Pts',(-7.99555721143471,-12.7861861558057,
120.051970421724)) ;
#192666 = CARTESIAN_POINT('Ctrl Pts',(-8.01413980083932,-12.739152618366,
120.108569992759)) ;
#192667 = CARTESIAN_POINT('Ctrl Pts',(-8.03272239024394,-12.6921190809264,
120.165169563794)) ;
#192668 = CARTESIAN_POINT('Ctrl Pts',(-8.10652625385659,-12.692119161533,
120.140938583612)) ;
#192669 = CARTESIAN_POINT('Ctrl Pts',(-8.18033011746921,-12.6921192421396,
120.11670760343)) ;
#192670 = CARTESIAN_POINT('Ctrl Pts',(-8.1617475280646,-12.7391527795793,
120.060108032395)) ;
#192671 = CARTESIAN_POINT('Ctrl Pts',(-8.08553845111122,-12.5377712145214,
119.86347894876)) ;
#192672 = CARTESIAN_POINT('Ctrl Pts',(-8.07151433693855,-12.5989350569668,
119.82076375785)) ;
#192673 = CARTESIAN_POINT('Ctrl Pts',(-7.9977104683385,-12.5989349988532,
119.844994722841)) ;
#192674 = CARTESIAN_POINT('Ctrl Pts',(-7.92390659973845,-12.5989349407397,
119.869225687832)) ;
#192675 = CARTESIAN_POINT('Ctrl Pts',(-7.93793071391114,-12.5377710982944,
119.911940878743)) ;
#192676 = CARTESIAN_POINT('Ctrl Pts',(-7.9519548280838,-12.476607255849,119.954656069653)) ;
#192677 = CARTESIAN_POINT('Ctrl Pts',(-8.02575869668384,-12.4766073139625,
119.930425104662)) ;
#192678 = CARTESIAN_POINT('Ctrl Pts',(-8.09956256528389,-12.476607372076,
119.90619413967)) ;
#192679 = CARTESIAN_POINT('Ctrl Pts',(-8.08553845111122,-12.5377712145214,
119.86347894876)) ;
#192680 = CARTESIAN_POINT('Ctrl Pts',(-7.99493866021685,-12.3995925801182,
119.623032110138)) ;
#192681 = CARTESIAN_POINT('Ctrl Pts',(-7.98648424887465,-12.4704956782947,
119.597281335481)) ;
#192682 = CARTESIAN_POINT('Ctrl Pts',(-7.91268037787084,-12.4704956456056,
119.621512293151)) ;
#192683 = CARTESIAN_POINT('Ctrl Pts',(-7.83887650686702,-12.4704956129164,
119.64574325082)) ;
#192684 = CARTESIAN_POINT('Ctrl Pts',(-7.84733091820922,-12.39959251474,119.671494025477)) ;
#192685 = CARTESIAN_POINT('Ctrl Pts',(-7.85578532955141,-12.3286894165636,
119.697244800134)) ;
#192686 = CARTESIAN_POINT('Ctrl Pts',(-7.92958920055522,-12.3286894492527,
119.673013842464)) ;
#192687 = CARTESIAN_POINT('Ctrl Pts',(-8.00339307155904,-12.3286894819418,
119.648782884794)) ;
#192688 = CARTESIAN_POINT('Ctrl Pts',(-7.99493866021685,-12.3995925801182,
119.623032110138)) ;
#192689 = CARTESIAN_POINT('Ctrl Pts',(-7.89593436549806,-12.33457880474,119.356931430303)) ;
#192690 = CARTESIAN_POINT('Ctrl Pts',(-7.89364599672396,-12.4101277476762,
119.349961426533)) ;
#192691 = CARTESIAN_POINT('Ctrl Pts',(-7.8198421257994,-12.4101277401761,
119.374192384444)) ;
#192692 = CARTESIAN_POINT('Ctrl Pts',(-7.74603825487482,-12.410127732676,
119.398423342356)) ;
#192693 = CARTESIAN_POINT('Ctrl Pts',(-7.74832662364891,-12.3345787897397,
119.405393346125)) ;
#192694 = CARTESIAN_POINT('Ctrl Pts',(-7.750614992423,-12.2590298468035,119.412363349895)) ;
#192695 = CARTESIAN_POINT('Ctrl Pts',(-7.82441886334756,-12.2590298543036,
119.388132391984)) ;
#192696 = CARTESIAN_POINT('Ctrl Pts',(-7.89822273427213,-12.2590298618037,
119.363901434073)) ;
#192697 = CARTESIAN_POINT('Ctrl Pts',(-7.89593436549806,-12.33457880474,119.356931430303)) ;
#192698 = CARTESIAN_POINT('Ctrl Pts',(-7.79477633291221,-12.3470312097476,
119.084250661337)) ;
#192699 = CARTESIAN_POINT('Ctrl Pts',(-7.7988141092919,-12.4218246112721,
119.096549075109)) ;
#192700 = CARTESIAN_POINT('Ctrl Pts',(-7.72501024069841,-12.4218246263605,
119.120780040121)) ;
#192701 = CARTESIAN_POINT('Ctrl Pts',(-7.65120637210492,-12.4218246414487,
119.145011005132)) ;
#192702 = CARTESIAN_POINT('Ctrl Pts',(-7.64716859572525,-12.3470312399242,
119.13271259136)) ;
#192703 = CARTESIAN_POINT('Ctrl Pts',(-7.64313081934554,-12.2722378383997,
119.120414177587)) ;
#192704 = CARTESIAN_POINT('Ctrl Pts',(-7.71693468793903,-12.2722378233114,
119.096183212576)) ;
#192705 = CARTESIAN_POINT('Ctrl Pts',(-7.79073855653252,-12.2722378082231,
119.071952247565)) ;
#192706 = CARTESIAN_POINT('Ctrl Pts',(-7.79477633291221,-12.3470312097476,
119.084250661337)) ;
#192707 = CARTESIAN_POINT('Ctrl Pts',(-7.6977506200353,-12.4361986060041,
118.824206306285)) ;
#192708 = CARTESIAN_POINT('Ctrl Pts',(-7.7078345844544,-12.5048795255924,
118.854920433421)) ;
#192709 = CARTESIAN_POINT('Ctrl Pts',(-7.63403072013485,-12.5048795584336,
118.87915141145)) ;
#192710 = CARTESIAN_POINT('Ctrl Pts',(-7.56022685581533,-12.5048795912748,
118.903382389479)) ;
#192711 = CARTESIAN_POINT('Ctrl Pts',(-7.55014289139622,-12.4361986716865,
118.872668262343)) ;
#192712 = CARTESIAN_POINT('Ctrl Pts',(-7.54005892697714,-12.3675177520983,
118.841954135207)) ;
#192713 = CARTESIAN_POINT('Ctrl Pts',(-7.61386279129669,-12.367517719257,
118.817723157178)) ;
#192714 = CARTESIAN_POINT('Ctrl Pts',(-7.68766665561624,-12.3675176864158,
118.793492179149)) ;
#192715 = CARTESIAN_POINT('Ctrl Pts',(-7.6977506200353,-12.4361986060041,
118.824206306285)) ;
#192716 = CARTESIAN_POINT('Ctrl Pts',(-7.61114947056002,-12.5959885808789,
118.595944474179)) ;
#192717 = CARTESIAN_POINT('Ctrl Pts',(-7.62656038830856,-12.6536171134987,
118.642883641819)) ;
#192718 = CARTESIAN_POINT('Ctrl Pts',(-7.55275652944442,-12.6536171574683,
118.667114636464)) ;
#192719 = CARTESIAN_POINT('Ctrl Pts',(-7.47895267058027,-12.653617201438,
118.69134563111)) ;
#192720 = CARTESIAN_POINT('Ctrl Pts',(-7.46354175283175,-12.5959886688182,
118.64440646347)) ;
#192721 = CARTESIAN_POINT('Ctrl Pts',(-7.44813083508317,-12.5383601361984,
118.597467295831)) ;
#192722 = CARTESIAN_POINT('Ctrl Pts',(-7.52193469394733,-12.5383600922288,
118.573236301185)) ;
#192723 = CARTESIAN_POINT('Ctrl Pts',(-7.59573855281146,-12.5383600482591,
118.54900530654)) ;
#192724 = CARTESIAN_POINT('Ctrl Pts',(-7.61114947056002,-12.5959885808789,
118.595944474179)) ;
#192725 = CARTESIAN_POINT('Ctrl Pts',(-7.54064541308495,-12.8143066918053,
118.416638915935)) ;
#192726 = CARTESIAN_POINT('Ctrl Pts',(-7.56026899454005,-12.8567794160869,
118.476409177672)) ;
#192727 = CARTESIAN_POINT('Ctrl Pts',(-7.48646514127264,-12.8567794648258,
118.500640189364)) ;
#192728 = CARTESIAN_POINT('Ctrl Pts',(-7.41266128800525,-12.8567795135646,
118.524871201056)) ;
#192729 = CARTESIAN_POINT('Ctrl Pts',(-7.39303770655016,-12.814306789283,
118.46510093932)) ;
#192730 = CARTESIAN_POINT('Ctrl Pts',(-7.37341412509507,-12.7718340650015,
118.405330677583)) ;
#192731 = CARTESIAN_POINT('Ctrl Pts',(-7.44721797836247,-12.7718340162626,
118.381099665891)) ;
#192732 = CARTESIAN_POINT('Ctrl Pts',(-7.52102183162987,-12.7718339675238,
118.356868654199)) ;
#192733 = CARTESIAN_POINT('Ctrl Pts',(-7.54064541308495,-12.8143066918053,
118.416638915935)) ;
#192734 = CARTESIAN_POINT('Ctrl Pts',(-7.49026997235467,-13.0760276863323,
118.29867594851)) ;
#192735 = CARTESIAN_POINT('Ctrl Pts',(-7.51270657196419,-13.1002911910354,
118.367014209835)) ;
#192736 = CARTESIAN_POINT('Ctrl Pts',(-7.4389027239676,-13.1002912381593,
118.391245237581)) ;
#192737 = CARTESIAN_POINT('Ctrl Pts',(-7.36509887597101,-13.1002912852831,
118.415476265327)) ;
#192738 = CARTESIAN_POINT('Ctrl Pts',(-7.34266227636148,-13.07602778058,118.347138004003)) ;
#192739 = CARTESIAN_POINT('Ctrl Pts',(-7.32022567675194,-13.0517642758768,
118.278799742678)) ;
#192740 = CARTESIAN_POINT('Ctrl Pts',(-7.39402952474855,-13.051764228753,
118.254568714932)) ;
#192741 = CARTESIAN_POINT('Ctrl Pts',(-7.46783337274512,-13.0517641816292,
118.230337687185)) ;
#192742 = CARTESIAN_POINT('Ctrl Pts',(-7.49026997235467,-13.0760276863323,
118.29867594851)) ;
#192743 = CARTESIAN_POINT('Ctrl Pts',(-7.46298666678461,-13.3628060373472,
118.251109449983)) ;
#192744 = CARTESIAN_POINT('Ctrl Pts',(-7.48662704438139,-13.3670829170375,
118.32311422501)) ;
#192745 = CARTESIAN_POINT('Ctrl Pts',(-7.41282320058781,-13.3670829569658,
118.347345265558)) ;
#192746 = CARTESIAN_POINT('Ctrl Pts',(-7.33901935679421,-13.3670829968941,
118.371576306106)) ;
#192747 = CARTESIAN_POINT('Ctrl Pts',(-7.31537897919742,-13.3628061172038,
118.299571531079)) ;
#192748 = CARTESIAN_POINT('Ctrl Pts',(-7.2917386016006,-13.3585292375136,
118.227566756052)) ;
#192749 = CARTESIAN_POINT('Ctrl Pts',(-7.36554244539421,-13.3585291975852,
118.203335715504)) ;
#192750 = CARTESIAN_POINT('Ctrl Pts',(-7.4393462891878,-13.3585291576569,
118.179104674956)) ;
#192751 = CARTESIAN_POINT('Ctrl Pts',(-7.46298666678461,-13.3628060373472,
118.251109449983)) ;
#192752 = CARTESIAN_POINT('Ctrl Pts',(-7.46006094552524,-13.6523296523906,
118.277586231545)) ;
#192753 = CARTESIAN_POINT('Ctrl Pts',(-7.48320907995678,-13.6363976370677,
118.348091713465)) ;
#192754 = CARTESIAN_POINT('Ctrl Pts',(-7.40940523890514,-13.636397668316,
118.372322762364)) ;
#192755 = CARTESIAN_POINT('Ctrl Pts',(-7.33560139785351,-13.6363976995644,
118.396553811264)) ;
#192756 = CARTESIAN_POINT('Ctrl Pts',(-7.31245326342196,-13.6523297148873,
118.326048329344)) ;
#192757 = CARTESIAN_POINT('Ctrl Pts',(-7.2893051289904,-13.6682617302103,
118.255542847425)) ;
#192758 = CARTESIAN_POINT('Ctrl Pts',(-7.36310897004204,-13.6682616989619,
118.231311798525)) ;
#192759 = CARTESIAN_POINT('Ctrl Pts',(-7.43691281109367,-13.6682616677135,
118.207080749626)) ;
#192760 = CARTESIAN_POINT('Ctrl Pts',(-7.46006094552524,-13.6523296523906,
118.277586231545)) ;
#192761 = CARTESIAN_POINT('Ctrl Pts',(-7.48069545348148,-13.9253061411165,
118.375831770847)) ;
#192762 = CARTESIAN_POINT('Ctrl Pts',(-7.50170537191064,-13.8902899618178,
118.439824591971)) ;
#192763 = CARTESIAN_POINT('Ctrl Pts',(-7.42790153228325,-13.8902899830873,
118.464055645208)) ;
#192764 = CARTESIAN_POINT('Ctrl Pts',(-7.35409769265585,-13.8902900043567,
118.488286698446)) ;
#192765 = CARTESIAN_POINT('Ctrl Pts',(-7.3330877742267,-13.9253061836553,
118.424293877322)) ;
#192766 = CARTESIAN_POINT('Ctrl Pts',(-7.31207785579753,-13.960322362954,
118.360301056197)) ;
#192767 = CARTESIAN_POINT('Ctrl Pts',(-7.38588169542493,-13.9603223416845,
118.33607000296)) ;
#192768 = CARTESIAN_POINT('Ctrl Pts',(-7.45968553505234,-13.9603223204151,
118.311838949722)) ;
#192769 = CARTESIAN_POINT('Ctrl Pts',(-7.48069545348148,-13.9253061411165,
118.375831770847)) ;
#192770 = CARTESIAN_POINT('Ctrl Pts',(-7.52318773450401,-14.1634851116196,
118.540904235974)) ;
#192771 = CARTESIAN_POINT('Ctrl Pts',(-7.54052484427258,-14.1117847123966,
118.593710274701)) ;
#192772 = CARTESIAN_POINT('Ctrl Pts',(-7.46672100428935,-14.1117847230889,
118.617941326854)) ;
#192773 = CARTESIAN_POINT('Ctrl Pts',(-7.39291716430611,-14.1117847337813,
118.642172379008)) ;
#192774 = CARTESIAN_POINT('Ctrl Pts',(-7.37558005453754,-14.1634851330044,
118.589366340281)) ;
#192775 = CARTESIAN_POINT('Ctrl Pts',(-7.35824294476899,-14.2151855322274,
118.536560301554)) ;
#192776 = CARTESIAN_POINT('Ctrl Pts',(-7.43204678475222,-14.215185521535,
118.512329249401)) ;
#192777 = CARTESIAN_POINT('Ctrl Pts',(-7.50585062473544,-14.2151855108427,
118.488098197247)) ;
#192778 = CARTESIAN_POINT('Ctrl Pts',(-7.52318773450401,-14.1634851116196,
118.540904235974)) ;
#192779 = CARTESIAN_POINT('Ctrl Pts',(-7.58295692722175,-14.3462889334782,
118.758272828896)) ;
#192780 = CARTESIAN_POINT('Ctrl Pts',(-7.59541578115089,-14.2817465742021,
118.796220487547)) ;
#192781 = CARTESIAN_POINT('Ctrl Pts',(-7.52161194040355,-14.2817465788419,
118.820451537374)) ;
#192782 = CARTESIAN_POINT('Ctrl Pts',(-7.44780809965619,-14.2817465834817,
118.8446825872)) ;
#192783 = CARTESIAN_POINT('Ctrl Pts',(-7.43534924572705,-14.3462889427578,
118.806734928548)) ;
#192784 = CARTESIAN_POINT('Ctrl Pts',(-7.42289039179789,-14.4108313020339,
118.768787269897)) ;
#192785 = CARTESIAN_POINT('Ctrl Pts',(-7.49669423254526,-14.4108312973941,
118.74455622007)) ;
#192786 = CARTESIAN_POINT('Ctrl Pts',(-7.5704980732926,-14.4108312927542,
118.720325170244)) ;
#192787 = CARTESIAN_POINT('Ctrl Pts',(-7.58295692722175,-14.3462889334782,
118.758272828896)) ;
#192788 = CARTESIAN_POINT('Ctrl Pts',(-7.65565943967387,-14.463737953108,
119.015219281916)) ;
#192789 = CARTESIAN_POINT('Ctrl Pts',(-7.66232572208676,-14.3908972873577,
119.035523702473)) ;
#192790 = CARTESIAN_POINT('Ctrl Pts',(-7.58852187983193,-14.3908972879061,
119.059754747708)) ;
#192791 = CARTESIAN_POINT('Ctrl Pts',(-7.51471803757708,-14.3908972884545,
119.083985792943)) ;
#192792 = CARTESIAN_POINT('Ctrl Pts',(-7.50805175516422,-14.4637379542048,
119.063681372385)) ;
#192793 = CARTESIAN_POINT('Ctrl Pts',(-7.50138547275135,-14.5365786199551,
119.043376951828)) ;
#192794 = CARTESIAN_POINT('Ctrl Pts',(-7.57518931500617,-14.5365786194067,
119.019145906593)) ;
#192795 = CARTESIAN_POINT('Ctrl Pts',(-7.64899315726101,-14.5365786188583,
118.994914861359)) ;
#192796 = CARTESIAN_POINT('Ctrl Pts',(-7.65565943967387,-14.463737953108,
119.015219281916)) ;
#192797 = CARTESIAN_POINT('Ctrl Pts',(-7.7350979162589,-14.5058926586063,
119.292671656904)) ;
#192798 = CARTESIAN_POINT('Ctrl Pts',(-7.73549259249236,-14.4299991748241,
119.293873777041)) ;
#192799 = CARTESIAN_POINT('Ctrl Pts',(-7.66168874891406,-14.4299991745337,
119.318104818244)) ;
#192800 = CARTESIAN_POINT('Ctrl Pts',(-7.58788490533576,-14.4299991742434,
119.342335859448)) ;
#192801 = CARTESIAN_POINT('Ctrl Pts',(-7.5874902291023,-14.5058926580256,
119.341133739311)) ;
#192802 = CARTESIAN_POINT('Ctrl Pts',(-7.58709555286883,-14.5817861418077,
119.339931619175)) ;
#192803 = CARTESIAN_POINT('Ctrl Pts',(-7.66089939644714,-14.5817861420981,
119.315700577971)) ;
#192804 = CARTESIAN_POINT('Ctrl Pts',(-7.73470324002543,-14.5817861423884,
119.291469536767)) ;
#192805 = CARTESIAN_POINT('Ctrl Pts',(-7.7350979162589,-14.5058926586063,
119.292671656904)) ;
#192806 = CARTESIAN_POINT('Ctrl Pts',(-7.81459046386314,-14.4703114180475,
119.570193330485)) ;
#192807 = CARTESIAN_POINT('Ctrl Pts',(-7.80870234557667,-14.3967894542526,
119.552259072284)) ;
#192808 = CARTESIAN_POINT('Ctrl Pts',(-7.73489850128906,-14.3967894548516,
119.576490111328)) ;
#192809 = CARTESIAN_POINT('Ctrl Pts',(-7.66109465700145,-14.3967894554506,
119.600721150371)) ;
#192810 = CARTESIAN_POINT('Ctrl Pts',(-7.6669827752879,-14.4703114192455,
119.618655408572)) ;
#192811 = CARTESIAN_POINT('Ctrl Pts',(-7.67287089357435,-14.5438333830403,
119.636589666772)) ;
#192812 = CARTESIAN_POINT('Ctrl Pts',(-7.74667473786198,-14.5438333824413,
119.612358627729)) ;
#192813 = CARTESIAN_POINT('Ctrl Pts',(-7.82047858214959,-14.5438333818423,
119.588127588686)) ;
#192814 = CARTESIAN_POINT('Ctrl Pts',(-7.81459046386314,-14.4703114180475,
119.570193330485)) ;
#192815 = CARTESIAN_POINT('Ctrl Pts',(-7.88822750778698,-14.359046732277,
119.83002759752)) ;
#192816 = CARTESIAN_POINT('Ctrl Pts',(-7.87645281961665,-14.2931851690986,
119.794163797256)) ;
#192817 = CARTESIAN_POINT('Ctrl Pts',(-7.80264897532485,-14.2931851708445,
119.818394836286)) ;
#192818 = CARTESIAN_POINT('Ctrl Pts',(-7.72884513103306,-14.2931851725905,
119.842625875317)) ;
#192819 = CARTESIAN_POINT('Ctrl Pts',(-7.74061981920339,-14.3590467357689,
119.878489675581)) ;
#192820 = CARTESIAN_POINT('Ctrl Pts',(-7.75239450737372,-14.4249082989473,
119.914353475844)) ;
#192821 = CARTESIAN_POINT('Ctrl Pts',(-7.82619835166552,-14.4249082972013,
119.890122436814)) ;
#192822 = CARTESIAN_POINT('Ctrl Pts',(-7.90000219595731,-14.4249082954554,
119.865891397783)) ;
#192823 = CARTESIAN_POINT('Ctrl Pts',(-7.88822750778698,-14.359046732277,
119.83002759752)) ;
#192824 = CARTESIAN_POINT('Ctrl Pts',(-7.94951260678091,-14.1801475215603,
120.05219962572)) ;
#192825 = CARTESIAN_POINT('Ctrl Pts',(-7.93270627576756,-14.1266811735188,
120.001010253166)) ;
#192826 = CARTESIAN_POINT('Ctrl Pts',(-7.8589024321799,-14.1266811744766,
120.025241294341)) ;
#192827 = CARTESIAN_POINT('Ctrl Pts',(-7.78509858859223,-14.1266811754344,
120.049472335516)) ;
#192828 = CARTESIAN_POINT('Ctrl Pts',(-7.80190491960559,-14.1801475234759,
120.100661708071)) ;
#192829 = CARTESIAN_POINT('Ctrl Pts',(-7.81871125061892,-14.2336138715174,
120.151851080625)) ;
#192830 = CARTESIAN_POINT('Ctrl Pts',(-7.89251509420659,-14.2336138705596,
120.12762003945)) ;
#192831 = CARTESIAN_POINT('Ctrl Pts',(-7.96631893779426,-14.2336138696018,
120.103388998275)) ;
#192832 = CARTESIAN_POINT('Ctrl Pts',(-7.94951260678091,-14.1801475215603,
120.05219962572)) ;
#192833 = CARTESIAN_POINT('Ctrl Pts',(-7.99329952727136,-13.9475293921824,
120.220946453046)) ;
#192834 = CARTESIAN_POINT('Ctrl Pts',(-7.97267903201572,-13.9102276293421,
120.158139751557)) ;
#192835 = CARTESIAN_POINT('Ctrl Pts',(-7.89887518906826,-13.9102276274691,
120.182370794682)) ;
#192836 = CARTESIAN_POINT('Ctrl Pts',(-7.82507134612079,-13.910227625596,
120.206601837807)) ;
#192837 = CARTESIAN_POINT('Ctrl Pts',(-7.84569184137644,-13.9475293884362,
120.269408539297)) ;
#192838 = CARTESIAN_POINT('Ctrl Pts',(-7.86631233663205,-13.9848311512765,
120.332215240786)) ;
#192839 = CARTESIAN_POINT('Ctrl Pts',(-7.94011617957952,-13.9848311531496,
120.307984197661)) ;
#192840 = CARTESIAN_POINT('Ctrl Pts',(-8.01392002252699,-13.9848311550226,
120.283753154536)) ;
#192841 = CARTESIAN_POINT('Ctrl Pts',(-7.99329952727136,-13.9475293921824,
120.220946453046)) ;
#192842 = CARTESIAN_POINT('Ctrl Pts',(-8.01597054361897,-13.6767289638667,
120.325436166346)) ;
#192843 = CARTESIAN_POINT('Ctrl Pts',(-7.99300362757276,-13.6582814319255,
120.255482645625)) ;
#192844 = CARTESIAN_POINT('Ctrl Pts',(-7.91919978485194,-13.6582814248753,
120.279713689441)) ;
#192845 = CARTESIAN_POINT('Ctrl Pts',(-7.84539594213114,-13.658281417825,
120.303944733256)) ;
#192846 = CARTESIAN_POINT('Ctrl Pts',(-7.86836285817735,-13.6767289497662,
120.373898253977)) ;
#192847 = CARTESIAN_POINT('Ctrl Pts',(-7.89132977422359,-13.6951764817073,
120.443851774699)) ;
#192848 = CARTESIAN_POINT('Ctrl Pts',(-7.96513361694439,-13.6951764887576,
120.419620730883)) ;
#192849 = CARTESIAN_POINT('Ctrl Pts',(-8.0389374596652,-13.6951764958078,
120.395389687068)) ;
#192850 = CARTESIAN_POINT('Ctrl Pts',(-8.01597054361897,-13.6767289638667,
120.325436166346)) ;
#192851 = CARTESIAN_POINT('Ctrl Pts',(-8.01511316564377,-13.3875048973073,
120.358247068628)) ;
#192852 = CARTESIAN_POINT('Ctrl Pts',(-7.99143972407433,-13.3892252145517,
120.286141585044)) ;
#192853 = CARTESIAN_POINT('Ctrl Pts',(-7.91763588076485,-13.3892252011116,
120.310372627067)) ;
#192854 = CARTESIAN_POINT('Ctrl Pts',(-7.84383203745539,-13.3892251876716,
120.334603669089)) ;
#192855 = CARTESIAN_POINT('Ctrl Pts',(-7.86750547902483,-13.3875048704272,
120.406709152673)) ;
#192856 = CARTESIAN_POINT('Ctrl Pts',(-7.89117892059427,-13.3857845531828,
120.478814636257)) ;
#192857 = CARTESIAN_POINT('Ctrl Pts',(-7.96498276390374,-13.3857845666228,
120.454583594235)) ;
#192858 = CARTESIAN_POINT('Ctrl Pts',(-8.03878660721323,-13.3857845800629,
120.430352552212)) ;
#192859 = CARTESIAN_POINT('Ctrl Pts',(-8.01511316564377,-13.3875048973073,
120.358247068628)) ;
#192860 = CARTESIAN_POINT('Ctrl Pts',(-7.98972953882453,-13.0987597443669,
120.316574379657)) ;
#192861 = CARTESIAN_POINT('Ctrl Pts',(-7.96705640494142,-13.1206437742592,
120.247515671714)) ;
#192862 = CARTESIAN_POINT('Ctrl Pts',(-7.89325255970313,-13.1206437527101,
120.271746707862)) ;
#192863 = CARTESIAN_POINT('Ctrl Pts',(-7.81944871446484,-13.120643731161,
120.29597774401)) ;
#192864 = CARTESIAN_POINT('Ctrl Pts',(-7.84212184834797,-13.0987597012687,
120.365036451953)) ;
#192865 = CARTESIAN_POINT('Ctrl Pts',(-7.86479498223106,-13.0768756713763,
120.434095159895)) ;
#192866 = CARTESIAN_POINT('Ctrl Pts',(-7.93859882746936,-13.0768756929254,
120.409864123748)) ;
#192867 = CARTESIAN_POINT('Ctrl Pts',(-8.01240267270764,-13.0768757144745,
120.3856330876)) ;
#192868 = CARTESIAN_POINT('Ctrl Pts',(-7.98972953882453,-13.0987597443669,
120.316574379657)) ;
#192869 = CARTESIAN_POINT('Ctrl Pts',(-7.94136503643611,-12.8352678817982,
120.204599796384)) ;
#192870 = CARTESIAN_POINT('Ctrl Pts',(-7.92130486660037,-12.8755807524781,
120.143499755195)) ;
#192871 = CARTESIAN_POINT('Ctrl Pts',(-7.84750101846071,-12.8755807274115,
120.167730782505)) ;
#192872 = CARTESIAN_POINT('Ctrl Pts',(-7.77369717032104,-12.8755807023449,
120.191961809816)) ;
#192873 = CARTESIAN_POINT('Ctrl Pts',(-7.79375734015679,-12.8352678316651,
120.253061851005)) ;
#192874 = CARTESIAN_POINT('Ctrl Pts',(-7.81381750999251,-12.7949549609852,
120.314161892194)) ;
#192875 = CARTESIAN_POINT('Ctrl Pts',(-7.88762135813219,-12.7949549860518,
120.289930864884)) ;
#192876 = CARTESIAN_POINT('Ctrl Pts',(-7.96142520627183,-12.7949550111184,
120.265699837573)) ;
#192877 = CARTESIAN_POINT('Ctrl Pts',(-7.94136503643611,-12.8352678817982,
120.204599796384)) ;
#192878 = CARTESIAN_POINT('Ctrl Pts',(-7.87242988112024,-12.6124277096966,
120.030091934832)) ;
#192879 = CARTESIAN_POINT('Ctrl Pts',(-7.85642008035131,-12.6683576543549,
119.981328664133)) ;
#192880 = CARTESIAN_POINT('Ctrl Pts',(-7.78261622841542,-12.6683576284383,
120.005559679881)) ;
#192881 = CARTESIAN_POINT('Ctrl Pts',(-7.7088123764795,-12.6683576025217,
120.029790695629)) ;
#192882 = CARTESIAN_POINT('Ctrl Pts',(-7.72482217724844,-12.6124276578634,
120.078553966327)) ;
#192883 = CARTESIAN_POINT('Ctrl Pts',(-7.74083197801737,-12.5564977132051,
120.127317237025)) ;
#192884 = CARTESIAN_POINT('Ctrl Pts',(-7.81463582995329,-12.5564977391217,
120.103086221278)) ;
#192885 = CARTESIAN_POINT('Ctrl Pts',(-7.88843968188919,-12.5564977650383,
120.07885520553)) ;
#192886 = CARTESIAN_POINT('Ctrl Pts',(-7.87242988112024,-12.6124277096966,
120.030091934832)) ;
#192887 = CARTESIAN_POINT('Ctrl Pts',(-7.78683899646572,-12.4469021309738,
119.804959929397)) ;
#192888 = CARTESIAN_POINT('Ctrl Pts',(-7.77604602433129,-12.5144700927407,
119.772086276799)) ;
#192889 = CARTESIAN_POINT('Ctrl Pts',(-7.70224216784834,-12.5144700706049,
119.796317278697)) ;
#192890 = CARTESIAN_POINT('Ctrl Pts',(-7.62843831136542,-12.514470048469,
119.820548280595)) ;
#192891 = CARTESIAN_POINT('Ctrl Pts',(-7.63923128349984,-12.4469020867021,
119.853421933193)) ;
#192892 = CARTESIAN_POINT('Ctrl Pts',(-7.65002425563427,-12.3793341249352,
119.88629558579)) ;
#192893 = CARTESIAN_POINT('Ctrl Pts',(-7.72382811211722,-12.3793341470711,
119.862064583892)) ;
#192894 = CARTESIAN_POINT('Ctrl Pts',(-7.79763196860014,-12.3793341692069,
119.837833581994)) ;
#192895 = CARTESIAN_POINT('Ctrl Pts',(-7.78683899646572,-12.4469021309738,
119.804959929397)) ;
#192896 = CARTESIAN_POINT('Ctrl Pts',(-7.69042550523445,-12.3516623128813,
119.546789981741)) ;
#192897 = CARTESIAN_POINT('Ctrl Pts',(-7.68561405170315,-12.425977537866,
119.532135069522)) ;
#192898 = CARTESIAN_POINT('Ctrl Pts',(-7.61181019112561,-12.4259775261186,
119.556366058948)) ;
#192899 = CARTESIAN_POINT('Ctrl Pts',(-7.53800633054808,-12.4259775143711,
119.580597048375)) ;
#192900 = CARTESIAN_POINT('Ctrl Pts',(-7.5428177840794,-12.3516622893864,
119.595251960594)) ;
#192901 = CARTESIAN_POINT('Ctrl Pts',(-7.54762923761071,-12.2773470644017,
119.609906872813)) ;
#192902 = CARTESIAN_POINT('Ctrl Pts',(-7.62143309818823,-12.2773470761492,
119.585675883387)) ;
#192903 = CARTESIAN_POINT('Ctrl Pts',(-7.69523695876578,-12.2773470878966,
119.56144489396)) ;
#192904 = CARTESIAN_POINT('Ctrl Pts',(-7.69042550523445,-12.3516623128813,
119.546789981741)) ;
#192905 = CARTESIAN_POINT('Ctrl Pts',(-7.58980441319952,-12.3325403630455,
119.275594411463)) ;
#192906 = CARTESIAN_POINT('Ctrl Pts',(-7.59128119877771,-12.4082975181779,
119.280092460837)) ;
#192907 = CARTESIAN_POINT('Ctrl Pts',(-7.51747733573818,-12.4082975217576,
119.304323442765)) ;
#192908 = CARTESIAN_POINT('Ctrl Pts',(-7.44367347269863,-12.4082975253373,
119.328554424693)) ;
#192909 = CARTESIAN_POINT('Ctrl Pts',(-7.44219668712044,-12.3325403702048,
119.324056375318)) ;
#192910 = CARTESIAN_POINT('Ctrl Pts',(-7.44071990154224,-12.2567832150723,
119.319558325943)) ;
#192911 = CARTESIAN_POINT('Ctrl Pts',(-7.51452376458177,-12.2567832114927,
119.295327344016)) ;
#192912 = CARTESIAN_POINT('Ctrl Pts',(-7.58832762762131,-12.256783207913,
119.271096362088)) ;
#192913 = CARTESIAN_POINT('Ctrl Pts',(-7.58980441319952,-12.3325403630455,
119.275594411463)) ;
#192914 = CARTESIAN_POINT('Ctrl Pts',(-7.48997422897821,-12.3912337324793,
119.007116896225)) ;
#192915 = CARTESIAN_POINT('Ctrl Pts',(-7.49768665308937,-12.4630030921761,
119.030607694275)) ;
#192916 = CARTESIAN_POINT('Ctrl Pts',(-7.42388278832447,-12.4630031154162,
119.054838670948)) ;
#192917 = CARTESIAN_POINT('Ctrl Pts',(-7.35007892355954,-12.4630031386562,
119.07906964762)) ;
#192918 = CARTESIAN_POINT('Ctrl Pts',(-7.34236649944839,-12.3912337789595,
119.05557884957)) ;
#192919 = CARTESIAN_POINT('Ctrl Pts',(-7.33465407533718,-12.3194644192627,
119.03208805152)) ;
#192920 = CARTESIAN_POINT('Ctrl Pts',(-7.40845794010213,-12.3194643960226,
119.007857074848)) ;
#192921 = CARTESIAN_POINT('Ctrl Pts',(-7.48226180486705,-12.3194643727826,
118.983626098175)) ;
#192922 = CARTESIAN_POINT('Ctrl Pts',(-7.48997422897821,-12.3912337324793,
119.007116896225)) ;
#192923 = CARTESIAN_POINT('Ctrl Pts',(-7.39875944406223,-12.5231371749147,
118.764667007709)) ;
#192924 = CARTESIAN_POINT('Ctrl Pts',(-7.41211941150982,-12.5858011581757,
118.805359311403)) ;
#192925 = CARTESIAN_POINT('Ctrl Pts',(-7.33831554770245,-12.5858012027222,
118.829590290992)) ;
#192926 = CARTESIAN_POINT('Ctrl Pts',(-7.26451168389508,-12.5858012472688,
118.853821270581)) ;
#192927 = CARTESIAN_POINT('Ctrl Pts',(-7.25115171644747,-12.5231372640078,
118.813128966887)) ;
#192928 = CARTESIAN_POINT('Ctrl Pts',(-7.23779174899989,-12.4604732807469,
118.772436663194)) ;
#192929 = CARTESIAN_POINT('Ctrl Pts',(-7.31159561280726,-12.4604732362004,
118.748205683605)) ;
#192930 = CARTESIAN_POINT('Ctrl Pts',(-7.38539947661462,-12.4604731916538,
118.723974704016)) ;
#192931 = CARTESIAN_POINT('Ctrl Pts',(-7.39875944406223,-12.5231371749147,
118.764667007709)) ;
#192932 = CARTESIAN_POINT('Ctrl Pts',(-7.32109196511771,-12.7192715563506,
118.563578484396)) ;
#192933 = CARTESIAN_POINT('Ctrl Pts',(-7.33915980720696,-12.7683330936011,
118.618610214499)) ;
#192934 = CARTESIAN_POINT('Ctrl Pts',(-7.26535594639935,-12.7683331592754,
118.642841203224)) ;
#192935 = CARTESIAN_POINT('Ctrl Pts',(-7.19155208559172,-12.7683332249497,
118.66707219195)) ;
#192936 = CARTESIAN_POINT('Ctrl Pts',(-7.17348424350248,-12.7192716876992,
118.612040461847)) ;
#192937 = CARTESIAN_POINT('Ctrl Pts',(-7.15541640141324,-12.6702101504487,
118.557008731744)) ;
#192938 = CARTESIAN_POINT('Ctrl Pts',(-7.22922026222085,-12.6702100847745,
118.532777743019)) ;
#192939 = CARTESIAN_POINT('Ctrl Pts',(-7.30302412302846,-12.6702100191002,
118.508546754293)) ;
#192940 = CARTESIAN_POINT('Ctrl Pts',(-7.32109196511771,-12.7192715563506,
118.563578484396)) ;
#192941 = CARTESIAN_POINT('Ctrl Pts',(-7.2620202481857,-12.9657766439547,
118.419157789103)) ;
#192942 = CARTESIAN_POINT('Ctrl Pts',(-7.28350399172834,-12.9976995891968,
118.484593803754)) ;
#192943 = CARTESIAN_POINT('Ctrl Pts',(-7.20970013616424,-12.9976996732378,
118.508824808451)) ;
#192944 = CARTESIAN_POINT('Ctrl Pts',(-7.13589628060013,-12.9976997572788,
118.533055813148)) ;
#192945 = CARTESIAN_POINT('Ctrl Pts',(-7.11441253705749,-12.9657768120367,
118.467619798496)) ;
#192946 = CARTESIAN_POINT('Ctrl Pts',(-7.09292879351483,-12.9338538667946,
118.402183783844)) ;
#192947 = CARTESIAN_POINT('Ctrl Pts',(-7.16673264907895,-12.9338537827536,
118.377952779148)) ;
#192948 = CARTESIAN_POINT('Ctrl Pts',(-7.24053650464305,-12.9338536987126,
118.353721774451)) ;
#192949 = CARTESIAN_POINT('Ctrl Pts',(-7.2620202481857,-12.9657766439547,
118.419157789103)) ;
#192950 = CARTESIAN_POINT('Ctrl Pts',(-7.22513421757712,-13.2450968718509,
118.342353707646)) ;
#192951 = CARTESIAN_POINT('Ctrl Pts',(-7.24848915948865,-13.2575654456473,
118.413489090504)) ;
#192952 = CARTESIAN_POINT('Ctrl Pts',(-7.17468531110378,-13.2575655425572,
118.437720117068)) ;
#192953 = CARTESIAN_POINT('Ctrl Pts',(-7.10088146271888,-13.2575656394672,
118.461951143631)) ;
#192954 = CARTESIAN_POINT('Ctrl Pts',(-7.07752652080735,-13.2450970656709,
118.390815760773)) ;
#192955 = CARTESIAN_POINT('Ctrl Pts',(-7.05417157889581,-13.2326284918745,
118.319680377915)) ;
#192956 = CARTESIAN_POINT('Ctrl Pts',(-7.12797542728071,-13.2326283949646,
118.295449351351)) ;
#192957 = CARTESIAN_POINT('Ctrl Pts',(-7.20177927566557,-13.2326282980546,
118.271218324788)) ;
#192958 = CARTESIAN_POINT('Ctrl Pts',(-7.22513421757712,-13.2450968718509,
118.342353707646)) ;
#192959 = CARTESIAN_POINT('Ctrl Pts',(-7.21230856442975,-13.5349426349563,
118.338600442269)) ;
#192960 = CARTESIAN_POINT('Ctrl Pts',(-7.23586232244513,-13.527193346992,
118.410341386832)) ;
#192961 = CARTESIAN_POINT('Ctrl Pts',(-7.16205848236148,-13.5271934482019,
118.43457243868)) ;
#192962 = CARTESIAN_POINT('Ctrl Pts',(-7.08825464227779,-13.5271935494119,
118.458803490528)) ;
#192963 = CARTESIAN_POINT('Ctrl Pts',(-7.06470088426242,-13.5349428373762,
118.387062545964)) ;
#192964 = CARTESIAN_POINT('Ctrl Pts',(-7.04114712624704,-13.5426921253405,
118.315321601401)) ;
#192965 = CARTESIAN_POINT('Ctrl Pts',(-7.11495096633071,-13.5426920241306,
118.291090549553)) ;
#192966 = CARTESIAN_POINT('Ctrl Pts',(-7.18875480641438,-13.5426919229206,
118.266859497706)) ;
#192967 = CARTESIAN_POINT('Ctrl Pts',(-7.21230856442975,-13.5349426349563,
118.338600442269)) ;
#192968 = CARTESIAN_POINT('Ctrl Pts',(-7.22361844319658,-13.8188180807124,
118.408663003465)) ;
#192969 = CARTESIAN_POINT('Ctrl Pts',(-7.24568040056356,-13.791238496166,
118.475860163881)) ;
#192970 = CARTESIAN_POINT('Ctrl Pts',(-7.17187656922055,-13.7912385944122,
118.500091242351)) ;
#192971 = CARTESIAN_POINT('Ctrl Pts',(-7.09807273787748,-13.7912386926585,
118.524322320821)) ;
#192972 = CARTESIAN_POINT('Ctrl Pts',(-7.07601078051048,-13.8188182772049,
118.457125160405)) ;
#192973 = CARTESIAN_POINT('Ctrl Pts',(-7.05394882314345,-13.8463978617513,
118.389927999989)) ;
#192974 = CARTESIAN_POINT('Ctrl Pts',(-7.12775265448651,-13.846397763505,
118.365696921519)) ;
#192975 = CARTESIAN_POINT('Ctrl Pts',(-7.20155648582953,-13.8463976652588,
118.341465843049)) ;
#192976 = CARTESIAN_POINT('Ctrl Pts',(-7.22361844319658,-13.8188180807124,
118.408663003465)) ;
#192977 = CARTESIAN_POINT('Ctrl Pts',(-7.25761606914801,-14.0726519250138,
118.547677268349)) ;
#192978 = CARTESIAN_POINT('Ctrl Pts',(-7.27660315486712,-14.027309972795,
118.605508865817)) ;
#192979 = CARTESIAN_POINT('Ctrl Pts',(-7.20279933161886,-14.027310058674,
118.629739968943)) ;
#192980 = CARTESIAN_POINT('Ctrl Pts',(-7.12899550837061,-14.027310144553,
118.653971072068)) ;
#192981 = CARTESIAN_POINT('Ctrl Pts',(-7.11000842265151,-14.0726520967719,
118.5961394746)) ;
#192982 = CARTESIAN_POINT('Ctrl Pts',(-7.09102133693241,-14.1179940489907,
118.538307877132)) ;
#192983 = CARTESIAN_POINT('Ctrl Pts',(-7.16482516018067,-14.1179939631117,
118.514076774006)) ;
#192984 = CARTESIAN_POINT('Ctrl Pts',(-7.23862898342892,-14.1179938772327,
118.489845670881)) ;
#192985 = CARTESIAN_POINT('Ctrl Pts',(-7.25761606914801,-14.0726519250138,
118.547677268349)) ;
#192986 = CARTESIAN_POINT('Ctrl Pts',(-7.31074749652634,-14.2790221021537,
118.744844621079)) ;
#192987 = CARTESIAN_POINT('Ctrl Pts',(-7.32532187540961,-14.2192053591173,
118.789235825497)) ;
#192988 = CARTESIAN_POINT('Ctrl Pts',(-7.25151805873997,-14.2192054253214,
118.81346694866)) ;
#192989 = CARTESIAN_POINT('Ctrl Pts',(-7.17771424207032,-14.2192054915256,
118.837698071823)) ;
#192990 = CARTESIAN_POINT('Ctrl Pts',(-7.16313986318704,-14.279022234562,
118.793306867405)) ;
#192991 = CARTESIAN_POINT('Ctrl Pts',(-7.14856548430374,-14.3388389775984,
118.748915662987)) ;
#192992 = CARTESIAN_POINT('Ctrl Pts',(-7.22236930097341,-14.3388389113943,
118.724684539824)) ;
#192993 = CARTESIAN_POINT('Ctrl Pts',(-7.29617311764304,-14.3388388451902,
118.700453416661)) ;
#192994 = CARTESIAN_POINT('Ctrl Pts',(-7.31074749652634,-14.2790221021537,
118.744844621079)) ;
#192995 = CARTESIAN_POINT('Ctrl Pts',(-7.3788953125628,-14.4246999098251,
118.987880383812)) ;
#192996 = CARTESIAN_POINT('Ctrl Pts',(-7.38799957408608,-14.3546239086375,
119.015610493352)) ;
#192997 = CARTESIAN_POINT('Ctrl Pts',(-7.31419576194719,-14.3546239496232,
119.039841630315)) ;
#192998 = CARTESIAN_POINT('Ctrl Pts',(-7.24039194980831,-14.3546239906089,
119.064072767278)) ;
#192999 = CARTESIAN_POINT('Ctrl Pts',(-7.23128768828504,-14.4246999917965,
119.036342657738)) ;
#193000 = CARTESIAN_POINT('Ctrl Pts',(-7.22218342676176,-14.4947759929842,
119.008612548198)) ;
#193001 = CARTESIAN_POINT('Ctrl Pts',(-7.29598723890066,-14.4947759519985,
118.984381411236)) ;
#193002 = CARTESIAN_POINT('Ctrl Pts',(-7.36979105103954,-14.4947759110128,
118.960150274273)) ;
#193003 = CARTESIAN_POINT('Ctrl Pts',(-7.3788953125628,-14.4246999098251,
118.987880383812)) ;
#193004 = CARTESIAN_POINT('Ctrl Pts',(-7.45654115033611,-14.4982101688668,
119.259955705994)) ;
#193005 = CARTESIAN_POINT('Ctrl Pts',(-7.45950188374549,-14.4228974545996,
119.268973620183)) ;
#193006 = CARTESIAN_POINT('Ctrl Pts',(-7.38569807341447,-14.4228974671485,
119.293204762652)) ;
#193007 = CARTESIAN_POINT('Ctrl Pts',(-7.31189426308347,-14.4228974796974,
119.317435905121)) ;
#193008 = CARTESIAN_POINT('Ctrl Pts',(-7.30893352967411,-14.4982101939646,
119.308417990932)) ;
#193009 = CARTESIAN_POINT('Ctrl Pts',(-7.30597279626475,-14.5735229082318,
119.299400076744)) ;
#193010 = CARTESIAN_POINT('Ctrl Pts',(-7.37977660659575,-14.5735228956829,
119.275168934274)) ;
#193011 = CARTESIAN_POINT('Ctrl Pts',(-7.45358041692675,-14.573522883134,
119.250937791805)) ;
#193012 = CARTESIAN_POINT('Ctrl Pts',(-7.45654115033611,-14.4982101688668,
119.259955705994)) ;
#193013 = CARTESIAN_POINT('Ctrl Pts',(-7.53681769059801,-14.4940193671701,
119.539912255601)) ;
#193014 = CARTESIAN_POINT('Ctrl Pts',(-7.53344471814759,-14.4188869609571,
119.529638723729)) ;
#193015 = CARTESIAN_POINT('Ctrl Pts',(-7.45964090689752,-14.4188869452096,
119.553869863399)) ;
#193016 = CARTESIAN_POINT('Ctrl Pts',(-7.38583709564743,-14.4188869294622,
119.578101003069)) ;
#193017 = CARTESIAN_POINT('Ctrl Pts',(-7.38921006809786,-14.4940193356751,
119.588374534941)) ;
#193018 = CARTESIAN_POINT('Ctrl Pts',(-7.39258304054826,-14.5691517418881,
119.598648066814)) ;
#193019 = CARTESIAN_POINT('Ctrl Pts',(-7.46638685179835,-14.5691517576355,
119.574416927144)) ;
#193020 = CARTESIAN_POINT('Ctrl Pts',(-7.54019066304844,-14.569151773383,
119.550185787474)) ;
#193021 = CARTESIAN_POINT('Ctrl Pts',(-7.53681769059801,-14.4940193671701,
119.539912255601)) ;
#193022 = CARTESIAN_POINT('Ctrl Pts',(-7.61359015495078,-14.4126640845972,
119.809245865358)) ;
#193023 = CARTESIAN_POINT('Ctrl Pts',(-7.6041176047322,-14.3430991702555,
119.780394003839)) ;
#193024 = CARTESIAN_POINT('Ctrl Pts',(-7.53031378994821,-14.3430991291711,
119.804625132746)) ;
#193025 = CARTESIAN_POINT('Ctrl Pts',(-7.45650997516426,-14.3430990880866,
119.828856261652)) ;
#193026 = CARTESIAN_POINT('Ctrl Pts',(-7.46598252538283,-14.4126640024283,
119.857708123171)) ;
#193027 = CARTESIAN_POINT('Ctrl Pts',(-7.47545507560144,-14.48222891677,119.886559984689)) ;
#193028 = CARTESIAN_POINT('Ctrl Pts',(-7.54925889038541,-14.4822289578544,
119.862328855783)) ;
#193029 = CARTESIAN_POINT('Ctrl Pts',(-7.62306270516939,-14.4822289989389,
119.838097726877)) ;
#193030 = CARTESIAN_POINT('Ctrl Pts',(-7.61359015495078,-14.4126640845972,
119.809245865358)) ;
#193031 = CARTESIAN_POINT('Ctrl Pts',(-7.68028577616197,-14.2606219622614,
120.047758542915)) ;
#193032 = CARTESIAN_POINT('Ctrl Pts',(-7.66541066509042,-14.2015682240357,
120.002451352817)) ;
#193033 = CARTESIAN_POINT('Ctrl Pts',(-7.59160684489074,-14.2015681626728,
120.026682465228)) ;
#193034 = CARTESIAN_POINT('Ctrl Pts',(-7.51780302469103,-14.2015681013099,
120.050913577639)) ;
#193035 = CARTESIAN_POINT('Ctrl Pts',(-7.53267813576259,-14.2606218395355,
120.096220767737)) ;
#193036 = CARTESIAN_POINT('Ctrl Pts',(-7.54755324683412,-14.3196755777612,
120.141527957835)) ;
#193037 = CARTESIAN_POINT('Ctrl Pts',(-7.62135706703383,-14.3196756391241,
120.117296845424)) ;
#193038 = CARTESIAN_POINT('Ctrl Pts',(-7.6951608872335,-14.319675700487,120.093065733013)) ;
#193039 = CARTESIAN_POINT('Ctrl Pts',(-7.68028577616197,-14.2606219622614,
120.047758542915)) ;
#193040 = CARTESIAN_POINT('Ctrl Pts',(-7.7318882296266,-14.047641669402,120.240446930669)) ;
#193041 = CARTESIAN_POINT('Ctrl Pts',(-7.71265306933839,-14.003368790847,
120.181859734261)) ;
#193042 = CARTESIAN_POINT('Ctrl Pts',(-7.63884924213539,-14.0033687165429,
120.206090825341)) ;
#193043 = CARTESIAN_POINT('Ctrl Pts',(-7.56504541493244,-14.0033686422388,
120.230321916421)) ;
#193044 = CARTESIAN_POINT('Ctrl Pts',(-7.58428057522066,-14.0476415207938,
120.28890911283)) ;
#193045 = CARTESIAN_POINT('Ctrl Pts',(-7.60351573550891,-14.0919143993488,
120.347496309238)) ;
#193046 = CARTESIAN_POINT('Ctrl Pts',(-7.67731956271188,-14.0919144736529,
120.323265218158)) ;
#193047 = CARTESIAN_POINT('Ctrl Pts',(-7.75112338991485,-14.0919145479569,
120.299034127078)) ;
#193048 = CARTESIAN_POINT('Ctrl Pts',(-7.7318882296266,-14.047641669402,120.240446930669)) ;
#193049 = CARTESIAN_POINT('Ctrl Pts',(-7.76358715017083,-13.7890886844739,
120.37254159039)) ;
#193050 = CARTESIAN_POINT('Ctrl Pts',(-7.74137425025259,-13.7628006589206,
120.304884679662)) ;
#193051 = CARTESIAN_POINT('Ctrl Pts',(-7.6675704155426,-13.7628005801191,
120.329115747877)) ;
#193052 = CARTESIAN_POINT('Ctrl Pts',(-7.59376658083258,-13.7628005013175,
120.353346816092)) ;
#193053 = CARTESIAN_POINT('Ctrl Pts',(-7.61597948075081,-13.7890885268708,
120.42100372682)) ;
#193054 = CARTESIAN_POINT('Ctrl Pts',(-7.63819238066901,-13.8153765524241,
120.488660637548)) ;
#193055 = CARTESIAN_POINT('Ctrl Pts',(-7.71199621537903,-13.8153766312257,
120.464429569334)) ;
#193056 = CARTESIAN_POINT('Ctrl Pts',(-7.78580005008903,-13.8153767100272,
120.440198501119)) ;
#193057 = CARTESIAN_POINT('Ctrl Pts',(-7.76358715017083,-13.7890886844739,
120.37254159039)) ;
#193058 = CARTESIAN_POINT('Ctrl Pts',(-7.77233151699431,-13.5048564724281,
120.434599900892)) ;
#193059 = CARTESIAN_POINT('Ctrl Pts',(-7.7487415484172,-13.4983736613525,
120.362748661352)) ;
#193060 = CARTESIAN_POINT('Ctrl Pts',(-7.67493770671943,-13.4983735848724,
120.386979708283)) ;
#193061 = CARTESIAN_POINT('Ctrl Pts',(-7.60113386502165,-13.4983735083923,
120.411210755214)) ;
#193062 = CARTESIAN_POINT('Ctrl Pts',(-7.62472383359876,-13.5048563194679,
120.483061994755)) ;
#193063 = CARTESIAN_POINT('Ctrl Pts',(-7.64831380217588,-13.5113391305435,
120.554913234296)) ;
#193064 = CARTESIAN_POINT('Ctrl Pts',(-7.72211764387365,-13.5113392070236,
120.530682187364)) ;
#193065 = CARTESIAN_POINT('Ctrl Pts',(-7.79592148557143,-13.5113392835037,
120.506451140433)) ;
#193066 = CARTESIAN_POINT('Ctrl Pts',(-7.77233151699431,-13.5048564724281,
120.434599900892)) ;
#193067 = CARTESIAN_POINT('Ctrl Pts',(-7.75695691433069,-13.2147190164361,
120.42316254752)) ;
#193068 = CARTESIAN_POINT('Ctrl Pts',(-7.73367243907768,-13.2284837281292,
120.352241791491)) ;
#193069 = CARTESIAN_POINT('Ctrl Pts',(-7.65986859140231,-13.2284836599234,
120.376472820216)) ;
#193070 = CARTESIAN_POINT('Ctrl Pts',(-7.58606474372696,-13.2284835917175,
120.40070384894)) ;
#193071 = CARTESIAN_POINT('Ctrl Pts',(-7.60934921897998,-13.2147188800244,
120.471624604969)) ;
#193072 = CARTESIAN_POINT('Ctrl Pts',(-7.63263369423298,-13.2009541683313,
120.542545360997)) ;
#193073 = CARTESIAN_POINT('Ctrl Pts',(-7.70643754190834,-13.2009542365372,
120.518314332273)) ;
#193074 = CARTESIAN_POINT('Ctrl Pts',(-7.7802413895837,-13.200954304743,120.494083303548)) ;
#193075 = CARTESIAN_POINT('Ctrl Pts',(-7.75695691433069,-13.2147190164361,
120.42316254752)) ;
#193076 = CARTESIAN_POINT('Ctrl Pts',(-7.71767702013797,-12.9381997507725,
120.339020142556)) ;
#193077 = CARTESIAN_POINT('Ctrl Pts',(-7.69636520807471,-12.9712919342548,
120.27410780048)) ;
#193078 = CARTESIAN_POINT('Ctrl Pts',(-7.62256135601241,-12.9712918799021,
120.298338815843)) ;
#193079 = CARTESIAN_POINT('Ctrl Pts',(-7.5487575039501,-12.9712918255494,
120.322569831205)) ;
#193080 = CARTESIAN_POINT('Ctrl Pts',(-7.5700693160134,-12.9381996420671,
120.387482173282)) ;
#193081 = CARTESIAN_POINT('Ctrl Pts',(-7.59138112807666,-12.9051074585849,
120.452394515358)) ;
#193082 = CARTESIAN_POINT('Ctrl Pts',(-7.66518498013894,-12.9051075129375,
120.428163499995)) ;
#193083 = CARTESIAN_POINT('Ctrl Pts',(-7.73898883220124,-12.9051075672902,
120.403932484633)) ;
#193084 = CARTESIAN_POINT('Ctrl Pts',(-7.71767702013797,-12.9381997507725,
120.339020142556)) ;
#193085 = CARTESIAN_POINT('Ctrl Pts',(-7.65626840330517,-12.695688487741,
120.187572939771)) ;
#193086 = CARTESIAN_POINT('Ctrl Pts',(-7.63847525050966,-12.745763523541,
120.133377866284)) ;
#193087 = CARTESIAN_POINT('Ctrl Pts',(-7.56467139637205,-12.7457634857973,
120.157608875326)) ;
#193088 = CARTESIAN_POINT('Ctrl Pts',(-7.49086754223442,-12.7457634480537,
120.181839884368)) ;
#193089 = CARTESIAN_POINT('Ctrl Pts',(-7.50866069502992,-12.6956884122536,
120.236034957854)) ;
#193090 = CARTESIAN_POINT('Ctrl Pts',(-7.5264538478254,-12.6456133764535,
120.29023003134)) ;
#193091 = CARTESIAN_POINT('Ctrl Pts',(-7.60025770196303,-12.6456134141972,
120.265999022298)) ;
#193092 = CARTESIAN_POINT('Ctrl Pts',(-7.67406155610066,-12.6456134519409,
120.241768013257)) ;
#193093 = CARTESIAN_POINT('Ctrl Pts',(-7.65626840330517,-12.695688487741,
120.187572939771)) ;
#193094 = CARTESIAN_POINT('Ctrl Pts',(-7.57742636721781,-12.5067830863174,
119.982680330359)) ;
#193095 = CARTESIAN_POINT('Ctrl Pts',(-7.56438187186315,-12.5701233290617,
119.942948901362)) ;
#193096 = CARTESIAN_POINT('Ctrl Pts',(-7.49057801659502,-12.5701233053132,
119.96717990696)) ;
#193097 = CARTESIAN_POINT('Ctrl Pts',(-7.41677416132687,-12.5701232815646,
119.991410912558)) ;
#193098 = CARTESIAN_POINT('Ctrl Pts',(-7.42981865668153,-12.5067830388203,
120.031142341556)) ;
#193099 = CARTESIAN_POINT('Ctrl Pts',(-7.4428631520362,-12.443442796076,120.070873770554)) ;
#193100 = CARTESIAN_POINT('Ctrl Pts',(-7.51666700730434,-12.4434428198246,
120.046642764955)) ;
#193101 = CARTESIAN_POINT('Ctrl Pts',(-7.59047086257249,-12.4434428435731,
120.022411759357)) ;
#193102 = CARTESIAN_POINT('Ctrl Pts',(-7.57742636721781,-12.5067830863174,
119.982680330359)) ;
#193103 = CARTESIAN_POINT('Ctrl Pts',(-7.48481654092851,-12.3815987000844,
119.736103835712)) ;
#193104 = CARTESIAN_POINT('Ctrl Pts',(-7.47748391483476,-12.4537757553205,
119.713769839082)) ;
#193105 = CARTESIAN_POINT('Ctrl Pts',(-7.40368006110229,-12.4537757450517,
119.738000849357)) ;
#193106 = CARTESIAN_POINT('Ctrl Pts',(-7.32987620736981,-12.453775734783,
119.762231859633)) ;
#193107 = CARTESIAN_POINT('Ctrl Pts',(-7.33720883346358,-12.3815986795469,
119.784565856264)) ;
#193108 = CARTESIAN_POINT('Ctrl Pts',(-7.34454145955733,-12.3094216243108,
119.806899852894)) ;
#193109 = CARTESIAN_POINT('Ctrl Pts',(-7.41834531328979,-12.3094216345796,
119.782668842618)) ;
#193110 = CARTESIAN_POINT('Ctrl Pts',(-7.49214916702227,-12.3094216448483,
119.758437832343)) ;
#193111 = CARTESIAN_POINT('Ctrl Pts',(-7.48481654092851,-12.3815987000844,
119.736103835712)) ;
#193112 = CARTESIAN_POINT('Ctrl Pts',(-7.38482566750453,-12.3308693682488,
119.467020622765)) ;
#193113 = CARTESIAN_POINT('Ctrl Pts',(-7.3837295176536,-12.4066980840519,
119.463681926591)) ;
#193114 = CARTESIAN_POINT('Ctrl Pts',(-7.30992566488976,-12.4066980849149,
119.487912939817)) ;
#193115 = CARTESIAN_POINT('Ctrl Pts',(-7.2361218121259,-12.4066980857778,
119.512143953043)) ;
#193116 = CARTESIAN_POINT('Ctrl Pts',(-7.23721796197683,-12.3308693699746,
119.515482649216)) ;
#193117 = CARTESIAN_POINT('Ctrl Pts',(-7.23831411182774,-12.2550406541715,
119.51882134539)) ;
#193118 = CARTESIAN_POINT('Ctrl Pts',(-7.3121179645916,-12.2550406533085,
119.494590332164)) ;
#193119 = CARTESIAN_POINT('Ctrl Pts',(-7.38592181735545,-12.2550406524456,
119.470359318938)) ;
#193120 = CARTESIAN_POINT('Ctrl Pts',(-7.38482566750453,-12.3308693682488,
119.467020622765)) ;
#193121 = CARTESIAN_POINT('Ctrl Pts',(-7.28361307124184,-12.3583046491224,
119.194307222016)) ;
#193122 = CARTESIAN_POINT('Ctrl Pts',(-7.28884656543599,-12.4323324318187,
119.210247600737)) ;
#193123 = CARTESIAN_POINT('Ctrl Pts',(-7.21504271877939,-12.4323324320423,
119.234478632564)) ;
#193124 = CARTESIAN_POINT('Ctrl Pts',(-7.14123887212279,-12.4323324322659,
119.258709664392)) ;
#193125 = CARTESIAN_POINT('Ctrl Pts',(-7.13600537792864,-12.3583046495696,
119.242769285671)) ;
#193126 = CARTESIAN_POINT('Ctrl Pts',(-7.13077188373449,-12.2842768668734,
119.226828906951)) ;
#193127 = CARTESIAN_POINT('Ctrl Pts',(-7.20457573039108,-12.2842768666498,
119.202597875123)) ;
#193128 = CARTESIAN_POINT('Ctrl Pts',(-7.27837957704766,-12.2842768664262,
119.178366843295)) ;
#193129 = CARTESIAN_POINT('Ctrl Pts',(-7.28361307124184,-12.3583046491224,
119.194307222016)) ;
#193130 = CARTESIAN_POINT('Ctrl Pts',(-7.18835949562826,-12.4612718878677,
118.939567373986)) ;
#193131 = CARTESIAN_POINT('Ctrl Pts',(-7.19951931791275,-12.5282228863583,
118.973558391361)) ;
#193132 = CARTESIAN_POINT('Ctrl Pts',(-7.12571546644994,-12.5282229072686,
118.99778940855)) ;
#193133 = CARTESIAN_POINT('Ctrl Pts',(-7.05191161498712,-12.5282229281789,
119.022020425739)) ;
#193134 = CARTESIAN_POINT('Ctrl Pts',(-7.04075179270263,-12.4612719296883,
118.988029408363)) ;
#193135 = CARTESIAN_POINT('Ctrl Pts',(-7.02959197041813,-12.3943209311977,
118.954038390988)) ;
#193136 = CARTESIAN_POINT('Ctrl Pts',(-7.10339582188094,-12.3943209102874,
118.929807373799)) ;
#193137 = CARTESIAN_POINT('Ctrl Pts',(-7.17719967334377,-12.3943208893771,
118.90557635661)) ;
#193138 = CARTESIAN_POINT('Ctrl Pts',(-7.18835949562826,-12.4612718878677,
118.939567373986)) ;
#193139 = CARTESIAN_POINT('Ctrl Pts',(-7.10418260554018,-12.6338543702633,
118.718793259027)) ;
#193140 = CARTESIAN_POINT('Ctrl Pts',(-7.12050081610633,-12.6888516916321,
118.768495896363)) ;
#193141 = CARTESIAN_POINT('Ctrl Pts',(-7.04669698043341,-12.6888516559685,
118.792726961645)) ;
#193142 = CARTESIAN_POINT('Ctrl Pts',(-6.97289314476051,-12.6888516203049,
118.816958026928)) ;
#193143 = CARTESIAN_POINT('Ctrl Pts',(-6.95657493419437,-12.6338542989361,
118.767255389592)) ;
#193144 = CARTESIAN_POINT('Ctrl Pts',(-6.94025672362824,-12.5788569775673,
118.717552752256)) ;
#193145 = CARTESIAN_POINT('Ctrl Pts',(-7.01406055930115,-12.5788570132309,
118.693321686974)) ;
#193146 = CARTESIAN_POINT('Ctrl Pts',(-7.08786439497406,-12.5788570488945,
118.669090621691)) ;
#193147 = CARTESIAN_POINT('Ctrl Pts',(-7.10418260554018,-12.6338543702633,
118.718793259027)) ;
#193148 = CARTESIAN_POINT('Ctrl Pts',(-7.0375316550567,-12.8606317098419,
118.5510569042)) ;
#193149 = CARTESIAN_POINT('Ctrl Pts',(-7.0577969319441,-12.8998873118664,
118.612781665881)) ;
#193150 = CARTESIAN_POINT('Ctrl Pts',(-6.98399307643361,-12.8998874003437,
118.637012670741)) ;
#193151 = CARTESIAN_POINT('Ctrl Pts',(-6.9101892209231,-12.8998874888211,
118.661243675601)) ;
#193152 = CARTESIAN_POINT('Ctrl Pts',(-6.88992394403571,-12.8606318867965,
118.599518913921)) ;
#193153 = CARTESIAN_POINT('Ctrl Pts',(-6.86965866714829,-12.821376284772,
118.53779415224)) ;
#193154 = CARTESIAN_POINT('Ctrl Pts',(-6.94346252265879,-12.8213761962946,
118.51356314738)) ;
#193155 = CARTESIAN_POINT('Ctrl Pts',(-7.0172663781693,-12.8213761078173,
118.48933214252)) ;
#193156 = CARTESIAN_POINT('Ctrl Pts',(-7.0375316550567,-12.8606317098419,
118.5510569042)) ;
#193157 = CARTESIAN_POINT('Ctrl Pts',(-6.99116353791501,-13.129518595729,
118.445436488303)) ;
#193158 = CARTESIAN_POINT('Ctrl Pts',(-7.01396188878876,-13.1500300138352,
118.514876590014)) ;
#193159 = CARTESIAN_POINT('Ctrl Pts',(-6.94015805847674,-13.1500298440004,
118.539107671625)) ;
#193160 = CARTESIAN_POINT('Ctrl Pts',(-6.86635422816467,-13.1500296741656,
118.563338753236)) ;
#193161 = CARTESIAN_POINT('Ctrl Pts',(-6.84355587729091,-13.1295182560594,
118.493898651524)) ;
#193162 = CARTESIAN_POINT('Ctrl Pts',(-6.82075752641711,-13.1090068379532,
118.424458549812)) ;
#193163 = CARTESIAN_POINT('Ctrl Pts',(-6.89456135672918,-13.109007007788,
118.400227468202)) ;
#193164 = CARTESIAN_POINT('Ctrl Pts',(-6.96836518704121,-13.1090071776228,
118.375996386591)) ;
#193165 = CARTESIAN_POINT('Ctrl Pts',(-6.99116353791501,-13.129518595729,
118.445436488303)) ;
#193166 = CARTESIAN_POINT('Ctrl Pts',(-6.97612463268656,-13.3215354698077,
118.423228166981)) ;
#193167 = CARTESIAN_POINT('Ctrl Pts',(-6.99950616509918,-13.3286998701254,
118.494444538894)) ;
#193168 = CARTESIAN_POINT('Ctrl Pts',(-6.92570231417953,-13.3287000326328,
118.518675557737)) ;
#193169 = CARTESIAN_POINT('Ctrl Pts',(-6.85189846325988,-13.3287001951402,
118.54290657658)) ;
#193170 = CARTESIAN_POINT('Ctrl Pts',(-6.82851693084728,-13.3215357948224,
118.471690204667)) ;
#193171 = CARTESIAN_POINT('Ctrl Pts',(-6.80513539843466,-13.3143713945047,
118.400473832754)) ;
#193172 = CARTESIAN_POINT('Ctrl Pts',(-6.87893924935431,-13.3143712319973,
118.376242813911)) ;
#193173 = CARTESIAN_POINT('Ctrl Pts',(-6.95274310027397,-13.31437106949,118.352011795068)) ;
#193174 = CARTESIAN_POINT('Ctrl Pts',(-6.97612463268656,-13.3215354698077,
118.423228166981)) ;
#193175 = CARTESIAN_POINT('Ctrl Pts',(-6.97260578432847,-13.4175644257172,
118.424310057455)) ;
#193176 = CARTESIAN_POINT('Ctrl Pts',(-6.9960004985664,-13.4180062659798,
118.495566580825)) ;
#193177 = CARTESIAN_POINT('Ctrl Pts',(-6.92219665515706,-13.4180063413679,
118.519797622544)) ;
#193178 = CARTESIAN_POINT('Ctrl Pts',(-6.8483928117477,-13.4180064167561,
118.544028664262)) ;
#193179 = CARTESIAN_POINT('Ctrl Pts',(-6.82499809750977,-13.4175645764935,
118.472772140891)) ;
#193180 = CARTESIAN_POINT('Ctrl Pts',(-6.80160338327183,-13.4171227362309,
118.40151561752)) ;
#193181 = CARTESIAN_POINT('Ctrl Pts',(-6.87540722668119,-13.4171226608428,
118.377284575802)) ;
#193182 = CARTESIAN_POINT('Ctrl Pts',(-6.94921107009053,-13.4171225854547,
118.353053534084)) ;
#193183 = CARTESIAN_POINT('Ctrl Pts',(-6.97260578432847,-13.4175644257172,
118.424310057455)) ;
#193184 = CARTESIAN_POINT('',(-18.0519478151656,-12.9727494438644,116.948041367699)) ;
#193185 = CARTESIAN_POINT('Ctrl Pts',(-18.0519478151656,-12.9727494438644,
116.948041367699)) ;
#193186 = CARTESIAN_POINT('Ctrl Pts',(-18.0518351564328,-12.972911356665,
116.947698227376)) ;
#193187 = CARTESIAN_POINT('Ctrl Pts',(-18.0517398746792,-12.9731380019778,
116.947408014528)) ;
#193188 = CARTESIAN_POINT('Ctrl Pts',(-18.051557848478,-12.9737505696884,
116.946853592089)) ;
#193189 = CARTESIAN_POINT('Ctrl Pts',(-18.0514805222992,-12.9741371839328,
116.946618069025)) ;
#193190 = CARTESIAN_POINT('Ctrl Pts',(-18.0512622202171,-12.9755496760429,
116.945953156106)) ;
#193191 = CARTESIAN_POINT('Ctrl Pts',(-18.0511751709774,-12.97682332725,116.945688018167)) ;
#193192 = CARTESIAN_POINT('Ctrl Pts',(-18.0510064245869,-12.9812525255352,
116.945174043889)) ;
#193193 = CARTESIAN_POINT('Ctrl Pts',(-18.0510736978366,-12.985581022285,
116.945378947353)) ;
#193194 = CARTESIAN_POINT('Ctrl Pts',(-18.0517201914724,-13.002503579703,
116.947348062656)) ;
#193195 = CARTESIAN_POINT('Ctrl Pts',(-18.0528587996904,-13.0192459488949,
116.950816079578)) ;
#193196 = CARTESIAN_POINT('Ctrl Pts',(-18.0577446071666,-13.0885454351125,
116.965697460829)) ;
#193197 = CARTESIAN_POINT('Ctrl Pts',(-18.0628205806372,-13.1573238043938,
116.981158057011)) ;
#193198 = CARTESIAN_POINT('Ctrl Pts',(-18.070265376874,-13.3846429728194,
117.003833705135)) ;
#193199 = CARTESIAN_POINT('Ctrl Pts',(-18.0664059866463,-13.5028371896565,
116.992078625212)) ;
#193200 = CARTESIAN_POINT('Ctrl Pts',(-18.0512043586578,-13.7248060299085,
116.945776919132)) ;
#193201 = CARTESIAN_POINT('Ctrl Pts',(-18.0359840744941,-13.842674137476,
116.899418389356)) ;
#193202 = CARTESIAN_POINT('Ctrl Pts',(-17.9911943603994,-14.0637456275394,
116.762996147017)) ;
#193203 = CARTESIAN_POINT('Ctrl Pts',(-17.9610731268689,-14.1629071646497,
116.671251729724)) ;
#193204 = CARTESIAN_POINT('Ctrl Pts',(-17.8991243194425,-14.2984535233359,
116.482565657706)) ;
#193205 = CARTESIAN_POINT('Ctrl Pts',(-17.869856325191,-14.3434390384379,
116.393420069521)) ;
#193206 = CARTESIAN_POINT('Ctrl Pts',(-17.8089893867879,-14.4029494275453,
116.208029195989)) ;
#193207 = CARTESIAN_POINT('Ctrl Pts',(-17.7780240150196,-14.4178650105577,
116.113713669896)) ;
#193208 = CARTESIAN_POINT('Ctrl Pts',(-17.7467422306778,-14.4181080983633,
116.018434402088)) ;
#193209 = CARTESIAN_POINT('Ctrl Pts',(-17.7467422306778,-14.4181080983633,
116.018434402088)) ;
#193210 = CARTESIAN_POINT('Ctrl Pts',(-17.7140007578702,-14.4183625292707,
115.918709158733)) ;
#193211 = CARTESIAN_POINT('Ctrl Pts',(-17.68151856153,-14.4025181298829,115.819773629628)) ;
#193212 = CARTESIAN_POINT('Ctrl Pts',(-17.6187304295439,-14.3392564455755,
115.628531110426)) ;
#193213 = CARTESIAN_POINT('Ctrl Pts',(-17.5887791967788,-14.2916003512295,
115.53730448808)) ;
#193214 = CARTESIAN_POINT('Ctrl Pts',(-17.5267705078295,-14.151880704718,
115.348436026605)) ;
#193215 = CARTESIAN_POINT('Ctrl Pts',(-17.4969972022272,-14.0512183347572,
115.257751341639)) ;
#193216 = CARTESIAN_POINT('Ctrl Pts',(-17.4510294071444,-13.8180971458324,
115.117740854693)) ;
#193217 = CARTESIAN_POINT('Ctrl Pts',(-17.4355506602779,-13.6895955424913,
115.070595089804)) ;
#193218 = CARTESIAN_POINT('Ctrl Pts',(-17.4187282219778,-13.4061630903328,
115.019356657033)) ;
#193219 = CARTESIAN_POINT('Ctrl Pts',(-17.4210961950408,-13.2885837862808,
115.026569120331)) ;
#193220 = CARTESIAN_POINT('Ctrl Pts',(-17.4202558521708,-13.2246311944419,
115.024009571538)) ;
#193221 = CARTESIAN_POINT('Ctrl Pts',(-17.4200515924295,-13.2164449755186,
115.023387429323)) ;
#193222 = CARTESIAN_POINT('Ctrl Pts',(-17.419495435267,-13.2089958125066,
115.021693464342)) ;
#193223 = CARTESIAN_POINT('Ctrl Pts',(-17.4193193828814,-13.207197753218,
115.021157237182)) ;
#193224 = CARTESIAN_POINT('Ctrl Pts',(-17.4189816481387,-13.205177369771,
115.020128551648)) ;
#193225 = CARTESIAN_POINT('Ctrl Pts',(-17.4188544998161,-13.2045590817019,
115.019741278373)) ;
#193226 = CARTESIAN_POINT('Ctrl Pts',(-17.4186056718147,-13.203773671671,
115.018983388429)) ;
#193227 = CARTESIAN_POINT('Ctrl Pts',(-17.4184997792349,-13.2035184810664,
115.018660856717)) ;
#193228 = CARTESIAN_POINT('Ctrl Pts',(-17.4182739978371,-13.2031822301827,
115.017973163009)) ;
#193229 = CARTESIAN_POINT('Ctrl Pts',(-17.4181622393295,-13.2030933380482,
115.017632764627)) ;
#193230 = CARTESIAN_POINT('Ctrl Pts',(-17.4179050608403,-13.203058589859,
115.016849440444)) ;
#193231 = CARTESIAN_POINT('Ctrl Pts',(-17.4177674591844,-13.2031450748712,
115.016430328002)) ;
#193232 = CARTESIAN_POINT('Ctrl Pts',(-17.41741777442,-13.2035491479371,115.015365244631)) ;
#193233 = CARTESIAN_POINT('Ctrl Pts',(-17.4172111107158,-13.2039870459215,
115.014735780413)) ;
#193234 = CARTESIAN_POINT('Ctrl Pts',(-17.4163518420265,-13.2062236928396,
115.012118586628)) ;
#193235 = CARTESIAN_POINT('Ctrl Pts',(-17.4156755712042,-13.2094171488092,
115.010058774739)) ;
#193236 = CARTESIAN_POINT('Ctrl Pts',(-17.412733790245,-13.2255158773085,
115.001098584593)) ;
#193237 = CARTESIAN_POINT('Ctrl Pts',(-17.4096601818318,-13.2522859045867,
114.991736869173)) ;
#193238 = CARTESIAN_POINT('Ctrl Pts',(-17.4014133873562,-13.36215960263,114.966618463816)) ;
#193239 = CARTESIAN_POINT('Ctrl Pts',(-17.3966396346497,-13.4847220177897,
114.952078383432)) ;
#193240 = CARTESIAN_POINT('Ctrl Pts',(-17.4101561115219,-13.7731365150372,
114.993247391109)) ;
#193241 = CARTESIAN_POINT('Ctrl Pts',(-17.4252785357613,-13.9063209144051,
115.039307855321)) ;
#193242 = CARTESIAN_POINT('Ctrl Pts',(-17.471242209048,-14.1522077768049,
115.179305787941)) ;
#193243 = CARTESIAN_POINT('Ctrl Pts',(-17.5023193439156,-14.261499390111,
115.273961726498)) ;
#193244 = CARTESIAN_POINT('Ctrl Pts',(-17.5689134939929,-14.4189847550274,
115.476796762707)) ;
#193245 = CARTESIAN_POINT('Ctrl Pts',(-17.6022386411003,-14.4742659640219,
115.578299783772)) ;
#193246 = CARTESIAN_POINT('Ctrl Pts',(-17.6729310682834,-14.5486809816127,
115.79361751079)) ;
#193247 = CARTESIAN_POINT('Ctrl Pts',(-17.7096845119904,-14.5675899683415,
115.905562570207)) ;
#193248 = CARTESIAN_POINT('Ctrl Pts',(-17.746742230677,-14.5678329226988,
116.018434402086)) ;
#193249 = CARTESIAN_POINT('Ctrl Pts',(-17.746742167295,-14.5678329187858,
116.01843442664)) ;
#193250 = CARTESIAN_POINT('Ctrl Pts',(-17.7601895243844,-14.567921082103,
116.05939291695)) ;
#193251 = CARTESIAN_POINT('Ctrl Pts',(-17.773650564873,-14.5655508478998,
116.100392846403)) ;
#193252 = CARTESIAN_POINT('Ctrl Pts',(-17.787031093405,-14.5607116311535,
116.141147777371)) ;
#193253 = CARTESIAN_POINT('Ctrl Pts',(-17.79258814348,-14.5587018622779,116.158073655273)) ;
#193254 = CARTESIAN_POINT('Ctrl Pts',(-17.7981318063432,-14.556266107077,
116.174958757887)) ;
#193255 = CARTESIAN_POINT('Ctrl Pts',(-17.8036553329622,-14.5534035696439,
116.191782528751)) ;
#193256 = CARTESIAN_POINT('Ctrl Pts',(-17.8294913073762,-14.5400142173367,
116.270474738197)) ;
#193257 = CARTESIAN_POINT('Ctrl Pts',(-17.8548772100185,-14.5172883204691,
116.347795870618)) ;
#193258 = CARTESIAN_POINT('Ctrl Pts',(-17.8791197239657,-14.4859963413062,
116.421634818916)) ;
#193259 = CARTESIAN_POINT('Ctrl Pts',(-17.8846519651774,-14.4788553831903,
116.438485170067)) ;
#193260 = CARTESIAN_POINT('Ctrl Pts',(-17.890124692269,-14.4712685294595,
116.45515424542)) ;
#193261 = CARTESIAN_POINT('Ctrl Pts',(-17.895529724337,-14.463245285136,116.471617101)) ;
#193262 = CARTESIAN_POINT('Ctrl Pts',(-17.9197140688182,-14.4273459783168,
116.545278712161)) ;
#193263 = CARTESIAN_POINT('Ctrl Pts',(-17.9425421210597,-14.3827067354943,
116.614809758227)) ;
#193264 = CARTESIAN_POINT('Ctrl Pts',(-17.9635089553104,-14.3303836683813,
116.678671009225)) ;
#193265 = CARTESIAN_POINT('Ctrl Pts',(-17.9677674696046,-14.3197564784796,
116.691641686961)) ;
#193266 = CARTESIAN_POINT('Ctrl Pts',(-17.9719492216382,-14.3088124559315,
116.70437855954)) ;
#193267 = CARTESIAN_POINT('Ctrl Pts',(-17.9760500025897,-14.2975606758145,
116.716868876659)) ;
#193268 = CARTESIAN_POINT('Ctrl Pts',(-17.9948816875145,-14.2458900353894,
116.774227150459)) ;
#193269 = CARTESIAN_POINT('Ctrl Pts',(-18.0120038023616,-14.1877300152514,
116.826380183859)) ;
#193270 = CARTESIAN_POINT('Ctrl Pts',(-18.0269924392848,-14.1246319652718,
116.872032027455)) ;
#193271 = CARTESIAN_POINT('Ctrl Pts',(-18.0313506096886,-14.1062852633422,
116.885305983896)) ;
#193272 = CARTESIAN_POINT('Ctrl Pts',(-18.0355284323829,-14.0875212502638,
116.898030577)) ;
#193273 = CARTESIAN_POINT('Ctrl Pts',(-18.0395155550469,-14.0683784694332,
116.910174709315)) ;
#193274 = CARTESIAN_POINT('Ctrl Pts',(-18.052265981228,-14.0071617388601,
116.949010450189)) ;
#193275 = CARTESIAN_POINT('Ctrl Pts',(-18.0630631813206,-13.9420796939719,
116.981902915811)) ;
#193276 = CARTESIAN_POINT('Ctrl Pts',(-18.0717325065314,-13.8743660366255,
117.008305304809)) ;
#193277 = CARTESIAN_POINT('Ctrl Pts',(-18.0751147082918,-13.8479486113349,
117.018605784301)) ;
#193278 = CARTESIAN_POINT('Ctrl Pts',(-18.0781729329666,-13.8211309228485,
117.027918845113)) ;
#193279 = CARTESIAN_POINT('Ctrl Pts',(-18.0808963466438,-13.7939873904681,
117.036213923753)) ;
#193280 = CARTESIAN_POINT('Ctrl Pts',(-18.0833540191079,-13.7694924293578,
117.043699597535)) ;
#193281 = CARTESIAN_POINT('Ctrl Pts',(-18.0855717988214,-13.7443945944633,
117.050454735962)) ;
#193282 = CARTESIAN_POINT('Ctrl Pts',(-18.0875136590947,-13.7189305603966,
117.056369343325)) ;
#193283 = CARTESIAN_POINT('Ctrl Pts',(-18.0894566273483,-13.6934519971449,
117.062287325424)) ;
#193284 = CARTESIAN_POINT('Ctrl Pts',(-18.0911232849302,-13.667607492928,
117.067363606227)) ;
#193285 = CARTESIAN_POINT('Ctrl Pts',(-18.0924927843825,-13.641651804631,
117.071534784123)) ;
#193286 = CARTESIAN_POINT('Ctrl Pts',(-18.0938629088252,-13.6156842710903,
117.075707865594)) ;
#193287 = CARTESIAN_POINT('Ctrl Pts',(-18.0949355652063,-13.5896061785709,
117.078974927764)) ;
#193288 = CARTESIAN_POINT('Ctrl Pts',(-18.0957059946265,-13.5636797249849,
117.081321564011)) ;
#193289 = CARTESIAN_POINT('Ctrl Pts',(-18.0963885652904,-13.5407098900162,
117.083400592951)) ;
#193290 = CARTESIAN_POINT('Ctrl Pts',(-18.0968341419202,-13.5178594986715,
117.084757876611)) ;
#193291 = CARTESIAN_POINT('Ctrl Pts',(-18.0970501559553,-13.4953086850252,
117.085415820508)) ;
#193292 = CARTESIAN_POINT('Ctrl Pts',(-18.0972343972258,-13.4760747933397,
117.085976989691)) ;
#193293 = CARTESIAN_POINT('Ctrl Pts',(-18.0972584721256,-13.4562541583979,
117.086051100861)) ;
#193294 = CARTESIAN_POINT('Ctrl Pts',(-18.0970972387754,-13.4361251533928,
117.085560320937)) ;
#193295 = CARTESIAN_POINT('Ctrl Pts',(-18.096936270928,-13.4160292948047,
117.08507034918)) ;
#193296 = CARTESIAN_POINT('Ctrl Pts',(-18.0965905110925,-13.3956265064346,
117.084017108433)) ;
#193297 = CARTESIAN_POINT('Ctrl Pts',(-18.0960511480064,-13.3751969407049,
117.082373828394)) ;
#193298 = CARTESIAN_POINT('Ctrl Pts',(-18.0955200215003,-13.3550793535937,
117.080755642782)) ;
#193299 = CARTESIAN_POINT('Ctrl Pts',(-18.0948011763854,-13.3349362383173,
117.078565410166)) ;
#193300 = CARTESIAN_POINT('Ctrl Pts',(-18.0939024233134,-13.315031695618,
117.075827468671)) ;
#193301 = CARTESIAN_POINT('Ctrl Pts',(-18.0929827637773,-13.2946641407518,
117.073025838185)) ;
#193302 = CARTESIAN_POINT('Ctrl Pts',(-18.0918747072663,-13.2745468745331,
117.069650725061)) ;
#193303 = CARTESIAN_POINT('Ctrl Pts',(-18.0906039399014,-13.2549521381173,
117.065780494704)) ;
#193304 = CARTESIAN_POINT('Ctrl Pts',(-18.0893331725365,-13.2353574017014,
117.061910264347)) ;
#193305 = CARTESIAN_POINT('Ctrl Pts',(-18.0878998109875,-13.2162855561395,
117.057545346139)) ;
#193306 = CARTESIAN_POINT('Ctrl Pts',(-18.0863458477046,-13.1979917937502,
117.05281222471)) ;
#193307 = CARTESIAN_POINT('Ctrl Pts',(-18.0852303988916,-13.1848603666647,
117.049414747603)) ;
#193308 = CARTESIAN_POINT('Ctrl Pts',(-18.0839869321607,-13.1713626479556,
117.045627555924)) ;
#193309 = CARTESIAN_POINT('Ctrl Pts',(-18.0826311641542,-13.1578519278585,
117.041498054669)) ;
#193310 = CARTESIAN_POINT('Ctrl Pts',(-18.0812653772353,-13.1442413656633,
117.037338037049)) ;
#193311 = CARTESIAN_POINT('Ctrl Pts',(-18.0797855761015,-13.1306181206681,
117.032830587708)) ;
#193312 = CARTESIAN_POINT('Ctrl Pts',(-18.0782238294761,-13.1173287413436,
117.028073704578)) ;
#193313 = CARTESIAN_POINT('Ctrl Pts',(-18.0766620828508,-13.1040393620192,
117.023316821449)) ;
#193314 = CARTESIAN_POINT('Ctrl Pts',(-18.0750184927648,-13.0910842149795,
117.018310929226)) ;
#193315 = CARTESIAN_POINT('Ctrl Pts',(-18.0733406173676,-13.078788559479,
117.01320039149)) ;
#193316 = CARTESIAN_POINT('Ctrl Pts',(-18.0721098671841,-13.0697694867344,
117.009451725012)) ;
#193317 = CARTESIAN_POINT('Ctrl Pts',(-18.0707717001157,-13.0604578336815,
117.005375967919)) ;
#193318 = CARTESIAN_POINT('Ctrl Pts',(-18.0693721051686,-13.0513039505984,
117.001112954701)) ;
#193319 = CARTESIAN_POINT('Ctrl Pts',(-18.067964052392,-13.0420947500949,
116.99682417986)) ;
#193320 = CARTESIAN_POINT('Ctrl Pts',(-18.0664938193825,-13.033045638422,
116.99234609624)) ;
#193321 = CARTESIAN_POINT('Ctrl Pts',(-18.0650230520561,-13.0245905007115,
116.987866421264)) ;
#193322 = CARTESIAN_POINT('Ctrl Pts',(-18.0648621543254,-13.0236655328759,
116.987376357659)) ;
#193323 = CARTESIAN_POINT('Ctrl Pts',(-18.0647012643362,-13.0227476464585,
116.986886316111)) ;
#193324 = CARTESIAN_POINT('Ctrl Pts',(-18.0645404729608,-13.0218373893616,
116.986396571525)) ;
#193325 = CARTESIAN_POINT('Ctrl Pts',(-18.0634316111312,-13.0155600044732,
116.983019157306)) ;
#193326 = CARTESIAN_POINT('Ctrl Pts',(-18.0622287233154,-13.0090948676773,
116.979355343084)) ;
#193327 = CARTESIAN_POINT('Ctrl Pts',(-18.0610103124457,-13.0030224151989,
116.975644247746)) ;
#193328 = CARTESIAN_POINT('Ctrl Pts',(-18.0604262701594,-13.0001115998758,
116.973865343224)) ;
#193329 = CARTESIAN_POINT('Ctrl Pts',(-18.0598388640937,-12.9972905938871,
116.972076229518)) ;
#193330 = CARTESIAN_POINT('Ctrl Pts',(-18.059257840653,-12.9946208870877,
116.970306525865)) ;
#193331 = CARTESIAN_POINT('Ctrl Pts',(-18.0582667075183,-12.9900667939414,
116.967287694256)) ;
#193332 = CARTESIAN_POINT('Ctrl Pts',(-18.0571961007361,-12.9855090222264,
116.964026798739)) ;
#193333 = CARTESIAN_POINT('Ctrl Pts',(-18.0561685336678,-12.9817420257543,
116.960896995246)) ;
#193334 = CARTESIAN_POINT('Ctrl Pts',(-18.0555646065479,-12.9795280667821,
116.959057530682)) ;
#193335 = CARTESIAN_POINT('Ctrl Pts',(-18.0549412511537,-12.977460262646,
116.957158890829)) ;
#193336 = CARTESIAN_POINT('Ctrl Pts',(-18.0543480872734,-12.9758473023832,
116.955352209356)) ;
#193337 = CARTESIAN_POINT('Ctrl Pts',(-18.0534287572029,-12.9733474150479,
116.952552078295)) ;
#193338 = CARTESIAN_POINT('Ctrl Pts',(-18.0525577104548,-12.9718729041419,
116.949899010344)) ;
#193339 = CARTESIAN_POINT('Ctrl Pts',(-18.0519478151656,-12.9727494438644,
116.948041367699)) ;
#193340 = CARTESIAN_POINT('',(-29.1489187358159,-13.1500241806476,113.370642219953)) ;
#193341 = CARTESIAN_POINT('Ctrl Pts',(-29.1489187358159,-13.1500241806476,
113.370642219953)) ;
#193342 = CARTESIAN_POINT('Ctrl Pts',(-29.1481908350552,-13.1438552129684,
113.369207785981)) ;
#193343 = CARTESIAN_POINT('Ctrl Pts',(-29.1363218176444,-13.045472096163,
113.345565010115)) ;
#193344 = CARTESIAN_POINT('Ctrl Pts',(-29.1042713188461,-12.8597742993635,
113.272543581875)) ;
#193345 = CARTESIAN_POINT('Ctrl Pts',(-29.0373324850924,-12.6327839415056,
113.104016096402)) ;
#193346 = CARTESIAN_POINT('Ctrl Pts',(-28.9535211541043,-12.4610780963096,
112.884187309328)) ;
#193347 = CARTESIAN_POINT('Ctrl Pts',(-28.8575946335874,-12.3578311300529,
112.627637093626)) ;
#193348 = CARTESIAN_POINT('Ctrl Pts',(-28.7572250300145,-12.3309709098726,
112.357185420699)) ;
#193349 = CARTESIAN_POINT('Ctrl Pts',(-28.6569634591251,-12.3817310335918,
112.087380599263)) ;
#193350 = CARTESIAN_POINT('Ctrl Pts',(-28.564509082064,-12.5067458714326,
111.841211648264)) ;
#193351 = CARTESIAN_POINT('Ctrl Pts',(-28.4851946394043,-12.6971218835384,
111.635119922408)) ;
#193352 = CARTESIAN_POINT('Ctrl Pts',(-28.4241475022264,-12.9391053860727,
111.48464558118)) ;
#193353 = CARTESIAN_POINT('Ctrl Pts',(-28.3849524033199,-13.2152764852227,
111.400718831589)) ;
#193354 = CARTESIAN_POINT('Ctrl Pts',(-28.3695728344553,-13.505784356226,
111.389304759768)) ;
#193355 = CARTESIAN_POINT('Ctrl Pts',(-28.3785666018913,-13.7916119971123,
111.452340850324)) ;
#193356 = CARTESIAN_POINT('Ctrl Pts',(-28.4102051428863,-14.0480477215918,
111.583997783673)) ;
#193357 = CARTESIAN_POINT('Ctrl Pts',(-28.4617096973959,-14.2608003622883,
111.776342484654)) ;
#193358 = CARTESIAN_POINT('Ctrl Pts',(-28.5285966908039,-14.4130997833176,
112.015523906653)) ;
#193359 = CARTESIAN_POINT('Ctrl Pts',(-28.6055369658778,-14.494276858583,
112.285430331193)) ;
#193360 = CARTESIAN_POINT('Ctrl Pts',(-28.6858402113565,-14.4979516536895,
112.565480733191)) ;
#193361 = CARTESIAN_POINT('Ctrl Pts',(-28.7630866534358,-14.4245500702158,
112.836167498554)) ;
#193362 = CARTESIAN_POINT('Ctrl Pts',(-28.8312032669878,-14.27912481409,113.079082108179)) ;
#193363 = CARTESIAN_POINT('Ctrl Pts',(-28.8845697171654,-14.0717728276009,
113.277121444909)) ;
#193364 = CARTESIAN_POINT('Ctrl Pts',(-28.9184685925918,-13.8168218187551,
113.415944332688)) ;
#193365 = CARTESIAN_POINT('Ctrl Pts',(-28.9296288975394,-13.535324035321,
113.485246560678)) ;
#193366 = CARTESIAN_POINT('Ctrl Pts',(-28.9167824586136,-13.2440746292406,
113.481603030049)) ;
#193367 = CARTESIAN_POINT('Ctrl Pts',(-28.879724619622,-12.9648031401168,
113.404286512872)) ;
#193368 = CARTESIAN_POINT('Ctrl Pts',(-28.8209010350444,-12.7194345507308,
113.260464724787)) ;
#193369 = CARTESIAN_POINT('Ctrl Pts',(-28.7430943016509,-12.5228537207888,
113.059023280909)) ;
#193370 = CARTESIAN_POINT('Ctrl Pts',(-28.6517657151193,-12.3910219564108,
112.816257416584)) ;
#193371 = CARTESIAN_POINT('Ctrl Pts',(-28.5519605561705,-12.3324946198483,
112.547844627311)) ;
#193372 = CARTESIAN_POINT('Ctrl Pts',(-28.4511785871551,-12.3517941049946,
112.2762149844)) ;
#193373 = CARTESIAN_POINT('Ctrl Pts',(-28.3546167960162,-12.4476532719571,
112.01766426386)) ;
#193374 = CARTESIAN_POINT('Ctrl Pts',(-28.2694260224947,-12.6128436094032,
111.793615869469)) ;
#193375 = CARTESIAN_POINT('Ctrl Pts',(-28.2004725461681,-12.8354722898284,
111.619033756946)) ;
#193376 = CARTESIAN_POINT('Ctrl Pts',(-28.1518872197862,-13.101408894203,
111.506681708968)) ;
#193377 = CARTESIAN_POINT('Ctrl Pts',(-28.1269130732857,-13.3874022195482,
111.465903939157)) ;
#193378 = CARTESIAN_POINT('Ctrl Pts',(-28.1259581954368,-13.6768759171903,
111.498450514514)) ;
#193379 = CARTESIAN_POINT('Ctrl Pts',(-28.1487784107379,-13.948608493865,
111.603521104352)) ;
#193380 = CARTESIAN_POINT('Ctrl Pts',(-28.1927422454497,-14.181257681225,
111.772854625694)) ;
#193381 = CARTESIAN_POINT('Ctrl Pts',(-28.25389994631,-14.3592650506284,111.994525378914)) ;
#193382 = CARTESIAN_POINT('Ctrl Pts',(-28.3273391635443,-14.4703402370834,
112.253666401676)) ;
#193383 = CARTESIAN_POINT('Ctrl Pts',(-28.4071790901361,-14.5059089260168,
112.532398419472)) ;
#193384 = CARTESIAN_POINT('Ctrl Pts',(-28.4863373455099,-14.4635906108697,
112.808879001028)) ;
#193385 = CARTESIAN_POINT('Ctrl Pts',(-28.5590864820887,-14.3462861335646,
113.06597539471)) ;
#193386 = CARTESIAN_POINT('Ctrl Pts',(-28.6190888482877,-14.1620807273187,
113.284252795165)) ;
#193387 = CARTESIAN_POINT('Ctrl Pts',(-28.6611716634273,-13.9257450561724,
113.447780698845)) ;
#193388 = CARTESIAN_POINT('Ctrl Pts',(-28.6819629618819,-13.6518932520307,
113.54663327576)) ;
#193389 = CARTESIAN_POINT('Ctrl Pts',(-28.6788957975661,-13.361350209501,
113.572794442411)) ;
#193390 = CARTESIAN_POINT('Ctrl Pts',(-28.6515753370969,-13.0754523993138,
113.525017916636)) ;
#193391 = CARTESIAN_POINT('Ctrl Pts',(-28.6012644802897,-12.8139381990977,
113.407216883436)) ;
#193392 = CARTESIAN_POINT('Ctrl Pts',(-28.530312795938,-12.5948180944483,
113.22672545771)) ;
#193393 = CARTESIAN_POINT('Ctrl Pts',(-28.4441820785393,-12.4362800048722,
112.999678378)) ;
#193394 = CARTESIAN_POINT('Ctrl Pts',(-28.3470854955192,-12.346922078608,
112.739452029468)) ;
#193395 = CARTESIAN_POINT('Ctrl Pts',(-28.2458303935604,-12.3346186385411,
112.466505819017)) ;
#193396 = CARTESIAN_POINT('Ctrl Pts',(-28.1468306373285,-12.3998225687949,
112.200422951598)) ;
#193397 = CARTESIAN_POINT('Ctrl Pts',(-28.056410402061,-12.5378477500096,
111.960460656517)) ;
#193398 = CARTESIAN_POINT('Ctrl Pts',(-27.9801392408926,-12.7392396507352,
111.763656314593)) ;
#193399 = CARTESIAN_POINT('Ctrl Pts',(-27.9229728782281,-12.989236405783,
111.625017894805)) ;
#193400 = CARTESIAN_POINT('Ctrl Pts',(-27.8882165238537,-13.269049028932,
111.554529970124)) ;
#193401 = CARTESIAN_POINT('Ctrl Pts',(-27.8773822820719,-13.560604521515,
111.557039247534)) ;
#193402 = CARTESIAN_POINT('Ctrl Pts',(-27.8908274487406,-13.8423158077137,
111.633558215579)) ;
#193403 = CARTESIAN_POINT('Ctrl Pts',(-27.9264541508921,-14.0920492190499,
111.777413603601)) ;
#193404 = CARTESIAN_POINT('Ctrl Pts',(-27.9814414275838,-14.2950965364046,
111.980481540082)) ;
#193405 = CARTESIAN_POINT('Ctrl Pts',(-28.0507461501417,-14.434335219557,
112.227053017501)) ;
#193406 = CARTESIAN_POINT('Ctrl Pts',(-28.1282740613558,-14.5007530721094,
112.498487082343)) ;
#193407 = CARTESIAN_POINT('Ctrl Pts',(-28.2086863670135,-14.4901437351793,
112.778942561062)) ;
#193408 = CARTESIAN_POINT('Ctrl Pts',(-28.2850462508329,-14.402041943339,
113.047107750682)) ;
#193409 = CARTESIAN_POINT('Ctrl Pts',(-28.3507008692899,-14.243691286176,
113.282525581938)) ;
#193410 = CARTESIAN_POINT('Ctrl Pts',(-28.4004336980104,-14.0272168477211,
113.469327044574)) ;
#193411 = CARTESIAN_POINT('Ctrl Pts',(-28.4302808069805,-13.7664028194368,
113.595698173527)) ;
#193412 = CARTESIAN_POINT('Ctrl Pts',(-28.4370991249928,-13.4798811075686,
113.652008520853)) ;
#193413 = CARTESIAN_POINT('Ctrl Pts',(-28.4194035357479,-13.1885796838075,
113.633702115265)) ;
#193414 = CARTESIAN_POINT('Ctrl Pts',(-28.378412477973,-12.9166253502417,
113.544054690634)) ;
#193415 = CARTESIAN_POINT('Ctrl Pts',(-28.3154270405176,-12.6775835687805,
113.387804302381)) ;
#193416 = CARTESIAN_POINT('Ctrl Pts',(-28.2345655221718,-12.4925681740676,
113.177035535843)) ;
#193417 = CARTESIAN_POINT('Ctrl Pts',(-28.1415965309447,-12.3743553948694,
112.929153696932)) ;
#193418 = CARTESIAN_POINT('Ctrl Pts',(-28.0408341461004,-12.3300586716913,
112.657878333238)) ;
#193419 = CARTESIAN_POINT('Ctrl Pts',(-27.9401092157344,-12.3643855283945,
112.386554127362)) ;
#193420 = CARTESIAN_POINT('Ctrl Pts',(-27.8457507930179,-12.4735026256636,
112.134502190906)) ;
#193421 = CARTESIAN_POINT('Ctrl Pts',(-27.7630645931825,-12.6505044221707,
111.918129912256)) ;
#193422 = CARTESIAN_POINT('Ctrl Pts',(-27.6975343400792,-12.883421947767,
111.754113424243)) ;
#193423 = CARTESIAN_POINT('Ctrl Pts',(-27.6534936872668,-13.1527514798463,
111.655293821054)) ;
#193424 = CARTESIAN_POINT('Ctrl Pts',(-27.6327547212792,-13.4437023579035,
111.627785242889)) ;
#193425 = CARTESIAN_POINT('Ctrl Pts',(-27.6365620199519,-13.7306193771303,
111.674768692016)) ;
#193426 = CARTESIAN_POINT('Ctrl Pts',(-27.6633603539813,-13.9949086675026,
111.791717285722)) ;
#193427 = CARTESIAN_POINT('Ctrl Pts',(-27.7111136241826,-14.2196906214034,
111.972774236008)) ;
#193428 = CARTESIAN_POINT('Ctrl Pts',(-27.7749357041157,-14.3856064052365,
112.20251553552)) ;
#193429 = CARTESIAN_POINT('Ctrl Pts',(-27.850139433854,-14.4829720573525,
112.467091440401)) ;
#193430 = CARTESIAN_POINT('Ctrl Pts',(-27.9301015626753,-14.5039687036518,
112.746047500903)) ;
#193431 = CARTESIAN_POINT('Ctrl Pts',(-28.0091089868232,-14.4466173797893,
113.02236063873)) ;
#193432 = CARTESIAN_POINT('Ctrl Pts',(-28.0794461167512,-14.3162716014842,
113.27191318261)) ;
#193433 = CARTESIAN_POINT('Ctrl Pts',(-28.1364440614567,-14.1214968775469,
113.480983026046)) ;
#193434 = CARTESIAN_POINT('Ctrl Pts',(-28.1749613485906,-13.8749956323593,
113.633913814206)) ;
#193435 = CARTESIAN_POINT('Ctrl Pts',(-28.1911734256759,-13.5974682752699,
113.718666176969)) ;
#193436 = CARTESIAN_POINT('Ctrl Pts',(-28.1836078259768,-13.3070931499256,
113.731008103206)) ;
#193437 = CARTESIAN_POINT('Ctrl Pts',(-28.1517250328214,-13.0233508116479,
113.669448037719)) ;
#193438 = CARTESIAN_POINT('Ctrl Pts',(-28.0972991812598,-12.7688607554056,
113.539098836946)) ;
#193439 = CARTESIAN_POINT('Ctrl Pts',(-28.0232821783549,-12.5604071436069,
113.349142464811)) ;
#193440 = CARTESIAN_POINT('Ctrl Pts',(-27.9344209561679,-12.4137261008746,
113.113916473714)) ;
#193441 = CARTESIAN_POINT('Ctrl Pts',(-27.8363120109697,-12.3387040702925,
112.850499990527)) ;
#193442 = CARTESIAN_POINT('Ctrl Pts',(-27.7346441044334,-12.3410592400664,
112.576417227786)) ;
#193443 = CARTESIAN_POINT('Ctrl Pts',(-27.6369370950116,-12.4205041979803,
112.314216816515)) ;
#193444 = CARTESIAN_POINT('Ctrl Pts',(-27.5486712808213,-12.5715202421064,
112.080868685751)) ;
#193445 = CARTESIAN_POINT('Ctrl Pts',(-27.4757703775428,-12.7831706996134,
111.894290358998)) ;
#193446 = CARTESIAN_POINT('Ctrl Pts',(-27.4226294303003,-13.0400861903177,
111.76787608117)) ;
#193447 = CARTESIAN_POINT('Ctrl Pts',(-27.3922395133834,-13.3242719779506,
111.710785133111)) ;
#193448 = CARTESIAN_POINT('Ctrl Pts',(-27.3860860135596,-13.6152878377403,
111.727526925979)) ;
#193449 = CARTESIAN_POINT('Ctrl Pts',(-27.4038644204004,-13.8920338673762,
111.817147898947)) ;
#193450 = CARTESIAN_POINT('Ctrl Pts',(-27.4434672264958,-14.1346381572922,
111.973208058208)) ;
#193451 = CARTESIAN_POINT('Ctrl Pts',(-27.5014596989945,-14.3262307223465,
112.185343141529)) ;
#193452 = CARTESIAN_POINT('Ctrl Pts',(-27.572610257217,-14.4523301137118,
112.437438559264)) ;
#193453 = CARTESIAN_POINT('Ctrl Pts',(-27.6514424913783,-14.5048566464616,
112.713014331691)) ;
#193454 = CARTESIAN_POINT('Ctrl Pts',(-27.7316184422369,-14.4792282215674,
112.992772623)) ;
#193455 = CARTESIAN_POINT('Ctrl Pts',(-27.8061587870981,-14.3776591931245,
113.255243325012)) ;
#193456 = CARTESIAN_POINT('Ctrl Pts',(-27.8693284879629,-14.2073582471136,
113.483114722588)) ;
#193457 = CARTESIAN_POINT('Ctrl Pts',(-27.9157562377959,-13.980463190757,
113.659992780597)) ;
#193458 = CARTESIAN_POINT('Ctrl Pts',(-27.9413702245525,-13.7134648384933,
113.773453223393)) ;
#193459 = CARTESIAN_POINT('Ctrl Pts',(-27.9436004920684,-13.4252028157263,
113.815706568897)) ;
#193460 = CARTESIAN_POINT('Ctrl Pts',(-27.9215804554763,-13.136660084581,
113.78406473884)) ;
#193461 = CARTESIAN_POINT('Ctrl Pts',(-27.8759261543426,-12.8674128564449,
113.680553643697)) ;
#193462 = CARTESIAN_POINT('Ctrl Pts',(-27.8094158631442,-12.6383938778605,
113.513414911382)) ;
#193463 = CARTESIAN_POINT('Ctrl Pts',(-27.7259260844217,-12.465038874388,
113.294584641188)) ;
#193464 = CARTESIAN_POINT('Ctrl Pts',(-27.630761291581,-12.3599344396702,
113.040172878809)) ;
#193465 = CARTESIAN_POINT('Ctrl Pts',(-27.5296719419162,-12.3306429195518,
112.767809456319)) ;
#193466 = CARTESIAN_POINT('Ctrl Pts',(-27.4298006531373,-12.3792038030185,
112.499012174243)) ;
#193467 = CARTESIAN_POINT('Ctrl Pts',(-27.3368869719151,-12.502250920438,
112.251503904024)) ;
#193468 = CARTESIAN_POINT('Ctrl Pts',(-27.2572469138254,-12.690704289041,
112.044366413114)) ;
#193469 = CARTESIAN_POINT('Ctrl Pts',(-27.1956046752294,-12.9312491813812,
111.892066772438)) ;
#193470 = CARTESIAN_POINT('Ctrl Pts',(-27.1556968251946,-13.2069304836541,
111.805999837402)) ;
#193471 = CARTESIAN_POINT('Ctrl Pts',(-27.1396183503164,-13.4971323588194,
111.792434998313)) ;
#193472 = CARTESIAN_POINT('Ctrl Pts',(-27.1478926952953,-13.7832858649534,
111.853261517309)) ;
#193473 = CARTESIAN_POINT('Ctrl Pts',(-27.1788426100833,-14.0408293277911,
111.98281261947)) ;
#193474 = CARTESIAN_POINT('Ctrl Pts',(-27.2300778195774,-14.255952322556,
112.174490901595)) ;
#193475 = CARTESIAN_POINT('Ctrl Pts',(-27.2963594840731,-14.4094466686143,
112.411688111103)) ;
#193476 = CARTESIAN_POINT('Ctrl Pts',(-27.3730829374615,-14.4929694646286,
112.680938243989)) ;
#193477 = CARTESIAN_POINT('Ctrl Pts',(-27.4533942328739,-14.4990155260453,
112.961017342185)) ;
#193478 = CARTESIAN_POINT('Ctrl Pts',(-27.5309746225123,-14.4275804860338,
113.232800584045)) ;
#193479 = CARTESIAN_POINT('Ctrl Pts',(-27.5993744489561,-14.284309082368,
113.476532018314)) ;
#193480 = CARTESIAN_POINT('Ctrl Pts',(-27.6533609863589,-14.0775350374868,
113.67660042095)) ;
#193481 = CARTESIAN_POINT('Ctrl Pts',(-27.6875986228682,-13.8261134335288,
113.816121058213)) ;
#193482 = CARTESIAN_POINT('Ctrl Pts',(-27.6996267717849,-13.5428648342343,
113.888368399397)) ;
#193483 = CARTESIAN_POINT('Ctrl Pts',(-27.6873576347831,-13.252182353688,
113.886407116913)) ;
#193484 = CARTESIAN_POINT('Ctrl Pts',(-27.651195526548,-12.9730234465435,
113.811707238471)) ;
#193485 = CARTESIAN_POINT('Ctrl Pts',(-27.5924502457676,-12.724731390434,
113.668397807756)) ;
#193486 = CARTESIAN_POINT('Ctrl Pts',(-27.5156633000477,-12.5280561031159,
113.469790960335)) ;
#193487 = CARTESIAN_POINT('Ctrl Pts',(-27.4242158235811,-12.3935893009494,
113.226845172422)) ;
#193488 = CARTESIAN_POINT('Ctrl Pts',(-27.3251142958241,-12.333081965445,
112.960365809793)) ;
#193489 = CARTESIAN_POINT('Ctrl Pts',(-27.2233916702717,-12.3505128306963,
112.686197908057)) ;
#193490 = CARTESIAN_POINT('Ctrl Pts',(-27.12763956026,-12.4433828921911,112.429728050708)) ;
#193491 = CARTESIAN_POINT('Ctrl Pts',(-27.0415094033996,-12.607349424796,
112.20302769542)) ;
#193492 = CARTESIAN_POINT('Ctrl Pts',(-26.9722746864344,-12.8279036385121,
112.027468698458)) ;
#193493 = CARTESIAN_POINT('Ctrl Pts',(-26.9229312024064,-13.0930059035689,
111.912843276643)) ;
#193494 = CARTESIAN_POINT('Ctrl Pts',(-26.8972324155193,-13.3789266137586,
111.86989142793)) ;
#193495 = CARTESIAN_POINT('Ctrl Pts',(-26.89559593885,-13.6686885717782,111.900373113643)) ;
#193496 = CARTESIAN_POINT('Ctrl Pts',(-26.9176753989106,-13.9407698971193,
112.00311647252)) ;
#193497 = CARTESIAN_POINT('Ctrl Pts',(-26.9611957529866,-14.1754452261927,
112.171205228785)) ;
#193498 = CARTESIAN_POINT('Ctrl Pts',(-27.0218558744677,-14.3550939223612,
112.391319568465)) ;
#193499 = CARTESIAN_POINT('Ctrl Pts',(-27.0954919754477,-14.468598908444,
112.65127280273)) ;
#193500 = CARTESIAN_POINT('Ctrl Pts',(-27.1747095469528,-14.5058659881171,
112.927861658512)) ;
#193501 = CARTESIAN_POINT('Ctrl Pts',(-27.2540706728051,-14.465907705861,
113.205009023131)) ;
#193502 = CARTESIAN_POINT('Ctrl Pts',(-27.3270117595021,-14.3507454275659,
113.462647263951)) ;
#193503 = CARTESIAN_POINT('Ctrl Pts',(-27.3874657468428,-14.1684902162708,
113.682288696207)) ;
#193504 = CARTESIAN_POINT('Ctrl Pts',(-27.4302106667087,-13.9330107336615,
113.847901657391)) ;
#193505 = CARTESIAN_POINT('Ctrl Pts',(-27.4515998140738,-13.6600763512271,
113.948553659072)) ;
#193506 = CARTESIAN_POINT('Ctrl Pts',(-27.4493246185078,-13.3704757504778,
113.977035138527)) ;
#193507 = CARTESIAN_POINT('Ctrl Pts',(-27.4224958680665,-13.0823700026988,
113.93098284499)) ;
#193508 = CARTESIAN_POINT('Ctrl Pts',(-27.3729809937545,-12.8213180178566,
113.815427357995)) ;
#193509 = CARTESIAN_POINT('Ctrl Pts',(-27.3028037991072,-12.6009816910039,
113.637217641596)) ;
#193510 = CARTESIAN_POINT('Ctrl Pts',(-27.2168540748088,-12.4399155910324,
113.410819058086)) ;
#193511 = CARTESIAN_POINT('Ctrl Pts',(-27.1197079246416,-12.3483508718252,
113.15053363995)) ;
#193512 = CARTESIAN_POINT('Ctrl Pts',(-27.0187802117475,-12.3338872424077,
112.878480782108)) ;
#193513 = CARTESIAN_POINT('Ctrl Pts',(-26.9193985159767,-12.396923495094,
112.611312558498)) ;
#193514 = CARTESIAN_POINT('Ctrl Pts',(-26.8285566748927,-12.5334553693914,
112.370120041222)) ;
#193515 = CARTESIAN_POINT('Ctrl Pts',(-26.7522001619182,-12.7322215761211,
112.172876186384)) ;
#193516 = CARTESIAN_POINT('Ctrl Pts',(-26.6943187231654,-12.9810049412899,
112.032078055127)) ;
#193517 = CARTESIAN_POINT('Ctrl Pts',(-26.6587912592978,-13.2609753303157,
111.959335470938)) ;
#193518 = CARTESIAN_POINT('Ctrl Pts',(-26.647319062969,-13.5522070361543,
111.959866894059)) ;
#193519 = CARTESIAN_POINT('Ctrl Pts',(-26.6599556627793,-13.8335794690488,
112.033796091262)) ;
#193520 = CARTESIAN_POINT('Ctrl Pts',(-26.6950792057711,-14.0854850074698,
112.176258032588)) ;
#193521 = CARTESIAN_POINT('Ctrl Pts',(-26.7493678080384,-14.2893882283517,
112.377063192394)) ;
#193522 = CARTESIAN_POINT('Ctrl Pts',(-26.8182694831193,-14.4310416708449,
112.622412303935)) ;
#193523 = CARTESIAN_POINT('Ctrl Pts',(-26.8960209759952,-14.4999960091202,
112.894701404491)) ;
#193524 = CARTESIAN_POINT('Ctrl Pts',(-26.9762322526902,-14.4914668725251,
113.174447910469)) ;
#193525 = CARTESIAN_POINT('Ctrl Pts',(-27.0525399232105,-14.4062237339893,
113.44231798111)) ;
#193526 = CARTESIAN_POINT('Ctrl Pts',(-27.1188648773087,-14.2495321967945,
113.679899921954)) ;
#193527 = CARTESIAN_POINT('Ctrl Pts',(-27.1692281183874,-14.0340281298451,
113.868701151054)) ;
#193528 = CARTESIAN_POINT('Ctrl Pts',(-27.1996623984703,-13.7742259092907,
113.99685412237)) ;
#193529 = CARTESIAN_POINT('Ctrl Pts',(-27.2071696580136,-13.488993839479,
114.055160255525)) ;
#193530 = CARTESIAN_POINT('Ctrl Pts',(-27.1902825049831,-13.1975717487405,
114.039308325117)) ;
#193531 = CARTESIAN_POINT('Ctrl Pts',(-27.1498141482332,-12.9237175982201,
113.951393026303)) ;
#193532 = CARTESIAN_POINT('Ctrl Pts',(-27.0872605509044,-12.6833926232874,
113.796490915852)) ;
#193533 = CARTESIAN_POINT('Ctrl Pts',(-27.0073325603644,-12.4975233316372,
113.588365552072)) ;
#193534 = CARTESIAN_POINT('Ctrl Pts',(-26.9141377906141,-12.3765652756753,
113.339997758843)) ;
#193535 = CARTESIAN_POINT('Ctrl Pts',(-26.8140599847601,-12.3303669115662,
113.070599618917)) ;
#193536 = CARTESIAN_POINT('Ctrl Pts',(-26.7130188584353,-12.3620831181533,
112.798392930309)) ;
#193537 = CARTESIAN_POINT('Ctrl Pts',(-26.6179903821788,-12.4697592102098,
112.544455169899)) ;
#193538 = CARTESIAN_POINT('Ctrl Pts',(-26.5351639179177,-12.6447797711106,
112.32756700901)) ;
#193539 = CARTESIAN_POINT('Ctrl Pts',(-26.4692769172657,-12.8750273852739,
112.162297586987)) ;
#193540 = CARTESIAN_POINT('Ctrl Pts',(-26.4243077785298,-13.1453257818208,
112.060890975421)) ;
#193541 = CARTESIAN_POINT('Ctrl Pts',(-26.403013785645,-13.4336234546741,
112.031393920208)) ;
#193542 = CARTESIAN_POINT('Ctrl Pts',(-26.4060165852795,-13.7229316022969,
112.076174503052)) ;
#193543 = CARTESIAN_POINT('Ctrl Pts',(-26.4323125416507,-13.9881204584926,
112.191610815065)) ;
#193544 = CARTESIAN_POINT('Ctrl Pts',(-26.4792881537362,-14.2135626266573,
112.370156392619)) ;
#193545 = CARTESIAN_POINT('Ctrl Pts',(-26.5430286631922,-14.3820856851378,
112.599827193971)) ;
#193546 = CARTESIAN_POINT('Ctrl Pts',(-26.6176671822151,-14.4811007735871,
112.862516248575)) ;
#193547 = CARTESIAN_POINT('Ctrl Pts',(-26.6978612990312,-14.5043853087956,
113.142314338476)) ;
#193548 = CARTESIAN_POINT('Ctrl Pts',(-26.7765022627845,-14.4497319209782,
113.417276345146)) ;
#193549 = CARTESIAN_POINT('Ctrl Pts',(-26.8476800485963,-14.3208489038209,
113.669628788919)) ;
#193550 = CARTESIAN_POINT('Ctrl Pts',(-26.9051290746846,-14.1269083086763,
113.880141966721)) ;
#193551 = CARTESIAN_POINT('Ctrl Pts',(-26.9439250946234,-13.8839530008224,
114.033597139485)) ;
#193552 = CARTESIAN_POINT('Ctrl Pts',(-26.9610011688202,-13.6058131007772,
114.121164169516)) ;
#193553 = CARTESIAN_POINT('Ctrl Pts',(-26.9541142012214,-13.3154623494247,
114.135571911121)) ;
#193554 = CARTESIAN_POINT('Ctrl Pts',(-26.9227927789619,-13.0305252756843,
114.075814770893)) ;
#193555 = CARTESIAN_POINT('Ctrl Pts',(-26.8691774398986,-12.7760411077928,
113.947787130553)) ;
#193556 = CARTESIAN_POINT('Ctrl Pts',(-26.7957043233195,-12.5658693797106,
113.759493744326)) ;
#193557 = CARTESIAN_POINT('Ctrl Pts',(-26.7071990036801,-12.4170609140262,
113.52535902764)) ;
#193558 = CARTESIAN_POINT('Ctrl Pts',(-26.6088521342578,-12.3396249333132,
113.261367652909)) ;
#193559 = CARTESIAN_POINT('Ctrl Pts',(-26.5073352253782,-12.340046412335,
112.987690769148)) ;
#193560 = CARTESIAN_POINT('Ctrl Pts',(-26.4097025231263,-12.4170460254182,
112.725620310096)) ;
#193561 = CARTESIAN_POINT('Ctrl Pts',(-26.3209819060534,-12.5662136094611,
112.490921752616)) ;
#193562 = CARTESIAN_POINT('Ctrl Pts',(-26.2476333327786,-12.7760199991739,
112.30293791623)) ;
#193563 = CARTESIAN_POINT('Ctrl Pts',(-26.1937928662736,-13.0322696653641,
112.174451982578)) ;
#193564 = CARTESIAN_POINT('Ctrl Pts',(-26.1627547455184,-13.3151090323585,
112.115281050215)) ;
#193565 = CARTESIAN_POINT('Ctrl Pts',(-26.1558631196965,-13.6075492018493,
112.129940953347)) ;
#193566 = CARTESIAN_POINT('Ctrl Pts',(-26.1729300005076,-13.8839937911961,
112.217263774275)) ;
#193567 = CARTESIAN_POINT('Ctrl Pts',(-26.2120071941306,-14.1283418739825,
112.371799593747)) ;
#193568 = CARTESIAN_POINT('Ctrl Pts',(-26.2693072989749,-14.321085337762,
112.58170002845)) ;
#193569 = CARTESIAN_POINT('Ctrl Pts',(-26.3405926471782,-14.4501544762085,
112.834435287317)) ;
#193570 = CARTESIAN_POINT('Ctrl Pts',(-26.4193828840965,-14.504350239421,
113.109906480253)) ;
#193571 = CARTESIAN_POINT('Ctrl Pts',(-26.4990873137165,-14.4811635345991,
113.387994186648)) ;
#193572 = CARTESIAN_POINT('Ctrl Pts',(-26.5741035318335,-14.3816036851556,
113.652018746242)) ;
#193573 = CARTESIAN_POINT('Ctrl Pts',(-26.6376352371572,-14.2132115910195,
113.88096634118)) ;
#193574 = CARTESIAN_POINT('Ctrl Pts',(-26.6847308687247,-13.9871283531687,
114.059972839669)) ;
#193575 = CARTESIAN_POINT('Ctrl Pts',(-26.7108828323385,-13.7209751384546,
114.175063486759)) ;
#193576 = CARTESIAN_POINT('Ctrl Pts',(-26.7138425852466,-13.4341833204507,
114.21939759733)) ;
#193577 = CARTESIAN_POINT('Ctrl Pts',(-26.692396148443,-13.1440226446982,
114.18967350618)) ;
#193578 = CARTESIAN_POINT('Ctrl Pts',(-26.6475602009265,-12.8750223963181,
114.08850476367)) ;
#193579 = CARTESIAN_POINT('Ctrl Pts',(-26.5813161216274,-12.6437154561283,
113.922329063855)) ;
#193580 = CARTESIAN_POINT('Ctrl Pts',(-26.4986543480993,-12.4695015573388,
113.705836185377)) ;
#193581 = CARTESIAN_POINT('Ctrl Pts',(-26.40350334832,-12.3618253102505,113.451569423215)) ;
#193582 = CARTESIAN_POINT('Ctrl Pts',(-26.3025135279916,-12.3304086987919,
113.179494242336)) ;
#193583 = CARTESIAN_POINT('Ctrl Pts',(-26.2025781370336,-12.3767667157857,
112.910488649315)) ;
#193584 = CARTESIAN_POINT('Ctrl Pts',(-26.1095364919782,-12.4973266925111,
112.662514220771)) ;
#193585 = CARTESIAN_POINT('Ctrl Pts',(-26.0290482236216,-12.6849702880242,
112.452967860837)) ;
#193586 = CARTESIAN_POINT('Ctrl Pts',(-25.967020193737,-12.9239536141708,
112.299425204879)) ;
#193587 = CARTESIAN_POINT('Ctrl Pts',(-25.9264894675845,-13.198264514804,
112.211386234531)) ;
#193588 = CARTESIAN_POINT('Ctrl Pts',(-25.9096865137876,-13.4887696764051,
112.195672545383)) ;
#193589 = CARTESIAN_POINT('Ctrl Pts',(-25.9171975165263,-13.7747050880232,
112.254081199622)) ;
#193590 = CARTESIAN_POINT('Ctrl Pts',(-25.9477017056163,-14.0346989777519,
112.382474254739)) ;
#193591 = CARTESIAN_POINT('Ctrl Pts',(-25.9983172672415,-14.2504823475427,
112.572150154809)) ;
#193592 = CARTESIAN_POINT('Ctrl Pts',(-26.0642269575703,-14.4061007577842,
112.808231529626)) ;
#193593 = CARTESIAN_POINT('Ctrl Pts',(-26.141044455505,-14.4917978275685,
113.07789332878)) ;
#193594 = CARTESIAN_POINT('Ctrl Pts',(-26.2209372515167,-14.4998539330622,
113.356520375798)) ;
#193595 = CARTESIAN_POINT('Ctrl Pts',(-26.2986502411454,-14.4309092256038,
113.628683576885)) ;
#193596 = CARTESIAN_POINT('Ctrl Pts',(-26.3674757304941,-14.2894596882656,
113.873752815504)) ;
#193597 = CARTESIAN_POINT('Ctrl Pts',(-26.4219359703617,-14.0846391379262,
114.075220353395)) ;
#193598 = CARTESIAN_POINT('Ctrl Pts',(-26.4568504724485,-13.833584389583,
114.216907404291)) ;
#193599 = CARTESIAN_POINT('Ctrl Pts',(-26.469569796329,-13.5522887119168,
114.291086084856)) ;
#193600 = CARTESIAN_POINT('Ctrl Pts',(-26.4579117148728,-13.2592972529684,
114.291267191308)) ;
#193601 = CARTESIAN_POINT('Ctrl Pts',(-26.4225035557811,-12.9811038250668,
114.218671706621)) ;
#193602 = CARTESIAN_POINT('Ctrl Pts',(-26.3646027960108,-12.7319954339599,
114.077855142364)) ;
#193603 = CARTESIAN_POINT('Ctrl Pts',(-26.2880633731457,-12.5329045763516,
113.880121143368)) ;
#193604 = CARTESIAN_POINT('Ctrl Pts',(-26.1969121836829,-12.3964115152595,
113.638084995048)) ;
#193605 = CARTESIAN_POINT('Ctrl Pts',(-26.097882878132,-12.3338312624075,
113.371853705732)) ;
#193606 = CARTESIAN_POINT('Ctrl Pts',(-25.9966525666846,-12.3486707517994,
113.098994699644)) ;
#193607 = CARTESIAN_POINT('Ctrl Pts',(-25.9000472227805,-12.4397941697449,
112.840152077552)) ;
#193608 = CARTESIAN_POINT('Ctrl Pts',(-25.8135929246481,-12.6021170084136,
112.612453782006)) ;
#193609 = CARTESIAN_POINT('Ctrl Pts',(-25.7439720862117,-12.8208593941247,
112.435659485376)) ;
#193610 = CARTESIAN_POINT('Ctrl Pts',(-25.6940349138125,-13.084370773037,
112.319151955814)) ;
#193611 = CARTESIAN_POINT('Ctrl Pts',(-25.6675129647773,-13.3711928765175,
112.273852263887)) ;
#193612 = CARTESIAN_POINT('Ctrl Pts',(-25.6652923171855,-13.6609866789311,
112.302537231817)) ;
#193613 = CARTESIAN_POINT('Ctrl Pts',(-25.6865853284364,-13.9327616913683,
112.402736133509)) ;
#193614 = CARTESIAN_POINT('Ctrl Pts',(-25.7296598130416,-14.1696775509721,
112.569592493143)) ;
#193615 = CARTESIAN_POINT('Ctrl Pts',(-25.789817147401,-14.3505522399701,
112.788110084322)) ;
#193616 = CARTESIAN_POINT('Ctrl Pts',(-25.8627735208457,-14.4659895814683,
113.045823772028)) ;
#193617 = CARTESIAN_POINT('Ctrl Pts',(-25.9424652085819,-14.5060552317741,
113.324112272392)) ;
#193618 = CARTESIAN_POINT('Ctrl Pts',(-26.0220030697392,-14.4677867862301,
113.601843781957)) ;
#193619 = CARTESIAN_POINT('Ctrl Pts',(-26.094854630819,-14.3553856703914,
113.859024726864)) ;
#193620 = CARTESIAN_POINT('Ctrl Pts',(-26.1560900365016,-14.1738642018268,
114.081250316961)) ;
#193621 = CARTESIAN_POINT('Ctrl Pts',(-26.1991928753205,-13.9401973275635,
114.247846762684)) ;
#193622 = CARTESIAN_POINT('Ctrl Pts',(-26.2212325199795,-13.6684975496401,
114.35043177796)) ;
#193623 = CARTESIAN_POINT('Ctrl Pts',(-26.2196857700443,-13.3792258998284,
114.381117503958)) ;
#193624 = CARTESIAN_POINT('Ctrl Pts',(-26.1935600200775,-13.0905267308239,
114.337229266664)) ;
#193625 = CARTESIAN_POINT('Ctrl Pts',(-26.1446708799254,-12.8284630006125,
114.223586216955)) ;
#193626 = CARTESIAN_POINT('Ctrl Pts',(-26.0750221134765,-12.6065365051644,
114.046995192604)) ;
#193627 = CARTESIAN_POINT('Ctrl Pts',(-25.9893085808254,-12.4434900571409,
113.821371187434)) ;
#193628 = CARTESIAN_POINT('Ctrl Pts',(-25.8927472268414,-12.3500508502058,
113.562734682547)) ;
#193629 = CARTESIAN_POINT('Ctrl Pts',(-25.7915387238206,-12.3331953888952,
113.289941672903)) ;
#193630 = CARTESIAN_POINT('Ctrl Pts',(-25.6921668349445,-12.3940161187778,
113.022744551192)) ;
#193631 = CARTESIAN_POINT('Ctrl Pts',(-25.6010011665108,-12.5284976067023,
112.780567517695)) ;
#193632 = CARTESIAN_POINT('Ctrl Pts',(-25.5241403849889,-12.7253590046235,
112.581767024192)) ;
#193633 = CARTESIAN_POINT('Ctrl Pts',(-25.4653269966594,-12.9750336085797,
112.438402703222)) ;
#193634 = CARTESIAN_POINT('Ctrl Pts',(-25.4295219032565,-13.2518773391213,
112.364484091442)) ;
#193635 = CARTESIAN_POINT('Ctrl Pts',(-25.4172132742783,-13.5442043587849,
112.36261312341)) ;
#193636 = CARTESIAN_POINT('Ctrl Pts',(-25.4292212348024,-13.8259451748865,
112.434602285511)) ;
#193637 = CARTESIAN_POINT('Ctrl Pts',(-25.4637880029618,-14.0792480619856,
112.575412566812)) ;
#193638 = CARTESIAN_POINT('Ctrl Pts',(-25.5175967023213,-14.2845087011992,
112.774736681666)) ;
#193639 = CARTESIAN_POINT('Ctrl Pts',(-25.58604236121,-14.4278905637469,113.018639551001)) ;
#193640 = CARTESIAN_POINT('Ctrl Pts',(-25.6636620375048,-14.49909499359,113.290546274635)) ;
#193641 = CARTESIAN_POINT('Ctrl Pts',(-25.7439225347513,-14.492829252027,
113.570454450893)) ;
#193642 = CARTESIAN_POINT('Ctrl Pts',(-25.8206456678488,-14.4093444300335,
113.83969383373)) ;
#193643 = CARTESIAN_POINT('Ctrl Pts',(-25.8872186639727,-14.2544052422715,
114.077996994067)) ;
#193644 = CARTESIAN_POINT('Ctrl Pts',(-25.9379469965569,-14.0410991720381,
114.267799990034)) ;
#193645 = CARTESIAN_POINT('Ctrl Pts',(-25.9690716034183,-13.7816895970119,
114.398141043581)) ;
#193646 = CARTESIAN_POINT('Ctrl Pts',(-25.977202611184,-13.4976199910735,
114.4582556851)) ;
#193647 = CARTESIAN_POINT('Ctrl Pts',(-25.9611123344456,-13.2063007087737,
114.444798177741)) ;
#193648 = CARTESIAN_POINT('Ctrl Pts',(-25.9211552662506,-12.9308185504047,
114.358558160609)) ;
#193649 = CARTESIAN_POINT('Ctrl Pts',(-25.8593713827175,-12.690040453889,
114.205882675566)) ;
#193650 = CARTESIAN_POINT('Ctrl Pts',(-25.7799037685495,-12.5021903792694,
113.999176989546)) ;
#193651 = CARTESIAN_POINT('Ctrl Pts',(-25.6868876116915,-12.3790435207342,
113.751397700364)) ;
#193652 = CARTESIAN_POINT('Ctrl Pts',(-25.5868978508818,-12.3305042760163,
113.482273898361)) ;
#193653 = CARTESIAN_POINT('Ctrl Pts',(-25.4854179660145,-12.3604684800267,
113.208869990196)) ;
#193654 = CARTESIAN_POINT('Ctrl Pts',(-25.3908722354269,-12.4650891112354,
112.956114236995)) ;
#193655 = CARTESIAN_POINT('Ctrl Pts',(-25.3069218934639,-12.6397680496829,
112.736110244212)) ;
#193656 = CARTESIAN_POINT('Ctrl Pts',(-25.2409292762661,-12.8673926753431,
112.570297954244)) ;
#193657 = CARTESIAN_POINT('Ctrl Pts',(-25.1950431269417,-13.138383085188,
112.466309655478)) ;
#193658 = CARTESIAN_POINT('Ctrl Pts',(-25.1732970592646,-13.4250580301084,
112.435262725168)) ;
#193659 = CARTESIAN_POINT('Ctrl Pts',(-25.175431424128,-13.713663843469,112.477262712461)) ;
#193660 = CARTESIAN_POINT('Ctrl Pts',(-25.2013058612131,-13.9818996954329,
112.591702432285)) ;
#193661 = CARTESIAN_POINT('Ctrl Pts',(-25.2475462461254,-14.2073240866329,
112.767809158823)) ;
#193662 = CARTESIAN_POINT('Ctrl Pts',(-25.3107801482558,-14.3779496982449,
112.995927736214)) ;
#193663 = CARTESIAN_POINT('Ctrl Pts',(-25.3855441089235,-14.4795452062324,
113.25916632019)) ;
#193664 = CARTESIAN_POINT('Ctrl Pts',(-25.4657056298432,-14.504675613756,
113.538873967324)) ;
#193665 = CARTESIAN_POINT('Ctrl Pts',(-25.5441348471131,-14.4524935600785,
113.813035826526)) ;
#193666 = CARTESIAN_POINT('Ctrl Pts',(-25.6158038670484,-14.3253673837965,
114.066976143731)) ;
#193667 = CARTESIAN_POINT('Ctrl Pts',(-25.6735934060056,-14.1335026343525,
114.278447647152)) ;
#193668 = CARTESIAN_POINT('Ctrl Pts',(-25.713031726844,-13.8914689377216,
114.433910815975)) ;
#193669 = CARTESIAN_POINT('Ctrl Pts',(-25.7307687812816,-13.6147208150664,
114.523401386807)) ;
#193670 = CARTESIAN_POINT('Ctrl Pts',(-25.7245757601632,-13.3237687258409,
114.540012491979)) ;
#193671 = CARTESIAN_POINT('Ctrl Pts',(-25.6941237439954,-13.0396242352637,
114.482736350999)) ;
#193672 = CARTESIAN_POINT('Ctrl Pts',(-25.6410851839242,-12.7830678889279,
114.356574719083)) ;
#193673 = CARTESIAN_POINT('Ctrl Pts',(-25.5676997033759,-12.5704752635878,
114.168721963641)) ;
#193674 = CARTESIAN_POINT('Ctrl Pts',(-25.4799422590946,-12.4206416986158,
113.936696566694)) ;
#193675 = CARTESIAN_POINT('Ctrl Pts',(-25.381998179666,-12.3408954926335,
113.673866420762)) ;
#193676 = CARTESIAN_POINT('Ctrl Pts',(-25.2803675767541,-12.3388375024718,
113.399883536457)) ;
#193677 = CARTESIAN_POINT('Ctrl Pts',(-25.1823213194761,-12.413706142133,
113.136628920894)) ;
#193678 = CARTESIAN_POINT('Ctrl Pts',(-25.092980715359,-12.5617183582742,
112.900167957605)) ;
#193679 = CARTESIAN_POINT('Ctrl Pts',(-25.0195846393668,-12.7688407831079,
112.711834010416)) ;
#193680 = CARTESIAN_POINT('Ctrl Pts',(-24.9649866794184,-13.0241117816514,
112.581077125632)) ;
#193681 = CARTESIAN_POINT('Ctrl Pts',(-24.9332536836434,-13.3070010234793,
112.51985755415)) ;
#193682 = CARTESIAN_POINT('Ctrl Pts',(-24.925629722327,-13.5985554109386,
112.532164471356)) ;
#193683 = CARTESIAN_POINT('Ctrl Pts',(-24.9421245854702,-13.8770852609277,
112.617931075453)) ;
#193684 = CARTESIAN_POINT('Ctrl Pts',(-24.9804514510273,-14.1214182763711,
112.770005884966)) ;
#193685 = CARTESIAN_POINT('Ctrl Pts',(-25.0373635997591,-14.3164119676812,
112.978804934412)) ;
#193686 = CARTESIAN_POINT('Ctrl Pts',(-25.1082654742619,-14.4472714989735,
113.230330811616)) ;
#193687 = CARTESIAN_POINT('Ctrl Pts',(-25.1868459524037,-14.5039655219921,
113.505134344491)) ;
#193688 = CARTESIAN_POINT('Ctrl Pts',(-25.267129516287,-14.4826373105238,
113.785223901541)) ;
#193689 = CARTESIAN_POINT('Ctrl Pts',(-25.3418916496393,-14.3855815012644,
114.048250710986)) ;
#193690 = CARTESIAN_POINT('Ctrl Pts',(-25.4059102519348,-14.2190969785884,
114.278710495903)) ;
#193691 = CARTESIAN_POINT('Ctrl Pts',(-25.4534572816173,-13.9949296481822,
114.4590197693)) ;
#193692 = CARTESIAN_POINT('Ctrl Pts',(-25.4803949407615,-13.7298783707897,
114.576500255508)) ;
#193693 = CARTESIAN_POINT('Ctrl Pts',(-25.4839639384194,-13.4411780607526,
114.622967439281)) ;
#193694 = CARTESIAN_POINT('Ctrl Pts',(-25.4634405619125,-13.1535366585443,
114.595704133561)) ;
#193695 = CARTESIAN_POINT('Ctrl Pts',(-25.4188861853407,-12.8812078446008,
114.495722751362)) ;
#193696 = CARTESIAN_POINT('Ctrl Pts',(-25.3535678038264,-12.6502697095916,
114.332121264411)) ;
#193697 = CARTESIAN_POINT('Ctrl Pts',(-25.271268624716,-12.4736381112203,
114.116796974903)) ;
#193698 = CARTESIAN_POINT('Ctrl Pts',(-25.1760059663422,-12.3636957343507,
113.862315910691)) ;
#193699 = CARTESIAN_POINT('Ctrl Pts',(-25.0755208022999,-12.3303161657527,
113.59162885322)) ;
#193700 = CARTESIAN_POINT('Ctrl Pts',(-24.975387420301,-12.3741418831008,
113.322042926048)) ;
#193701 = CARTESIAN_POINT('Ctrl Pts',(-24.8815379026335,-12.4937241519796,
113.071825125992)) ;
#193702 = CARTESIAN_POINT('Ctrl Pts',(-24.8012449463837,-12.6783961032596,
112.862605193765)) ;
#193703 = CARTESIAN_POINT('Ctrl Pts',(-24.738447605087,-12.9163766433386,
112.706791373276)) ;
#193704 = CARTESIAN_POINT('Ctrl Pts',(-24.697217131185,-13.1903758945546,
112.616669578636)) ;
#193705 = CARTESIAN_POINT('Ctrl Pts',(-24.679735225327,-13.481432819081,112.598974089601)) ;
#193706 = CARTESIAN_POINT('Ctrl Pts',(-24.6866566649467,-13.7673558416161,
112.655538950219)) ;
#193707 = CARTESIAN_POINT('Ctrl Pts',(-24.7163960105244,-14.0271101613543,
112.781439555252)) ;
#193708 = CARTESIAN_POINT('Ctrl Pts',(-24.7663270399,-14.2445027860115,112.968989653976)) ;
#193709 = CARTESIAN_POINT('Ctrl Pts',(-24.8322750811479,-14.4028029107363,
113.205401926826)) ;
#193710 = CARTESIAN_POINT('Ctrl Pts',(-24.9082113685337,-14.4900131921161,
113.472067220855)) ;
#193711 = CARTESIAN_POINT('Ctrl Pts',(-24.9884934184206,-14.5009049303826,
113.752069619527)) ;
#193712 = CARTESIAN_POINT('Ctrl Pts',(-25.0666037768646,-14.4337694493022,
114.025547084295)) ;
#193713 = CARTESIAN_POINT('Ctrl Pts',(-25.1357889459536,-14.2939322119372,
114.271744953977)) ;
#193714 = CARTESIAN_POINT('Ctrl Pts',(-25.1905524181362,-14.0911613446941,
114.474041191823)) ;
#193715 = CARTESIAN_POINT('Ctrl Pts',(-25.2261345436437,-13.8412394795533,
114.617769466887)) ;
#193716 = CARTESIAN_POINT('Ctrl Pts',(-25.2394283887284,-13.5592605313859,
114.693848406936)) ;
#193717 = CARTESIAN_POINT('Ctrl Pts',(-25.2286664367361,-13.2696223387077,
114.696342245869)) ;
#193718 = CARTESIAN_POINT('Ctrl Pts',(-25.1937485823441,-12.9883139496615,
114.625551828042)) ;
#193719 = CARTESIAN_POINT('Ctrl Pts',(-25.1365175245661,-12.7386910562247,
114.486687971447)) ;
#193720 = CARTESIAN_POINT('Ctrl Pts',(-25.0603010182413,-12.5375785963018,
114.290016712916)) ;
#193721 = CARTESIAN_POINT('Ctrl Pts',(-24.9698092052317,-12.3995778757378,
114.049856870399)) ;
#193722 = CARTESIAN_POINT('Ctrl Pts',(-24.8707009033833,-12.3345174279643,
113.783475116184)) ;
#193723 = CARTESIAN_POINT('Ctrl Pts',(-24.7695605990675,-12.3471393395654,
113.510844338411)) ;
#193724 = CARTESIAN_POINT('Ctrl Pts',(-24.6727328214046,-12.4360428670471,
113.251326381663)) ;
#193725 = CARTESIAN_POINT('Ctrl Pts',(-24.5859199646112,-12.5962612233629,
113.022510647249)) ;
#193726 = CARTESIAN_POINT('Ctrl Pts',(-24.5156431401964,-12.8139558923281,
112.843788818509)) ;
#193727 = CARTESIAN_POINT('Ctrl Pts',(-24.4652008507486,-13.0756188660845,
112.725627916536)) ;
#193728 = CARTESIAN_POINT('Ctrl Pts',(-24.4379052691479,-13.3624251132735,
112.678030789951)) ;
#193729 = CARTESIAN_POINT('Ctrl Pts',(-24.4348796019806,-13.651982180129,
112.704196399724)) ;
#193730 = CARTESIAN_POINT('Ctrl Pts',(-24.4558001085789,-13.9268736432231,
112.803588355088)) ;
#193731 = CARTESIAN_POINT('Ctrl Pts',(-24.4978634283469,-14.1624927779437,
112.966970517185)) ;
#193732 = CARTESIAN_POINT('Ctrl Pts',(-24.5579911299017,-14.3467872124729,
113.185684905417)) ;
#193733 = CARTESIAN_POINT('Ctrl Pts',(-24.6305363548121,-14.4636106389172,
113.442047638809)) ;
#193734 = CARTESIAN_POINT('Ctrl Pts',(-24.7098618797107,-14.505904926533,
113.719115599711)) ;
#193735 = CARTESIAN_POINT('Ctrl Pts',(-24.789457567232,-14.4703681622542,
113.996992018783)) ;
#193736 = CARTESIAN_POINT('Ctrl Pts',(-24.8630886166822,-14.359008640194,
114.256813432633)) ;
#193737 = CARTESIAN_POINT('Ctrl Pts',(-24.9242076077781,-14.1808823670753,
114.478358262173)) ;
#193738 = CARTESIAN_POINT('Ctrl Pts',(-24.9681883548515,-13.9476582149858,
114.647809634132)) ;
#193739 = CARTESIAN_POINT('Ctrl Pts',(-24.9908627448388,-13.6767014389998,
114.75232403868)) ;
#193740 = CARTESIAN_POINT('Ctrl Pts',(-24.9899695835005,-13.3872299120028,
114.785058404499)) ;
#193741 = CARTESIAN_POINT('Ctrl Pts',(-24.9646913454561,-13.0993467868879,
114.743596413779)) ;
#193742 = CARTESIAN_POINT('Ctrl Pts',(-24.9162024965776,-12.8349662721153,
114.631357615901)) ;
#193743 = CARTESIAN_POINT('Ctrl Pts',(-24.847245455251,-12.6123125745559,
114.45676980248)) ;
#193744 = CARTESIAN_POINT('Ctrl Pts',(-24.7618055368288,-12.447065748415,
114.232038687256)) ;
#193745 = CARTESIAN_POINT('Ctrl Pts',(-24.6654288827052,-12.3516677675638,
113.973971864171)) ;
#193746 = CARTESIAN_POINT('Ctrl Pts',(-24.5645423752006,-12.3325934792249,
113.702063110992)) ;
#193747 = CARTESIAN_POINT('Ctrl Pts',(-24.4649295396859,-12.3910918553195,
113.434163508363)) ;
#193748 = CARTESIAN_POINT('Ctrl Pts',(-24.37322692579,-12.5239274893633,113.190432787571)) ;
#193749 = CARTESIAN_POINT('Ctrl Pts',(-24.2960054560042,-12.7192927751428,
112.990520520361)) ;
#193750 = CARTESIAN_POINT('Ctrl Pts',(-24.2369143117434,-12.9658343070978,
112.84605739491)) ;
#193751 = CARTESIAN_POINT('Ctrl Pts',(-24.2000431301647,-13.2443245338218,
112.769193829695)) ;
#193752 = CARTESIAN_POINT('Ctrl Pts',(-24.187186648989,-13.5367809605308,
112.765670474547)) ;
#193753 = CARTESIAN_POINT('Ctrl Pts',(-24.198485812454,-13.8179726435299,
112.835367593194)) ;
#193754 = CARTESIAN_POINT('Ctrl Pts',(-24.2324273152291,-14.0724753431544,
112.974281755024)) ;
#193755 = CARTESIAN_POINT('Ctrl Pts',(-24.2856593105687,-14.279096140685,
113.171804870744)) ;
#193756 = CARTESIAN_POINT('Ctrl Pts',(-24.3538376843237,-14.4248617955916,
113.414949069186)) ;
#193757 = CARTESIAN_POINT('Ctrl Pts',(-24.4316472822689,-14.4982152843021,
113.687591297354)) ;
#193758 = CARTESIAN_POINT('Ctrl Pts',(-24.511415885813,-14.4941260357652,
113.965774681427)) ;
#193759 = CARTESIAN_POINT('Ctrl Pts',(-24.588572932717,-14.4126782343137,
114.236447003153)) ;
#193760 = CARTESIAN_POINT('Ctrl Pts',(-24.6553633361676,-14.2599648668114,
114.475326275185)) ;
#193761 = CARTESIAN_POINT('Ctrl Pts',(-24.7066777082595,-14.0478524029628,
114.666975267341)) ;
#193762 = CARTESIAN_POINT('Ctrl Pts',(-24.7383886959719,-13.7904112840523,
114.79898244504)) ;
#193763 = CARTESIAN_POINT('Ctrl Pts',(-24.7472587412919,-13.5044552055669,
114.861642887694)) ;
#193764 = CARTESIAN_POINT('Ctrl Pts',(-24.7317360628477,-13.2137879040768,
114.849818087154)) ;
#193765 = CARTESIAN_POINT('Ctrl Pts',(-24.6925768386914,-12.9385963486889,
114.765886618446)) ;
#193766 = CARTESIAN_POINT('Ctrl Pts',(-24.6315155721698,-12.6966955833364,
114.615366123145)) ;
#193767 = CARTESIAN_POINT('Ctrl Pts',(-24.5521621899109,-12.5064217313258,
114.409158146371)) ;
#193768 = CARTESIAN_POINT('Ctrl Pts',(-24.4595930056771,-12.3814205030376,
114.162674429355)) ;
#193769 = CARTESIAN_POINT('Ctrl Pts',(-24.3591960058421,-12.3309490204366,
113.892499417778)) ;
#193770 = CARTESIAN_POINT('Ctrl Pts',(-24.2590492512348,-12.3579787522632,
113.62264874675)) ;
#193771 = CARTESIAN_POINT('Ctrl Pts',(-24.1631094563438,-12.461461206882,
113.36607630111)) ;
#193772 = CARTESIAN_POINT('Ctrl Pts',(-24.0794846118896,-12.6327579824641,
113.146729045038)) ;
#193773 = CARTESIAN_POINT('Ctrl Pts',(-24.0122990421959,-12.8610649262646,
112.977629767465)) ;
#193774 = CARTESIAN_POINT('Ctrl Pts',(-23.9662485633249,-13.1282120035714,
112.872739576532)) ;
#193775 = CARTESIAN_POINT('Ctrl Pts',(-23.9434524616525,-13.4170777357306,
112.838817161117)) ;
#193776 = CARTESIAN_POINT('Ctrl Pts',(-23.9449981053748,-13.7056413839055,
112.878978183992)) ;
#193777 = CARTESIAN_POINT('Ctrl Pts',(-23.9701821735012,-13.9747406301587,
112.991309111019)) ;
#193778 = CARTESIAN_POINT('Ctrl Pts',(-24.0160072122531,-14.201974810105,
113.166223946965)) ;
#193779 = CARTESIAN_POINT('Ctrl Pts',(-24.0787453413408,-14.3739130003505,
113.392766421991)) ;
#193780 = CARTESIAN_POINT('Ctrl Pts',(-24.153021958778,-14.4775305035498,
113.654416785986)) ;
#193781 = CARTESIAN_POINT('Ctrl Pts',(-24.2334081776458,-14.5050608269986,
113.934939965511)) ;
#193782 = CARTESIAN_POINT('Ctrl Pts',(-24.3118138425738,-14.4551363613954,
114.208959708269)) ;
#193783 = CARTESIAN_POINT('Ctrl Pts',(-24.3838624730078,-14.3298705824412,
114.464102745858)) ;
#193784 = CARTESIAN_POINT('Ctrl Pts',(-24.4418657884039,-14.1407879039854,
114.676048055119)) ;
#193785 = CARTESIAN_POINT('Ctrl Pts',(-24.4821519623665,-13.8991517087972,
114.83424842299)) ;
#193786 = CARTESIAN_POINT('Ctrl Pts',(-24.5005313129686,-13.622377664187,
114.925775683021)) ;
#193787 = CARTESIAN_POINT('Ctrl Pts',(-24.49501436777,-13.3324243748073,114.944342617232)) ;
#193788 = CARTESIAN_POINT('Ctrl Pts',(-24.4653775774576,-13.0478498918573,
114.889526808152)) ;
#193789 = CARTESIAN_POINT('Ctrl Pts',(-24.4124318331185,-12.7884262570381,
114.76392923946)) ;
#193790 = CARTESIAN_POINT('Ctrl Pts',(-24.3401997969462,-12.5764203972658,
114.57925123095)) ;
#193791 = CARTESIAN_POINT('Ctrl Pts',(-24.2523979814976,-12.4236100991773,
114.347280755597)) ;
#193792 = CARTESIAN_POINT('Ctrl Pts',(-24.1544007543503,-12.3419562515338,
114.084359044048)) ;
#193793 = CARTESIAN_POINT('Ctrl Pts',(-24.0529879307825,-12.3379525743983,
113.810967700911)) ;
#193794 = CARTESIAN_POINT('Ctrl Pts',(-23.9551105454002,-12.4104778611719,
113.54810794873)) ;
#193795 = CARTESIAN_POINT('Ctrl Pts',(-23.8656364276719,-12.5557718304403,
113.311130140898)) ;
#193796 = CARTESIAN_POINT('Ctrl Pts',(-23.7913251487216,-12.7621800376528,
113.120181789862)) ;
#193797 = CARTESIAN_POINT('Ctrl Pts',(-23.7361036954528,-13.0168738808962,
112.987578292511)) ;
#193798 = CARTESIAN_POINT('Ctrl Pts',(-23.703804074422,-13.2984278863564,
112.924531497575)) ;
#193799 = CARTESIAN_POINT('Ctrl Pts',(-23.6954444130968,-13.5897265030932,
112.93456078648)) ;
#193800 = CARTESIAN_POINT('Ctrl Pts',(-23.7111888510481,-13.8688372211758,
113.018021310344)) ;
#193801 = CARTESIAN_POINT('Ctrl Pts',(-23.7490277618584,-14.1152016754008,
113.168722954981)) ;
#193802 = CARTESIAN_POINT('Ctrl Pts',(-23.8054647064364,-14.3116011164225,
113.376051058603)) ;
#193803 = CARTESIAN_POINT('Ctrl Pts',(-23.8758475364015,-14.4442909382302,
113.625906113769)) ;
#193804 = CARTESIAN_POINT('Ctrl Pts',(-23.9543884340958,-14.5033545209173,
113.900640311808)) ;
#193805 = CARTESIAN_POINT('Ctrl Pts',(-24.034459322074,-14.4845849990311,
114.179961742102)) ;
#193806 = CARTESIAN_POINT('Ctrl Pts',(-24.1098198340275,-14.3894948595566,
114.444970199635)) ;
#193807 = CARTESIAN_POINT('Ctrl Pts',(-24.1743167962616,-14.2243477865837,
114.676951586264)) ;
#193808 = CARTESIAN_POINT('Ctrl Pts',(-24.222244696456,-14.0022176408066,
114.858320300605)) ;
#193809 = CARTESIAN_POINT('Ctrl Pts',(-24.249840889695,-13.738467096939,114.977769983769)) ;
#193810 = CARTESIAN_POINT('Ctrl Pts',(-24.2541673118349,-13.4497089979361,
115.026595498721)) ;
#193811 = CARTESIAN_POINT('Ctrl Pts',(-24.2342295189752,-13.1612741016994,
115.001189108722)) ;
#193812 = CARTESIAN_POINT('Ctrl Pts',(-24.190640216784,-12.8897094409154,
114.903930822118)) ;
#193813 = CARTESIAN_POINT('Ctrl Pts',(-24.12571950388,-12.6562456914582,114.741683307062)) ;
#193814 = CARTESIAN_POINT('Ctrl Pts',(-24.0436220945344,-12.4776727385034,
114.527047044572)) ;
#193815 = CARTESIAN_POINT('Ctrl Pts',(-23.949166950014,-12.3662041520314,
114.27482871689)) ;
#193816 = CARTESIAN_POINT('Ctrl Pts',(-23.8486819494618,-12.3300379060018,
114.004176603024)) ;
#193817 = CARTESIAN_POINT('Ctrl Pts',(-23.7479716280047,-12.3719948524369,
113.733003975022)) ;
#193818 = CARTESIAN_POINT('Ctrl Pts',(-23.6544815761993,-12.4886302946211,
113.483633344995)) ;
#193819 = CARTESIAN_POINT('Ctrl Pts',(-23.5734119895845,-12.6716133926028,
113.272144861852)) ;
#193820 = CARTESIAN_POINT('Ctrl Pts',(-23.5097546848615,-12.9096205473869,
113.113892958082)) ;
#193821 = CARTESIAN_POINT('Ctrl Pts',(-23.4680736791357,-13.1819739695916,
113.02227623672)) ;
#193822 = CARTESIAN_POINT('Ctrl Pts',(-23.4498548257593,-13.4720244815185,
113.002241777348)) ;
#193823 = CARTESIAN_POINT('Ctrl Pts',(-23.4559991647249,-13.7591219512168,
113.056520534112)) ;
#193824 = CARTESIAN_POINT('Ctrl Pts',(-23.4853259386765,-14.0209982570872,
113.181335126666)) ;
#193825 = CARTESIAN_POINT('Ctrl Pts',(-23.5345041189141,-14.2386408615737,
113.36640397491)) ;
#193826 = CARTESIAN_POINT('Ctrl Pts',(-23.6001054827243,-14.3991847031552,
113.601804261301)) ;
#193827 = CARTESIAN_POINT('Ctrl Pts',(-23.6758396635348,-14.4885294284138,
113.867853985645)) ;
#193828 = CARTESIAN_POINT('Ctrl Pts',(-23.7560787132041,-14.5016597743674,
114.147723270265)) ;
#193829 = CARTESIAN_POINT('Ctrl Pts',(-23.8342305464961,-14.437009415365,
114.421263368043)) ;
#193830 = CARTESIAN_POINT('Ctrl Pts',(-23.9038790142128,-14.2988734246617,
114.668946179201)) ;
#193831 = CARTESIAN_POINT('Ctrl Pts',(-23.9589267388881,-14.0989764690058,
114.871924271344)) ;
#193832 = CARTESIAN_POINT('Ctrl Pts',(-23.9954157212117,-13.8484694868484,
115.01867831934)) ;
#193833 = CARTESIAN_POINT('Ctrl Pts',(-24.0092992091124,-13.5679794956402,
115.096428165126)) ;
#193834 = CARTESIAN_POINT('Ctrl Pts',(-23.9992431261541,-13.2778704302602,
115.101136556638)) ;
#193835 = CARTESIAN_POINT('Ctrl Pts',(-23.9651195032617,-12.9966579805532,
115.03267001783)) ;
#193836 = CARTESIAN_POINT('Ctrl Pts',(-23.9083188929157,-12.7449733317735,
114.895243151894)) ;
#193837 = CARTESIAN_POINT('Ctrl Pts',(-23.8326075291051,-12.5424420519023,
114.700085714252)) ;
#193838 = CARTESIAN_POINT('Ctrl Pts',(-23.7423558200825,-12.4024494998622,
114.460690641158)) ;
#193839 = CARTESIAN_POINT('Ctrl Pts',(-23.6437350301605,-12.33540698977,114.195676204108)) ;
#193840 = CARTESIAN_POINT('Ctrl Pts',(-23.54230497616,-12.3455818235887,113.922252265825)) ;
#193841 = CARTESIAN_POINT('Ctrl Pts',(-23.4449159493085,-12.433061741337,
113.661165866049)) ;
#193842 = CARTESIAN_POINT('Ctrl Pts',(-23.3581859160956,-12.5907670484714,
113.432424558756)) ;
#193843 = CARTESIAN_POINT('Ctrl Pts',(-23.2872506370322,-12.8072730343164,
113.25175834982)) ;
#193844 = CARTESIAN_POINT('Ctrl Pts',(-23.2361882931638,-13.0681776762317,
113.131728504028)) ;
#193845 = CARTESIAN_POINT('Ctrl Pts',(-23.2082374843446,-13.3550287065478,
113.082188386664)) ;
#193846 = CARTESIAN_POINT('Ctrl Pts',(-23.2046137347424,-13.6436167217993,
113.106398539743)) ;
#193847 = CARTESIAN_POINT('Ctrl Pts',(-23.2246473462219,-13.9180811572707,
113.202915786182)) ;
#193848 = CARTESIAN_POINT('Ctrl Pts',(-23.2663198478807,-14.156549136634,
113.365316344901)) ;
#193849 = CARTESIAN_POINT('Ctrl Pts',(-23.3260277991125,-14.3423727651068,
113.58274099428)) ;
#193850 = CARTESIAN_POINT('Ctrl Pts',(-23.3982430302962,-14.4613427108393,
113.838084052962)) ;
#193851 = CARTESIAN_POINT('Ctrl Pts',(-23.4778308247352,-14.5057889124528,
114.116110858595)) ;
#193852 = CARTESIAN_POINT('Ctrl Pts',(-23.5571252249388,-14.4724226584541,
114.392900262027)) ;
#193853 = CARTESIAN_POINT('Ctrl Pts',(-23.6311473330998,-14.3630839653471,
114.653969620511)) ;
#193854 = CARTESIAN_POINT('Ctrl Pts',(-23.6926670750486,-14.1865023299291,
114.87674421223)) ;
#193855 = CARTESIAN_POINT('Ctrl Pts',(-23.737109657086,-13.9552367476643,
115.047514669265)) ;
#193856 = CARTESIAN_POINT('Ctrl Pts',(-23.7605010634612,-13.6844063432408,
115.1543055001)) ;
#193857 = CARTESIAN_POINT('Ctrl Pts',(-23.760236922336,-13.395616216205,115.188901213406)) ;
#193858 = CARTESIAN_POINT('Ctrl Pts',(-23.7358042656124,-13.1080920804484,
115.149918807693)) ;
#193859 = CARTESIAN_POINT('Ctrl Pts',(-23.6876957397051,-12.8414911099526,
115.039017564153)) ;
#193860 = CARTESIAN_POINT('Ctrl Pts',(-23.6196197911873,-12.6185827250958,
114.866926329754)) ;
#193861 = CARTESIAN_POINT('Ctrl Pts',(-23.5344644232555,-12.4509854490646,
114.643132785995)) ;
#193862 = CARTESIAN_POINT('Ctrl Pts',(-23.4384531446303,-12.3534810644787,
114.386130027561)) ;
#193863 = CARTESIAN_POINT('Ctrl Pts',(-23.3373005505562,-12.3320089256095,
114.113522831925)) ;
#193864 = CARTESIAN_POINT('Ctrl Pts',(-23.2376722572993,-12.3884256006082,
113.845536510079)) ;
#193865 = CARTESIAN_POINT('Ctrl Pts',(-23.1459449956219,-12.5185566369419,
113.601605269859)) ;
#193866 = CARTESIAN_POINT('Ctrl Pts',(-23.0678884204578,-12.7128146761132,
113.399287149443)) ;
#193867 = CARTESIAN_POINT('Ctrl Pts',(-23.0080726213499,-12.9591843124397,
113.25274040277)) ;
#193868 = CARTESIAN_POINT('Ctrl Pts',(-22.9707781839292,-13.2359003760254,
113.174438606138)) ;
#193869 = CARTESIAN_POINT('Ctrl Pts',(-22.9571487392571,-13.5269168879405,
113.168395654949)) ;
#193870 = CARTESIAN_POINT('Ctrl Pts',(-22.9677330810903,-13.8100818853549,
113.236088284649)) ;
#193871 = CARTESIAN_POINT('Ctrl Pts',(-23.0011086677166,-14.0658493622321,
113.373303697314)) ;
#193872 = CARTESIAN_POINT('Ctrl Pts',(-23.0539725203832,-14.2744004374724,
113.569778136137)) ;
#193873 = CARTESIAN_POINT('Ctrl Pts',(-23.1216893204055,-14.4215076088756,
113.811439149396)) ;
#193874 = CARTESIAN_POINT('Ctrl Pts',(-23.1988440710271,-14.4970287487176,
114.081882466236)) ;
#193875 = CARTESIAN_POINT('Ctrl Pts',(-23.2792349709217,-14.495364180026,
114.362233916425)) ;
#193876 = CARTESIAN_POINT('Ctrl Pts',(-23.3563637359517,-14.4159600881982,
114.632728072821)) ;
#193877 = CARTESIAN_POINT('Ctrl Pts',(-23.4233024681412,-14.2660479877099,
114.871922390373)) ;
#193878 = CARTESIAN_POINT('Ctrl Pts',(-23.4754105644669,-14.0549162780305,
115.066119893745)) ;
#193879 = CARTESIAN_POINT('Ctrl Pts',(-23.5077572471595,-13.7973888984154,
115.200198351239)) ;
#193880 = CARTESIAN_POINT('Ctrl Pts',(-23.5172572061641,-13.5143192821472,
115.264479052943)) ;
#193881 = CARTESIAN_POINT('Ctrl Pts',(-23.5025567461663,-13.2228141005811,
115.255249135668)) ;
#193882 = CARTESIAN_POINT('Ctrl Pts',(-23.4640229788602,-12.9463122499942,
115.173287772294)) ;
#193883 = CARTESIAN_POINT('Ctrl Pts',(-23.4033068584606,-12.7025112775513,
115.023933887441)) ;
#193884 = CARTESIAN_POINT('Ctrl Pts',(-23.3247469439269,-12.5113386435153,
114.819989036996)) ;
#193885 = CARTESIAN_POINT('Ctrl Pts',(-23.2322554152184,-12.3839986409936,
114.573835678973)) ;
#193886 = CARTESIAN_POINT('Ctrl Pts',(-23.1325124738357,-12.3313598679509,
114.305463729675)) ;
#193887 = CARTESIAN_POINT('Ctrl Pts',(-23.0315695868954,-12.3561484752169,
114.033447032347)) ;
#193888 = CARTESIAN_POINT('Ctrl Pts',(-22.9354487583315,-12.4578681360596,
113.776309520322)) ;
#193889 = CARTESIAN_POINT('Ctrl Pts',(-22.8516194022014,-12.6270814220524,
113.556268256684)) ;
#193890 = CARTESIAN_POINT('Ctrl Pts',(-22.7839838450555,-12.8533401319523,
113.385716322209)) ;
#193891 = CARTESIAN_POINT('Ctrl Pts',(-22.737057523416,-13.1210491167834,
113.278349913962)) ;
#193892 = CARTESIAN_POINT('Ctrl Pts',(-22.7137114782824,-13.40900770729,113.242669521787)) ;
#193893 = CARTESIAN_POINT('Ctrl Pts',(-22.7145790475153,-13.6972694862933,
113.280702081642)) ;
#193894 = CARTESIAN_POINT('Ctrl Pts',(-22.73888971428,-13.9663054532962,113.390221067271)) ;
#193895 = CARTESIAN_POINT('Ctrl Pts',(-22.7845308373615,-14.1969043333081,
113.564878486232)) ;
#193896 = CARTESIAN_POINT('Ctrl Pts',(-22.8467313080852,-14.3698914257013,
113.789672047739)) ;
#193897 = CARTESIAN_POINT('Ctrl Pts',(-22.9207425971933,-14.4755193866787,
114.050515802976)) ;
#193898 = CARTESIAN_POINT('Ctrl Pts',(-23.0006816978968,-14.5054697818126,
114.329505017033)) ;
#193899 = CARTESIAN_POINT('Ctrl Pts',(-23.0797492263395,-14.4574393177702,
114.6057916227)) ;
#193900 = CARTESIAN_POINT('Ctrl Pts',(-23.1516520346911,-14.3349211938034,
114.860267274073)) ;
#193901 = CARTESIAN_POINT('Ctrl Pts',(-23.2103873638468,-14.1470800055845,
115.074578542204)) ;
#193902 = CARTESIAN_POINT('Ctrl Pts',(-23.2512289756988,-13.9065331674936,
115.234478316148)) ;
#193903 = CARTESIAN_POINT('Ctrl Pts',(-23.2702582801817,-13.630738678715,
115.327956236279)) ;
#193904 = CARTESIAN_POINT('Ctrl Pts',(-23.2654718156878,-13.3408270196336,
115.34875619149)) ;
#193905 = CARTESIAN_POINT('Ctrl Pts',(-23.2364052797184,-13.0553492265632,
115.295741122605)) ;
#193906 = CARTESIAN_POINT('Ctrl Pts',(-23.184450119502,-12.7963986353394,
115.172941175961)) ;
#193907 = CARTESIAN_POINT('Ctrl Pts',(-23.112508885965,-12.581755675213,114.98929825524)) ;
#193908 = CARTESIAN_POINT('Ctrl Pts',(-23.0250710503237,-12.4271874700909,
114.758426315697)) ;
#193909 = CARTESIAN_POINT('Ctrl Pts',(-22.9276247608224,-12.3434882644401,
114.49706508371)) ;
#193910 = CARTESIAN_POINT('Ctrl Pts',(-22.826190770514,-12.3367187774922,
114.223618478407)) ;
#193911 = CARTESIAN_POINT('Ctrl Pts',(-22.7275355764204,-12.4076100218016,
113.958611864948)) ;
#193912 = CARTESIAN_POINT('Ctrl Pts',(-22.6381489586998,-12.5503272886106,
113.721728947846)) ;
#193913 = CARTESIAN_POINT('Ctrl Pts',(-22.5630668542689,-12.7556871760659,
113.528549608634)) ;
#193914 = CARTESIAN_POINT('Ctrl Pts',(-22.5073121196337,-13.0091921750313,
113.394296840887)) ;
#193915 = CARTESIAN_POINT('Ctrl Pts',(-22.4743110003687,-13.2902503547293,
113.32912295841)) ;
#193916 = CARTESIAN_POINT('Ctrl Pts',(-22.4652747457874,-13.5823834440121,
113.337185548665)) ;
#193917 = CARTESIAN_POINT('Ctrl Pts',(-22.4804477896373,-13.8618181146796,
113.418880666887)) ;
#193918 = CARTESIAN_POINT('Ctrl Pts',(-22.517518476082,-14.1083106024044,
113.567088552821)) ;
#193919 = CARTESIAN_POINT('Ctrl Pts',(-22.5736052210533,-14.3070623418306,
113.773452298608)) ;
#193920 = CARTESIAN_POINT('Ctrl Pts',(-22.6439238545744,-14.4418892785907,
114.023216814566)) ;
#193921 = CARTESIAN_POINT('Ctrl Pts',(-22.7221906575843,-14.502692884587,
114.29704932502)) ;
#193922 = CARTESIAN_POINT('Ctrl Pts',(-22.8020413108005,-14.4862255258319,
114.575584821507)) ;
#193923 = CARTESIAN_POINT('Ctrl Pts',(-22.877609829832,-14.3934141564473,
114.841215988645)) ;
#193924 = CARTESIAN_POINT('Ctrl Pts',(-22.9425681516689,-14.2302607448999,
115.074611405796)) ;
#193925 = CARTESIAN_POINT('Ctrl Pts',(-22.9912511714667,-14.0081666908763,
115.258483536822)) ;
#193926 = CARTESIAN_POINT('Ctrl Pts',(-23.0192337790016,-13.7466548362381,
115.378918754356)) ;
#193927 = CARTESIAN_POINT('Ctrl Pts',(-23.0243744063994,-13.4587847124533,
115.430169417964)) ;
#193928 = CARTESIAN_POINT('Ctrl Pts',(-23.0049652251957,-13.1685102080527,
115.4065743669)) ;
#193929 = CARTESIAN_POINT('Ctrl Pts',(-22.9622751071858,-12.8978336872395,
115.311834565575)) ;
#193930 = CARTESIAN_POINT('Ctrl Pts',(-22.8977448880343,-12.6619537350285,
115.150913911777)) ;
#193931 = CARTESIAN_POINT('Ctrl Pts',(-22.8158701194052,-12.4816257056073,
114.937014037923)) ;
#193932 = CARTESIAN_POINT('Ctrl Pts',(-22.7221314995921,-12.3684889471066,
114.686813418536)) ;
#193933 = CARTESIAN_POINT('Ctrl Pts',(-22.6211642213523,-12.3299903879882,
114.414896154153)) ;
#193934 = CARTESIAN_POINT('Ctrl Pts',(-22.5210459323926,-12.3696139932957,
114.145284395622)) ;
#193935 = CARTESIAN_POINT('Ctrl Pts',(-22.4270329126327,-12.4839372794238,
113.894388923213)) ;
#193936 = CARTESIAN_POINT('Ctrl Pts',(-22.3450439580957,-12.6667316342934,
113.680343028654)) ;
#193937 = CARTESIAN_POINT('Ctrl Pts',(-22.2812994602008,-12.9020313562946,
113.521591306162)) ;
#193938 = CARTESIAN_POINT('Ctrl Pts',(-22.2388473261469,-13.1740426154344,
113.427694180976)) ;
#193939 = CARTESIAN_POINT('Ctrl Pts',(-22.2199943655419,-13.4634545824485,
113.40566955685)) ;
#193940 = CARTESIAN_POINT('Ctrl Pts',(-22.2254048356507,-13.7505708131454,
113.45766775839)) ;
#193941 = CARTESIAN_POINT('Ctrl Pts',(-22.253988225315,-14.0133363300327,
113.580184190739)) ;
#193942 = CARTESIAN_POINT('Ctrl Pts',(-22.302884463881,-14.2335678065818,
113.764575325811)) ;
#193943 = CARTESIAN_POINT('Ctrl Pts',(-22.3681132301931,-14.3958087768564,
113.998825699408)) ;
#193944 = CARTESIAN_POINT('Ctrl Pts',(-22.443875331704,-14.4872051600084,
114.265066140511)) ;
#193945 = CARTESIAN_POINT('Ctrl Pts',(-22.5236867142171,-14.5023836342265,
114.543451391417)) ;
#193946 = CARTESIAN_POINT('Ctrl Pts',(-22.6023114828813,-14.4395233841403,
114.8185888207)) ;
#193947 = CARTESIAN_POINT('Ctrl Pts',(-22.6719122092473,-14.3038981389521,
115.065942143316)) ;
#193948 = CARTESIAN_POINT('Ctrl Pts',(-22.7275755368524,-14.1052991872385,
115.270872462987)) ;
#193949 = CARTESIAN_POINT('Ctrl Pts',(-22.7645650054977,-13.8563431079666,
115.419085314818)) ;
#193950 = CARTESIAN_POINT('Ctrl Pts',(-22.7791798044281,-13.5768529523028,
115.499023031472)) ;
#193951 = CARTESIAN_POINT('Ctrl Pts',(-22.7697827423378,-13.2855121533732,
115.505888509514)) ;
#193952 = CARTESIAN_POINT('Ctrl Pts',(-22.736267599059,-13.0041275578471,
115.439237761638)) ;
#193953 = CARTESIAN_POINT('Ctrl Pts',(-22.6804050530378,-12.7524010633512,
115.304496989377)) ;
#193954 = CARTESIAN_POINT('Ctrl Pts',(-22.6049368462365,-12.5474082659178,
115.110214285938)) ;
#193955 = CARTESIAN_POINT('Ctrl Pts',(-22.5152721436028,-12.4057612857423,
114.872509443197)) ;
#193956 = CARTESIAN_POINT('Ctrl Pts',(-22.416477982246,-12.3361751661113,
114.607093665793)) ;
#193957 = CARTESIAN_POINT('Ctrl Pts',(-22.3151654199719,-12.3442704255669,
114.333978009921)) ;
#193958 = CARTESIAN_POINT('Ctrl Pts',(-22.2178317346334,-12.4291570429794,
114.072959782331)) ;
#193959 = CARTESIAN_POINT('Ctrl Pts',(-22.1305576720065,-12.5849331529663,
113.842608904662)) ;
#193960 = CARTESIAN_POINT('Ctrl Pts',(-22.0589049961337,-12.8005108515807,
113.659850775532)) ;
#193961 = CARTESIAN_POINT('Ctrl Pts',(-22.0073169664416,-13.060269126664,
113.538192775077)) ;
#193962 = CARTESIAN_POINT('Ctrl Pts',(-21.978691089474,-13.3453693583979,
113.486439374298)) ;
#193963 = CARTESIAN_POINT('Ctrl Pts',(-21.9743140972656,-13.6361640667827,
113.508607131723)) ;
#193964 = CARTESIAN_POINT('Ctrl Pts',(-21.9936997725589,-13.9104324089111,
113.603035067072)) ;
#193965 = CARTESIAN_POINT('Ctrl Pts',(-22.0347431039267,-14.1501784561149,
113.763511943349)) ;
#193966 = CARTESIAN_POINT('Ctrl Pts',(-22.0939751521265,-14.3377944456025,
113.979478469494)) ;
#193967 = CARTESIAN_POINT('Ctrl Pts',(-22.1659929301065,-14.4588735568458,
114.234265903067)) ;
#193968 = CARTESIAN_POINT('Ctrl Pts',(-22.2451385688619,-14.5056122473976,
114.510797193633)) ;
#193969 = CARTESIAN_POINT('Ctrl Pts',(-22.324940686415,-14.4743736272664,
114.789329071983)) ;
#193970 = CARTESIAN_POINT('Ctrl Pts',(-22.3988824387203,-14.3676054099568,
115.049984802301)) ;
#193971 = CARTESIAN_POINT('Ctrl Pts',(-22.4609934584054,-14.1926642104704,
115.274637530722)) ;
#193972 = CARTESIAN_POINT('Ctrl Pts',(-22.5060098471497,-13.9629645552833,
115.447132030502)) ;
#193973 = CARTESIAN_POINT('Ctrl Pts',(-22.5301282053753,-13.6916669453695,
115.556308146258)) ;
#193974 = CARTESIAN_POINT('Ctrl Pts',(-22.5305152960144,-13.4042886281479,
115.592739547311)) ;
#193975 = CARTESIAN_POINT('Ctrl Pts',(-22.5067605017534,-13.1160881842174,
115.55586845108)) ;
#193976 = CARTESIAN_POINT('Ctrl Pts',(-22.4595154178549,-12.8495738757798,
115.447455103037)) ;
#193977 = CARTESIAN_POINT('Ctrl Pts',(-22.3918481625051,-12.6242652876755,
115.276723191289)) ;
#193978 = CARTESIAN_POINT('Ctrl Pts',(-22.3066463098264,-12.4543477917217,
115.052950743928)) ;
#193979 = CARTESIAN_POINT('Ctrl Pts',(-22.2113534668614,-12.3553371823295,
114.797951573092)) ;
#193980 = CARTESIAN_POINT('Ctrl Pts',(-22.1099317335009,-12.3315537600446,
114.524642057895)) ;
#193981 = CARTESIAN_POINT('Ctrl Pts',(-22.010593220664,-12.3856473127391,
114.257389293014)) ;
#193982 = CARTESIAN_POINT('Ctrl Pts',(-21.9183564548921,-12.513656004823,
114.011961870334)) ;
#193983 = CARTESIAN_POINT('Ctrl Pts',(-21.839571054505,-12.707439556573,113.807586885716)) ;
#193984 = CARTESIAN_POINT('Ctrl Pts',(-21.7797609837458,-12.9500051005904,
113.660688819678)) ;
#193985 = CARTESIAN_POINT('Ctrl Pts',(-21.741415490494,-13.2274462581565,
113.579389468672)) ;
#193986 = CARTESIAN_POINT('Ctrl Pts',(-21.7271451352815,-13.5192262317475,
113.571491516801)) ;
#193987 = CARTESIAN_POINT('Ctrl Pts',(-21.7370271436767,-13.8018769048648,
113.636919707644)) ;
#193988 = CARTESIAN_POINT('Ctrl Pts',(-21.7697376558309,-14.058784271986,
113.772109441117)) ;
#193989 = CARTESIAN_POINT('Ctrl Pts',(-21.8220819037483,-14.2690401451517,
113.967006518844)) ;
#193990 = CARTESIAN_POINT('Ctrl Pts',(-21.8895943124559,-14.418345814643,
114.208124022186)) ;
#193991 = CARTESIAN_POINT('Ctrl Pts',(-21.966477791396,-14.4960013207205,
114.477695371654)) ;
#193992 = CARTESIAN_POINT('Ctrl Pts',(-22.0471672488081,-14.4962457299704,
114.759096539096)) ;
#193993 = CARTESIAN_POINT('Ctrl Pts',(-22.1237856140213,-14.4198799151553,
115.027702043525)) ;
#193994 = CARTESIAN_POINT('Ctrl Pts',(-22.1916978524243,-14.2709014086462,
115.270163302908)) ;
#193995 = CARTESIAN_POINT('Ctrl Pts',(-22.244095479827,-14.0614284920593,
115.465166551261)) ;
#193996 = CARTESIAN_POINT('Ctrl Pts',(-22.2770600984898,-13.8059370930909,
115.601015529285)) ;
#193997 = CARTESIAN_POINT('Ctrl Pts',(-22.2872367367097,-13.5211628984478,
115.667631143365)) ;
#193998 = CARTESIAN_POINT('Ctrl Pts',(-22.2733014770103,-13.2317212421624,
115.660460390471)) ;
#193999 = CARTESIAN_POINT('Ctrl Pts',(-22.2352493339622,-12.953209842425,
115.580148172852)) ;
#194000 = CARTESIAN_POINT('Ctrl Pts',(-22.1754856836276,-12.7094642616823,
115.433485637688)) ;
#194001 = CARTESIAN_POINT('Ctrl Pts',(-22.0966448910796,-12.5150572905195,
115.22901210739)) ;
#194002 = CARTESIAN_POINT('Ctrl Pts',(-22.0054187277231,-12.3871819681861,
114.986327553014)) ;
#194003 = CARTESIAN_POINT('Ctrl Pts',(-21.905263733452,-12.3316884564228,
114.716909806915)) ;
#194004 = CARTESIAN_POINT('Ctrl Pts',(-21.8045903005962,-12.3542922095437,
114.445593550072)) ;
#194005 = CARTESIAN_POINT('Ctrl Pts',(-21.7081146500002,-12.4537268763868,
114.187411168182)) ;
#194006 = CARTESIAN_POINT('Ctrl Pts',(-21.6237862011861,-12.6212675456056,
113.965882774821)) ;
#194007 = CARTESIAN_POINT('Ctrl Pts',(-21.5556046478956,-12.846192059173,
113.793679096726)) ;
#194008 = CARTESIAN_POINT('Ctrl Pts',(-21.5080827888729,-13.1124184461725,
113.684427311798)) ;
#194009 = CARTESIAN_POINT('Ctrl Pts',(-21.483971454148,-13.400879749144,113.646523677771)) ;
#194010 = CARTESIAN_POINT('Ctrl Pts',(-21.4841119720974,-13.6891262166377,
113.682294540054)) ;
#194011 = CARTESIAN_POINT('Ctrl Pts',(-21.5080695511385,-13.9605413879786,
113.790974309993)) ;
#194012 = CARTESIAN_POINT('Ctrl Pts',(-21.5525393505442,-14.1894540736428,
113.961580396736)) ;
#194013 = CARTESIAN_POINT('Ctrl Pts',(-21.6146814088062,-14.3660067048925,
114.186472926776)) ;
#194014 = CARTESIAN_POINT('Ctrl Pts',(-21.6884351663154,-14.4734792612079,
114.446508526122)) ;
#194015 = CARTESIAN_POINT('Ctrl Pts',(-21.7683784809354,-14.5056975632985,
114.725551946228)) ;
#194016 = CARTESIAN_POINT('Ctrl Pts',(-21.8474157178673,-14.4599236721213,
115.001679784935)) ;
#194017 = CARTESIAN_POINT('Ctrl Pts',(-21.9195991566158,-14.3395761921465,
115.257002682461)) ;
#194018 = CARTESIAN_POINT('Ctrl Pts',(-21.9788462429372,-14.1535350418836,
115.472880057577)) ;
#194019 = CARTESIAN_POINT('Ctrl Pts',(-22.0203775008148,-13.9130985111844,
115.635036561647)) ;
#194020 = CARTESIAN_POINT('Ctrl Pts',(-22.0399483640035,-13.6395736822347,
115.72995984664)) ;
#194021 = CARTESIAN_POINT('Ctrl Pts',(-22.0358686869632,-13.3487006076146,
115.75305462755)) ;
#194022 = CARTESIAN_POINT('Ctrl Pts',(-22.0075438310689,-13.0636371844073,
115.70218883906)) ;
#194023 = CARTESIAN_POINT('Ctrl Pts',(-21.9561819767785,-12.803286823163,
115.581244291729)) ;
#194024 = CARTESIAN_POINT('Ctrl Pts',(-21.8847933182746,-12.5872505028287,
115.399264233317)) ;
#194025 = CARTESIAN_POINT('Ctrl Pts',(-21.7976012004924,-12.4304809457012,
115.169196272267)) ;
#194026 = CARTESIAN_POINT('Ctrl Pts',(-21.700169966331,-12.3447676693836,
114.907940821846)) ;
#194027 = CARTESIAN_POINT('Ctrl Pts',(-21.5992738440407,-12.3358385329225,
114.635951321801)) ;
#194028 = CARTESIAN_POINT('Ctrl Pts',(-21.5003785782672,-12.4042599768703,
114.370232214751)) ;
#194029 = CARTESIAN_POINT('Ctrl Pts',(-21.4104042015346,-12.5454038835963,
114.131652978612)) ;
#194030 = CARTESIAN_POINT('Ctrl Pts',(-21.3349456169578,-12.7490645526663,
113.9372922249)) ;
#194031 = CARTESIAN_POINT('Ctrl Pts',(-21.278705237238,-13.0004109945635,
113.801433245637)) ;
#194032 = CARTESIAN_POINT('Ctrl Pts',(-21.2448570719353,-13.281956740539,
113.733818494743)) ;
#194033 = CARTESIAN_POINT('Ctrl Pts',(-21.2351498447256,-13.573019683806,
113.739702682927)) ;
#194034 = CARTESIAN_POINT('Ctrl Pts',(-21.2495046916565,-13.8532505028034,
113.818910957215)) ;
#194035 = CARTESIAN_POINT('Ctrl Pts',(-21.2861585371864,-14.1021597581384,
113.966023254985)) ;
#194036 = CARTESIAN_POINT('Ctrl Pts',(-21.3416525533176,-14.3018608409922,
114.170484973414)) ;
#194037 = CARTESIAN_POINT('Ctrl Pts',(-21.411315277641,-14.4384983198451,
114.418115610093)) ;
#194038 = CARTESIAN_POINT('Ctrl Pts',(-21.4896790967479,-14.5020770602936,
114.692365991293)) ;
#194039 = CARTESIAN_POINT('Ctrl Pts',(-21.5697542529171,-14.48777877411,114.971664919752)) ;
#194040 = CARTESIAN_POINT('Ctrl Pts',(-21.6455150626232,-14.3970097456745,
115.237875186916)) ;
#194041 = CARTESIAN_POINT('Ctrl Pts',(-21.7106846353234,-14.2362612997962,
115.471811422078)) ;
#194042 = CARTESIAN_POINT('Ctrl Pts',(-21.7599663610644,-14.0159101115065,
115.65749922043)) ;
#194043 = CARTESIAN_POINT('Ctrl Pts',(-21.7887254354454,-13.7543350935969,
115.7804395058)) ;
#194044 = CARTESIAN_POINT('Ctrl Pts',(-21.7944517107035,-13.4665595551094,
115.833506874945)) ;
#194045 = CARTESIAN_POINT('Ctrl Pts',(-21.7759076496093,-13.1776643244991,
115.812347038779)) ;
#194046 = CARTESIAN_POINT('Ctrl Pts',(-21.7336480522878,-12.90467088677,115.719119626664)) ;
#194047 = CARTESIAN_POINT('Ctrl Pts',(-21.670032619818,-12.6688603640825,
115.560779753081)) ;
#194048 = CARTESIAN_POINT('Ctrl Pts',(-21.5885287279957,-12.48602188738,115.348081223403)) ;
#194049 = CARTESIAN_POINT('Ctrl Pts',(-21.4945267923872,-12.3704601308902,
115.097266800152)) ;
#194050 = CARTESIAN_POINT('Ctrl Pts',(-21.3942570657881,-12.3301504850153,
114.827261741778)) ;
#194051 = CARTESIAN_POINT('Ctrl Pts',(-21.2939223840727,-12.3670848663884,
114.557023720825)) ;
#194052 = CARTESIAN_POINT('Ctrl Pts',(-21.1989536269659,-12.4806961242678,
114.303499956068)) ;
#194053 = CARTESIAN_POINT('Ctrl Pts',(-21.1174616220678,-12.659847054779,
114.090572179847)) ;
#194054 = CARTESIAN_POINT('Ctrl Pts',(-21.0527943299023,-12.8944266812495,
113.929149642183)) ;
#194055 = CARTESIAN_POINT('Ctrl Pts',(-21.009715412858,-13.1656332510844,
113.833333116255)) ;
#194056 = CARTESIAN_POINT('Ctrl Pts',(-20.9901169836703,-13.455130793988,
113.809077738093)) ;
#194057 = CARTESIAN_POINT('Ctrl Pts',(-20.9948751859287,-13.7427936624919,
113.859110662264)) ;
#194058 = CARTESIAN_POINT('Ctrl Pts',(-21.0227622802631,-14.0059776158613,
113.979433797495)) ;
#194059 = CARTESIAN_POINT('Ctrl Pts',(-21.0711237055155,-14.2279037819529,
114.162216793604)) ;
#194060 = CARTESIAN_POINT('Ctrl Pts',(-21.1359737665809,-14.3919406672911,
114.39531754647)) ;
#194061 = CARTESIAN_POINT('Ctrl Pts',(-21.211254131552,-14.4855253459423,
114.659978503316)) ;
#194062 = CARTESIAN_POINT('Ctrl Pts',(-21.2915339470349,-14.5029122651219,
114.940022641269)) ;
#194063 = CARTESIAN_POINT('Ctrl Pts',(-21.3695938610987,-14.4429567945224,
115.213104290298)) ;
#194064 = CARTESIAN_POINT('Ctrl Pts',(-21.4400444498509,-14.3088313127917,
115.463288416723)) ;
#194065 = CARTESIAN_POINT('Ctrl Pts',(-21.4961500025639,-14.1118280044828,
115.669548634659)) ;
#194066 = CARTESIAN_POINT('Ctrl Pts',(-21.5338004050003,-13.8633524569287,
115.819871913818)) ;
#194067 = CARTESIAN_POINT('Ctrl Pts',(-21.5489972331909,-13.5856086171591,
115.901434129162)) ;
#194068 = CARTESIAN_POINT('Ctrl Pts',(-21.540363783719,-13.29429050433,115.910632149051)) ;
#194069 = CARTESIAN_POINT('Ctrl Pts',(-21.5075688559681,-13.0122145331766,
115.846182232389)) ;
#194070 = CARTESIAN_POINT('Ctrl Pts',(-21.4520578760768,-12.7583429519339,
115.712662082996)) ;
#194071 = CARTESIAN_POINT('Ctrl Pts',(-21.377127791228,-12.5522896132778,
115.51996437081)) ;
#194072 = CARTESIAN_POINT('Ctrl Pts',(-21.2880636112646,-12.4090180636989,
115.283992249369)) ;
#194073 = CARTESIAN_POINT('Ctrl Pts',(-21.1893528871873,-12.3371174607651,
115.018865437518)) ;
#194074 = CARTESIAN_POINT('Ctrl Pts',(-21.0881345102603,-12.3428658905722,
114.745994676073)) ;
#194075 = CARTESIAN_POINT('Ctrl Pts',(-20.9904482281693,-12.4257351119528,
114.483961462618)) ;
#194076 = CARTESIAN_POINT('Ctrl Pts',(-20.9030223342738,-12.5790185234623,
114.253042471409)) ;
#194077 = CARTESIAN_POINT('Ctrl Pts',(-20.8305192061514,-12.7940406828703,
114.067860324909)) ;
#194078 = CARTESIAN_POINT('Ctrl Pts',(-20.7785061884323,-13.0518842131347,
113.944776920917)) ;
#194079 = CARTESIAN_POINT('Ctrl Pts',(-20.74911735469,-13.3370763555055,113.890776267983)) ;
#194080 = CARTESIAN_POINT('Ctrl Pts',(-20.7440079729999,-13.6270297095458,
113.910587476447)) ;
#194081 = CARTESIAN_POINT('Ctrl Pts',(-20.7628136407268,-13.9038567932623,
114.003478096107)) ;
#194082 = CARTESIAN_POINT('Ctrl Pts',(-20.8034569028155,-14.1447030861545,
114.162759758855)) ;
#194083 = CARTESIAN_POINT('Ctrl Pts',(-20.8618372427062,-14.332817774621,
114.375897727997)) ;
#194084 = CARTESIAN_POINT('Ctrl Pts',(-20.9337388829321,-14.45646682902,114.630435787986)) ;
#194085 = CARTESIAN_POINT('Ctrl Pts',(-21.0127215247643,-14.5053560860543,
114.906444434635)) ;
#194086 = CARTESIAN_POINT('Ctrl Pts',(-21.0928080257603,-14.4762759602464,
115.185935827809)) ;
#194087 = CARTESIAN_POINT('Ctrl Pts',(-21.166945453464,-14.3712943997113,
115.44718234613)) ;
#194088 = CARTESIAN_POINT('Ctrl Pts',(-21.22925533612,-14.1990455522355,115.672287786187)) ;
#194089 = CARTESIAN_POINT('Ctrl Pts',(-21.275036309889,-13.969268231171,115.847326008971)) ;
#194090 = CARTESIAN_POINT('Ctrl Pts',(-21.2996282826531,-13.7012052922517,
115.957629225369)) ;
#194091 = CARTESIAN_POINT('Ctrl Pts',(-21.300776790549,-13.4115854195081,
115.996699140416)) ;
#194092 = CARTESIAN_POINT('Ctrl Pts',(-21.2776657782434,-13.1240520278943,
115.961667884177)) ;
#194093 = CARTESIAN_POINT('Ctrl Pts',(-21.2310997495999,-12.8565945311091,
115.85532524094)) ;
#194094 = CARTESIAN_POINT('Ctrl Pts',(-21.1639038965067,-12.6299321000607,
115.686042104693)) ;
#194095 = CARTESIAN_POINT('Ctrl Pts',(-21.0795308737286,-12.458754218581,
115.464633703423)) ;
#194096 = CARTESIAN_POINT('Ctrl Pts',(-20.9840008114821,-12.3569969390507,
115.209096703892)) ;
#194097 = CARTESIAN_POINT('Ctrl Pts',(-20.8827940549326,-12.3311725454961,
114.936383442419)) ;
#194098 = CARTESIAN_POINT('Ctrl Pts',(-20.7831194155453,-12.3830921654557,
114.668177530527)) ;
#194099 = CARTESIAN_POINT('Ctrl Pts',(-20.6905057252182,-12.5097082549453,
114.421659452315)) ;
#194100 = CARTESIAN_POINT('Ctrl Pts',(-20.611889484645,-12.6999655173835,
114.217488910924)) ;
#194101 = CARTESIAN_POINT('Ctrl Pts',(-20.5509672408573,-12.9431519741363,
114.067493771152)) ;
#194102 = CARTESIAN_POINT('Ctrl Pts',(-20.5121852559406,-13.2187420743147,
113.984700488241)) ;
#194103 = CARTESIAN_POINT('Ctrl Pts',(-20.4971344280026,-13.5111774969548,
113.974526122815)) ;
#194104 = CARTESIAN_POINT('Ctrl Pts',(-20.5063387268511,-13.7940494918521,
114.037849430853)) ;
#194105 = CARTESIAN_POINT('Ctrl Pts',(-20.5386101711866,-14.0529110285333,
114.171842551174)) ;
#194106 = CARTESIAN_POINT('Ctrl Pts',(-20.5902344604345,-14.2634870650102,
114.364365229605)) ;
#194107 = CARTESIAN_POINT('Ctrl Pts',(-20.6572920468694,-14.4148461022599,
114.60407461122)) ;
#194108 = CARTESIAN_POINT('Ctrl Pts',(-20.7340710302273,-14.494780073978,
114.873368689738)) ;
#194109 = CARTESIAN_POINT('Ctrl Pts',(-20.814667921946,-14.4974507314962,
115.154444310866)) ;
#194110 = CARTESIAN_POINT('Ctrl Pts',(-20.8916746371351,-14.4229495346006,
115.424337435555)) ;
#194111 = CARTESIAN_POINT('Ctrl Pts',(-20.9596595247132,-14.2768020033666,
115.6668461103)) ;
#194112 = CARTESIAN_POINT('Ctrl Pts',(-21.012974127338,-14.0672719747909,
115.864923528027)) ;
#194113 = CARTESIAN_POINT('Ctrl Pts',(-21.0462752479574,-13.8140437794069,
116.001605423442)) ;
#194114 = CARTESIAN_POINT('Ctrl Pts',(-21.057235818105,-13.5305545368903,
116.070529359299)) ;
#194115 = CARTESIAN_POINT('Ctrl Pts',(-21.0439982208835,-13.2400469135056,
116.065602507524)) ;
#194116 = CARTESIAN_POINT('Ctrl Pts',(-21.0066020047252,-12.9607801917685,
115.987295334548)) ;
#194117 = CARTESIAN_POINT('Ctrl Pts',(-20.9473443980316,-12.7157522020321,
115.842202222821)) ;
#194118 = CARTESIAN_POINT('Ctrl Pts',(-20.8694399766873,-12.5205021117526,
115.640390114338)) ;
#194119 = CARTESIAN_POINT('Ctrl Pts',(-20.7779765651367,-12.3896091910669,
115.397208988666)) ;
#194120 = CARTESIAN_POINT('Ctrl Pts',(-20.6779561212234,-12.3322116649338,
115.128190401515)) ;
#194121 = CARTESIAN_POINT('Ctrl Pts',(-20.5774147689211,-12.3526193896652,
114.857217210318)) ;
#194122 = CARTESIAN_POINT('Ctrl Pts',(-20.480876963674,-12.4495335034968,
114.598771665885)) ;
#194123 = CARTESIAN_POINT('Ctrl Pts',(-20.3957540886572,-12.6159519111974,
114.374983031782)) ;
#194124 = CARTESIAN_POINT('Ctrl Pts',(-20.3271536623197,-12.8395609374739,
114.201485817632)) ;
#194125 = CARTESIAN_POINT('Ctrl Pts',(-20.2791583118047,-13.1036924153161,
114.090643871318)) ;
#194126 = CARTESIAN_POINT('Ctrl Pts',(-20.2542197759365,-13.3927905140901,
114.05034234162)) ;
#194127 = CARTESIAN_POINT('Ctrl Pts',(-20.2537651631048,-13.6807940128297,
114.084250210379)) ;
#194128 = CARTESIAN_POINT('Ctrl Pts',(-20.2767369580529,-13.9516407801447,
114.189702183706)) ;
#194129 = CARTESIAN_POINT('Ctrl Pts',(-20.3212515827195,-14.1848191645832,
114.360909549778)) ;
#194130 = CARTESIAN_POINT('Ctrl Pts',(-20.3823727653949,-14.3611535147467,
114.582313485388)) ;
#194131 = CARTESIAN_POINT('Ctrl Pts',(-20.4563210601665,-14.4717132500286,
114.843190270097)) ;
#194132 = CARTESIAN_POINT('Ctrl Pts',(-20.5359913410577,-14.5058049610956,
115.121300978399)) ;
#194133 = CARTESIAN_POINT('Ctrl Pts',(-20.6152285993297,-14.4622432474708,
115.398086166475)) ;
#194134 = CARTESIAN_POINT('Ctrl Pts',(-20.6876764922037,-14.343914063795,
115.654200032397)) ;
#194135 = CARTESIAN_POINT('Ctrl Pts',(-20.7473748229597,-14.1592285094383,
115.871492526232)) ;
#194136 = CARTESIAN_POINT('Ctrl Pts',(-20.7892502687807,-13.9218383285055,
116.034450676081)) ;
#194137 = CARTESIAN_POINT('Ctrl Pts',(-20.8096697160064,-13.6477929587425,
116.132141353103)) ;
#194138 = CARTESIAN_POINT('Ctrl Pts',(-20.8062757150026,-13.3573882946602,
116.157281504951)) ;
#194139 = CARTESIAN_POINT('Ctrl Pts',(-20.7786075112858,-13.0713760146383,
116.108481462324)) ;
#194140 = CARTESIAN_POINT('Ctrl Pts',(-20.727862298227,-12.8101300373193,
115.989403245096)) ;
#194141 = CARTESIAN_POINT('Ctrl Pts',(-20.6569850715304,-12.5926203368979,
115.808983189136)) ;
#194142 = CARTESIAN_POINT('Ctrl Pts',(-20.5702654370651,-12.4341144288436,
115.580315447972)) ;
#194143 = CARTESIAN_POINT('Ctrl Pts',(-20.4730652679923,-12.346259851331,
115.319760267267)) ;
#194144 = CARTESIAN_POINT('Ctrl Pts',(-20.372232841033,-12.3348158852733,
115.047945482228)) ;
#194145 = CARTESIAN_POINT('Ctrl Pts',(-20.272459099619,-12.4019396871859,
114.779822675992)) ;
#194146 = CARTESIAN_POINT('Ctrl Pts',(-20.1830070427554,-12.5400212389952,
114.542504031555)) ;
#194147 = CARTESIAN_POINT('Ctrl Pts',(-20.1067029971044,-12.7426569389483,
114.345713360105)) ;
#194148 = CARTESIAN_POINT('Ctrl Pts',(-20.0499392060894,-12.9928209893326,
114.208234860581)) ;
#194149 = CARTESIAN_POINT('Ctrl Pts',(-20.0153853295519,-13.274121349933,
114.138514811439)) ;
#194150 = CARTESIAN_POINT('Ctrl Pts',(-20.0050410507883,-13.5650423075934,
114.142439305779)) ;
#194151 = CARTESIAN_POINT('Ctrl Pts',(-20.0186971571549,-13.8454220244642,
114.219462038445)) ;
#194152 = CARTESIAN_POINT('Ctrl Pts',(-20.0547596385372,-14.095635489283,
114.36479225159)) ;
#194153 = CARTESIAN_POINT('Ctrl Pts',(-20.1097879472539,-14.2970558104585,
114.56784725279)) ;
#194154 = CARTESIAN_POINT('Ctrl Pts',(-20.1793472667708,-14.4359480747077,
114.815266815336)) ;
#194155 = CARTESIAN_POINT('Ctrl Pts',(-20.2575026754292,-14.501304829004,
115.088848135438)) ;
#194156 = CARTESIAN_POINT('Ctrl Pts',(-20.3373604074522,-14.4893139259723,
115.367374582084)) ;
#194157 = CARTESIAN_POINT('Ctrl Pts',(-20.4135150495728,-14.4004454436412,
115.63486985746)) ;
#194158 = CARTESIAN_POINT('Ctrl Pts',(-20.4788768821726,-14.2418718140722,
115.86930035727)) ;
#194159 = CARTESIAN_POINT('Ctrl Pts',(-20.5287019786929,-14.0233785235775,
116.056610441429)) ;
#194160 = CARTESIAN_POINT('Ctrl Pts',(-20.5581714230433,-13.7618917263419,
116.181832379666)) ;
#194161 = CARTESIAN_POINT('Ctrl Pts',(-20.5645519553757,-13.4754623735639,
116.236774706755)) ;
#194162 = CARTESIAN_POINT('Ctrl Pts',(-20.5467688213249,-13.1862230579374,
116.217949995558)) ;
#194163 = CARTESIAN_POINT('Ctrl Pts',(-20.5051147908571,-12.9121173454345,
116.12661145186)) ;
#194164 = CARTESIAN_POINT('Ctrl Pts',(-20.4420769531017,-12.6748571224349,
115.970037261179)) ;
#194165 = CARTESIAN_POINT('Ctrl Pts',(-20.3606399883835,-12.4898752939566,
115.757680794649)) ;
#194166 = CARTESIAN_POINT('Ctrl Pts',(-20.267669228754,-12.3730682967797,
115.5097223699)) ;
#194167 = CARTESIAN_POINT('Ctrl Pts',(-20.166688706548,-12.330125354393,115.237846370994)) ;
#194168 = CARTESIAN_POINT('Ctrl Pts',(-20.0667473533349,-12.3650026478225,
114.968634787347)) ;
#194169 = CARTESIAN_POINT('Ctrl Pts',(-19.9714448335891,-12.4764750890778,
114.714120708034)) ;
#194170 = CARTESIAN_POINT('Ctrl Pts',(-19.8896127307638,-12.6535586984017,
114.500104289073)) ;
#194171 = CARTESIAN_POINT('Ctrl Pts',(-19.8242138693162,-12.8875907025722,
114.33656955619)) ;
#194172 = CARTESIAN_POINT('Ctrl Pts',(-19.7806786916706,-13.1564738506933,
114.239166113218)) ;
#194173 = CARTESIAN_POINT('Ctrl Pts',(-19.7602296026469,-13.4476180482474,
114.212556713675)) ;
#194174 = CARTESIAN_POINT('Ctrl Pts',(-19.7643490688689,-13.7346448783816,
114.260518004658)) ;
#194175 = CARTESIAN_POINT('Ctrl Pts',(-19.7916546783398,-13.9993799399049,
114.37915348673)) ;
#194176 = CARTESIAN_POINT('Ctrl Pts',(-19.8393939276307,-14.2219559568416,
114.559939768172)) ;
#194177 = CARTESIAN_POINT('Ctrl Pts',(-19.9035549276073,-14.3877271051732,
114.790823935463)) ;
#194178 = CARTESIAN_POINT('Ctrl Pts',(-19.9791956729631,-14.4840522417127,
115.05686055136)) ;
#194179 = CARTESIAN_POINT('Ctrl Pts',(-20.0588167420593,-14.5035551456864,
115.334617178698)) ;
#194180 = CARTESIAN_POINT('Ctrl Pts',(-20.1375552337769,-14.4455933724693,
115.610012047624)) ;
#194181 = CARTESIAN_POINT('Ctrl Pts',(-20.2080701569904,-14.3137077173971,
115.860269168483)) ;
#194182 = CARTESIAN_POINT('Ctrl Pts',(-20.2646911851614,-14.118290994482,
116.068126903514)) ;
#194183 = CARTESIAN_POINT('Ctrl Pts',(-20.3028224443455,-13.8721339097932,
116.21976440383)) ;
#194184 = CARTESIAN_POINT('Ctrl Pts',(-20.3188675383437,-13.5943341067766,
116.304015063102)) ;
#194185 = CARTESIAN_POINT('Ctrl Pts',(-20.310817084727,-13.3016132059809,
116.315163697483)) ;
#194186 = CARTESIAN_POINT('Ctrl Pts',(-20.2787910861107,-13.0203974601351,
116.252886906067)) ;
#194187 = CARTESIAN_POINT('Ctrl Pts',(-20.2240804356435,-12.7657619407627,
116.121738912419)) ;
#194188 = CARTESIAN_POINT('Ctrl Pts',(-20.149613612166,-12.5577255499837,
115.930492489718)) ;
#194189 = CARTESIAN_POINT('Ctrl Pts',(-20.0607208453583,-12.4120606642955,
115.695117936638)) ;
#194190 = CARTESIAN_POINT('Ctrl Pts',(-19.9618159399851,-12.3380220880362,
115.429525652929)) ;
#194191 = CARTESIAN_POINT('Ctrl Pts',(-19.8611741252131,-12.3416277493325,
115.158205582033)) ;
#194192 = CARTESIAN_POINT('Ctrl Pts',(-19.7631652821149,-12.4221117178776,
114.895226151352)) ;
#194193 = CARTESIAN_POINT('Ctrl Pts',(-19.6752313663645,-12.5739000669618,
114.662827645649)) ;
#194194 = CARTESIAN_POINT('Ctrl Pts',(-19.6024167491396,-12.7865530350162,
114.47657434342)) ;
#194195 = CARTESIAN_POINT('Ctrl Pts',(-19.5495231103684,-13.044698151263,
114.350994766483)) ;
#194196 = CARTESIAN_POINT('Ctrl Pts',(-19.5196225512715,-13.328059924083,
114.29525984895)) ;
#194197 = CARTESIAN_POINT('Ctrl Pts',(-19.5137354281578,-13.6187777866059,
114.312782448992)) ;
#194198 = CARTESIAN_POINT('Ctrl Pts',(-19.5318785681101,-13.8959727795492,
114.403613733301)) ;
#194199 = CARTESIAN_POINT('Ctrl Pts',(-19.5718247752165,-14.1380897314584,
114.560743510385)) ;
#194200 = CARTESIAN_POINT('Ctrl Pts',(-19.6301836363791,-14.3289912800735,
114.774053959867)) ;
#194201 = CARTESIAN_POINT('Ctrl Pts',(-19.7013725695596,-14.4536834307714,
115.026197380429)) ;
#194202 = CARTESIAN_POINT('Ctrl Pts',(-19.7802758537962,-14.5050447602448,
115.301993496295)) ;
#194203 = CARTESIAN_POINT('Ctrl Pts',(-19.8602648502565,-14.4782940097224,
115.581115798134)) ;
#194204 = CARTESIAN_POINT('Ctrl Pts',(-19.9347147614836,-14.3758709565101,
115.843310818207)) ;
#194205 = CARTESIAN_POINT('Ctrl Pts',(-19.9978520690189,-14.2038414128419,
116.071213910054)) ;
#194206 = CARTESIAN_POINT('Ctrl Pts',(-20.0437608055394,-13.9777022974474,
116.246290431743)) ;
#194207 = CARTESIAN_POINT('Ctrl Pts',(-20.0692545667737,-13.7081471730545,
116.359670607939)) ;
#194208 = CARTESIAN_POINT('Ctrl Pts',(-20.0710088126816,-13.4207218926891,
116.400338260626)) ;
#194209 = CARTESIAN_POINT('Ctrl Pts',(-20.0486389329938,-13.1323473586493,
116.367635760185)) ;
#194210 = CARTESIAN_POINT('Ctrl Pts',(-20.0027585392029,-12.8640039527127,
116.26336619867)) ;
#194211 = CARTESIAN_POINT('Ctrl Pts',(-19.935788026807,-12.6351955964259,
116.094916391057)) ;
#194212 = CARTESIAN_POINT('Ctrl Pts',(-19.8524350019228,-12.4633049543151,
115.876360547653)) ;
#194213 = CARTESIAN_POINT('Ctrl Pts',(-19.7565552164464,-12.3586842738095,
115.619991906947)) ;
#194214 = CARTESIAN_POINT('Ctrl Pts',(-19.6559368636795,-12.3308701665295,
115.348879090383)) ;
#194215 = CARTESIAN_POINT('Ctrl Pts',(-19.5559630364021,-12.3804185210795,
115.079826490949)) ;
#194216 = CARTESIAN_POINT('Ctrl Pts',(-19.4632285523152,-12.5045865657479,
114.832858816864)) ;
#194217 = CARTESIAN_POINT('Ctrl Pts',(-19.3838405577288,-12.6936012415773,
114.626458033077)) ;
#194218 = CARTESIAN_POINT('Ctrl Pts',(-19.3222105618298,-12.9362801376937,
114.474398641739)) ;
#194219 = CARTESIAN_POINT('Ctrl Pts',(-19.2828604657008,-13.2112926431605,
114.389881775346)) ;
#194220 = CARTESIAN_POINT('Ctrl Pts',(-19.2671542279157,-13.5026318637497,
114.377588421652)) ;
#194221 = CARTESIAN_POINT('Ctrl Pts',(-19.2757419733594,-13.7865927515763,
114.439120363259)) ;
#194222 = CARTESIAN_POINT('Ctrl Pts',(-19.3070927419327,-14.0445932154009,
114.570030945766)) ;
#194223 = CARTESIAN_POINT('Ctrl Pts',(-19.358347515694,-14.2581092551482,
114.761608730446)) ;
#194224 = CARTESIAN_POINT('Ctrl Pts',(-19.4252783091883,-14.4117380229187,
115.001038317045)) ;
#194225 = CARTESIAN_POINT('Ctrl Pts',(-19.5019526631148,-14.4936441507055,
115.270046158408)) ;
#194226 = CARTESIAN_POINT('Ctrl Pts',(-19.5823198515389,-14.4983888239063,
115.550327419762)) ;
#194227 = CARTESIAN_POINT('Ctrl Pts',(-19.6595477418913,-14.426207251784,
115.82090191206)) ;
#194228 = CARTESIAN_POINT('Ctrl Pts',(-19.7280764038109,-14.2809809264381,
116.065217208955)) ;
#194229 = CARTESIAN_POINT('Ctrl Pts',(-19.7813206021368,-14.0755731076895,
116.262663449883)) ;
#194230 = CARTESIAN_POINT('Ctrl Pts',(-19.8156285654698,-13.8214647968314,
116.402723704513)) ;
#194231 = CARTESIAN_POINT('Ctrl Pts',(-19.8271835709341,-13.5390721929965,
116.473371097639)) ;
#194232 = CARTESIAN_POINT('Ctrl Pts',(-19.8146134378266,-13.2479213210197,
116.470556422711)) ;
#194233 = CARTESIAN_POINT('Ctrl Pts',(-19.7780274303114,-12.9689956696526,
116.394584966036)) ;
#194234 = CARTESIAN_POINT('Ctrl Pts',(-19.7192534733058,-12.7220961737177,
116.251055118297)) ;
#194235 = CARTESIAN_POINT('Ctrl Pts',(-19.6419060205883,-12.5254520180373,
116.050893527524)) ;
#194236 = CARTESIAN_POINT('Ctrl Pts',(-19.5507750838464,-12.3924871288094,
115.808727229059)) ;
#194237 = CARTESIAN_POINT('Ctrl Pts',(-19.4509678272437,-12.3327720085306,
115.540332649395)) ;
#194238 = CARTESIAN_POINT('Ctrl Pts',(-19.3501879158993,-12.3509988977752,
115.268703339782)) ;
#194239 = CARTESIAN_POINT('Ctrl Pts',(-19.2537109950385,-12.4453838611795,
115.010328377215)) ;
#194240 = CARTESIAN_POINT('Ctrl Pts',(-19.1680396764701,-12.6100760699984,
114.78492817834)) ;
#194241 = CARTESIAN_POINT('Ctrl Pts',(-19.0989285208918,-12.8316470477012,
114.609808039742)) ;
#194242 = CARTESIAN_POINT('Ctrl Pts',(-19.0499531759888,-13.0973555362981,
114.496308559562)) ;
#194243 = CARTESIAN_POINT('Ctrl Pts',(-19.0246223482772,-13.3829827267331,
114.454418834067)) ;
#194244 = CARTESIAN_POINT('Ctrl Pts',(-19.0233599186535,-13.6735145155205,
114.486149491012)) ;
#194245 = CARTESIAN_POINT('Ctrl Pts',(-19.0457709783456,-13.9443960540442,
114.589809022558)) ;
#194246 = CARTESIAN_POINT('Ctrl Pts',(-19.0894428117511,-14.1780473237906,
114.75829138369)) ;
#194247 = CARTESIAN_POINT('Ctrl Pts',(-19.1503829732197,-14.3571729772058,
114.97930953691)) ;
#194248 = CARTESIAN_POINT('Ctrl Pts',(-19.2242001392869,-14.4697035049953,
115.239834214336)) ;
#194249 = CARTESIAN_POINT('Ctrl Pts',(-19.3035102564175,-14.5058316151569,
115.516726782394)) ;
#194250 = CARTESIAN_POINT('Ctrl Pts',(-19.3827642308923,-14.4647781183691,
115.793520482864)) ;
#194251 = CARTESIAN_POINT('Ctrl Pts',(-19.4555982839664,-14.3484987257117,
116.050853216229)) ;
#194252 = CARTESIAN_POINT('Ctrl Pts',(-19.5158156777424,-14.1655053892491,
116.26975198964)) ;
#194253 = CARTESIAN_POINT('Ctrl Pts',(-19.5583308176863,-13.9286208259661,
116.434763630565)) ;
#194254 = CARTESIAN_POINT('Ctrl Pts',(-19.5793222342617,-13.6565946963034,
116.5340328038)) ;
#194255 = CARTESIAN_POINT('Ctrl Pts',(-19.5766443908906,-13.3650274692435,
116.561521687916)) ;
#194256 = CARTESIAN_POINT('Ctrl Pts',(-19.5495669925005,-13.0788343995772,
116.514498473725)) ;
#194257 = CARTESIAN_POINT('Ctrl Pts',(-19.4996422792964,-12.8175211583994,
116.397794021949)) ;
#194258 = CARTESIAN_POINT('Ctrl Pts',(-19.4293404722098,-12.5984995679009,
116.219119607498)) ;
#194259 = CARTESIAN_POINT('Ctrl Pts',(-19.3431976343271,-12.4381081950322,
115.992149215875)) ;
#194260 = CARTESIAN_POINT('Ctrl Pts',(-19.2456411710222,-12.3474840033873,
115.730719198245)) ;
#194261 = CARTESIAN_POINT('Ctrl Pts',(-19.1449743145035,-12.3342746176406,
115.45936107608)) ;
#194262 = CARTESIAN_POINT('Ctrl Pts',(-19.0456937210243,-12.3983523506611,
115.192496748361)) ;
#194263 = CARTESIAN_POINT('Ctrl Pts',(-18.9551049831602,-12.5353914606374,
114.952015661837)) ;
#194264 = CARTESIAN_POINT('Ctrl Pts',(-18.8783820413473,-12.7368848040207,
114.753966045534)) ;
#194265 = CARTESIAN_POINT('Ctrl Pts',(-18.8212505018881,-12.9849643669818,
114.615234103962)) ;
#194266 = CARTESIAN_POINT('Ctrl Pts',(-18.785989087223,-13.2657001242146,
114.543367393447)) ;
#194267 = CARTESIAN_POINT('Ctrl Pts',(-18.7749409518522,-13.5562446654925,
114.545103589634)) ;
#194268 = CARTESIAN_POINT('Ctrl Pts',(-18.7878772786409,-13.837740260252,
114.619989429758)) ;
#194269 = CARTESIAN_POINT('Ctrl Pts',(-18.823586104698,-14.0900089023239,
114.76439949876)) ;
#194270 = CARTESIAN_POINT('Ctrl Pts',(-18.8778061466655,-14.2916996646196,
114.964766086765)) ;
#194271 = CARTESIAN_POINT('Ctrl Pts',(-18.9472129540579,-14.4330905333239,
115.211832429368)) ;
#194272 = CARTESIAN_POINT('Ctrl Pts',(-19.0250383188823,-14.5004556458798,
115.484322413278)) ;
#194273 = CARTESIAN_POINT('Ctrl Pts',(-19.1050415480743,-14.4906784452632,
115.763353035226)) ;
#194274 = CARTESIAN_POINT('Ctrl Pts',(-19.1811866606781,-14.4044504861589,
116.030699387926)) ;
#194275 = CARTESIAN_POINT('Ctrl Pts',(-19.2474615033651,-14.2464177648016,
116.26820558113)) ;
#194276 = CARTESIAN_POINT('Ctrl Pts',(-19.2975522404832,-14.0296079395376,
116.456228657709)) ;
#194277 = CARTESIAN_POINT('Ctrl Pts',(-19.3275320163761,-13.7700542634679,
116.582883427607)) ;
#194278 = CARTESIAN_POINT('Ctrl Pts',(-19.3346750163065,-13.4844393542531,
116.640102123225)) ;
#194279 = CARTESIAN_POINT('Ctrl Pts',(-19.3174944725961,-13.1938467066394,
116.623262581033)) ;
#194280 = CARTESIAN_POINT('Ctrl Pts',(-19.2765712704978,-12.9193998282655,
116.534084192877)) ;
#194281 = CARTESIAN_POINT('Ctrl Pts',(-19.2136556163805,-12.679977460876,
116.378071311553)) ;
#194282 = CARTESIAN_POINT('Ctrl Pts',(-19.1338523199838,-12.4956043021029,
116.170183536347)) ;
#194283 = CARTESIAN_POINT('Ctrl Pts',(-19.0401108727425,-12.3751190535725,
115.920306886088)) ;
#194284 = CARTESIAN_POINT('Ctrl Pts',(-18.9401330390511,-12.3303020351126,
115.651151126256)) ;
#194285 = CARTESIAN_POINT('Ctrl Pts',(-18.839178326217,-12.3631774170788,
115.379196252521)) ;
#194286 = CARTESIAN_POINT('Ctrl Pts',(-18.7446035699514,-12.4713342743348,
115.126509818248)) ;
#194287 = CARTESIAN_POINT('Ctrl Pts',(-18.6616637495359,-12.6476404276989,
114.909396069518)) ;
#194288 = CARTESIAN_POINT('Ctrl Pts',(-18.5959843317389,-12.8790215196565,
114.744812606196)) ;
#194289 = CARTESIAN_POINT('Ctrl Pts',(-18.5513499003185,-13.1499133657009,
114.644442101082)) ;
#194290 = CARTESIAN_POINT('Ctrl Pts',(-18.5304611078023,-13.4386144880716,
114.616209853643)) ;
#194291 = CARTESIAN_POINT('Ctrl Pts',(-18.5338401235194,-13.7268235527867,
114.662025079469)) ;
#194292 = CARTESIAN_POINT('Ctrl Pts',(-18.5603928248668,-13.9914324144424,
114.778219545102)) ;
#194293 = CARTESIAN_POINT('Ctrl Pts',(-18.6076829202727,-14.2164140691066,
114.957760632545)) ;
#194294 = CARTESIAN_POINT('Ctrl Pts',(-18.6716131600408,-14.384032579335,
115.188003285153)) ;
#194295 = CARTESIAN_POINT('Ctrl Pts',(-18.7465062676533,-14.4820529544929,
115.451530561366)) ;
#194296 = CARTESIAN_POINT('Ctrl Pts',(-18.8266090365466,-14.5042250600488,
115.730991693486)) ;
#194297 = CARTESIAN_POINT('Ctrl Pts',(-18.9055245763069,-14.4479097103847,
116.006958567327)) ;
#194298 = CARTESIAN_POINT('Ctrl Pts',(-18.9759850270256,-14.3189148106109,
116.25684843315)) ;
#194299 = CARTESIAN_POINT('Ctrl Pts',(-19.0333811299086,-14.1239822238445,
116.467278862587)) ;
#194300 = CARTESIAN_POINT('Ctrl Pts',(-19.0719097483262,-13.8804446676162,
116.619916310961)) ;
#194301 = CARTESIAN_POINT('Ctrl Pts',(-19.088702598421,-13.6007259227713,
116.70677615132)) ;
#194302 = CARTESIAN_POINT('Ctrl Pts',(-19.0813475062609,-13.310886389785,
116.719690814776)) ;
#194303 = CARTESIAN_POINT('Ctrl Pts',(-19.0499358228212,-13.0275729196668,
116.659478806876)) ;
#194304 = CARTESIAN_POINT('Ctrl Pts',(-18.9956010454947,-12.7715214711428,
116.529545008738)) ;
#194305 = CARTESIAN_POINT('Ctrl Pts',(-18.9217241255641,-12.5625540682405,
116.340023816642)) ;
#194306 = CARTESIAN_POINT('Ctrl Pts',(-18.8334781141802,-12.4155360311479,
116.106499613622)) ;
#194307 = CARTESIAN_POINT('Ctrl Pts',(-18.7350882955953,-12.339199302571,
115.842366036142)) ;
#194308 = CARTESIAN_POINT('Ctrl Pts',(-18.6339421925997,-12.3403409953756,
115.569683136395)) ;
#194309 = CARTESIAN_POINT('Ctrl Pts',(-18.5356154875398,-12.4190382667156,
115.305787998287)) ;
#194310 = CARTESIAN_POINT('Ctrl Pts',(-18.4475845571782,-12.5685297170459,
115.072992627023)) ;
#194311 = CARTESIAN_POINT('Ctrl Pts',(-18.3743096061269,-12.7793086778933,
114.885300417553)) ;
#194312 = CARTESIAN_POINT('Ctrl Pts',(-18.3207591758651,-13.0361487300971,
114.757699953502)) ;
#194313 = CARTESIAN_POINT('Ctrl Pts',(-18.2900556295031,-13.3199156358865,
114.699632332883)) ;
#194314 = CARTESIAN_POINT('Ctrl Pts',(-18.2835244771423,-13.61053350134,114.715169773089)) ;
#194315 = CARTESIAN_POINT('Ctrl Pts',(-18.300904682681,-13.8877845324202,
114.80358738621)) ;
#194316 = CARTESIAN_POINT('Ctrl Pts',(-18.3402955625269,-14.1315208949384,
114.95907694666)) ;
#194317 = CARTESIAN_POINT('Ctrl Pts',(-18.3979499293583,-14.3236676354294,
115.170121270634)) ;
#194318 = CARTESIAN_POINT('Ctrl Pts',(-18.4691141873596,-14.451213086268,
115.422348614941)) ;
#194319 = CARTESIAN_POINT('Ctrl Pts',(-18.5480547946809,-14.5046478984509,
115.698323016836)) ;
#194320 = CARTESIAN_POINT('Ctrl Pts',(-18.6278722273307,-14.4801334339684,
115.976822091214)) ;
#194321 = CARTESIAN_POINT('Ctrl Pts',(-18.7025035045635,-14.3800974324411,
116.239533090197)) ;
#194322 = CARTESIAN_POINT('Ctrl Pts',(-18.7661852178501,-14.2097836883392,
116.469145099282)) ;
#194323 = CARTESIAN_POINT('Ctrl Pts',(-18.8126736298305,-13.9844447661634,
116.646062755378)) ;
#194324 = CARTESIAN_POINT('Ctrl Pts',(-18.8387106000838,-13.7175338810347,
116.760872830317)) ;
#194325 = CARTESIAN_POINT('Ctrl Pts',(-18.8412499966495,-13.4290941380284,
116.804105500737)) ;
#194326 = CARTESIAN_POINT('Ctrl Pts',(-18.8195971871137,-13.1407025280343,
116.773545460015)) ;
#194327 = CARTESIAN_POINT('Ctrl Pts',(-18.7741929648226,-12.8707969653127,
116.670833856634)) ;
#194328 = CARTESIAN_POINT('Ctrl Pts',(-18.7081893525992,-12.6417711077458,
116.505122794438)) ;
#194329 = CARTESIAN_POINT('Ctrl Pts',(-18.624745958435,-12.4670674817275,
116.286513958254)) ;
#194330 = CARTESIAN_POINT('Ctrl Pts',(-18.5299237726579,-12.3610581795072,
116.033065517688)) ;
#194331 = CARTESIAN_POINT('Ctrl Pts',(-18.4285423943449,-12.3304705905987,
115.759931665259)) ;
#194332 = CARTESIAN_POINT('Ctrl Pts',(-18.3286734717406,-12.3780041179342,
115.491117750201)) ;
#194333 = CARTESIAN_POINT('Ctrl Pts',(-18.2355472337233,-12.5002675543906,
115.242998586149)) ;
#194334 = CARTESIAN_POINT('Ctrl Pts',(-18.1559065411703,-12.6872113223539,
115.03574587489)) ;
#194335 = CARTESIAN_POINT('Ctrl Pts',(-18.0936528156396,-12.928470822573,
114.881781285062)) ;
#194336 = CARTESIAN_POINT('Ctrl Pts',(-18.053566961881,-13.2034657060163,
114.795110966265)) ;
#194337 = CARTESIAN_POINT('Ctrl Pts',(-18.0372153758526,-13.4939400108665,
114.780761585915)) ;
#194338 = CARTESIAN_POINT('Ctrl Pts',(-18.045087176113,-13.7785749983251,
114.84013824791)) ;
#194339 = CARTESIAN_POINT('Ctrl Pts',(-18.0758126785522,-14.0376123935157,
114.969142216543)) ;
#194340 = CARTESIAN_POINT('Ctrl Pts',(-18.126546298458,-14.2526152270872,
115.159131089373)) ;
#194341 = CARTESIAN_POINT('Ctrl Pts',(-18.1929627182085,-14.4080507138092,
115.39693012817)) ;
#194342 = CARTESIAN_POINT('Ctrl Pts',(-18.2695829032393,-14.4922598223547,
115.665846830142)) ;
#194343 = CARTESIAN_POINT('Ctrl Pts',(-18.3495327203372,-14.4995566650645,
115.94467290167)) ;
#194344 = CARTESIAN_POINT('Ctrl Pts',(-18.4275077803074,-14.4291954268347,
116.217786788456)) ;
#194345 = CARTESIAN_POINT('Ctrl Pts',(-18.4961354751818,-14.2862746553945,
116.462278671806)) ;
#194346 = CARTESIAN_POINT('Ctrl Pts',(-18.5499768620455,-14.0821782924177,
116.661608442272)) ;
#194347 = CARTESIAN_POINT('Ctrl Pts',(-18.5848332719322,-13.8298750263426,
116.803243954575)) ;
#194348 = CARTESIAN_POINT('Ctrl Pts',(-18.597136541653,-13.5470860719876,
116.876296357144)) ;
#194349 = CARTESIAN_POINT('Ctrl Pts',(-18.5852386802465,-13.2560613841224,
116.875504551637)) ;
#194350 = CARTESIAN_POINT('Ctrl Pts',(-18.549259012026,-12.9762949722028,
116.801413358043)) ;
#194351 = CARTESIAN_POINT('Ctrl Pts',(-18.4912772241492,-12.729021213087,
116.66017876415)) ;
#194352 = CARTESIAN_POINT('Ctrl Pts',(-18.4142572250889,-12.5300504685621,
116.461103914665)) ;
#194353 = CARTESIAN_POINT('Ctrl Pts',(-18.3230315098279,-12.3949013412461,
116.218789967548)) ;
#194354 = CARTESIAN_POINT('Ctrl Pts',(-18.223852812221,-12.3334783627152,
115.952132037095)) ;
#194355 = CARTESIAN_POINT('Ctrl Pts',(-18.1228645176016,-12.3494129205617,
115.679929191813)) ;
#194356 = CARTESIAN_POINT('Ctrl Pts',(-18.0261149973896,-12.4418688951199,
115.420743578469)) ;
#194357 = CARTESIAN_POINT('Ctrl Pts',(-17.9399661082425,-12.6051421932678,
115.193941498684)) ;
#194358 = CARTESIAN_POINT('Ctrl Pts',(-17.8706577437902,-12.824581983231,
115.018086912983)) ;
#194359 = CARTESIAN_POINT('Ctrl Pts',(-17.8211647568461,-13.0878606072953,
114.902837359147)) ;
#194360 = CARTESIAN_POINT('Ctrl Pts',(-17.7949112979524,-13.3747557627756,
114.858346400162)) ;
#194361 = CARTESIAN_POINT('Ctrl Pts',(-17.7930142307547,-13.6654070056361,
114.888132109586)) ;
#194362 = CARTESIAN_POINT('Ctrl Pts',(-17.8147252087611,-13.9370542943595,
114.989647338605)) ;
#194363 = CARTESIAN_POINT('Ctrl Pts',(-17.8580728556449,-14.1729033532404,
115.157292589129)) ;
#194364 = CARTESIAN_POINT('Ctrl Pts',(-17.9184133421674,-14.3528610645483,
115.376351104933)) ;
#194365 = CARTESIAN_POINT('Ctrl Pts',(-17.991766676009,-14.4673900074207,
115.635384696762)) ;
#194366 = CARTESIAN_POINT('Ctrl Pts',(-18.0711284340199,-14.5059091307987,
115.912498667304)) ;
#194367 = CARTESIAN_POINT('Ctrl Pts',(-18.1505342643703,-14.467003448986,
116.1897784186)) ;
#194368 = CARTESIAN_POINT('Ctrl Pts',(-18.2236575677772,-14.3526296857438,
116.448006484568)) ;
#194369 = CARTESIAN_POINT('Ctrl Pts',(-18.2841253649015,-14.1719531187117,
116.667560097024)) ;
#194370 = CARTESIAN_POINT('Ctrl Pts',(-18.3272925522858,-13.936583984801,
116.834555335885)) ;
#194371 = CARTESIAN_POINT('Ctrl Pts',(-18.3489789369998,-13.6642946874373,
116.936073490923)) ;
#194372 = CARTESIAN_POINT('Ctrl Pts',(-18.3470303613831,-13.3747428455626,
116.965562261399)) ;
#194373 = CARTESIAN_POINT('Ctrl Pts',(-18.3207665837922,-13.0876482903165,
116.921069134503)) ;
#194374 = CARTESIAN_POINT('Ctrl Pts',(-18.2712815660308,-12.8243385253649,
116.805840132971)) ;
#194375 = CARTESIAN_POINT('Ctrl Pts',(-18.2015034322164,-12.6038922563675,
116.628754857575)) ;
#194376 = CARTESIAN_POINT('Ctrl Pts',(-18.1155659825145,-12.4415502102937,
116.402472433253)) ;
#194377 = CARTESIAN_POINT('Ctrl Pts',(-18.0188186140626,-12.3493107874977,
116.143292052209)) ;
#194378 = CARTESIAN_POINT('Ctrl Pts',(-17.917965944462,-12.3333698024851,
115.871447888668)) ;
#194379 = CARTESIAN_POINT('Ctrl Pts',(-17.8179951285442,-12.3958418590805,
115.602676622725)) ;
#194380 = CARTESIAN_POINT('Ctrl Pts',(-17.7275667072708,-12.5305465195612,
115.362515531508)) ;
#194381 = CARTESIAN_POINT('Ctrl Pts',(-17.6506148333136,-12.7291635452138,
115.163608506426)) ;
#194382 = CARTESIAN_POINT('Ctrl Pts',(-17.5925315518145,-12.9771312925897,
115.022149073148)) ;
#194383 = CARTESIAN_POINT('Ctrl Pts',(-17.5565878319294,-13.2574946761857,
114.948229481288)) ;
#194384 = CARTESIAN_POINT('Ctrl Pts',(-17.5448475110634,-13.5486172877669,
114.947929919244)) ;
#194385 = CARTESIAN_POINT('Ctrl Pts',(-17.5571682124288,-13.8299622964239,
115.020863384168)) ;
#194386 = CARTESIAN_POINT('Ctrl Pts',(-17.5919536420937,-14.082140489746,
115.162256577588)) ;
#194387 = CARTESIAN_POINT('Ctrl Pts',(-17.6460547424978,-14.2871395255682,
115.362533542529)) ;
#194388 = CARTESIAN_POINT('Ctrl Pts',(-17.7149985645736,-14.4298488440199,
115.608097682744)) ;
#194389 = CARTESIAN_POINT('Ctrl Pts',(-17.7923224785126,-14.4994383097765,
115.878923588417)) ;
#194390 = CARTESIAN_POINT('Ctrl Pts',(-17.8726588843966,-14.4922423916848,
116.159099968041)) ;
#194391 = CARTESIAN_POINT('Ctrl Pts',(-17.9492605892441,-14.4074859363464,
116.427972082509)) ;
#194392 = CARTESIAN_POINT('Ctrl Pts',(-18.0153695983152,-14.2527213410347,
116.664674816876)) ;
#194393 = CARTESIAN_POINT('Ctrl Pts',(-18.0662184898938,-14.0372448891262,
116.855097648155)) ;
#194394 = CARTESIAN_POINT('Ctrl Pts',(-18.0969238178348,-13.7782273369584,
116.984027397216)) ;
#194395 = CARTESIAN_POINT('Ctrl Pts',(-18.1047200617367,-13.4921296981973,
117.043351119596)) ;
#194396 = CARTESIAN_POINT('Ctrl Pts',(-18.0891514169294,-13.217409939261,
117.029459791734)) ;
#194397 = CARTESIAN_POINT('Ctrl Pts',(-18.0654405919642,-13.0469696088692,
116.979117868373)) ;
#194398 = CARTESIAN_POINT('Ctrl Pts',(-18.0519478151656,-12.9727494438644,
116.948041367699)) ;
#194399 = CARTESIAN_POINT('',(-29.0978033499347,-13.1317299129408,113.463978642533)) ;
#194400 = CARTESIAN_POINT('Origin',(-29.0751148924065,-13.1500241806476,113.394873261672)) ;
#194401 = CARTESIAN_POINT('',(-29.0524264348783,-13.1683184483544,113.32576788081)) ;
#194402 = CARTESIAN_POINT('Origin',(-29.0751148924065,-13.1500241806476,113.394873261672)) ;
#194403 = CARTESIAN_POINT('Origin',(-29.0751148924065,-13.1500241806476,113.394873261672)) ;
#194404 = CARTESIAN_POINT('Ctrl Pts',(-29.1489187358159,-13.1500241806476,
113.370642219953)) ;
#194405 = CARTESIAN_POINT('Ctrl Pts',(-29.1501712550706,-13.1861488576831,
113.380503101533)) ;
#194406 = CARTESIAN_POINT('Ctrl Pts',(-29.1532918849611,-13.2629207728781,
113.383238925643)) ;
#194407 = CARTESIAN_POINT('Ctrl Pts',(-29.158850654713,-13.3681754735787,
113.336140363464)) ;
#194408 = CARTESIAN_POINT('Ctrl Pts',(-29.1641549311487,-13.4419954208924,
113.247282880188)) ;
#194409 = CARTESIAN_POINT('Ctrl Pts',(-29.1668024185619,-13.4603090867706,
113.172355715138)) ;
#194410 = CARTESIAN_POINT('Ctrl Pts',(-29.1677657801251,-13.4607127643287,
113.134762231593)) ;
#194411 = CARTESIAN_POINT('Ctrl Pts',(-29.1262302782877,-13.1683184483544,
113.301536839092)) ;
#194412 = CARTESIAN_POINT('Ctrl Pts',(-29.12711604839,-13.1940059114669,113.308742056967)) ;
#194413 = CARTESIAN_POINT('Ctrl Pts',(-29.1293290715985,-13.2486867737934,
113.311073820728)) ;
#194414 = CARTESIAN_POINT('Ctrl Pts',(-29.1332857460124,-13.3239058135206,
113.278044278162)) ;
#194415 = CARTESIAN_POINT('Ctrl Pts',(-29.1370736300659,-13.3769362528745,
113.215107919416)) ;
#194416 = CARTESIAN_POINT('Ctrl Pts',(-29.1389728533701,-13.3903536795156,
113.161819186649)) ;
#194417 = CARTESIAN_POINT('Ctrl Pts',(-29.1396668443893,-13.3908270508895,
113.135038642707)) ;
#194418 = CARTESIAN_POINT('Ctrl Pts',(-29.0524264348783,-13.1683184483544,
113.32576788081)) ;
#194419 = CARTESIAN_POINT('Ctrl Pts',(-29.0534550311952,-13.1977103078297,
113.333412909135)) ;
#194420 = CARTESIAN_POINT('Ctrl Pts',(-29.0560057529408,-13.2599976587319,
113.334883492462)) ;
#194421 = CARTESIAN_POINT('Ctrl Pts',(-29.0605207617359,-13.3449026924378,
113.295661398383)) ;
#194422 = CARTESIAN_POINT('Ctrl Pts',(-29.0648049091706,-13.4039111623081,
113.222879629767)) ;
#194423 = CARTESIAN_POINT('Ctrl Pts',(-29.0669264092244,-13.4180394153483,
113.161936094993)) ;
#194424 = CARTESIAN_POINT('Ctrl Pts',(-29.0676926945815,-13.4180036036418,
113.131444278443)) ;
#194425 = CARTESIAN_POINT('Ctrl Pts',(-28.9786225914689,-13.1683184483544,
113.349998922528)) ;
#194426 = CARTESIAN_POINT('Ctrl Pts',(-28.9797940140003,-13.2014147041926,
113.358083761303)) ;
#194427 = CARTESIAN_POINT('Ctrl Pts',(-28.9826824342832,-13.2713085436704,
113.358693164196)) ;
#194428 = CARTESIAN_POINT('Ctrl Pts',(-28.9877557774593,-13.365899571355,
113.313278518605)) ;
#194429 = CARTESIAN_POINT('Ctrl Pts',(-28.9925361882752,-13.4308860717416,
113.230651340118)) ;
#194430 = CARTESIAN_POINT('Ctrl Pts',(-28.9948799650788,-13.4457251511809,
113.162053003337)) ;
#194431 = CARTESIAN_POINT('Ctrl Pts',(-28.9957185447737,-13.445180156394,
113.12784991418)) ;
#194432 = CARTESIAN_POINT('Ctrl Pts',(-29.0013110489971,-13.1500241806476,
113.41910430339)) ;
#194433 = CARTESIAN_POINT('Ctrl Pts',(-29.002849220681,-13.1935576504088,
113.429844805869)) ;
#194434 = CARTESIAN_POINT('Ctrl Pts',(-29.0066452476457,-13.2855425427551,
113.430858269111)) ;
#194435 = CARTESIAN_POINT('Ctrl Pts',(-29.0133206861599,-13.4101692314131,
113.371374603907)) ;
#194436 = CARTESIAN_POINT('Ctrl Pts',(-29.019617489358,-13.4959452397595,
113.26282630089)) ;
#194437 = CARTESIAN_POINT('Ctrl Pts',(-29.0227095302706,-13.515680558436,
113.172589531826)) ;
#194438 = CARTESIAN_POINT('Ctrl Pts',(-29.0238174805094,-13.5150658698332,
113.127573503066)) ;
#194439 = CARTESIAN_POINT('Ctrl Pts',(-29.0239995065253,-13.1317299129408,
113.488209684252)) ;
#194440 = CARTESIAN_POINT('Ctrl Pts',(-29.0259044273616,-13.185700596625,
113.501605850436)) ;
#194441 = CARTESIAN_POINT('Ctrl Pts',(-29.0306080610083,-13.2997765418398,
113.503023374026)) ;
#194442 = CARTESIAN_POINT('Ctrl Pts',(-29.0388855948605,-13.4544388914713,
113.429470689208)) ;
#194443 = CARTESIAN_POINT('Ctrl Pts',(-29.0466987904407,-13.5610044077774,
113.295001261662)) ;
#194444 = CARTESIAN_POINT('Ctrl Pts',(-29.0505390954623,-13.585635965691,
113.183126060316)) ;
#194445 = CARTESIAN_POINT('Ctrl Pts',(-29.0519164162452,-13.5849515832724,
113.127297091952)) ;
#194446 = CARTESIAN_POINT('Ctrl Pts',(-29.0978033499347,-13.1317299129408,
113.463978642533)) ;
#194447 = CARTESIAN_POINT('Ctrl Pts',(-29.0995654445564,-13.1819962002622,
113.476934998268)) ;
#194448 = CARTESIAN_POINT('Ctrl Pts',(-29.103931379666,-13.2884656569013,
113.479213702292)) ;
#194449 = CARTESIAN_POINT('Ctrl Pts',(-29.111650579137,-13.433442012554,113.411853568987)) ;
#194450 = CARTESIAN_POINT('Ctrl Pts',(-29.1189675113361,-13.5340294983438,
113.287229551311)) ;
#194451 = CARTESIAN_POINT('Ctrl Pts',(-29.122585539608,-13.5579502298583,
113.183009151971)) ;
#194452 = CARTESIAN_POINT('Ctrl Pts',(-29.1238905660531,-13.5577750305201,
113.130891456215)) ;
#194453 = CARTESIAN_POINT('Ctrl Pts',(-29.1716071933441,-13.1317299129408,
113.439747600815)) ;
#194454 = CARTESIAN_POINT('Ctrl Pts',(-29.1732264617512,-13.1782918038993,
113.4522641461)) ;
#194455 = CARTESIAN_POINT('Ctrl Pts',(-29.1772546983237,-13.2771547719628,
113.455404030558)) ;
#194456 = CARTESIAN_POINT('Ctrl Pts',(-29.1844155634136,-13.4124451336368,
113.394236448766)) ;
#194457 = CARTESIAN_POINT('Ctrl Pts',(-29.1912362322315,-13.5070545889103,
113.27945784096)) ;
#194458 = CARTESIAN_POINT('Ctrl Pts',(-29.1946319837536,-13.5302644940257,
113.182892243627)) ;
#194459 = CARTESIAN_POINT('Ctrl Pts',(-29.1958647158609,-13.5305984777679,
113.134485820479)) ;
#194460 = CARTESIAN_POINT('Ctrl Pts',(-29.1489187358159,-13.1500241806476,
113.370642219953)) ;
#194461 = CARTESIAN_POINT('Ctrl Pts',(-29.1501712550706,-13.1861488576831,
113.380503101533)) ;
#194462 = CARTESIAN_POINT('Ctrl Pts',(-29.1532918849611,-13.2629207728781,
113.383238925643)) ;
#194463 = CARTESIAN_POINT('Ctrl Pts',(-29.158850654713,-13.3681754735787,
113.336140363464)) ;
#194464 = CARTESIAN_POINT('Ctrl Pts',(-29.1641549311487,-13.4419954208924,
113.247282880188)) ;
#194465 = CARTESIAN_POINT('Ctrl Pts',(-29.1668024185619,-13.4603090867706,
113.172355715138)) ;
#194466 = CARTESIAN_POINT('Ctrl Pts',(-29.1677657801251,-13.4607127643287,
113.134762231593)) ;
#194467 = CARTESIAN_POINT('',(-29.1677657801251,-13.4607127643287,113.134762231593)) ;
#194468 = CARTESIAN_POINT('Ctrl Pts',(-29.1489187358159,-13.1500241806476,
113.370642219953)) ;
#194469 = CARTESIAN_POINT('Ctrl Pts',(-29.1501712550706,-13.1861488576831,
113.380503101533)) ;
#194470 = CARTESIAN_POINT('Ctrl Pts',(-29.1532918849611,-13.2629207728781,
113.383238925643)) ;
#194471 = CARTESIAN_POINT('Ctrl Pts',(-29.158850654713,-13.3681754735787,
113.336140363464)) ;
#194472 = CARTESIAN_POINT('Ctrl Pts',(-29.1641549311487,-13.4419954208924,
113.247282880188)) ;
#194473 = CARTESIAN_POINT('Ctrl Pts',(-29.1668024185619,-13.4603090867706,
113.172355715138)) ;
#194474 = CARTESIAN_POINT('Ctrl Pts',(-29.1677657801251,-13.4607127643287,
113.134762231593)) ;
#194475 = CARTESIAN_POINT('Origin',(-29.0957916303173,-13.4878893170809,113.131167867329)) ;
#194476 = CARTESIAN_POINT('Ctrl Pts',(-29.1677657801251,-13.4607127643287,
113.134762231593)) ;
#194477 = CARTESIAN_POINT('Ctrl Pts',(-29.1774333842888,-13.4607136600768,
112.751611216526)) ;
#194478 = CARTESIAN_POINT('Ctrl Pts',(-29.1871009884525,-13.460714555825,
112.368460201459)) ;
#194479 = CARTESIAN_POINT('Ctrl Pts',(-29.1967685926162,-13.4607154515732,
111.985309186393)) ;
#194480 = CARTESIAN_POINT('Ctrl Pts',(-29.1396668443893,-13.3908270508895,
113.135038642707)) ;
#194481 = CARTESIAN_POINT('Ctrl Pts',(-29.149334448553,-13.3908279466377,
112.75188762764)) ;
#194482 = CARTESIAN_POINT('Ctrl Pts',(-29.1590020527167,-13.3908288423858,
112.368736612573)) ;
#194483 = CARTESIAN_POINT('Ctrl Pts',(-29.1686696568804,-13.390829738134,
111.985585597507)) ;
#194484 = CARTESIAN_POINT('Ctrl Pts',(-29.0676926945815,-13.4180036036418,
113.131444278443)) ;
#194485 = CARTESIAN_POINT('Ctrl Pts',(-29.0773602987452,-13.4180044993899,
112.748293263377)) ;
#194486 = CARTESIAN_POINT('Ctrl Pts',(-29.0870279029089,-13.4180053951381,
112.36514224831)) ;
#194487 = CARTESIAN_POINT('Ctrl Pts',(-29.0966955070725,-13.4180062908863,
111.981991233243)) ;
#194488 = CARTESIAN_POINT('Ctrl Pts',(-28.9957185447737,-13.445180156394,
113.12784991418)) ;
#194489 = CARTESIAN_POINT('Ctrl Pts',(-29.0053861489373,-13.4451810521422,
112.744698899113)) ;
#194490 = CARTESIAN_POINT('Ctrl Pts',(-29.015053753101,-13.4451819478904,
112.361547884046)) ;
#194491 = CARTESIAN_POINT('Ctrl Pts',(-29.0247213572647,-13.4451828436386,
111.97839686898)) ;
#194492 = CARTESIAN_POINT('Ctrl Pts',(-29.0238174805094,-13.5150658698332,
113.127573503066)) ;
#194493 = CARTESIAN_POINT('Ctrl Pts',(-29.0334850846731,-13.5150667655814,
112.744422487999)) ;
#194494 = CARTESIAN_POINT('Ctrl Pts',(-29.0431526888368,-13.5150676613296,
112.361271472932)) ;
#194495 = CARTESIAN_POINT('Ctrl Pts',(-29.0528202930005,-13.5150685570778,
111.978120457866)) ;
#194496 = CARTESIAN_POINT('Ctrl Pts',(-29.0519164162452,-13.5849515832724,
113.127297091952)) ;
#194497 = CARTESIAN_POINT('Ctrl Pts',(-29.0615840204089,-13.5849524790206,
112.744146076885)) ;
#194498 = CARTESIAN_POINT('Ctrl Pts',(-29.0712516245726,-13.5849533747688,
112.360995061818)) ;
#194499 = CARTESIAN_POINT('Ctrl Pts',(-29.0809192287363,-13.5849542705169,
111.977844046752)) ;
#194500 = CARTESIAN_POINT('Ctrl Pts',(-29.1238905660531,-13.5577750305201,
113.130891456215)) ;
#194501 = CARTESIAN_POINT('Ctrl Pts',(-29.1335581702167,-13.5577759262683,
112.747740441148)) ;
#194502 = CARTESIAN_POINT('Ctrl Pts',(-29.1432257743804,-13.5577768220165,
112.364589426082)) ;
#194503 = CARTESIAN_POINT('Ctrl Pts',(-29.1528933785441,-13.5577777177647,
111.981438411015)) ;
#194504 = CARTESIAN_POINT('Ctrl Pts',(-29.1958647158609,-13.5305984777679,
113.134485820479)) ;
#194505 = CARTESIAN_POINT('Ctrl Pts',(-29.2055323200246,-13.530599373516,
112.751334805412)) ;
#194506 = CARTESIAN_POINT('Ctrl Pts',(-29.2151999241883,-13.5306002692642,
112.368183790345)) ;
#194507 = CARTESIAN_POINT('Ctrl Pts',(-29.2248675283519,-13.5306011650124,
111.985032775279)) ;
#194508 = CARTESIAN_POINT('Ctrl Pts',(-29.1677657801251,-13.4607127643287,
113.134762231593)) ;
#194509 = CARTESIAN_POINT('Ctrl Pts',(-29.1774333842888,-13.4607136600768,
112.751611216526)) ;
#194510 = CARTESIAN_POINT('Ctrl Pts',(-29.1871009884525,-13.460714555825,
112.368460201459)) ;
#194511 = CARTESIAN_POINT('Ctrl Pts',(-29.1967685926162,-13.4607154515732,
111.985309186393)) ;
#194512 = CARTESIAN_POINT('',(-29.1967685926162,-13.4607154515732,111.985309186393)) ;
#194513 = CARTESIAN_POINT('',(-29.1677657801251,-13.4607127643287,113.134762231593)) ;
#194514 = CARTESIAN_POINT('',(-29.1248995454595,-13.562875855635,111.980154590046)) ;
#194515 = CARTESIAN_POINT('Origin',(-29.1247944428083,-13.4878920043255,111.981714822129)) ;
#194516 = CARTESIAN_POINT('',(-29.1246892014358,-13.4129081530202,111.983275048377)) ;
#194517 = CARTESIAN_POINT('Origin',(-29.1247944428083,-13.4878920043255,111.981714822129)) ;
#194518 = CARTESIAN_POINT('Origin',(-29.1247944428083,-13.4878920043255,111.981714822129)) ;
#194519 = CARTESIAN_POINT('Ctrl Pts',(-29.1967685926162,-13.4607154515732,
111.985309186393)) ;
#194520 = CARTESIAN_POINT('Ctrl Pts',(-29.20372433272,-13.4607154515732,111.919496169812)) ;
#194521 = CARTESIAN_POINT('Ctrl Pts',(-29.2391616569514,-13.4607154515732,
111.786249874406)) ;
#194522 = CARTESIAN_POINT('Ctrl Pts',(-29.3531737828725,-13.4607154515732,
111.608725138771)) ;
#194523 = CARTESIAN_POINT('Ctrl Pts',(-29.5178000156693,-13.4607154515732,
111.473552139375)) ;
#194524 = CARTESIAN_POINT('Ctrl Pts',(-29.7125058569765,-13.4607154515732,
111.39418874148)) ;
#194525 = CARTESIAN_POINT('Ctrl Pts',(-29.9214770342181,-13.4607154515732,
111.374286592167)) ;
#194526 = CARTESIAN_POINT('Ctrl Pts',(-30.129031067933,-13.4607154515732,
111.417939881308)) ;
#194527 = CARTESIAN_POINT('Ctrl Pts',(-30.3108273632114,-13.4607154515732,
111.522718871897)) ;
#194528 = CARTESIAN_POINT('Ctrl Pts',(-30.4475054824147,-13.4607154515732,
111.674400413727)) ;
#194529 = CARTESIAN_POINT('Ctrl Pts',(-30.5306819470581,-13.4607154515732,
111.859696163125)) ;
#194530 = CARTESIAN_POINT('Ctrl Pts',(-30.5515845507338,-13.4607154515732,
112.065598309889)) ;
#194531 = CARTESIAN_POINT('Ctrl Pts',(-30.505144819815,-13.4607154515732,
112.268886698136)) ;
#194532 = CARTESIAN_POINT('Ctrl Pts',(-30.3992903014189,-13.4607154515732,
112.446856086907)) ;
#194533 = CARTESIAN_POINT('Ctrl Pts',(-30.2443913742949,-13.4607154515732,
112.587215246961)) ;
#194534 = CARTESIAN_POINT('Ctrl Pts',(-30.0504246992742,-13.4607154515732,
112.677419162906)) ;
#194535 = CARTESIAN_POINT('Ctrl Pts',(-29.8384424605617,-13.4607154515732,
112.704782293005)) ;
#194536 = CARTESIAN_POINT('Ctrl Pts',(-29.7003053480643,-13.4607154515732,
112.680623972109)) ;
#194537 = CARTESIAN_POINT('Ctrl Pts',(-29.6364905070076,-13.4607154515732,
112.659288401873)) ;
#194538 = CARTESIAN_POINT('Ctrl Pts',(-29.1686696568804,-13.390829738134,
111.985585597507)) ;
#194539 = CARTESIAN_POINT('Ctrl Pts',(-29.1756547434426,-13.390829738134,
111.917020083641)) ;
#194540 = CARTESIAN_POINT('Ctrl Pts',(-29.212039584699,-13.390829738134,111.778121325125)) ;
#194541 = CARTESIAN_POINT('Ctrl Pts',(-29.3300921411966,-13.390829738134,
111.59281646223)) ;
#194542 = CARTESIAN_POINT('Ctrl Pts',(-29.5010310293307,-13.390829738134,
111.451428992033)) ;
#194543 = CARTESIAN_POINT('Ctrl Pts',(-29.7035209080743,-13.390829738134,
111.368050962531)) ;
#194544 = CARTESIAN_POINT('Ctrl Pts',(-29.9211042383572,-13.390829738134,
111.346544328624)) ;
#194545 = CARTESIAN_POINT('Ctrl Pts',(-30.1374625031161,-13.390829738134,
111.391231429979)) ;
#194546 = CARTESIAN_POINT('Ctrl Pts',(-30.3272332269861,-13.390829738134,
111.499672718509)) ;
#194547 = CARTESIAN_POINT('Ctrl Pts',(-30.4701946296492,-13.390829738134,
111.657128061289)) ;
#194548 = CARTESIAN_POINT('Ctrl Pts',(-30.557562095135,-13.390829738134,111.84978988896)) ;
#194549 = CARTESIAN_POINT('Ctrl Pts',(-30.5801472209913,-13.390829738134,
112.064144238615)) ;
#194550 = CARTESIAN_POINT('Ctrl Pts',(-30.5325790354759,-13.390829738134,
112.276027895464)) ;
#194551 = CARTESIAN_POINT('Ctrl Pts',(-30.4230251037581,-13.390829738134,
112.4617653852)) ;
#194552 = CARTESIAN_POINT('Ctrl Pts',(-30.262238546402,-13.390829738134,112.608517564604)) ;
#194553 = CARTESIAN_POINT('Ctrl Pts',(-30.0605613896538,-13.390829738134,
112.703182459841)) ;
#194554 = CARTESIAN_POINT('Ctrl Pts',(-29.8398712403783,-13.390829738134,
112.732470410434)) ;
#194555 = CARTESIAN_POINT('Ctrl Pts',(-29.6958938251326,-13.390829738134,
112.707826831835)) ;
#194556 = CARTESIAN_POINT('Ctrl Pts',(-29.629340767279,-13.390829738134,112.685845544367)) ;
#194557 = CARTESIAN_POINT('Ctrl Pts',(-29.0966955070725,-13.4180062908863,
111.981991233243)) ;
#194558 = CARTESIAN_POINT('Ctrl Pts',(-29.1042018243928,-13.4180062908863,
111.906366156869)) ;
#194559 = CARTESIAN_POINT('Ctrl Pts',(-29.1439282935352,-13.4180062908863,
111.753105943509)) ;
#194560 = CARTESIAN_POINT('Ctrl Pts',(-29.2735847434014,-13.4180062908863,
111.548452874742)) ;
#194561 = CARTESIAN_POINT('Ctrl Pts',(-29.4616903508979,-13.4180062908863,
111.392083350338)) ;
#194562 = CARTESIAN_POINT('Ctrl Pts',(-29.6847569451829,-13.4180062908863,
111.299594335584)) ;
#194563 = CARTESIAN_POINT('Ctrl Pts',(-29.9246462294043,-13.4180062908863,
111.275288997659)) ;
#194564 = CARTESIAN_POINT('Ctrl Pts',(-30.163374541951,-13.4180062908863,
111.323977785698)) ;
#194565 = CARTESIAN_POINT('Ctrl Pts',(-30.3729651263444,-13.4180062908863,
111.443039456787)) ;
#194566 = CARTESIAN_POINT('Ctrl Pts',(-30.531075074711,-13.4180062908863,
111.616275157639)) ;
#194567 = CARTESIAN_POINT('Ctrl Pts',(-30.6279770680687,-13.4180062908863,
111.828483329082)) ;
#194568 = CARTESIAN_POINT('Ctrl Pts',(-30.6534993343581,-13.4180062908863,
112.064787262698)) ;
#194569 = CARTESIAN_POINT('Ctrl Pts',(-30.601649394132,-13.4180062908863,
112.298557128891)) ;
#194570 = CARTESIAN_POINT('Ctrl Pts',(-30.4813664747353,-13.4180062908863,
112.503664191636)) ;
#194571 = CARTESIAN_POINT('Ctrl Pts',(-30.3044722648641,-13.4180062908863,
112.665921754)) ;
#194572 = CARTESIAN_POINT('Ctrl Pts',(-30.0823343436128,-13.4180062908863,
112.770854415123)) ;
#194573 = CARTESIAN_POINT('Ctrl Pts',(-29.839041196435,-13.4180062908863,
112.803748518785)) ;
#194574 = CARTESIAN_POINT('Ctrl Pts',(-29.6801920694942,-13.4180062908863,
112.77696504109)) ;
#194575 = CARTESIAN_POINT('Ctrl Pts',(-29.6067342129979,-13.4180062908863,
112.752907176841)) ;
#194576 = CARTESIAN_POINT('Ctrl Pts',(-29.0247213572647,-13.4451828436386,
111.97839686898)) ;
#194577 = CARTESIAN_POINT('Ctrl Pts',(-29.0327489053431,-13.4451828436386,
111.895712230097)) ;
#194578 = CARTESIAN_POINT('Ctrl Pts',(-29.0758170023715,-13.4451828436386,
111.728090561893)) ;
#194579 = CARTESIAN_POINT('Ctrl Pts',(-29.2170773456061,-13.4451828436386,
111.504089287253)) ;
#194580 = CARTESIAN_POINT('Ctrl Pts',(-29.4223496724652,-13.4451828436386,
111.332737708643)) ;
#194581 = CARTESIAN_POINT('Ctrl Pts',(-29.6659929822914,-13.4451828436386,
111.231137708637)) ;
#194582 = CARTESIAN_POINT('Ctrl Pts',(-29.9281882204513,-13.4451828436386,
111.204033666694)) ;
#194583 = CARTESIAN_POINT('Ctrl Pts',(-30.189286580786,-13.4451828436386,
111.256724141416)) ;
#194584 = CARTESIAN_POINT('Ctrl Pts',(-30.4186970257026,-13.4451828436386,
111.386406195065)) ;
#194585 = CARTESIAN_POINT('Ctrl Pts',(-30.5919555197728,-13.4451828436386,
111.575422253988)) ;
#194586 = CARTESIAN_POINT('Ctrl Pts',(-30.6983920410023,-13.4451828436386,
111.807176769205)) ;
#194587 = CARTESIAN_POINT('Ctrl Pts',(-30.7268514477248,-13.4451828436386,
112.065430286781)) ;
#194588 = CARTESIAN_POINT('Ctrl Pts',(-30.6707197527881,-13.4451828436386,
112.321086362319)) ;
#194589 = CARTESIAN_POINT('Ctrl Pts',(-30.5397078457124,-13.4451828436386,
112.545562998072)) ;
#194590 = CARTESIAN_POINT('Ctrl Pts',(-30.3467059833262,-13.4451828436386,
112.723325943396)) ;
#194591 = CARTESIAN_POINT('Ctrl Pts',(-30.1041072975719,-13.4451828436386,
112.838526370406)) ;
#194592 = CARTESIAN_POINT('Ctrl Pts',(-29.8382111524917,-13.4451828436386,
112.875026627135)) ;
#194593 = CARTESIAN_POINT('Ctrl Pts',(-29.6644903138558,-13.4451828436386,
112.846103250345)) ;
#194594 = CARTESIAN_POINT('Ctrl Pts',(-29.5841276587169,-13.4451828436386,
112.819968809314)) ;
#194595 = CARTESIAN_POINT('Ctrl Pts',(-29.0528202930005,-13.5150685570778,
111.978120457866)) ;
#194596 = CARTESIAN_POINT('Ctrl Pts',(-29.0608184946204,-13.5150685570778,
111.898188316268)) ;
#194597 = CARTESIAN_POINT('Ctrl Pts',(-29.1029390746239,-13.5150685570778,
111.736219111174)) ;
#194598 = CARTESIAN_POINT('Ctrl Pts',(-29.2401589872819,-13.5150685570778,
111.519997963795)) ;
#194599 = CARTESIAN_POINT('Ctrl Pts',(-29.4391186588037,-13.5150685570778,
111.354860855985)) ;
#194600 = CARTESIAN_POINT('Ctrl Pts',(-29.6749779311936,-13.5150685570778,
111.257275487585)) ;
#194601 = CARTESIAN_POINT('Ctrl Pts',(-29.9285610163122,-13.5150685570778,
111.231775930237)) ;
#194602 = CARTESIAN_POINT('Ctrl Pts',(-30.1808551456028,-13.5150685570778,
111.283432592745)) ;
#194603 = CARTESIAN_POINT('Ctrl Pts',(-30.4022911619279,-13.5150685570778,
111.409452348454)) ;
#194604 = CARTESIAN_POINT('Ctrl Pts',(-30.5692663725382,-13.5150685570778,
111.592694606426)) ;
#194605 = CARTESIAN_POINT('Ctrl Pts',(-30.6715118929254,-13.5150685570778,
111.817083043369)) ;
#194606 = CARTESIAN_POINT('Ctrl Pts',(-30.6982887774674,-13.5150685570778,
112.066884358055)) ;
#194607 = CARTESIAN_POINT('Ctrl Pts',(-30.6432855371273,-13.5150685570778,
112.313945164991)) ;
#194608 = CARTESIAN_POINT('Ctrl Pts',(-30.5159730433732,-13.5150685570778,
112.530653699779)) ;
#194609 = CARTESIAN_POINT('Ctrl Pts',(-30.3288588112191,-13.5150685570778,
112.702023625753)) ;
#194610 = CARTESIAN_POINT('Ctrl Pts',(-30.0939706071923,-13.5150685570778,
112.812763073471)) ;
#194611 = CARTESIAN_POINT('Ctrl Pts',(-29.8367823726751,-13.5150685570778,
112.847338509706)) ;
#194612 = CARTESIAN_POINT('Ctrl Pts',(-29.6689018367874,-13.5150685570778,
112.818900390618)) ;
#194613 = CARTESIAN_POINT('Ctrl Pts',(-29.5912773984455,-13.5150685570778,
112.79341166682)) ;
#194614 = CARTESIAN_POINT('Ctrl Pts',(-29.0809192287363,-13.5849542705169,
111.977844046752)) ;
#194615 = CARTESIAN_POINT('Ctrl Pts',(-29.0888880838978,-13.5849542705169,
111.90066440244)) ;
#194616 = CARTESIAN_POINT('Ctrl Pts',(-29.1300611468763,-13.5849542705169,
111.744347660455)) ;
#194617 = CARTESIAN_POINT('Ctrl Pts',(-29.2632406289578,-13.5849542705169,
111.535906640336)) ;
#194618 = CARTESIAN_POINT('Ctrl Pts',(-29.4558876451423,-13.5849542705169,
111.376984003328)) ;
#194619 = CARTESIAN_POINT('Ctrl Pts',(-29.6839628800958,-13.5849542705169,
111.283413266534)) ;
#194620 = CARTESIAN_POINT('Ctrl Pts',(-29.9289338121731,-13.5849542705169,
111.259518193781)) ;
#194621 = CARTESIAN_POINT('Ctrl Pts',(-30.1724237104197,-13.5849542705169,
111.310141044074)) ;
#194622 = CARTESIAN_POINT('Ctrl Pts',(-30.3858852981532,-13.5849542705169,
111.432498501842)) ;
#194623 = CARTESIAN_POINT('Ctrl Pts',(-30.5465772253037,-13.5849542705169,
111.609966958864)) ;
#194624 = CARTESIAN_POINT('Ctrl Pts',(-30.6446317448485,-13.5849542705169,
111.826989317534)) ;
#194625 = CARTESIAN_POINT('Ctrl Pts',(-30.6697261072099,-13.5849542705169,
112.068338429329)) ;
#194626 = CARTESIAN_POINT('Ctrl Pts',(-30.6158513214665,-13.5849542705169,
112.306803967663)) ;
#194627 = CARTESIAN_POINT('Ctrl Pts',(-30.492238241034,-13.5849542705169,
112.515744401486)) ;
#194628 = CARTESIAN_POINT('Ctrl Pts',(-30.311011639112,-13.5849542705169,
112.680721308109)) ;
#194629 = CARTESIAN_POINT('Ctrl Pts',(-30.0838339168126,-13.5849542705169,
112.786999776536)) ;
#194630 = CARTESIAN_POINT('Ctrl Pts',(-29.8353535928585,-13.5849542705169,
112.819650392276)) ;
#194631 = CARTESIAN_POINT('Ctrl Pts',(-29.6733133597191,-13.5849542705169,
112.791697530891)) ;
#194632 = CARTESIAN_POINT('Ctrl Pts',(-29.5984271381742,-13.5849542705169,
112.766854524325)) ;
#194633 = CARTESIAN_POINT('Ctrl Pts',(-29.1528933785441,-13.5577777177647,
111.981438411015)) ;
#194634 = CARTESIAN_POINT('Ctrl Pts',(-29.1603410029476,-13.5577777177647,
111.911318329212)) ;
#194635 = CARTESIAN_POINT('Ctrl Pts',(-29.19817243804,-13.5577777177647,111.769363042071)) ;
#194636 = CARTESIAN_POINT('Ctrl Pts',(-29.319748026753,-13.5577777177647,
111.580270227824)) ;
#194637 = CARTESIAN_POINT('Ctrl Pts',(-29.4952283235751,-13.5577777177647,
111.436329645022)) ;
#194638 = CARTESIAN_POINT('Ctrl Pts',(-29.7027268429873,-13.5577777177647,
111.351869893481)) ;
#194639 = CARTESIAN_POINT('Ctrl Pts',(-29.925391821126,-13.5577777177647,
111.330773524746)) ;
#194640 = CARTESIAN_POINT('Ctrl Pts',(-30.1465116715848,-13.5577777177647,
111.377394688355)) ;
#194641 = CARTESIAN_POINT('Ctrl Pts',(-30.340153398795,-13.5577777177647,
111.489131763564)) ;
#194642 = CARTESIAN_POINT('Ctrl Pts',(-30.4856967802419,-13.5577777177647,
111.650819862515)) ;
#194643 = CARTESIAN_POINT('Ctrl Pts',(-30.5742167719148,-13.5577777177647,
111.848295877412)) ;
#194644 = CARTESIAN_POINT('Ctrl Pts',(-30.5963739938431,-13.5577777177647,
112.067695405246)) ;
#194645 = CARTESIAN_POINT('Ctrl Pts',(-30.5467809628103,-13.5577777177647,
112.284274734236)) ;
#194646 = CARTESIAN_POINT('Ctrl Pts',(-30.4338968700568,-13.5577777177647,
112.473845595049)) ;
#194647 = CARTESIAN_POINT('Ctrl Pts',(-30.2687779206499,-13.5577777177647,
112.623317118714)) ;
#194648 = CARTESIAN_POINT('Ctrl Pts',(-30.0620609628536,-13.5577777177647,
112.719327821253)) ;
#194649 = CARTESIAN_POINT('Ctrl Pts',(-29.8361836368019,-13.5577777177647,
112.748372283926)) ;
#194650 = CARTESIAN_POINT('Ctrl Pts',(-29.6890151153575,-13.5577777177647,
112.722559321637)) ;
#194651 = CARTESIAN_POINT('Ctrl Pts',(-29.6210336924552,-13.5577777177647,
112.699792891852)) ;
#194652 = CARTESIAN_POINT('Ctrl Pts',(-29.2248675283519,-13.5306011650124,
111.985032775279)) ;
#194653 = CARTESIAN_POINT('Ctrl Pts',(-29.2317939219973,-13.5306011650124,
111.921972255984)) ;
#194654 = CARTESIAN_POINT('Ctrl Pts',(-29.2662837292037,-13.5306011650124,
111.794378423687)) ;
#194655 = CARTESIAN_POINT('Ctrl Pts',(-29.3762554245483,-13.5306011650124,
111.624633815312)) ;
#194656 = CARTESIAN_POINT('Ctrl Pts',(-29.5345690020079,-13.5306011650124,
111.495675286717)) ;
#194657 = CARTESIAN_POINT('Ctrl Pts',(-29.7214908058787,-13.5306011650124,
111.420326520428)) ;
#194658 = CARTESIAN_POINT('Ctrl Pts',(-29.921849830079,-13.5306011650124,
111.402028855711)) ;
#194659 = CARTESIAN_POINT('Ctrl Pts',(-30.1205996327499,-13.5306011650124,
111.444648332636)) ;
#194660 = CARTESIAN_POINT('Ctrl Pts',(-30.2944214994368,-13.5306011650124,
111.545765025285)) ;
#194661 = CARTESIAN_POINT('Ctrl Pts',(-30.4248163351801,-13.5306011650124,
111.691672766166)) ;
#194662 = CARTESIAN_POINT('Ctrl Pts',(-30.5038017989812,-13.5306011650124,
111.86960243729)) ;
#194663 = CARTESIAN_POINT('Ctrl Pts',(-30.5230218804764,-13.5306011650124,
112.067052381163)) ;
#194664 = CARTESIAN_POINT('Ctrl Pts',(-30.4777106041542,-13.5306011650124,
112.261745500808)) ;
#194665 = CARTESIAN_POINT('Ctrl Pts',(-30.3755554990797,-13.5306011650124,
112.431946788613)) ;
#194666 = CARTESIAN_POINT('Ctrl Pts',(-30.2265442021878,-13.5306011650124,
112.565912929318)) ;
#194667 = CARTESIAN_POINT('Ctrl Pts',(-30.0402880088946,-13.5306011650124,
112.65165586597)) ;
#194668 = CARTESIAN_POINT('Ctrl Pts',(-29.8370136807451,-13.5306011650124,
112.677094175575)) ;
#194669 = CARTESIAN_POINT('Ctrl Pts',(-29.7047168709959,-13.5306011650124,
112.653421112382)) ;
#194670 = CARTESIAN_POINT('Ctrl Pts',(-29.6436402467363,-13.5306011650124,
112.632731259378)) ;
#194671 = CARTESIAN_POINT('Ctrl Pts',(-29.1967685926162,-13.4607154515732,
111.985309186393)) ;
#194672 = CARTESIAN_POINT('Ctrl Pts',(-29.20372433272,-13.4607154515732,111.919496169812)) ;
#194673 = CARTESIAN_POINT('Ctrl Pts',(-29.2391616569514,-13.4607154515732,
111.786249874406)) ;
#194674 = CARTESIAN_POINT('Ctrl Pts',(-29.3531737828725,-13.4607154515732,
111.608725138771)) ;
#194675 = CARTESIAN_POINT('Ctrl Pts',(-29.5178000156693,-13.4607154515732,
111.473552139375)) ;
#194676 = CARTESIAN_POINT('Ctrl Pts',(-29.7125058569765,-13.4607154515732,
111.39418874148)) ;
#194677 = CARTESIAN_POINT('Ctrl Pts',(-29.9214770342181,-13.4607154515732,
111.374286592167)) ;
#194678 = CARTESIAN_POINT('Ctrl Pts',(-30.129031067933,-13.4607154515732,
111.417939881308)) ;
#194679 = CARTESIAN_POINT('Ctrl Pts',(-30.3108273632114,-13.4607154515732,
111.522718871897)) ;
#194680 = CARTESIAN_POINT('Ctrl Pts',(-30.4475054824147,-13.4607154515732,
111.674400413727)) ;
#194681 = CARTESIAN_POINT('Ctrl Pts',(-30.5306819470581,-13.4607154515732,
111.859696163125)) ;
#194682 = CARTESIAN_POINT('Ctrl Pts',(-30.5515845507338,-13.4607154515732,
112.065598309889)) ;
#194683 = CARTESIAN_POINT('Ctrl Pts',(-30.505144819815,-13.4607154515732,
112.268886698136)) ;
#194684 = CARTESIAN_POINT('Ctrl Pts',(-30.3992903014189,-13.4607154515732,
112.446856086907)) ;
#194685 = CARTESIAN_POINT('Ctrl Pts',(-30.2443913742949,-13.4607154515732,
112.587215246961)) ;
#194686 = CARTESIAN_POINT('Ctrl Pts',(-30.0504246992742,-13.4607154515732,
112.677419162906)) ;
#194687 = CARTESIAN_POINT('Ctrl Pts',(-29.8384424605617,-13.4607154515732,
112.704782293005)) ;
#194688 = CARTESIAN_POINT('Ctrl Pts',(-29.7003053480643,-13.4607154515732,
112.680623972109)) ;
#194689 = CARTESIAN_POINT('Ctrl Pts',(-29.6364905070076,-13.4607154515732,
112.659288401873)) ;
#194690 = CARTESIAN_POINT('Ctrl Pts',(-29.1967685926162,-13.4607154515732,
111.985309186393)) ;
#194691 = CARTESIAN_POINT('Ctrl Pts',(-29.20372433272,-13.4607154515732,111.919496169812)) ;
#194692 = CARTESIAN_POINT('Ctrl Pts',(-29.2391616569514,-13.4607154515732,
111.786249874406)) ;
#194693 = CARTESIAN_POINT('Ctrl Pts',(-29.3531737828725,-13.4607154515732,
111.608725138771)) ;
#194694 = CARTESIAN_POINT('Ctrl Pts',(-29.5178000156693,-13.4607154515732,
111.473552139375)) ;
#194695 = CARTESIAN_POINT('Ctrl Pts',(-29.7125058569765,-13.4607154515732,
111.39418874148)) ;
#194696 = CARTESIAN_POINT('Ctrl Pts',(-29.9214770342181,-13.4607154515732,
111.374286592167)) ;
#194697 = CARTESIAN_POINT('Ctrl Pts',(-30.129031067933,-13.4607154515732,
111.417939881308)) ;
#194698 = CARTESIAN_POINT('Ctrl Pts',(-30.3108273632114,-13.4607154515732,
111.522718871897)) ;
#194699 = CARTESIAN_POINT('Ctrl Pts',(-30.4475054824147,-13.4607154515732,
111.674400413727)) ;
#194700 = CARTESIAN_POINT('Ctrl Pts',(-30.5306819470581,-13.4607154515732,
111.859696163125)) ;
#194701 = CARTESIAN_POINT('Ctrl Pts',(-30.5515845507338,-13.4607154515732,
112.065598309889)) ;
#194702 = CARTESIAN_POINT('Ctrl Pts',(-30.505144819815,-13.4607154515732,
112.268886698136)) ;
#194703 = CARTESIAN_POINT('Ctrl Pts',(-30.3992903014189,-13.4607154515732,
112.446856086907)) ;
#194704 = CARTESIAN_POINT('Ctrl Pts',(-30.2443913742949,-13.4607154515732,
112.587215246961)) ;
#194705 = CARTESIAN_POINT('Ctrl Pts',(-30.0504246992742,-13.4607154515732,
112.677419162906)) ;
#194706 = CARTESIAN_POINT('Ctrl Pts',(-29.8384424605617,-13.4607154515732,
112.704782293005)) ;
#194707 = CARTESIAN_POINT('Ctrl Pts',(-29.7003053480643,-13.4607154515732,
112.680623972109)) ;
#194708 = CARTESIAN_POINT('Ctrl Pts',(-29.6364905070076,-13.4607154515732,
112.659288401873)) ;
#194709 = CARTESIAN_POINT('Origin',(-17.8642992765666,-11.5234495205728,116.376494196106)) ;
#194710 = CARTESIAN_POINT('Origin',(-17.6291851847899,-11.5234495205728,115.660374608073)) ;
#194711 = CARTESIAN_POINT('Origin',(-62.2357882624759,4.95951629533962E-11,
66.631932161929)) ;
#194712 = CARTESIAN_POINT('',(-60.3236060552914,4.95951629533962E-11,66.91989597577)) ;
#194713 = CARTESIAN_POINT('',(-64.1479704696604,4.95951629533962E-11,66.343968348088)) ;
#194714 = CARTESIAN_POINT('',(-60.3236060552914,4.95951629533962E-11,66.91989597577)) ;
#194715 = CARTESIAN_POINT('',(-64.1479704696604,3.00000000004959,66.343968348088)) ;
#194716 = CARTESIAN_POINT('',(-64.1479704696604,4.95951629533962E-11,66.343968348088)) ;
#194717 = CARTESIAN_POINT('',(-60.3236060552914,3.00000000004959,66.91989597577)) ;
#194718 = CARTESIAN_POINT('',(-60.3236060552914,3.00000000004959,66.91989597577)) ;
#194719 = CARTESIAN_POINT('',(-60.3236060552914,4.95951629533962E-11,66.91989597577)) ;
#194720 = CARTESIAN_POINT('Ctrl Pts',(-64.1479704696604,4.95951629533962E-11,
66.343968348088)) ;
#194721 = CARTESIAN_POINT('Ctrl Pts',(-64.1479704696604,3.6000000000496,66.343968348088)) ;
#194722 = CARTESIAN_POINT('Ctrl Pts',(-48.5009761261745,4.95951629533962E-11,
91.9190517712764)) ;
#194723 = CARTESIAN_POINT('Ctrl Pts',(-48.5009761261745,3.6000000000496,91.9190517712764)) ;
#194724 = CARTESIAN_POINT('Ctrl Pts',(-35.1273171461558,4.95951629533962E-11,
118.752958858659)) ;
#194725 = CARTESIAN_POINT('Ctrl Pts',(-35.1273171461558,3.6000000000496,118.752958858659)) ;
#194726 = CARTESIAN_POINT('',(-35.1273171461558,4.95951629533962E-11,118.752958858659)) ;
#194727 = CARTESIAN_POINT('Origin',(-653.750510408462,4.95951629534048E-11,
427.066451816625)) ;
#194728 = CARTESIAN_POINT('',(-35.1273171461558,3.00000000004959,118.752958858659)) ;
#194729 = CARTESIAN_POINT('',(-35.1273171461558,4.95951629533962E-11,118.752958858659)) ;
#194730 = CARTESIAN_POINT('Origin',(-653.750510408462,3.00000000005019,427.066451816625)) ;
#194731 = CARTESIAN_POINT('Origin',(-37.3648272827455,4.95951629533962E-11,
119.868103866564)) ;
#194732 = CARTESIAN_POINT('',(-34.8664381173996,4.95951629533962E-11,119.957834454884)) ;
#194733 = CARTESIAN_POINT('Origin',(-37.3648272827455,4.95951629533962E-11,
119.868103866564)) ;
#194734 = CARTESIAN_POINT('',(-34.8664381173996,3.00000000004959,119.957834454884)) ;
#194735 = CARTESIAN_POINT('',(-34.8664381173996,4.95951629533962E-11,119.957834454884)) ;
#194736 = CARTESIAN_POINT('Origin',(-37.3648272827455,3.00000000004959,119.868103866564)) ;
#194737 = CARTESIAN_POINT('Origin',(-28.8703041205692,4.95951629533962E-11,
120.173187866852)) ;
#194738 = CARTESIAN_POINT('',(-34.5457502165649,4.95951629533962E-11,122.11980329149)) ;
#194739 = CARTESIAN_POINT('Origin',(-28.8703041205692,4.95951629533962E-11,
120.173187866852)) ;
#194740 = CARTESIAN_POINT('',(-34.5457502165649,3.00000000004959,122.11980329149)) ;
#194741 = CARTESIAN_POINT('',(-34.5457502165649,4.95951629533962E-11,122.11980329149)) ;
#194742 = CARTESIAN_POINT('Origin',(-28.8703041205692,3.00000000004959,120.173187866852)) ;
#194743 = CARTESIAN_POINT('Origin',(-36.9105194232301,4.95951629533962E-11,
122.930893051756)) ;
#194744 = CARTESIAN_POINT('',(-35.3359939804146,4.95951629533962E-11,124.872765763838)) ;
#194745 = CARTESIAN_POINT('Origin',(-36.9105194232301,4.95951629533962E-11,
122.930893051756)) ;
#194746 = CARTESIAN_POINT('',(-35.3359939804146,3.00000000004959,124.872765763838)) ;
#194747 = CARTESIAN_POINT('',(-35.3359939804146,4.95951629533962E-11,124.872765763838)) ;
#194748 = CARTESIAN_POINT('Origin',(-36.9105194232301,3.00000000004959,122.930893051756)) ;
#194749 = CARTESIAN_POINT('Origin',(-33.9682898421302,4.95951629533962E-11,
126.55956438399)) ;
#194750 = CARTESIAN_POINT('',(-32.066048812378,4.95951629533962E-11,127.607125007321)) ;
#194751 = CARTESIAN_POINT('Origin',(-33.9682898421302,4.95951629533962E-11,
126.55956438399)) ;
#194752 = CARTESIAN_POINT('',(-32.066048812378,3.00000000004959,127.607125007321)) ;
#194753 = CARTESIAN_POINT('',(-32.066048812378,4.95951629533962E-11,127.607125007321)) ;
#194754 = CARTESIAN_POINT('Origin',(-33.9682898421302,3.00000000004959,126.55956438399)) ;
#194755 = CARTESIAN_POINT('Origin',(-29.8761549487317,4.95951629533962E-11,
128.813095515238)) ;
#194756 = CARTESIAN_POINT('',(-29.0664859793916,4.95951629533962E-11,126.447839469883)) ;
#194757 = CARTESIAN_POINT('Origin',(-29.8761549487317,4.95951629533962E-11,
128.813095515238)) ;
#194758 = CARTESIAN_POINT('',(-29.0664859793916,3.00000000004959,126.447839469883)) ;
#194759 = CARTESIAN_POINT('',(-29.0664859793916,4.95951629533962E-11,126.447839469883)) ;
#194760 = CARTESIAN_POINT('Origin',(-29.8761549487317,3.0000000000496,128.813095515238)) ;
#194761 = CARTESIAN_POINT('Origin',(-25.2094857224778,4.95951629533962E-11,
127.768158861474)) ;
#194762 = CARTESIAN_POINT('',(-21.3524854655639,4.95951629533962E-11,129.088478253065)) ;
#194763 = CARTESIAN_POINT('',(-29.0664859793916,4.95951629533962E-11,126.447839469883)) ;
#194764 = CARTESIAN_POINT('',(-21.3524854655639,3.00000000004959,129.088478253065)) ;
#194765 = CARTESIAN_POINT('',(-21.3524854655639,4.95951629533962E-11,129.088478253065)) ;
#194766 = CARTESIAN_POINT('',(-29.0664859793916,3.00000000004959,126.447839469883)) ;
#194767 = CARTESIAN_POINT('Origin',(-19.4092799391475,4.95951629533962E-11,
123.411863744214)) ;
#194768 = CARTESIAN_POINT('',(-14.7050516300984,4.95951629533962E-11,127.136140320455)) ;
#194769 = CARTESIAN_POINT('Origin',(-19.4092799391475,4.95951629533962E-11,
123.411863744213)) ;
#194770 = CARTESIAN_POINT('',(-14.7050516300984,3.00000000004959,127.136140320455)) ;
#194771 = CARTESIAN_POINT('',(-14.7050516300984,4.95951629533962E-11,127.136140320455)) ;
#194772 = CARTESIAN_POINT('Origin',(-19.4092799391475,3.0000000000496,123.411863744213)) ;
#194773 = CARTESIAN_POINT('Origin',(-18.0975728496786,4.95951629533962E-11,
125.974820316764)) ;
#194774 = CARTESIAN_POINT('',(-21.4900940692588,4.95951629533962E-11,124.813500313073)) ;
#194775 = CARTESIAN_POINT('',(-14.7050516300984,4.95951629533962E-11,127.136140320455)) ;
#194776 = CARTESIAN_POINT('',(-21.4900940692588,3.00000000004959,124.813500313073)) ;
#194777 = CARTESIAN_POINT('',(-21.4900940692588,4.95951629533962E-11,124.813500313073)) ;
#194778 = CARTESIAN_POINT('',(-14.7050516300984,3.00000000004959,127.136140320455)) ;
#194779 = CARTESIAN_POINT('Origin',(-20.6804250999186,4.95951629533962E-11,
122.448244267718)) ;
#194780 = CARTESIAN_POINT('',(-23.0892130471686,4.95951629533962E-11,121.779110032169)) ;
#194781 = CARTESIAN_POINT('Origin',(-20.6804250999186,4.95951629533962E-11,
122.448244267718)) ;
#194782 = CARTESIAN_POINT('',(-23.0892130471686,3.00000000004959,121.779110032169)) ;
#194783 = CARTESIAN_POINT('',(-23.0892130471686,4.95951629533962E-11,121.779110032169)) ;
#194784 = CARTESIAN_POINT('Origin',(-20.6804250999186,3.00000000004959,122.448244267718)) ;
#194785 = CARTESIAN_POINT('Origin',(-28.8703041205687,4.95951629533962E-11,
120.173187866852)) ;
#194786 = CARTESIAN_POINT('',(-26.1564910676883,4.95951629533962E-11,114.82199933401)) ;
#194787 = CARTESIAN_POINT('Origin',(-28.8703041205686,4.95951629533962E-11,
120.173187866852)) ;
#194788 = CARTESIAN_POINT('',(-26.1564910676883,3.00000000004959,114.82199933401)) ;
#194789 = CARTESIAN_POINT('',(-26.1564910676883,4.95951629533962E-11,114.82199933401)) ;
#194790 = CARTESIAN_POINT('Origin',(-28.8703041205686,3.00000000004959,120.173187866852)) ;
#194791 = CARTESIAN_POINT('Origin',(-25.0257356289886,4.95951629533962E-11,
112.592337445326)) ;
#194792 = CARTESIAN_POINT('',(-27.0782045465628,4.95951629533962E-11,114.019702620182)) ;
#194793 = CARTESIAN_POINT('Origin',(-25.0257356289885,4.95951629533962E-11,
112.592337445326)) ;
#194794 = CARTESIAN_POINT('',(-27.0782045465628,3.00000000004959,114.019702620182)) ;
#194795 = CARTESIAN_POINT('',(-27.0782045465628,4.95951629533962E-11,114.019702620182)) ;
#194796 = CARTESIAN_POINT('Origin',(-25.0257356289885,3.00000000004959,112.592337445326)) ;
#194797 = CARTESIAN_POINT('Ctrl Pts',(-27.0782045465628,4.95951629533962E-11,
114.019702620182)) ;
#194798 = CARTESIAN_POINT('Ctrl Pts',(-27.0782045465628,3.6000000000496,114.019702620182)) ;
#194799 = CARTESIAN_POINT('Ctrl Pts',(-43.5517103463888,4.95951629533962E-11,
90.3317500112603)) ;
#194800 = CARTESIAN_POINT('Ctrl Pts',(-43.5517103463888,3.6000000000496,90.3317500112603)) ;
#194801 = CARTESIAN_POINT('Ctrl Pts',(-57.8226594504937,4.95951629533962E-11,
65.2551572640889)) ;
#194802 = CARTESIAN_POINT('Ctrl Pts',(-57.8226594504937,3.6000000000496,65.2551572640889)) ;
#194803 = CARTESIAN_POINT('',(-57.8226594504937,4.95951629533962E-11,65.2551572640889)) ;
#194804 = CARTESIAN_POINT('Origin',(497.372422143233,4.9595162953412E-11,
-250.703267875912)) ;
#194805 = CARTESIAN_POINT('',(-57.8226594504937,3.00000000004959,65.2551572640889)) ;
#194806 = CARTESIAN_POINT('',(-57.8226594504937,4.95951629533962E-11,65.2551572640889)) ;
#194807 = CARTESIAN_POINT('Origin',(497.372422143233,3.00000000004959,-250.703267875912)) ;
#194808 = CARTESIAN_POINT('Origin',(-59.0731327528925,4.95951629533962E-11,
66.0875266199294)) ;
#194809 = CARTESIAN_POINT('',(-57.8226594504937,4.95951629533962E-11,65.2551572640889)) ;
#194810 = CARTESIAN_POINT('',(-57.8226594504937,3.00000000004959,65.2551572640889)) ;
#194811 = CARTESIAN_POINT('Origin',(-28.8703041205685,4.95951629533962E-11,
120.173187866852)) ;
#194812 = CARTESIAN_POINT('',(-27.8320398342445,3.00000000004959,121.882575848483)) ;
#194813 = CARTESIAN_POINT('Origin',(-28.8703041205685,3.00000000004959,120.173187866852)) ;
#194814 = CARTESIAN_POINT('',(-27.8320398342445,4.95951629533962E-11,121.882575848483)) ;
#194815 = CARTESIAN_POINT('',(-27.8320398342445,4.95951629533962E-11,121.882575848483)) ;
#194816 = CARTESIAN_POINT('Origin',(-28.8703041205685,4.95951629533962E-11,
120.173187866852)) ;
#194817 = CARTESIAN_POINT('Origin',(-33.9682898421303,4.95951629533962E-11,
126.55956438399)) ;
#194818 = CARTESIAN_POINT('',(-32.9683885367277,3.00000000004959,126.545515204144)) ;
#194819 = CARTESIAN_POINT('Origin',(-33.9682898421302,3.00000000004959,126.55956438399)) ;
#194820 = CARTESIAN_POINT('',(-32.9683885367277,4.95951629533962E-11,126.545515204144)) ;
#194821 = CARTESIAN_POINT('',(-32.9683885367278,4.95951629533962E-11,126.545515204144)) ;
#194822 = CARTESIAN_POINT('Origin',(-33.9682898421302,4.95951629533962E-11,
126.55956438399)) ;
#194823 = CARTESIAN_POINT('Origin',(-27.8320398342445,4.95951629533962E-11,
121.882575848483)) ;
#194824 = CARTESIAN_POINT('Origin',(-27.8320398342445,3.00000000004959,121.882575848483)) ;
#194825 = CARTESIAN_POINT('Origin',(2.26485497023532E-13,9.2000000000496,
130.056003483261)) ;
#194826 = CARTESIAN_POINT('',(4.36473211795044,-6.19999999995041,135.528581809656)) ;
#194827 = CARTESIAN_POINT('Origin',(5.55111512312578E-16,-6.19999999995041,
130.056003483261)) ;
#194828 = CARTESIAN_POINT('',(4.36473211795044,-9.1999999999504,135.528581809656)) ;
#194829 = CARTESIAN_POINT('',(4.36473211795089,9.2000000000496,135.528581809656)) ;
#194830 = CARTESIAN_POINT('Origin',(5.55111512312578E-16,-9.1999999999504,
130.056003483261)) ;
#194831 = CARTESIAN_POINT('Origin',(4.36473211795044,9.2000000000496,135.528581809656)) ;
#194832 = CARTESIAN_POINT('',(4.36473211795044,9.2000000000496,135.528581809656)) ;
#194833 = CARTESIAN_POINT('Origin',(5.55111512312578E-16,9.2000000000496,
130.056003483261)) ;
#194834 = CARTESIAN_POINT('',(-1.55739642948599,9.2000000000496,127.491921510814)) ;
#194835 = CARTESIAN_POINT('Origin',(9.54791801177635E-14,9.2000000000496,
130.056003483261)) ;
#194836 = CARTESIAN_POINT('Origin',(4.36473211795044,-9.1999999999504,135.528581809656)) ;
#194837 = CARTESIAN_POINT('',(-1.55739642948599,-9.19999999995041,127.491921510814)) ;
#194838 = CARTESIAN_POINT('Origin',(9.54791801177635E-14,-9.19999999995041,
130.056003483261)) ;
#194839 = CARTESIAN_POINT('Origin',(1.99840144432528E-14,6.2000000000496,
130.056003483261)) ;
#194840 = CARTESIAN_POINT('',(-9.59119572100644,6.2000000000496,139.904279557834)) ;
#194841 = CARTESIAN_POINT('Origin',(1.34336985979644E-13,6.2000000000496,
130.056003483261)) ;
#194842 = CARTESIAN_POINT('',(-9.59119572100644,-6.19999999995041,139.904279557834)) ;
#194843 = CARTESIAN_POINT('',(-9.59119572100651,6.2000000000496,139.904279557834)) ;
#194844 = CARTESIAN_POINT('Origin',(1.34336985979644E-13,-6.19999999995041,
130.056003483261)) ;
#194845 = CARTESIAN_POINT('Origin',(-9.59119572100644,6.2000000000496,139.904279557834)) ;
#194846 = CARTESIAN_POINT('',(4.36473211795044,6.2000000000496,135.528581809656)) ;
#194847 = CARTESIAN_POINT('Origin',(5.55111512312578E-16,6.2000000000496,
130.056003483261)) ;
#194848 = CARTESIAN_POINT('Origin',(-9.59119572100644,-6.19999999995041,139.904279557834)) ;
#194849 = CARTESIAN_POINT('Origin',(2.26485497023532E-13,9.2000000000496,
130.056003483261)) ;
#194850 = CARTESIAN_POINT('',(4.36473211795089,9.2000000000496,135.528581809656)) ;
#194851 = CARTESIAN_POINT('Origin',(3.60822483003176E-14,4.9595882956055E-11,
130.056003483261)) ;
#194852 = CARTESIAN_POINT('',(-1.55739642948599,4.9595882956055E-11,127.491921510814)) ;
#194853 = CARTESIAN_POINT('Origin',(59.7994569137529,3.00000000004983,67.2203874623164)) ;
#194854 = CARTESIAN_POINT('',(60.0566078658528,3.00000000004983,66.9917599116864)) ;
#194855 = CARTESIAN_POINT('',(59.542305961653,3.00000000004982,67.4490150129465)) ;
#194856 = CARTESIAN_POINT('',(60.0566078658528,3.00000000004983,66.9917599116864)) ;
#194857 = CARTESIAN_POINT('',(59.542305961653,-2.99999999995018,67.4490150129464)) ;
#194858 = CARTESIAN_POINT('',(59.542305961653,3.00000000004982,67.4490150129465)) ;
#194859 = CARTESIAN_POINT('',(60.0566078658528,-2.99999999995017,66.9917599116863)) ;
#194860 = CARTESIAN_POINT('',(60.0566078658528,-2.99999999995017,66.9917599116863)) ;
#194861 = CARTESIAN_POINT('',(60.0566078658528,3.00000000004983,66.9917599116864)) ;
#194862 = CARTESIAN_POINT('Ctrl Pts',(59.542305961653,3.00000000004982,67.4490150129465)) ;
#194863 = CARTESIAN_POINT('Ctrl Pts',(59.542305961653,-4.19999999995018,67.4490150129464)) ;
#194864 = CARTESIAN_POINT('Ctrl Pts',(59.5414850140413,3.00000000004983,67.447985689744)) ;
#194865 = CARTESIAN_POINT('Ctrl Pts',(59.5414850140413,-4.19999999995018,
67.447985689744)) ;
#194866 = CARTESIAN_POINT('Ctrl Pts',(59.5406625872324,3.00000000004983,67.44695754941)) ;
#194867 = CARTESIAN_POINT('Ctrl Pts',(59.5406625872324,-4.19999999995018,
67.4469575494099)) ;
#194868 = CARTESIAN_POINT('Ctrl Pts',(57.0984025861256,3.00000000004986,64.3938153283195)) ;
#194869 = CARTESIAN_POINT('Ctrl Pts',(57.0984025861256,-4.19999999995015,
64.3938153283194)) ;
#194870 = CARTESIAN_POINT('Ctrl Pts',(50.3765961969602,3.0000000000498,69.658693810807)) ;
#194871 = CARTESIAN_POINT('Ctrl Pts',(50.3765961969602,-4.1999999999502,69.6586938108069)) ;
#194872 = CARTESIAN_POINT('',(50.3765961969604,3.0000000000498,69.6586938108071)) ;
#194873 = CARTESIAN_POINT('Origin',(52.7209259427923,3.00000000004977,72.9021800116133)) ;
#194874 = CARTESIAN_POINT('',(50.3765961969604,-2.9999999999502,69.658693810807)) ;
#194875 = CARTESIAN_POINT('',(50.3765961969604,3.0000000000498,69.6586938108071)) ;
#194876 = CARTESIAN_POINT('Origin',(52.720925942792,-2.99999999995023,72.9021800116138)) ;
#194877 = CARTESIAN_POINT('Origin',(51.5487610698759,3.00000000004979,71.2804369112112)) ;
#194878 = CARTESIAN_POINT('',(52.7209259427917,3.00000000004977,72.9021800116154)) ;
#194879 = CARTESIAN_POINT('',(50.3765961969604,3.0000000000498,69.6586938108071)) ;
#194880 = CARTESIAN_POINT('',(52.7209259427917,-2.99999999995023,72.9021800116153)) ;
#194881 = CARTESIAN_POINT('',(52.7209259427917,3.00000000004977,72.9021800116154)) ;
#194882 = CARTESIAN_POINT('',(50.3765961969604,-2.9999999999502,69.658693810807)) ;
#194883 = CARTESIAN_POINT('Origin',(52.4412856039855,3.00000000004977,73.1026755227506)) ;
#194884 = CARTESIAN_POINT('',(52.1616452651796,3.00000000004977,73.3031710338859)) ;
#194885 = CARTESIAN_POINT('',(52.7209259427917,3.00000000004977,72.9021800116154)) ;
#194886 = CARTESIAN_POINT('',(52.1616452651796,-2.99999999995024,73.3031710338858)) ;
#194887 = CARTESIAN_POINT('',(52.1616452651796,3.00000000004977,73.3031710338859)) ;
#194888 = CARTESIAN_POINT('',(52.7209259427917,-2.99999999995023,72.9021800116153)) ;
#194889 = CARTESIAN_POINT('Ctrl Pts',(52.1616452651794,3.00000000004977,73.3031710338858)) ;
#194890 = CARTESIAN_POINT('Ctrl Pts',(52.1616452651794,-4.19999999995024,
73.3031710338858)) ;
#194891 = CARTESIAN_POINT('Ctrl Pts',(52.1609364083768,3.00000000004977,73.3020615370311)) ;
#194892 = CARTESIAN_POINT('Ctrl Pts',(52.1609364083768,-4.19999999995024,
73.3020615370311)) ;
#194893 = CARTESIAN_POINT('Ctrl Pts',(52.1602259568374,3.00000000004977,73.3009530619476)) ;
#194894 = CARTESIAN_POINT('Ctrl Pts',(52.1602259568374,-4.19999999995024,
73.3009530619475)) ;
#194895 = CARTESIAN_POINT('Ctrl Pts',(50.050485176063,3.0000000000498,70.0092505885835)) ;
#194896 = CARTESIAN_POINT('Ctrl Pts',(50.050485176063,-4.19999999995021,70.0092505885834)) ;
#194897 = CARTESIAN_POINT('Ctrl Pts',(42.8151718885461,3.00000000004975,74.5426674236288)) ;
#194898 = CARTESIAN_POINT('Ctrl Pts',(42.8151718885461,-4.19999999995025,
74.5426674236287)) ;
#194899 = CARTESIAN_POINT('',(42.8151718885463,3.00000000004975,74.5426674236288)) ;
#194900 = CARTESIAN_POINT('Origin',(44.8076225225366,3.00000000004971,78.0134346533848)) ;
#194901 = CARTESIAN_POINT('',(42.8151718885463,-2.99999999995025,74.5426674236287)) ;
#194902 = CARTESIAN_POINT('',(42.8151718885463,3.00000000004975,74.5426674236288)) ;
#194903 = CARTESIAN_POINT('Origin',(44.8076225225365,-2.99999999995029,78.0134346533847)) ;
#194904 = CARTESIAN_POINT('Origin',(43.8113972055423,3.00000000004974,76.2780510385053)) ;
#194905 = CARTESIAN_POINT('',(44.8076225225385,3.00000000004972,78.0134346533818)) ;
#194906 = CARTESIAN_POINT('',(42.8151718885463,3.00000000004975,74.5426674236288)) ;
#194907 = CARTESIAN_POINT('',(44.8076225225385,-2.99999999995028,78.0134346533818)) ;
#194908 = CARTESIAN_POINT('',(44.8076225225385,3.00000000004972,78.0134346533819)) ;
#194909 = CARTESIAN_POINT('',(42.8151718885463,-2.99999999995025,74.5426674236288)) ;
#194910 = CARTESIAN_POINT('Origin',(44.5085565950966,3.00000000004971,78.183601454246)) ;
#194911 = CARTESIAN_POINT('',(44.2094906676548,3.00000000004971,78.3537682551101)) ;
#194912 = CARTESIAN_POINT('',(44.8076225225385,3.00000000004972,78.0134346533819)) ;
#194913 = CARTESIAN_POINT('',(44.2094906676548,-2.99999999995029,78.35376825511)) ;
#194914 = CARTESIAN_POINT('',(44.2094906676548,3.00000000004971,78.3537682551101)) ;
#194915 = CARTESIAN_POINT('',(44.8076225225385,-2.99999999995028,78.0134346533818)) ;
#194916 = CARTESIAN_POINT('Ctrl Pts',(44.2094906676547,3.00000000004971,78.35376825511)) ;
#194917 = CARTESIAN_POINT('Ctrl Pts',(44.2094906676547,-4.19999999995029,
78.3537682551099)) ;
#194918 = CARTESIAN_POINT('Ctrl Pts',(44.2089016680448,3.00000000004971,78.3525907404827)) ;
#194919 = CARTESIAN_POINT('Ctrl Pts',(44.2089016680448,-4.19999999995029,
78.3525907404826)) ;
#194920 = CARTESIAN_POINT('Ctrl Pts',(44.2083109756305,3.00000000004971,78.3514140753339)) ;
#194921 = CARTESIAN_POINT('Ctrl Pts',(44.2083109756305,-4.19999999995029,
78.3514140753338)) ;
#194922 = CARTESIAN_POINT('Ctrl Pts',(42.4542041766734,3.00000000004975,74.8572159308281)) ;
#194923 = CARTESIAN_POINT('Ctrl Pts',(42.4542041766734,-4.19999999995026,
74.857215930828)) ;
#194924 = CARTESIAN_POINT('Ctrl Pts',(34.7846555972706,3.00000000004971,78.6095020549076)) ;
#194925 = CARTESIAN_POINT('Ctrl Pts',(34.7846555972706,-4.1999999999503,78.6095020549075)) ;
#194926 = CARTESIAN_POINT('',(34.7846555972707,3.00000000004971,78.6095020549077)) ;
#194927 = CARTESIAN_POINT('Origin',(36.4033974133286,3.00000000004968,82.2695238615344)) ;
#194928 = CARTESIAN_POINT('',(34.7846555972707,-2.99999999995029,78.6095020549076)) ;
#194929 = CARTESIAN_POINT('',(34.7846555972707,3.00000000004971,78.6095020549076)) ;
#194930 = CARTESIAN_POINT('Origin',(36.4033974133284,-2.99999999995033,82.2695238615347)) ;
#194931 = CARTESIAN_POINT('Origin',(35.5940265053006,3.00000000004969,80.4395129582195)) ;
#194932 = CARTESIAN_POINT('',(36.4033974133305,3.00000000004967,82.2695238615314)) ;
#194933 = CARTESIAN_POINT('',(34.7846555972707,3.00000000004971,78.6095020549076)) ;
#194934 = CARTESIAN_POINT('',(36.4033974133305,-2.99999999995033,82.2695238615314)) ;
#194935 = CARTESIAN_POINT('',(36.4033974133305,3.00000000004967,82.2695238615314)) ;
#194936 = CARTESIAN_POINT('',(34.7846555972707,-2.99999999995029,78.6095020549076)) ;
#194937 = CARTESIAN_POINT('Origin',(36.0881825261374,3.00000000004967,82.4074975690443)) ;
#194938 = CARTESIAN_POINT('',(35.7729676389444,3.00000000004967,82.5454712765571)) ;
#194939 = CARTESIAN_POINT('',(36.4033974133305,3.00000000004967,82.2695238615314)) ;
#194940 = CARTESIAN_POINT('',(35.7729676389444,-2.99999999995033,82.5454712765571)) ;
#194941 = CARTESIAN_POINT('',(35.7729676389443,3.00000000004967,82.5454712765571)) ;
#194942 = CARTESIAN_POINT('',(36.4033974133305,-2.99999999995033,82.2695238615314)) ;
#194943 = CARTESIAN_POINT('Ctrl Pts',(35.7729676389443,3.00000000004967,82.5454712765571)) ;
#194944 = CARTESIAN_POINT('Ctrl Pts',(35.7729676389443,-4.19999999995034,
82.545471276557)) ;
#194945 = CARTESIAN_POINT('Ctrl Pts',(35.7725049497303,3.00000000004967,82.5442386452546)) ;
#194946 = CARTESIAN_POINT('Ctrl Pts',(35.7725049497303,-4.19999999995034,
82.5442386452545)) ;
#194947 = CARTESIAN_POINT('Ctrl Pts',(35.7720404881907,3.00000000004967,82.5430066818299)) ;
#194948 = CARTESIAN_POINT('Ctrl Pts',(35.7720404881907,-4.19999999995034,
82.5430066818298)) ;
#194949 = CARTESIAN_POINT('Ctrl Pts',(34.3927860322115,3.00000000004971,78.8845960322615)) ;
#194950 = CARTESIAN_POINT('Ctrl Pts',(34.3927860322115,-4.1999999999503,78.8845960322614)) ;
#194951 = CARTESIAN_POINT('Ctrl Pts',(26.373031340114,3.00000000004968,81.8146406133832)) ;
#194952 = CARTESIAN_POINT('Ctrl Pts',(26.373031340114,-4.19999999995033,81.8146406133831)) ;
#194953 = CARTESIAN_POINT('',(26.3730313401142,3.00000000004968,81.8146406133833)) ;
#194954 = CARTESIAN_POINT('Origin',(27.6003290641584,3.00000000004964,85.6238170320596)) ;
#194955 = CARTESIAN_POINT('',(26.3730313401142,-2.99999999995032,81.8146406133832)) ;
#194956 = CARTESIAN_POINT('',(26.3730313401142,3.00000000004968,81.8146406133833)) ;
#194957 = CARTESIAN_POINT('Origin',(27.6003290641572,-2.99999999995036,85.6238170320607)) ;
#194958 = CARTESIAN_POINT('Origin',(26.9866802021375,3.00000000004966,83.7192288227197)) ;
#194959 = CARTESIAN_POINT('',(27.6003290641612,3.00000000004964,85.6238170320561)) ;
#194960 = CARTESIAN_POINT('',(26.3730313401142,3.00000000004968,81.8146406133833)) ;
#194961 = CARTESIAN_POINT('',(27.6003290641612,-2.99999999995036,85.6238170320561)) ;
#194962 = CARTESIAN_POINT('',(27.6003290641612,3.00000000004964,85.6238170320561)) ;
#194963 = CARTESIAN_POINT('',(26.3730313401142,-2.99999999995032,81.8146406133832)) ;
#194964 = CARTESIAN_POINT('Origin',(27.2724187774839,3.00000000004964,85.7280859774054)) ;
#194965 = CARTESIAN_POINT('',(26.9445084908067,3.00000000004964,85.8323549227545)) ;
#194966 = CARTESIAN_POINT('',(27.6003290641612,3.00000000004964,85.6238170320561)) ;
#194967 = CARTESIAN_POINT('',(26.9445084908067,-2.99999999995036,85.8323549227545)) ;
#194968 = CARTESIAN_POINT('',(26.9445084908067,3.00000000004964,85.8323549227546)) ;
#194969 = CARTESIAN_POINT('',(27.6003290641612,-2.99999999995036,85.6238170320561)) ;
#194970 = CARTESIAN_POINT('Ctrl Pts',(26.9445084908067,3.00000000004964,85.8323549227545)) ;
#194971 = CARTESIAN_POINT('Ctrl Pts',(26.9445084908067,-4.19999999995036,
85.8323549227544)) ;
#194972 = CARTESIAN_POINT('Ctrl Pts',(26.9441771813086,3.00000000004964,85.8310806797426)) ;
#194973 = CARTESIAN_POINT('Ctrl Pts',(26.9441771813086,-4.19999999995036,
85.8310806797425)) ;
#194974 = CARTESIAN_POINT('Ctrl Pts',(26.9438440393814,3.00000000004964,85.8298069156914)) ;
#194975 = CARTESIAN_POINT('Ctrl Pts',(26.9438440393814,-4.19999999995036,
85.8298069156913)) ;
#194976 = CARTESIAN_POINT('Ctrl Pts',(25.9545533268276,3.00000000004968,82.0472660737088)) ;
#194977 = CARTESIAN_POINT('Ctrl Pts',(25.9545533268276,-4.19999999995032,
82.0472660737087)) ;
#194978 = CARTESIAN_POINT('Ctrl Pts',(17.6724586326834,3.00000000004966,84.1229669302911)) ;
#194979 = CARTESIAN_POINT('Ctrl Pts',(17.6724586326834,-4.19999999995034,
84.122966930291)) ;
#194980 = CARTESIAN_POINT('',(17.6724586326837,3.00000000004966,84.1229669302912)) ;
#194981 = CARTESIAN_POINT('Origin',(18.494865734023,3.00000000004962,88.0395638270497)) ;
#194982 = CARTESIAN_POINT('',(17.6724586326837,-2.99999999995035,84.1229669302911)) ;
#194983 = CARTESIAN_POINT('',(17.6724586326838,3.00000000004966,84.1229669302912)) ;
#194984 = CARTESIAN_POINT('Origin',(18.4948657340247,-2.99999999995039,88.0395638270483)) ;
#194985 = CARTESIAN_POINT('Origin',(18.0836621833541,3.00000000004964,86.0812653786697)) ;
#194986 = CARTESIAN_POINT('',(18.4948657340249,3.00000000004962,88.0395638270482)) ;
#194987 = CARTESIAN_POINT('',(17.6724586326838,3.00000000004966,84.1229669302912)) ;
#194988 = CARTESIAN_POINT('',(18.4948657340249,-2.99999999995039,88.0395638270482)) ;
#194989 = CARTESIAN_POINT('',(18.4948657340249,3.00000000004962,88.0395638270483)) ;
#194990 = CARTESIAN_POINT('',(17.6724586326838,-2.99999999995035,84.1229669302912)) ;
#194991 = CARTESIAN_POINT('Origin',(18.1578527015839,3.00000000004962,88.1089856178489)) ;
#194992 = CARTESIAN_POINT('',(17.8208396691431,3.00000000004961,88.1784074086498)) ;
#194993 = CARTESIAN_POINT('',(18.4948657340249,3.00000000004962,88.0395638270483)) ;
#194994 = CARTESIAN_POINT('',(17.8208396691431,-2.99999999995039,88.1784074086497)) ;
#194995 = CARTESIAN_POINT('',(17.8208396691431,3.00000000004962,88.1784074086499)) ;
#194996 = CARTESIAN_POINT('',(18.4948657340249,-2.99999999995039,88.0395638270482)) ;
#194997 = CARTESIAN_POINT('Ctrl Pts',(17.8208396691429,3.00000000004961,88.1784074086497)) ;
#194998 = CARTESIAN_POINT('Ctrl Pts',(17.8208396691429,-4.19999999995039,
88.1784074086496)) ;
#194999 = CARTESIAN_POINT('Ctrl Pts',(17.8206433692571,3.00000000004961,88.1771055148015)) ;
#195000 = CARTESIAN_POINT('Ctrl Pts',(17.8206433692571,-4.19999999995039,
88.1771055148014)) ;
#195001 = CARTESIAN_POINT('Ctrl Pts',(17.820445196915,3.00000000004961,88.1758039057497)) ;
#195002 = CARTESIAN_POINT('Ctrl Pts',(17.820445196915,-4.19999999995039,88.1758039057496)) ;
#195003 = CARTESIAN_POINT('Ctrl Pts',(17.2319571038551,3.00000000004966,84.3105751803646)) ;
#195004 = CARTESIAN_POINT('Ctrl Pts',(17.2319571038551,-4.19999999995035,
84.3105751803645)) ;
#195005 = CARTESIAN_POINT('Ctrl Pts',(8.77826277027357,3.00000000004964,85.5091904994544)) ;
#195006 = CARTESIAN_POINT('Ctrl Pts',(8.77826277027357,-4.19999999995037,
85.5091904994543)) ;
#195007 = CARTESIAN_POINT('',(8.77826277027361,3.00000000004964,85.5091904994544)) ;
#195008 = CARTESIAN_POINT('Origin',(9.18676878460585,3.0000000000496,89.490296819095)) ;
#195009 = CARTESIAN_POINT('',(8.77826277027361,-2.99999999995036,85.5091904994543)) ;
#195010 = CARTESIAN_POINT('',(8.77826277027362,3.00000000004964,85.5091904994544)) ;
#195011 = CARTESIAN_POINT('Origin',(9.18676878460804,-2.99999999995041,89.4902968190937)) ;
#195012 = CARTESIAN_POINT('Origin',(8.98251577744044,3.00000000004962,87.4997436592745)) ;
#195013 = CARTESIAN_POINT('',(9.18676878460724,3.0000000000496,89.4902968190945)) ;
#195014 = CARTESIAN_POINT('',(8.77826277027362,3.00000000004964,85.5091904994544)) ;
#195015 = CARTESIAN_POINT('',(9.18676878460724,-2.9999999999504,89.4902968190944)) ;
#195016 = CARTESIAN_POINT('',(9.18676878460724,3.0000000000496,89.4902968190945)) ;
#195017 = CARTESIAN_POINT('',(8.77826277027362,-2.99999999995036,85.5091904994543)) ;
#195018 = CARTESIAN_POINT('Origin',(8.84434539171061,3.0000000000496,89.5241108556793)) ;
#195019 = CARTESIAN_POINT('',(8.50192199881383,3.0000000000496,89.5579248922642)) ;
#195020 = CARTESIAN_POINT('',(9.18676878460724,3.0000000000496,89.4902968190945)) ;
#195021 = CARTESIAN_POINT('',(8.50192199881383,-2.9999999999504,89.5579248922642)) ;
#195022 = CARTESIAN_POINT('',(8.50192199881383,3.0000000000496,89.5579248922642)) ;
#195023 = CARTESIAN_POINT('',(9.18676878460724,-2.9999999999504,89.4902968190944)) ;
#195024 = CARTESIAN_POINT('Ctrl Pts',(8.50192199881385,3.0000000000496,89.5579248922642)) ;
#195025 = CARTESIAN_POINT('Ctrl Pts',(8.50192199881385,-4.19999999995041,
89.5579248922641)) ;
#195026 = CARTESIAN_POINT('Ctrl Pts',(8.50186285924251,3.0000000000496,89.5566096114014)) ;
#195027 = CARTESIAN_POINT('Ctrl Pts',(8.50186285924251,-4.19999999995041,
89.5566096114013)) ;
#195028 = CARTESIAN_POINT('Ctrl Pts',(8.50180182770343,3.0000000000496,89.5552944180496)) ;
#195029 = CARTESIAN_POINT('Ctrl Pts',(8.50180182770343,-4.19999999995041,
89.5552944180495)) ;
#195030 = CARTESIAN_POINT('Ctrl Pts',(8.32056395283395,3.00000000004964,85.6497260640287)) ;
#195031 = CARTESIAN_POINT('Ctrl Pts',(8.32056395283395,-4.19999999995037,
85.6497260640286)) ;
#195032 = CARTESIAN_POINT('Ctrl Pts',(-0.212109576016898,3.00000000004964,
85.9581235653636)) ;
#195033 = CARTESIAN_POINT('Ctrl Pts',(-0.212109576016898,-4.19999999995037,
85.9581235653635)) ;
#195034 = CARTESIAN_POINT('',(-0.212109576016928,3.00000000004964,85.9581235653636)) ;
#195035 = CARTESIAN_POINT('Origin',(-0.221980326067951,3.00000000004959,89.9601214739474)) ;
#195036 = CARTESIAN_POINT('',(-0.212109576016928,-2.99999999995036,85.9581235653635)) ;
#195037 = CARTESIAN_POINT('',(-0.212109576016928,3.00000000004963,85.9581235653635)) ;
#195038 = CARTESIAN_POINT('Origin',(-0.221980326066147,-2.99999999995041,
89.9601214739464)) ;
#195039 = CARTESIAN_POINT('Origin',(-0.217044951043372,3.00000000004962,87.9591225196562)) ;
#195040 = CARTESIAN_POINT('',(-0.221980326069911,3.00000000004959,89.9601214739486)) ;
#195041 = CARTESIAN_POINT('',(-0.212109576016928,3.00000000004963,85.9581235653635)) ;
#195042 = CARTESIAN_POINT('',(-0.221980326069911,-2.9999999999504,89.9601214739485)) ;
#195043 = CARTESIAN_POINT('',(-0.221980326069911,3.00000000004959,89.9601214739485)) ;
#195044 = CARTESIAN_POINT('',(-0.212109576016928,-2.99999999995036,85.9581235653634)) ;
#195045 = CARTESIAN_POINT('Origin',(-0.566062417072776,3.0000000000496,89.9579572826566)) ;
#195046 = CARTESIAN_POINT('',(-0.91014450807586,3.00000000004959,89.9557930913646)) ;
#195047 = CARTESIAN_POINT('',(-0.221980326069911,3.00000000004959,89.9601214739485)) ;
#195048 = CARTESIAN_POINT('',(-0.91014450807586,-2.9999999999504,89.9557930913645)) ;
#195049 = CARTESIAN_POINT('',(-0.910144508075859,3.00000000004959,89.9557930913646)) ;
#195050 = CARTESIAN_POINT('',(-0.221980326069911,-2.9999999999504,89.9601214739484)) ;
#195051 = CARTESIAN_POINT('Ctrl Pts',(-0.91014450807588,3.0000000000496,89.9557930913647)) ;
#195052 = CARTESIAN_POINT('Ctrl Pts',(-0.91014450807588,-4.1999999999504,
89.9557930913646)) ;
#195053 = CARTESIAN_POINT('Ctrl Pts',(-0.910065839387319,3.0000000000496,
89.9544788339794)) ;
#195054 = CARTESIAN_POINT('Ctrl Pts',(-0.910065839387319,-4.1999999999504,
89.9544788339793)) ;
#195055 = CARTESIAN_POINT('Ctrl Pts',(-0.909989061449521,3.0000000000496,
89.9531644658614)) ;
#195056 = CARTESIAN_POINT('Ctrl Pts',(-0.909989061449521,-4.19999999995041,
89.9531644658614)) ;
#195057 = CARTESIAN_POINT('Ctrl Pts',(-0.681991038044035,3.00000000004963,
86.0500467073845)) ;
#195058 = CARTESIAN_POINT('Ctrl Pts',(-0.681991038044035,-4.19999999995037,
86.0500467073845)) ;
#195059 = CARTESIAN_POINT('Ctrl Pts',(-9.20015800540569,3.00000000004964,
85.4648475234035)) ;
#195060 = CARTESIAN_POINT('Ctrl Pts',(-9.20015800540569,-4.19999999995036,
85.4648475234034)) ;
#195061 = CARTESIAN_POINT('',(-9.2001580054058,3.00000000004964,85.4648475234036)) ;
#195062 = CARTESIAN_POINT('Origin',(-9.62829737384348,3.0000000000496,89.4438902943758)) ;
#195063 = CARTESIAN_POINT('',(-9.2001580054058,-2.99999999995036,85.4648475234035)) ;
#195064 = CARTESIAN_POINT('',(-9.2001580054058,3.00000000004964,85.4648475234036)) ;
#195065 = CARTESIAN_POINT('Origin',(-9.62829737384347,-2.9999999999504,89.4438902943758)) ;
#195066 = CARTESIAN_POINT('Origin',(-9.41422768962381,3.00000000004962,87.4543689088892)) ;
#195067 = CARTESIAN_POINT('',(-9.62829737384186,3.0000000000496,89.443890294375)) ;
#195068 = CARTESIAN_POINT('',(-9.2001580054058,3.00000000004964,85.4648475234036)) ;
#195069 = CARTESIAN_POINT('',(-9.62829737384186,-2.9999999999504,89.443890294375)) ;
#195070 = CARTESIAN_POINT('',(-9.62829737384186,3.0000000000496,89.443890294375)) ;
#195071 = CARTESIAN_POINT('',(-9.2001580054058,-2.99999999995036,85.4648475234035)) ;
#195072 = CARTESIAN_POINT('Origin',(-9.97026832755854,3.0000000000496,89.4057715865388)) ;
#195073 = CARTESIAN_POINT('',(-10.3122392812752,3.0000000000496,89.3676528787028)) ;
#195074 = CARTESIAN_POINT('',(-9.62829737384186,3.0000000000496,89.443890294375)) ;
#195075 = CARTESIAN_POINT('',(-10.3122392812752,-2.9999999999504,89.3676528787027)) ;
#195076 = CARTESIAN_POINT('',(-10.3122392812752,3.0000000000496,89.3676528787028)) ;
#195077 = CARTESIAN_POINT('',(-9.62829737384186,-2.9999999999504,89.443890294375)) ;
#195078 = CARTESIAN_POINT('Ctrl Pts',(-10.3122392812751,3.0000000000496,89.3676528787027)) ;
#195079 = CARTESIAN_POINT('Ctrl Pts',(-10.3122392812751,-4.19999999995041,
89.3676528787026)) ;
#195080 = CARTESIAN_POINT('Ctrl Pts',(-10.3120236662372,3.0000000000496,89.3663540440742)) ;
#195081 = CARTESIAN_POINT('Ctrl Pts',(-10.3120236662372,-4.19999999995041,
89.3663540440741)) ;
#195082 = CARTESIAN_POINT('Ctrl Pts',(-10.3118099200173,3.0000000000496,89.3650549016823)) ;
#195083 = CARTESIAN_POINT('Ctrl Pts',(-10.3118099200173,-4.19999999995041,
89.3650549016822)) ;
#195084 = CARTESIAN_POINT('Ctrl Pts',(-9.67707399239374,3.00000000004964,
85.5071511136907)) ;
#195085 = CARTESIAN_POINT('Ctrl Pts',(-9.67707399239374,-4.19999999995037,
85.5071511136907)) ;
#195086 = CARTESIAN_POINT('Ctrl Pts',(-18.0874075784306,3.00000000004966,
84.0347668091144)) ;
#195087 = CARTESIAN_POINT('Ctrl Pts',(-18.0874075784306,-4.19999999995035,
84.0347668091143)) ;
#195088 = CARTESIAN_POINT('',(-18.0874075784307,3.00000000004966,84.0347668091144)) ;
#195089 = CARTESIAN_POINT('Origin',(-18.9291247807382,3.00000000004961,87.9472592172066)) ;
#195090 = CARTESIAN_POINT('',(-18.0874075784307,-2.99999999995034,84.0347668091144)) ;
#195091 = CARTESIAN_POINT('',(-18.0874075784307,3.00000000004966,84.0347668091144)) ;
#195092 = CARTESIAN_POINT('Origin',(-18.9291247807369,-2.99999999995038,87.9472592172062)) ;
#195093 = CARTESIAN_POINT('Origin',(-18.5082661795829,3.00000000004964,85.9910130131597)) ;
#195094 = CARTESIAN_POINT('',(-18.9291247807354,3.00000000004962,87.9472592172052)) ;
#195095 = CARTESIAN_POINT('',(-18.0874075784307,3.00000000004966,84.0347668091144)) ;
#195096 = CARTESIAN_POINT('',(-18.9291247807354,-2.99999999995038,87.9472592172051)) ;
#195097 = CARTESIAN_POINT('',(-18.9291247807354,3.00000000004962,87.9472592172052)) ;
#195098 = CARTESIAN_POINT('',(-18.0874075784307,-2.99999999995034,84.0347668091144)) ;
#195099 = CARTESIAN_POINT('Origin',(-19.2652378918346,3.00000000004962,87.8736036293648)) ;
#195100 = CARTESIAN_POINT('',(-19.6013510029339,3.00000000004962,87.7999480415246)) ;
#195101 = CARTESIAN_POINT('',(-18.9291247807354,3.00000000004962,87.9472592172052)) ;
#195102 = CARTESIAN_POINT('',(-19.6013510029339,-2.99999999995038,87.7999480415245)) ;
#195103 = CARTESIAN_POINT('',(-19.6013510029339,3.00000000004962,87.7999480415246)) ;
#195104 = CARTESIAN_POINT('',(-18.9291247807354,-2.99999999995038,87.9472592172051)) ;
#195105 = CARTESIAN_POINT('Ctrl Pts',(-19.6013510029339,3.00000000004962,
87.7999480415246)) ;
#195106 = CARTESIAN_POINT('Ctrl Pts',(-19.6013510029339,-4.1999999999504,
87.7999480415245)) ;
#195107 = CARTESIAN_POINT('Ctrl Pts',(-19.6010008038698,3.00000000004962,
87.7986788599565)) ;
#195108 = CARTESIAN_POINT('Ctrl Pts',(-19.6010008038698,-4.19999999995039,
87.7986788599564)) ;
#195109 = CARTESIAN_POINT('Ctrl Pts',(-19.6006524312165,3.00000000004962,
87.7974091769667)) ;
#195110 = CARTESIAN_POINT('Ctrl Pts',(-19.6006524312165,-4.1999999999504,
87.7974091769666)) ;
#195111 = CARTESIAN_POINT('Ctrl Pts',(-18.5661328990248,3.00000000004966,
84.0269873606799)) ;
#195112 = CARTESIAN_POINT('Ctrl Pts',(-18.5661328990248,-4.19999999995036,
84.0269873606798)) ;
#195113 = CARTESIAN_POINT('Ctrl Pts',(-26.7764877289929,3.00000000004968,
81.6835496860654)) ;
#195114 = CARTESIAN_POINT('Ctrl Pts',(-26.7764877289929,-4.19999999995033,
81.6835496860653)) ;
#195115 = CARTESIAN_POINT('',(-26.7764877289929,3.00000000004968,81.6835496860653)) ;
#195116 = CARTESIAN_POINT('Origin',(-28.0225607353604,3.00000000004964,85.4866256457122)) ;
#195117 = CARTESIAN_POINT('',(-26.7764877289929,-2.99999999995032,81.6835496860653)) ;
#195118 = CARTESIAN_POINT('',(-26.7764877289929,3.00000000004968,81.6835496860653)) ;
#195119 = CARTESIAN_POINT('Origin',(-28.0225607353587,-2.99999999995036,85.4866256457119)) ;
#195120 = CARTESIAN_POINT('Origin',(-27.3995242321751,3.00000000004966,83.5850876658882)) ;
#195121 = CARTESIAN_POINT('',(-28.0225607353573,3.00000000004964,85.4866256457111)) ;
#195122 = CARTESIAN_POINT('',(-26.7764877289929,3.00000000004968,81.6835496860653)) ;
#195123 = CARTESIAN_POINT('',(-28.0225607353573,-2.99999999995036,85.486625645711)) ;
#195124 = CARTESIAN_POINT('',(-28.0225607353573,3.00000000004964,85.4866256457111)) ;
#195125 = CARTESIAN_POINT('',(-26.7764877289929,-2.99999999995032,81.6835496860653)) ;
#195126 = CARTESIAN_POINT('Origin',(-28.3491334782579,3.00000000004964,85.3782401639004)) ;
#195127 = CARTESIAN_POINT('',(-28.6757062211584,3.00000000004964,85.2698546820896)) ;
#195128 = CARTESIAN_POINT('',(-28.0225607353573,3.00000000004964,85.4866256457111)) ;
#195129 = CARTESIAN_POINT('',(-28.6757062211584,-2.99999999995036,85.2698546820896)) ;
#195130 = CARTESIAN_POINT('',(-28.6757062211584,3.00000000004964,85.2698546820896)) ;
#195131 = CARTESIAN_POINT('',(-28.0225607353573,-2.99999999995036,85.486625645711)) ;
#195132 = CARTESIAN_POINT('Ctrl Pts',(-28.6757062211583,3.00000000004964,
85.2698546820896)) ;
#195133 = CARTESIAN_POINT('Ctrl Pts',(-28.6757062211583,-4.1999999999504,
85.2698546820895)) ;
#195134 = CARTESIAN_POINT('Ctrl Pts',(-28.6752252749224,3.00000000004964,
85.2686290590011)) ;
#195135 = CARTESIAN_POINT('Ctrl Pts',(-28.6752252749224,-4.1999999999504,
85.268629059001)) ;
#195136 = CARTESIAN_POINT('Ctrl Pts',(-28.6747460926791,3.00000000004964,
85.2674027463255)) ;
#195137 = CARTESIAN_POINT('Ctrl Pts',(-28.6747460926791,-4.1999999999504,
85.2674027463254)) ;
#195138 = CARTESIAN_POINT('Ctrl Pts',(-27.2517773684014,3.00000000004968,
81.6257724321745)) ;
#195139 = CARTESIAN_POINT('Ctrl Pts',(-27.2517773684014,-4.19999999995036,
81.6257724321744)) ;
#195140 = CARTESIAN_POINT('Ctrl Pts',(-35.172199076656,3.00000000004971,78.4369565810807)) ;
#195141 = CARTESIAN_POINT('Ctrl Pts',(-35.172199076656,-4.19999999995033,
78.4369565810806)) ;
#195142 = CARTESIAN_POINT('',(-35.1721990766561,3.00000000004971,78.4369565810808)) ;
#195143 = CARTESIAN_POINT('Origin',(-36.8089756504653,3.00000000004967,82.0889487962232)) ;
#195144 = CARTESIAN_POINT('',(-35.1721990766561,-2.99999999995029,78.4369565810807)) ;
#195145 = CARTESIAN_POINT('',(-35.1721990766561,3.00000000004971,78.4369565810808)) ;
#195146 = CARTESIAN_POINT('Origin',(-36.8089756504651,-2.99999999995032,82.0889487962231)) ;
#195147 = CARTESIAN_POINT('Origin',(-35.9905873635603,3.0000000000497,80.2629526886517)) ;
#195148 = CARTESIAN_POINT('',(-36.8089756504645,3.00000000004968,82.0889487962226)) ;
#195149 = CARTESIAN_POINT('',(-35.1721990766561,3.00000000004971,78.4369565810808)) ;
#195150 = CARTESIAN_POINT('',(-36.8089756504645,-2.99999999995033,82.0889487962225)) ;
#195151 = CARTESIAN_POINT('',(-36.8089756504645,3.00000000004968,82.0889487962226)) ;
#195152 = CARTESIAN_POINT('',(-35.1721990766561,-2.99999999995029,78.4369565810807)) ;
#195153 = CARTESIAN_POINT('Origin',(-37.1224300258554,3.00000000004968,81.9470209144612)) ;
#195154 = CARTESIAN_POINT('',(-37.4358844012463,3.00000000004968,81.8050930326999)) ;
#195155 = CARTESIAN_POINT('',(-36.8089756504645,3.00000000004968,82.0889487962226)) ;
#195156 = CARTESIAN_POINT('',(-37.4358844012463,-2.99999999995032,81.8050930326999)) ;
#195157 = CARTESIAN_POINT('',(-37.4358844012463,3.00000000004968,81.8050930326999)) ;
#195158 = CARTESIAN_POINT('',(-36.8089756504645,-2.99999999995033,82.0889487962225)) ;
#195159 = CARTESIAN_POINT('Ctrl Pts',(-37.4358844012462,3.00000000004968,
81.8050930326999)) ;
#195160 = CARTESIAN_POINT('Ctrl Pts',(-37.4358844012462,-4.19999999995034,
81.8050930326998)) ;
#195161 = CARTESIAN_POINT('Ctrl Pts',(-37.4352779771863,3.00000000004968,
81.8039243962738)) ;
#195162 = CARTESIAN_POINT('Ctrl Pts',(-37.4352779771863,-4.19999999995034,
81.8039243962737)) ;
#195163 = CARTESIAN_POINT('Ctrl Pts',(-37.4346732353739,3.00000000004968,
81.8027548896506)) ;
#195164 = CARTESIAN_POINT('Ctrl Pts',(-37.4346732353739,-4.19999999995034,
81.8027548896505)) ;
#195165 = CARTESIAN_POINT('Ctrl Pts',(-35.6388456621282,3.00000000004971,
78.3298145414176)) ;
#195166 = CARTESIAN_POINT('Ctrl Pts',(-35.6388456621282,-4.1999999999503,
78.3298145414175)) ;
#195167 = CARTESIAN_POINT('Ctrl Pts',(-43.1825564509794,3.00000000004975,
74.3305578476115)) ;
#195168 = CARTESIAN_POINT('Ctrl Pts',(-43.1825564509794,-4.19999999995026,
74.3305578476115)) ;
#195169 = CARTESIAN_POINT('',(-43.1825564509793,3.00000000004975,74.3305578476115)) ;
#195170 = CARTESIAN_POINT('Origin',(-45.1921037255759,3.00000000004972,77.7914543273124)) ;
#195171 = CARTESIAN_POINT('',(-43.1825564509793,-2.99999999995025,74.3305578476114)) ;
#195172 = CARTESIAN_POINT('',(-43.1825564509793,3.00000000004975,74.3305578476115)) ;
#195173 = CARTESIAN_POINT('Origin',(-45.1921037255757,-2.99999999995028,77.7914543273123)) ;
#195174 = CARTESIAN_POINT('Origin',(-44.1873300882757,3.00000000004974,76.0610060874618)) ;
#195175 = CARTESIAN_POINT('',(-45.192103725572,3.00000000004972,77.7914543273121)) ;
#195176 = CARTESIAN_POINT('',(-43.1825564509793,3.00000000004975,74.3305578476115)) ;
#195177 = CARTESIAN_POINT('',(-45.192103725572,-2.99999999995028,77.791454327312)) ;
#195178 = CARTESIAN_POINT('',(-45.192103725572,3.00000000004972,77.791454327312)) ;
#195179 = CARTESIAN_POINT('',(-43.1825564509793,-2.99999999995025,74.3305578476114)) ;
#195180 = CARTESIAN_POINT('Origin',(-45.489005461722,3.00000000004972,77.617539037173)) ;
#195181 = CARTESIAN_POINT('',(-45.7859071978719,3.00000000004972,77.443623747034)) ;
#195182 = CARTESIAN_POINT('',(-45.192103725572,3.00000000004972,77.791454327312)) ;
#195183 = CARTESIAN_POINT('',(-45.7859071978719,-2.99999999995028,77.4436237470339)) ;
#195184 = CARTESIAN_POINT('',(-45.7859071978719,3.00000000004972,77.4436237470339)) ;
#195185 = CARTESIAN_POINT('',(-45.192103725572,-2.99999999995028,77.791454327312)) ;
#195186 = CARTESIAN_POINT('Ctrl Pts',(-45.7859071978719,3.00000000004972,
77.443623747034)) ;
#195187 = CARTESIAN_POINT('Ctrl Pts',(-45.7859071978719,-4.19999999995028,
77.443623747034)) ;
#195188 = CARTESIAN_POINT('Ctrl Pts',(-45.7851819400964,3.00000000004972,
77.4425249010956)) ;
#195189 = CARTESIAN_POINT('Ctrl Pts',(-45.7851819400964,-4.19999999995028,
77.4425249010955)) ;
#195190 = CARTESIAN_POINT('Ctrl Pts',(-45.7844582643927,3.00000000004972,
77.4414250138846)) ;
#195191 = CARTESIAN_POINT('Ctrl Pts',(-45.7844582643927,-4.19999999995028,
77.4414250138846)) ;
#195192 = CARTESIAN_POINT('Ctrl Pts',(-43.6354473048728,3.00000000004976,
74.1752248927841)) ;
#195193 = CARTESIAN_POINT('Ctrl Pts',(-43.6354473048728,-4.19999999995024,
74.175224892784)) ;
#195194 = CARTESIAN_POINT('Ctrl Pts',(-50.7197967002948,3.00000000004981,
69.4093440495017)) ;
#195195 = CARTESIAN_POINT('Ctrl Pts',(-50.7197967002948,-4.1999999999502,
69.4093440495016)) ;
#195196 = CARTESIAN_POINT('',(-50.7197967002948,3.00000000004981,69.4093440495017)) ;
#195197 = CARTESIAN_POINT('Origin',(-53.0800976552041,3.00000000004977,72.64122648769)) ;
#195198 = CARTESIAN_POINT('',(-50.7197967002948,-2.9999999999502,69.4093440495017)) ;
#195199 = CARTESIAN_POINT('',(-50.7197967002948,3.00000000004981,69.4093440495017)) ;
#195200 = CARTESIAN_POINT('Origin',(-53.0800976552046,-2.99999999995023,72.6412264876899)) ;
#195201 = CARTESIAN_POINT('Origin',(-51.8999471777507,3.00000000004979,71.0252852685956)) ;
#195202 = CARTESIAN_POINT('',(-53.0800976552065,3.00000000004977,72.6412264876896)) ;
#195203 = CARTESIAN_POINT('',(-50.7197967002948,3.00000000004981,69.4093440495017)) ;
#195204 = CARTESIAN_POINT('',(-53.0800976552065,-2.99999999995023,72.6412264876895)) ;
#195205 = CARTESIAN_POINT('',(-53.0800976552065,3.00000000004977,72.6412264876896)) ;
#195206 = CARTESIAN_POINT('',(-50.7197967002948,-2.9999999999502,69.4093440495017)) ;
#195207 = CARTESIAN_POINT('Origin',(-53.3571938345634,3.00000000004977,72.4372292414858)) ;
#195208 = CARTESIAN_POINT('',(-53.6342900139203,3.00000000004978,72.2332319952821)) ;
#195209 = CARTESIAN_POINT('',(-53.0800976552065,3.00000000004977,72.6412264876896)) ;
#195210 = CARTESIAN_POINT('',(-53.6342900139203,-2.99999999995022,72.233231995282)) ;
#195211 = CARTESIAN_POINT('',(-53.6342900139203,3.00000000004978,72.2332319952821)) ;
#195212 = CARTESIAN_POINT('',(-53.0800976552065,-2.99999999995023,72.6412264876895)) ;
#195213 = CARTESIAN_POINT('Ctrl Pts',(-53.6342900139204,3.00000000004978,
72.233231995282)) ;
#195214 = CARTESIAN_POINT('Ctrl Pts',(-53.6342900139204,-4.19999999995022,
72.2332319952819)) ;
#195215 = CARTESIAN_POINT('Ctrl Pts',(-53.6334538685056,3.00000000004978,
72.2322149790174)) ;
#195216 = CARTESIAN_POINT('Ctrl Pts',(-53.6334538685056,-4.19999999995023,
72.2322149790173)) ;
#195217 = CARTESIAN_POINT('Ctrl Pts',(-53.6326191876533,3.00000000004978,
72.2311967618127)) ;
#195218 = CARTESIAN_POINT('Ctrl Pts',(-53.6326191876533,-4.19999999995023,
72.2311967618126)) ;
#195219 = CARTESIAN_POINT('Ctrl Pts',(-51.1539698556413,3.00000000004981,
69.2075220398674)) ;
#195220 = CARTESIAN_POINT('Ctrl Pts',(-51.1539698556413,-4.19999999995019,
69.2075220398673)) ;
#195221 = CARTESIAN_POINT('Ctrl Pts',(-57.7013402431623,3.00000000004986,
63.7272330349523)) ;
#195222 = CARTESIAN_POINT('Ctrl Pts',(-57.7013402431623,-4.19999999995014,
63.7272330349523)) ;
#195223 = CARTESIAN_POINT('',(-57.7013402431622,3.00000000004986,63.7272330349524)) ;
#195224 = CARTESIAN_POINT('Origin',(-60.3865349272081,3.00000000004984,66.6946922513203)) ;
#195225 = CARTESIAN_POINT('',(-57.7013402431622,-2.99999999995014,63.7272330349524)) ;
#195226 = CARTESIAN_POINT('',(-57.7013402431622,3.00000000004986,63.7272330349524)) ;
#195227 = CARTESIAN_POINT('Origin',(-60.3865349272089,-2.99999999995017,66.69469225132)) ;
#195228 = CARTESIAN_POINT('Origin',(-59.0439375851841,3.00000000004985,65.2109626431365)) ;
#195229 = CARTESIAN_POINT('',(-60.3865349272058,3.00000000004983,66.6946922513205)) ;
#195230 = CARTESIAN_POINT('',(-57.7013402431622,3.00000000004986,63.7272330349524)) ;
#195231 = CARTESIAN_POINT('',(-60.3865349272058,-2.99999999995017,66.6946922513204)) ;
#195232 = CARTESIAN_POINT('',(-60.3865349272058,3.00000000004983,66.6946922513205)) ;
#195233 = CARTESIAN_POINT('',(-57.7013402431622,-2.99999999995014,63.7272330349524)) ;
#195234 = CARTESIAN_POINT('Origin',(-60.6407896260427,3.00000000004984,66.4628480855705)) ;
#195235 = CARTESIAN_POINT('',(-60.8950443248795,3.00000000004984,66.2310039198205)) ;
#195236 = CARTESIAN_POINT('',(-60.3865349272058,3.00000000004983,66.6946922513205)) ;
#195237 = CARTESIAN_POINT('',(-60.8950443248795,-2.99999999995016,66.2310039198205)) ;
#195238 = CARTESIAN_POINT('',(-60.8950443248795,3.00000000004984,66.2310039198205)) ;
#195239 = CARTESIAN_POINT('',(-60.3865349272058,-2.99999999995017,66.6946922513204)) ;
#195240 = CARTESIAN_POINT('Ctrl Pts',(-60.8950443248795,3.00000000004984,
66.2310039198205)) ;
#195241 = CARTESIAN_POINT('Ctrl Pts',(-60.8950443248795,-4.19999999995016,
66.2310039198204)) ;
#195242 = CARTESIAN_POINT('Ctrl Pts',(-60.8941064528096,3.00000000004984,
66.2300798758727)) ;
#195243 = CARTESIAN_POINT('Ctrl Pts',(-60.8941064528096,-4.19999999995016,
66.2300798758727)) ;
#195244 = CARTESIAN_POINT('Ctrl Pts',(-60.8931699117466,3.00000000004984,
66.2291544844751)) ;
#195245 = CARTESIAN_POINT('Ctrl Pts',(-60.8931699117466,-4.19999999995016,
66.2291544844751)) ;
#195246 = CARTESIAN_POINT('Ctrl Pts',(-58.112038808014,3.00000000004987,63.4811331746838)) ;
#195247 = CARTESIAN_POINT('Ctrl Pts',(-58.112038808014,-4.19999999995014,
63.4811331746838)) ;
#195248 = CARTESIAN_POINT('Ctrl Pts',(-64.0506958275439,3.00000000004993,
57.3464792012979)) ;
#195249 = CARTESIAN_POINT('Ctrl Pts',(-64.0506958275439,-4.19999999995007,
57.3464792012979)) ;
#195250 = CARTESIAN_POINT('',(-64.050695827544,3.00000000004993,57.346479201298)) ;
#195251 = CARTESIAN_POINT('Origin',(-67.0313646858506,3.0000000000499,60.0170030916901)) ;
#195252 = CARTESIAN_POINT('',(-64.050695827544,-2.99999999995007,57.3464792012979)) ;
#195253 = CARTESIAN_POINT('',(-64.050695827544,3.00000000004993,57.3464792012979)) ;
#195254 = CARTESIAN_POINT('Origin',(-67.0313646858511,-2.9999999999501,60.0170030916897)) ;
#195255 = CARTESIAN_POINT('Origin',(-65.5410302566959,3.00000000004991,58.6817411464945)) ;
#195256 = CARTESIAN_POINT('',(-67.0313646858481,3.0000000000499,60.017003091691)) ;
#195257 = CARTESIAN_POINT('',(-64.050695827544,3.00000000004993,57.3464792012979)) ;
#195258 = CARTESIAN_POINT('',(-67.0313646858481,-2.9999999999501,60.017003091691)) ;
#195259 = CARTESIAN_POINT('',(-67.0313646858481,3.0000000000499,60.017003091691)) ;
#195260 = CARTESIAN_POINT('',(-64.050695827544,-2.99999999995007,57.3464792012979)) ;
#195261 = CARTESIAN_POINT('Origin',(-67.2599922364783,3.0000000000499,59.7598521395911)) ;
#195262 = CARTESIAN_POINT('',(-67.4886197871086,3.00000000004991,59.5027011874913)) ;
#195263 = CARTESIAN_POINT('',(-67.0313646858481,3.0000000000499,60.017003091691)) ;
#195264 = CARTESIAN_POINT('',(-67.4886197871086,-2.99999999995009,59.5027011874912)) ;
#195265 = CARTESIAN_POINT('',(-67.4886197871085,3.00000000004991,59.5027011874913)) ;
#195266 = CARTESIAN_POINT('',(-67.0313646858481,-2.9999999999501,60.0170030916909)) ;
#195267 = CARTESIAN_POINT('Ctrl Pts',(-67.4886197871085,3.0000000000499,59.5027011874913)) ;
#195268 = CARTESIAN_POINT('Ctrl Pts',(-67.4886197871085,-4.1999999999501,
59.5027011874912)) ;
#195269 = CARTESIAN_POINT('Ctrl Pts',(-67.4875904639056,3.00000000004991,
59.5018802398793)) ;
#195270 = CARTESIAN_POINT('Ctrl Pts',(-67.4875904639056,-4.1999999999501,
59.5018802398792)) ;
#195271 = CARTESIAN_POINT('Ctrl Pts',(-67.4865623235721,3.00000000004991,
59.5010578130706)) ;
#195272 = CARTESIAN_POINT('Ctrl Pts',(-67.4865623235721,-4.19999999995009,
59.5010578130705)) ;
#195273 = CARTESIAN_POINT('Ctrl Pts',(-64.4334201024814,3.00000000004993,
57.0587978119635)) ;
#195274 = CARTESIAN_POINT('Ctrl Pts',(-64.4334201024814,-4.19999999995007,
57.0587978119634)) ;
#195275 = CARTESIAN_POINT('Ctrl Pts',(-69.6982985849688,3.00000000005,50.3369914227983)) ;
#195276 = CARTESIAN_POINT('Ctrl Pts',(-69.6982985849688,-4.19999999995,50.3369914227982)) ;
#195277 = CARTESIAN_POINT('',(-69.6982985849687,3.00000000005,50.3369914227984)) ;
#195278 = CARTESIAN_POINT('Origin',(-72.9417847857762,3.00000000004998,52.6813211686304)) ;
#195279 = CARTESIAN_POINT('',(-69.6982985849687,-2.99999999995,50.3369914227983)) ;
#195280 = CARTESIAN_POINT('',(-69.6982985849687,3.00000000005,50.3369914227984)) ;
#195281 = CARTESIAN_POINT('Origin',(-72.9417847857764,-2.99999999995003,52.6813211686303)) ;
#195282 = CARTESIAN_POINT('Origin',(-71.3200416853732,3.00000000004999,51.509156295714)) ;
#195283 = CARTESIAN_POINT('',(-72.9417847857773,3.00000000004998,52.6813211686299)) ;
#195284 = CARTESIAN_POINT('',(-69.6982985849687,3.00000000005,50.3369914227984)) ;
#195285 = CARTESIAN_POINT('',(-72.9417847857773,-2.99999999995002,52.6813211686298)) ;
#195286 = CARTESIAN_POINT('',(-72.9417847857773,3.00000000004998,52.6813211686299)) ;
#195287 = CARTESIAN_POINT('',(-69.6982985849687,-2.99999999995,50.3369914227983)) ;
#195288 = CARTESIAN_POINT('Origin',(-73.1422802969127,3.00000000004998,52.4016808298238)) ;
#195289 = CARTESIAN_POINT('',(-73.3427758080476,3.00000000004998,52.1220404910179)) ;
#195290 = CARTESIAN_POINT('',(-72.9417847857773,3.00000000004998,52.6813211686299)) ;
#195291 = CARTESIAN_POINT('',(-73.3427758080476,-2.99999999995002,52.1220404910178)) ;
#195292 = CARTESIAN_POINT('',(-73.3427758080477,3.00000000004998,52.1220404910179)) ;
#195293 = CARTESIAN_POINT('',(-72.9417847857773,-2.99999999995003,52.6813211686298)) ;
#195294 = CARTESIAN_POINT('Ctrl Pts',(-73.3427758080479,3.00000000004998,
52.1220404910178)) ;
#195295 = CARTESIAN_POINT('Ctrl Pts',(-73.3427758080479,-4.19999999995002,
52.1220404910177)) ;
#195296 = CARTESIAN_POINT('Ctrl Pts',(-73.3416663111934,3.00000000004998,
52.1213316342151)) ;
#195297 = CARTESIAN_POINT('Ctrl Pts',(-73.3416663111934,-4.19999999995002,
52.121331634215)) ;
#195298 = CARTESIAN_POINT('Ctrl Pts',(-73.3405578361091,3.00000000004998,
52.1206211826759)) ;
#195299 = CARTESIAN_POINT('Ctrl Pts',(-73.3405578361091,-4.19999999995002,
52.1206211826759)) ;
#195300 = CARTESIAN_POINT('Ctrl Pts',(-70.0488553627454,3.00000000005,50.0108804019009)) ;
#195301 = CARTESIAN_POINT('Ctrl Pts',(-70.0488553627454,-4.19999999995,50.0108804019008)) ;
#195302 = CARTESIAN_POINT('Ctrl Pts',(-74.5822721977904,3.00000000005008,
42.7755671143843)) ;
#195303 = CARTESIAN_POINT('Ctrl Pts',(-74.5822721977904,-4.19999999994992,
42.7755671143842)) ;
#195304 = CARTESIAN_POINT('',(-74.5822721977904,3.00000000005008,42.7755671143843)) ;
#195305 = CARTESIAN_POINT('Origin',(-78.0530394275431,3.00000000005006,44.7680177483762)) ;
#195306 = CARTESIAN_POINT('',(-74.5822721977904,-2.99999999994992,42.7755671143842)) ;
#195307 = CARTESIAN_POINT('',(-74.5822721977904,3.00000000005008,42.7755671143843)) ;
#195308 = CARTESIAN_POINT('Origin',(-78.0530394275428,-2.99999999994995,44.7680177483764)) ;
#195309 = CARTESIAN_POINT('Origin',(-76.3176558126671,3.00000000005007,43.7717924313804)) ;
#195310 = CARTESIAN_POINT('',(-78.0530394275436,3.00000000005006,44.7680177483765)) ;
#195311 = CARTESIAN_POINT('',(-74.5822721977904,3.00000000005008,42.7755671143843)) ;
#195312 = CARTESIAN_POINT('',(-78.0530394275436,-2.99999999994994,44.7680177483764)) ;
#195313 = CARTESIAN_POINT('',(-78.0530394275436,3.00000000005006,44.7680177483765)) ;
#195314 = CARTESIAN_POINT('',(-74.5822721977904,-2.99999999994992,42.7755671143843)) ;
#195315 = CARTESIAN_POINT('Origin',(-78.2232062284076,3.00000000005006,44.4689518209346)) ;
#195316 = CARTESIAN_POINT('',(-78.3933730292715,3.00000000005006,44.1698858934927)) ;
#195317 = CARTESIAN_POINT('',(-78.0530394275436,3.00000000005006,44.7680177483765)) ;
#195318 = CARTESIAN_POINT('',(-78.3933730292715,-2.99999999994994,44.1698858934927)) ;
#195319 = CARTESIAN_POINT('',(-78.3933730292715,3.00000000005006,44.1698858934927)) ;
#195320 = CARTESIAN_POINT('',(-78.0530394275436,-2.99999999994994,44.7680177483764)) ;
#195321 = CARTESIAN_POINT('Ctrl Pts',(-78.3933730292716,3.00000000005006,
44.1698858934927)) ;
#195322 = CARTESIAN_POINT('Ctrl Pts',(-78.3933730292716,-4.19999999994994,
44.1698858934927)) ;
#195323 = CARTESIAN_POINT('Ctrl Pts',(-78.3921955146446,3.00000000005006,
44.1692968938833)) ;
#195324 = CARTESIAN_POINT('Ctrl Pts',(-78.3921955146446,-4.19999999994994,
44.1692968938832)) ;
#195325 = CARTESIAN_POINT('Ctrl Pts',(-78.3910188494957,3.00000000005006,
44.1687062014689)) ;
#195326 = CARTESIAN_POINT('Ctrl Pts',(-78.3910188494957,-4.19999999994994,
44.1687062014688)) ;
#195327 = CARTESIAN_POINT('Ctrl Pts',(-74.8968207049898,3.00000000005008,
42.4145994025118)) ;
#195328 = CARTESIAN_POINT('Ctrl Pts',(-74.8968207049898,-4.19999999994992,
42.4145994025117)) ;
#195329 = CARTESIAN_POINT('Ctrl Pts',(-78.6491068290692,3.00000000005016,
34.7450508231087)) ;
#195330 = CARTESIAN_POINT('Ctrl Pts',(-78.6491068290692,-4.19999999994984,
34.7450508231086)) ;
#195331 = CARTESIAN_POINT('',(-78.6491068290692,3.00000000005016,34.7450508231087)) ;
#195332 = CARTESIAN_POINT('Origin',(-82.3091286356931,3.00000000005014,36.3637926391687)) ;
#195333 = CARTESIAN_POINT('',(-78.6491068290692,-2.99999999994984,34.7450508231086)) ;
#195334 = CARTESIAN_POINT('',(-78.6491068290692,3.00000000005016,34.7450508231087)) ;
#195335 = CARTESIAN_POINT('Origin',(-82.3091286356924,-2.99999999994986,36.3637926391692)) ;
#195336 = CARTESIAN_POINT('Origin',(-80.4791177323812,3.00000000005015,35.5544217311386)) ;
#195337 = CARTESIAN_POINT('',(-82.3091286356932,3.00000000005014,36.3637926391685)) ;
#195338 = CARTESIAN_POINT('',(-78.6491068290692,3.00000000005016,34.7450508231087)) ;
#195339 = CARTESIAN_POINT('',(-82.3091286356932,-2.99999999994986,36.3637926391684)) ;
#195340 = CARTESIAN_POINT('',(-82.3091286356932,3.00000000005014,36.3637926391685)) ;
#195341 = CARTESIAN_POINT('',(-78.6491068290692,-2.99999999994984,34.7450508231086)) ;
#195342 = CARTESIAN_POINT('Origin',(-82.447102343206,3.00000000005014,36.0485777519755)) ;
#195343 = CARTESIAN_POINT('',(-82.585076050719,3.00000000005015,35.7333628647823)) ;
#195344 = CARTESIAN_POINT('',(-82.3091286356932,3.00000000005014,36.3637926391685)) ;
#195345 = CARTESIAN_POINT('',(-82.585076050719,-2.99999999994985,35.7333628647822)) ;
#195346 = CARTESIAN_POINT('',(-82.585076050719,3.00000000005015,35.7333628647823)) ;
#195347 = CARTESIAN_POINT('',(-82.3091286356932,-2.99999999994986,36.3637926391684)) ;
#195348 = CARTESIAN_POINT('Ctrl Pts',(-82.5850760507189,3.00000000005015,
35.7333628647824)) ;
#195349 = CARTESIAN_POINT('Ctrl Pts',(-82.5850760507189,-4.19999999994985,
35.7333628647823)) ;
#195350 = CARTESIAN_POINT('Ctrl Pts',(-82.5838434194163,3.00000000005015,
35.7329001755683)) ;
#195351 = CARTESIAN_POINT('Ctrl Pts',(-82.5838434194163,-4.19999999994985,
35.7329001755682)) ;
#195352 = CARTESIAN_POINT('Ctrl Pts',(-82.5826114559916,3.00000000005015,
35.732435714029)) ;
#195353 = CARTESIAN_POINT('Ctrl Pts',(-82.5826114559916,-4.19999999994985,
35.7324357140289)) ;
#195354 = CARTESIAN_POINT('Ctrl Pts',(-78.9242008064233,3.00000000005016,
34.3531812580496)) ;
#195355 = CARTESIAN_POINT('Ctrl Pts',(-78.9242008064233,-4.19999999994984,
34.3531812580496)) ;
#195356 = CARTESIAN_POINT('Ctrl Pts',(-81.8542453875451,3.00000000005024,
26.3334265659522)) ;
#195357 = CARTESIAN_POINT('Ctrl Pts',(-81.8542453875451,-4.19999999994976,
26.3334265659521)) ;
#195358 = CARTESIAN_POINT('',(-81.854245387545,3.00000000005024,26.3334265659522)) ;
#195359 = CARTESIAN_POINT('Origin',(-85.6634218062174,3.00000000005023,27.5607242899997)) ;
#195360 = CARTESIAN_POINT('',(-81.854245387545,-2.99999999994976,26.3334265659521)) ;
#195361 = CARTESIAN_POINT('',(-81.854245387545,3.00000000005024,26.3334265659522)) ;
#195362 = CARTESIAN_POINT('Origin',(-85.6634218062175,-2.99999999994977,27.5607242899996)) ;
#195363 = CARTESIAN_POINT('Origin',(-83.7588335968814,3.00000000005024,26.9470754279756)) ;
#195364 = CARTESIAN_POINT('',(-85.6634218062177,3.00000000005023,27.5607242899993)) ;
#195365 = CARTESIAN_POINT('',(-81.854245387545,3.00000000005024,26.3334265659522)) ;
#195366 = CARTESIAN_POINT('',(-85.6634218062177,-2.99999999994977,27.5607242899992)) ;
#195367 = CARTESIAN_POINT('',(-85.6634218062177,3.00000000005023,27.5607242899993)) ;
#195368 = CARTESIAN_POINT('',(-81.854245387545,-2.99999999994976,26.3334265659521)) ;
#195369 = CARTESIAN_POINT('Origin',(-85.7676907515672,3.00000000005023,27.2328140033222)) ;
#195370 = CARTESIAN_POINT('',(-85.8719596969165,3.00000000005024,26.9049037166451)) ;
#195371 = CARTESIAN_POINT('',(-85.6634218062177,3.00000000005023,27.5607242899993)) ;
#195372 = CARTESIAN_POINT('',(-85.8719596969165,-2.99999999994976,26.904903716645)) ;
#195373 = CARTESIAN_POINT('',(-85.8719596969165,3.00000000005024,26.9049037166451)) ;
#195374 = CARTESIAN_POINT('',(-85.6634218062177,-2.99999999994977,27.5607242899992)) ;
#195375 = CARTESIAN_POINT('Ctrl Pts',(-85.8719596969165,3.00000000005024,
26.9049037166451)) ;
#195376 = CARTESIAN_POINT('Ctrl Pts',(-85.8719596969165,-4.19999999994976,
26.904903716645)) ;
#195377 = CARTESIAN_POINT('Ctrl Pts',(-85.8706854539044,3.00000000005024,
26.904572407147)) ;
#195378 = CARTESIAN_POINT('Ctrl Pts',(-85.8706854539044,-4.19999999994976,
26.9045724071469)) ;
#195379 = CARTESIAN_POINT('Ctrl Pts',(-85.8694116898535,3.00000000005024,
26.9042392652197)) ;
#195380 = CARTESIAN_POINT('Ctrl Pts',(-85.8694116898535,-4.19999999994976,
26.9042392652196)) ;
#195381 = CARTESIAN_POINT('Ctrl Pts',(-82.0868708478705,3.00000000005025,
25.9149485526655)) ;
#195382 = CARTESIAN_POINT('Ctrl Pts',(-82.0868708478705,-4.19999999994975,
25.9149485526654)) ;
#195383 = CARTESIAN_POINT('Ctrl Pts',(-84.1625717044525,3.00000000005033,
17.6328538585215)) ;
#195384 = CARTESIAN_POINT('Ctrl Pts',(-84.1625717044525,-4.19999999994967,
17.6328538585214)) ;
#195385 = CARTESIAN_POINT('',(-84.1625717044525,3.00000000005033,17.6328538585214)) ;
#195386 = CARTESIAN_POINT('Origin',(-88.0791686012115,3.00000000005033,18.4552609598614)) ;
#195387 = CARTESIAN_POINT('',(-84.1625717044525,-2.99999999994967,17.6328538585214)) ;
#195388 = CARTESIAN_POINT('',(-84.1625717044525,3.00000000005033,17.6328538585214)) ;
#195389 = CARTESIAN_POINT('Origin',(-88.0791686012115,-2.99999999994968,18.4552609598614)) ;
#195390 = CARTESIAN_POINT('Origin',(-86.1208701528312,3.00000000005033,18.0440574091923)) ;
#195391 = CARTESIAN_POINT('',(-88.0791686012098,3.00000000005032,18.455260959863)) ;
#195392 = CARTESIAN_POINT('',(-84.1625717044525,3.00000000005033,17.6328538585214)) ;
#195393 = CARTESIAN_POINT('',(-88.0791686012098,-2.99999999994968,18.4552609598629)) ;
#195394 = CARTESIAN_POINT('',(-88.0791686012098,3.00000000005032,18.455260959863)) ;
#195395 = CARTESIAN_POINT('',(-84.1625717044525,-2.99999999994967,17.6328538585214)) ;
#195396 = CARTESIAN_POINT('Origin',(-88.1485903920105,3.00000000005033,18.1182479274222)) ;
#195397 = CARTESIAN_POINT('',(-88.2180121828115,3.00000000005033,17.7812348949813)) ;
#195398 = CARTESIAN_POINT('',(-88.0791686012098,3.00000000005032,18.455260959863)) ;
#195399 = CARTESIAN_POINT('',(-88.2180121828115,-2.99999999994967,17.7812348949812)) ;
#195400 = CARTESIAN_POINT('',(-88.2180121828115,3.00000000005033,17.7812348949813)) ;
#195401 = CARTESIAN_POINT('',(-88.0791686012098,-2.99999999994968,18.4552609598629)) ;
#195402 = CARTESIAN_POINT('Ctrl Pts',(-88.2180121828114,3.00000000005033,
17.7812348949813)) ;
#195403 = CARTESIAN_POINT('Ctrl Pts',(-88.2180121828114,-4.19999999994967,
17.7812348949812)) ;
#195404 = CARTESIAN_POINT('Ctrl Pts',(-88.2167102889633,3.00000000005033,
17.7810385950953)) ;
#195405 = CARTESIAN_POINT('Ctrl Pts',(-88.2167102889633,-4.19999999994967,
17.7810385950953)) ;
#195406 = CARTESIAN_POINT('Ctrl Pts',(-88.2154086799115,3.00000000005033,
17.7808404227533)) ;
#195407 = CARTESIAN_POINT('Ctrl Pts',(-88.2154086799115,-4.19999999994967,
17.7808404227532)) ;
#195408 = CARTESIAN_POINT('Ctrl Pts',(-84.3501799545264,3.00000000005034,
17.1923523296933)) ;
#195409 = CARTESIAN_POINT('Ctrl Pts',(-84.3501799545264,-4.19999999994966,
17.1923523296932)) ;
#195410 = CARTESIAN_POINT('Ctrl Pts',(-85.5487952736159,3.00000000005042,
8.73865799611182)) ;
#195411 = CARTESIAN_POINT('Ctrl Pts',(-85.5487952736159,-4.19999999994958,
8.73865799611175)) ;
#195412 = CARTESIAN_POINT('',(-85.548795273616,3.00000000005042,8.7386579961118)) ;
#195413 = CARTESIAN_POINT('Origin',(-89.5299015932563,3.00000000005042,9.1471640104453)) ;
#195414 = CARTESIAN_POINT('',(-85.548795273616,-2.99999999994958,8.73865799611174)) ;
#195415 = CARTESIAN_POINT('',(-85.548795273616,3.00000000005042,8.7386579961118)) ;
#195416 = CARTESIAN_POINT('Origin',(-89.5299015932563,-2.99999999994958,9.14716401044516)) ;
#195417 = CARTESIAN_POINT('Origin',(-87.539348433436,3.00000000005042,8.94291100327852)) ;
#195418 = CARTESIAN_POINT('',(-89.5299015932563,3.00000000005042,9.14716401044524)) ;
#195419 = CARTESIAN_POINT('',(-85.548795273616,3.00000000005042,8.7386579961118)) ;
#195420 = CARTESIAN_POINT('',(-89.5299015932563,-2.99999999994958,9.14716401044518)) ;
#195421 = CARTESIAN_POINT('',(-89.5299015932563,3.00000000005042,9.14716401044524)) ;
#195422 = CARTESIAN_POINT('',(-85.548795273616,-2.99999999994958,8.73865799611174)) ;
#195423 = CARTESIAN_POINT('Origin',(-89.563715629841,3.00000000005042,8.8047406175488)) ;
#195424 = CARTESIAN_POINT('',(-89.5975296664259,3.00000000005043,8.46231722465223)) ;
#195425 = CARTESIAN_POINT('',(-89.5299015932563,3.00000000005042,9.14716401044524)) ;
#195426 = CARTESIAN_POINT('',(-89.5975296664259,-2.99999999994957,8.46231722465217)) ;
#195427 = CARTESIAN_POINT('',(-89.5975296664259,3.00000000005042,8.46231722465223)) ;
#195428 = CARTESIAN_POINT('',(-89.5299015932563,-2.99999999994958,9.14716401044518)) ;
#195429 = CARTESIAN_POINT('Ctrl Pts',(-89.5975296664258,3.00000000005042,
8.46231722465223)) ;
#195430 = CARTESIAN_POINT('Ctrl Pts',(-89.5975296664258,-4.19999999994958,
8.46231722465216)) ;
#195431 = CARTESIAN_POINT('Ctrl Pts',(-89.5962143855632,3.00000000005042,
8.46225808508051)) ;
#195432 = CARTESIAN_POINT('Ctrl Pts',(-89.5962143855632,-4.19999999994958,
8.46225808508044)) ;
#195433 = CARTESIAN_POINT('Ctrl Pts',(-89.5948991922115,3.00000000005043,
8.4621970535414)) ;
#195434 = CARTESIAN_POINT('Ctrl Pts',(-89.5948991922115,-4.19999999994958,
8.46219705354133)) ;
#195435 = CARTESIAN_POINT('Ctrl Pts',(-85.6893308381907,3.00000000005043,
8.28095917867225)) ;
#195436 = CARTESIAN_POINT('Ctrl Pts',(-85.6893308381907,-4.19999999994957,
8.28095917867218)) ;
#195437 = CARTESIAN_POINT('Ctrl Pts',(-85.9977283395255,3.00000000005051,
-0.251714350178572)) ;
#195438 = CARTESIAN_POINT('Ctrl Pts',(-85.9977283395255,-4.19999999994949,
-0.251714350178644)) ;
#195439 = CARTESIAN_POINT('',(-85.9977283395255,3.00000000005051,-0.251714350178527)) ;
#195440 = CARTESIAN_POINT('Origin',(-89.9997262481113,3.00000000005051,-0.261585100232212)) ;
#195441 = CARTESIAN_POINT('',(-85.9977283395255,-2.99999999994949,-0.251714350178588)) ;
#195442 = CARTESIAN_POINT('',(-85.9977283395255,3.00000000005051,-0.251714350178527)) ;
#195443 = CARTESIAN_POINT('Origin',(-89.9997262481114,-2.99999999994948,-0.26158510023235)) ;
#195444 = CARTESIAN_POINT('Origin',(-87.9987272938179,3.00000000005051,-0.256649725205155)) ;
#195445 = CARTESIAN_POINT('',(-89.9997262481103,3.00000000005051,-0.261585100231687)) ;
#195446 = CARTESIAN_POINT('',(-85.9977283395255,3.00000000005051,-0.251714350178527)) ;
#195447 = CARTESIAN_POINT('',(-89.9997262481103,-2.99999999994949,-0.261585100231748)) ;
#195448 = CARTESIAN_POINT('',(-89.9997262481103,3.00000000005051,-0.261585100231687)) ;
#195449 = CARTESIAN_POINT('',(-85.9977283395255,-2.99999999994949,-0.251714350178588)) ;
#195450 = CARTESIAN_POINT('Origin',(-89.9975620568182,3.00000000005052,-0.605667191234735)) ;
#195451 = CARTESIAN_POINT('',(-89.9953978655262,3.00000000005052,-0.949749282237835)) ;
#195452 = CARTESIAN_POINT('',(-89.9997262481103,3.00000000005051,-0.261585100231687)) ;
#195453 = CARTESIAN_POINT('',(-89.9953978655262,-2.99999999994948,-0.949749282237896)) ;
#195454 = CARTESIAN_POINT('',(-89.9953978655262,3.00000000005052,-0.949749282237835)) ;
#195455 = CARTESIAN_POINT('',(-89.9997262481103,-2.99999999994949,-0.261585100231748)) ;
#195456 = CARTESIAN_POINT('Ctrl Pts',(-89.9953978655262,3.00000000005052,
-0.949749282237899)) ;
#195457 = CARTESIAN_POINT('Ctrl Pts',(-89.9953978655262,-4.19999999994948,
-0.949749282237972)) ;
#195458 = CARTESIAN_POINT('Ctrl Pts',(-89.9940836081412,3.00000000005052,
-0.949670613549396)) ;
#195459 = CARTESIAN_POINT('Ctrl Pts',(-89.9940836081412,-4.19999999994948,
-0.94967061354947)) ;
#195460 = CARTESIAN_POINT('Ctrl Pts',(-89.9927692400234,3.00000000005052,
-0.949593835611227)) ;
#195461 = CARTESIAN_POINT('Ctrl Pts',(-89.9927692400234,-4.19999999994948,
-0.9495938356113)) ;
#195462 = CARTESIAN_POINT('Ctrl Pts',(-86.0896514815463,3.00000000005052,
-0.721595812205907)) ;
#195463 = CARTESIAN_POINT('Ctrl Pts',(-86.0896514815463,-4.19999999994948,
-0.721595812205981)) ;
#195464 = CARTESIAN_POINT('Ctrl Pts',(-85.5044522975653,3.00000000005061,
-9.23976277956772)) ;
#195465 = CARTESIAN_POINT('Ctrl Pts',(-85.5044522975653,-4.1999999999494,
-9.23976277956779)) ;
#195466 = CARTESIAN_POINT('',(-85.5044522975653,3.00000000005061,-9.23976277956773)) ;
#195467 = CARTESIAN_POINT('Origin',(-89.4834950685368,3.00000000005062,-9.66790214800468)) ;
#195468 = CARTESIAN_POINT('',(-85.5044522975653,-2.99999999994939,-9.23976277956779)) ;
#195469 = CARTESIAN_POINT('',(-85.5044522975653,3.00000000005061,-9.23976277956773)) ;
#195470 = CARTESIAN_POINT('Origin',(-89.4834950685368,-2.9999999999494,-9.66790214800469)) ;
#195471 = CARTESIAN_POINT('Origin',(-87.493973683051,3.00000000005061,-9.4538324637858)) ;
#195472 = CARTESIAN_POINT('',(-89.4834950685366,3.00000000005061,-9.66790214800376)) ;
#195473 = CARTESIAN_POINT('',(-85.5044522975653,3.00000000005061,-9.23976277956773)) ;
#195474 = CARTESIAN_POINT('',(-89.4834950685366,-2.99999999994939,-9.66790214800382)) ;
#195475 = CARTESIAN_POINT('',(-89.4834950685366,3.00000000005061,-9.66790214800376)) ;
#195476 = CARTESIAN_POINT('',(-85.5044522975653,-2.99999999994939,-9.23976277956779)) ;
#195477 = CARTESIAN_POINT('Origin',(-89.4453763607008,3.00000000005061,-10.0098731017204)) ;
#195478 = CARTESIAN_POINT('',(-89.4072576528647,3.00000000005062,-10.3518440554371)) ;
#195479 = CARTESIAN_POINT('',(-89.4834950685366,3.00000000005061,-9.66790214800376)) ;
#195480 = CARTESIAN_POINT('',(-89.4072576528647,-2.99999999994938,-10.3518440554372)) ;
#195481 = CARTESIAN_POINT('',(-89.4072576528647,3.00000000005062,-10.3518440554371)) ;
#195482 = CARTESIAN_POINT('',(-89.4834950685366,-2.99999999994939,-9.66790214800382)) ;
#195483 = CARTESIAN_POINT('Ctrl Pts',(-89.4072576528647,3.00000000005062,
-10.3518440554371)) ;
#195484 = CARTESIAN_POINT('Ctrl Pts',(-89.4072576528647,-4.19999999994939,
-10.3518440554372)) ;
#195485 = CARTESIAN_POINT('Ctrl Pts',(-89.4059588182361,3.00000000005062,
-10.3516284403988)) ;
#195486 = CARTESIAN_POINT('Ctrl Pts',(-89.4059588182361,-4.19999999994939,
-10.3516284403988)) ;
#195487 = CARTESIAN_POINT('Ctrl Pts',(-89.404659675844,3.00000000005062,-10.351414694179)) ;
#195488 = CARTESIAN_POINT('Ctrl Pts',(-89.404659675844,-4.19999999994939,
-10.3514146941791)) ;
#195489 = CARTESIAN_POINT('Ctrl Pts',(-85.5467558878524,3.00000000005061,
-9.71667876655564)) ;
#195490 = CARTESIAN_POINT('Ctrl Pts',(-85.5467558878524,-4.19999999994939,
-9.71667876655571)) ;
#195491 = CARTESIAN_POINT('Ctrl Pts',(-84.074371583276,3.0000000000507,-18.1270123525924)) ;
#195492 = CARTESIAN_POINT('Ctrl Pts',(-84.074371583276,-4.19999999994931,
-18.1270123525924)) ;
#195493 = CARTESIAN_POINT('',(-84.074371583276,3.0000000000507,-18.1270123525923)) ;
#195494 = CARTESIAN_POINT('Origin',(-87.9868639913669,3.0000000000507,-18.9687295548975)) ;
#195495 = CARTESIAN_POINT('',(-84.074371583276,-2.9999999999493,-18.1270123525924)) ;
#195496 = CARTESIAN_POINT('',(-84.074371583276,3.0000000000507,-18.1270123525923)) ;
#195497 = CARTESIAN_POINT('Origin',(-87.9868639913669,-2.9999999999493,-18.9687295548977)) ;
#195498 = CARTESIAN_POINT('Origin',(-86.0306177873215,3.0000000000507,-18.5478709537447)) ;
#195499 = CARTESIAN_POINT('',(-87.9868639913672,3.00000000005071,-18.9687295548971)) ;
#195500 = CARTESIAN_POINT('',(-84.074371583276,3.0000000000507,-18.1270123525923)) ;
#195501 = CARTESIAN_POINT('',(-87.9868639913672,-2.9999999999493,-18.9687295548972)) ;
#195502 = CARTESIAN_POINT('',(-87.9868639913672,3.00000000005071,-18.9687295548971)) ;
#195503 = CARTESIAN_POINT('',(-84.074371583276,-2.9999999999493,-18.1270123525924)) ;
#195504 = CARTESIAN_POINT('Origin',(-87.9132084035268,3.00000000005071,-19.3048426659964)) ;
#195505 = CARTESIAN_POINT('',(-87.8395528156864,3.00000000005071,-19.6409557770956)) ;
#195506 = CARTESIAN_POINT('',(-87.9868639913672,3.00000000005071,-18.9687295548971)) ;
#195507 = CARTESIAN_POINT('',(-87.8395528156864,-2.99999999994929,-19.6409557770957)) ;
#195508 = CARTESIAN_POINT('',(-87.8395528156864,3.00000000005071,-19.6409557770956)) ;
#195509 = CARTESIAN_POINT('',(-87.9868639913672,-2.9999999999493,-18.9687295548972)) ;
#195510 = CARTESIAN_POINT('Ctrl Pts',(-87.8395528156864,3.00000000005071,
-19.6409557770957)) ;
#195511 = CARTESIAN_POINT('Ctrl Pts',(-87.8395528156864,-4.19999999994929,
-19.6409557770957)) ;
#195512 = CARTESIAN_POINT('Ctrl Pts',(-87.8382836341185,3.00000000005071,
-19.6406055780315)) ;
#195513 = CARTESIAN_POINT('Ctrl Pts',(-87.8382836341185,-4.19999999994929,
-19.6406055780316)) ;
#195514 = CARTESIAN_POINT('Ctrl Pts',(-87.8370139511284,3.00000000005071,
-19.640257205378)) ;
#195515 = CARTESIAN_POINT('Ctrl Pts',(-87.8370139511284,-4.19999999994929,
-19.6402572053781)) ;
#195516 = CARTESIAN_POINT('Ctrl Pts',(-84.0665921348419,3.0000000000507,-18.6057376731866)) ;
#195517 = CARTESIAN_POINT('Ctrl Pts',(-84.0665921348419,-4.1999999999493,
-18.6057376731866)) ;
#195518 = CARTESIAN_POINT('Ctrl Pts',(-81.7231544602273,3.00000000005078,
-26.8160925031547)) ;
#195519 = CARTESIAN_POINT('Ctrl Pts',(-81.7231544602273,-4.19999999994922,
-26.8160925031548)) ;
#195520 = CARTESIAN_POINT('',(-81.7231544602271,3.00000000005079,-26.8160925031548)) ;
#195521 = CARTESIAN_POINT('Origin',(-85.5262304198732,3.0000000000508,-28.0621655095208)) ;
#195522 = CARTESIAN_POINT('',(-81.7231544602271,-2.99999999994922,-26.8160925031548)) ;
#195523 = CARTESIAN_POINT('',(-81.7231544602271,3.00000000005079,-26.8160925031548)) ;
#195524 = CARTESIAN_POINT('Origin',(-85.5262304198732,-2.99999999994921,-28.0621655095209)) ;
#195525 = CARTESIAN_POINT('Origin',(-83.6246924400503,3.00000000005079,-27.4391290063367)) ;
#195526 = CARTESIAN_POINT('',(-85.526230419873,3.0000000000508,-28.0621655095189)) ;
#195527 = CARTESIAN_POINT('',(-81.7231544602271,3.00000000005079,-26.8160925031548)) ;
#195528 = CARTESIAN_POINT('',(-85.526230419873,-2.9999999999492,-28.062165509519)) ;
#195529 = CARTESIAN_POINT('',(-85.526230419873,3.0000000000508,-28.0621655095189)) ;
#195530 = CARTESIAN_POINT('',(-81.7231544602271,-2.99999999994922,-26.8160925031548)) ;
#195531 = CARTESIAN_POINT('Origin',(-85.4178449380624,3.0000000000508,-28.3887382524195)) ;
#195532 = CARTESIAN_POINT('',(-85.3094594562516,3.0000000000508,-28.71531099532)) ;
#195533 = CARTESIAN_POINT('',(-85.526230419873,3.0000000000508,-28.0621655095189)) ;
#195534 = CARTESIAN_POINT('',(-85.3094594562516,-2.9999999999492,-28.7153109953201)) ;
#195535 = CARTESIAN_POINT('',(-85.3094594562516,3.0000000000508,-28.71531099532)) ;
#195536 = CARTESIAN_POINT('',(-85.526230419873,-2.9999999999492,-28.062165509519)) ;
#195537 = CARTESIAN_POINT('Ctrl Pts',(-85.3094594562517,3.0000000000508,-28.71531099532)) ;
#195538 = CARTESIAN_POINT('Ctrl Pts',(-85.3094594562517,-4.1999999999492,
-28.7153109953201)) ;
#195539 = CARTESIAN_POINT('Ctrl Pts',(-85.308233833163,3.0000000000508,-28.714830049084)) ;
#195540 = CARTESIAN_POINT('Ctrl Pts',(-85.308233833163,-4.1999999999492,-28.7148300490841)) ;
#195541 = CARTESIAN_POINT('Ctrl Pts',(-85.3070075204872,3.0000000000508,-28.7143508668407)) ;
#195542 = CARTESIAN_POINT('Ctrl Pts',(-85.3070075204872,-4.1999999999492,
-28.7143508668408)) ;
#195543 = CARTESIAN_POINT('Ctrl Pts',(-81.6653772063365,3.00000000005079,
-27.2913821425628)) ;
#195544 = CARTESIAN_POINT('Ctrl Pts',(-81.6653772063365,-4.19999999994921,
-27.2913821425629)) ;
#195545 = CARTESIAN_POINT('Ctrl Pts',(-78.4765613552426,3.00000000005087,
-35.2118038508177)) ;
#195546 = CARTESIAN_POINT('Ctrl Pts',(-78.4765613552426,-4.19999999994913,
-35.2118038508178)) ;
#195547 = CARTESIAN_POINT('',(-78.4765613552426,3.00000000005087,-35.2118038508177)) ;
#195548 = CARTESIAN_POINT('Origin',(-82.1285535703849,3.00000000005089,-36.8485804246292)) ;
#195549 = CARTESIAN_POINT('',(-78.4765613552426,-2.99999999994913,-35.2118038508178)) ;
#195550 = CARTESIAN_POINT('',(-78.4765613552426,3.00000000005087,-35.2118038508177)) ;
#195551 = CARTESIAN_POINT('Origin',(-82.1285535703849,-2.99999999994912,-36.8485804246294)) ;
#195552 = CARTESIAN_POINT('Origin',(-80.3025574628135,3.00000000005088,-36.0301921377219)) ;
#195553 = CARTESIAN_POINT('',(-82.1285535703842,3.00000000005089,-36.8485804246263)) ;
#195554 = CARTESIAN_POINT('',(-78.4765613552426,3.00000000005087,-35.2118038508177)) ;
#195555 = CARTESIAN_POINT('',(-82.1285535703842,-2.99999999994911,-36.8485804246263)) ;
#195556 = CARTESIAN_POINT('',(-82.1285535703842,3.00000000005089,-36.8485804246263)) ;
#195557 = CARTESIAN_POINT('',(-78.4765613552426,-2.99999999994913,-35.2118038508178)) ;
#195558 = CARTESIAN_POINT('Origin',(-81.9866256886229,3.00000000005089,-37.1620348000171)) ;
#195559 = CARTESIAN_POINT('',(-81.8446978068616,3.00000000005089,-37.4754891754079)) ;
#195560 = CARTESIAN_POINT('',(-82.1285535703842,3.00000000005089,-36.8485804246263)) ;
#195561 = CARTESIAN_POINT('',(-81.8446978068616,-2.99999999994911,-37.475489175408)) ;
#195562 = CARTESIAN_POINT('',(-81.8446978068616,3.00000000005089,-37.4754891754079)) ;
#195563 = CARTESIAN_POINT('',(-82.1285535703842,-2.99999999994911,-36.8485804246264)) ;
#195564 = CARTESIAN_POINT('Ctrl Pts',(-81.8446978068617,3.00000000005089,
-37.4754891754079)) ;
#195565 = CARTESIAN_POINT('Ctrl Pts',(-81.8446978068617,-4.19999999994911,
-37.475489175408)) ;
#195566 = CARTESIAN_POINT('Ctrl Pts',(-81.8435291704357,3.00000000005089,
-37.4748827513478)) ;
#195567 = CARTESIAN_POINT('Ctrl Pts',(-81.8435291704357,-4.19999999994911,
-37.4748827513479)) ;
#195568 = CARTESIAN_POINT('Ctrl Pts',(-81.8423596638125,3.00000000005089,
-37.4742780095355)) ;
#195569 = CARTESIAN_POINT('Ctrl Pts',(-81.8423596638125,-4.19999999994911,
-37.4742780095356)) ;
#195570 = CARTESIAN_POINT('Ctrl Pts',(-78.3694193155794,3.00000000005088,
-35.6784504362897)) ;
#195571 = CARTESIAN_POINT('Ctrl Pts',(-78.3694193155794,-4.19999999994913,
-35.6784504362897)) ;
#195572 = CARTESIAN_POINT('Ctrl Pts',(-74.3701626217736,3.00000000005095,
-43.2221612251409)) ;
#195573 = CARTESIAN_POINT('Ctrl Pts',(-74.3701626217736,-4.19999999994906,
-43.222161225141)) ;
#195574 = CARTESIAN_POINT('',(-74.3701626217736,3.00000000005095,-43.2221612251409)) ;
#195575 = CARTESIAN_POINT('Origin',(-77.831059101474,3.00000000005098,-45.231708499739)) ;
#195576 = CARTESIAN_POINT('',(-74.3701626217736,-2.99999999994905,-43.222161225141)) ;
#195577 = CARTESIAN_POINT('',(-74.3701626217736,3.00000000005095,-43.2221612251409)) ;
#195578 = CARTESIAN_POINT('Origin',(-77.8310591014741,-2.99999999994903,-45.2317084997386)) ;
#195579 = CARTESIAN_POINT('Origin',(-76.1006108616236,3.00000000005096,-44.2269348624374)) ;
#195580 = CARTESIAN_POINT('',(-77.831059101474,3.00000000005097,-45.2317084997338)) ;
#195581 = CARTESIAN_POINT('',(-74.3701626217736,3.00000000005095,-43.2221612251409)) ;
#195582 = CARTESIAN_POINT('',(-77.831059101474,-2.99999999994903,-45.2317084997339)) ;
#195583 = CARTESIAN_POINT('',(-77.831059101474,3.00000000005097,-45.2317084997338)) ;
#195584 = CARTESIAN_POINT('',(-74.3701626217736,-2.99999999994905,-43.222161225141)) ;
#195585 = CARTESIAN_POINT('Origin',(-77.657143811335,3.00000000005098,-45.5286102358837)) ;
#195586 = CARTESIAN_POINT('',(-77.4832285211961,3.00000000005098,-45.8255119720335)) ;
#195587 = CARTESIAN_POINT('',(-77.831059101474,3.00000000005097,-45.2317084997338)) ;
#195588 = CARTESIAN_POINT('',(-77.4832285211961,-2.99999999994902,-45.8255119720336)) ;
#195589 = CARTESIAN_POINT('',(-77.4832285211961,3.00000000005098,-45.8255119720335)) ;
#195590 = CARTESIAN_POINT('',(-77.831059101474,-2.99999999994903,-45.2317084997339)) ;
#195591 = CARTESIAN_POINT('Ctrl Pts',(-77.4832285211961,3.00000000005098,
-45.8255119720335)) ;
#195592 = CARTESIAN_POINT('Ctrl Pts',(-77.4832285211961,-4.19999999994902,
-45.8255119720336)) ;
#195593 = CARTESIAN_POINT('Ctrl Pts',(-77.4821296752578,3.00000000005098,
-45.8247867142581)) ;
#195594 = CARTESIAN_POINT('Ctrl Pts',(-77.4821296752578,-4.19999999994902,
-45.8247867142582)) ;
#195595 = CARTESIAN_POINT('Ctrl Pts',(-77.4810297880467,3.00000000005098,
-45.8240630385544)) ;
#195596 = CARTESIAN_POINT('Ctrl Pts',(-77.4810297880467,-4.19999999994902,
-45.8240630385545)) ;
#195597 = CARTESIAN_POINT('Ctrl Pts',(-74.2148296669459,3.00000000005096,
-43.6750520790345)) ;
#195598 = CARTESIAN_POINT('Ctrl Pts',(-74.2148296669459,-4.19999999994905,
-43.6750520790346)) ;
#195599 = CARTESIAN_POINT('Ctrl Pts',(-69.4489488236634,3.00000000005103,
-50.7594014744564)) ;
#195600 = CARTESIAN_POINT('Ctrl Pts',(-69.4489488236634,-4.19999999994897,
-50.7594014744564)) ;
#195601 = CARTESIAN_POINT('',(-69.4489488236635,3.00000000005103,-50.7594014744564)) ;
#195602 = CARTESIAN_POINT('Origin',(-72.6808312618518,3.00000000005105,-53.1197024293663)) ;
#195603 = CARTESIAN_POINT('',(-69.4489488236635,-2.99999999994897,-50.7594014744565)) ;
#195604 = CARTESIAN_POINT('',(-69.4489488236635,3.00000000005103,-50.7594014744564)) ;
#195605 = CARTESIAN_POINT('Origin',(-72.6808312618517,-2.99999999994895,-53.1197024293665)) ;
#195606 = CARTESIAN_POINT('Origin',(-71.0648900427576,3.00000000005104,-51.9395519519123)) ;
#195607 = CARTESIAN_POINT('',(-72.6808312618515,3.00000000005105,-53.1197024293682)) ;
#195608 = CARTESIAN_POINT('',(-69.4489488236635,3.00000000005103,-50.7594014744564)) ;
#195609 = CARTESIAN_POINT('',(-72.6808312618515,-2.99999999994895,-53.1197024293683)) ;
#195610 = CARTESIAN_POINT('',(-72.6808312618515,3.00000000005105,-53.1197024293682)) ;
#195611 = CARTESIAN_POINT('',(-69.4489488236635,-2.99999999994897,-50.7594014744565)) ;
#195612 = CARTESIAN_POINT('Origin',(-72.4768340156477,3.00000000005106,-53.3967986087252)) ;
#195613 = CARTESIAN_POINT('',(-72.2728367694438,3.00000000005106,-53.6738947880823)) ;
#195614 = CARTESIAN_POINT('',(-72.6808312618515,3.00000000005105,-53.1197024293682)) ;
#195615 = CARTESIAN_POINT('',(-72.2728367694438,-2.99999999994894,-53.6738947880823)) ;
#195616 = CARTESIAN_POINT('',(-72.2728367694438,3.00000000005106,-53.6738947880822)) ;
#195617 = CARTESIAN_POINT('',(-72.6808312618515,-2.99999999994895,-53.1197024293683)) ;
#195618 = CARTESIAN_POINT('Ctrl Pts',(-72.2728367694438,3.00000000005106,
-53.6738947880822)) ;
#195619 = CARTESIAN_POINT('Ctrl Pts',(-72.2728367694438,-4.19999999994894,
-53.6738947880823)) ;
#195620 = CARTESIAN_POINT('Ctrl Pts',(-72.2718197531795,3.00000000005106,
-53.6730586426677)) ;
#195621 = CARTESIAN_POINT('Ctrl Pts',(-72.2718197531795,-4.19999999994894,
-53.6730586426678)) ;
#195622 = CARTESIAN_POINT('Ctrl Pts',(-72.2708015359745,3.00000000005106,
-53.6722239618152)) ;
#195623 = CARTESIAN_POINT('Ctrl Pts',(-72.2708015359745,-4.19999999994894,
-53.6722239618153)) ;
#195624 = CARTESIAN_POINT('Ctrl Pts',(-69.2471268140292,3.00000000005103,
-51.1935746298029)) ;
#195625 = CARTESIAN_POINT('Ctrl Pts',(-69.2471268140292,-4.19999999994897,
-51.1935746298029)) ;
#195626 = CARTESIAN_POINT('Ctrl Pts',(-63.7668378091141,3.0000000000511,-57.7409450173242)) ;
#195627 = CARTESIAN_POINT('Ctrl Pts',(-63.7668378091141,-4.1999999999489,
-57.7409450173243)) ;
#195628 = CARTESIAN_POINT('',(-63.7668378091141,3.0000000000511,-57.7409450173242)) ;
#195629 = CARTESIAN_POINT('Origin',(-66.7342970254822,3.00000000005113,-60.4261397013694)) ;
#195630 = CARTESIAN_POINT('',(-63.7668378091141,-2.9999999999489,-57.7409450173243)) ;
#195631 = CARTESIAN_POINT('',(-63.7668378091141,3.0000000000511,-57.7409450173242)) ;
#195632 = CARTESIAN_POINT('Origin',(-66.7342970254822,-2.99999999994887,-60.4261397013694)) ;
#195633 = CARTESIAN_POINT('Origin',(-65.2505674172983,3.00000000005111,-59.0835423593459)) ;
#195634 = CARTESIAN_POINT('',(-66.7342970254824,3.00000000005113,-60.4261397013678)) ;
#195635 = CARTESIAN_POINT('',(-63.7668378091141,3.0000000000511,-57.7409450173242)) ;
#195636 = CARTESIAN_POINT('',(-66.7342970254824,-2.99999999994887,-60.4261397013679)) ;
#195637 = CARTESIAN_POINT('',(-66.7342970254824,3.00000000005113,-60.4261397013678)) ;
#195638 = CARTESIAN_POINT('',(-63.7668378091141,-2.9999999999489,-57.7409450173243)) ;
#195639 = CARTESIAN_POINT('Origin',(-66.5024528597323,3.00000000005113,-60.6803944002046)) ;
#195640 = CARTESIAN_POINT('',(-66.2706086939824,3.00000000005113,-60.9346490990415)) ;
#195641 = CARTESIAN_POINT('',(-66.7342970254824,3.00000000005113,-60.4261397013678)) ;
#195642 = CARTESIAN_POINT('',(-66.2706086939824,-2.99999999994887,-60.9346490990415)) ;
#195643 = CARTESIAN_POINT('',(-66.2706086939824,3.00000000005113,-60.9346490990415)) ;
#195644 = CARTESIAN_POINT('',(-66.7342970254824,-2.99999999994887,-60.4261397013679)) ;
#195645 = CARTESIAN_POINT('Ctrl Pts',(-66.2706086939822,3.00000000005113,
-60.9346490990415)) ;
#195646 = CARTESIAN_POINT('Ctrl Pts',(-66.2706086939822,-4.19999999994887,
-60.9346490990416)) ;
#195647 = CARTESIAN_POINT('Ctrl Pts',(-66.2696846500344,3.00000000005113,
-60.9337112269716)) ;
#195648 = CARTESIAN_POINT('Ctrl Pts',(-66.2696846500344,-4.19999999994888,
-60.9337112269717)) ;
#195649 = CARTESIAN_POINT('Ctrl Pts',(-66.268759258637,3.00000000005113,-60.9327746859086)) ;
#195650 = CARTESIAN_POINT('Ctrl Pts',(-66.268759258637,-4.19999999994888,
-60.9327746859087)) ;
#195651 = CARTESIAN_POINT('Ctrl Pts',(-63.5207379488454,3.0000000000511,-58.1516435821762)) ;
#195652 = CARTESIAN_POINT('Ctrl Pts',(-63.5207379488454,-4.1999999999489,
-58.1516435821762)) ;
#195653 = CARTESIAN_POINT('Ctrl Pts',(-57.3860839754599,3.00000000005116,
-64.0903006017057)) ;
#195654 = CARTESIAN_POINT('Ctrl Pts',(-57.3860839754599,-4.19999999994884,
-64.0903006017058)) ;
#195655 = CARTESIAN_POINT('',(-57.3860839754598,3.00000000005116,-64.0903006017057)) ;
#195656 = CARTESIAN_POINT('Origin',(-60.0566078658523,3.0000000000512,-67.0709694600124)) ;
#195657 = CARTESIAN_POINT('',(-57.3860839754598,-2.99999999994884,-64.0903006017058)) ;
#195658 = CARTESIAN_POINT('',(-57.3860839754598,3.00000000005116,-64.0903006017057)) ;
#195659 = CARTESIAN_POINT('Origin',(-60.0566078658524,-2.9999999999488,-67.0709694600122)) ;
#195660 = CARTESIAN_POINT('Origin',(-58.7213459206564,3.00000000005118,-65.5806350308578)) ;
#195661 = CARTESIAN_POINT('',(-60.0566078658526,3.00000000005119,-67.0709694600098)) ;
#195662 = CARTESIAN_POINT('',(-57.3860839754598,3.00000000005116,-64.0903006017057)) ;
#195663 = CARTESIAN_POINT('',(-60.0566078658526,-2.99999999994881,-67.0709694600099)) ;
#195664 = CARTESIAN_POINT('',(-60.0566078658526,3.00000000005119,-67.0709694600098)) ;
#195665 = CARTESIAN_POINT('',(-57.3860839754598,-2.99999999994884,-64.0903006017058)) ;
#195666 = CARTESIAN_POINT('Origin',(-59.799456913753,3.0000000000512,-67.2995970106399)) ;
#195667 = CARTESIAN_POINT('',(-59.5423059616533,3.0000000000512,-67.52822456127)) ;
#195668 = CARTESIAN_POINT('',(-60.0566078658526,3.00000000005119,-67.0709694600098)) ;
#195669 = CARTESIAN_POINT('',(-59.5423059616533,-2.9999999999488,-67.5282245612701)) ;
#195670 = CARTESIAN_POINT('',(-59.5423059616533,3.0000000000512,-67.52822456127)) ;
#195671 = CARTESIAN_POINT('',(-60.0566078658526,-2.99999999994881,-67.0709694600099)) ;
#195672 = CARTESIAN_POINT('Ctrl Pts',(-59.5423059616532,3.0000000000512,-67.52822456127)) ;
#195673 = CARTESIAN_POINT('Ctrl Pts',(-59.5423059616532,-4.19999999994881,
-67.5282245612701)) ;
#195674 = CARTESIAN_POINT('Ctrl Pts',(-59.5414850140409,3.0000000000512,-67.5271952380677)) ;
#195675 = CARTESIAN_POINT('Ctrl Pts',(-59.5414850140409,-4.19999999994881,
-67.5271952380678)) ;
#195676 = CARTESIAN_POINT('Ctrl Pts',(-59.5406625872325,3.0000000000512,-67.5261670977339)) ;
#195677 = CARTESIAN_POINT('Ctrl Pts',(-59.5406625872325,-4.19999999994881,
-67.526167097734)) ;
#195678 = CARTESIAN_POINT('Ctrl Pts',(-57.0984025861253,3.00000000005117,
-64.4730248766433)) ;
#195679 = CARTESIAN_POINT('Ctrl Pts',(-57.0984025861253,-4.19999999994884,
-64.4730248766434)) ;
#195680 = CARTESIAN_POINT('Ctrl Pts',(-50.3765961969604,3.00000000005122,
-69.7379033591308)) ;
#195681 = CARTESIAN_POINT('Ctrl Pts',(-50.3765961969604,-4.19999999994878,
-69.7379033591309)) ;
#195682 = CARTESIAN_POINT('',(-50.3765961969605,3.00000000005122,-69.7379033591309)) ;
#195683 = CARTESIAN_POINT('Origin',(-52.7209259427919,3.00000000005125,-72.9813895599401)) ;
#195684 = CARTESIAN_POINT('',(-50.3765961969605,-2.99999999994878,-69.7379033591309)) ;
#195685 = CARTESIAN_POINT('',(-50.3765961969605,3.00000000005122,-69.7379033591309)) ;
#195686 = CARTESIAN_POINT('Origin',(-52.7209259427916,-2.99999999994874,-72.9813895599407)) ;
#195687 = CARTESIAN_POINT('Origin',(-51.5487610698761,3.00000000005124,-71.3596464595349)) ;
#195688 = CARTESIAN_POINT('',(-52.720925942792,3.00000000005125,-72.9813895599391)) ;
#195689 = CARTESIAN_POINT('',(-50.3765961969605,3.00000000005122,-69.7379033591309)) ;
#195690 = CARTESIAN_POINT('',(-52.720925942792,-2.99999999994875,-72.9813895599392)) ;
#195691 = CARTESIAN_POINT('',(-52.7209259427919,3.00000000005125,-72.9813895599391)) ;
#195692 = CARTESIAN_POINT('',(-50.3765961969605,-2.99999999994878,-69.7379033591309)) ;
#195693 = CARTESIAN_POINT('Origin',(-52.4412856039857,3.00000000005126,-73.1818850710742)) ;
#195694 = CARTESIAN_POINT('',(-52.1616452651797,3.00000000005126,-73.3823805822094)) ;
#195695 = CARTESIAN_POINT('',(-52.7209259427919,3.00000000005125,-72.9813895599391)) ;
#195696 = CARTESIAN_POINT('',(-52.1616452651797,-2.99999999994874,-73.3823805822095)) ;
#195697 = CARTESIAN_POINT('',(-52.1616452651797,3.00000000005126,-73.3823805822094)) ;
#195698 = CARTESIAN_POINT('',(-52.7209259427919,-2.99999999994874,-72.9813895599392)) ;
#195699 = CARTESIAN_POINT('Ctrl Pts',(-52.1616452651797,3.00000000005126,
-73.3823805822094)) ;
#195700 = CARTESIAN_POINT('Ctrl Pts',(-52.1616452651797,-4.19999999994875,
-73.3823805822095)) ;
#195701 = CARTESIAN_POINT('Ctrl Pts',(-52.1609364083768,3.00000000005126,
-73.3812710853549)) ;
#195702 = CARTESIAN_POINT('Ctrl Pts',(-52.1609364083768,-4.19999999994875,
-73.3812710853549)) ;
#195703 = CARTESIAN_POINT('Ctrl Pts',(-52.1602259568379,3.00000000005126,
-73.3801626102712)) ;
#195704 = CARTESIAN_POINT('Ctrl Pts',(-52.1602259568379,-4.19999999994875,
-73.3801626102713)) ;
#195705 = CARTESIAN_POINT('Ctrl Pts',(-50.0504851760628,3.00000000005122,
-70.0884601369073)) ;
#195706 = CARTESIAN_POINT('Ctrl Pts',(-50.0504851760628,-4.19999999994878,
-70.0884601369073)) ;
#195707 = CARTESIAN_POINT('Ctrl Pts',(-42.8151718885463,3.00000000005127,
-74.6218769719522)) ;
#195708 = CARTESIAN_POINT('Ctrl Pts',(-42.8151718885463,-4.19999999994874,
-74.6218769719522)) ;
#195709 = CARTESIAN_POINT('',(-42.8151718885463,3.00000000005127,-74.6218769719522)) ;
#195710 = CARTESIAN_POINT('Origin',(-44.8076225225372,3.00000000005131,-78.0926442017079)) ;
#195711 = CARTESIAN_POINT('',(-42.8151718885463,-2.99999999994873,-74.6218769719522)) ;
#195712 = CARTESIAN_POINT('',(-42.8151718885463,3.00000000005127,-74.6218769719522)) ;
#195713 = CARTESIAN_POINT('Origin',(-44.8076225225367,-2.99999999994869,-78.0926442017088)) ;
#195714 = CARTESIAN_POINT('Origin',(-43.8113972055423,3.00000000005129,-76.3572605868288)) ;
#195715 = CARTESIAN_POINT('',(-44.8076225225385,3.00000000005131,-78.0926442017055)) ;
#195716 = CARTESIAN_POINT('',(-42.8151718885463,3.00000000005127,-74.6218769719522)) ;
#195717 = CARTESIAN_POINT('',(-44.8076225225385,-2.99999999994869,-78.0926442017056)) ;
#195718 = CARTESIAN_POINT('',(-44.8076225225385,3.00000000005131,-78.0926442017055)) ;
#195719 = CARTESIAN_POINT('',(-42.8151718885463,-2.99999999994873,-74.6218769719522)) ;
#195720 = CARTESIAN_POINT('Origin',(-44.5085565950966,3.00000000005131,-78.2628110025695)) ;
#195721 = CARTESIAN_POINT('',(-44.2094906676548,3.00000000005131,-78.4329778034335)) ;
#195722 = CARTESIAN_POINT('',(-44.8076225225385,3.00000000005131,-78.0926442017055)) ;
#195723 = CARTESIAN_POINT('',(-44.2094906676548,-2.99999999994869,-78.4329778034335)) ;
#195724 = CARTESIAN_POINT('',(-44.2094906676548,3.00000000005131,-78.4329778034335)) ;
#195725 = CARTESIAN_POINT('',(-44.8076225225385,-2.99999999994869,-78.0926442017056)) ;
#195726 = CARTESIAN_POINT('Ctrl Pts',(-44.2094906676548,3.00000000005131,
-78.4329778034335)) ;
#195727 = CARTESIAN_POINT('Ctrl Pts',(-44.2094906676548,-4.1999999999487,
-78.4329778034335)) ;
#195728 = CARTESIAN_POINT('Ctrl Pts',(-44.2089016680447,3.00000000005131,
-78.4318002888068)) ;
#195729 = CARTESIAN_POINT('Ctrl Pts',(-44.2089016680447,-4.19999999994869,
-78.4318002888068)) ;
#195730 = CARTESIAN_POINT('Ctrl Pts',(-44.2083109756307,3.00000000005131,
-78.4306236236576)) ;
#195731 = CARTESIAN_POINT('Ctrl Pts',(-44.2083109756307,-4.19999999994869,
-78.4306236236577)) ;
#195732 = CARTESIAN_POINT('Ctrl Pts',(-42.4542041766736,3.00000000005127,
-74.936425479152)) ;
#195733 = CARTESIAN_POINT('Ctrl Pts',(-42.4542041766736,-4.19999999994873,
-74.9364254791521)) ;
#195734 = CARTESIAN_POINT('Ctrl Pts',(-34.7846555972706,3.00000000005131,
-78.6887116032311)) ;
#195735 = CARTESIAN_POINT('Ctrl Pts',(-34.7846555972706,-4.19999999994869,
-78.6887116032311)) ;
#195736 = CARTESIAN_POINT('',(-34.7846555972706,3.00000000005131,-78.688711603231)) ;
#195737 = CARTESIAN_POINT('Origin',(-36.4033974133306,3.00000000005135,-82.3487334098553)) ;
#195738 = CARTESIAN_POINT('',(-34.7846555972706,-2.99999999994869,-78.688711603231)) ;
#195739 = CARTESIAN_POINT('',(-34.7846555972706,3.00000000005131,-78.688711603231)) ;
#195740 = CARTESIAN_POINT('Origin',(-36.4033974133303,-2.99999999994865,-82.3487334098556)) ;
#195741 = CARTESIAN_POINT('Origin',(-35.5940265053004,3.00000000005133,-80.5187225065432)) ;
#195742 = CARTESIAN_POINT('',(-36.4033974133301,3.00000000005135,-82.3487334098552)) ;
#195743 = CARTESIAN_POINT('',(-34.7846555972706,3.00000000005131,-78.688711603231)) ;
#195744 = CARTESIAN_POINT('',(-36.4033974133301,-2.99999999994865,-82.3487334098553)) ;
#195745 = CARTESIAN_POINT('',(-36.4033974133301,3.00000000005135,-82.3487334098552)) ;
#195746 = CARTESIAN_POINT('',(-34.7846555972706,-2.99999999994869,-78.688711603231)) ;
#195747 = CARTESIAN_POINT('Origin',(-36.0881825261373,3.00000000005135,-82.486707117368)) ;
#195748 = CARTESIAN_POINT('',(-35.7729676389441,3.00000000005135,-82.6246808248807)) ;
#195749 = CARTESIAN_POINT('',(-36.4033974133301,3.00000000005135,-82.3487334098552)) ;
#195750 = CARTESIAN_POINT('',(-35.7729676389441,-2.99999999994865,-82.6246808248808)) ;
#195751 = CARTESIAN_POINT('',(-35.7729676389441,3.00000000005135,-82.6246808248807)) ;
#195752 = CARTESIAN_POINT('',(-36.4033974133301,-2.99999999994865,-82.3487334098553)) ;
#195753 = CARTESIAN_POINT('Ctrl Pts',(-35.7729676389442,3.00000000005135,
-82.6246808248807)) ;
#195754 = CARTESIAN_POINT('Ctrl Pts',(-35.7729676389442,-4.19999999994865,
-82.6246808248808)) ;
#195755 = CARTESIAN_POINT('Ctrl Pts',(-35.7725049497304,3.00000000005135,
-82.623448193578)) ;
#195756 = CARTESIAN_POINT('Ctrl Pts',(-35.7725049497304,-4.19999999994865,
-82.6234481935781)) ;
#195757 = CARTESIAN_POINT('Ctrl Pts',(-35.7720404881909,3.00000000005135,
-82.6222162301533)) ;
#195758 = CARTESIAN_POINT('Ctrl Pts',(-35.7720404881909,-4.19999999994865,
-82.6222162301534)) ;
#195759 = CARTESIAN_POINT('Ctrl Pts',(-34.3927860322115,3.00000000005132,
-78.9638055805851)) ;
#195760 = CARTESIAN_POINT('Ctrl Pts',(-34.3927860322115,-4.19999999994869,
-78.9638055805852)) ;
#195761 = CARTESIAN_POINT('Ctrl Pts',(-26.3730313401139,3.00000000005135,
-81.8938501617067)) ;
#195762 = CARTESIAN_POINT('Ctrl Pts',(-26.3730313401139,-4.19999999994866,
-81.8938501617068)) ;
#195763 = CARTESIAN_POINT('',(-26.3730313401137,3.00000000005134,-81.8938501617067)) ;
#195764 = CARTESIAN_POINT('Origin',(-27.6003290641614,3.00000000005139,-85.7030265803784)) ;
#195765 = CARTESIAN_POINT('',(-26.3730313401137,-2.99999999994865,-81.8938501617068)) ;
#195766 = CARTESIAN_POINT('',(-26.3730313401137,3.00000000005135,-81.8938501617067)) ;
#195767 = CARTESIAN_POINT('Origin',(-27.6003290641614,-2.99999999994862,-85.7030265803784)) ;
#195768 = CARTESIAN_POINT('Origin',(-26.9866802021376,3.00000000005137,-83.798438371043)) ;
#195769 = CARTESIAN_POINT('',(-27.6003290641611,3.00000000005138,-85.7030265803795)) ;
#195770 = CARTESIAN_POINT('',(-26.3730313401137,3.00000000005135,-81.8938501617067)) ;
#195771 = CARTESIAN_POINT('',(-27.6003290641611,-2.99999999994862,-85.7030265803796)) ;
#195772 = CARTESIAN_POINT('',(-27.6003290641611,3.00000000005138,-85.7030265803795)) ;
#195773 = CARTESIAN_POINT('',(-26.3730313401137,-2.99999999994865,-81.8938501617068)) ;
#195774 = CARTESIAN_POINT('Origin',(-27.272418777484,3.00000000005138,-85.8072955257288)) ;
#195775 = CARTESIAN_POINT('',(-26.9445084908068,3.00000000005139,-85.9115644710781)) ;
#195776 = CARTESIAN_POINT('',(-27.6003290641611,3.00000000005138,-85.7030265803795)) ;
#195777 = CARTESIAN_POINT('',(-26.9445084908068,-2.99999999994861,-85.9115644710782)) ;
#195778 = CARTESIAN_POINT('',(-26.9445084908068,3.00000000005139,-85.9115644710781)) ;
#195779 = CARTESIAN_POINT('',(-27.6003290641611,-2.99999999994862,-85.7030265803796)) ;
#195780 = CARTESIAN_POINT('Ctrl Pts',(-26.9445084908069,3.00000000005139,
-85.9115644710781)) ;
#195781 = CARTESIAN_POINT('Ctrl Pts',(-26.9445084908069,-4.19999999994862,
-85.9115644710782)) ;
#195782 = CARTESIAN_POINT('Ctrl Pts',(-26.9441771813088,3.00000000005139,
-85.9102902280661)) ;
#195783 = CARTESIAN_POINT('Ctrl Pts',(-26.9441771813088,-4.19999999994862,
-85.9102902280662)) ;
#195784 = CARTESIAN_POINT('Ctrl Pts',(-26.9438440393815,3.00000000005139,
-85.9090164640151)) ;
#195785 = CARTESIAN_POINT('Ctrl Pts',(-26.9438440393815,-4.19999999994862,
-85.9090164640151)) ;
#195786 = CARTESIAN_POINT('Ctrl Pts',(-25.9545533268275,3.00000000005135,
-82.1264756220326)) ;
#195787 = CARTESIAN_POINT('Ctrl Pts',(-25.9545533268275,-4.19999999994866,
-82.1264756220326)) ;
#195788 = CARTESIAN_POINT('Ctrl Pts',(-17.6724586326836,3.00000000005137,
-84.2021764786145)) ;
#195789 = CARTESIAN_POINT('Ctrl Pts',(-17.6724586326836,-4.19999999994864,
-84.2021764786145)) ;
#195790 = CARTESIAN_POINT('',(-17.6724586326835,3.00000000005137,-84.2021764786144)) ;
#195791 = CARTESIAN_POINT('Origin',(-18.4948657340208,3.00000000005141,-88.1187733753747)) ;
#195792 = CARTESIAN_POINT('',(-17.6724586326835,-2.99999999994863,-84.2021764786145)) ;
#195793 = CARTESIAN_POINT('',(-17.6724586326835,3.00000000005137,-84.2021764786144)) ;
#195794 = CARTESIAN_POINT('Origin',(-18.4948657340221,-2.99999999994859,-88.1187733753737)) ;
#195795 = CARTESIAN_POINT('Origin',(-18.0836621833542,3.00000000005139,-86.1604749269931)) ;
#195796 = CARTESIAN_POINT('',(-18.4948657340249,3.00000000005141,-88.1187733753717)) ;
#195797 = CARTESIAN_POINT('',(-17.6724586326835,3.00000000005137,-84.2021764786144)) ;
#195798 = CARTESIAN_POINT('',(-18.4948657340249,-2.99999999994859,-88.1187733753718)) ;
#195799 = CARTESIAN_POINT('',(-18.4948657340249,3.00000000005141,-88.1187733753717)) ;
#195800 = CARTESIAN_POINT('',(-17.6724586326835,-2.99999999994863,-84.2021764786145)) ;
#195801 = CARTESIAN_POINT('Origin',(-18.157852701584,3.00000000005141,-88.1881951661725)) ;
#195802 = CARTESIAN_POINT('',(-17.820839669143,3.00000000005141,-88.2576169569733)) ;
#195803 = CARTESIAN_POINT('',(-18.4948657340249,3.00000000005141,-88.1187733753717)) ;
#195804 = CARTESIAN_POINT('',(-17.820839669143,-2.99999999994859,-88.2576169569734)) ;
#195805 = CARTESIAN_POINT('',(-17.820839669143,3.00000000005141,-88.2576169569733)) ;
#195806 = CARTESIAN_POINT('',(-18.4948657340249,-2.99999999994859,-88.1187733753718)) ;
#195807 = CARTESIAN_POINT('Ctrl Pts',(-17.8208396691431,3.00000000005141,
-88.2576169569734)) ;
#195808 = CARTESIAN_POINT('Ctrl Pts',(-17.8208396691431,-4.19999999994862,
-88.2576169569734)) ;
#195809 = CARTESIAN_POINT('Ctrl Pts',(-17.8206433692572,3.00000000005141,
-88.2563150631251)) ;
#195810 = CARTESIAN_POINT('Ctrl Pts',(-17.8206433692572,-4.19999999994862,
-88.2563150631251)) ;
#195811 = CARTESIAN_POINT('Ctrl Pts',(-17.820445196915,3.00000000005141,-88.2550134540732)) ;
#195812 = CARTESIAN_POINT('Ctrl Pts',(-17.820445196915,-4.19999999994862,
-88.2550134540732)) ;
#195813 = CARTESIAN_POINT('Ctrl Pts',(-17.2319571038551,3.00000000005137,
-84.3897847286881)) ;
#195814 = CARTESIAN_POINT('Ctrl Pts',(-17.2319571038551,-4.19999999994866,
-84.3897847286881)) ;
#195815 = CARTESIAN_POINT('Ctrl Pts',(-8.77826277027359,3.00000000005138,
-85.588400047778)) ;
#195816 = CARTESIAN_POINT('Ctrl Pts',(-8.77826277027359,-4.19999999994865,
-85.588400047778)) ;
#195817 = CARTESIAN_POINT('',(-8.77826277027339,3.00000000005138,-85.5884000477779)) ;
#195818 = CARTESIAN_POINT('Origin',(-9.18676878460829,3.00000000005142,-89.5695063674171)) ;
#195819 = CARTESIAN_POINT('',(-8.77826277027339,-2.99999999994862,-85.5884000477779)) ;
#195820 = CARTESIAN_POINT('',(-8.77826277027339,3.00000000005138,-85.5884000477779)) ;
#195821 = CARTESIAN_POINT('Origin',(-9.18676878460891,-2.99999999994858,-89.5695063674169)) ;
#195822 = CARTESIAN_POINT('Origin',(-8.98251577744032,3.0000000000514,-87.578953207598)) ;
#195823 = CARTESIAN_POINT('',(-9.18676878460678,3.00000000005142,-89.5695063674181)) ;
#195824 = CARTESIAN_POINT('',(-8.77826277027339,3.00000000005138,-85.5884000477779)) ;
#195825 = CARTESIAN_POINT('',(-9.18676878460678,-2.99999999994858,-89.5695063674181)) ;
#195826 = CARTESIAN_POINT('',(-9.18676878460679,3.00000000005143,-89.5695063674181)) ;
#195827 = CARTESIAN_POINT('',(-8.77826277027339,-2.99999999994862,-85.5884000477779)) ;
#195828 = CARTESIAN_POINT('Origin',(-8.84434539171035,3.00000000005142,-89.603320404003)) ;
#195829 = CARTESIAN_POINT('',(-8.50192199881371,3.00000000005142,-89.6371344405877)) ;
#195830 = CARTESIAN_POINT('',(-9.18676878460679,3.00000000005143,-89.5695063674181)) ;
#195831 = CARTESIAN_POINT('',(-8.50192199881371,-2.99999999994858,-89.6371344405878)) ;
#195832 = CARTESIAN_POINT('',(-8.50192199881372,3.00000000005143,-89.6371344405877)) ;
#195833 = CARTESIAN_POINT('',(-9.18676878460679,-2.99999999994858,-89.5695063674182)) ;
#195834 = CARTESIAN_POINT('Ctrl Pts',(-8.50192199881377,3.00000000005142,
-89.6371344405878)) ;
#195835 = CARTESIAN_POINT('Ctrl Pts',(-8.50192199881377,-4.19999999994858,
-89.6371344405879)) ;
#195836 = CARTESIAN_POINT('Ctrl Pts',(-8.50186285924238,3.00000000005143,
-89.635819159725)) ;
#195837 = CARTESIAN_POINT('Ctrl Pts',(-8.50186285924238,-4.19999999994858,
-89.6358191597251)) ;
#195838 = CARTESIAN_POINT('Ctrl Pts',(-8.50180182770284,3.00000000005142,
-89.6345039663731)) ;
#195839 = CARTESIAN_POINT('Ctrl Pts',(-8.50180182770284,-4.19999999994858,
-89.6345039663732)) ;
#195840 = CARTESIAN_POINT('Ctrl Pts',(-8.32056395283379,3.00000000005138,
-85.7289356123527)) ;
#195841 = CARTESIAN_POINT('Ctrl Pts',(-8.32056395283379,-4.19999999994862,
-85.7289356123528)) ;
#195842 = CARTESIAN_POINT('Ctrl Pts',(0.212109576017282,3.00000000005139,
-86.0373331136874)) ;
#195843 = CARTESIAN_POINT('Ctrl Pts',(0.212109576017282,-4.19999999994861,
-86.0373331136875)) ;
#195844 = CARTESIAN_POINT('',(0.212109576017269,3.00000000005139,-86.0373331136874)) ;
#195845 = CARTESIAN_POINT('Origin',(0.221980326072865,3.00000000005143,-90.0393310222739)) ;
#195846 = CARTESIAN_POINT('',(0.212109576017269,-2.99999999994861,-86.0373331136874)) ;
#195847 = CARTESIAN_POINT('',(0.212109576017269,3.00000000005139,-86.0373331136874)) ;
#195848 = CARTESIAN_POINT('Origin',(0.221980326071444,-2.99999999994857,-90.0393310222733)) ;
#195849 = CARTESIAN_POINT('Origin',(0.217044951043621,3.00000000005141,-88.0383320679796)) ;
#195850 = CARTESIAN_POINT('',(0.221980326069911,3.00000000005143,-90.039331022272)) ;
#195851 = CARTESIAN_POINT('',(0.212109576017269,3.00000000005139,-86.0373331136874)) ;
#195852 = CARTESIAN_POINT('',(0.221980326069911,-2.99999999994857,-90.0393310222721)) ;
#195853 = CARTESIAN_POINT('',(0.221980326069911,3.00000000005143,-90.039331022272)) ;
#195854 = CARTESIAN_POINT('',(0.212109576017269,-2.99999999994861,-86.0373331136874)) ;
#195855 = CARTESIAN_POINT('Origin',(0.56606241707283,3.00000000005143,-90.0371668309801)) ;
#195856 = CARTESIAN_POINT('',(0.910144508075746,3.00000000005143,-90.0350026396881)) ;
#195857 = CARTESIAN_POINT('',(0.221980326069911,3.00000000005143,-90.039331022272)) ;
#195858 = CARTESIAN_POINT('',(0.910144508075746,-2.99999999994857,-90.0350026396881)) ;
#195859 = CARTESIAN_POINT('',(0.910144508075746,3.00000000005143,-90.0350026396881)) ;
#195860 = CARTESIAN_POINT('',(0.221980326069911,-2.99999999994857,-90.0393310222721)) ;
#195861 = CARTESIAN_POINT('Ctrl Pts',(0.910144508075857,3.00000000005143,
-90.0350026396881)) ;
#195862 = CARTESIAN_POINT('Ctrl Pts',(0.910144508075857,-4.19999999994857,
-90.0350026396882)) ;
#195863 = CARTESIAN_POINT('Ctrl Pts',(0.910065839387194,3.00000000005143,
-90.0336883823031)) ;
#195864 = CARTESIAN_POINT('Ctrl Pts',(0.910065839387194,-4.19999999994857,
-90.0336883823032)) ;
#195865 = CARTESIAN_POINT('Ctrl Pts',(0.909989061449121,3.00000000005143,
-90.0323740141851)) ;
#195866 = CARTESIAN_POINT('Ctrl Pts',(0.909989061449121,-4.19999999994857,
-90.0323740141852)) ;
#195867 = CARTESIAN_POINT('Ctrl Pts',(0.681991038044217,3.00000000005139,
-86.1292562557081)) ;
#195868 = CARTESIAN_POINT('Ctrl Pts',(0.681991038044217,-4.19999999994861,
-86.1292562557082)) ;
#195869 = CARTESIAN_POINT('Ctrl Pts',(9.20015800540581,3.00000000005138,-85.544057071727)) ;
#195870 = CARTESIAN_POINT('Ctrl Pts',(9.20015800540581,-4.19999999994862,
-85.5440570717271)) ;
#195871 = CARTESIAN_POINT('',(9.2001580054058,3.00000000005138,-85.544057071727)) ;
#195872 = CARTESIAN_POINT('Origin',(9.62829737384105,3.00000000005142,-89.5230998426979)) ;
#195873 = CARTESIAN_POINT('',(9.2001580054058,-2.99999999994862,-85.5440570717271)) ;
#195874 = CARTESIAN_POINT('',(9.2001580054058,3.00000000005138,-85.544057071727)) ;
#195875 = CARTESIAN_POINT('Origin',(9.62829737384009,-2.99999999994858,-89.5230998426976)) ;
#195876 = CARTESIAN_POINT('Origin',(9.41422768962381,3.0000000000514,-87.5335784572127)) ;
#195877 = CARTESIAN_POINT('',(9.62829737384209,3.00000000005142,-89.5230998426984)) ;
#195878 = CARTESIAN_POINT('',(9.2001580054058,3.00000000005138,-85.544057071727)) ;
#195879 = CARTESIAN_POINT('',(9.62829737384209,-2.99999999994858,-89.5230998426985)) ;
#195880 = CARTESIAN_POINT('',(9.62829737384209,3.00000000005142,-89.5230998426984)) ;
#195881 = CARTESIAN_POINT('',(9.2001580054058,-2.99999999994862,-85.5440570717271)) ;
#195882 = CARTESIAN_POINT('Origin',(9.97026832755857,3.00000000005142,-89.4849811348624)) ;
#195883 = CARTESIAN_POINT('',(10.3122392812754,3.00000000005142,-89.4468624270263)) ;
#195884 = CARTESIAN_POINT('',(9.62829737384209,3.00000000005142,-89.5230998426984)) ;
#195885 = CARTESIAN_POINT('',(10.3122392812754,-2.99999999994858,-89.4468624270264)) ;
#195886 = CARTESIAN_POINT('',(10.3122392812754,3.00000000005142,-89.4468624270263)) ;
#195887 = CARTESIAN_POINT('',(9.62829737384209,-2.99999999994858,-89.5230998426985)) ;
#195888 = CARTESIAN_POINT('Ctrl Pts',(10.3122392812753,3.00000000005142,-89.4468624270263)) ;
#195889 = CARTESIAN_POINT('Ctrl Pts',(10.3122392812753,-4.19999999994858,
-89.4468624270264)) ;
#195890 = CARTESIAN_POINT('Ctrl Pts',(10.312023666237,3.00000000005142,-89.4455635923977)) ;
#195891 = CARTESIAN_POINT('Ctrl Pts',(10.312023666237,-4.19999999994858,-89.4455635923978)) ;
#195892 = CARTESIAN_POINT('Ctrl Pts',(10.3118099200172,3.00000000005142,-89.4442644500057)) ;
#195893 = CARTESIAN_POINT('Ctrl Pts',(10.3118099200172,-4.19999999994858,
-89.4442644500058)) ;
#195894 = CARTESIAN_POINT('Ctrl Pts',(9.67707399239405,3.00000000005138,-85.5863606620143)) ;
#195895 = CARTESIAN_POINT('Ctrl Pts',(9.67707399239405,-4.19999999994862,
-85.5863606620144)) ;
#195896 = CARTESIAN_POINT('Ctrl Pts',(18.0874075784307,3.00000000005137,-84.1139763574378)) ;
#195897 = CARTESIAN_POINT('Ctrl Pts',(18.0874075784307,-4.19999999994863,
-84.1139763574379)) ;
#195898 = CARTESIAN_POINT('',(18.0874075784309,3.00000000005137,-84.1139763574378)) ;
#195899 = CARTESIAN_POINT('Origin',(18.9291247807328,3.00000000005141,-88.0264687655279)) ;
#195900 = CARTESIAN_POINT('',(18.0874075784309,-2.99999999994863,-84.1139763574379)) ;
#195901 = CARTESIAN_POINT('',(18.0874075784309,3.00000000005137,-84.1139763574378)) ;
#195902 = CARTESIAN_POINT('Origin',(18.9291247807335,-2.99999999994859,-88.026468765528)) ;
#195903 = CARTESIAN_POINT('Origin',(18.5082661795829,3.00000000005139,-86.0702225614833)) ;
#195904 = CARTESIAN_POINT('',(18.9291247807354,3.00000000005141,-88.026468765529)) ;
#195905 = CARTESIAN_POINT('',(18.0874075784309,3.00000000005137,-84.1139763574378)) ;
#195906 = CARTESIAN_POINT('',(18.9291247807354,-2.99999999994859,-88.026468765529)) ;
#195907 = CARTESIAN_POINT('',(18.9291247807354,3.00000000005141,-88.026468765529)) ;
#195908 = CARTESIAN_POINT('',(18.0874075784309,-2.99999999994863,-84.1139763574379)) ;
#195909 = CARTESIAN_POINT('Origin',(19.2652378918346,3.00000000005141,-87.9528131776886)) ;
#195910 = CARTESIAN_POINT('',(19.6013510029341,3.00000000005141,-87.8791575898483)) ;
#195911 = CARTESIAN_POINT('',(18.9291247807354,3.00000000005141,-88.026468765529)) ;
#195912 = CARTESIAN_POINT('',(19.6013510029341,-2.99999999994859,-87.8791575898484)) ;
#195913 = CARTESIAN_POINT('',(19.6013510029341,3.00000000005141,-87.8791575898483)) ;
#195914 = CARTESIAN_POINT('',(18.9291247807354,-2.99999999994859,-88.026468765529)) ;
#195915 = CARTESIAN_POINT('Ctrl Pts',(19.601351002934,3.00000000005141,-87.8791575898484)) ;
#195916 = CARTESIAN_POINT('Ctrl Pts',(19.601351002934,-4.19999999994859,-87.8791575898484)) ;
#195917 = CARTESIAN_POINT('Ctrl Pts',(19.6010008038698,3.00000000005141,-87.8778884082803)) ;
#195918 = CARTESIAN_POINT('Ctrl Pts',(19.6010008038698,-4.19999999994859,
-87.8778884082804)) ;
#195919 = CARTESIAN_POINT('Ctrl Pts',(19.6006524312164,3.00000000005141,-87.8766187252903)) ;
#195920 = CARTESIAN_POINT('Ctrl Pts',(19.6006524312164,-4.19999999994859,
-87.8766187252903)) ;
#195921 = CARTESIAN_POINT('Ctrl Pts',(18.5661328990248,3.00000000005137,-84.1061969090035)) ;
#195922 = CARTESIAN_POINT('Ctrl Pts',(18.5661328990248,-4.19999999994863,
-84.1061969090036)) ;
#195923 = CARTESIAN_POINT('Ctrl Pts',(26.7764877289929,3.00000000005134,-81.7627592343891)) ;
#195924 = CARTESIAN_POINT('Ctrl Pts',(26.7764877289929,-4.19999999994866,
-81.7627592343892)) ;
#195925 = CARTESIAN_POINT('',(26.7764877289931,3.00000000005134,-81.7627592343891)) ;
#195926 = CARTESIAN_POINT('Origin',(28.0225607353579,3.00000000005138,-85.5658351940353)) ;
#195927 = CARTESIAN_POINT('',(26.7764877289931,-2.99999999994866,-81.7627592343891)) ;
#195928 = CARTESIAN_POINT('',(26.7764877289931,3.00000000005134,-81.7627592343891)) ;
#195929 = CARTESIAN_POINT('Origin',(28.022560735356,-2.99999999994862,-85.5658351940352)) ;
#195930 = CARTESIAN_POINT('Origin',(27.399524232175,3.00000000005136,-83.6642972142119)) ;
#195931 = CARTESIAN_POINT('',(28.0225607353573,3.00000000005138,-85.5658351940347)) ;
#195932 = CARTESIAN_POINT('',(26.7764877289931,3.00000000005134,-81.7627592343891)) ;
#195933 = CARTESIAN_POINT('',(28.0225607353573,-2.99999999994862,-85.5658351940348)) ;
#195934 = CARTESIAN_POINT('',(28.0225607353573,3.00000000005138,-85.5658351940347)) ;
#195935 = CARTESIAN_POINT('',(26.7764877289931,-2.99999999994866,-81.7627592343891)) ;
#195936 = CARTESIAN_POINT('Origin',(28.3491334782577,3.00000000005138,-85.4574497122239)) ;
#195937 = CARTESIAN_POINT('',(28.6757062211584,3.00000000005138,-85.3490642304132)) ;
#195938 = CARTESIAN_POINT('',(28.0225607353573,3.00000000005138,-85.5658351940347)) ;
#195939 = CARTESIAN_POINT('',(28.6757062211584,-2.99999999994862,-85.3490642304132)) ;
#195940 = CARTESIAN_POINT('',(28.6757062211584,3.00000000005138,-85.3490642304132)) ;
#195941 = CARTESIAN_POINT('',(28.0225607353573,-2.99999999994862,-85.5658351940348)) ;
#195942 = CARTESIAN_POINT('Ctrl Pts',(28.6757062211582,3.00000000005138,-85.3490642304131)) ;
#195943 = CARTESIAN_POINT('Ctrl Pts',(28.6757062211582,-4.19999999994862,
-85.3490642304132)) ;
#195944 = CARTESIAN_POINT('Ctrl Pts',(28.6752252749223,3.00000000005138,-85.3478386073249)) ;
#195945 = CARTESIAN_POINT('Ctrl Pts',(28.6752252749223,-4.19999999994862,
-85.347838607325)) ;
#195946 = CARTESIAN_POINT('Ctrl Pts',(28.6747460926787,3.00000000005138,-85.3466122946489)) ;
#195947 = CARTESIAN_POINT('Ctrl Pts',(28.6747460926787,-4.19999999994862,
-85.346612294649)) ;
#195948 = CARTESIAN_POINT('Ctrl Pts',(27.2517773684009,3.00000000005134,-81.704981980498)) ;
#195949 = CARTESIAN_POINT('Ctrl Pts',(27.2517773684009,-4.19999999994866,
-81.7049819804981)) ;
#195950 = CARTESIAN_POINT('Ctrl Pts',(35.1721990766558,3.00000000005131,-78.5161661294042)) ;
#195951 = CARTESIAN_POINT('Ctrl Pts',(35.1721990766558,-4.19999999994869,
-78.5161661294042)) ;
#195952 = CARTESIAN_POINT('',(35.1721990766558,3.00000000005131,-78.5161661294041)) ;
#195953 = CARTESIAN_POINT('Origin',(36.8089756504653,3.00000000005135,-82.1681583445459)) ;
#195954 = CARTESIAN_POINT('',(35.1721990766558,-2.99999999994869,-78.5161661294042)) ;
#195955 = CARTESIAN_POINT('',(35.1721990766558,3.00000000005131,-78.5161661294041)) ;
#195956 = CARTESIAN_POINT('Origin',(36.8089756504651,-2.99999999994865,-82.168158344546)) ;
#195957 = CARTESIAN_POINT('Origin',(35.9905873635602,3.00000000005133,-80.3421622369752)) ;
#195958 = CARTESIAN_POINT('',(36.8089756504646,3.00000000005135,-82.1681583445461)) ;
#195959 = CARTESIAN_POINT('',(35.1721990766558,3.00000000005131,-78.5161661294041)) ;
#195960 = CARTESIAN_POINT('',(36.8089756504646,-2.99999999994865,-82.1681583445461)) ;
#195961 = CARTESIAN_POINT('',(36.8089756504646,3.00000000005135,-82.1681583445461)) ;
#195962 = CARTESIAN_POINT('',(35.1721990766558,-2.99999999994869,-78.5161661294042)) ;
#195963 = CARTESIAN_POINT('Origin',(37.1224300258553,3.00000000005135,-82.0262304627848)) ;
#195964 = CARTESIAN_POINT('',(37.4358844012462,3.00000000005135,-81.8843025810235)) ;
#195965 = CARTESIAN_POINT('',(36.8089756504646,3.00000000005135,-82.1681583445461)) ;
#195966 = CARTESIAN_POINT('',(37.4358844012462,-2.99999999994866,-81.8843025810236)) ;
#195967 = CARTESIAN_POINT('',(37.4358844012462,3.00000000005135,-81.8843025810235)) ;
#195968 = CARTESIAN_POINT('',(36.8089756504646,-2.99999999994865,-82.1681583445461)) ;
#195969 = CARTESIAN_POINT('Ctrl Pts',(37.4358844012461,3.00000000005135,-81.8843025810236)) ;
#195970 = CARTESIAN_POINT('Ctrl Pts',(37.4358844012461,-4.19999999994867,
-81.8843025810236)) ;
#195971 = CARTESIAN_POINT('Ctrl Pts',(37.4352779771861,3.00000000005135,-81.8831339445975)) ;
#195972 = CARTESIAN_POINT('Ctrl Pts',(37.4352779771861,-4.19999999994867,
-81.8831339445976)) ;
#195973 = CARTESIAN_POINT('Ctrl Pts',(37.4346732353735,3.00000000005135,-81.8819644379744)) ;
#195974 = CARTESIAN_POINT('Ctrl Pts',(37.4346732353735,-4.19999999994867,
-81.8819644379745)) ;
#195975 = CARTESIAN_POINT('Ctrl Pts',(35.6388456621278,3.00000000005131,-78.4090240897414)) ;
#195976 = CARTESIAN_POINT('Ctrl Pts',(35.6388456621278,-4.1999999999487,-78.4090240897414)) ;
#195977 = CARTESIAN_POINT('Ctrl Pts',(43.1825564509792,3.00000000005127,-74.4097673959352)) ;
#195978 = CARTESIAN_POINT('Ctrl Pts',(43.1825564509792,-4.19999999994874,
-74.4097673959353)) ;
#195979 = CARTESIAN_POINT('',(43.1825564509793,3.00000000005127,-74.4097673959352)) ;
#195980 = CARTESIAN_POINT('Origin',(45.1921037255721,3.00000000005131,-77.8706638756356)) ;
#195981 = CARTESIAN_POINT('',(43.1825564509793,-2.99999999994873,-74.4097673959353)) ;
#195982 = CARTESIAN_POINT('',(43.1825564509793,3.00000000005127,-74.4097673959352)) ;
#195983 = CARTESIAN_POINT('Origin',(45.1921037255727,-2.99999999994869,-77.8706638756356)) ;
#195984 = CARTESIAN_POINT('Origin',(44.1873300882756,3.00000000005129,-76.1402156357854)) ;
#195985 = CARTESIAN_POINT('',(45.1921037255719,3.0000000000513,-77.8706638756355)) ;
#195986 = CARTESIAN_POINT('',(43.1825564509793,3.00000000005127,-74.4097673959352)) ;
#195987 = CARTESIAN_POINT('',(45.1921037255719,-2.9999999999487,-77.8706638756356)) ;
#195988 = CARTESIAN_POINT('',(45.1921037255719,3.00000000005131,-77.8706638756356)) ;
#195989 = CARTESIAN_POINT('',(43.1825564509793,-2.99999999994873,-74.4097673959353)) ;
#195990 = CARTESIAN_POINT('Origin',(45.4890054617218,3.0000000000513,-77.6967485854965)) ;
#195991 = CARTESIAN_POINT('',(45.7859071978719,3.0000000000513,-77.5228332953575)) ;
#195992 = CARTESIAN_POINT('',(45.1921037255719,3.00000000005131,-77.8706638756356)) ;
#195993 = CARTESIAN_POINT('',(45.7859071978719,-2.9999999999487,-77.5228332953575)) ;
#195994 = CARTESIAN_POINT('',(45.7859071978719,3.0000000000513,-77.5228332953575)) ;
#195995 = CARTESIAN_POINT('',(45.1921037255719,-2.9999999999487,-77.8706638756356)) ;
#195996 = CARTESIAN_POINT('Ctrl Pts',(45.7859071978719,3.0000000000513,-77.5228332953575)) ;
#195997 = CARTESIAN_POINT('Ctrl Pts',(45.7859071978719,-4.1999999999487,-77.5228332953576)) ;
#195998 = CARTESIAN_POINT('Ctrl Pts',(45.7851819400962,3.0000000000513,-77.5217344494193)) ;
#195999 = CARTESIAN_POINT('Ctrl Pts',(45.7851819400962,-4.1999999999487,-77.5217344494194)) ;
#196000 = CARTESIAN_POINT('Ctrl Pts',(45.7844582643926,3.0000000000513,-77.5206345622083)) ;
#196001 = CARTESIAN_POINT('Ctrl Pts',(45.7844582643926,-4.1999999999487,-77.5206345622084)) ;
#196002 = CARTESIAN_POINT('Ctrl Pts',(43.6354473048724,3.00000000005127,-74.2544344411075)) ;
#196003 = CARTESIAN_POINT('Ctrl Pts',(43.6354473048724,-4.19999999994873,
-74.2544344411076)) ;
#196004 = CARTESIAN_POINT('Ctrl Pts',(50.7197967002949,3.00000000005122,-69.4885535978252)) ;
#196005 = CARTESIAN_POINT('Ctrl Pts',(50.7197967002949,-4.19999999994878,
-69.4885535978253)) ;
#196006 = CARTESIAN_POINT('',(50.719796700295,3.00000000005122,-69.4885535978252)) ;
#196007 = CARTESIAN_POINT('Origin',(53.0800976552053,3.00000000005125,-72.7204360360131)) ;
#196008 = CARTESIAN_POINT('',(50.719796700295,-2.99999999994878,-69.4885535978253)) ;
#196009 = CARTESIAN_POINT('',(50.719796700295,3.00000000005122,-69.4885535978252)) ;
#196010 = CARTESIAN_POINT('Origin',(53.0800976552044,-2.99999999994875,-72.7204360360132)) ;
#196011 = CARTESIAN_POINT('Origin',(51.8999471777507,3.00000000005124,-71.1044948169192)) ;
#196012 = CARTESIAN_POINT('',(53.0800976552065,3.00000000005125,-72.7204360360133)) ;
#196013 = CARTESIAN_POINT('',(50.719796700295,3.00000000005122,-69.4885535978252)) ;
#196014 = CARTESIAN_POINT('',(53.0800976552065,-2.99999999994875,-72.7204360360134)) ;
#196015 = CARTESIAN_POINT('',(53.0800976552065,3.00000000005125,-72.7204360360133)) ;
#196016 = CARTESIAN_POINT('',(50.719796700295,-2.99999999994878,-69.4885535978253)) ;
#196017 = CARTESIAN_POINT('Origin',(53.3571938345634,3.00000000005125,-72.5164387898095)) ;
#196018 = CARTESIAN_POINT('',(53.6342900139205,3.00000000005125,-72.3124415436058)) ;
#196019 = CARTESIAN_POINT('',(53.0800976552065,3.00000000005125,-72.7204360360133)) ;
#196020 = CARTESIAN_POINT('',(53.6342900139205,-2.99999999994875,-72.3124415436058)) ;
#196021 = CARTESIAN_POINT('',(53.6342900139205,3.00000000005125,-72.3124415436058)) ;
#196022 = CARTESIAN_POINT('',(53.0800976552065,-2.99999999994875,-72.7204360360134)) ;
#196023 = CARTESIAN_POINT('Ctrl Pts',(53.6342900139204,3.00000000005125,-72.3124415436058)) ;
#196024 = CARTESIAN_POINT('Ctrl Pts',(53.6342900139204,-4.19999999994875,
-72.3124415436059)) ;
#196025 = CARTESIAN_POINT('Ctrl Pts',(53.6334538685055,3.00000000005125,-72.3114245273411)) ;
#196026 = CARTESIAN_POINT('Ctrl Pts',(53.6334538685055,-4.19999999994875,
-72.3114245273412)) ;
#196027 = CARTESIAN_POINT('Ctrl Pts',(53.6326191876532,3.00000000005125,-72.3104063101364)) ;
#196028 = CARTESIAN_POINT('Ctrl Pts',(53.6326191876532,-4.19999999994875,
-72.3104063101364)) ;
#196029 = CARTESIAN_POINT('Ctrl Pts',(51.153969855641,3.00000000005122,-69.2867315881914)) ;
#196030 = CARTESIAN_POINT('Ctrl Pts',(51.153969855641,-4.19999999994878,-69.2867315881915)) ;
#196031 = CARTESIAN_POINT('Ctrl Pts',(57.7013402431622,3.00000000005116,-63.8064425832762)) ;
#196032 = CARTESIAN_POINT('Ctrl Pts',(57.7013402431622,-4.19999999994884,
-63.8064425832763)) ;
#196033 = CARTESIAN_POINT('',(57.7013402431622,3.00000000005116,-63.8064425832762)) ;
#196034 = CARTESIAN_POINT('Origin',(60.38653492721,3.00000000005119,-66.7739017996431)) ;
#196035 = CARTESIAN_POINT('',(57.7013402431622,-2.99999999994884,-63.8064425832763)) ;
#196036 = CARTESIAN_POINT('',(57.7013402431622,3.00000000005116,-63.8064425832763)) ;
#196037 = CARTESIAN_POINT('Origin',(60.3865349272097,-2.99999999994881,-66.7739017996433)) ;
#196038 = CARTESIAN_POINT('Origin',(59.0439375851841,3.00000000005118,-65.2901721914601)) ;
#196039 = CARTESIAN_POINT('',(60.386534927206,3.00000000005119,-66.7739017996442)) ;
#196040 = CARTESIAN_POINT('',(57.7013402431622,3.00000000005116,-63.8064425832763)) ;
#196041 = CARTESIAN_POINT('',(60.386534927206,-2.99999999994881,-66.7739017996442)) ;
#196042 = CARTESIAN_POINT('',(60.386534927206,3.00000000005119,-66.7739017996442)) ;
#196043 = CARTESIAN_POINT('',(57.7013402431622,-2.99999999994884,-63.8064425832763)) ;
#196044 = CARTESIAN_POINT('Origin',(60.6407896260427,3.00000000005119,-66.5420576338941)) ;
#196045 = CARTESIAN_POINT('',(60.8950443248793,3.00000000005119,-66.3102134681442)) ;
#196046 = CARTESIAN_POINT('',(60.386534927206,3.00000000005119,-66.7739017996442)) ;
#196047 = CARTESIAN_POINT('',(60.8950443248793,-2.99999999994881,-66.3102134681442)) ;
#196048 = CARTESIAN_POINT('',(60.8950443248793,3.00000000005119,-66.3102134681442)) ;
#196049 = CARTESIAN_POINT('',(60.386534927206,-2.99999999994881,-66.7739017996443)) ;
#196050 = CARTESIAN_POINT('Ctrl Pts',(60.8950443248792,3.00000000005119,-66.3102134681441)) ;
#196051 = CARTESIAN_POINT('Ctrl Pts',(60.8950443248792,-4.19999999994881,
-66.3102134681442)) ;
#196052 = CARTESIAN_POINT('Ctrl Pts',(60.8941064528093,3.00000000005119,-66.3092894241962)) ;
#196053 = CARTESIAN_POINT('Ctrl Pts',(60.8941064528093,-4.19999999994881,
-66.3092894241963)) ;
#196054 = CARTESIAN_POINT('Ctrl Pts',(60.8931699117464,3.00000000005119,-66.3083640327988)) ;
#196055 = CARTESIAN_POINT('Ctrl Pts',(60.8931699117464,-4.19999999994881,
-66.3083640327988)) ;
#196056 = CARTESIAN_POINT('Ctrl Pts',(58.1120388080142,3.00000000005116,-63.5603427230073)) ;
#196057 = CARTESIAN_POINT('Ctrl Pts',(58.1120388080142,-4.19999999994884,
-63.5603427230074)) ;
#196058 = CARTESIAN_POINT('Ctrl Pts',(64.0506958275435,3.0000000000511,-57.4256887496219)) ;
#196059 = CARTESIAN_POINT('Ctrl Pts',(64.0506958275435,-4.1999999999489,-57.425688749622)) ;
#196060 = CARTESIAN_POINT('',(64.0506958275436,3.0000000000511,-57.4256887496218)) ;
#196061 = CARTESIAN_POINT('Origin',(67.0313646858498,3.00000000005112,-60.0962126400144)) ;
#196062 = CARTESIAN_POINT('',(64.0506958275436,-2.9999999999489,-57.4256887496219)) ;
#196063 = CARTESIAN_POINT('',(64.0506958275436,3.0000000000511,-57.4256887496218)) ;
#196064 = CARTESIAN_POINT('Origin',(67.0313646858495,-2.99999999994887,-60.0962126400146)) ;
#196065 = CARTESIAN_POINT('Origin',(65.5410302566959,3.00000000005111,-58.7609506948182)) ;
#196066 = CARTESIAN_POINT('',(67.0313646858483,3.00000000005112,-60.0962126400146)) ;
#196067 = CARTESIAN_POINT('',(64.0506958275436,3.0000000000511,-57.4256887496218)) ;
#196068 = CARTESIAN_POINT('',(67.0313646858483,-2.99999999994888,-60.0962126400146)) ;
#196069 = CARTESIAN_POINT('',(67.0313646858483,3.00000000005112,-60.0962126400146)) ;
#196070 = CARTESIAN_POINT('',(64.0506958275436,-2.9999999999489,-57.4256887496219)) ;
#196071 = CARTESIAN_POINT('Origin',(67.2599922364783,3.00000000005112,-59.8390616879149)) ;
#196072 = CARTESIAN_POINT('',(67.4886197871085,3.00000000005112,-59.5819107358151)) ;
#196073 = CARTESIAN_POINT('',(67.0313646858483,3.00000000005112,-60.0962126400146)) ;
#196074 = CARTESIAN_POINT('',(67.4886197871085,-2.99999999994888,-59.5819107358151)) ;
#196075 = CARTESIAN_POINT('',(67.4886197871085,3.00000000005112,-59.5819107358151)) ;
#196076 = CARTESIAN_POINT('',(67.0313646858483,-2.99999999994888,-60.0962126400146)) ;
#196077 = CARTESIAN_POINT('Ctrl Pts',(67.4886197871084,3.00000000005112,-59.5819107358151)) ;
#196078 = CARTESIAN_POINT('Ctrl Pts',(67.4886197871084,-4.19999999994888,
-59.5819107358152)) ;
#196079 = CARTESIAN_POINT('Ctrl Pts',(67.487590463906,3.00000000005112,-59.5810897882029)) ;
#196080 = CARTESIAN_POINT('Ctrl Pts',(67.487590463906,-4.19999999994888,-59.581089788203)) ;
#196081 = CARTESIAN_POINT('Ctrl Pts',(67.4865623235722,3.00000000005112,-59.5802673613943)) ;
#196082 = CARTESIAN_POINT('Ctrl Pts',(67.4865623235722,-4.19999999994888,
-59.5802673613944)) ;
#196083 = CARTESIAN_POINT('Ctrl Pts',(64.4334201024814,3.00000000005109,-57.1380073602873)) ;
#196084 = CARTESIAN_POINT('Ctrl Pts',(64.4334201024814,-4.19999999994891,
-57.1380073602874)) ;
#196085 = CARTESIAN_POINT('Ctrl Pts',(69.6982985849691,3.00000000005102,-50.4162009711221)) ;
#196086 = CARTESIAN_POINT('Ctrl Pts',(69.6982985849691,-4.19999999994898,
-50.4162009711222)) ;
#196087 = CARTESIAN_POINT('',(69.6982985849692,3.00000000005102,-50.4162009711221)) ;
#196088 = CARTESIAN_POINT('Origin',(72.9417847857807,3.00000000005105,-52.7605307169523)) ;
#196089 = CARTESIAN_POINT('',(69.6982985849692,-2.99999999994898,-50.4162009711222)) ;
#196090 = CARTESIAN_POINT('',(69.6982985849692,3.00000000005102,-50.4162009711221)) ;
#196091 = CARTESIAN_POINT('Origin',(72.9417847857812,-2.99999999994895,-52.7605307169521)) ;
#196092 = CARTESIAN_POINT('Origin',(71.3200416853732,3.00000000005104,-51.5883658440379)) ;
#196093 = CARTESIAN_POINT('',(72.9417847857773,3.00000000005105,-52.7605307169534)) ;
#196094 = CARTESIAN_POINT('',(69.6982985849692,3.00000000005102,-50.4162009711221)) ;
#196095 = CARTESIAN_POINT('',(72.9417847857773,-2.99999999994895,-52.7605307169535)) ;
#196096 = CARTESIAN_POINT('',(72.9417847857773,3.00000000005105,-52.7605307169534)) ;
#196097 = CARTESIAN_POINT('',(69.6982985849692,-2.99999999994898,-50.4162009711222)) ;
#196098 = CARTESIAN_POINT('Origin',(73.1422802969124,3.00000000005105,-52.4808903781475)) ;
#196099 = CARTESIAN_POINT('',(73.3427758080477,3.00000000005104,-52.2012500393414)) ;
#196100 = CARTESIAN_POINT('',(72.9417847857773,3.00000000005105,-52.7605307169534)) ;
#196101 = CARTESIAN_POINT('',(73.3427758080477,-2.99999999994896,-52.2012500393415)) ;
#196102 = CARTESIAN_POINT('',(73.3427758080477,3.00000000005104,-52.2012500393414)) ;
#196103 = CARTESIAN_POINT('',(72.9417847857773,-2.99999999994895,-52.7605307169535)) ;
#196104 = CARTESIAN_POINT('Ctrl Pts',(73.3427758080477,3.00000000005104,-52.2012500393414)) ;
#196105 = CARTESIAN_POINT('Ctrl Pts',(73.3427758080477,-4.19999999994896,
-52.2012500393415)) ;
#196106 = CARTESIAN_POINT('Ctrl Pts',(73.3416663111929,3.00000000005104,-52.2005411825387)) ;
#196107 = CARTESIAN_POINT('Ctrl Pts',(73.3416663111929,-4.19999999994896,
-52.2005411825388)) ;
#196108 = CARTESIAN_POINT('Ctrl Pts',(73.3405578361089,3.00000000005104,-52.1998307309995)) ;
#196109 = CARTESIAN_POINT('Ctrl Pts',(73.3405578361089,-4.19999999994896,
-52.1998307309995)) ;
#196110 = CARTESIAN_POINT('Ctrl Pts',(70.0488553627452,3.00000000005102,-50.0900899502248)) ;
#196111 = CARTESIAN_POINT('Ctrl Pts',(70.0488553627452,-4.19999999994898,
-50.0900899502248)) ;
#196112 = CARTESIAN_POINT('Ctrl Pts',(74.5822721977904,3.00000000005095,-42.8547766627078)) ;
#196113 = CARTESIAN_POINT('Ctrl Pts',(74.5822721977904,-4.19999999994905,
-42.8547766627079)) ;
#196114 = CARTESIAN_POINT('',(74.5822721977904,3.00000000005095,-42.8547766627078)) ;
#196115 = CARTESIAN_POINT('Origin',(78.0530394275431,3.00000000005097,-44.8472272966999)) ;
#196116 = CARTESIAN_POINT('',(74.5822721977904,-2.99999999994905,-42.8547766627079)) ;
#196117 = CARTESIAN_POINT('',(74.5822721977904,3.00000000005095,-42.8547766627078)) ;
#196118 = CARTESIAN_POINT('Origin',(78.053039427543,-2.99999999994903,-44.8472272967)) ;
#196119 = CARTESIAN_POINT('Origin',(76.3176558126671,3.00000000005096,-43.851001979704)) ;
#196120 = CARTESIAN_POINT('',(78.0530394275438,3.00000000005097,-44.8472272967001)) ;
#196121 = CARTESIAN_POINT('',(74.5822721977904,3.00000000005095,-42.8547766627078)) ;
#196122 = CARTESIAN_POINT('',(78.0530394275438,-2.99999999994903,-44.8472272967002)) ;
#196123 = CARTESIAN_POINT('',(78.0530394275438,3.00000000005097,-44.8472272967001)) ;
#196124 = CARTESIAN_POINT('',(74.5822721977904,-2.99999999994905,-42.8547766627079)) ;
#196125 = CARTESIAN_POINT('Origin',(78.2232062284078,3.00000000005097,-44.5481613692583)) ;
#196126 = CARTESIAN_POINT('',(78.3933730292717,3.00000000005096,-44.2490954418165)) ;
#196127 = CARTESIAN_POINT('',(78.0530394275438,3.00000000005097,-44.8472272967001)) ;
#196128 = CARTESIAN_POINT('',(78.3933730292717,-2.99999999994904,-44.2490954418166)) ;
#196129 = CARTESIAN_POINT('',(78.3933730292717,3.00000000005096,-44.2490954418165)) ;
#196130 = CARTESIAN_POINT('',(78.0530394275438,-2.99999999994903,-44.8472272967002)) ;
#196131 = CARTESIAN_POINT('Ctrl Pts',(78.3933730292716,3.00000000005096,-44.2490954418165)) ;
#196132 = CARTESIAN_POINT('Ctrl Pts',(78.3933730292716,-4.19999999994904,
-44.2490954418165)) ;
#196133 = CARTESIAN_POINT('Ctrl Pts',(78.392195514644,3.00000000005096,-44.2485064422069)) ;
#196134 = CARTESIAN_POINT('Ctrl Pts',(78.392195514644,-4.19999999994904,-44.248506442207)) ;
#196135 = CARTESIAN_POINT('Ctrl Pts',(78.391018849496,3.00000000005096,-44.2479157497924)) ;
#196136 = CARTESIAN_POINT('Ctrl Pts',(78.391018849496,-4.19999999994904,-44.2479157497925)) ;
#196137 = CARTESIAN_POINT('Ctrl Pts',(74.8968207049897,3.00000000005094,-42.4938089508354)) ;
#196138 = CARTESIAN_POINT('Ctrl Pts',(74.8968207049897,-4.19999999994906,
-42.4938089508355)) ;
#196139 = CARTESIAN_POINT('Ctrl Pts',(78.6491068290694,3.00000000005087,-34.8242603714322)) ;
#196140 = CARTESIAN_POINT('Ctrl Pts',(78.6491068290694,-4.19999999994914,
-34.8242603714323)) ;
#196141 = CARTESIAN_POINT('',(78.6491068290693,3.00000000005087,-34.8242603714323)) ;
#196142 = CARTESIAN_POINT('Origin',(82.3091286356952,3.00000000005088,-36.4430021874914)) ;
#196143 = CARTESIAN_POINT('',(78.6491068290693,-2.99999999994913,-34.8242603714324)) ;
#196144 = CARTESIAN_POINT('',(78.6491068290693,3.00000000005087,-34.8242603714323)) ;
#196145 = CARTESIAN_POINT('Origin',(82.3091286356951,-2.99999999994912,-36.4430021874917)) ;
#196146 = CARTESIAN_POINT('Origin',(80.4791177323813,3.00000000005087,-35.6336312794621)) ;
#196147 = CARTESIAN_POINT('',(82.3091286356934,3.00000000005088,-36.4430021874921)) ;
#196148 = CARTESIAN_POINT('',(78.6491068290693,3.00000000005087,-34.8242603714323)) ;
#196149 = CARTESIAN_POINT('',(82.3091286356934,-2.99999999994912,-36.4430021874922)) ;
#196150 = CARTESIAN_POINT('',(82.3091286356934,3.00000000005088,-36.4430021874921)) ;
#196151 = CARTESIAN_POINT('',(78.6491068290693,-2.99999999994913,-34.8242603714324)) ;
#196152 = CARTESIAN_POINT('Origin',(82.4471023432062,3.00000000005088,-36.1277873002989)) ;
#196153 = CARTESIAN_POINT('',(82.5850760507188,3.00000000005088,-35.812572413106)) ;
#196154 = CARTESIAN_POINT('',(82.3091286356934,3.00000000005088,-36.4430021874921)) ;
#196155 = CARTESIAN_POINT('',(82.5850760507188,-2.99999999994912,-35.8125724131061)) ;
#196156 = CARTESIAN_POINT('',(82.5850760507188,3.00000000005088,-35.812572413106)) ;
#196157 = CARTESIAN_POINT('',(82.3091286356934,-2.99999999994912,-36.4430021874921)) ;
#196158 = CARTESIAN_POINT('Ctrl Pts',(82.5850760507189,3.00000000005088,-35.8125724131059)) ;
#196159 = CARTESIAN_POINT('Ctrl Pts',(82.5850760507189,-4.19999999994912,
-35.812572413106)) ;
#196160 = CARTESIAN_POINT('Ctrl Pts',(82.5838434194159,3.00000000005088,-35.8121097238921)) ;
#196161 = CARTESIAN_POINT('Ctrl Pts',(82.5838434194159,-4.19999999994912,
-35.8121097238922)) ;
#196162 = CARTESIAN_POINT('Ctrl Pts',(82.5826114559914,3.00000000005088,-35.8116452623523)) ;
#196163 = CARTESIAN_POINT('Ctrl Pts',(82.5826114559914,-4.19999999994912,
-35.8116452623524)) ;
#196164 = CARTESIAN_POINT('Ctrl Pts',(78.9242008064232,3.00000000005086,-34.4323908063735)) ;
#196165 = CARTESIAN_POINT('Ctrl Pts',(78.9242008064232,-4.19999999994914,
-34.4323908063736)) ;
#196166 = CARTESIAN_POINT('Ctrl Pts',(81.8542453875446,3.00000000005078,-26.4126361142756)) ;
#196167 = CARTESIAN_POINT('Ctrl Pts',(81.8542453875446,-4.19999999994922,
-26.4126361142757)) ;
#196168 = CARTESIAN_POINT('',(81.8542453875448,3.00000000005078,-26.4126361142757)) ;
#196169 = CARTESIAN_POINT('Origin',(85.6634218062183,3.00000000005079,-27.6399338383216)) ;
#196170 = CARTESIAN_POINT('',(81.8542453875448,-2.99999999994922,-26.4126361142757)) ;
#196171 = CARTESIAN_POINT('',(81.8542453875448,3.00000000005078,-26.4126361142757)) ;
#196172 = CARTESIAN_POINT('Origin',(85.6634218062184,-2.99999999994921,-27.6399338383216)) ;
#196173 = CARTESIAN_POINT('Origin',(83.7588335968811,3.00000000005079,-27.0262849762992)) ;
#196174 = CARTESIAN_POINT('',(85.6634218062177,3.00000000005079,-27.6399338383229)) ;
#196175 = CARTESIAN_POINT('',(81.8542453875448,3.00000000005078,-26.4126361142757)) ;
#196176 = CARTESIAN_POINT('',(85.6634218062177,-2.99999999994921,-27.639933838323)) ;
#196177 = CARTESIAN_POINT('',(85.6634218062177,3.00000000005079,-27.6399338383229)) ;
#196178 = CARTESIAN_POINT('',(81.8542453875448,-2.99999999994922,-26.4126361142757)) ;
#196179 = CARTESIAN_POINT('Origin',(85.7676907515669,3.00000000005079,-27.3120235516457)) ;
#196180 = CARTESIAN_POINT('',(85.8719596969164,3.00000000005079,-26.9841132649686)) ;
#196181 = CARTESIAN_POINT('',(85.6634218062177,3.00000000005079,-27.6399338383229)) ;
#196182 = CARTESIAN_POINT('',(85.8719596969164,-2.99999999994921,-26.9841132649687)) ;
#196183 = CARTESIAN_POINT('',(85.8719596969164,3.00000000005079,-26.9841132649686)) ;
#196184 = CARTESIAN_POINT('',(85.6634218062177,-2.99999999994921,-27.639933838323)) ;
#196185 = CARTESIAN_POINT('Ctrl Pts',(85.8719596969164,3.00000000005079,-26.9841132649686)) ;
#196186 = CARTESIAN_POINT('Ctrl Pts',(85.8719596969164,-4.19999999994922,
-26.9841132649687)) ;
#196187 = CARTESIAN_POINT('Ctrl Pts',(85.8706854539043,3.00000000005079,-26.9837819554707)) ;
#196188 = CARTESIAN_POINT('Ctrl Pts',(85.8706854539043,-4.19999999994922,
-26.9837819554707)) ;
#196189 = CARTESIAN_POINT('Ctrl Pts',(85.8694116898534,3.00000000005079,-26.9834488135434)) ;
#196190 = CARTESIAN_POINT('Ctrl Pts',(85.8694116898534,-4.19999999994922,
-26.9834488135435)) ;
#196191 = CARTESIAN_POINT('Ctrl Pts',(82.0868708478707,3.00000000005078,-25.9941581009892)) ;
#196192 = CARTESIAN_POINT('Ctrl Pts',(82.0868708478707,-4.19999999994923,
-25.9941581009893)) ;
#196193 = CARTESIAN_POINT('Ctrl Pts',(84.1625717044526,3.00000000005069,-17.7120634068452)) ;
#196194 = CARTESIAN_POINT('Ctrl Pts',(84.1625717044526,-4.19999999994931,
-17.7120634068453)) ;
#196195 = CARTESIAN_POINT('',(84.1625717044528,3.00000000005069,-17.7120634068453)) ;
#196196 = CARTESIAN_POINT('Origin',(88.0791686012132,3.0000000000507,-18.5344705081823)) ;
#196197 = CARTESIAN_POINT('',(84.1625717044528,-2.99999999994931,-17.7120634068454)) ;
#196198 = CARTESIAN_POINT('',(84.1625717044528,3.00000000005069,-17.7120634068453)) ;
#196199 = CARTESIAN_POINT('Origin',(88.0791686012132,-2.9999999999493,-18.5344705081823)) ;
#196200 = CARTESIAN_POINT('Origin',(86.1208701528311,3.0000000000507,-18.1232669575159)) ;
#196201 = CARTESIAN_POINT('',(88.0791686012095,3.0000000000507,-18.5344705081866)) ;
#196202 = CARTESIAN_POINT('',(84.1625717044528,3.00000000005069,-17.7120634068453)) ;
#196203 = CARTESIAN_POINT('',(88.0791686012095,-2.9999999999493,-18.5344705081866)) ;
#196204 = CARTESIAN_POINT('',(88.0791686012095,3.0000000000507,-18.5344705081866)) ;
#196205 = CARTESIAN_POINT('',(84.1625717044528,-2.99999999994931,-17.7120634068453)) ;
#196206 = CARTESIAN_POINT('Origin',(88.1485903920104,3.0000000000507,-18.1974574757458)) ;
#196207 = CARTESIAN_POINT('',(88.2180121828114,3.00000000005069,-17.8604444433051)) ;
#196208 = CARTESIAN_POINT('',(88.0791686012095,3.0000000000507,-18.5344705081866)) ;
#196209 = CARTESIAN_POINT('',(88.2180121828114,-2.99999999994931,-17.8604444433052)) ;
#196210 = CARTESIAN_POINT('',(88.2180121828114,3.00000000005069,-17.8604444433051)) ;
#196211 = CARTESIAN_POINT('',(88.0791686012095,-2.9999999999493,-18.5344705081866)) ;
#196212 = CARTESIAN_POINT('Ctrl Pts',(88.2180121828113,3.00000000005069,-17.8604444433051)) ;
#196213 = CARTESIAN_POINT('Ctrl Pts',(88.2180121828113,-4.19999999994931,
-17.8604444433051)) ;
#196214 = CARTESIAN_POINT('Ctrl Pts',(88.2167102889633,3.00000000005069,-17.8602481434188)) ;
#196215 = CARTESIAN_POINT('Ctrl Pts',(88.2167102889633,-4.19999999994931,
-17.8602481434189)) ;
#196216 = CARTESIAN_POINT('Ctrl Pts',(88.2154086799115,3.00000000005069,-17.8600499710769)) ;
#196217 = CARTESIAN_POINT('Ctrl Pts',(88.2154086799115,-4.19999999994931,
-17.860049971077)) ;
#196218 = CARTESIAN_POINT('Ctrl Pts',(84.3501799545264,3.00000000005069,-17.2715618780168)) ;
#196219 = CARTESIAN_POINT('Ctrl Pts',(84.3501799545264,-4.19999999994932,
-17.2715618780169)) ;
#196220 = CARTESIAN_POINT('Ctrl Pts',(85.5487952736163,3.0000000000506,-8.81786754443537)) ;
#196221 = CARTESIAN_POINT('Ctrl Pts',(85.5487952736163,-4.1999999999494,-8.81786754443545)) ;
#196222 = CARTESIAN_POINT('',(85.5487952736163,3.0000000000506,-8.81786754443542)) ;
#196223 = CARTESIAN_POINT('Origin',(89.5299015932572,3.00000000005061,-9.22637355876851)) ;
#196224 = CARTESIAN_POINT('',(85.5487952736163,-2.9999999999494,-8.81786754443548)) ;
#196225 = CARTESIAN_POINT('',(85.5487952736163,3.0000000000506,-8.81786754443542)) ;
#196226 = CARTESIAN_POINT('Origin',(89.5299015932573,-2.99999999994939,-9.2263735587685)) ;
#196227 = CARTESIAN_POINT('Origin',(87.5393484334361,3.0000000000506,-9.02212055160212)) ;
#196228 = CARTESIAN_POINT('',(89.5299015932564,3.0000000000506,-9.22637355876897)) ;
#196229 = CARTESIAN_POINT('',(85.5487952736163,3.0000000000506,-8.81786754443542)) ;
#196230 = CARTESIAN_POINT('',(89.5299015932564,-2.9999999999494,-9.22637355876903)) ;
#196231 = CARTESIAN_POINT('',(89.5299015932564,3.0000000000506,-9.22637355876897)) ;
#196232 = CARTESIAN_POINT('',(85.5487952736163,-2.9999999999494,-8.81786754443549)) ;
#196233 = CARTESIAN_POINT('Origin',(89.5637156298411,3.0000000000506,-8.88395016587238)) ;
#196234 = CARTESIAN_POINT('',(89.5975296664262,3.0000000000506,-8.54152677297597)) ;
#196235 = CARTESIAN_POINT('',(89.5299015932564,3.0000000000506,-9.22637355876897)) ;
#196236 = CARTESIAN_POINT('',(89.5975296664262,-2.9999999999494,-8.54152677297603)) ;
#196237 = CARTESIAN_POINT('',(89.5975296664262,3.0000000000506,-8.54152677297597)) ;
#196238 = CARTESIAN_POINT('',(89.5299015932564,-2.9999999999494,-9.22637355876903)) ;
#196239 = CARTESIAN_POINT('Ctrl Pts',(89.597529666426,3.0000000000506,-8.54152677297593)) ;
#196240 = CARTESIAN_POINT('Ctrl Pts',(89.597529666426,-4.1999999999494,-8.541526772976)) ;
#196241 = CARTESIAN_POINT('Ctrl Pts',(89.5962143855631,3.0000000000506,-8.54146763340456)) ;
#196242 = CARTESIAN_POINT('Ctrl Pts',(89.5962143855631,-4.1999999999494,-8.54146763340463)) ;
#196243 = CARTESIAN_POINT('Ctrl Pts',(89.5948991922115,3.0000000000506,-8.54140660186496)) ;
#196244 = CARTESIAN_POINT('Ctrl Pts',(89.5948991922115,-4.1999999999494,-8.54140660186504)) ;
#196245 = CARTESIAN_POINT('Ctrl Pts',(85.6893308381908,3.0000000000506,-8.36016872699591)) ;
#196246 = CARTESIAN_POINT('Ctrl Pts',(85.6893308381908,-4.19999999994941,
-8.36016872699598)) ;
#196247 = CARTESIAN_POINT('Ctrl Pts',(85.9977283395256,3.00000000005051,0.172504801855261)) ;
#196248 = CARTESIAN_POINT('Ctrl Pts',(85.9977283395256,-4.19999999994949,
0.172504801855188)) ;
#196249 = CARTESIAN_POINT('',(85.9977283395256,3.00000000005051,0.172504801855252)) ;
#196250 = CARTESIAN_POINT('Origin',(89.999726248113,3.00000000005051,0.182375551912067)) ;
#196251 = CARTESIAN_POINT('',(85.9977283395256,-2.99999999994949,0.172504801855191)) ;
#196252 = CARTESIAN_POINT('',(85.9977283395256,3.00000000005051,0.172504801855252)) ;
#196253 = CARTESIAN_POINT('Origin',(89.999726248113,-2.99999999994949,0.182375551911981)) ;
#196254 = CARTESIAN_POINT('Origin',(87.9987272938181,3.00000000005051,0.177440176881581)) ;
#196255 = CARTESIAN_POINT('',(89.9997262481107,3.00000000005051,0.182375551907936)) ;
#196256 = CARTESIAN_POINT('',(85.9977283395256,3.00000000005051,0.172504801855252)) ;
#196257 = CARTESIAN_POINT('',(89.9997262481107,-2.99999999994949,0.182375551907875)) ;
#196258 = CARTESIAN_POINT('',(89.9997262481107,3.00000000005051,0.182375551907936)) ;
#196259 = CARTESIAN_POINT('',(85.9977283395256,-2.99999999994949,0.172504801855191)) ;
#196260 = CARTESIAN_POINT('Origin',(89.9975620568185,3.00000000005051,0.52645764291101)) ;
#196261 = CARTESIAN_POINT('',(89.9953978655267,3.0000000000505,0.870539733914034)) ;
#196262 = CARTESIAN_POINT('',(89.9997262481107,3.00000000005051,0.182375551907936)) ;
#196263 = CARTESIAN_POINT('',(89.9953978655267,-2.9999999999495,0.870539733913973)) ;
#196264 = CARTESIAN_POINT('',(89.9953978655267,3.0000000000505,0.870539733914034)) ;
#196265 = CARTESIAN_POINT('',(89.9997262481107,-2.99999999994949,0.182375551907875)) ;
#196266 = CARTESIAN_POINT('Ctrl Pts',(89.9953978655265,3.0000000000505,0.870539733914057)) ;
#196267 = CARTESIAN_POINT('Ctrl Pts',(89.9953978655265,-4.1999999999495,0.870539733913984)) ;
#196268 = CARTESIAN_POINT('Ctrl Pts',(89.9940836081412,3.0000000000505,0.870461065225228)) ;
#196269 = CARTESIAN_POINT('Ctrl Pts',(89.9940836081412,-4.1999999999495,0.870461065225154)) ;
#196270 = CARTESIAN_POINT('Ctrl Pts',(89.9927692400232,3.0000000000505,0.870384287287441)) ;
#196271 = CARTESIAN_POINT('Ctrl Pts',(89.9927692400232,-4.1999999999495,0.870384287287368)) ;
#196272 = CARTESIAN_POINT('Ctrl Pts',(86.0896514815462,3.0000000000505,0.642386263882138)) ;
#196273 = CARTESIAN_POINT('Ctrl Pts',(86.0896514815462,-4.1999999999495,0.642386263882064)) ;
#196274 = CARTESIAN_POINT('Ctrl Pts',(85.5044522975655,3.00000000005042,9.16055323124422)) ;
#196275 = CARTESIAN_POINT('Ctrl Pts',(85.5044522975655,-4.19999999994958,
9.16055323124414)) ;
#196276 = CARTESIAN_POINT('',(85.5044522975654,3.00000000005042,9.16055323124416)) ;
#196277 = CARTESIAN_POINT('Origin',(89.4834950685362,3.00000000005041,9.58869259967878)) ;
#196278 = CARTESIAN_POINT('',(85.5044522975654,-2.99999999994958,9.1605532312441)) ;
#196279 = CARTESIAN_POINT('',(85.5044522975654,3.00000000005042,9.16055323124416)) ;
#196280 = CARTESIAN_POINT('Origin',(89.4834950685362,-2.99999999994959,9.58869259967875)) ;
#196281 = CARTESIAN_POINT('Origin',(87.4939736830512,3.00000000005042,9.37462291546208)) ;
#196282 = CARTESIAN_POINT('',(89.4834950685366,3.00000000005041,9.58869259968009)) ;
#196283 = CARTESIAN_POINT('',(85.5044522975654,3.00000000005042,9.16055323124416)) ;
#196284 = CARTESIAN_POINT('',(89.4834950685366,-2.99999999994959,9.58869259968003)) ;
#196285 = CARTESIAN_POINT('',(89.4834950685366,3.00000000005041,9.58869259968009)) ;
#196286 = CARTESIAN_POINT('',(85.5044522975654,-2.99999999994958,9.1605532312441)) ;
#196287 = CARTESIAN_POINT('Origin',(89.4453763607007,3.00000000005041,9.93066355339673)) ;
#196288 = CARTESIAN_POINT('',(89.4072576528648,3.00000000005041,10.2726345071134)) ;
#196289 = CARTESIAN_POINT('',(89.4834950685366,3.00000000005041,9.58869259968009)) ;
#196290 = CARTESIAN_POINT('',(89.4072576528648,-2.99999999994959,10.2726345071134)) ;
#196291 = CARTESIAN_POINT('',(89.4072576528648,3.00000000005041,10.2726345071134)) ;
#196292 = CARTESIAN_POINT('',(89.4834950685366,-2.99999999994959,9.58869259968003)) ;
#196293 = CARTESIAN_POINT('Ctrl Pts',(89.4072576528647,3.00000000005041,10.2726345071135)) ;
#196294 = CARTESIAN_POINT('Ctrl Pts',(89.4072576528647,-4.19999999994959,
10.2726345071134)) ;
#196295 = CARTESIAN_POINT('Ctrl Pts',(89.4059588182358,3.00000000005041,10.2724188920751)) ;
#196296 = CARTESIAN_POINT('Ctrl Pts',(89.4059588182358,-4.19999999994959,
10.2724188920751)) ;
#196297 = CARTESIAN_POINT('Ctrl Pts',(89.404659675844,3.00000000005041,10.2722051458554)) ;
#196298 = CARTESIAN_POINT('Ctrl Pts',(89.404659675844,-4.19999999994959,10.2722051458553)) ;
#196299 = CARTESIAN_POINT('Ctrl Pts',(85.5467558878525,3.00000000005041,9.63746921823198)) ;
#196300 = CARTESIAN_POINT('Ctrl Pts',(85.5467558878525,-4.19999999994959,
9.63746921823191)) ;
#196301 = CARTESIAN_POINT('Ctrl Pts',(84.0743715832764,3.00000000005033,18.0478028042689)) ;
#196302 = CARTESIAN_POINT('Ctrl Pts',(84.0743715832764,-4.19999999994967,
18.0478028042688)) ;
#196303 = CARTESIAN_POINT('',(84.0743715832764,3.00000000005033,18.0478028042688)) ;
#196304 = CARTESIAN_POINT('Origin',(87.986863991367,3.00000000005032,18.8895200065722)) ;
#196305 = CARTESIAN_POINT('',(84.0743715832764,-2.99999999994967,18.0478028042687)) ;
#196306 = CARTESIAN_POINT('',(84.0743715832764,3.00000000005033,18.0478028042688)) ;
#196307 = CARTESIAN_POINT('Origin',(87.986863991367,-2.99999999994968,18.8895200065722)) ;
#196308 = CARTESIAN_POINT('Origin',(86.0306177873216,3.00000000005032,18.4686614054212)) ;
#196309 = CARTESIAN_POINT('',(87.9868639913669,3.00000000005032,18.8895200065734)) ;
#196310 = CARTESIAN_POINT('',(84.0743715832764,3.00000000005033,18.0478028042688)) ;
#196311 = CARTESIAN_POINT('',(87.9868639913669,-2.99999999994968,18.8895200065733)) ;
#196312 = CARTESIAN_POINT('',(87.9868639913669,3.00000000005032,18.8895200065734)) ;
#196313 = CARTESIAN_POINT('',(84.0743715832764,-2.99999999994967,18.0478028042687)) ;
#196314 = CARTESIAN_POINT('Origin',(87.9132084035267,3.00000000005032,19.2256331176729)) ;
#196315 = CARTESIAN_POINT('',(87.8395528156865,3.00000000005031,19.5617462287721)) ;
#196316 = CARTESIAN_POINT('',(87.9868639913669,3.00000000005032,18.8895200065734)) ;
#196317 = CARTESIAN_POINT('',(87.8395528156865,-2.99999999994969,19.5617462287721)) ;
#196318 = CARTESIAN_POINT('',(87.8395528156865,3.00000000005031,19.5617462287721)) ;
#196319 = CARTESIAN_POINT('',(87.9868639913669,-2.99999999994968,18.8895200065733)) ;
#196320 = CARTESIAN_POINT('Ctrl Pts',(87.8395528156866,3.00000000005031,19.5617462287722)) ;
#196321 = CARTESIAN_POINT('Ctrl Pts',(87.8395528156866,-4.19999999994969,
19.5617462287721)) ;
#196322 = CARTESIAN_POINT('Ctrl Pts',(87.8382836341184,3.00000000005031,19.5613960297078)) ;
#196323 = CARTESIAN_POINT('Ctrl Pts',(87.8382836341184,-4.19999999994969,
19.5613960297077)) ;
#196324 = CARTESIAN_POINT('Ctrl Pts',(87.8370139511282,3.00000000005031,19.5610476570545)) ;
#196325 = CARTESIAN_POINT('Ctrl Pts',(87.8370139511282,-4.19999999994969,
19.5610476570545)) ;
#196326 = CARTESIAN_POINT('Ctrl Pts',(84.0665921348418,3.00000000005032,18.526528124863)) ;
#196327 = CARTESIAN_POINT('Ctrl Pts',(84.0665921348418,-4.19999999994968,
18.5265281248629)) ;
#196328 = CARTESIAN_POINT('Ctrl Pts',(81.7231544602271,3.00000000005024,26.7368829548309)) ;
#196329 = CARTESIAN_POINT('Ctrl Pts',(81.7231544602271,-4.19999999994976,
26.7368829548308)) ;
#196330 = CARTESIAN_POINT('',(81.723154460227,3.00000000005024,26.7368829548309)) ;
#196331 = CARTESIAN_POINT('Origin',(85.5262304198725,3.00000000005022,27.9829559611932)) ;
#196332 = CARTESIAN_POINT('',(81.723154460227,-2.99999999994976,26.7368829548309)) ;
#196333 = CARTESIAN_POINT('',(81.723154460227,3.00000000005024,26.7368829548309)) ;
#196334 = CARTESIAN_POINT('Origin',(85.5262304198726,-2.99999999994977,27.9829559611934)) ;
#196335 = CARTESIAN_POINT('Origin',(83.6246924400499,3.00000000005023,27.359919458013)) ;
#196336 = CARTESIAN_POINT('',(85.5262304198725,3.00000000005023,27.9829559611952)) ;
#196337 = CARTESIAN_POINT('',(81.723154460227,3.00000000005024,26.7368829548309)) ;
#196338 = CARTESIAN_POINT('',(85.5262304198725,-2.99999999994977,27.9829559611951)) ;
#196339 = CARTESIAN_POINT('',(85.5262304198725,3.00000000005023,27.9829559611952)) ;
#196340 = CARTESIAN_POINT('',(81.723154460227,-2.99999999994976,26.7368829548309)) ;
#196341 = CARTESIAN_POINT('Origin',(85.4178449380619,3.00000000005022,28.3095287040958)) ;
#196342 = CARTESIAN_POINT('',(85.3094594562511,3.00000000005022,28.6361014469966)) ;
#196343 = CARTESIAN_POINT('',(85.5262304198725,3.00000000005023,27.9829559611952)) ;
#196344 = CARTESIAN_POINT('',(85.3094594562511,-2.99999999994978,28.6361014469965)) ;
#196345 = CARTESIAN_POINT('',(85.3094594562511,3.00000000005022,28.6361014469966)) ;
#196346 = CARTESIAN_POINT('',(85.5262304198725,-2.99999999994977,27.9829559611951)) ;
#196347 = CARTESIAN_POINT('Ctrl Pts',(85.3094594562513,3.00000000005022,28.6361014469965)) ;
#196348 = CARTESIAN_POINT('Ctrl Pts',(85.3094594562513,-4.19999999994978,
28.6361014469964)) ;
#196349 = CARTESIAN_POINT('Ctrl Pts',(85.3082338331627,3.00000000005022,28.6356205007604)) ;
#196350 = CARTESIAN_POINT('Ctrl Pts',(85.3082338331627,-4.19999999994978,
28.6356205007604)) ;
#196351 = CARTESIAN_POINT('Ctrl Pts',(85.3070075204873,3.00000000005022,28.635141318517)) ;
#196352 = CARTESIAN_POINT('Ctrl Pts',(85.3070075204873,-4.19999999994978,
28.635141318517)) ;
#196353 = CARTESIAN_POINT('Ctrl Pts',(81.6653772063361,3.00000000005024,27.212172594239)) ;
#196354 = CARTESIAN_POINT('Ctrl Pts',(81.6653772063361,-4.19999999994977,
27.212172594239)) ;
#196355 = CARTESIAN_POINT('Ctrl Pts',(78.4765613552424,3.00000000005015,35.1325943024941)) ;
#196356 = CARTESIAN_POINT('Ctrl Pts',(78.4765613552424,-4.19999999994985,
35.132594302494)) ;
#196357 = CARTESIAN_POINT('',(78.4765613552424,3.00000000005015,35.1325943024941)) ;
#196358 = CARTESIAN_POINT('Origin',(82.1285535703842,3.00000000005014,36.7693708763001)) ;
#196359 = CARTESIAN_POINT('',(78.4765613552424,-2.99999999994985,35.132594302494)) ;
#196360 = CARTESIAN_POINT('',(78.4765613552424,3.00000000005015,35.1325943024941)) ;
#196361 = CARTESIAN_POINT('Origin',(82.1285535703842,-2.99999999994986,36.7693708763003)) ;
#196362 = CARTESIAN_POINT('Origin',(80.3025574628131,3.00000000005015,35.9509825893984)) ;
#196363 = CARTESIAN_POINT('',(82.1285535703842,3.00000000005014,36.7693708763029)) ;
#196364 = CARTESIAN_POINT('',(78.4765613552424,3.00000000005015,35.1325943024941)) ;
#196365 = CARTESIAN_POINT('',(82.1285535703842,-2.99999999994986,36.7693708763028)) ;
#196366 = CARTESIAN_POINT('',(82.1285535703842,3.00000000005014,36.7693708763029)) ;
#196367 = CARTESIAN_POINT('',(78.4765613552424,-2.99999999994985,35.132594302494)) ;
#196368 = CARTESIAN_POINT('Origin',(81.9866256886228,3.00000000005013,37.0828252516937)) ;
#196369 = CARTESIAN_POINT('',(81.8446978068619,3.00000000005013,37.3962796270845)) ;
#196370 = CARTESIAN_POINT('',(82.1285535703842,3.00000000005014,36.7693708763029)) ;
#196371 = CARTESIAN_POINT('',(81.8446978068619,-2.99999999994987,37.3962796270845)) ;
#196372 = CARTESIAN_POINT('',(81.8446978068619,3.00000000005013,37.3962796270845)) ;
#196373 = CARTESIAN_POINT('',(82.1285535703842,-2.99999999994986,36.7693708763028)) ;
#196374 = CARTESIAN_POINT('Ctrl Pts',(81.8446978068617,3.00000000005013,37.3962796270845)) ;
#196375 = CARTESIAN_POINT('Ctrl Pts',(81.8446978068617,-4.19999999994988,
37.3962796270845)) ;
#196376 = CARTESIAN_POINT('Ctrl Pts',(81.8435291704356,3.00000000005013,37.3956732030243)) ;
#196377 = CARTESIAN_POINT('Ctrl Pts',(81.8435291704356,-4.19999999994988,
37.3956732030242)) ;
#196378 = CARTESIAN_POINT('Ctrl Pts',(81.8423596638126,3.00000000005013,37.3950684612118)) ;
#196379 = CARTESIAN_POINT('Ctrl Pts',(81.8423596638126,-4.19999999994988,
37.3950684612117)) ;
#196380 = CARTESIAN_POINT('Ctrl Pts',(78.3694193155791,3.00000000005015,35.5992408879661)) ;
#196381 = CARTESIAN_POINT('Ctrl Pts',(78.3694193155791,-4.19999999994986,
35.599240887966)) ;
#196382 = CARTESIAN_POINT('Ctrl Pts',(74.3701626217736,3.00000000005007,43.1429516768174)) ;
#196383 = CARTESIAN_POINT('Ctrl Pts',(74.3701626217736,-4.19999999994994,
43.1429516768174)) ;
#196384 = CARTESIAN_POINT('',(74.3701626217736,3.00000000005007,43.1429516768173)) ;
#196385 = CARTESIAN_POINT('Origin',(77.8310591014742,3.00000000005005,45.1524989514095)) ;
#196386 = CARTESIAN_POINT('',(74.3701626217736,-2.99999999994993,43.1429516768173)) ;
#196387 = CARTESIAN_POINT('',(74.3701626217736,3.00000000005007,43.1429516768173)) ;
#196388 = CARTESIAN_POINT('Origin',(77.8310591014742,-2.99999999994995,45.152498951409)) ;
#196389 = CARTESIAN_POINT('Origin',(76.1006108616236,3.00000000005006,44.1477253141138)) ;
#196390 = CARTESIAN_POINT('',(77.8310591014736,3.00000000005005,45.1524989514102)) ;
#196391 = CARTESIAN_POINT('',(74.3701626217736,3.00000000005007,43.1429516768173)) ;
#196392 = CARTESIAN_POINT('',(77.8310591014736,-2.99999999994995,45.1524989514101)) ;
#196393 = CARTESIAN_POINT('',(77.8310591014736,3.00000000005005,45.1524989514102)) ;
#196394 = CARTESIAN_POINT('',(74.3701626217736,-2.99999999994993,43.1429516768173)) ;
#196395 = CARTESIAN_POINT('Origin',(77.6571438113347,3.00000000005005,45.4494006875601)) ;
#196396 = CARTESIAN_POINT('',(77.4832285211958,3.00000000005005,45.74630242371)) ;
#196397 = CARTESIAN_POINT('',(77.8310591014736,3.00000000005005,45.1524989514102)) ;
#196398 = CARTESIAN_POINT('',(77.4832285211958,-2.99999999994995,45.7463024237099)) ;
#196399 = CARTESIAN_POINT('',(77.4832285211958,3.00000000005004,45.7463024237099)) ;
#196400 = CARTESIAN_POINT('',(77.8310591014736,-2.99999999994995,45.1524989514101)) ;
#196401 = CARTESIAN_POINT('Ctrl Pts',(77.4832285211958,3.00000000005004,45.7463024237099)) ;
#196402 = CARTESIAN_POINT('Ctrl Pts',(77.4832285211958,-4.19999999994996,
45.7463024237099)) ;
#196403 = CARTESIAN_POINT('Ctrl Pts',(77.4821296752576,3.00000000005005,45.7455771659345)) ;
#196404 = CARTESIAN_POINT('Ctrl Pts',(77.4821296752576,-4.19999999994995,
45.7455771659344)) ;
#196405 = CARTESIAN_POINT('Ctrl Pts',(77.4810297880463,3.00000000005005,45.7448534902309)) ;
#196406 = CARTESIAN_POINT('Ctrl Pts',(77.4810297880463,-4.19999999994995,
45.7448534902308)) ;
#196407 = CARTESIAN_POINT('Ctrl Pts',(74.2148296669458,3.00000000005007,43.5958425307108)) ;
#196408 = CARTESIAN_POINT('Ctrl Pts',(74.2148296669458,-4.19999999994993,
43.5958425307107)) ;
#196409 = CARTESIAN_POINT('Ctrl Pts',(69.4489488236634,3.00000000005,50.6801919261331)) ;
#196410 = CARTESIAN_POINT('Ctrl Pts',(69.4489488236634,-4.19999999995,50.680191926133)) ;
#196411 = CARTESIAN_POINT('',(69.4489488236634,3.00000000005,50.6801919261331)) ;
#196412 = CARTESIAN_POINT('Origin',(72.680831261851,3.00000000004997,53.0404928810471)) ;
#196413 = CARTESIAN_POINT('',(69.4489488236634,-2.99999999995,50.680191926133)) ;
#196414 = CARTESIAN_POINT('',(69.4489488236634,3.00000000005,50.6801919261331)) ;
#196415 = CARTESIAN_POINT('Origin',(72.6808312618511,-2.99999999995003,53.0404928810464)) ;
#196416 = CARTESIAN_POINT('Origin',(71.0648900427574,3.00000000004998,51.8603424035888)) ;
#196417 = CARTESIAN_POINT('',(72.6808312618513,3.00000000004997,53.0404928810446)) ;
#196418 = CARTESIAN_POINT('',(69.4489488236634,3.00000000005,50.6801919261331)) ;
#196419 = CARTESIAN_POINT('',(72.6808312618513,-2.99999999995003,53.0404928810445)) ;
#196420 = CARTESIAN_POINT('',(72.6808312618513,3.00000000004997,53.0404928810446)) ;
#196421 = CARTESIAN_POINT('',(69.4489488236634,-2.99999999995,50.680191926133)) ;
#196422 = CARTESIAN_POINT('Origin',(72.4768340156477,3.00000000004997,53.3175890604016)) ;
#196423 = CARTESIAN_POINT('',(72.2728367694436,3.00000000004997,53.5946852397585)) ;
#196424 = CARTESIAN_POINT('',(72.6808312618513,3.00000000004997,53.0404928810446)) ;
#196425 = CARTESIAN_POINT('',(72.2728367694436,-2.99999999995003,53.5946852397584)) ;
#196426 = CARTESIAN_POINT('',(72.2728367694436,3.00000000004997,53.5946852397585)) ;
#196427 = CARTESIAN_POINT('',(72.6808312618513,-2.99999999995003,53.0404928810445)) ;
#196428 = CARTESIAN_POINT('Ctrl Pts',(72.2728367694439,3.00000000004997,53.5946852397585)) ;
#196429 = CARTESIAN_POINT('Ctrl Pts',(72.2728367694439,-4.19999999995003,
53.5946852397584)) ;
#196430 = CARTESIAN_POINT('Ctrl Pts',(72.2718197531794,3.00000000004997,53.5938490943438)) ;
#196431 = CARTESIAN_POINT('Ctrl Pts',(72.2718197531794,-4.19999999995003,
53.5938490943437)) ;
#196432 = CARTESIAN_POINT('Ctrl Pts',(72.2708015359745,3.00000000004997,53.5930144134914)) ;
#196433 = CARTESIAN_POINT('Ctrl Pts',(72.2708015359745,-4.19999999995003,
53.5930144134913)) ;
#196434 = CARTESIAN_POINT('Ctrl Pts',(69.2471268140295,3.00000000004999,51.1143650814791)) ;
#196435 = CARTESIAN_POINT('Ctrl Pts',(69.2471268140295,-4.19999999995001,
51.114365081479)) ;
#196436 = CARTESIAN_POINT('Ctrl Pts',(63.7668378091141,3.00000000004992,57.6617354690004)) ;
#196437 = CARTESIAN_POINT('Ctrl Pts',(63.7668378091141,-4.19999999995008,
57.6617354690003)) ;
#196438 = CARTESIAN_POINT('',(63.7668378091141,3.00000000004992,57.6617354690004)) ;
#196439 = CARTESIAN_POINT('Origin',(66.7342970254818,3.0000000000499,60.3469301530462)) ;
#196440 = CARTESIAN_POINT('',(63.7668378091141,-2.99999999995008,57.6617354690003)) ;
#196441 = CARTESIAN_POINT('',(63.7668378091141,3.00000000004992,57.6617354690003)) ;
#196442 = CARTESIAN_POINT('Origin',(66.7342970254818,-2.9999999999501,60.3469301530459)) ;
#196443 = CARTESIAN_POINT('Origin',(65.2505674172981,3.00000000004991,59.0043328110222)) ;
#196444 = CARTESIAN_POINT('',(66.7342970254824,3.0000000000499,60.3469301530442)) ;
#196445 = CARTESIAN_POINT('',(63.7668378091141,3.00000000004992,57.6617354690003)) ;
#196446 = CARTESIAN_POINT('',(66.7342970254824,-2.9999999999501,60.3469301530441)) ;
#196447 = CARTESIAN_POINT('',(66.7342970254824,3.0000000000499,60.3469301530442)) ;
#196448 = CARTESIAN_POINT('',(63.7668378091141,-2.99999999995008,57.6617354690003)) ;
#196449 = CARTESIAN_POINT('Origin',(66.5024528597322,3.00000000004989,60.6011848518809)) ;
#196450 = CARTESIAN_POINT('',(66.2706086939821,3.00000000004989,60.8554395507177)) ;
#196451 = CARTESIAN_POINT('',(66.7342970254824,3.0000000000499,60.3469301530442)) ;
#196452 = CARTESIAN_POINT('',(66.2706086939821,-2.99999999995011,60.8554395507176)) ;
#196453 = CARTESIAN_POINT('',(66.2706086939821,3.00000000004989,60.8554395507176)) ;
#196454 = CARTESIAN_POINT('',(66.7342970254824,-2.9999999999501,60.3469301530441)) ;
#196455 = CARTESIAN_POINT('Ctrl Pts',(66.2706086939821,3.00000000004989,60.8554395507177)) ;
#196456 = CARTESIAN_POINT('Ctrl Pts',(66.2706086939821,-4.19999999995012,
60.8554395507177)) ;
#196457 = CARTESIAN_POINT('Ctrl Pts',(66.2696846500344,3.00000000004989,60.8545016786479)) ;
#196458 = CARTESIAN_POINT('Ctrl Pts',(66.2696846500344,-4.19999999995012,
60.8545016786478)) ;
#196459 = CARTESIAN_POINT('Ctrl Pts',(66.2687592586371,3.00000000004989,60.853565137585)) ;
#196460 = CARTESIAN_POINT('Ctrl Pts',(66.2687592586371,-4.19999999995012,
60.8535651375849)) ;
#196461 = CARTESIAN_POINT('Ctrl Pts',(63.5207379488458,3.00000000004992,58.0724340338524)) ;
#196462 = CARTESIAN_POINT('Ctrl Pts',(63.5207379488458,-4.19999999995009,
58.0724340338523)) ;
#196463 = CARTESIAN_POINT('Ctrl Pts',(57.3860839754601,3.00000000004986,64.0110910533819)) ;
#196464 = CARTESIAN_POINT('Ctrl Pts',(57.3860839754601,-4.19999999995015,
64.0110910533819)) ;
#196465 = CARTESIAN_POINT('',(57.3860839754601,3.00000000004986,64.0110910533819)) ;
#196466 = CARTESIAN_POINT('Origin',(60.0566078658524,3.00000000004983,66.9917599116882)) ;
#196467 = CARTESIAN_POINT('',(57.3860839754601,-2.99999999995014,64.0110910533818)) ;
#196468 = CARTESIAN_POINT('',(57.3860839754601,3.00000000004986,64.0110910533819)) ;
#196469 = CARTESIAN_POINT('Origin',(60.0566078658524,-2.99999999995017,66.9917599116879)) ;
#196470 = CARTESIAN_POINT('Origin',(58.7213459206563,3.00000000004985,65.5014254825341)) ;
#196471 = CARTESIAN_POINT('',(57.3860839754601,3.00000000004986,64.0110910533819)) ;
#196472 = CARTESIAN_POINT('',(57.3860839754601,-2.99999999995014,64.0110910533818)) ;
#196473 = CARTESIAN_POINT('Origin',(60.0566078658528,3.00000000004983,66.9917599116864)) ;
#196474 = CARTESIAN_POINT('',(-46.0841176604154,3.00000000005113,-60.613533327286)) ;
#196475 = CARTESIAN_POINT('',(-5.85091647147829,3.00000000005069,-17.9146369823475)) ;
#196476 = CARTESIAN_POINT('',(-46.0841176604154,3.00000000005113,-60.613533327286)) ;
#196477 = CARTESIAN_POINT('',(-45.712767762275,3.00000000005117,-64.3658262435518)) ;
#196478 = CARTESIAN_POINT('Origin',(-44.2645963709399,3.00000000005114,-62.3279843406267)) ;
#196479 = CARTESIAN_POINT('',(35.6411531528819,3.00000000005123,-70.4471903523474)) ;
#196480 = CARTESIAN_POINT('Origin',(4.44089209850063E-15,3.00000000005052,
-0.039604774162747)) ;
#196481 = CARTESIAN_POINT('',(36.5662411594172,3.00000000005119,-66.7918086956022)) ;
#196482 = CARTESIAN_POINT('Origin',(34.512048509326,3.0000000000512,-68.2166920439193)) ;
#196483 = CARTESIAN_POINT('',(3.12835464206557,3.0000000000507,-18.5858549944469)) ;
#196484 = CARTESIAN_POINT('',(3.12835464206557,3.0000000000507,-18.5858549944469)) ;
#196485 = CARTESIAN_POINT('',(0.939891742978034,3.00000000005069,-17.5143466466889)) ;
#196486 = CARTESIAN_POINT('Origin',(1.07416199197492,3.00000000005071,-20.0107383427636)) ;
#196487 = CARTESIAN_POINT('',(-3.52747078425273,3.00000000005069,-17.1804025929978)) ;
#196488 = CARTESIAN_POINT('Origin',(-7.0832228971085E-13,3.00000000005055,
-0.0396047741727124)) ;
#196489 = CARTESIAN_POINT('Origin',(-4.03139518200323,3.00000000005071,-19.6290879956887)) ;
#196490 = CARTESIAN_POINT('',(-7.97774182302844,3.00000000005051,0.556746971962394)) ;
#196491 = CARTESIAN_POINT('Origin',(4.21884749357559E-14,3.00000000005051,
-0.0396047741617706)) ;
#196492 = CARTESIAN_POINT('',(-71.8500049958893,3.00000000005026,25.0706222855197)) ;
#196493 = CARTESIAN_POINT('',(-18.8081984829363,3.00000000005051,0.00125873500750827)) ;
#196494 = CARTESIAN_POINT('',(-71.8500049958893,3.00000000005026,25.0706222855197)) ;
#196495 = CARTESIAN_POINT('',(-75.3038941955674,3.00000000005027,23.5579252660689)) ;
#196496 = CARTESIAN_POINT('Origin',(-72.9182818039207,3.00000000005028,22.8103602074803)) ;
#196497 = CARTESIAN_POINT('',(-55.9478710373819,3.00000000005108,-55.6934962050514)) ;
#196498 = CARTESIAN_POINT('Origin',(-1.36779476633819E-12,3.00000000005052,
-0.0396047741619743)) ;
#196499 = CARTESIAN_POINT('',(-52.1855285778765,3.00000000005108,-55.4437321289526)) ;
#196500 = CARTESIAN_POINT('Origin',(-54.1754536098524,3.00000000005106,-53.9303919929892)) ;
#196501 = CARTESIAN_POINT('',(-16.671817376013,3.0000000000506,-8.74595334177845)) ;
#196502 = CARTESIAN_POINT('',(-16.671817376013,3.0000000000506,-8.74595334177845)) ;
#196503 = CARTESIAN_POINT('',(-16.3290246069902,3.00000000005058,-6.3334871518594)) ;
#196504 = CARTESIAN_POINT('Origin',(-18.6617424079881,3.00000000005057,-7.23261320581606)) ;
#196505 = CARTESIAN_POINT('',(-17.3919158795974,3.00000000005053,-1.98157852192261)) ;
#196506 = CARTESIAN_POINT('Origin',(-1.83275616905121E-11,3.00000000005052,
-0.0396047741661859)) ;
#196507 = CARTESIAN_POINT('Origin',(-19.8764752909687,3.00000000005054,-2.25900334303152)) ;
#196508 = CARTESIAN_POINT('',(1.67837248110618,3.00000000004974,76.0532975670735)) ;
#196509 = CARTESIAN_POINT('',(-5.77318945813033,3.00000000005033,17.8606824715907)) ;
#196510 = CARTESIAN_POINT('',(1.67837248110618,3.00000000004974,76.0532975670735)) ;
#196511 = CARTESIAN_POINT('',(-0.827598335811217,3.00000000004971,78.8706923106381)) ;
#196512 = CARTESIAN_POINT('Origin',(-0.801380185125995,3.00000000004973,76.3708297927037)) ;
#196513 = CARTESIAN_POINT('',(-70.2188390521795,3.00000000005014,35.9719842935381)) ;
#196514 = CARTESIAN_POINT('Origin',(-6.21724893790088E-13,3.00000000005051,
-0.0396047741604288)) ;
#196515 = CARTESIAN_POINT('',(-68.8186715414237,3.00000000005018,32.4709653249907)) ;
#196516 = CARTESIAN_POINT('Origin',(-67.9943201961579,3.00000000005016,34.8311443138723)) ;
#196517 = CARTESIAN_POINT('',(-13.4321044346723,3.00000000005038,13.1258261134328)) ;
#196518 = CARTESIAN_POINT('',(-13.4321044346723,3.00000000005038,13.1258261134328)) ;
#196519 = CARTESIAN_POINT('',(-11.0317839532312,3.00000000005037,13.5453038677549)) ;
#196520 = CARTESIAN_POINT('Origin',(-12.6077530894068,3.00000000005033,15.4860051023136)) ;
#196521 = CARTESIAN_POINT('',(-7.22132435881713,3.00000000005035,15.9009872632986)) ;
#196522 = CARTESIAN_POINT('Origin',(-6.28497254240301E-12,3.00000000005062,
-0.0396047741513206)) ;
#196523 = CARTESIAN_POINT('Origin',(-8.25294212436289,3.00000000005033,18.1782146972216)) ;
#196524 = CARTESIAN_POINT('',(72.8872962349953,3.00000000005029,21.8781681156668)) ;
#196525 = CARTESIAN_POINT('',(15.240171174319,3.0000000000504,10.9825176429304)) ;
#196526 = CARTESIAN_POINT('',(72.8872962349953,3.00000000005029,21.8781681156668)) ;
#196527 = CARTESIAN_POINT('',(74.7924102950029,3.00000000005026,25.1321108463659)) ;
#196528 = CARTESIAN_POINT('Origin',(72.423001611602,3.00000000005026,24.3346759016687)) ;
#196529 = CARTESIAN_POINT('',(12.5502418525765,3.00000000004972,77.8706726894606)) ;
#196530 = CARTESIAN_POINT('Origin',(7.48290318597356E-13,3.00000000005051,
-0.0396047741607486)) ;
#196531 = CARTESIAN_POINT('',(9.65325050466174,3.00000000004974,75.4571598955414)) ;
#196532 = CARTESIAN_POINT('Origin',(12.1526526866832,3.00000000004974,75.402490594241)) ;
#196533 = CARTESIAN_POINT('',(8.37032029494708,3.00000000005034,16.8034275585261)) ;
#196534 = CARTESIAN_POINT('',(8.37032029494708,3.00000000005034,16.8034275585261)) ;
#196535 = CARTESIAN_POINT('',(9.51100716734754,3.00000000005036,14.6502128783026)) ;
#196536 = CARTESIAN_POINT('Origin',(10.869722476968,3.00000000005034,16.7487582572255)) ;
#196537 = CARTESIAN_POINT('',(12.9288919820607,3.00000000005039,11.7541966535456)) ;
#196538 = CARTESIAN_POINT('Origin',(4.6385117968839E-12,3.00000000005017,
-0.0396047741558747)) ;
#196539 = CARTESIAN_POINT('Origin',(14.7758765509265,3.00000000005038,13.4390254289324)) ;
#196540 = CARTESIAN_POINT('',(43.3684539402033,3.00000000005115,-62.5865785117813)) ;
#196541 = CARTESIAN_POINT('',(15.192133238226,3.00000000005062,-11.1278457379885)) ;
#196542 = CARTESIAN_POINT('',(43.3684539402033,3.00000000005115,-62.5865785117813)) ;
#196543 = CARTESIAN_POINT('',(47.0518499986506,3.00000000005116,-63.3929260503283)) ;
#196544 = CARTESIAN_POINT('Origin',(45.5612567483845,3.00000000005113,-61.3859054320336)) ;
#196545 = CARTESIAN_POINT('',(77.9753150841032,3.00000000005039,12.1000057035926)) ;
#196546 = CARTESIAN_POINT('Origin',(1.30562227695918E-12,3.00000000005051,
-0.0396047741618544)) ;
#196547 = CARTESIAN_POINT('',(74.7847084552218,3.00000000005037,14.109391733215)) ;
#196548 = CARTESIAN_POINT('Origin',(75.5050726100008,3.00000000005039,11.7154252579882)) ;
#196549 = CARTESIAN_POINT('',(18.6052468736726,3.00000000005054,-2.79546920654119)) ;
#196550 = CARTESIAN_POINT('',(18.6052468736726,3.00000000005054,-2.79546920654119)) ;
#196551 = CARTESIAN_POINT('',(16.909909649896,3.00000000005056,-4.54570681831662)) ;
#196552 = CARTESIAN_POINT('Origin',(19.3256110284515,3.00000000005055,-5.1894356817668)) ;
#196553 = CARTESIAN_POINT('',(15.2118190406069,3.0000000000506,-8.69122667273134)) ;
#196554 = CARTESIAN_POINT('Origin',(8.04245559038463E-12,3.0000000000501,
-0.0396047741647687)) ;
#196555 = CARTESIAN_POINT('Origin',(17.3849360464078,3.00000000005063,-9.92717265824142)) ;
#196556 = CARTESIAN_POINT('Origin',(60.0566078658528,-2.99999999995017,66.9917599116863)) ;
#196557 = CARTESIAN_POINT('',(-1.38175761627864,-2.99999999994865,-83.3427827144731)) ;
#196558 = CARTESIAN_POINT('Origin',(4.413136522885E-14,-2.99999999994949,
-0.0396047741616457)) ;
#196559 = CARTESIAN_POINT('Origin',(-7.51482209793153E-13,5.05127219874221E-11,
-0.0396047741696215)) ;
#196560 = CARTESIAN_POINT('',(0.939891742978034,-2.99999999994931,-17.5143466466889)) ;
#196561 = CARTESIAN_POINT('',(0.939891742978034,3.00000000005069,-17.5143466466889)) ;
#196562 = CARTESIAN_POINT('',(-3.52747078425273,-2.99999999994931,-17.1804025929979)) ;
#196563 = CARTESIAN_POINT('Origin',(-8.10462807976364E-13,-2.99999999994978,
-0.0396047741726324)) ;
#196564 = CARTESIAN_POINT('',(-3.52747078425273,3.00000000005069,-17.1804025929978)) ;
#196565 = CARTESIAN_POINT('Origin',(-4.0313951820033,5.07108855651976E-11,
-19.6290879956884)) ;
#196566 = CARTESIAN_POINT('',(-5.85091647147829,-2.99999999994931,-17.9146369823476)) ;
#196567 = CARTESIAN_POINT('Origin',(-4.03139518200323,-2.99999999994929,-19.6290879956887)) ;
#196568 = CARTESIAN_POINT('',(-5.85091647147829,3.00000000005069,-17.9146369823475)) ;
#196569 = CARTESIAN_POINT('Origin',(-5.85091647147829,5.06927833043846E-11,
-17.9146369823476)) ;
#196570 = CARTESIAN_POINT('',(-46.0841176604154,-2.99999999994887,-60.6135333272861)) ;
#196571 = CARTESIAN_POINT('',(-46.0841176604154,3.00000000005113,-60.613533327286)) ;
#196572 = CARTESIAN_POINT('',(-46.0841176604154,-2.99999999994887,-60.6135333272861)) ;
#196573 = CARTESIAN_POINT('Origin',(-44.2645963709396,5.11477689214468E-11,
-62.3279843406269)) ;
#196574 = CARTESIAN_POINT('',(-45.712767762275,-2.99999999994883,-64.3658262435519)) ;
#196575 = CARTESIAN_POINT('Origin',(-44.2645963709399,-2.99999999994886,-62.3279843406268)) ;
#196576 = CARTESIAN_POINT('',(-45.712767762275,3.00000000005117,-64.3658262435518)) ;
#196577 = CARTESIAN_POINT('Origin',(-4.44089209850063E-13,5.05069715077991E-11,
-0.0396047741635108)) ;
#196578 = CARTESIAN_POINT('',(35.6411531528819,-2.99999999994877,-70.4471903523475)) ;
#196579 = CARTESIAN_POINT('Origin',(4.44089209850063E-15,-2.99999999994949,
-0.0396047741628003)) ;
#196580 = CARTESIAN_POINT('',(35.6411531528819,3.00000000005123,-70.4471903523474)) ;
#196581 = CARTESIAN_POINT('Origin',(34.5120485093257,5.12090018418964E-11,
-68.2166920439191)) ;
#196582 = CARTESIAN_POINT('',(36.5662411594172,-2.99999999994881,-66.7918086956023)) ;
#196583 = CARTESIAN_POINT('Origin',(34.512048509326,-2.99999999994881,-68.2166920439194)) ;
#196584 = CARTESIAN_POINT('',(36.5662411594172,3.00000000005119,-66.7918086956022)) ;
#196585 = CARTESIAN_POINT('Origin',(36.5662411594171,5.11901632194167E-11,
-66.7918086956023)) ;
#196586 = CARTESIAN_POINT('',(3.12835464206557,-2.9999999999493,-18.5858549944469)) ;
#196587 = CARTESIAN_POINT('',(3.12835464206557,-2.9999999999493,-18.5858549944469)) ;
#196588 = CARTESIAN_POINT('',(3.12835464206557,3.0000000000507,-18.5858549944469)) ;
#196589 = CARTESIAN_POINT('Origin',(1.07416199197442,5.07138545131367E-11,
-20.0107383427642)) ;
#196590 = CARTESIAN_POINT('Origin',(1.07416199197492,-2.99999999994927,-20.0107383427637)) ;
#196591 = CARTESIAN_POINT('Origin',(-7.66053886991358E-14,5.05179569195172E-11,
-0.0396047741617249)) ;
#196592 = CARTESIAN_POINT('',(-7.97774182302844,-2.99999999994949,0.556746971962333)) ;
#196593 = CARTESIAN_POINT('Origin',(3.99680288865056E-14,-2.99999999994949,
-0.0396047741618317)) ;
#196594 = CARTESIAN_POINT('',(-7.97774182302844,5.05118844343928E-11,0.556746971962363)) ;
#196595 = CARTESIAN_POINT('Origin',(-1.30118138486068E-11,5.0511046670509E-11,
-0.0396047741651795)) ;
#196596 = CARTESIAN_POINT('',(-16.3290246069902,-2.99999999994942,-6.33348715185946)) ;
#196597 = CARTESIAN_POINT('',(-16.3290246069902,3.00000000005058,-6.3334871518594)) ;
#196598 = CARTESIAN_POINT('',(-17.3919158795974,-2.99999999994947,-1.98157852192267)) ;
#196599 = CARTESIAN_POINT('Origin',(-1.83542070431031E-11,-2.99999999994958,
-0.0396047741661992)) ;
#196600 = CARTESIAN_POINT('',(-17.3919158795974,3.00000000005053,-1.98157852192261)) ;
#196601 = CARTESIAN_POINT('Origin',(-19.8764752909685,5.05335163215292E-11,
-2.25900334303148)) ;
#196602 = CARTESIAN_POINT('',(-18.8081984829363,-2.99999999994949,0.00125873500744717)) ;
#196603 = CARTESIAN_POINT('Origin',(-19.8764752909687,-2.99999999994946,-2.25900334303158)) ;
#196604 = CARTESIAN_POINT('',(-18.8081984829363,3.00000000005051,0.00125873500750827)) ;
#196605 = CARTESIAN_POINT('Origin',(-18.8081984829363,5.05107067283461E-11,
0.00125873500742087)) ;
#196606 = CARTESIAN_POINT('',(-71.8500049958893,-2.99999999994974,25.0706222855196)) ;
#196607 = CARTESIAN_POINT('',(-71.8500049958893,3.00000000005026,25.0706222855197)) ;
#196608 = CARTESIAN_POINT('',(-71.8500049958893,-2.99999999994974,25.0706222855196)) ;
#196609 = CARTESIAN_POINT('Origin',(-72.9182818039209,5.02782135032148E-11,
22.8103602074799)) ;
#196610 = CARTESIAN_POINT('',(-75.3038941955674,-2.99999999994973,23.5579252660688)) ;
#196611 = CARTESIAN_POINT('Origin',(-72.9182818039207,-2.99999999994972,22.8103602074803)) ;
#196612 = CARTESIAN_POINT('',(-75.3038941955674,3.00000000005027,23.5579252660689)) ;
#196613 = CARTESIAN_POINT('Origin',(-1.87405646556726E-12,5.05125615832167E-11,
-0.0396047741619432)) ;
#196614 = CARTESIAN_POINT('',(-55.9478710373819,-2.99999999994892,-55.6934962050515)) ;
#196615 = CARTESIAN_POINT('Origin',(-1.4299672557172E-12,-2.99999999994949,
-0.0396047741618766)) ;
#196616 = CARTESIAN_POINT('',(-55.9478710373819,3.00000000005108,-55.6934962050514)) ;
#196617 = CARTESIAN_POINT('Origin',(-54.1754536098523,5.10588644666463E-11,
-53.9303919929891)) ;
#196618 = CARTESIAN_POINT('',(-52.1855285778765,-2.99999999994892,-55.4437321289526)) ;
#196619 = CARTESIAN_POINT('Origin',(-54.1754536098524,-2.99999999994894,-53.9303919929893)) ;
#196620 = CARTESIAN_POINT('',(-52.1855285778765,3.00000000005108,-55.4437321289526)) ;
#196621 = CARTESIAN_POINT('Origin',(-52.1855285778767,5.1076920470905E-11,
-55.4437321289526)) ;
#196622 = CARTESIAN_POINT('',(-16.671817376013,-2.9999999999494,-8.74595334177851)) ;
#196623 = CARTESIAN_POINT('',(-16.671817376013,-2.9999999999494,-8.74595334177851)) ;
#196624 = CARTESIAN_POINT('',(-16.671817376013,3.0000000000506,-8.74595334177845)) ;
#196625 = CARTESIAN_POINT('Origin',(-18.6617424079886,5.05884672997123E-11,
-7.23261320581591)) ;
#196626 = CARTESIAN_POINT('Origin',(-18.6617424079882,-2.99999999994939,-7.23261320581612)) ;
#196627 = CARTESIAN_POINT('Origin',(-5.98188165668034E-12,5.05112930172867E-11,
-0.0396047741518712)) ;
#196628 = CARTESIAN_POINT('',(-11.0317839532312,-2.99999999994963,13.5453038677548)) ;
#196629 = CARTESIAN_POINT('',(-11.0317839532312,3.00000000005037,13.5453038677549)) ;
#196630 = CARTESIAN_POINT('',(-7.22132435881713,-2.99999999994965,15.9009872632985)) ;
#196631 = CARTESIAN_POINT('Origin',(-6.17617068598975E-12,-2.99999999994964,
-0.0396047741515204)) ;
#196632 = CARTESIAN_POINT('',(-7.22132435881713,3.00000000005035,15.9009872632986)) ;
#196633 = CARTESIAN_POINT('Origin',(-8.25294212436249,5.0325584525273E-11,
18.1782146972211)) ;
#196634 = CARTESIAN_POINT('',(-5.77318945813033,-2.99999999994967,17.8606824715907)) ;
#196635 = CARTESIAN_POINT('Origin',(-8.25294212436291,-2.99999999994968,18.1782146972216)) ;
#196636 = CARTESIAN_POINT('',(-5.77318945813033,3.00000000005033,17.8606824715907)) ;
#196637 = CARTESIAN_POINT('Origin',(-5.77318945813045,5.03308505983568E-11,
17.8606824715907)) ;
#196638 = CARTESIAN_POINT('',(1.67837248110618,-2.99999999995026,76.0532975670734)) ;
#196639 = CARTESIAN_POINT('',(1.67837248110618,3.00000000004974,76.0532975670735)) ;
#196640 = CARTESIAN_POINT('',(1.67837248110618,-2.99999999995026,76.0532975670734)) ;
#196641 = CARTESIAN_POINT('Origin',(-0.801380185126325,4.97325191999056E-11,
76.3708297927036)) ;
#196642 = CARTESIAN_POINT('',(-0.827598335811217,-2.99999999995029,78.870692310638)) ;
#196643 = CARTESIAN_POINT('Origin',(-0.801380185126014,-2.99999999995027,
76.3708297927036)) ;
#196644 = CARTESIAN_POINT('',(-0.827598335811217,3.00000000004971,78.8706923106381)) ;
#196645 = CARTESIAN_POINT('Origin',(-8.15458811587177E-13,5.0476842336372E-11,
-0.0396047741597982)) ;
#196646 = CARTESIAN_POINT('',(-70.2188390521795,-2.99999999994985,35.971984293538)) ;
#196647 = CARTESIAN_POINT('Origin',(-6.21724893790088E-13,-2.99999999994948,
-0.039604774160491)) ;
#196648 = CARTESIAN_POINT('',(-70.2188390521795,3.00000000005014,35.9719842935381)) ;
#196649 = CARTESIAN_POINT('Origin',(-67.9943201961576,5.01582369534571E-11,
34.8311443138724)) ;
#196650 = CARTESIAN_POINT('',(-68.8186715414237,-2.99999999994982,32.4709653249907)) ;
#196651 = CARTESIAN_POINT('Origin',(-67.9943201961579,-2.99999999994984,34.8311443138722)) ;
#196652 = CARTESIAN_POINT('',(-68.8186715414237,3.00000000005018,32.4709653249907)) ;
#196653 = CARTESIAN_POINT('Origin',(-68.8186715414238,5.01776398209586E-11,
32.4709653249907)) ;
#196654 = CARTESIAN_POINT('',(-13.4321044346723,-2.99999999994962,13.1258261134327)) ;
#196655 = CARTESIAN_POINT('',(-13.4321044346723,-2.99999999994962,13.1258261134327)) ;
#196656 = CARTESIAN_POINT('',(-13.4321044346723,3.00000000005038,13.1258261134328)) ;
#196657 = CARTESIAN_POINT('Origin',(-12.6077530894068,5.03536114333649E-11,
15.4860051023138)) ;
#196658 = CARTESIAN_POINT('Origin',(-12.6077530894068,-2.99999999994965,15.4860051023136)) ;
#196659 = CARTESIAN_POINT('Origin',(4.57522908448027E-12,5.05123757157332E-11,
-0.0396047741559635)) ;
#196660 = CARTESIAN_POINT('',(9.51100716734754,-2.99999999994964,14.6502128783025)) ;
#196661 = CARTESIAN_POINT('',(9.51100716734754,3.00000000005036,14.6502128783026)) ;
#196662 = CARTESIAN_POINT('',(12.9288919820607,-2.99999999994961,11.7541966535455)) ;
#196663 = CARTESIAN_POINT('Origin',(4.49862369578113E-12,-2.99999999994982,
-0.0396047741559302)) ;
#196664 = CARTESIAN_POINT('',(12.9288919820607,3.00000000005039,11.7541966535456)) ;
#196665 = CARTESIAN_POINT('Origin',(14.7758765509261,5.03736560984678E-11,
13.4390254289319)) ;
#196666 = CARTESIAN_POINT('',(15.240171174319,-2.9999999999496,10.9825176429303)) ;
#196667 = CARTESIAN_POINT('Origin',(14.7758765509265,-2.99999999994962,13.4390254289324)) ;
#196668 = CARTESIAN_POINT('',(15.240171174319,3.0000000000504,10.9825176429304)) ;
#196669 = CARTESIAN_POINT('Origin',(15.240171174319,5.04019048719329E-11,
10.9825176429304)) ;
#196670 = CARTESIAN_POINT('',(72.8872962349953,-2.99999999994971,21.8781681156667)) ;
#196671 = CARTESIAN_POINT('',(72.8872962349953,3.00000000005029,21.8781681156668)) ;
#196672 = CARTESIAN_POINT('',(72.8872962349953,-2.99999999994971,21.8781681156667)) ;
#196673 = CARTESIAN_POINT('Origin',(72.4230016116015,5.02615989705098E-11,
24.3346759016693)) ;
#196674 = CARTESIAN_POINT('',(74.7924102950029,-2.99999999994974,25.1321108463658)) ;
#196675 = CARTESIAN_POINT('Origin',(72.423001611602,-2.99999999994973,24.3346759016686)) ;
#196676 = CARTESIAN_POINT('',(74.7924102950029,3.00000000005026,25.1321108463659)) ;
#196677 = CARTESIAN_POINT('Origin',(7.8159700933611E-13,5.0513139743634E-11,
-0.0396047741607131)) ;
#196678 = CARTESIAN_POINT('',(12.5502418525765,-2.99999999995028,77.8706726894606)) ;
#196679 = CARTESIAN_POINT('Origin',(7.105427357601E-13,-2.99999999994951,
-0.0396047741608285)) ;
#196680 = CARTESIAN_POINT('',(12.5502418525765,3.00000000004972,77.8706726894606)) ;
#196681 = CARTESIAN_POINT('Origin',(12.1526526866834,4.97404318529672E-11,
75.4024905942403)) ;
#196682 = CARTESIAN_POINT('',(9.65325050466174,-2.99999999995026,75.4571598955413)) ;
#196683 = CARTESIAN_POINT('Origin',(12.1526526866832,-2.99999999995026,75.402490594241)) ;
#196684 = CARTESIAN_POINT('',(9.65325050466174,3.00000000004974,75.4571598955414)) ;
#196685 = CARTESIAN_POINT('Origin',(9.65325050466163,4.97402119492563E-11,
75.4571598955414)) ;
#196686 = CARTESIAN_POINT('',(8.37032029494708,-2.99999999994966,16.8034275585261)) ;
#196687 = CARTESIAN_POINT('',(8.37032029494708,-2.99999999994966,16.8034275585261)) ;
#196688 = CARTESIAN_POINT('',(8.37032029494708,3.00000000005034,16.8034275585261)) ;
#196689 = CARTESIAN_POINT('Origin',(10.8697224769681,5.03425161977803E-11,
16.7487582572254)) ;
#196690 = CARTESIAN_POINT('Origin',(10.869722476968,-2.99999999994966,16.7487582572254)) ;
#196691 = CARTESIAN_POINT('Origin',(6.82343070934621E-12,5.05114052809432E-11,
-0.0396047741643929)) ;
#196692 = CARTESIAN_POINT('',(16.909909649896,-2.99999999994944,-4.54570681831668)) ;
#196693 = CARTESIAN_POINT('',(16.909909649896,3.00000000005056,-4.54570681831662)) ;
#196694 = CARTESIAN_POINT('',(15.2118190406069,-2.9999999999494,-8.6912266727314)) ;
#196695 = CARTESIAN_POINT('Origin',(8.07576228112339E-12,-2.99999999994975,
-0.0396047741648997)) ;
#196696 = CARTESIAN_POINT('',(15.2118190406069,3.0000000000506,-8.69122667273134)) ;
#196697 = CARTESIAN_POINT('Origin',(17.3849360464075,5.0614323268569E-11,
-9.92717265824137)) ;
#196698 = CARTESIAN_POINT('',(15.192133238226,-2.99999999994937,-11.1278457379886)) ;
#196699 = CARTESIAN_POINT('Origin',(17.3849360464078,-2.99999999994938,-9.92717265824148)) ;
#196700 = CARTESIAN_POINT('',(15.192133238226,3.00000000005062,-11.1278457379885)) ;
#196701 = CARTESIAN_POINT('Origin',(15.1921332382259,5.06217290308086E-11,
-11.1278457379886)) ;
#196702 = CARTESIAN_POINT('',(43.3684539402033,-2.99999999994885,-62.5865785117814)) ;
#196703 = CARTESIAN_POINT('',(43.3684539402033,3.00000000005115,-62.5865785117813)) ;
#196704 = CARTESIAN_POINT('',(43.3684539402033,-2.99999999994885,-62.5865785117814)) ;
#196705 = CARTESIAN_POINT('Origin',(45.5612567483847,5.11356786146817E-11,
-61.3859054320333)) ;
#196706 = CARTESIAN_POINT('',(47.0518499986506,-2.99999999994884,-63.3929260503284)) ;
#196707 = CARTESIAN_POINT('Origin',(45.5612567483845,-2.99999999994886,-61.3859054320336)) ;
#196708 = CARTESIAN_POINT('',(47.0518499986506,3.00000000005116,-63.3929260503283)) ;
#196709 = CARTESIAN_POINT('Origin',(1.58983937126322E-12,5.05264937529502E-11,
-0.0396047741621075)) ;
#196710 = CARTESIAN_POINT('',(77.9753150841032,-2.99999999994961,12.1000057035925)) ;
#196711 = CARTESIAN_POINT('Origin',(1.34114941374719E-12,-2.99999999994948,
-0.0396047741619077)) ;
#196712 = CARTESIAN_POINT('',(77.9753150841032,3.00000000005039,12.1000057035926)) ;
#196713 = CARTESIAN_POINT('Origin',(75.5050726100009,5.03925206957646E-11,
11.7154252579883)) ;
#196714 = CARTESIAN_POINT('',(74.7847084552218,-2.99999999994963,14.109391733215)) ;
#196715 = CARTESIAN_POINT('Origin',(75.5050726100008,-2.99999999994961,11.7154252579881)) ;
#196716 = CARTESIAN_POINT('',(74.7847084552218,3.00000000005037,14.109391733215)) ;
#196717 = CARTESIAN_POINT('Origin',(74.7847084552217,5.03663777351449E-11,
14.109391733215)) ;
#196718 = CARTESIAN_POINT('',(18.6052468736726,-2.99999999994946,-2.79546920654126)) ;
#196719 = CARTESIAN_POINT('',(18.6052468736726,-2.99999999994946,-2.79546920654126)) ;
#196720 = CARTESIAN_POINT('',(18.6052468736726,3.00000000005054,-2.79546920654119)) ;
#196721 = CARTESIAN_POINT('Origin',(19.3256110284516,5.05639742890559E-11,
-5.18943568176694)) ;
#196722 = CARTESIAN_POINT('Origin',(19.3256110284515,-2.99999999994942,-5.18943568176686)) ;
#196723 = CARTESIAN_POINT('Origin',(8.99280649946377E-14,-4.74303254878962,
-0.0396047741615924)) ;
#196724 = CARTESIAN_POINT('',(-1.38175761627864,-1.60984001328294,-83.3427827144731)) ;
#196725 = CARTESIAN_POINT('',(-1.38175761627864,-4.74303254878868,-83.3427827144731)) ;
#196726 = CARTESIAN_POINT('Origin',(1.51545442861334E-13,-1.60984001328399,
-0.0396047741615924)) ;
#196727 = CARTESIAN_POINT('Origin',(1.96231919602496E-13,-4.74303254878962,
-0.0396047741618233)) ;
#196728 = CARTESIAN_POINT('',(-1.34527102914679,-1.60984001328296,-81.1430852968819)) ;
#196729 = CARTESIAN_POINT('Origin',(5.63438184997267E-14,-1.60984001328399,
-0.0396047741615391)) ;
#196730 = CARTESIAN_POINT('',(-1.34527102914679,-2.99999999994868,-81.1430852968819)) ;
#196731 = CARTESIAN_POINT('',(-1.34527102914679,-4.7430325487887,-81.1430852968819)) ;
#196732 = CARTESIAN_POINT('Origin',(8.79851747015437E-14,-2.99999999994949,
-0.0396047741615924)) ;
#196733 = CARTESIAN_POINT('Origin',(1.34527102914717,-1.60984001328482,81.0638757485583)) ;
#196734 = CARTESIAN_POINT('Origin',(60.0566078658528,-2.99999999995017,66.9917599116863)) ;
#196735 = CARTESIAN_POINT('',(0.,0.,0.)) ;
#196736 = UNCERTAINTY_MEASURE_WITH_UNIT(LENGTH_MEASURE(0.01),#196742,
'DISTANCE_ACCURACY_VALUE',
'Maximum model space distance between geometric entities at asserted c
onnectivities') ;
#196737 = UNCERTAINTY_MEASURE_WITH_UNIT(LENGTH_MEASURE(0.01),#196742,
'DISTANCE_ACCURACY_VALUE',
'Maximum model space distance between geometric entities at asserted c
onnectivities') ;
#196738 = UNCERTAINTY_MEASURE_WITH_UNIT(LENGTH_MEASURE(0.01),#196742,
'DISTANCE_ACCURACY_VALUE',
'Maximum model space distance between geometric entities at asserted c
onnectivities') ;
#196739 = (
GEOMETRIC_REPRESENTATION_CONTEXT(3)
GLOBAL_UNCERTAINTY_ASSIGNED_CONTEXT((#196736))
GLOBAL_UNIT_ASSIGNED_CONTEXT((#196742,#196744,#196745))
REPRESENTATION_CONTEXT('','3D')
) ;
#196740 = (
GEOMETRIC_REPRESENTATION_CONTEXT(3)
GLOBAL_UNCERTAINTY_ASSIGNED_CONTEXT((#196737))
GLOBAL_UNIT_ASSIGNED_CONTEXT((#196742,#196744,#196745))
REPRESENTATION_CONTEXT('','3D')
) ;
#196741 = (
GEOMETRIC_REPRESENTATION_CONTEXT(3)
GLOBAL_UNCERTAINTY_ASSIGNED_CONTEXT((#196738))
GLOBAL_UNIT_ASSIGNED_CONTEXT((#196742,#196744,#196745))
REPRESENTATION_CONTEXT('','3D')
) ;
#196742 = (
LENGTH_UNIT()
NAMED_UNIT(*)
SI_UNIT(.MILLI.,.METRE.)
) ;
#196743 = (
LENGTH_UNIT()
NAMED_UNIT(*)
SI_UNIT($,.METRE.)
) ;
#196744 = (
NAMED_UNIT(*)
PLANE_ANGLE_UNIT()
SI_UNIT($,.RADIAN.)
) ;
#196745 = (
NAMED_UNIT(*)
SI_UNIT($,.STERADIAN.)
SOLID_ANGLE_UNIT()
) ;
#196746 = SHAPE_DEFINITION_REPRESENTATION(#196748,#196751) ;
#196748 = PRODUCT_DEFINITION_SHAPE('',$,#196754) ;
#196751 = SHAPE_REPRESENTATION ( 'MAS-211', ( #8746, #9454, #197242, #197255, #197268, #197281, #197294, #197307, #197320, #197333, #197346, #197359, #197372, #197385, #197398, #197411, #197424, #197437, #197450, #197463, #197476, #197489, #197502 ), #196739 ) ;
#196753 = PRODUCT_DEFINITION_CONTEXT('part definition',#196761,'design') ;
#196754 = PRODUCT_DEFINITION('MAS-211',
'MAS-211',#196756,#196753) ;
#196756 = PRODUCT_DEFINITION_FORMATION('',$,#196763) ;
#196758 = PRODUCT_RELATED_PRODUCT_CATEGORY('part',
'',(#196763)) ;
#196760 = APPLICATION_PROTOCOL_DEFINITION('international standard',
'automotive_design',2009,#196761) ;
#196761 = APPLICATION_CONTEXT(
'Core Data for Automotive Mechanical Design Process') ;
#196762 = PRODUCT_CONTEXT('part definition',#196761,'mechanical') ;
#196763 = PRODUCT('MAS-211','MAS-211',$,(#196762)) ;
#196765 = PRESENTATION_STYLE_ASSIGNMENT((#196767)) ;
#196766 = PRESENTATION_STYLE_ASSIGNMENT((#196768)) ;
#196767 = SURFACE_STYLE_USAGE(.BOTH.,#196769) ;
#196768 = SURFACE_STYLE_USAGE(.BOTH.,#196770) ;
#196769 = SURFACE_SIDE_STYLE('',(#196771)) ;
#196770 = SURFACE_SIDE_STYLE('',(#196772)) ;
#196771 = SURFACE_STYLE_FILL_AREA(#196773) ;
#196772 = SURFACE_STYLE_FILL_AREA(#196774) ;
#196773 = FILL_AREA_STYLE('Steel - Satin',(#196775)) ;
#196774 = FILL_AREA_STYLE('Opaque(0,127,0)',(#196776)) ;
#196775 = FILL_AREA_STYLE_COLOUR('Steel - Satin',#196777) ;
#196776 = FILL_AREA_STYLE_COLOUR('Opaque(0,127,0)',#196778) ;
#196777 = COLOUR_RGB('Steel - Satin', 0.09019608, 0.27058824, 0.51372549) ;
#196778 = COLOUR_RGB('Opaque(0,127,0)', 0.66274510, 0.83137255, 0.94901961) ;
#196779 = CARTESIAN_POINT ( '', ( 0.0, 0.0, 0.0 ) ) ;
#196780 = DIRECTION ( '', ( 0.0, 0.0, 1.0 ) ) ;
#196781 = DIRECTION ( '', ( 1.0, 0.0, 0.0 ) ) ;
#196782 = AXIS2_PLACEMENT_3D ( '', #196779, #196780, #196781 ) ;
#196783 = ADVANCED_BREP_SHAPE_REPRESENTATION ( 'Pendulum Rod', ( #338, #196782, #196793, #197238 ), #196740 ) ;
#196784 = PRODUCT( 'Pendulum Rod', 'Pendulum Rod', '', ( #196762 ) ) ;
#196785 = PRODUCT_DEFINITION_FORMATION ( '', '', #196784 ) ;
#196786 = PRODUCT_DEFINITION( 'Pendulum Rod', 'Pendulum Rod', #196785, #196753 ) ;
#196787 = PRODUCT_DEFINITION_SHAPE ( '', '', #196786 ) ;
#196788 = SHAPE_DEFINITION_REPRESENTATION ( #196787, #196783 ) ;
#196789 = PRODUCT_RELATED_PRODUCT_CATEGORY ( 'part', '', ( #196784 ) ) ;
#196790 = CARTESIAN_POINT ( '', ( 0.0, 0.0, 0.0 ) ) ;
#196791 = DIRECTION ( '', ( 0.0, 0.0, 1.0 ) ) ;
#196792 = DIRECTION ( '', ( 1.0, 0.0, 0.0 ) ) ;
#196793 = AXIS2_PLACEMENT_3D ( '', #196790, #196791, #196792 ) ;
#196803 = CARTESIAN_POINT ( '', ( 0.0, 0.0, 0.0 ) ) ;
#196804 = DIRECTION ( '', ( 0.0, 0.0, 1.0 ) ) ;
#196805 = DIRECTION ( '', ( 1.0, 0.0, 0.0 ) ) ;
#196806 = AXIS2_PLACEMENT_3D ( '', #196803, #196804, #196805 ) ;
#196807 = ADVANCED_BREP_SHAPE_REPRESENTATION ( 'Arbor', ( #339, #196806, #196817, #197251 ), #196740 ) ;
#196808 = PRODUCT( 'Arbor', 'Arbor', '', ( #196762 ) ) ;
#196809 = PRODUCT_DEFINITION_FORMATION ( '', '', #196808 ) ;
#196810 = PRODUCT_DEFINITION( 'Arbor', 'Arbor', #196809, #196753 ) ;
#196811 = PRODUCT_DEFINITION_SHAPE ( '', '', #196810 ) ;
#196812 = SHAPE_DEFINITION_REPRESENTATION ( #196811, #196807 ) ;
#196813 = PRODUCT_RELATED_PRODUCT_CATEGORY ( 'part', '', ( #196808 ) ) ;
#196814 = CARTESIAN_POINT ( '', ( 0.0, 0.0, 0.0 ) ) ;
#196815 = DIRECTION ( '', ( 0.0, 0.0, 1.0 ) ) ;
#196816 = DIRECTION ( '', ( 1.0, 0.0, 0.0 ) ) ;
#196817 = AXIS2_PLACEMENT_3D ( '', #196814, #196815, #196816 ) ;
#196827 = CARTESIAN_POINT ( '', ( 0.0, 0.0, 0.0 ) ) ;
#196828 = DIRECTION ( '', ( 0.0, 0.0, 1.0 ) ) ;
#196829 = DIRECTION ( '', ( 1.0, 0.0, 0.0 ) ) ;
#196830 = AXIS2_PLACEMENT_3D ( '', #196827, #196828, #196829 ) ;
#196831 = ADVANCED_BREP_SHAPE_REPRESENTATION ( 'Entry Pallet Nib', ( #340, #196830, #196841, #197264 ), #196740 ) ;
#196832 = PRODUCT( 'Entry Pallet Nib', 'Entry Pallet Nib', '', ( #196762 ) ) ;
#196833 = PRODUCT_DEFINITION_FORMATION ( '', '', #196832 ) ;
#196834 = PRODUCT_DEFINITION( 'Entry Pallet Nib', 'Entry Pallet Nib', #196833, #196753 ) ;
#196835 = PRODUCT_DEFINITION_SHAPE ( '', '', #196834 ) ;
#196836 = SHAPE_DEFINITION_REPRESENTATION ( #196835, #196831 ) ;
#196837 = PRODUCT_RELATED_PRODUCT_CATEGORY ( 'part', '', ( #196832 ) ) ;
#196838 = CARTESIAN_POINT ( '', ( 0.0, 0.0, 0.0 ) ) ;
#196839 = DIRECTION ( '', ( 0.0, 0.0, 1.0 ) ) ;
#196840 = DIRECTION ( '', ( 1.0, 0.0, 0.0 ) ) ;
#196841 = AXIS2_PLACEMENT_3D ( '', #196838, #196839, #196840 ) ;
#196851 = CARTESIAN_POINT ( '', ( 0.0, 0.0, 0.0 ) ) ;
#196852 = DIRECTION ( '', ( 0.0, 0.0, 1.0 ) ) ;
#196853 = DIRECTION ( '', ( 1.0, 0.0, 0.0 ) ) ;
#196854 = AXIS2_PLACEMENT_3D ( '', #196851, #196852, #196853 ) ;
#196855 = ADVANCED_BREP_SHAPE_REPRESENTATION ( 'Exit Pallet Nib', ( #341, #196854, #196865, #197277 ), #196740 ) ;
#196856 = PRODUCT( 'Exit Pallet Nib', 'Exit Pallet Nib', '', ( #196762 ) ) ;
#196857 = PRODUCT_DEFINITION_FORMATION ( '', '', #196856 ) ;
#196858 = PRODUCT_DEFINITION( 'Exit Pallet Nib', 'Exit Pallet Nib', #196857, #196753 ) ;
#196859 = PRODUCT_DEFINITION_SHAPE ( '', '', #196858 ) ;
#196860 = SHAPE_DEFINITION_REPRESENTATION ( #196859, #196855 ) ;
#196861 = PRODUCT_RELATED_PRODUCT_CATEGORY ( 'part', '', ( #196856 ) ) ;
#196862 = CARTESIAN_POINT ( '', ( 0.0, 0.0, 0.0 ) ) ;
#196863 = DIRECTION ( '', ( 0.0, 0.0, 1.0 ) ) ;
#196864 = DIRECTION ( '', ( 1.0, 0.0, 0.0 ) ) ;
#196865 = AXIS2_PLACEMENT_3D ( '', #196862, #196863, #196864 ) ;
#196875 = CARTESIAN_POINT ( '', ( 0.0, 0.0, 0.0 ) ) ;
#196876 = DIRECTION ( '', ( 0.0, 0.0, 1.0 ) ) ;
#196877 = DIRECTION ( '', ( 1.0, 0.0, 0.0 ) ) ;
#196878 = AXIS2_PLACEMENT_3D ( '', #196875, #196876, #196877 ) ;
#196879 = ADVANCED_BREP_SHAPE_REPRESENTATION ( 'Pivot Collar', ( #342, #196878, #196889, #197290, #197485 ), #196740 ) ;
#196880 = PRODUCT( 'Pivot Collar', 'Pivot Collar', '', ( #196762 ) ) ;
#196881 = PRODUCT_DEFINITION_FORMATION ( '', '', #196880 ) ;
#196882 = PRODUCT_DEFINITION( 'Pivot Collar', 'Pivot Collar', #196881, #196753 ) ;
#196883 = PRODUCT_DEFINITION_SHAPE ( '', '', #196882 ) ;
#196884 = SHAPE_DEFINITION_REPRESENTATION ( #196883, #196879 ) ;
#196885 = PRODUCT_RELATED_PRODUCT_CATEGORY ( 'part', '', ( #196880 ) ) ;
#196886 = CARTESIAN_POINT ( '', ( 0.0, 0.0, 0.0 ) ) ;
#196887 = DIRECTION ( '', ( 0.0, 0.0, 1.0 ) ) ;
#196888 = DIRECTION ( '', ( 1.0, 0.0, 0.0 ) ) ;
#196889 = AXIS2_PLACEMENT_3D ( '', #196886, #196887, #196888 ) ;
#196923 = CARTESIAN_POINT ( '', ( 0.0, 0.0, 0.0 ) ) ;
#196924 = DIRECTION ( '', ( 0.0, 0.0, 1.0 ) ) ;
#196925 = DIRECTION ( '', ( 1.0, 0.0, 0.0 ) ) ;
#196926 = AXIS2_PLACEMENT_3D ( '', #196923, #196924, #196925 ) ;
#196927 = ADVANCED_BREP_SHAPE_REPRESENTATION ( 'Entry Pallet Arm', ( #344, #196926, #196937, #197316 ), #196740 ) ;
#196928 = PRODUCT( 'Entry Pallet Arm', 'Entry Pallet Arm', '', ( #196762 ) ) ;
#196929 = PRODUCT_DEFINITION_FORMATION ( '', '', #196928 ) ;
#196930 = PRODUCT_DEFINITION( 'Entry Pallet Arm', 'Entry Pallet Arm', #196929, #196753 ) ;
#196931 = PRODUCT_DEFINITION_SHAPE ( '', '', #196930 ) ;
#196932 = SHAPE_DEFINITION_REPRESENTATION ( #196931, #196927 ) ;
#196933 = PRODUCT_RELATED_PRODUCT_CATEGORY ( 'part', '', ( #196928 ) ) ;
#196934 = CARTESIAN_POINT ( '', ( 0.0, 0.0, 0.0 ) ) ;
#196935 = DIRECTION ( '', ( 0.0, 0.0, 1.0 ) ) ;
#196936 = DIRECTION ( '', ( 1.0, 0.0, 0.0 ) ) ;
#196937 = AXIS2_PLACEMENT_3D ( '', #196934, #196935, #196936 ) ;
#196947 = CARTESIAN_POINT ( '', ( 0.0, 0.0, 0.0 ) ) ;
#196948 = DIRECTION ( '', ( 0.0, 0.0, 1.0 ) ) ;
#196949 = DIRECTION ( '', ( 1.0, 0.0, 0.0 ) ) ;
#196950 = AXIS2_PLACEMENT_3D ( '', #196947, #196948, #196949 ) ;
#196951 = ADVANCED_BREP_SHAPE_REPRESENTATION ( 'Exit Pallet Arm', ( #345, #196950, #196961, #197329 ), #196740 ) ;
#196952 = PRODUCT( 'Exit Pallet Arm', 'Exit Pallet Arm', '', ( #196762 ) ) ;
#196953 = PRODUCT_DEFINITION_FORMATION ( '', '', #196952 ) ;
#196954 = PRODUCT_DEFINITION( 'Exit Pallet Arm', 'Exit Pallet Arm', #196953, #196753 ) ;
#196955 = PRODUCT_DEFINITION_SHAPE ( '', '', #196954 ) ;
#196956 = SHAPE_DEFINITION_REPRESENTATION ( #196955, #196951 ) ;
#196957 = PRODUCT_RELATED_PRODUCT_CATEGORY ( 'part', '', ( #196952 ) ) ;
#196958 = CARTESIAN_POINT ( '', ( 0.0, 0.0, 0.0 ) ) ;
#196959 = DIRECTION ( '', ( 0.0, 0.0, 1.0 ) ) ;
#196960 = DIRECTION ( '', ( 1.0, 0.0, 0.0 ) ) ;
#196961 = AXIS2_PLACEMENT_3D ( '', #196958, #196959, #196960 ) ;
#196971 = CARTESIAN_POINT ( '', ( 0.0, 0.0, 0.0 ) ) ;
#196972 = DIRECTION ( '', ( 0.0, 0.0, 1.0 ) ) ;
#196973 = DIRECTION ( '', ( 1.0, 0.0, 0.0 ) ) ;
#196974 = AXIS2_PLACEMENT_3D ( '', #196971, #196972, #196973 ) ;
#196975 = ADVANCED_BREP_SHAPE_REPRESENTATION ( 'Pallet Pivot Pin', ( #346, #196974, #196985, #197342 ), #196740 ) ;
#196976 = PRODUCT( 'Pallet Pivot Pin', 'Pallet Pivot Pin', '', ( #196762 ) ) ;
#196977 = PRODUCT_DEFINITION_FORMATION ( '', '', #196976 ) ;
#196978 = PRODUCT_DEFINITION( 'Pallet Pivot Pin', 'Pallet Pivot Pin', #196977, #196753 ) ;
#196979 = PRODUCT_DEFINITION_SHAPE ( '', '', #196978 ) ;
#196980 = SHAPE_DEFINITION_REPRESENTATION ( #196979, #196975 ) ;
#196981 = PRODUCT_RELATED_PRODUCT_CATEGORY ( 'part', '', ( #196976 ) ) ;
#196982 = CARTESIAN_POINT ( '', ( 0.0, 0.0, 0.0 ) ) ;
#196983 = DIRECTION ( '', ( 0.0, 0.0, 1.0 ) ) ;
#196984 = DIRECTION ( '', ( 1.0, 0.0, 0.0 ) ) ;
#196985 = AXIS2_PLACEMENT_3D ( '', #196982, #196983, #196984 ) ;
#196995 = CARTESIAN_POINT ( '', ( 0.0, 0.0, 0.0 ) ) ;
#196996 = DIRECTION ( '', ( 0.0, 0.0, 1.0 ) ) ;
#196997 = DIRECTION ( '', ( 1.0, 0.0, 0.0 ) ) ;
#196998 = AXIS2_PLACEMENT_3D ( '', #196995, #196996, #196997 ) ;
#196999 = ADVANCED_BREP_SHAPE_REPRESENTATION ( 'Composer Arm', ( #347, #196998, #197009, #197355 ), #196740 ) ;
#197000 = PRODUCT( 'Composer Arm', 'Composer Arm', '', ( #196762 ) ) ;
#197001 = PRODUCT_DEFINITION_FORMATION ( '', '', #197000 ) ;
#197002 = PRODUCT_DEFINITION( 'Composer Arm', 'Composer Arm', #197001, #196753 ) ;
#197003 = PRODUCT_DEFINITION_SHAPE ( '', '', #197002 ) ;
#197004 = SHAPE_DEFINITION_REPRESENTATION ( #197003, #196999 ) ;
#197005 = PRODUCT_RELATED_PRODUCT_CATEGORY ( 'part', '', ( #197000 ) ) ;
#197006 = CARTESIAN_POINT ( '', ( 0.0, 0.0, 0.0 ) ) ;
#197007 = DIRECTION ( '', ( 0.0, 0.0, 1.0 ) ) ;
#197008 = DIRECTION ( '', ( 1.0, 0.0, 0.0 ) ) ;
#197009 = AXIS2_PLACEMENT_3D ( '', #197006, #197007, #197008 ) ;
#197019 = CARTESIAN_POINT ( '', ( 0.0, 0.0, 0.0 ) ) ;
#197020 = DIRECTION ( '', ( 0.0, 0.0, 1.0 ) ) ;
#197021 = DIRECTION ( '', ( 1.0, 0.0, 0.0 ) ) ;
#197022 = AXIS2_PLACEMENT_3D ( '', #197019, #197020, #197021 ) ;
#197023 = ADVANCED_BREP_SHAPE_REPRESENTATION ( 'Composer Pin', ( #348, #197022, #197033, #197368, #197498 ), #196740 ) ;
#197024 = PRODUCT( 'Composer Pin', 'Composer Pin', '', ( #196762 ) ) ;
#197025 = PRODUCT_DEFINITION_FORMATION ( '', '', #197024 ) ;
#197026 = PRODUCT_DEFINITION( 'Composer Pin', 'Composer Pin', #197025, #196753 ) ;
#197027 = PRODUCT_DEFINITION_SHAPE ( '', '', #197026 ) ;
#197028 = SHAPE_DEFINITION_REPRESENTATION ( #197027, #197023 ) ;
#197029 = PRODUCT_RELATED_PRODUCT_CATEGORY ( 'part', '', ( #197024 ) ) ;
#197030 = CARTESIAN_POINT ( '', ( 0.0, 0.0, 0.0 ) ) ;
#197031 = DIRECTION ( '', ( 0.0, 0.0, 1.0 ) ) ;
#197032 = DIRECTION ( '', ( 1.0, 0.0, 0.0 ) ) ;
#197033 = AXIS2_PLACEMENT_3D ( '', #197030, #197031, #197032 ) ;
#197067 = CARTESIAN_POINT ( '', ( 0.0, 0.0, 0.0 ) ) ;
#197068 = DIRECTION ( '', ( 0.0, 0.0, 1.0 ) ) ;
#197069 = DIRECTION ( '', ( 1.0, 0.0, 0.0 ) ) ;
#197070 = AXIS2_PLACEMENT_3D ( '', #197067, #197068, #197069 ) ;
#197071 = ADVANCED_BREP_SHAPE_REPRESENTATION ( 'Entry Return Spring', ( #350, #197070, #197081, #197394 ), #196740 ) ;
#197072 = PRODUCT( 'Entry Return Spring', 'Entry Return Spring', '', ( #196762 ) ) ;
#197073 = PRODUCT_DEFINITION_FORMATION ( '', '', #197072 ) ;
#197074 = PRODUCT_DEFINITION( 'Entry Return Spring', 'Entry Return Spring', #197073, #196753 ) ;
#197075 = PRODUCT_DEFINITION_SHAPE ( '', '', #197074 ) ;
#197076 = SHAPE_DEFINITION_REPRESENTATION ( #197075, #197071 ) ;
#197077 = PRODUCT_RELATED_PRODUCT_CATEGORY ( 'part', '', ( #197072 ) ) ;
#197078 = CARTESIAN_POINT ( '', ( 0.0, 0.0, 0.0 ) ) ;
#197079 = DIRECTION ( '', ( 0.0, 0.0, 1.0 ) ) ;
#197080 = DIRECTION ( '', ( 1.0, 0.0, 0.0 ) ) ;
#197081 = AXIS2_PLACEMENT_3D ( '', #197078, #197079, #197080 ) ;
#197091 = CARTESIAN_POINT ( '', ( 0.0, 0.0, 0.0 ) ) ;
#197092 = DIRECTION ( '', ( 0.0, 0.0, 1.0 ) ) ;
#197093 = DIRECTION ( '', ( 1.0, 0.0, 0.0 ) ) ;
#197094 = AXIS2_PLACEMENT_3D ( '', #197091, #197092, #197093 ) ;
#197095 = ADVANCED_BREP_SHAPE_REPRESENTATION ( 'Entry Stop Pin', ( #351, #197094, #197105, #197407 ), #196740 ) ;
#197096 = PRODUCT( 'Entry Stop Pin', 'Entry Stop Pin', '', ( #196762 ) ) ;
#197097 = PRODUCT_DEFINITION_FORMATION ( '', '', #197096 ) ;
#197098 = PRODUCT_DEFINITION( 'Entry Stop Pin', 'Entry Stop Pin', #197097, #196753 ) ;
#197099 = PRODUCT_DEFINITION_SHAPE ( '', '', #197098 ) ;
#197100 = SHAPE_DEFINITION_REPRESENTATION ( #197099, #197095 ) ;
#197101 = PRODUCT_RELATED_PRODUCT_CATEGORY ( 'part', '', ( #197096 ) ) ;
#197102 = CARTESIAN_POINT ( '', ( 0.0, 0.0, 0.0 ) ) ;
#197103 = DIRECTION ( '', ( 0.0, 0.0, 1.0 ) ) ;
#197104 = DIRECTION ( '', ( 1.0, 0.0, 0.0 ) ) ;
#197105 = AXIS2_PLACEMENT_3D ( '', #197102, #197103, #197104 ) ;
#197115 = CARTESIAN_POINT ( '', ( 0.0, 0.0, 0.0 ) ) ;
#197116 = DIRECTION ( '', ( 0.0, 0.0, 1.0 ) ) ;
#197117 = DIRECTION ( '', ( 1.0, 0.0, 0.0 ) ) ;
#197118 = AXIS2_PLACEMENT_3D ( '', #197115, #197116, #197117 ) ;
#197119 = ADVANCED_BREP_SHAPE_REPRESENTATION ( 'Exit Stop Pin', ( #352, #197118, #197129, #197420 ), #196740 ) ;
#197120 = PRODUCT( 'Exit Stop Pin', 'Exit Stop Pin', '', ( #196762 ) ) ;
#197121 = PRODUCT_DEFINITION_FORMATION ( '', '', #197120 ) ;
#197122 = PRODUCT_DEFINITION( 'Exit Stop Pin', 'Exit Stop Pin', #197121, #196753 ) ;
#197123 = PRODUCT_DEFINITION_SHAPE ( '', '', #197122 ) ;
#197124 = SHAPE_DEFINITION_REPRESENTATION ( #197123, #197119 ) ;
#197125 = PRODUCT_RELATED_PRODUCT_CATEGORY ( 'part', '', ( #197120 ) ) ;
#197126 = CARTESIAN_POINT ( '', ( 0.0, 0.0, 0.0 ) ) ;
#197127 = DIRECTION ( '', ( 0.0, 0.0, 1.0 ) ) ;
#197128 = DIRECTION ( '', ( 1.0, 0.0, 0.0 ) ) ;
#197129 = AXIS2_PLACEMENT_3D ( '', #197126, #197127, #197128 ) ;
#197139 = CARTESIAN_POINT ( '', ( 0.0, 0.0, 0.0 ) ) ;
#197140 = DIRECTION ( '', ( 0.0, 0.0, 1.0 ) ) ;
#197141 = DIRECTION ( '', ( 1.0, 0.0, 0.0 ) ) ;
#197142 = AXIS2_PLACEMENT_3D ( '', #197139, #197140, #197141 ) ;
#197143 = ADVANCED_BREP_SHAPE_REPRESENTATION ( 'Exit Return Spring', ( #353, #197142, #197153, #197433 ), #196740 ) ;
#197144 = PRODUCT( 'Exit Return Spring', 'Exit Return Spring', '', ( #196762 ) ) ;
#197145 = PRODUCT_DEFINITION_FORMATION ( '', '', #197144 ) ;
#197146 = PRODUCT_DEFINITION( 'Exit Return Spring', 'Exit Return Spring', #197145, #196753 ) ;
#197147 = PRODUCT_DEFINITION_SHAPE ( '', '', #197146 ) ;
#197148 = SHAPE_DEFINITION_REPRESENTATION ( #197147, #197143 ) ;
#197149 = PRODUCT_RELATED_PRODUCT_CATEGORY ( 'part', '', ( #197144 ) ) ;
#197150 = CARTESIAN_POINT ( '', ( 0.0, 0.0, 0.0 ) ) ;
#197151 = DIRECTION ( '', ( 0.0, 0.0, 1.0 ) ) ;
#197152 = DIRECTION ( '', ( 1.0, 0.0, 0.0 ) ) ;
#197153 = AXIS2_PLACEMENT_3D ( '', #197150, #197151, #197152 ) ;
#197163 = CARTESIAN_POINT ( '', ( 0.0, 0.0, 0.0 ) ) ;
#197164 = DIRECTION ( '', ( 0.0, 0.0, 1.0 ) ) ;
#197165 = DIRECTION ( '', ( 1.0, 0.0, 0.0 ) ) ;
#197166 = AXIS2_PLACEMENT_3D ( '', #197163, #197164, #197165 ) ;
#197167 = ADVANCED_BREP_SHAPE_REPRESENTATION ( 'Lever Arm', ( #354, #197166, #197177, #197446 ), #196740 ) ;
#197168 = PRODUCT( 'Lever Arm', 'Lever Arm', '', ( #196762 ) ) ;
#197169 = PRODUCT_DEFINITION_FORMATION ( '', '', #197168 ) ;
#197170 = PRODUCT_DEFINITION( 'Lever Arm', 'Lever Arm', #197169, #196753 ) ;
#197171 = PRODUCT_DEFINITION_SHAPE ( '', '', #197170 ) ;
#197172 = SHAPE_DEFINITION_REPRESENTATION ( #197171, #197167 ) ;
#197173 = PRODUCT_RELATED_PRODUCT_CATEGORY ( 'part', '', ( #197168 ) ) ;
#197174 = CARTESIAN_POINT ( '', ( 0.0, 0.0, 0.0 ) ) ;
#197175 = DIRECTION ( '', ( 0.0, 0.0, 1.0 ) ) ;
#197176 = DIRECTION ( '', ( 1.0, 0.0, 0.0 ) ) ;
#197177 = AXIS2_PLACEMENT_3D ( '', #197174, #197175, #197176 ) ;
#197187 = CARTESIAN_POINT ( '', ( 0.0, 0.0, 0.0 ) ) ;
#197188 = DIRECTION ( '', ( 0.0, 0.0, 1.0 ) ) ;
#197189 = DIRECTION ( '', ( 1.0, 0.0, 0.0 ) ) ;
#197190 = AXIS2_PLACEMENT_3D ( '', #197187, #197188, #197189 ) ;
#197191 = ADVANCED_BREP_SHAPE_REPRESENTATION ( 'Escape Wheel Hub', ( #355, #197190, #197201, #197459 ), #196740 ) ;
#197192 = PRODUCT( 'Escape Wheel Hub', 'Escape Wheel Hub', '', ( #196762 ) ) ;
#197193 = PRODUCT_DEFINITION_FORMATION ( '', '', #197192 ) ;
#197194 = PRODUCT_DEFINITION( 'Escape Wheel Hub', 'Escape Wheel Hub', #197193, #196753 ) ;
#197195 = PRODUCT_DEFINITION_SHAPE ( '', '', #197194 ) ;
#197196 = SHAPE_DEFINITION_REPRESENTATION ( #197195, #197191 ) ;
#197197 = PRODUCT_RELATED_PRODUCT_CATEGORY ( 'part', '', ( #197192 ) ) ;
#197198 = CARTESIAN_POINT ( '', ( 0.0, 0.0, 0.0 ) ) ;
#197199 = DIRECTION ( '', ( 0.0, 0.0, 1.0 ) ) ;
#197200 = DIRECTION ( '', ( 1.0, 0.0, 0.0 ) ) ;
#197201 = AXIS2_PLACEMENT_3D ( '', #197198, #197199, #197200 ) ;
#197211 = CARTESIAN_POINT ( '', ( 0.0, 0.0, 0.0 ) ) ;
#197212 = DIRECTION ( '', ( 0.0, 0.0, 1.0 ) ) ;
#197213 = DIRECTION ( '', ( 1.0, 0.0, 0.0 ) ) ;
#197214 = AXIS2_PLACEMENT_3D ( '', #197211, #197212, #197213 ) ;
#197215 = ADVANCED_BREP_SHAPE_REPRESENTATION ( 'Escape Wheel', ( #356, #197214, #197225, #197472 ), #196740 ) ;
#197216 = PRODUCT( 'Escape Wheel', 'Escape Wheel', '', ( #196762 ) ) ;
#197217 = PRODUCT_DEFINITION_FORMATION ( '', '', #197216 ) ;
#197218 = PRODUCT_DEFINITION( 'Escape Wheel', 'Escape Wheel', #197217, #196753 ) ;
#197219 = PRODUCT_DEFINITION_SHAPE ( '', '', #197218 ) ;
#197220 = SHAPE_DEFINITION_REPRESENTATION ( #197219, #197215 ) ;
#197221 = PRODUCT_RELATED_PRODUCT_CATEGORY ( 'part', '', ( #197216 ) ) ;
#197222 = CARTESIAN_POINT ( '', ( 0.0, 0.0, 0.0 ) ) ;
#197223 = DIRECTION ( '', ( 0.0, 0.0, 1.0 ) ) ;
#197224 = DIRECTION ( '', ( 1.0, 0.0, 0.0 ) ) ;
#197225 = AXIS2_PLACEMENT_3D ( '', #197222, #197223, #197224 ) ;
#197235 = CARTESIAN_POINT ( '', ( 0.0, 0.0, 0.0 ) ) ;
#197236 = DIRECTION ( '', ( 0.0, 0.0, 1.0 ) ) ;
#197237 = DIRECTION ( '', ( 1.0, 0.0, 0.0 ) ) ;
#197238 = AXIS2_PLACEMENT_3D ( '', #197235, #197236, #197237 ) ;
#197239 = CARTESIAN_POINT ( '', ( 0.0, 0.0, 0.0 ) ) ;
#197240 = DIRECTION ( '', ( 0.0, 0.0, 1.0 ) ) ;
#197241 = DIRECTION ( '', ( 1.0, 0.0, 0.0 ) ) ;
#197242 = AXIS2_PLACEMENT_3D ( '', #197239, #197240, #197241 ) ;
#197243 = NEXT_ASSEMBLY_USAGE_OCCURRENCE ( 'Pendulum Rod:1', 'Pendulum Rod:1', 'Pendulum Rod:1', #196754, #196786, $ ) ;
#197244 = PRODUCT_DEFINITION_SHAPE ( '', '', #197243 ) ;
#197245 = ITEM_DEFINED_TRANSFORMATION ( '', '', #197238, #197242 ) ;
#197246 = ( REPRESENTATION_RELATIONSHIP ( '', '', #196783, #196751 ) REPRESENTATION_RELATIONSHIP_WITH_TRANSFORMATION ( #197245 ) SHAPE_REPRESENTATION_RELATIONSHIP ( ) ) ;
#197247 = CONTEXT_DEPENDENT_SHAPE_REPRESENTATION ( #197246, #197244 ) ;
#197248 = CARTESIAN_POINT ( '', ( 0.0, 0.0, 0.0 ) ) ;
#197249 = DIRECTION ( '', ( 0.0, 0.0, 1.0 ) ) ;
#197250 = DIRECTION ( '', ( 1.0, 0.0, 0.0 ) ) ;
#197251 = AXIS2_PLACEMENT_3D ( '', #197248, #197249, #197250 ) ;
#197252 = CARTESIAN_POINT ( '', ( 0.0, 0.0, 0.0 ) ) ;
#197253 = DIRECTION ( '', ( 0.0, 0.0, 1.0 ) ) ;
#197254 = DIRECTION ( '', ( 1.0, 0.0, 0.0 ) ) ;
#197255 = AXIS2_PLACEMENT_3D ( '', #197252, #197253, #197254 ) ;
#197256 = NEXT_ASSEMBLY_USAGE_OCCURRENCE ( 'Arbor:1', 'Arbor:1', 'Arbor:1', #196754, #196810, $ ) ;
#197257 = PRODUCT_DEFINITION_SHAPE ( '', '', #197256 ) ;
#197258 = ITEM_DEFINED_TRANSFORMATION ( '', '', #197251, #197255 ) ;
#197259 = ( REPRESENTATION_RELATIONSHIP ( '', '', #196807, #196751 ) REPRESENTATION_RELATIONSHIP_WITH_TRANSFORMATION ( #197258 ) SHAPE_REPRESENTATION_RELATIONSHIP ( ) ) ;
#197260 = CONTEXT_DEPENDENT_SHAPE_REPRESENTATION ( #197259, #197257 ) ;
#197261 = CARTESIAN_POINT ( '', ( 0.0, 0.0, 0.0 ) ) ;
#197262 = DIRECTION ( '', ( 0.0, 0.0, 1.0 ) ) ;
#197263 = DIRECTION ( '', ( 1.0, 0.0, 0.0 ) ) ;
#197264 = AXIS2_PLACEMENT_3D ( '', #197261, #197262, #197263 ) ;
#197265 = CARTESIAN_POINT ( '', ( 0.0, 0.0, 0.0 ) ) ;
#197266 = DIRECTION ( '', ( 0.0, 0.0, 1.0 ) ) ;
#197267 = DIRECTION ( '', ( 1.0, 0.0, 0.0 ) ) ;
#197268 = AXIS2_PLACEMENT_3D ( '', #197265, #197266, #197267 ) ;
#197269 = NEXT_ASSEMBLY_USAGE_OCCURRENCE ( 'Entry Pallet Nib:1', 'Entry Pallet Nib:1', 'Entry Pallet Nib:1', #196754, #196834, $ ) ;
#197270 = PRODUCT_DEFINITION_SHAPE ( '', '', #197269 ) ;
#197271 = ITEM_DEFINED_TRANSFORMATION ( '', '', #197264, #197268 ) ;
#197272 = ( REPRESENTATION_RELATIONSHIP ( '', '', #196831, #196751 ) REPRESENTATION_RELATIONSHIP_WITH_TRANSFORMATION ( #197271 ) SHAPE_REPRESENTATION_RELATIONSHIP ( ) ) ;
#197273 = CONTEXT_DEPENDENT_SHAPE_REPRESENTATION ( #197272, #197270 ) ;
#197274 = CARTESIAN_POINT ( '', ( 0.0, 0.0, 0.0 ) ) ;
#197275 = DIRECTION ( '', ( 0.0, 0.0, 1.0 ) ) ;
#197276 = DIRECTION ( '', ( 1.0, 0.0, 0.0 ) ) ;
#197277 = AXIS2_PLACEMENT_3D ( '', #197274, #197275, #197276 ) ;
#197278 = CARTESIAN_POINT ( '', ( 0.0, 0.0, 0.0 ) ) ;
#197279 = DIRECTION ( '', ( 0.0, 0.0, 1.0 ) ) ;
#197280 = DIRECTION ( '', ( 1.0, 0.0, 0.0 ) ) ;
#197281 = AXIS2_PLACEMENT_3D ( '', #197278, #197279, #197280 ) ;
#197282 = NEXT_ASSEMBLY_USAGE_OCCURRENCE ( 'Exit Pallet Nib:1', 'Exit Pallet Nib:1', 'Exit Pallet Nib:1', #196754, #196858, $ ) ;
#197283 = PRODUCT_DEFINITION_SHAPE ( '', '', #197282 ) ;
#197284 = ITEM_DEFINED_TRANSFORMATION ( '', '', #197277, #197281 ) ;
#197285 = ( REPRESENTATION_RELATIONSHIP ( '', '', #196855, #196751 ) REPRESENTATION_RELATIONSHIP_WITH_TRANSFORMATION ( #197284 ) SHAPE_REPRESENTATION_RELATIONSHIP ( ) ) ;
#197286 = CONTEXT_DEPENDENT_SHAPE_REPRESENTATION ( #197285, #197283 ) ;
#197287 = CARTESIAN_POINT ( '', ( 0.0, 0.0, 0.0 ) ) ;
#197288 = DIRECTION ( '', ( 0.0, 0.0, 1.0 ) ) ;
#197289 = DIRECTION ( '', ( 1.0, 0.0, 0.0 ) ) ;
#197290 = AXIS2_PLACEMENT_3D ( '', #197287, #197288, #197289 ) ;
#197291 = CARTESIAN_POINT ( '', ( 0.0, 0.0, 0.0 ) ) ;
#197292 = DIRECTION ( '', ( 0.0, 0.0, 1.0 ) ) ;
#197293 = DIRECTION ( '', ( 1.0, 0.0, 0.0 ) ) ;
#197294 = AXIS2_PLACEMENT_3D ( '', #197291, #197292, #197293 ) ;
#197295 = NEXT_ASSEMBLY_USAGE_OCCURRENCE ( 'Pivot Collar:1', 'Pivot Collar:1', 'Pivot Collar:1', #196754, #196882, $ ) ;
#197296 = PRODUCT_DEFINITION_SHAPE ( '', '', #197295 ) ;
#197297 = ITEM_DEFINED_TRANSFORMATION ( '', '', #197290, #197294 ) ;
#197298 = ( REPRESENTATION_RELATIONSHIP ( '', '', #196879, #196751 ) REPRESENTATION_RELATIONSHIP_WITH_TRANSFORMATION ( #197297 ) SHAPE_REPRESENTATION_RELATIONSHIP ( ) ) ;
#197299 = CONTEXT_DEPENDENT_SHAPE_REPRESENTATION ( #197298, #197296 ) ;
#197304 = CARTESIAN_POINT ( '', ( 0.0, 0.0, 0.0 ) ) ;
#197305 = DIRECTION ( '', ( 0.0, 0.0, 1.0 ) ) ;
#197306 = DIRECTION ( '', ( 1.0, 0.0, 0.0 ) ) ;
#197307 = AXIS2_PLACEMENT_3D ( '', #197304, #197305, #197306 ) ;
#197313 = CARTESIAN_POINT ( '', ( 0.0, 0.0, 0.0 ) ) ;
#197314 = DIRECTION ( '', ( 0.0, 0.0, 1.0 ) ) ;
#197315 = DIRECTION ( '', ( 1.0, 0.0, 0.0 ) ) ;
#197316 = AXIS2_PLACEMENT_3D ( '', #197313, #197314, #197315 ) ;
#197317 = CARTESIAN_POINT ( '', ( 0.0, 0.0, 0.0 ) ) ;
#197318 = DIRECTION ( '', ( 0.0, 0.0, 1.0 ) ) ;
#197319 = DIRECTION ( '', ( 1.0, 0.0, 0.0 ) ) ;
#197320 = AXIS2_PLACEMENT_3D ( '', #197317, #197318, #197319 ) ;
#197321 = NEXT_ASSEMBLY_USAGE_OCCURRENCE ( 'Entry Pallet Arm:1', 'Entry Pallet Arm:1', 'Entry Pallet Arm:1', #196754, #196930, $ ) ;
#197322 = PRODUCT_DEFINITION_SHAPE ( '', '', #197321 ) ;
#197323 = ITEM_DEFINED_TRANSFORMATION ( '', '', #197316, #197320 ) ;
#197324 = ( REPRESENTATION_RELATIONSHIP ( '', '', #196927, #196751 ) REPRESENTATION_RELATIONSHIP_WITH_TRANSFORMATION ( #197323 ) SHAPE_REPRESENTATION_RELATIONSHIP ( ) ) ;
#197325 = CONTEXT_DEPENDENT_SHAPE_REPRESENTATION ( #197324, #197322 ) ;
#197326 = CARTESIAN_POINT ( '', ( 0.0, 0.0, 0.0 ) ) ;
#197327 = DIRECTION ( '', ( 0.0, 0.0, 1.0 ) ) ;
#197328 = DIRECTION ( '', ( 1.0, 0.0, 0.0 ) ) ;
#197329 = AXIS2_PLACEMENT_3D ( '', #197326, #197327, #197328 ) ;
#197330 = CARTESIAN_POINT ( '', ( 0.0, 0.0, 0.0 ) ) ;
#197331 = DIRECTION ( '', ( 0.0, 0.0, 1.0 ) ) ;
#197332 = DIRECTION ( '', ( 1.0, 0.0, 0.0 ) ) ;
#197333 = AXIS2_PLACEMENT_3D ( '', #197330, #197331, #197332 ) ;
#197334 = NEXT_ASSEMBLY_USAGE_OCCURRENCE ( 'Exit Pallet Arm:1', 'Exit Pallet Arm:1', 'Exit Pallet Arm:1', #196754, #196954, $ ) ;
#197335 = PRODUCT_DEFINITION_SHAPE ( '', '', #197334 ) ;
#197336 = ITEM_DEFINED_TRANSFORMATION ( '', '', #197329, #197333 ) ;
#197337 = ( REPRESENTATION_RELATIONSHIP ( '', '', #196951, #196751 ) REPRESENTATION_RELATIONSHIP_WITH_TRANSFORMATION ( #197336 ) SHAPE_REPRESENTATION_RELATIONSHIP ( ) ) ;
#197338 = CONTEXT_DEPENDENT_SHAPE_REPRESENTATION ( #197337, #197335 ) ;
#197339 = CARTESIAN_POINT ( '', ( 0.0, 0.0, 0.0 ) ) ;
#197340 = DIRECTION ( '', ( 0.0, 0.0, 1.0 ) ) ;
#197341 = DIRECTION ( '', ( 1.0, 0.0, 0.0 ) ) ;
#197342 = AXIS2_PLACEMENT_3D ( '', #197339, #197340, #197341 ) ;
#197343 = CARTESIAN_POINT ( '', ( 0.0, 0.0, 0.0 ) ) ;
#197344 = DIRECTION ( '', ( 0.0, 0.0, 1.0 ) ) ;
#197345 = DIRECTION ( '', ( 1.0, 0.0, 0.0 ) ) ;
#197346 = AXIS2_PLACEMENT_3D ( '', #197343, #197344, #197345 ) ;
#197347 = NEXT_ASSEMBLY_USAGE_OCCURRENCE ( 'Pallet Pivot Pin:1', 'Pallet Pivot Pin:1', 'Pallet Pivot Pin:1', #196754, #196978, $ ) ;
#197348 = PRODUCT_DEFINITION_SHAPE ( '', '', #197347 ) ;
#197349 = ITEM_DEFINED_TRANSFORMATION ( '', '', #197342, #197346 ) ;
#197350 = ( REPRESENTATION_RELATIONSHIP ( '', '', #196975, #196751 ) REPRESENTATION_RELATIONSHIP_WITH_TRANSFORMATION ( #197349 ) SHAPE_REPRESENTATION_RELATIONSHIP ( ) ) ;
#197351 = CONTEXT_DEPENDENT_SHAPE_REPRESENTATION ( #197350, #197348 ) ;
#197352 = CARTESIAN_POINT ( '', ( 0.0, 0.0, 0.0 ) ) ;
#197353 = DIRECTION ( '', ( 0.0, 0.0, 1.0 ) ) ;
#197354 = DIRECTION ( '', ( 1.0, 0.0, 0.0 ) ) ;
#197355 = AXIS2_PLACEMENT_3D ( '', #197352, #197353, #197354 ) ;
#197356 = CARTESIAN_POINT ( '', ( 0.0, 0.0, 0.0 ) ) ;
#197357 = DIRECTION ( '', ( 0.0, 0.0, 1.0 ) ) ;
#197358 = DIRECTION ( '', ( 1.0, 0.0, 0.0 ) ) ;
#197359 = AXIS2_PLACEMENT_3D ( '', #197356, #197357, #197358 ) ;
#197360 = NEXT_ASSEMBLY_USAGE_OCCURRENCE ( 'Composer Arm:1', 'Composer Arm:1', 'Composer Arm:1', #196754, #197002, $ ) ;
#197361 = PRODUCT_DEFINITION_SHAPE ( '', '', #197360 ) ;
#197362 = ITEM_DEFINED_TRANSFORMATION ( '', '', #197355, #197359 ) ;
#197363 = ( REPRESENTATION_RELATIONSHIP ( '', '', #196999, #196751 ) REPRESENTATION_RELATIONSHIP_WITH_TRANSFORMATION ( #197362 ) SHAPE_REPRESENTATION_RELATIONSHIP ( ) ) ;
#197364 = CONTEXT_DEPENDENT_SHAPE_REPRESENTATION ( #197363, #197361 ) ;
#197365 = CARTESIAN_POINT ( '', ( 0.0, 0.0, 0.0 ) ) ;
#197366 = DIRECTION ( '', ( 0.0, 0.0, 1.0 ) ) ;
#197367 = DIRECTION ( '', ( 1.0, 0.0, 0.0 ) ) ;
#197368 = AXIS2_PLACEMENT_3D ( '', #197365, #197366, #197367 ) ;
#197369 = CARTESIAN_POINT ( '', ( 0.0, 0.0, 0.0 ) ) ;
#197370 = DIRECTION ( '', ( 0.0, 0.0, 1.0 ) ) ;
#197371 = DIRECTION ( '', ( 1.0, 0.0, 0.0 ) ) ;
#197372 = AXIS2_PLACEMENT_3D ( '', #197369, #197370, #197371 ) ;
#197373 = NEXT_ASSEMBLY_USAGE_OCCURRENCE ( 'Composer Pin:1', 'Composer Pin:1', 'Composer Pin:1', #196754, #197026, $ ) ;
#197374 = PRODUCT_DEFINITION_SHAPE ( '', '', #197373 ) ;
#197375 = ITEM_DEFINED_TRANSFORMATION ( '', '', #197368, #197372 ) ;
#197376 = ( REPRESENTATION_RELATIONSHIP ( '', '', #197023, #196751 ) REPRESENTATION_RELATIONSHIP_WITH_TRANSFORMATION ( #197375 ) SHAPE_REPRESENTATION_RELATIONSHIP ( ) ) ;
#197377 = CONTEXT_DEPENDENT_SHAPE_REPRESENTATION ( #197376, #197374 ) ;
#197382 = CARTESIAN_POINT ( '', ( 0.0, 0.0, 0.0 ) ) ;
#197383 = DIRECTION ( '', ( 0.0, 0.0, 1.0 ) ) ;
#197384 = DIRECTION ( '', ( 1.0, 0.0, 0.0 ) ) ;
#197385 = AXIS2_PLACEMENT_3D ( '', #197382, #197383, #197384 ) ;
#197391 = CARTESIAN_POINT ( '', ( 0.0, 0.0, 0.0 ) ) ;
#197392 = DIRECTION ( '', ( 0.0, 0.0, 1.0 ) ) ;
#197393 = DIRECTION ( '', ( 1.0, 0.0, 0.0 ) ) ;
#197394 = AXIS2_PLACEMENT_3D ( '', #197391, #197392, #197393 ) ;
#197395 = CARTESIAN_POINT ( '', ( 0.0, 0.0, 0.0 ) ) ;
#197396 = DIRECTION ( '', ( 0.0, 0.0, 1.0 ) ) ;
#197397 = DIRECTION ( '', ( 1.0, 0.0, 0.0 ) ) ;
#197398 = AXIS2_PLACEMENT_3D ( '', #197395, #197396, #197397 ) ;
#197399 = NEXT_ASSEMBLY_USAGE_OCCURRENCE ( 'Entry Return Spring:1', 'Entry Return Spring:1', 'Entry Return Spring:1', #196754, #197074, $ ) ;
#197400 = PRODUCT_DEFINITION_SHAPE ( '', '', #197399 ) ;
#197401 = ITEM_DEFINED_TRANSFORMATION ( '', '', #197394, #197398 ) ;
#197402 = ( REPRESENTATION_RELATIONSHIP ( '', '', #197071, #196751 ) REPRESENTATION_RELATIONSHIP_WITH_TRANSFORMATION ( #197401 ) SHAPE_REPRESENTATION_RELATIONSHIP ( ) ) ;
#197403 = CONTEXT_DEPENDENT_SHAPE_REPRESENTATION ( #197402, #197400 ) ;
#197404 = CARTESIAN_POINT ( '', ( 0.0, 0.0, 0.0 ) ) ;
#197405 = DIRECTION ( '', ( 0.0, 0.0, 1.0 ) ) ;
#197406 = DIRECTION ( '', ( 1.0, 0.0, 0.0 ) ) ;
#197407 = AXIS2_PLACEMENT_3D ( '', #197404, #197405, #197406 ) ;
#197408 = CARTESIAN_POINT ( '', ( 0.0, 0.0, 0.0 ) ) ;
#197409 = DIRECTION ( '', ( 0.0, 0.0, 1.0 ) ) ;
#197410 = DIRECTION ( '', ( 1.0, 0.0, 0.0 ) ) ;
#197411 = AXIS2_PLACEMENT_3D ( '', #197408, #197409, #197410 ) ;
#197412 = NEXT_ASSEMBLY_USAGE_OCCURRENCE ( 'Entry Stop Pin:1', 'Entry Stop Pin:1', 'Entry Stop Pin:1', #196754, #197098, $ ) ;
#197413 = PRODUCT_DEFINITION_SHAPE ( '', '', #197412 ) ;
#197414 = ITEM_DEFINED_TRANSFORMATION ( '', '', #197407, #197411 ) ;
#197415 = ( REPRESENTATION_RELATIONSHIP ( '', '', #197095, #196751 ) REPRESENTATION_RELATIONSHIP_WITH_TRANSFORMATION ( #197414 ) SHAPE_REPRESENTATION_RELATIONSHIP ( ) ) ;
#197416 = CONTEXT_DEPENDENT_SHAPE_REPRESENTATION ( #197415, #197413 ) ;
#197417 = CARTESIAN_POINT ( '', ( 0.0, 0.0, 0.0 ) ) ;
#197418 = DIRECTION ( '', ( 0.0, 0.0, 1.0 ) ) ;
#197419 = DIRECTION ( '', ( 1.0, 0.0, 0.0 ) ) ;
#197420 = AXIS2_PLACEMENT_3D ( '', #197417, #197418, #197419 ) ;
#197421 = CARTESIAN_POINT ( '', ( 0.0, 0.0, 0.0 ) ) ;
#197422 = DIRECTION ( '', ( 0.0, 0.0, 1.0 ) ) ;
#197423 = DIRECTION ( '', ( 1.0, 0.0, 0.0 ) ) ;
#197424 = AXIS2_PLACEMENT_3D ( '', #197421, #197422, #197423 ) ;
#197425 = NEXT_ASSEMBLY_USAGE_OCCURRENCE ( 'Exit Stop Pin:1', 'Exit Stop Pin:1', 'Exit Stop Pin:1', #196754, #197122, $ ) ;
#197426 = PRODUCT_DEFINITION_SHAPE ( '', '', #197425 ) ;
#197427 = ITEM_DEFINED_TRANSFORMATION ( '', '', #197420, #197424 ) ;
#197428 = ( REPRESENTATION_RELATIONSHIP ( '', '', #197119, #196751 ) REPRESENTATION_RELATIONSHIP_WITH_TRANSFORMATION ( #197427 ) SHAPE_REPRESENTATION_RELATIONSHIP ( ) ) ;
#197429 = CONTEXT_DEPENDENT_SHAPE_REPRESENTATION ( #197428, #197426 ) ;
#197430 = CARTESIAN_POINT ( '', ( 0.0, 0.0, 0.0 ) ) ;
#197431 = DIRECTION ( '', ( 0.0, 0.0, 1.0 ) ) ;
#197432 = DIRECTION ( '', ( 1.0, 0.0, 0.0 ) ) ;
#197433 = AXIS2_PLACEMENT_3D ( '', #197430, #197431, #197432 ) ;
#197434 = CARTESIAN_POINT ( '', ( 0.0, 0.0, 0.0 ) ) ;
#197435 = DIRECTION ( '', ( 0.0, 0.0, 1.0 ) ) ;
#197436 = DIRECTION ( '', ( 1.0, 0.0, 0.0 ) ) ;
#197437 = AXIS2_PLACEMENT_3D ( '', #197434, #197435, #197436 ) ;
#197438 = NEXT_ASSEMBLY_USAGE_OCCURRENCE ( 'Exit Return Spring:1', 'Exit Return Spring:1', 'Exit Return Spring:1', #196754, #197146, $ ) ;
#197439 = PRODUCT_DEFINITION_SHAPE ( '', '', #197438 ) ;
#197440 = ITEM_DEFINED_TRANSFORMATION ( '', '', #197433, #197437 ) ;
#197441 = ( REPRESENTATION_RELATIONSHIP ( '', '', #197143, #196751 ) REPRESENTATION_RELATIONSHIP_WITH_TRANSFORMATION ( #197440 ) SHAPE_REPRESENTATION_RELATIONSHIP ( ) ) ;
#197442 = CONTEXT_DEPENDENT_SHAPE_REPRESENTATION ( #197441, #197439 ) ;
#197443 = CARTESIAN_POINT ( '', ( 0.0, 0.0, 0.0 ) ) ;
#197444 = DIRECTION ( '', ( 0.0, 0.0, 1.0 ) ) ;
#197445 = DIRECTION ( '', ( 1.0, 0.0, 0.0 ) ) ;
#197446 = AXIS2_PLACEMENT_3D ( '', #197443, #197444, #197445 ) ;
#197447 = CARTESIAN_POINT ( '', ( 0.0, 0.0, 0.0 ) ) ;
#197448 = DIRECTION ( '', ( 0.0, 0.0, 1.0 ) ) ;
#197449 = DIRECTION ( '', ( 1.0, 0.0, 0.0 ) ) ;
#197450 = AXIS2_PLACEMENT_3D ( '', #197447, #197448, #197449 ) ;
#197451 = NEXT_ASSEMBLY_USAGE_OCCURRENCE ( 'Lever Arm:1', 'Lever Arm:1', 'Lever Arm:1', #196754, #197170, $ ) ;
#197452 = PRODUCT_DEFINITION_SHAPE ( '', '', #197451 ) ;
#197453 = ITEM_DEFINED_TRANSFORMATION ( '', '', #197446, #197450 ) ;
#197454 = ( REPRESENTATION_RELATIONSHIP ( '', '', #197167, #196751 ) REPRESENTATION_RELATIONSHIP_WITH_TRANSFORMATION ( #197453 ) SHAPE_REPRESENTATION_RELATIONSHIP ( ) ) ;
#197455 = CONTEXT_DEPENDENT_SHAPE_REPRESENTATION ( #197454, #197452 ) ;
#197456 = CARTESIAN_POINT ( '', ( 0.0, 0.0, 0.0 ) ) ;
#197457 = DIRECTION ( '', ( 0.0, 0.0, 1.0 ) ) ;
#197458 = DIRECTION ( '', ( 1.0, 0.0, 0.0 ) ) ;
#197459 = AXIS2_PLACEMENT_3D ( '', #197456, #197457, #197458 ) ;
#197460 = CARTESIAN_POINT ( '', ( 0.0, 0.0, 0.0 ) ) ;
#197461 = DIRECTION ( '', ( 0.0, 0.0, 1.0 ) ) ;
#197462 = DIRECTION ( '', ( 1.0, 0.0, 0.0 ) ) ;
#197463 = AXIS2_PLACEMENT_3D ( '', #197460, #197461, #197462 ) ;
#197464 = NEXT_ASSEMBLY_USAGE_OCCURRENCE ( 'Escape Wheel Hub:1', 'Escape Wheel Hub:1', 'Escape Wheel Hub:1', #196754, #197194, $ ) ;
#197465 = PRODUCT_DEFINITION_SHAPE ( '', '', #197464 ) ;
#197466 = ITEM_DEFINED_TRANSFORMATION ( '', '', #197459, #197463 ) ;
#197467 = ( REPRESENTATION_RELATIONSHIP ( '', '', #197191, #196751 ) REPRESENTATION_RELATIONSHIP_WITH_TRANSFORMATION ( #197466 ) SHAPE_REPRESENTATION_RELATIONSHIP ( ) ) ;
#197468 = CONTEXT_DEPENDENT_SHAPE_REPRESENTATION ( #197467, #197465 ) ;
#197469 = CARTESIAN_POINT ( '', ( 0.0, 0.0, 0.0 ) ) ;
#197470 = DIRECTION ( '', ( 0.0, 0.0, 1.0 ) ) ;
#197471 = DIRECTION ( '', ( 1.0, 0.0, 0.0 ) ) ;
#197472 = AXIS2_PLACEMENT_3D ( '', #197469, #197470, #197471 ) ;
#197473 = CARTESIAN_POINT ( '', ( 0.0, 0.0, 0.0 ) ) ;
#197474 = DIRECTION ( '', ( 0.0, 0.0, 1.0 ) ) ;
#197475 = DIRECTION ( '', ( 1.0, 0.0, 0.0 ) ) ;
#197476 = AXIS2_PLACEMENT_3D ( '', #197473, #197474, #197475 ) ;
#197477 = NEXT_ASSEMBLY_USAGE_OCCURRENCE ( 'Escape Wheel:1', 'Escape Wheel:1', 'Escape Wheel:1', #196754, #197218, $ ) ;
#197478 = PRODUCT_DEFINITION_SHAPE ( '', '', #197477 ) ;
#197479 = ITEM_DEFINED_TRANSFORMATION ( '', '', #197472, #197476 ) ;
#197480 = ( REPRESENTATION_RELATIONSHIP ( '', '', #197215, #196751 ) REPRESENTATION_RELATIONSHIP_WITH_TRANSFORMATION ( #197479 ) SHAPE_REPRESENTATION_RELATIONSHIP ( ) ) ;
#197481 = CONTEXT_DEPENDENT_SHAPE_REPRESENTATION ( #197480, #197478 ) ;
#197482 = CARTESIAN_POINT ( '', ( 0.0, 0.0, 0.0 ) ) ;
#197483 = DIRECTION ( '', ( 0.0, 0.0, 1.0 ) ) ;
#197484 = DIRECTION ( '', ( 1.0, 0.0, 0.0 ) ) ;
#197485 = AXIS2_PLACEMENT_3D ( '', #197482, #197483, #197484 ) ;
#197486 = CARTESIAN_POINT ( '', ( 40.88338128606348, -3.637250500787559e-10, 13.995213900775354 ) ) ;
#197487 = DIRECTION ( '', ( -0.6128276062588245, 4.721437080032287e-12, 0.7902166316948026 ) ) ;
#197488 = DIRECTION ( '', ( -0.7902166316948023, 1.1269926107657996e-11, -0.6128276062588244 ) ) ;
#197489 = AXIS2_PLACEMENT_3D ( '', #197486, #197487, #197488 ) ;
#197490 = NEXT_ASSEMBLY_USAGE_OCCURRENCE ( 'Pivot Collar:2', 'Pivot Collar:2', 'Pivot Collar:2', #196754, #196882, $ ) ;
#197491 = PRODUCT_DEFINITION_SHAPE ( '', '', #197490 ) ;
#197492 = ITEM_DEFINED_TRANSFORMATION ( '', '', #197485, #197489 ) ;
#197493 = ( REPRESENTATION_RELATIONSHIP ( '', '', #196879, #196751 ) REPRESENTATION_RELATIONSHIP_WITH_TRANSFORMATION ( #197492 ) SHAPE_REPRESENTATION_RELATIONSHIP ( ) ) ;
#197494 = CONTEXT_DEPENDENT_SHAPE_REPRESENTATION ( #197493, #197491 ) ;
#197495 = CARTESIAN_POINT ( '', ( 0.0, 0.0, 0.0 ) ) ;
#197496 = DIRECTION ( '', ( 0.0, 0.0, 1.0 ) ) ;
#197497 = DIRECTION ( '', ( 1.0, 0.0, 0.0 ) ) ;
#197498 = AXIS2_PLACEMENT_3D ( '', #197495, #197496, #197497 ) ;
#197499 = CARTESIAN_POINT ( '', ( 23.307294819665387, -0.03150291979418096, 7.978426381042212 ) ) ;
#197500 = DIRECTION ( '', ( -7.833635727991909e-06, 0.00022072381488468602, 0.9999999756098156 ) ) ;
#197501 = DIRECTION ( '', ( 0.9999999970899505, -7.588458708888394e-05, 7.850385432332785e-06 ) ) ;
#197502 = AXIS2_PLACEMENT_3D ( '', #197499, #197500, #197501 ) ;
#197503 = NEXT_ASSEMBLY_USAGE_OCCURRENCE ( 'Composer Pin:2', 'Composer Pin:2', 'Composer Pin:2', #196754, #197026, $ ) ;
#197504 = PRODUCT_DEFINITION_SHAPE ( '', '', #197503 ) ;
#197505 = ITEM_DEFINED_TRANSFORMATION ( '', '', #197498, #197502 ) ;
#197506 = ( REPRESENTATION_RELATIONSHIP ( '', '', #197023, #196751 ) REPRESENTATION_RELATIONSHIP_WITH_TRANSFORMATION ( #197505 ) SHAPE_REPRESENTATION_RELATIONSHIP ( ) ) ;
#197507 = CONTEXT_DEPENDENT_SHAPE_REPRESENTATION ( #197506, #197504 ) ;
ENDSEC;
END-ISO-10303-21;
